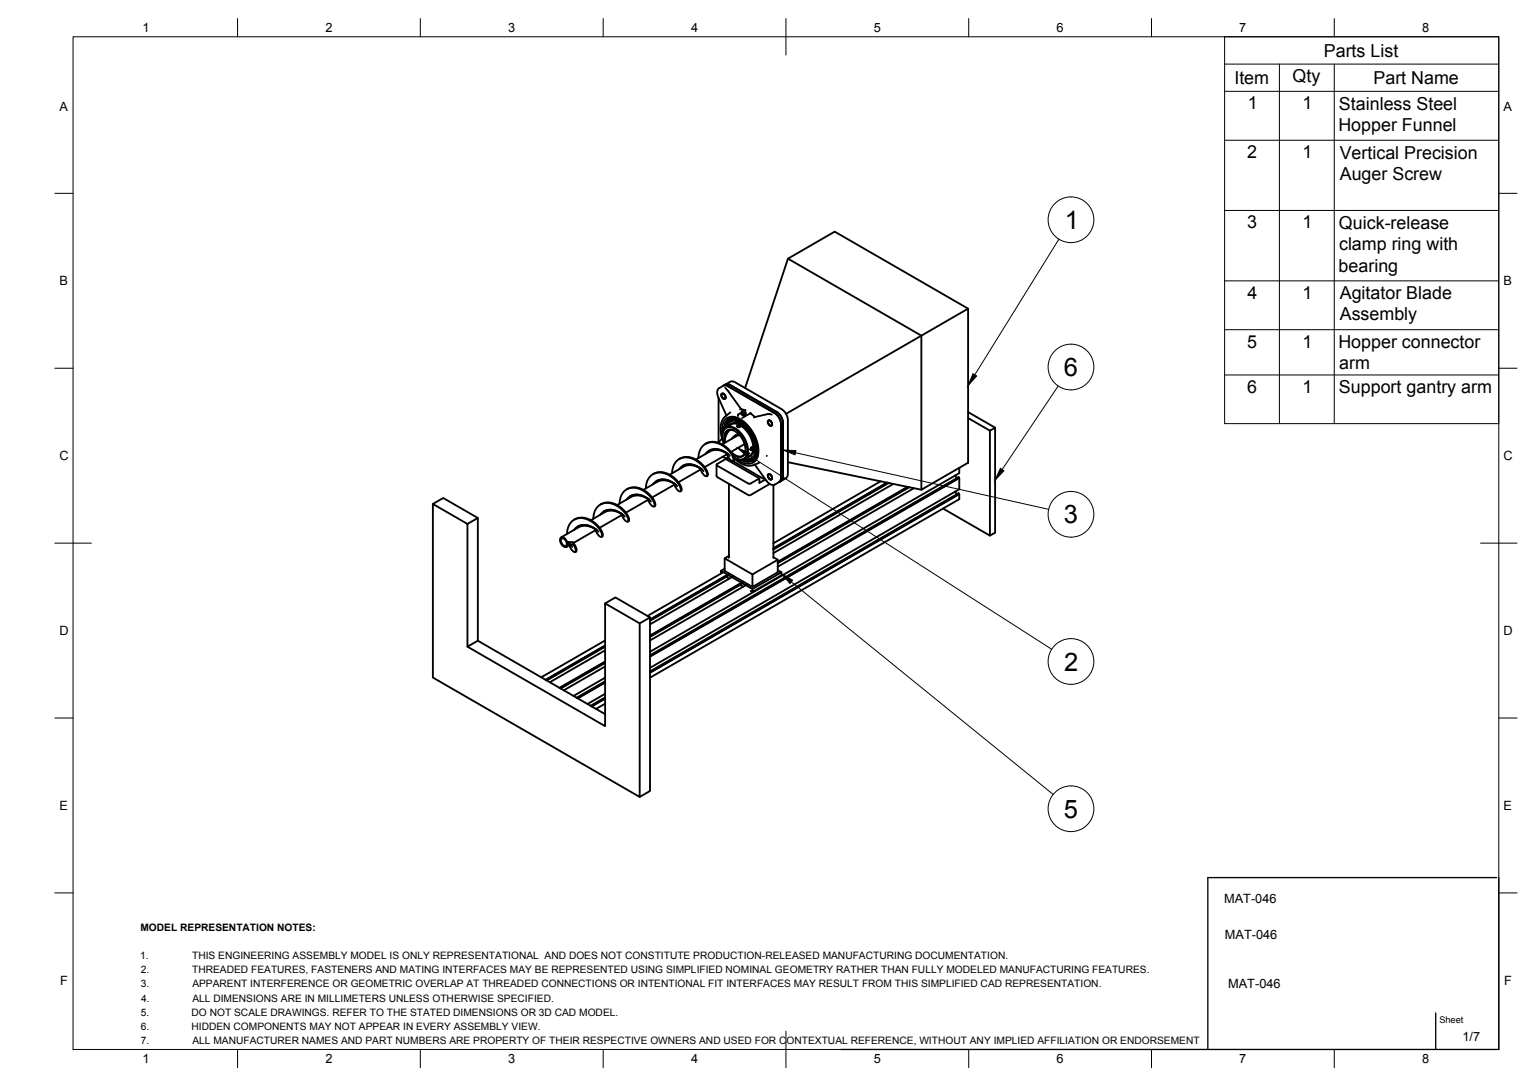
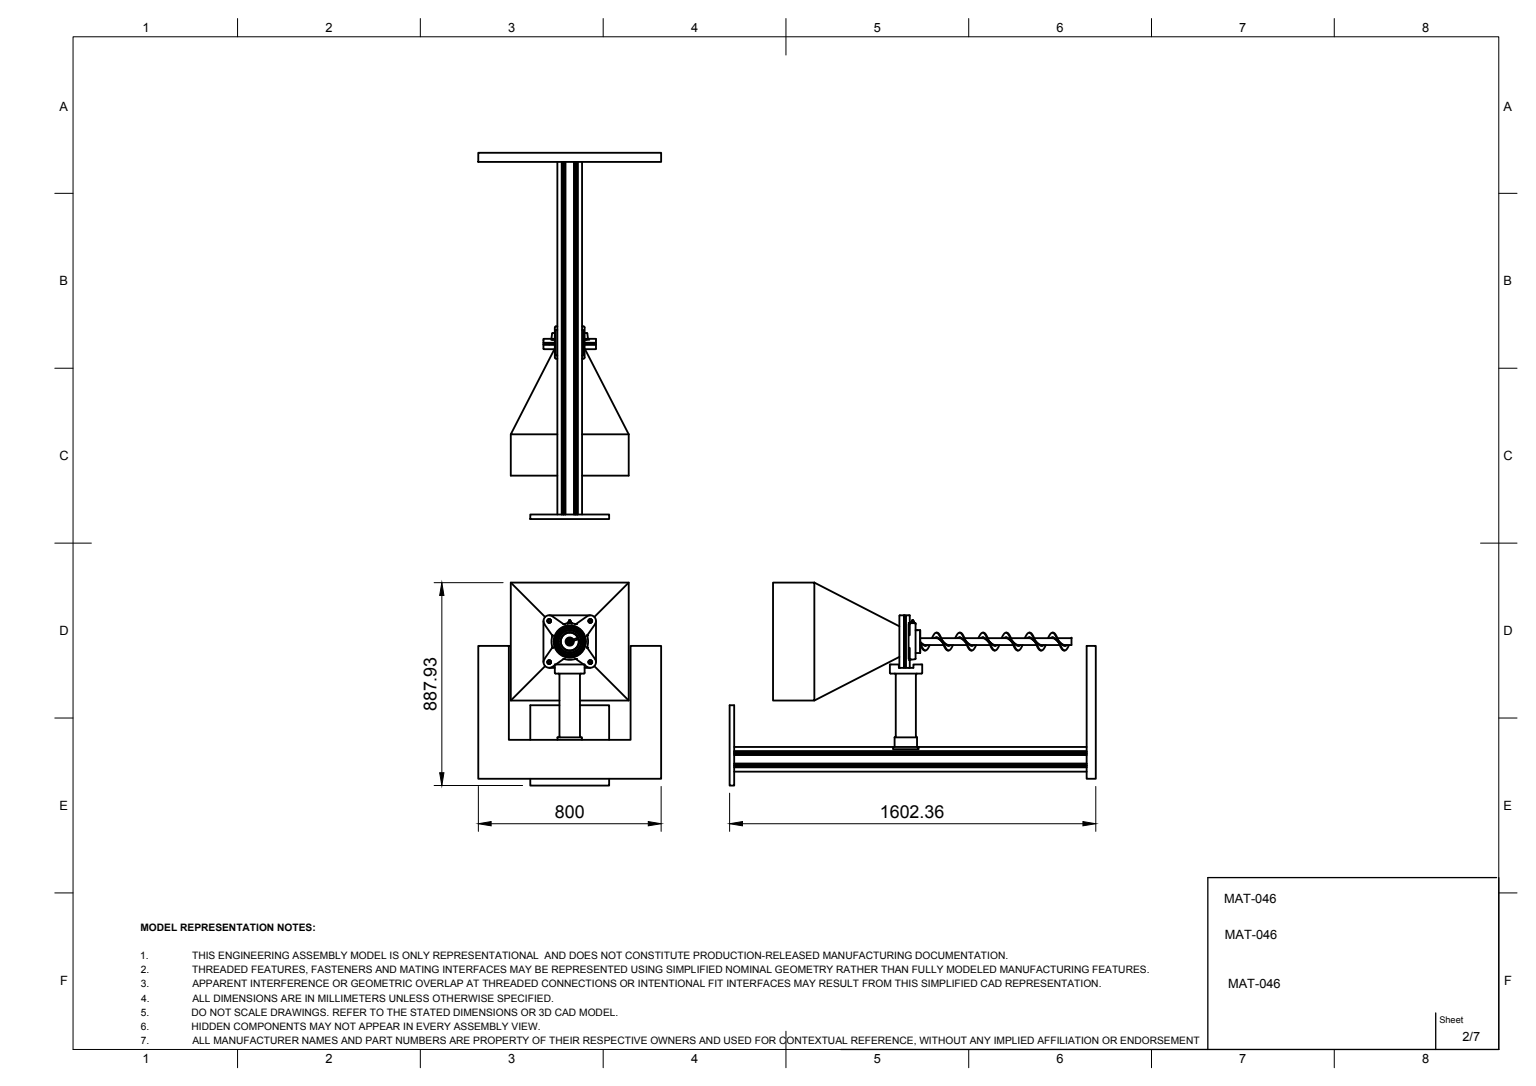
ISO-10303-21;
HEADER;
/* Generated by software containing ST-Developer
 * from STEP Tools, Inc. (www.steptools.com) 
 */

FILE_DESCRIPTION(
/* description */ ('STEP AP214'),
/* implementation_level */ '2;1');

FILE_NAME(
/* name */ 'MAT-046.step',
/* time_stamp */ '2026-11-14T22:16:48-08:00',
/* author */ (''),
/* organization */ (''),
/* preprocessor_version */ 'ST-DEVELOPER v20.2',
/* originating_system */ 'Autodesk Translation Framework v15.17.0.0',
/* authorisation */ '');

FILE_SCHEMA (('AUTOMOTIVE_DESIGN { 1 0 10303 214 3 1 1 }'));
ENDSEC;

DATA;
#10=MECHANICAL_DESIGN_GEOMETRIC_PRESENTATION_REPRESENTATION('',(#5472,#5473,
#5474,#5475,#5476,#5477,#5478,#5479,#5480,#5481,#5482,#5483,#5484,#5485,
#5486,#5487,#5488,#5489,#5490,#5491,#5492,#5493,#5494,#5495,#5496,#5497,
#5498,#5499,#5500),#276462);
#11=ITEM_DEFINED_TRANSFORMATION($,$,#98803,#111667);
#12=ITEM_DEFINED_TRANSFORMATION($,$,#98875,#111668);
#13=ITEM_DEFINED_TRANSFORMATION($,$,#98939,#111669);
#14=ITEM_DEFINED_TRANSFORMATION($,$,#110834,#111670);
#15=ITEM_DEFINED_TRANSFORMATION($,$,#110875,#111671);
#16=ITEM_DEFINED_TRANSFORMATION($,$,#110986,#111672);
#17=(
REPRESENTATION_RELATIONSHIP($,$,#276488,#276487)
REPRESENTATION_RELATIONSHIP_WITH_TRANSFORMATION(#11)
SHAPE_REPRESENTATION_RELATIONSHIP()
);
#18=(
REPRESENTATION_RELATIONSHIP($,$,#276489,#276487)
REPRESENTATION_RELATIONSHIP_WITH_TRANSFORMATION(#12)
SHAPE_REPRESENTATION_RELATIONSHIP()
);
#19=(
REPRESENTATION_RELATIONSHIP($,$,#276490,#276487)
REPRESENTATION_RELATIONSHIP_WITH_TRANSFORMATION(#13)
SHAPE_REPRESENTATION_RELATIONSHIP()
);
#20=(
REPRESENTATION_RELATIONSHIP($,$,#276491,#276487)
REPRESENTATION_RELATIONSHIP_WITH_TRANSFORMATION(#14)
SHAPE_REPRESENTATION_RELATIONSHIP()
);
#21=(
REPRESENTATION_RELATIONSHIP($,$,#276492,#276487)
REPRESENTATION_RELATIONSHIP_WITH_TRANSFORMATION(#15)
SHAPE_REPRESENTATION_RELATIONSHIP()
);
#22=(
REPRESENTATION_RELATIONSHIP($,$,#276493,#276487)
REPRESENTATION_RELATIONSHIP_WITH_TRANSFORMATION(#16)
SHAPE_REPRESENTATION_RELATIONSHIP()
);
#23=CONTEXT_DEPENDENT_SHAPE_REPRESENTATION(#17,#276481);
#24=CONTEXT_DEPENDENT_SHAPE_REPRESENTATION(#18,#276482);
#25=CONTEXT_DEPENDENT_SHAPE_REPRESENTATION(#19,#276483);
#26=CONTEXT_DEPENDENT_SHAPE_REPRESENTATION(#20,#276484);
#27=CONTEXT_DEPENDENT_SHAPE_REPRESENTATION(#21,#276485);
#28=CONTEXT_DEPENDENT_SHAPE_REPRESENTATION(#22,#276486);
#29=NEXT_ASSEMBLY_USAGE_OCCURRENCE('Stainless Steel Hopper Funnel:1',
'Stainless Steel Hopper Funnel:1','Stainless Steel Hopper Funnel:1',#276495,
#276496,'Stainless Steel Hopper Funnel:1');
#30=NEXT_ASSEMBLY_USAGE_OCCURRENCE('Vertical Precision Auger Screw:1',
'Vertical Precision Auger Screw:1','Vertical Precision Auger Screw:1',#276495,
#276497,'Vertical Precision Auger Screw:1');
#31=NEXT_ASSEMBLY_USAGE_OCCURRENCE(
'Quick-release clamp ring with bearing:1',
'Quick-release clamp ring with bearing:1',
'Quick-release clamp ring with bearing:1',#276495,#276498,
'Quick-release clamp ring with bearing:1');
#32=NEXT_ASSEMBLY_USAGE_OCCURRENCE('Agitator Blade Assembly:1',
'Agitator Blade Assembly:1','Agitator Blade Assembly:1',#276495,#276499,
'Agitator Blade Assembly:1');
#33=NEXT_ASSEMBLY_USAGE_OCCURRENCE('hopper connector arm:1',
'hopper connector arm:1','hopper connector arm:1',#276495,#276500,
'hopper connector arm:1');
#34=NEXT_ASSEMBLY_USAGE_OCCURRENCE('support gantry arm:1',
'support gantry arm:1','support gantry arm:1',#276495,#276501,
'support gantry arm:1');
#35=ORIENTED_CLOSED_SHELL('',*,#98725,.F.);
#36=ORIENTED_CLOSED_SHELL('',*,#98726,.F.);
#37=ORIENTED_CLOSED_SHELL('',*,#98727,.F.);
#38=ORIENTED_CLOSED_SHELL('',*,#98728,.F.);
#39=ORIENTED_CLOSED_SHELL('',*,#98729,.F.);
#40=ORIENTED_CLOSED_SHELL('',*,#98730,.F.);
#41=ORIENTED_CLOSED_SHELL('',*,#98731,.F.);
#42=ORIENTED_CLOSED_SHELL('',*,#98732,.F.);
#43=ORIENTED_CLOSED_SHELL('',*,#98733,.F.);
#44=BREP_WITH_VOIDS('Body1',#98734,(#35,#36,#37,#38,#39,#40,#41,#42,#43));
#45=SPHERICAL_SURFACE('',#98960,3.37686862486535);
#46=SPHERICAL_SURFACE('',#110483,1.905);
#47=SPHERICAL_SURFACE('',#110485,1.905);
#48=SPHERICAL_SURFACE('',#110508,0.952499999999998);
#49=SPHERICAL_SURFACE('',#110528,3.17500000000001);
#50=CONICAL_SURFACE('',#98946,5.55625,1.0471975511966);
#51=CONICAL_SURFACE('',#98951,5.55625,1.0471975511966);
#52=CONICAL_SURFACE('',#98954,3.78554799125932,1.22012705768434);
#53=CONICAL_SURFACE('',#98966,2.40973730802039,0.353951387855692);
#54=CONICAL_SURFACE('',#98977,5.55625,1.0471975511966);
#55=CONICAL_SURFACE('',#98978,5.55625,1.0471975511966);
#56=CONICAL_SURFACE('',#98979,5.55625,1.0471975511966);
#57=CONICAL_SURFACE('',#98980,5.55625,1.0471975511966);
#58=CONICAL_SURFACE('',#98981,5.55625,1.0471975511966);
#59=CONICAL_SURFACE('',#98989,5.55625,1.0471975511966);
#60=CONICAL_SURFACE('',#98990,5.55625,1.0471975511966);
#61=CONICAL_SURFACE('',#98991,5.55625,1.0471975511966);
#62=CONICAL_SURFACE('',#98992,5.55625,1.0471975511966);
#63=CONICAL_SURFACE('',#98993,5.55625,1.0471975511966);
#64=CONICAL_SURFACE('',#99119,64.0080199038439,0.558505360638178);
#65=CONICAL_SURFACE('',#99120,62.2224557307631,0.558505360638175);
#66=CONICAL_SURFACE('',#99239,58.6605641730809,0.558505360638184);
#67=CONICAL_SURFACE('',#99359,56.875,0.558505360638184);
#68=CONICAL_SURFACE('',#99369,60.4792282238308,0.523598775598302);
#69=CONICAL_SURFACE('',#99374,61.15975,0.523598775598289);
#70=CONICAL_SURFACE('',#99398,60.4792282238308,0.523598775598302);
#71=CONICAL_SURFACE('',#99403,61.15975,0.523598775598289);
#72=CONICAL_SURFACE('',#99427,60.4792282238308,0.523598775598302);
#73=CONICAL_SURFACE('',#99432,61.15975,0.523598775598289);
#74=CONICAL_SURFACE('',#99456,60.4792282238308,0.523598775598302);
#75=CONICAL_SURFACE('',#99461,61.15975,0.523598775598289);
#76=CONICAL_SURFACE('',#99485,60.4792282238308,0.523598775598302);
#77=CONICAL_SURFACE('',#99490,61.15975,0.523598775598289);
#78=CONICAL_SURFACE('',#99514,60.4792282238308,0.523598775598302);
#79=CONICAL_SURFACE('',#99519,61.15975,0.523598775598289);
#80=CONICAL_SURFACE('',#99543,60.4792282238308,0.523598775598302);
#81=CONICAL_SURFACE('',#99548,61.15975,0.523598775598289);
#82=CONICAL_SURFACE('',#99572,60.4792282238308,0.523598775598302);
#83=CONICAL_SURFACE('',#99577,61.15975,0.523598775598289);
#84=CONICAL_SURFACE('',#99601,60.4792282238308,0.523598775598302);
#85=CONICAL_SURFACE('',#99606,61.15975,0.523598775598289);
#86=CONICAL_SURFACE('',#99630,60.4792282238308,0.523598775598302);
#87=CONICAL_SURFACE('',#99635,61.15975,0.523598775598289);
#88=CONICAL_SURFACE('',#99659,60.4792282238308,0.523598775598302);
#89=CONICAL_SURFACE('',#99664,61.15975,0.523598775598289);
#90=CONICAL_SURFACE('',#99688,60.4792282238308,0.523598775598302);
#91=CONICAL_SURFACE('',#99693,61.15975,0.523598775598289);
#92=CONICAL_SURFACE('',#99717,60.4792282238308,0.523598775598302);
#93=CONICAL_SURFACE('',#99722,61.15975,0.523598775598289);
#94=CONICAL_SURFACE('',#99746,60.4792282238308,0.523598775598302);
#95=CONICAL_SURFACE('',#99751,61.15975,0.523598775598289);
#96=CONICAL_SURFACE('',#99775,60.4792282238308,0.523598775598302);
#97=CONICAL_SURFACE('',#99780,61.15975,0.523598775598289);
#98=CONICAL_SURFACE('',#99804,60.4792282238308,0.523598775598302);
#99=CONICAL_SURFACE('',#99809,61.15975,0.523598775598289);
#100=CONICAL_SURFACE('',#99833,60.4792282238308,0.523598775598302);
#101=CONICAL_SURFACE('',#99838,61.15975,0.523598775598289);
#102=CONICAL_SURFACE('',#99862,60.4792282238308,0.523598775598302);
#103=CONICAL_SURFACE('',#99867,61.15975,0.523598775598289);
#104=CONICAL_SURFACE('',#99891,60.4792282238308,0.523598775598302);
#105=CONICAL_SURFACE('',#99896,61.15975,0.523598775598289);
#106=CONICAL_SURFACE('',#99920,60.4792282238308,0.523598775598302);
#107=CONICAL_SURFACE('',#99925,61.15975,0.523598775598289);
#108=CONICAL_SURFACE('',#99949,60.4792282238308,0.523598775598302);
#109=CONICAL_SURFACE('',#99954,61.15975,0.523598775598289);
#110=CONICAL_SURFACE('',#99978,60.4792282238308,0.523598775598302);
#111=CONICAL_SURFACE('',#99983,61.15975,0.523598775598289);
#112=CONICAL_SURFACE('',#100007,60.4792282238308,0.523598775598302);
#113=CONICAL_SURFACE('',#100012,61.15975,0.523598775598289);
#114=CONICAL_SURFACE('',#100036,60.4792282238308,0.523598775598302);
#115=CONICAL_SURFACE('',#100041,61.15975,0.523598775598289);
#116=CONICAL_SURFACE('',#100065,60.4792282238308,0.523598775598302);
#117=CONICAL_SURFACE('',#100070,61.15975,0.523598775598289);
#118=CONICAL_SURFACE('',#100094,60.4792282238308,0.523598775598302);
#119=CONICAL_SURFACE('',#100099,61.15975,0.523598775598289);
#120=CONICAL_SURFACE('',#100123,60.4792282238308,0.523598775598302);
#121=CONICAL_SURFACE('',#100128,61.15975,0.523598775598289);
#122=CONICAL_SURFACE('',#100152,60.4792282238308,0.523598775598302);
#123=CONICAL_SURFACE('',#100157,61.15975,0.523598775598289);
#124=CONICAL_SURFACE('',#100181,60.4792282238308,0.523598775598302);
#125=CONICAL_SURFACE('',#100186,61.15975,0.523598775598289);
#126=CONICAL_SURFACE('',#100210,60.4792282238308,0.523598775598302);
#127=CONICAL_SURFACE('',#100215,61.15975,0.523598775598289);
#128=CONICAL_SURFACE('',#100239,60.4792282238308,0.523598775598302);
#129=CONICAL_SURFACE('',#100244,61.15975,0.523598775598289);
#130=CONICAL_SURFACE('',#100268,60.4792282238308,0.523598775598302);
#131=CONICAL_SURFACE('',#100273,61.15975,0.523598775598289);
#132=CONICAL_SURFACE('',#100297,60.4792282238308,0.523598775598302);
#133=CONICAL_SURFACE('',#100302,61.15975,0.523598775598289);
#134=CONICAL_SURFACE('',#100326,60.4792282238308,0.523598775598302);
#135=CONICAL_SURFACE('',#100331,61.15975,0.523598775598289);
#136=CONICAL_SURFACE('',#100355,60.4792282238308,0.523598775598302);
#137=CONICAL_SURFACE('',#100360,61.15975,0.523598775598289);
#138=CONICAL_SURFACE('',#100384,60.4792282238308,0.523598775598302);
#139=CONICAL_SURFACE('',#100389,61.15975,0.523598775598289);
#140=CONICAL_SURFACE('',#100413,60.4792282238308,0.523598775598302);
#141=CONICAL_SURFACE('',#100418,61.15975,0.523598775598289);
#142=CONICAL_SURFACE('',#100442,60.4792282238308,0.523598775598302);
#143=CONICAL_SURFACE('',#100447,61.15975,0.523598775598289);
#144=CONICAL_SURFACE('',#100471,60.4792282238308,0.523598775598302);
#145=CONICAL_SURFACE('',#100476,61.15975,0.523598775598289);
#146=CONICAL_SURFACE('',#100500,60.4792282238308,0.523598775598302);
#147=CONICAL_SURFACE('',#100505,61.15975,0.523598775598289);
#148=CONICAL_SURFACE('',#100529,60.4792282238308,0.523598775598302);
#149=CONICAL_SURFACE('',#100534,61.15975,0.523598775598289);
#150=CONICAL_SURFACE('',#100558,60.4792282238308,0.523598775598302);
#151=CONICAL_SURFACE('',#100563,61.15975,0.523598775598289);
#152=CONICAL_SURFACE('',#100587,60.4792282238308,0.523598775598302);
#153=CONICAL_SURFACE('',#100592,61.15975,0.523598775598289);
#154=CONICAL_SURFACE('',#100616,60.4792282238308,0.523598775598302);
#155=CONICAL_SURFACE('',#100621,61.15975,0.523598775598289);
#156=CONICAL_SURFACE('',#100645,60.4792282238308,0.523598775598302);
#157=CONICAL_SURFACE('',#100650,61.15975,0.523598775598289);
#158=CONICAL_SURFACE('',#100674,60.4792282238308,0.523598775598302);
#159=CONICAL_SURFACE('',#100679,61.15975,0.523598775598289);
#160=CONICAL_SURFACE('',#100703,60.4792282238308,0.523598775598302);
#161=CONICAL_SURFACE('',#100708,61.15975,0.523598775598289);
#162=CONICAL_SURFACE('',#100732,60.4792282238308,0.523598775598302);
#163=CONICAL_SURFACE('',#100737,61.15975,0.523598775598289);
#164=CONICAL_SURFACE('',#100761,60.4792282238308,0.523598775598302);
#165=CONICAL_SURFACE('',#100766,61.15975,0.523598775598289);
#166=CONICAL_SURFACE('',#100790,60.4792282238308,0.523598775598302);
#167=CONICAL_SURFACE('',#100795,61.15975,0.523598775598289);
#168=CONICAL_SURFACE('',#100819,60.4792282238308,0.523598775598302);
#169=CONICAL_SURFACE('',#100824,61.15975,0.523598775598289);
#170=CONICAL_SURFACE('',#100848,60.4792282238308,0.523598775598302);
#171=CONICAL_SURFACE('',#100853,61.15975,0.523598775598289);
#172=CONICAL_SURFACE('',#100877,60.4792282238308,0.523598775598302);
#173=CONICAL_SURFACE('',#100882,61.15975,0.523598775598289);
#174=CONICAL_SURFACE('',#100906,60.4792282238308,0.523598775598302);
#175=CONICAL_SURFACE('',#100911,61.15975,0.523598775598289);
#176=CONICAL_SURFACE('',#100935,60.4792282238308,0.523598775598302);
#177=CONICAL_SURFACE('',#100940,61.15975,0.523598775598289);
#178=CONICAL_SURFACE('',#100964,60.4792282238308,0.523598775598302);
#179=CONICAL_SURFACE('',#100969,61.15975,0.523598775598289);
#180=CONICAL_SURFACE('',#100993,60.4792282238308,0.523598775598302);
#181=CONICAL_SURFACE('',#100998,61.15975,0.523598775598289);
#182=CONICAL_SURFACE('',#101022,60.4792282238308,0.523598775598302);
#183=CONICAL_SURFACE('',#101027,61.15975,0.523598775598289);
#184=CONICAL_SURFACE('',#101051,60.4792282238308,0.523598775598302);
#185=CONICAL_SURFACE('',#101056,61.15975,0.523598775598289);
#186=CONICAL_SURFACE('',#101081,60.4792282238308,0.523598775598302);
#187=CONICAL_SURFACE('',#101086,61.15975,0.523598775598289);
#188=CONICAL_SURFACE('',#104673,64.0080199038439,0.558505360638178);
#189=CONICAL_SURFACE('',#104674,62.2224557307631,0.558505360638175);
#190=CONICAL_SURFACE('',#104793,58.6605641730809,0.558505360638184);
#191=CONICAL_SURFACE('',#104913,56.875,0.558505360638184);
#192=CONICAL_SURFACE('',#104923,60.4792282238308,0.523598775598302);
#193=CONICAL_SURFACE('',#104928,61.15975,0.523598775598289);
#194=CONICAL_SURFACE('',#104952,60.4792282238308,0.523598775598302);
#195=CONICAL_SURFACE('',#104957,61.15975,0.523598775598289);
#196=CONICAL_SURFACE('',#104981,60.4792282238308,0.523598775598302);
#197=CONICAL_SURFACE('',#104986,61.15975,0.523598775598289);
#198=CONICAL_SURFACE('',#105010,60.4792282238308,0.523598775598302);
#199=CONICAL_SURFACE('',#105015,61.15975,0.523598775598289);
#200=CONICAL_SURFACE('',#105039,60.4792282238308,0.523598775598302);
#201=CONICAL_SURFACE('',#105044,61.15975,0.523598775598289);
#202=CONICAL_SURFACE('',#105068,60.4792282238308,0.523598775598302);
#203=CONICAL_SURFACE('',#105073,61.15975,0.523598775598289);
#204=CONICAL_SURFACE('',#105097,60.4792282238308,0.523598775598302);
#205=CONICAL_SURFACE('',#105102,61.15975,0.523598775598289);
#206=CONICAL_SURFACE('',#105126,60.4792282238308,0.523598775598302);
#207=CONICAL_SURFACE('',#105131,61.15975,0.523598775598289);
#208=CONICAL_SURFACE('',#105155,60.4792282238308,0.523598775598302);
#209=CONICAL_SURFACE('',#105160,61.15975,0.523598775598289);
#210=CONICAL_SURFACE('',#105184,60.4792282238308,0.523598775598302);
#211=CONICAL_SURFACE('',#105189,61.15975,0.523598775598289);
#212=CONICAL_SURFACE('',#105213,60.4792282238308,0.523598775598302);
#213=CONICAL_SURFACE('',#105218,61.15975,0.523598775598289);
#214=CONICAL_SURFACE('',#105242,60.4792282238308,0.523598775598302);
#215=CONICAL_SURFACE('',#105247,61.15975,0.523598775598289);
#216=CONICAL_SURFACE('',#105271,60.4792282238308,0.523598775598302);
#217=CONICAL_SURFACE('',#105276,61.15975,0.523598775598289);
#218=CONICAL_SURFACE('',#105300,60.4792282238308,0.523598775598302);
#219=CONICAL_SURFACE('',#105305,61.15975,0.523598775598289);
#220=CONICAL_SURFACE('',#105329,60.4792282238308,0.523598775598302);
#221=CONICAL_SURFACE('',#105334,61.15975,0.523598775598289);
#222=CONICAL_SURFACE('',#105358,60.4792282238308,0.523598775598302);
#223=CONICAL_SURFACE('',#105363,61.15975,0.523598775598289);
#224=CONICAL_SURFACE('',#105387,60.4792282238308,0.523598775598302);
#225=CONICAL_SURFACE('',#105392,61.15975,0.523598775598289);
#226=CONICAL_SURFACE('',#105416,60.4792282238308,0.523598775598302);
#227=CONICAL_SURFACE('',#105421,61.15975,0.523598775598289);
#228=CONICAL_SURFACE('',#105445,60.4792282238308,0.523598775598302);
#229=CONICAL_SURFACE('',#105450,61.15975,0.523598775598289);
#230=CONICAL_SURFACE('',#105474,60.4792282238308,0.523598775598302);
#231=CONICAL_SURFACE('',#105479,61.15975,0.523598775598289);
#232=CONICAL_SURFACE('',#105503,60.4792282238308,0.523598775598302);
#233=CONICAL_SURFACE('',#105508,61.15975,0.523598775598289);
#234=CONICAL_SURFACE('',#105532,60.4792282238308,0.523598775598302);
#235=CONICAL_SURFACE('',#105537,61.15975,0.523598775598289);
#236=CONICAL_SURFACE('',#105561,60.4792282238308,0.523598775598302);
#237=CONICAL_SURFACE('',#105566,61.15975,0.523598775598289);
#238=CONICAL_SURFACE('',#105590,60.4792282238308,0.523598775598302);
#239=CONICAL_SURFACE('',#105595,61.15975,0.523598775598289);
#240=CONICAL_SURFACE('',#105619,60.4792282238308,0.523598775598302);
#241=CONICAL_SURFACE('',#105624,61.15975,0.523598775598289);
#242=CONICAL_SURFACE('',#105648,60.4792282238308,0.523598775598302);
#243=CONICAL_SURFACE('',#105653,61.15975,0.523598775598289);
#244=CONICAL_SURFACE('',#105677,60.4792282238308,0.523598775598302);
#245=CONICAL_SURFACE('',#105682,61.15975,0.523598775598289);
#246=CONICAL_SURFACE('',#105706,60.4792282238308,0.523598775598302);
#247=CONICAL_SURFACE('',#105711,61.15975,0.523598775598289);
#248=CONICAL_SURFACE('',#105735,60.4792282238308,0.523598775598302);
#249=CONICAL_SURFACE('',#105740,61.15975,0.523598775598289);
#250=CONICAL_SURFACE('',#105764,60.4792282238308,0.523598775598302);
#251=CONICAL_SURFACE('',#105769,61.15975,0.523598775598289);
#252=CONICAL_SURFACE('',#105793,60.4792282238308,0.523598775598302);
#253=CONICAL_SURFACE('',#105798,61.15975,0.523598775598289);
#254=CONICAL_SURFACE('',#105822,60.4792282238308,0.523598775598302);
#255=CONICAL_SURFACE('',#105827,61.15975,0.523598775598289);
#256=CONICAL_SURFACE('',#105851,60.4792282238308,0.523598775598302);
#257=CONICAL_SURFACE('',#105856,61.15975,0.523598775598289);
#258=CONICAL_SURFACE('',#105880,60.4792282238308,0.523598775598302);
#259=CONICAL_SURFACE('',#105885,61.15975,0.523598775598289);
#260=CONICAL_SURFACE('',#105909,60.4792282238308,0.523598775598302);
#261=CONICAL_SURFACE('',#105914,61.15975,0.523598775598289);
#262=CONICAL_SURFACE('',#105938,60.4792282238308,0.523598775598302);
#263=CONICAL_SURFACE('',#105943,61.15975,0.523598775598289);
#264=CONICAL_SURFACE('',#105967,60.4792282238308,0.523598775598302);
#265=CONICAL_SURFACE('',#105972,61.15975,0.523598775598289);
#266=CONICAL_SURFACE('',#105996,60.4792282238308,0.523598775598302);
#267=CONICAL_SURFACE('',#106001,61.15975,0.523598775598289);
#268=CONICAL_SURFACE('',#106025,60.4792282238308,0.523598775598302);
#269=CONICAL_SURFACE('',#106030,61.15975,0.523598775598289);
#270=CONICAL_SURFACE('',#106054,60.4792282238308,0.523598775598302);
#271=CONICAL_SURFACE('',#106059,61.15975,0.523598775598289);
#272=CONICAL_SURFACE('',#106083,60.4792282238308,0.523598775598302);
#273=CONICAL_SURFACE('',#106088,61.15975,0.523598775598289);
#274=CONICAL_SURFACE('',#106112,60.4792282238308,0.523598775598302);
#275=CONICAL_SURFACE('',#106117,61.15975,0.523598775598289);
#276=CONICAL_SURFACE('',#106141,60.4792282238308,0.523598775598302);
#277=CONICAL_SURFACE('',#106146,61.15975,0.523598775598289);
#278=CONICAL_SURFACE('',#106170,60.4792282238308,0.523598775598302);
#279=CONICAL_SURFACE('',#106175,61.15975,0.523598775598289);
#280=CONICAL_SURFACE('',#106199,60.4792282238308,0.523598775598302);
#281=CONICAL_SURFACE('',#106204,61.15975,0.523598775598289);
#282=CONICAL_SURFACE('',#106228,60.4792282238308,0.523598775598302);
#283=CONICAL_SURFACE('',#106233,61.15975,0.523598775598289);
#284=CONICAL_SURFACE('',#106257,60.4792282238308,0.523598775598302);
#285=CONICAL_SURFACE('',#106262,61.15975,0.523598775598289);
#286=CONICAL_SURFACE('',#106286,60.4792282238308,0.523598775598302);
#287=CONICAL_SURFACE('',#106291,61.15975,0.523598775598289);
#288=CONICAL_SURFACE('',#106315,60.4792282238308,0.523598775598302);
#289=CONICAL_SURFACE('',#106320,61.15975,0.523598775598289);
#290=CONICAL_SURFACE('',#106344,60.4792282238308,0.523598775598302);
#291=CONICAL_SURFACE('',#106349,61.15975,0.523598775598289);
#292=CONICAL_SURFACE('',#106373,60.4792282238308,0.523598775598302);
#293=CONICAL_SURFACE('',#106378,61.15975,0.523598775598289);
#294=CONICAL_SURFACE('',#106402,60.4792282238308,0.523598775598302);
#295=CONICAL_SURFACE('',#106407,61.15975,0.523598775598289);
#296=CONICAL_SURFACE('',#106431,60.4792282238308,0.523598775598302);
#297=CONICAL_SURFACE('',#106436,61.15975,0.523598775598289);
#298=CONICAL_SURFACE('',#106460,60.4792282238308,0.523598775598302);
#299=CONICAL_SURFACE('',#106465,61.15975,0.523598775598289);
#300=CONICAL_SURFACE('',#106489,60.4792282238308,0.523598775598302);
#301=CONICAL_SURFACE('',#106494,61.15975,0.523598775598289);
#302=CONICAL_SURFACE('',#106518,60.4792282238308,0.523598775598302);
#303=CONICAL_SURFACE('',#106523,61.15975,0.523598775598289);
#304=CONICAL_SURFACE('',#106547,60.4792282238308,0.523598775598302);
#305=CONICAL_SURFACE('',#106552,61.15975,0.523598775598289);
#306=CONICAL_SURFACE('',#106576,60.4792282238308,0.523598775598302);
#307=CONICAL_SURFACE('',#106581,61.15975,0.523598775598289);
#308=CONICAL_SURFACE('',#106605,60.4792282238308,0.523598775598302);
#309=CONICAL_SURFACE('',#106610,61.15975,0.523598775598289);
#310=CONICAL_SURFACE('',#106635,60.4792282238308,0.523598775598302);
#311=CONICAL_SURFACE('',#106640,61.15975,0.523598775598289);
#312=CONICAL_SURFACE('',#110283,80.,0.122173047639603);
#313=CONICAL_SURFACE('',#110573,56.2993860673093,0.55850536063818);
#314=CONICAL_SURFACE('',#110574,57.8669800961561,0.558505360638184);
#315=CONICAL_SURFACE('',#110605,4.74980000000001,0.78539816339745);
#316=CONICAL_SURFACE('',#110610,3.98780000000001,0.785398163397452);
#317=CONICAL_SURFACE('',#110625,2.7496306570156,0.78539816339745);
#318=CONICAL_SURFACE('',#110626,2.7496306570156,0.78539816339745);
#319=CONICAL_SURFACE('',#110627,2.7496306570156,0.78539816339745);
#320=CONICAL_SURFACE('',#110628,2.7496306570156,0.78539816339745);
#321=CONICAL_SURFACE('',#110629,2.7496306570156,0.78539816339745);
#322=CONICAL_SURFACE('',#110630,2.7496306570156,0.78539816339745);
#323=CONICAL_SURFACE('',#110657,4.74980000000001,0.78539816339745);
#324=CONICAL_SURFACE('',#110662,3.98780000000001,0.785398163397452);
#325=CONICAL_SURFACE('',#110677,2.7496306570156,0.78539816339745);
#326=CONICAL_SURFACE('',#110678,2.7496306570156,0.78539816339745);
#327=CONICAL_SURFACE('',#110679,2.7496306570156,0.78539816339745);
#328=CONICAL_SURFACE('',#110680,2.7496306570156,0.78539816339745);
#329=CONICAL_SURFACE('',#110681,2.7496306570156,0.78539816339745);
#330=CONICAL_SURFACE('',#110682,2.7496306570156,0.78539816339745);
#331=CONICAL_SURFACE('',#110691,40.,0.698131700797724);
#332=CONICAL_SURFACE('',#110694,40.,0.698131700797741);
#333=CONICAL_SURFACE('',#110698,48.4864729374055,0.872664625997157);
#334=CONICAL_SURFACE('',#110701,48.4864729374054,0.872664625997163);
#335=CONICAL_SURFACE('',#110842,3.4,1.02974425867665);
#336=ELLIPSE('',#98932,245.0752161313,242.710009632518);
#337=ELLIPSE('',#98935,18.0481778016316,18.048088900566);
#338=ELLIPSE('',#99385,0.599370291563849,0.555629413547353);
#339=ELLIPSE('',#99386,0.599370913936212,0.555630771247294);
#340=ELLIPSE('',#99388,0.239805704052526,0.222043163089743);
#341=ELLIPSE('',#99389,0.239805889069737,0.222043643391604);
#342=ELLIPSE('',#99391,0.239805882895812,0.222043378689669);
#343=ELLIPSE('',#99392,0.239805697268466,0.22204289662789);
#344=ELLIPSE('',#99414,0.599370913936647,0.555630771248094);
#345=ELLIPSE('',#99415,0.599370291565284,0.555629413550211);
#346=ELLIPSE('',#99417,0.239805889071228,0.222043643394759);
#347=ELLIPSE('',#99418,0.239805704054646,0.222043163093994);
#348=ELLIPSE('',#99420,0.239805697269572,0.222042896630273);
#349=ELLIPSE('',#99421,0.239805882893992,0.222043378685954);
#350=ELLIPSE('',#99443,0.599370913939605,0.555630771254153);
#351=ELLIPSE('',#99444,0.599370291563661,0.555629413546882);
#352=ELLIPSE('',#99446,0.23980588906817,0.222043643388294);
#353=ELLIPSE('',#99447,0.239805704052944,0.222043163090554);
#354=ELLIPSE('',#99449,0.239805697268366,0.222042896627733);
#355=ELLIPSE('',#99450,0.239805882894834,0.222043378687724);
#356=ELLIPSE('',#99472,0.599370913938154,0.55563077125104);
#357=ELLIPSE('',#99473,0.59937029156276,0.555629413545193);
#358=ELLIPSE('',#99475,0.239805889066608,0.222043643385116);
#359=ELLIPSE('',#99476,0.239805704053829,0.22204316309239);
#360=ELLIPSE('',#99478,0.239805697267153,0.222042896625171);
#361=ELLIPSE('',#99479,0.239805882894158,0.222043378686371);
#362=ELLIPSE('',#99501,0.599370913936745,0.55563077124828);
#363=ELLIPSE('',#99502,0.599370291565539,0.555629413550565);
#364=ELLIPSE('',#99504,0.239805889071284,0.222043643394696);
#365=ELLIPSE('',#99505,0.239805704051857,0.222043163088228);
#366=ELLIPSE('',#99507,0.239805697269279,0.222042896629737);
#367=ELLIPSE('',#99508,0.239805882895886,0.222043378689775);
#368=ELLIPSE('',#99530,0.599370913935051,0.555630771244647);
#369=ELLIPSE('',#99531,0.599370291563104,0.555629413545832);
#370=ELLIPSE('',#99533,0.239805889067115,0.222043643386276);
#371=ELLIPSE('',#99534,0.239805704053193,0.222043163090947);
#372=ELLIPSE('',#99536,0.239805697268009,0.222042896626989);
#373=ELLIPSE('',#99537,0.239805882895764,0.222043378689474);
#374=ELLIPSE('',#99559,0.599370913937216,0.555630771249188);
#375=ELLIPSE('',#99560,0.599370291563396,0.555629413546297);
#376=ELLIPSE('',#99562,0.239805889067743,0.222043643387537);
#377=ELLIPSE('',#99563,0.239805704055465,0.222043163095698);
#378=ELLIPSE('',#99565,0.239805697269418,0.222042896629816);
#379=ELLIPSE('',#99566,0.239805882894163,0.222043378686227);
#380=ELLIPSE('',#99588,0.599370913937631,0.555630771249981);
#381=ELLIPSE('',#99589,0.599370291563643,0.555629413546836);
#382=ELLIPSE('',#99591,0.239805889070487,0.222043643393142);
#383=ELLIPSE('',#99592,0.239805704052451,0.222043163089509);
#384=ELLIPSE('',#99594,0.239805697268519,0.222042896628072);
#385=ELLIPSE('',#99595,0.239805882895209,0.222043378688398);
#386=ELLIPSE('',#99617,0.599370913936379,0.555630771247499);
#387=ELLIPSE('',#99618,0.599370291564538,0.55562941354869);
#388=ELLIPSE('',#99620,0.239805889068884,0.222043643389916);
#389=ELLIPSE('',#99621,0.239805704050981,0.222043163086484);
#390=ELLIPSE('',#99623,0.239805697268942,0.222042896628818);
#391=ELLIPSE('',#99624,0.239805882895923,0.222043378689984);
#392=ELLIPSE('',#99646,0.59937091393689,0.555630771248566);
#393=ELLIPSE('',#99647,0.599370291565025,0.555629413549741);
#394=ELLIPSE('',#99649,0.239805889069351,0.222043643390883);
#395=ELLIPSE('',#99650,0.239805704051609,0.222043163087727);
#396=ELLIPSE('',#99652,0.239805697270396,0.222042896631823);
#397=ELLIPSE('',#99653,0.239805882896325,0.222043378690807);
#398=ELLIPSE('',#99675,0.599370913934826,0.555630771244343);
#399=ELLIPSE('',#99676,0.599370291564194,0.555629413547986);
#400=ELLIPSE('',#99678,0.239805889068253,0.222043643388627);
#401=ELLIPSE('',#99679,0.239805704053178,0.222043163090936);
#402=ELLIPSE('',#99681,0.239805697270034,0.22204289663126);
#403=ELLIPSE('',#99682,0.239805882893466,0.222043378684868);
#404=ELLIPSE('',#99704,0.59937091393641,0.55563077124766);
#405=ELLIPSE('',#99705,0.599370291564805,0.555629413549147);
#406=ELLIPSE('',#99707,0.239805889072066,0.222043643396362);
#407=ELLIPSE('',#99708,0.239805704052236,0.22204316308897);
#408=ELLIPSE('',#99710,0.23980569726934,0.222042896629804);
#409=ELLIPSE('',#99711,0.239805882895727,0.222043378689497);
#410=ELLIPSE('',#99733,0.599370913936658,0.555630771248057);
#411=ELLIPSE('',#99734,0.599370291562746,0.555629413545113);
#412=ELLIPSE('',#99736,0.239805889070185,0.222043643392531);
#413=ELLIPSE('',#99737,0.239805704053294,0.222043163091287);
#414=ELLIPSE('',#99739,0.239805697268977,0.222042896628983);
#415=ELLIPSE('',#99740,0.239805882896423,0.222043378690919);
#416=ELLIPSE('',#99762,0.59937091393644,0.555630771247594);
#417=ELLIPSE('',#99763,0.599370291561981,0.55562941354343);
#418=ELLIPSE('',#99765,0.239805889071035,0.222043643394202);
#419=ELLIPSE('',#99766,0.239805704052008,0.222043163088609);
#420=ELLIPSE('',#99768,0.239805697269648,0.222042896630424);
#421=ELLIPSE('',#99769,0.239805882895413,0.222043378688915);
#422=ELLIPSE('',#99791,0.599370913936381,0.555630771247481);
#423=ELLIPSE('',#99792,0.599370291564673,0.555629413548984);
#424=ELLIPSE('',#99794,0.239805889068991,0.222043643390099);
#425=ELLIPSE('',#99795,0.239805704053787,0.222043163092241);
#426=ELLIPSE('',#99797,0.239805697268383,0.222042896627734);
#427=ELLIPSE('',#99798,0.239805882893284,0.222043378684528);
#428=ELLIPSE('',#99820,0.599370913934144,0.555630771243034);
#429=ELLIPSE('',#99821,0.599370291566355,0.55562941355229);
#430=ELLIPSE('',#99823,0.239805889070614,0.222043643393421);
#431=ELLIPSE('',#99824,0.239805704053183,0.22204316309096);
#432=ELLIPSE('',#99826,0.239805697269667,0.222042896630443);
#433=ELLIPSE('',#99827,0.239805882894449,0.222043378686902);
#434=ELLIPSE('',#99849,0.599370913938034,0.555630771250937);
#435=ELLIPSE('',#99850,0.599370291564758,0.555629413549118);
#436=ELLIPSE('',#99852,0.239805889071379,0.222043643395086);
#437=ELLIPSE('',#99853,0.239805704051962,0.222043163088545);
#438=ELLIPSE('',#99855,0.239805697269236,0.222042896629485);
#439=ELLIPSE('',#99856,0.239805882895064,0.222043378688177);
#440=ELLIPSE('',#99878,0.599370913936816,0.555630771248509);
#441=ELLIPSE('',#99879,0.599370291562686,0.555629413544951);
#442=ELLIPSE('',#99881,0.239805889072334,0.222043643396888);
#443=ELLIPSE('',#99882,0.239805704051859,0.222043163088407);
#444=ELLIPSE('',#99884,0.239805697267012,0.222042896625054);
#445=ELLIPSE('',#99885,0.239805882894425,0.2220433786868);
#446=ELLIPSE('',#99907,0.599370913937916,0.555630771250686);
#447=ELLIPSE('',#99908,0.599370291561844,0.555629413543086);
#448=ELLIPSE('',#99910,0.239805889071215,0.222043643394601);
#449=ELLIPSE('',#99911,0.239805704052586,0.222043163089754);
#450=ELLIPSE('',#99913,0.239805697269129,0.222042896629312);
#451=ELLIPSE('',#99914,0.239805882895691,0.222043378689463);
#452=ELLIPSE('',#99936,0.599370913935739,0.555630771246241);
#453=ELLIPSE('',#99937,0.599370291565713,0.555629413551048);
#454=ELLIPSE('',#99939,0.239805889070012,0.222043643392159);
#455=ELLIPSE('',#99940,0.239805704055269,0.222043163095158);
#456=ELLIPSE('',#99942,0.239805697269079,0.22204289662915);
#457=ELLIPSE('',#99943,0.239805882893285,0.222043378684511);
#458=ELLIPSE('',#99965,0.5993709139378,0.555630771250281);
#459=ELLIPSE('',#99966,0.599370291564487,0.555629413548595);
#460=ELLIPSE('',#99968,0.239805889067021,0.222043643386073);
#461=ELLIPSE('',#99969,0.23980570405032,0.222043163085142);
#462=ELLIPSE('',#99971,0.239805697268822,0.222042896628661);
#463=ELLIPSE('',#99972,0.239805882895231,0.222043378688526);
#464=ELLIPSE('',#99994,0.599370913939247,0.555630771253286);
#465=ELLIPSE('',#99995,0.599370291564407,0.555629413548329);
#466=ELLIPSE('',#99997,0.239805889070316,0.22204364339277);
#467=ELLIPSE('',#99998,0.239805704051555,0.222043163087709);
#468=ELLIPSE('',#100000,0.23980569726812,0.222042896627117);
#469=ELLIPSE('',#100001,0.239805882894233,0.222043378686419);
#470=ELLIPSE('',#100023,0.599370913938812,0.555630771252417);
#471=ELLIPSE('',#100024,0.599370291562947,0.555629413545446);
#472=ELLIPSE('',#100026,0.239805889071155,0.222043643394403);
#473=ELLIPSE('',#100027,0.239805704051147,0.222043163086946);
#474=ELLIPSE('',#100029,0.239805697268128,0.222042896627196);
#475=ELLIPSE('',#100030,0.239805882895692,0.222043378689339);
#476=ELLIPSE('',#100052,0.599370913937403,0.555630771249492);
#477=ELLIPSE('',#100053,0.599370291564698,0.555629413548919);
#478=ELLIPSE('',#100055,0.239805889070393,0.222043643392999);
#479=ELLIPSE('',#100056,0.23980570405366,0.222043163091951);
#480=ELLIPSE('',#100058,0.239805697268035,0.222042896626935);
#481=ELLIPSE('',#100059,0.239805882893378,0.222043378684874);
#482=ELLIPSE('',#100081,0.599370913937259,0.555630771249076);
#483=ELLIPSE('',#100082,0.599370291562252,0.555629413544049);
#484=ELLIPSE('',#100084,0.239805889069568,0.22204364339119);
#485=ELLIPSE('',#100085,0.239805704052158,0.222043163089004);
#486=ELLIPSE('',#100087,0.239805697269194,0.222042896629392);
#487=ELLIPSE('',#100088,0.239805882896074,0.222043378690194);
#488=ELLIPSE('',#100110,0.599370913936119,0.555630771246838);
#489=ELLIPSE('',#100111,0.599370291565987,0.555629413551609);
#490=ELLIPSE('',#100113,0.239805889068597,0.222043643389295);
#491=ELLIPSE('',#100114,0.239805704052637,0.222043163089979);
#492=ELLIPSE('',#100116,0.239805697268707,0.222042896628356);
#493=ELLIPSE('',#100117,0.239805882896297,0.222043378690738);
#494=ELLIPSE('',#100139,0.59937091393601,0.555630771246725);
#495=ELLIPSE('',#100140,0.599370291562778,0.55562941354504);
#496=ELLIPSE('',#100142,0.239805889066727,0.222043643385389);
#497=ELLIPSE('',#100143,0.239805704051771,0.222043163088038);
#498=ELLIPSE('',#100145,0.239805697269733,0.222042896630494);
#499=ELLIPSE('',#100146,0.239805882893609,0.222043378685193);
#500=ELLIPSE('',#100168,0.599370913937713,0.555630771250117);
#501=ELLIPSE('',#100169,0.599370291561973,0.555629413543533);
#502=ELLIPSE('',#100171,0.239805889070764,0.222043643393701);
#503=ELLIPSE('',#100172,0.23980570405167,0.222043163087902);
#504=ELLIPSE('',#100174,0.239805697268835,0.222042896628737);
#505=ELLIPSE('',#100175,0.239805882892975,0.222043378683968);
#506=ELLIPSE('',#100197,0.599370913937063,0.555630771248936);
#507=ELLIPSE('',#100198,0.599370291565828,0.555629413551464);
#508=ELLIPSE('',#100200,0.239805889070764,0.222043643393715);
#509=ELLIPSE('',#100201,0.239805704049691,0.222043163083863);
#510=ELLIPSE('',#100203,0.239805697267964,0.222042896626842);
#511=ELLIPSE('',#100204,0.239805882894855,0.222043378687784);
#512=ELLIPSE('',#100226,0.599370913936629,0.555630771247946);
#513=ELLIPSE('',#100227,0.599370291564561,0.555629413548711);
#514=ELLIPSE('',#100229,0.239805889071998,0.222043643396255);
#515=ELLIPSE('',#100230,0.239805704055809,0.222043163096413);
#516=ELLIPSE('',#100232,0.239805697268767,0.222042896628554);
#517=ELLIPSE('',#100233,0.239805882895225,0.222043378688595);
#518=ELLIPSE('',#100255,0.599370913935967,0.555630771246675);
#519=ELLIPSE('',#100256,0.599370291564349,0.555629413548285);
#520=ELLIPSE('',#100258,0.239805889071902,0.222043643396007);
#521=ELLIPSE('',#100259,0.239805704053452,0.222043163091509);
#522=ELLIPSE('',#100261,0.239805697270489,0.222042896632057);
#523=ELLIPSE('',#100262,0.239805882894835,0.222043378687749);
#524=ELLIPSE('',#100284,0.599370913939248,0.555630771253297);
#525=ELLIPSE('',#100285,0.599370291563863,0.555629413547267);
#526=ELLIPSE('',#100287,0.239805889070602,0.222043643393333);
#527=ELLIPSE('',#100288,0.239805704052742,0.222043163090224);
#528=ELLIPSE('',#100290,0.239805697268792,0.222042896628584);
#529=ELLIPSE('',#100291,0.239805882894068,0.222043378686095);
#530=ELLIPSE('',#100313,0.599370913936219,0.555630771247178);
#531=ELLIPSE('',#100314,0.59937029156409,0.555629413547847);
#532=ELLIPSE('',#100316,0.239805889069997,0.222043643392213);
#533=ELLIPSE('',#100317,0.239805704052893,0.222043163090333);
#534=ELLIPSE('',#100319,0.239805697270079,0.222042896631273);
#535=ELLIPSE('',#100320,0.239805882895664,0.22204337868938);
#536=ELLIPSE('',#100342,0.599370913936394,0.555630771247526);
#537=ELLIPSE('',#100343,0.599370291564918,0.55562941354947);
#538=ELLIPSE('',#100345,0.239805889068249,0.222043643388543);
#539=ELLIPSE('',#100346,0.239805704052389,0.222043163089305);
#540=ELLIPSE('',#100348,0.239805697268477,0.222042896628032);
#541=ELLIPSE('',#100349,0.239805882896082,0.22204337869017);
#542=ELLIPSE('',#100371,0.599370913936562,0.555630771247845);
#543=ELLIPSE('',#100372,0.599370291564012,0.555629413547624);
#544=ELLIPSE('',#100374,0.23980588906986,0.222043643391904);
#545=ELLIPSE('',#100375,0.239805704051993,0.222043163088566);
#546=ELLIPSE('',#100377,0.239805697267169,0.222042896625307);
#547=ELLIPSE('',#100378,0.239805882896219,0.222043378690621);
#548=ELLIPSE('',#100400,0.599370913937084,0.555630771249008);
#549=ELLIPSE('',#100401,0.599370291564365,0.55562941354837);
#550=ELLIPSE('',#100403,0.239805889067811,0.222043643387605);
#551=ELLIPSE('',#100404,0.239805704053666,0.222043163091892);
#552=ELLIPSE('',#100406,0.239805697268621,0.222042896628293);
#553=ELLIPSE('',#100407,0.239805882895389,0.222043378688838);
#554=ELLIPSE('',#100429,0.599370913937905,0.555630771250672);
#555=ELLIPSE('',#100430,0.599370291564906,0.555629413549538);
#556=ELLIPSE('',#100432,0.23980588906824,0.222043643388556);
#557=ELLIPSE('',#100433,0.239805704052944,0.222043163090377);
#558=ELLIPSE('',#100435,0.239805697269778,0.222042896630677);
#559=ELLIPSE('',#100436,0.239805882894411,0.222043378686794);
#560=ELLIPSE('',#100458,0.599370913936309,0.555630771247401);
#561=ELLIPSE('',#100459,0.59937029156245,0.555629413544366);
#562=ELLIPSE('',#100461,0.239805889070967,0.222043643394125);
#563=ELLIPSE('',#100462,0.239805704052184,0.222043163088965);
#564=ELLIPSE('',#100464,0.239805697269359,0.222042896629841);
#565=ELLIPSE('',#100465,0.239805882895676,0.222043378689375);
#566=ELLIPSE('',#100487,0.599370913938664,0.555630771252272);
#567=ELLIPSE('',#100488,0.599370291563739,0.555629413547119);
#568=ELLIPSE('',#100490,0.239805889069012,0.222043643390162);
#569=ELLIPSE('',#100491,0.239805704051928,0.222043163088434);
#570=ELLIPSE('',#100493,0.239805697270961,0.222042896633077);
#571=ELLIPSE('',#100494,0.239805882894207,0.222043378686478);
#572=ELLIPSE('',#100516,0.599370913935456,0.555630771245561);
#573=ELLIPSE('',#100517,0.599370291564729,0.555629413549092);
#574=ELLIPSE('',#100519,0.239805889068523,0.222043643389264);
#575=ELLIPSE('',#100520,0.239805704050355,0.222043163085222);
#576=ELLIPSE('',#100522,0.239805697270177,0.222042896631395);
#577=ELLIPSE('',#100523,0.239805882895827,0.222043378689797);
#578=ELLIPSE('',#100545,0.599370913936989,0.55563077124874);
#579=ELLIPSE('',#100546,0.599370291565551,0.555629413550739);
#580=ELLIPSE('',#100548,0.239805889072759,0.222043643397765);
#581=ELLIPSE('',#100549,0.239805704052168,0.222043163088979);
#582=ELLIPSE('',#100551,0.239805697270002,0.222042896630934);
#583=ELLIPSE('',#100552,0.239805882896146,0.222043378690432);
#584=ELLIPSE('',#100574,0.599370913936148,0.555630771247047);
#585=ELLIPSE('',#100575,0.599370291563679,0.555629413546916);
#586=ELLIPSE('',#100577,0.239805889070217,0.222043643392595);
#587=ELLIPSE('',#100578,0.239805704051158,0.22204316308686);
#588=ELLIPSE('',#100580,0.239805697269515,0.222042896630024);
#589=ELLIPSE('',#100581,0.239805882896034,0.222043378690203);
#590=ELLIPSE('',#100603,0.59937091393771,0.555630771250091);
#591=ELLIPSE('',#100604,0.599370291564638,0.555629413548847);
#592=ELLIPSE('',#100606,0.239805889068323,0.222043643388684);
#593=ELLIPSE('',#100607,0.239805704051787,0.222043163088177);
#594=ELLIPSE('',#100609,0.239805697269453,0.222042896629885);
#595=ELLIPSE('',#100610,0.239805882894651,0.222043378687309);
#596=ELLIPSE('',#100632,0.599370913937892,0.555630771250547);
#597=ELLIPSE('',#100633,0.599370291564007,0.555629413547481);
#598=ELLIPSE('',#100635,0.239805889068112,0.222043643388263);
#599=ELLIPSE('',#100636,0.2398057040517,0.222043163087922);
#600=ELLIPSE('',#100638,0.239805697267627,0.222042896626236);
#601=ELLIPSE('',#100639,0.239805882895515,0.222043378689114);
#602=ELLIPSE('',#100661,0.599370913937969,0.555630771250674);
#603=ELLIPSE('',#100662,0.599370291564076,0.555629413547814);
#604=ELLIPSE('',#100664,0.239805889070403,0.222043643392942);
#605=ELLIPSE('',#100665,0.239805704051981,0.222043163088492);
#606=ELLIPSE('',#100667,0.239805697268631,0.22204289662828);
#607=ELLIPSE('',#100668,0.239805882894013,0.222043378686015);
#608=ELLIPSE('',#100690,0.599370913938002,0.555630771250828);
#609=ELLIPSE('',#100691,0.599370291563501,0.555629413546602);
#610=ELLIPSE('',#100693,0.239805889069064,0.222043643390311);
#611=ELLIPSE('',#100694,0.239805704053694,0.222043163092107);
#612=ELLIPSE('',#100696,0.239805697269181,0.222042896629446);
#613=ELLIPSE('',#100697,0.239805882894764,0.22204337868757);
#614=ELLIPSE('',#100719,0.599370913937269,0.555630771249286);
#615=ELLIPSE('',#100720,0.599370291564187,0.555629413548004);
#616=ELLIPSE('',#100722,0.239805889070155,0.222043643392431);
#617=ELLIPSE('',#100723,0.239805704053049,0.222043163090734);
#618=ELLIPSE('',#100725,0.239805697269303,0.222042896629634);
#619=ELLIPSE('',#100726,0.239805882894004,0.222043378685988);
#620=ELLIPSE('',#100748,0.599370913936729,0.555630771248111);
#621=ELLIPSE('',#100749,0.599370291565056,0.555629413549728);
#622=ELLIPSE('',#100751,0.239805889071609,0.22204364339536);
#623=ELLIPSE('',#100752,0.239805704051184,0.222043163086902);
#624=ELLIPSE('',#100754,0.239805697269678,0.222042896630412);
#625=ELLIPSE('',#100755,0.239805882895219,0.222043378688562);
#626=ELLIPSE('',#100777,0.599370913936915,0.555630771248569);
#627=ELLIPSE('',#100778,0.599370291563785,0.555629413547203);
#628=ELLIPSE('',#100780,0.239805889069398,0.222043643390908);
#629=ELLIPSE('',#100781,0.239805704051609,0.22204316308779);
#630=ELLIPSE('',#100783,0.239805697268669,0.222042896628271);
#631=ELLIPSE('',#100784,0.239805882894659,0.222043378687315);
#632=ELLIPSE('',#100806,0.599370913939075,0.555630771253124);
#633=ELLIPSE('',#100807,0.599370291563701,0.555629413547064);
#634=ELLIPSE('',#100809,0.239805889070192,0.222043643392424);
#635=ELLIPSE('',#100810,0.239805704053763,0.222043163092232);
#636=ELLIPSE('',#100812,0.239805697270319,0.222042896631767);
#637=ELLIPSE('',#100813,0.239805882896116,0.222043378690362);
#638=ELLIPSE('',#100835,0.599370913937333,0.555630771249332);
#639=ELLIPSE('',#100836,0.599370291564169,0.555629413548037);
#640=ELLIPSE('',#100838,0.239805889068326,0.222043643388653);
#641=ELLIPSE('',#100839,0.2398057040546,0.222043163093935);
#642=ELLIPSE('',#100841,0.239805697269039,0.222042896629057);
#643=ELLIPSE('',#100842,0.239805882895526,0.222043378689145);
#644=ELLIPSE('',#100864,0.599370913937793,0.555630771250455);
#645=ELLIPSE('',#100865,0.599370291564337,0.555629413548237);
#646=ELLIPSE('',#100867,0.239805889070937,0.222043643394056);
#647=ELLIPSE('',#100868,0.239805704052185,0.222043163089078);
#648=ELLIPSE('',#100870,0.239805697268221,0.222042896627553);
#649=ELLIPSE('',#100871,0.239805882894638,0.222043378687215);
#650=ELLIPSE('',#100893,0.599370913938291,0.555630771251308);
#651=ELLIPSE('',#100894,0.599370291564336,0.555629413548396);
#652=ELLIPSE('',#100896,0.239805889070951,0.222043643394117);
#653=ELLIPSE('',#100897,0.239805704052956,0.222043163090467);
#654=ELLIPSE('',#100899,0.239805697268216,0.222042896627409);
#655=ELLIPSE('',#100900,0.239805882895213,0.222043378688343);
#656=ELLIPSE('',#100922,0.5993709139375,0.555630771249788);
#657=ELLIPSE('',#100923,0.599370291564678,0.555629413548944);
#658=ELLIPSE('',#100925,0.239805889072709,0.222043643397697);
#659=ELLIPSE('',#100926,0.239805704051998,0.222043163088687);
#660=ELLIPSE('',#100928,0.239805697269515,0.222042896630098);
#661=ELLIPSE('',#100929,0.239805882895996,0.222043378690038);
#662=ELLIPSE('',#100951,0.599370913936987,0.555630771248767);
#663=ELLIPSE('',#100952,0.599370291562368,0.55562941354422);
#664=ELLIPSE('',#100954,0.239805889071445,0.222043643395052);
#665=ELLIPSE('',#100955,0.239805704051795,0.222043163088107);
#666=ELLIPSE('',#100957,0.239805697270211,0.222042896631472);
#667=ELLIPSE('',#100958,0.239805882896537,0.222043378691172);
#668=ELLIPSE('',#100980,0.599370913937439,0.55563077124968);
#669=ELLIPSE('',#100981,0.599370291563737,0.555629413547156);
#670=ELLIPSE('',#100983,0.239805889069886,0.222043643391976);
#671=ELLIPSE('',#100984,0.23980570405216,0.222043163088966);
#672=ELLIPSE('',#100986,0.239805697271986,0.222042896635182);
#673=ELLIPSE('',#100987,0.239805882895563,0.222043378689248);
#674=ELLIPSE('',#101009,0.599370913935863,0.555630771246414);
#675=ELLIPSE('',#101010,0.599370291562441,0.555629413544446);
#676=ELLIPSE('',#101012,0.239805889069274,0.222043643390651);
#677=ELLIPSE('',#101013,0.239805704051074,0.222043163086558);
#678=ELLIPSE('',#101015,0.239805697268375,0.222042896627818);
#679=ELLIPSE('',#101016,0.239805882894152,0.222043378686232);
#680=ELLIPSE('',#101038,0.599370913938186,0.555630771251263);
#681=ELLIPSE('',#101039,0.599370291564916,0.555629413549503);
#682=ELLIPSE('',#101041,0.239805889069667,0.222043643391434);
#683=ELLIPSE('',#101042,0.239805704053102,0.222043163090824);
#684=ELLIPSE('',#101044,0.239805697269289,0.222042896629566);
#685=ELLIPSE('',#101045,0.239805882895496,0.222043378689093);
#686=ELLIPSE('',#101067,0.599370913937337,0.555630771249432);
#687=ELLIPSE('',#101068,0.599370291563716,0.555629413547141);
#688=ELLIPSE('',#101070,0.239805889070521,0.222043643393123);
#689=ELLIPSE('',#101071,0.239805704052324,0.222043163089135);
#690=ELLIPSE('',#101073,0.23980569726921,0.222042896629472);
#691=ELLIPSE('',#101074,0.239805882895584,0.222043378689238);
#692=ELLIPSE('',#101099,0.599370913936554,0.555630771247927);
#693=ELLIPSE('',#101100,0.599370291563314,0.55562941354626);
#694=ELLIPSE('',#101102,0.239805889071973,0.222043643396186);
#695=ELLIPSE('',#101103,0.239805704053213,0.222043163091114);
#696=ELLIPSE('',#101105,0.239805697271176,0.222042896633431);
#697=ELLIPSE('',#101106,0.239805882895932,0.222043378689924);
#698=ELLIPSE('',#101111,0.472049204510934,0.428376857312556);
#699=ELLIPSE('',#101112,0.472048618390948,0.428376332980169);
#700=ELLIPSE('',#101113,0.354420976867702,0.321488380363305);
#701=ELLIPSE('',#101114,0.35442112183661,0.321488565199684);
#702=ELLIPSE('',#101116,0.472048618673449,0.428376333587109);
#703=ELLIPSE('',#101117,0.472049204212692,0.428376856671643);
#704=ELLIPSE('',#101118,0.354421145892225,0.321488604125491);
#705=ELLIPSE('',#101119,0.354421089423447,0.321488612089807);
#706=ELLIPSE('',#101123,0.146692861887116,0.127051669379107);
#707=ELLIPSE('',#101135,0.146691465567175,0.127050784764067);
#708=ELLIPSE('',#101152,0.146692861887708,0.127051669379573);
#709=ELLIPSE('',#101163,0.146691465566821,0.12705078476379);
#710=ELLIPSE('',#101170,0.472049204509289,0.428376857309266);
#711=ELLIPSE('',#101171,0.472048618391431,0.428376332981064);
#712=ELLIPSE('',#101172,0.354420976861821,0.321488380351383);
#713=ELLIPSE('',#101173,0.35442112183555,0.321488565197576);
#714=ELLIPSE('',#101175,0.472048618673252,0.428376333586691);
#715=ELLIPSE('',#101176,0.472049204211803,0.42837685666992);
#716=ELLIPSE('',#101177,0.354421145892588,0.321488604126162);
#717=ELLIPSE('',#101178,0.354421089426214,0.321488612095312);
#718=ELLIPSE('',#101183,0.472049204510492,0.428376857311686);
#719=ELLIPSE('',#101184,0.472048618390858,0.428376332979975);
#720=ELLIPSE('',#101185,0.35442097686338,0.321488380354659);
#721=ELLIPSE('',#101186,0.354421121834003,0.321488565194468);
#722=ELLIPSE('',#101188,0.472048618674824,0.428376333589875);
#723=ELLIPSE('',#101189,0.472049204214783,0.428376856675792);
#724=ELLIPSE('',#101190,0.354421145894039,0.3214886041291);
#725=ELLIPSE('',#101191,0.354421089420356,0.321488612083628);
#726=ELLIPSE('',#101196,0.472049204512028,0.428376857314658);
#727=ELLIPSE('',#101197,0.472048618391491,0.428376332981219);
#728=ELLIPSE('',#101198,0.354420976864179,0.32148838035634);
#729=ELLIPSE('',#101199,0.354421121836554,0.321488565199535);
#730=ELLIPSE('',#101201,0.47204861867433,0.428376333588862);
#731=ELLIPSE('',#101202,0.472049204212632,0.428376856671534);
#732=ELLIPSE('',#101203,0.354421145892885,0.321488604126847);
#733=ELLIPSE('',#101204,0.354421089422622,0.32148861208819);
#734=ELLIPSE('',#101209,0.472049204510256,0.428376857311203);
#735=ELLIPSE('',#101210,0.472048618390729,0.428376332979685);
#736=ELLIPSE('',#101211,0.354420976865746,0.321488380359374);
#737=ELLIPSE('',#101212,0.354421121834367,0.321488565195157);
#738=ELLIPSE('',#101214,0.472048618674276,0.428376333588791);
#739=ELLIPSE('',#101215,0.47204920421503,0.428376856676324);
#740=ELLIPSE('',#101216,0.354421145892976,0.321488604126937);
#741=ELLIPSE('',#101217,0.354421089421022,0.321488612084937);
#742=ELLIPSE('',#101222,0.472049204511253,0.428376857313146);
#743=ELLIPSE('',#101223,0.472048618391128,0.428376332980535);
#744=ELLIPSE('',#101224,0.354420976867073,0.321488380362121);
#745=ELLIPSE('',#101225,0.354421121836193,0.321488565198845);
#746=ELLIPSE('',#101227,0.472048618674679,0.428376333589555);
#747=ELLIPSE('',#101228,0.472049204213367,0.428376856673016);
#748=ELLIPSE('',#101229,0.354421145894509,0.321488604130019);
#749=ELLIPSE('',#101230,0.354421089422398,0.321488612087834);
#750=ELLIPSE('',#101235,0.472049204510515,0.428376857311735);
#751=ELLIPSE('',#101236,0.472048618392408,0.428376332983092);
#752=ELLIPSE('',#101237,0.354420976869297,0.321488380366511);
#753=ELLIPSE('',#101238,0.354421121835321,0.321488565197107);
#754=ELLIPSE('',#101240,0.472048618673807,0.428376333587843);
#755=ELLIPSE('',#101241,0.472049204212756,0.428376856671762);
#756=ELLIPSE('',#101242,0.35442114589341,0.321488604127871);
#757=ELLIPSE('',#101243,0.354421089425903,0.321488612094688);
#758=ELLIPSE('',#101248,0.47204920451107,0.428376857312822);
#759=ELLIPSE('',#101249,0.472048618392803,0.42837633298386);
#760=ELLIPSE('',#101250,0.354420976860346,0.321488380348543);
#761=ELLIPSE('',#101251,0.354421121835633,0.321488565197806);
#762=ELLIPSE('',#101253,0.472048618674335,0.428376333588864);
#763=ELLIPSE('',#101254,0.472049204215952,0.428376856678111);
#764=ELLIPSE('',#101255,0.354421145892473,0.32148860412602);
#765=ELLIPSE('',#101256,0.354421089425772,0.321488612094473);
#766=ELLIPSE('',#101261,0.472049204509577,0.428376857309888);
#767=ELLIPSE('',#101262,0.47204861839227,0.428376332982796);
#768=ELLIPSE('',#101263,0.354420976869843,0.321488380367727);
#769=ELLIPSE('',#101264,0.354421121834772,0.321488565196016);
#770=ELLIPSE('',#101266,0.47204861867332,0.428376333586849);
#771=ELLIPSE('',#101267,0.472049204213765,0.428376856673737);
#772=ELLIPSE('',#101268,0.354421145891297,0.321488604123706);
#773=ELLIPSE('',#101269,0.354421089426494,0.321488612095895);
#774=ELLIPSE('',#101274,0.472049204513559,0.428376857317697);
#775=ELLIPSE('',#101275,0.472048618390786,0.42837633297985);
#776=ELLIPSE('',#101276,0.354420976865086,0.321488380358123);
#777=ELLIPSE('',#101277,0.354421121835652,0.321488565197754);
#778=ELLIPSE('',#101279,0.472048618673356,0.428376333586975);
#779=ELLIPSE('',#101280,0.472049204213523,0.428376856673277);
#780=ELLIPSE('',#101281,0.354421145893169,0.321488604127372);
#781=ELLIPSE('',#101282,0.354421089422401,0.321488612087849);
#782=ELLIPSE('',#101287,0.472049204510991,0.42837685731263);
#783=ELLIPSE('',#101288,0.472048618392257,0.428376332982714);
#784=ELLIPSE('',#101289,0.354420976868145,0.321488380364194);
#785=ELLIPSE('',#101290,0.354421121839984,0.321488565206443);
#786=ELLIPSE('',#101292,0.472048618673911,0.42837633358801);
#787=ELLIPSE('',#101293,0.472049204212241,0.428376856670714);
#788=ELLIPSE('',#101294,0.354421145893723,0.321488604128517);
#789=ELLIPSE('',#101295,0.354421089425117,0.321488612093203);
#790=ELLIPSE('',#101300,0.472049204510948,0.428376857312567);
#791=ELLIPSE('',#101301,0.472048618392567,0.428376332983328);
#792=ELLIPSE('',#101302,0.354420976870575,0.32148838036909);
#793=ELLIPSE('',#101303,0.354421121835812,0.32148856519803);
#794=ELLIPSE('',#101305,0.472048618673876,0.428376333587938);
#795=ELLIPSE('',#101306,0.472049204212521,0.428376856671341);
#796=ELLIPSE('',#101307,0.35442114589272,0.321488604126533);
#797=ELLIPSE('',#101308,0.354421089422786,0.321488612088435);
#798=ELLIPSE('',#101313,0.472049204511237,0.428376857313125);
#799=ELLIPSE('',#101314,0.472048618391984,0.4283763329822);
#800=ELLIPSE('',#101315,0.354420976866854,0.321488380361489);
#801=ELLIPSE('',#101316,0.354421121834466,0.321488565195394);
#802=ELLIPSE('',#101318,0.47204861867381,0.428376333587779);
#803=ELLIPSE('',#101319,0.472049204212592,0.428376856671459);
#804=ELLIPSE('',#101320,0.354421145893299,0.321488604127691);
#805=ELLIPSE('',#101321,0.354421089420226,0.321488612083325);
#806=ELLIPSE('',#101326,0.47204920451174,0.428376857314134);
#807=ELLIPSE('',#101327,0.472048618391901,0.428376332982063);
#808=ELLIPSE('',#101328,0.354420976864801,0.32148838035758);
#809=ELLIPSE('',#101329,0.354421121835268,0.321488565197031);
#810=ELLIPSE('',#101331,0.472048618674594,0.428376333589358);
#811=ELLIPSE('',#101332,0.47204920421434,0.428376856675008);
#812=ELLIPSE('',#101333,0.354421145891958,0.321488604125045);
#813=ELLIPSE('',#101334,0.354421089422399,0.321488612087739);
#814=ELLIPSE('',#101339,0.472049204509969,0.428376857310649);
#815=ELLIPSE('',#101340,0.472048618393256,0.428376332984763);
#816=ELLIPSE('',#101341,0.354420976867452,0.321488380362875);
#817=ELLIPSE('',#101342,0.354421121834484,0.321488565195343);
#818=ELLIPSE('',#101344,0.472048618673314,0.428376333586792);
#819=ELLIPSE('',#101345,0.47204920421347,0.428376856673174);
#820=ELLIPSE('',#101346,0.35442114589289,0.321488604126797);
#821=ELLIPSE('',#101347,0.354421089422546,0.321488612087928);
#822=ELLIPSE('',#101352,0.472049204510775,0.42837685731223);
#823=ELLIPSE('',#101353,0.472048618391864,0.428376332982002);
#824=ELLIPSE('',#101354,0.354420976864984,0.321488380357738);
#825=ELLIPSE('',#101355,0.354421121837171,0.321488565200749);
#826=ELLIPSE('',#101357,0.472048618673496,0.428376333587201);
#827=ELLIPSE('',#101358,0.472049204213379,0.428376856673032);
#828=ELLIPSE('',#101359,0.354421145891953,0.321488604124905);
#829=ELLIPSE('',#101360,0.354421089421714,0.321488612086365);
#830=ELLIPSE('',#101365,0.47204920451033,0.428376857311353);
#831=ELLIPSE('',#101366,0.47204861839312,0.428376332984429);
#832=ELLIPSE('',#101367,0.35442097686122,0.321488380350427);
#833=ELLIPSE('',#101368,0.354421121834249,0.321488565194965);
#834=ELLIPSE('',#101370,0.472048618675574,0.42837633359129);
#835=ELLIPSE('',#101371,0.472049204211857,0.428376856669993);
#836=ELLIPSE('',#101372,0.354421145893558,0.321488604128205);
#837=ELLIPSE('',#101373,0.354421089424109,0.321488612091213);
#838=ELLIPSE('',#101378,0.472049204509653,0.428376857310002);
#839=ELLIPSE('',#101379,0.47204861839197,0.428376332982155);
#840=ELLIPSE('',#101380,0.354420976862621,0.321488380353224);
#841=ELLIPSE('',#101381,0.354421121835799,0.321488565198063);
#842=ELLIPSE('',#101383,0.472048618674322,0.428376333588805);
#843=ELLIPSE('',#101384,0.472049204212596,0.428376856671498);
#844=ELLIPSE('',#101385,0.354421145890905,0.321488604122786);
#845=ELLIPSE('',#101386,0.354421089421594,0.321488612086012);
#846=ELLIPSE('',#101391,0.472049204510696,0.428376857312045);
#847=ELLIPSE('',#101392,0.472048618392718,0.428376332983668);
#848=ELLIPSE('',#101393,0.354420976864736,0.321488380357433);
#849=ELLIPSE('',#101394,0.3544211218364,0.321488565199259);
#850=ELLIPSE('',#101396,0.472048618674399,0.428376333588995);
#851=ELLIPSE('',#101397,0.472049204215212,0.428376856676614);
#852=ELLIPSE('',#101398,0.354421145892403,0.321488604125829);
#853=ELLIPSE('',#101399,0.354421089423517,0.321488612090008);
#854=ELLIPSE('',#101404,0.472049204512178,0.428376857315023);
#855=ELLIPSE('',#101405,0.47204861839185,0.428376332981941);
#856=ELLIPSE('',#101406,0.354420976867694,0.321488380363225);
#857=ELLIPSE('',#101407,0.354421121836556,0.321488565199582);
#858=ELLIPSE('',#101409,0.472048618673223,0.428376333586608);
#859=ELLIPSE('',#101410,0.472049204212149,0.428376856670589);
#860=ELLIPSE('',#101411,0.35442114589271,0.321488604126449);
#861=ELLIPSE('',#101412,0.354421089422371,0.321488612087722);
#862=ELLIPSE('',#101417,0.472049204509814,0.428376857310301);
#863=ELLIPSE('',#101418,0.472048618390664,0.428376332979562);
#864=ELLIPSE('',#101419,0.354420976864669,0.321488380357242);
#865=ELLIPSE('',#101420,0.354421121834253,0.321488565194901);
#866=ELLIPSE('',#101422,0.472048618673726,0.428376333587664);
#867=ELLIPSE('',#101423,0.472049204213629,0.428376856673542);
#868=ELLIPSE('',#101424,0.354421145892419,0.321488604125935);
#869=ELLIPSE('',#101425,0.354421089422999,0.321488612088916);
#870=ELLIPSE('',#101430,0.472049204511287,0.428376857313303);
#871=ELLIPSE('',#101431,0.472048618393151,0.428376332984527);
#872=ELLIPSE('',#101432,0.354420976866975,0.32148838036195);
#873=ELLIPSE('',#101433,0.354421121832796,0.321488565191982);
#874=ELLIPSE('',#101435,0.472048618673619,0.428376333587397);
#875=ELLIPSE('',#101436,0.472049204212268,0.428376856670815);
#876=ELLIPSE('',#101437,0.35442114589314,0.321488604127281);
#877=ELLIPSE('',#101438,0.354421089424284,0.321488612091627);
#878=ELLIPSE('',#101443,0.472049204509935,0.428376857310618);
#879=ELLIPSE('',#101444,0.472048618393844,0.428376332985917);
#880=ELLIPSE('',#101445,0.354420976863435,0.321488380354774);
#881=ELLIPSE('',#101446,0.354421121833964,0.321488565194345);
#882=ELLIPSE('',#101448,0.472048618673275,0.428376333586788);
#883=ELLIPSE('',#101449,0.472049204212259,0.428376856670844);
#884=ELLIPSE('',#101450,0.354421145892702,0.321488604126391);
#885=ELLIPSE('',#101451,0.35442108942423,0.321488612091314);
#886=ELLIPSE('',#101456,0.472049204511814,0.428376857314329);
#887=ELLIPSE('',#101457,0.472048618393361,0.42837633298497);
#888=ELLIPSE('',#101458,0.354420976864889,0.321488380357681);
#889=ELLIPSE('',#101459,0.354421121832822,0.321488565192075);
#890=ELLIPSE('',#101461,0.472048618674648,0.428376333589447);
#891=ELLIPSE('',#101462,0.472049204213791,0.428376856673861);
#892=ELLIPSE('',#101463,0.354421145891276,0.321488604123623);
#893=ELLIPSE('',#101464,0.35442108942329,0.321488612089543);
#894=ELLIPSE('',#101469,0.472049204510388,0.428376857311443);
#895=ELLIPSE('',#101470,0.472048618394646,0.428376332987444);
#896=ELLIPSE('',#101471,0.354420976863241,0.321488380354416);
#897=ELLIPSE('',#101472,0.354421121835884,0.321488565198253);
#898=ELLIPSE('',#101474,0.472048618674055,0.428376333588331);
#899=ELLIPSE('',#101475,0.472049204214137,0.428376856674488);
#900=ELLIPSE('',#101476,0.354421145893446,0.321488604127902);
#901=ELLIPSE('',#101477,0.354421089423459,0.321488612089795);
#902=ELLIPSE('',#101482,0.472049204513525,0.428376857317664);
#903=ELLIPSE('',#101483,0.472048618392254,0.428376332982779);
#904=ELLIPSE('',#101484,0.354420976860599,0.321488380349097);
#905=ELLIPSE('',#101485,0.354421121836793,0.321488565199991);
#906=ELLIPSE('',#101487,0.472048618674402,0.428376333588992);
#907=ELLIPSE('',#101488,0.472049204211988,0.428376856670282);
#908=ELLIPSE('',#101489,0.354421145893076,0.321488604127166);
#909=ELLIPSE('',#101490,0.354421089420329,0.32148861208354);
#910=ELLIPSE('',#101495,0.47204920451197,0.42837685731465);
#911=ELLIPSE('',#101496,0.472048618392666,0.428376332983572);
#912=ELLIPSE('',#101497,0.354420976864991,0.321488380357901);
#913=ELLIPSE('',#101498,0.354421121835,0.321488565196478);
#914=ELLIPSE('',#101500,0.472048618673531,0.4283763335873);
#915=ELLIPSE('',#101501,0.472049204213755,0.42837685667382);
#916=ELLIPSE('',#101502,0.354421145893716,0.321488604128501);
#917=ELLIPSE('',#101503,0.354421089417468,0.3214886120778);
#918=ELLIPSE('',#101508,0.472049204511671,0.428376857313973);
#919=ELLIPSE('',#101509,0.472048618392204,0.428376332982662);
#920=ELLIPSE('',#101510,0.354420976865648,0.321488380359166);
#921=ELLIPSE('',#101511,0.354421121836227,0.321488565198991);
#922=ELLIPSE('',#101513,0.472048618673305,0.428376333586812);
#923=ELLIPSE('',#101514,0.472049204212258,0.428376856670813);
#924=ELLIPSE('',#101515,0.354421145893316,0.321488604127761);
#925=ELLIPSE('',#101516,0.354421089421102,0.321488612085023);
#926=ELLIPSE('',#101521,0.472049204511125,0.42837685731293);
#927=ELLIPSE('',#101522,0.472048618393819,0.428376332985859);
#928=ELLIPSE('',#101523,0.354420976867475,0.321488380362911);
#929=ELLIPSE('',#101524,0.354421121834505,0.321488565195489);
#930=ELLIPSE('',#101526,0.472048618672661,0.428376333585526);
#931=ELLIPSE('',#101527,0.4720492042127,0.428376856671722);
#932=ELLIPSE('',#101528,0.35442114589236,0.321488604125723);
#933=ELLIPSE('',#101529,0.354421089420201,0.321488612083387);
#934=ELLIPSE('',#101534,0.472049204510718,0.428376857312093);
#935=ELLIPSE('',#101535,0.472048618392984,0.428376332984173);
#936=ELLIPSE('',#101536,0.35442097686326,0.321488380354402);
#937=ELLIPSE('',#101537,0.354421121836511,0.321488565199487);
#938=ELLIPSE('',#101539,0.472048618673284,0.428376333586807);
#939=ELLIPSE('',#101540,0.47204920421238,0.428376856671024);
#940=ELLIPSE('',#101541,0.354421145894016,0.32148860412904);
#941=ELLIPSE('',#101542,0.354421089421678,0.321488612086348);
#942=ELLIPSE('',#101545,0.472049204512392,0.428376857315418);
#943=ELLIPSE('',#101546,0.472048618392041,0.428376332982344);
#944=ELLIPSE('',#101547,0.354420976863591,0.321488380355001);
#945=ELLIPSE('',#101548,0.354421121837232,0.321488565200917);
#946=ELLIPSE('',#101550,0.472048618674192,0.428376333588603);
#947=ELLIPSE('',#101551,0.472049204214532,0.428376856675342);
#948=ELLIPSE('',#101552,0.354421145894906,0.32148860413083);
#949=ELLIPSE('',#101553,0.354421089421235,0.321488612085373);
#950=ELLIPSE('',#101558,0.472049204511627,0.428376857313931);
#951=ELLIPSE('',#101559,0.472048618392463,0.428376332983136);
#952=ELLIPSE('',#101560,0.3544209768649,0.321488380357729);
#953=ELLIPSE('',#101561,0.354421121832693,0.321488565191817);
#954=ELLIPSE('',#101563,0.472048618673316,0.428376333586818);
#955=ELLIPSE('',#101564,0.472049204211302,0.428376856668882);
#956=ELLIPSE('',#101565,0.354421145891833,0.321488604124742);
#957=ELLIPSE('',#101566,0.354421089425509,0.321488612093896);
#958=ELLIPSE('',#101571,0.472049204512195,0.428376857315009);
#959=ELLIPSE('',#101572,0.472048618391479,0.428376332981225);
#960=ELLIPSE('',#101573,0.354420976869266,0.321488380366468);
#961=ELLIPSE('',#101574,0.354421121835294,0.321488565196967);
#962=ELLIPSE('',#101576,0.47204861867312,0.428376333586429);
#963=ELLIPSE('',#101577,0.472049204214062,0.428376856674387);
#964=ELLIPSE('',#101578,0.354421145892696,0.321488604126356);
#965=ELLIPSE('',#101579,0.354421089419382,0.321488612081602);
#966=ELLIPSE('',#101584,0.472049204513345,0.428376857317346);
#967=ELLIPSE('',#101585,0.472048618392493,0.428376332983225);
#968=ELLIPSE('',#101586,0.354420976866613,0.321488380361188);
#969=ELLIPSE('',#101587,0.35442112183346,0.321488565193417);
#970=ELLIPSE('',#101589,0.472048618674328,0.428376333588841);
#971=ELLIPSE('',#101590,0.472049204213543,0.428376856673368);
#972=ELLIPSE('',#101591,0.354421145891292,0.321488604123538);
#973=ELLIPSE('',#101592,0.354421089420917,0.321488612084688);
#974=ELLIPSE('',#101597,0.472049204510815,0.42837685731222);
#975=ELLIPSE('',#101598,0.472048618394316,0.428376332986803);
#976=ELLIPSE('',#101599,0.354420976863249,0.321488380354374);
#977=ELLIPSE('',#101600,0.354421121838533,0.321488565203565);
#978=ELLIPSE('',#101602,0.47204861867473,0.428376333589591);
#979=ELLIPSE('',#101603,0.47204920421248,0.428376856671206);
#980=ELLIPSE('',#101604,0.354421145892991,0.321488604127081);
#981=ELLIPSE('',#101605,0.354421089424507,0.321488612091936);
#982=ELLIPSE('',#101610,0.472049204513034,0.428376857316677);
#983=ELLIPSE('',#101611,0.472048618393481,0.428376332985152);
#984=ELLIPSE('',#101612,0.354420976863262,0.321488380354344);
#985=ELLIPSE('',#101613,0.354421121836168,0.321488565198842);
#986=ELLIPSE('',#101615,0.472048618674509,0.428376333589219);
#987=ELLIPSE('',#101616,0.472049204212553,0.428376856671371);
#988=ELLIPSE('',#101617,0.354421145893113,0.321488604127279);
#989=ELLIPSE('',#101618,0.354421089422416,0.321488612087729);
#990=ELLIPSE('',#101623,0.472049204514185,0.42837685731902);
#991=ELLIPSE('',#101624,0.47204861839253,0.428376332983218);
#992=ELLIPSE('',#101625,0.354420976864303,0.321488380356576);
#993=ELLIPSE('',#101626,0.354421121838416,0.321488565203263);
#994=ELLIPSE('',#101628,0.472048618673455,0.428376333587087);
#995=ELLIPSE('',#101629,0.472049204213923,0.428376856674092);
#996=ELLIPSE('',#101630,0.354421145891633,0.321488604124298);
#997=ELLIPSE('',#101631,0.35442108941833,0.321488612079527);
#998=ELLIPSE('',#101636,0.472049204511433,0.428376857313588);
#999=ELLIPSE('',#101637,0.472048618392048,0.428376332982336);
#1000=ELLIPSE('',#101638,0.354420976865362,0.321488380358623);
#1001=ELLIPSE('',#101639,0.354421121836458,0.321488565199375);
#1002=ELLIPSE('',#101641,0.472048618673689,0.428376333587614);
#1003=ELLIPSE('',#101642,0.472049204215152,0.428376856676502);
#1004=ELLIPSE('',#101643,0.354421145892952,0.321488604126922);
#1005=ELLIPSE('',#101644,0.354421089419767,0.321488612082466);
#1006=ELLIPSE('',#101649,0.472049204510861,0.428376857312365);
#1007=ELLIPSE('',#101650,0.472048618392299,0.428376332982868);
#1008=ELLIPSE('',#101651,0.354420976866964,0.321488380361803);
#1009=ELLIPSE('',#101652,0.354421121832281,0.321488565191073);
#1010=ELLIPSE('',#101654,0.472048618674435,0.428376333589046);
#1011=ELLIPSE('',#101655,0.472049204214429,0.428376856675097);
#1012=ELLIPSE('',#101656,0.354421145893817,0.321488604128667);
#1013=ELLIPSE('',#101657,0.354421089421098,0.321488612084989);
#1014=ELLIPSE('',#101662,0.472049204511699,0.428376857314077);
#1015=ELLIPSE('',#101663,0.472048618391712,0.428376332981672);
#1016=ELLIPSE('',#101664,0.354420976866376,0.3214883803606);
#1017=ELLIPSE('',#101665,0.354421121836721,0.321488565199902);
#1018=ELLIPSE('',#101667,0.472048618673185,0.428376333586588);
#1019=ELLIPSE('',#101668,0.47204920421276,0.428376856671811);
#1020=ELLIPSE('',#101669,0.354421145893024,0.321488604127051);
#1021=ELLIPSE('',#101670,0.354421089423307,0.321488612089635);
#1022=ELLIPSE('',#101675,0.472049204511707,0.428376857314097);
#1023=ELLIPSE('',#101676,0.472048618390853,0.428376332979992);
#1024=ELLIPSE('',#101677,0.354420976863852,0.321488380355569);
#1025=ELLIPSE('',#101678,0.354421121835684,0.321488565197847);
#1026=ELLIPSE('',#101680,0.472048618673115,0.428376333586399);
#1027=ELLIPSE('',#101681,0.472049204211315,0.428376856668929);
#1028=ELLIPSE('',#101682,0.354421145892319,0.321488604125627);
#1029=ELLIPSE('',#101683,0.354421089421244,0.321488612085423);
#1030=ELLIPSE('',#101688,0.472049204511408,0.428376857313473);
#1031=ELLIPSE('',#101689,0.472048618391248,0.428376332980779);
#1032=ELLIPSE('',#101690,0.354420976866618,0.321488380361027);
#1033=ELLIPSE('',#101691,0.354421121834844,0.321488565196103);
#1034=ELLIPSE('',#101693,0.472048618673682,0.428376333587622);
#1035=ELLIPSE('',#101694,0.472049204214136,0.428376856674501);
#1036=ELLIPSE('',#101695,0.354421145893116,0.321488604127322);
#1037=ELLIPSE('',#101696,0.354421089422313,0.321488612087442);
#1038=ELLIPSE('',#101701,0.472049204511621,0.428376857313938);
#1039=ELLIPSE('',#101702,0.472048618390109,0.428376332978471);
#1040=ELLIPSE('',#101703,0.354420976868012,0.321488380363899);
#1041=ELLIPSE('',#101704,0.354421121837676,0.321488565201838);
#1042=ELLIPSE('',#101706,0.47204861867375,0.428376333587659);
#1043=ELLIPSE('',#101707,0.472049204213172,0.428376856672594);
#1044=ELLIPSE('',#101708,0.354421145890316,0.321488604121659);
#1045=ELLIPSE('',#101709,0.354421089424265,0.321488612091441);
#1046=ELLIPSE('',#101714,0.472049204512371,0.42837685731542);
#1047=ELLIPSE('',#101715,0.47204861839267,0.428376332983581);
#1048=ELLIPSE('',#101716,0.35442097686673,0.321488380361359);
#1049=ELLIPSE('',#101717,0.354421121837488,0.321488565201474);
#1050=ELLIPSE('',#101719,0.472048618674121,0.428376333588414);
#1051=ELLIPSE('',#101720,0.472049204212625,0.428376856671558);
#1052=ELLIPSE('',#101721,0.354421145894598,0.321488604130197);
#1053=ELLIPSE('',#101722,0.354421089423111,0.321488612089106);
#1054=ELLIPSE('',#101727,0.47204920451016,0.42837685731105);
#1055=ELLIPSE('',#101728,0.472048618391775,0.428376332981819);
#1056=ELLIPSE('',#101729,0.354420976864999,0.321488380357909);
#1057=ELLIPSE('',#101730,0.354421121834633,0.321488565195725);
#1058=ELLIPSE('',#101732,0.472048618674818,0.428376333589819);
#1059=ELLIPSE('',#101733,0.472049204213572,0.428376856673319);
#1060=ELLIPSE('',#101734,0.354421145892993,0.321488604126976);
#1061=ELLIPSE('',#101735,0.354421089423447,0.321488612089824);
#1062=ELLIPSE('',#101738,0.472049204509326,0.428376857309374);
#1063=ELLIPSE('',#101739,0.472048618392612,0.428376332983476);
#1064=ELLIPSE('',#101740,0.354420976864962,0.321488380357948);
#1065=ELLIPSE('',#101741,0.354421121838444,0.321488565203383);
#1066=ELLIPSE('',#101743,0.472048618673401,0.42837633358704);
#1067=ELLIPSE('',#101744,0.472049204213379,0.428376856673032);
#1068=ELLIPSE('',#101745,0.354421145892966,0.32148860412693);
#1069=ELLIPSE('',#101746,0.354421089421848,0.321488612086605);
#1070=ELLIPSE('',#101751,0.472049204510816,0.428376857312366);
#1071=ELLIPSE('',#101752,0.472048618391678,0.428376332981601);
#1072=ELLIPSE('',#101753,0.354420976865417,0.321488380358783);
#1073=ELLIPSE('',#101754,0.354421121835397,0.321488565197237);
#1074=ELLIPSE('',#101756,0.47204861867394,0.428376333588068);
#1075=ELLIPSE('',#101757,0.47204920421229,0.428376856670855);
#1076=ELLIPSE('',#101758,0.354421145891317,0.321488604123643);
#1077=ELLIPSE('',#101759,0.35442108941965,0.321488612082172);
#1078=ELLIPSE('',#101764,0.472049204509708,0.428376857310086);
#1079=ELLIPSE('',#101765,0.472048618392543,0.428376332983298);
#1080=ELLIPSE('',#101766,0.354420976862898,0.321488380353674);
#1081=ELLIPSE('',#101767,0.354421121837047,0.321488565200586);
#1082=ELLIPSE('',#101769,0.472048618674403,0.428376333589021);
#1083=ELLIPSE('',#101770,0.472049204212828,0.428376856671933);
#1084=ELLIPSE('',#101771,0.354421145890464,0.321488604121916);
#1085=ELLIPSE('',#101772,0.354421089425979,0.321488612094869);
#1086=ELLIPSE('',#101777,0.472049204511167,0.428376857313033);
#1087=ELLIPSE('',#101778,0.472048618392917,0.428376332984035);
#1088=ELLIPSE('',#101779,0.354420976866564,0.321488380361024);
#1089=ELLIPSE('',#101780,0.354421121837239,0.321488565201024);
#1090=ELLIPSE('',#101782,0.47204861867434,0.428376333588864);
#1091=ELLIPSE('',#101783,0.472049204215799,0.428376856677852);
#1092=ELLIPSE('',#101784,0.354421145893017,0.321488604127082);
#1093=ELLIPSE('',#101785,0.354421089422275,0.32148861208739);
#1094=ELLIPSE('',#101790,0.472049204510112,0.428376857310949);
#1095=ELLIPSE('',#101791,0.472048618392829,0.428376332983904);
#1096=ELLIPSE('',#101792,0.354420976868174,0.321488380364233);
#1097=ELLIPSE('',#101793,0.354421121835105,0.321488565196644);
#1098=ELLIPSE('',#101795,0.47204861867308,0.428376333586349);
#1099=ELLIPSE('',#101796,0.472049204212913,0.428376856672089);
#1100=ELLIPSE('',#101797,0.354421145893018,0.321488604127051);
#1101=ELLIPSE('',#101798,0.354421089419571,0.321488612081999);
#1102=ELLIPSE('',#101803,0.47204920451173,0.428376857314131);
#1103=ELLIPSE('',#101804,0.472048618391224,0.428376332980738);
#1104=ELLIPSE('',#101805,0.354420976867017,0.321488380361812);
#1105=ELLIPSE('',#101806,0.354421121834112,0.32148856519467);
#1106=ELLIPSE('',#101808,0.472048618673977,0.428376333588137);
#1107=ELLIPSE('',#101809,0.472049204213291,0.428376856672807);
#1108=ELLIPSE('',#101810,0.354421145890671,0.321488604122366);
#1109=ELLIPSE('',#101811,0.354421089422301,0.32148861208759);
#1110=ELLIPSE('',#101816,0.472049204510848,0.428376857312395);
#1111=ELLIPSE('',#101817,0.472048618392992,0.428376332984159);
#1112=ELLIPSE('',#101818,0.354420976860473,0.321488380348803);
#1113=ELLIPSE('',#101819,0.354421121834424,0.321488565195281);
#1114=ELLIPSE('',#101821,0.472048618672387,0.428376333584996);
#1115=ELLIPSE('',#101822,0.472049204212593,0.428376856671442);
#1116=ELLIPSE('',#101823,0.354421145892271,0.321488604125565);
#1117=ELLIPSE('',#101824,0.354421089420506,0.321488612083924);
#1118=ELLIPSE('',#101829,0.472049204511836,0.428376857314351);
#1119=ELLIPSE('',#101830,0.472048618392818,0.4283763329839);
#1120=ELLIPSE('',#101831,0.354420976866767,0.32148838036158);
#1121=ELLIPSE('',#101832,0.354421121834996,0.321488565196547);
#1122=ELLIPSE('',#101834,0.472048618675398,0.428376333590942);
#1123=ELLIPSE('',#101835,0.472049204211585,0.428376856669487);
#1124=ELLIPSE('',#101836,0.354421145891481,0.321488604124059);
#1125=ELLIPSE('',#101837,0.354421089423297,0.321488612089601);
#1126=ELLIPSE('',#101842,0.47204920451136,0.428376857313437);
#1127=ELLIPSE('',#101843,0.472048618391754,0.428376332981795);
#1128=ELLIPSE('',#101844,0.35442097686543,0.321488380358688);
#1129=ELLIPSE('',#101845,0.354421121834514,0.321488565195397);
#1130=ELLIPSE('',#101847,0.472048618674643,0.42837633358945);
#1131=ELLIPSE('',#101848,0.472049204212558,0.428376856671375);
#1132=ELLIPSE('',#101849,0.354421145894868,0.321488604130772);
#1133=ELLIPSE('',#101850,0.354421089425284,0.321488612093512);
#1134=ELLIPSE('',#101855,0.472049204512137,0.428376857314884);
#1135=ELLIPSE('',#101856,0.472048618392142,0.428376332982475);
#1136=ELLIPSE('',#101857,0.354420976863592,0.321488380355156);
#1137=ELLIPSE('',#101858,0.354421121836417,0.321488565199247);
#1138=ELLIPSE('',#101860,0.472048618672645,0.428376333585489);
#1139=ELLIPSE('',#101861,0.472049204214127,0.428376856674531);
#1140=ELLIPSE('',#101862,0.354421145892333,0.321488604125701);
#1141=ELLIPSE('',#101863,0.354421089418798,0.321488612080517);
#1142=ELLIPSE('',#101868,0.472049204508436,0.428376857307603);
#1143=ELLIPSE('',#101869,0.472048618391932,0.428376332982128);
#1144=ELLIPSE('',#101870,0.354420976866755,0.321488380361313);
#1145=ELLIPSE('',#101871,0.35442112183523,0.321488565196882);
#1146=ELLIPSE('',#101873,0.472048618675024,0.428376333590223);
#1147=ELLIPSE('',#101874,0.472049204210922,0.428376856668115);
#1148=ELLIPSE('',#101875,0.354421145894346,0.32148860412975);
#1149=ELLIPSE('',#101876,0.354421089422433,0.321488612087672);
#1150=ELLIPSE('',#101881,0.472049204511066,0.428376857312761);
#1151=ELLIPSE('',#101882,0.472048618392184,0.428376332982542);
#1152=ELLIPSE('',#101883,0.354420976862911,0.321488380353758);
#1153=ELLIPSE('',#101884,0.354421121836188,0.321488565198844);
#1154=ELLIPSE('',#101886,0.472048618673788,0.428376333587768);
#1155=ELLIPSE('',#101887,0.472049204212535,0.428376856671301);
#1156=ELLIPSE('',#101888,0.3544211458936,0.321488604128272);
#1157=ELLIPSE('',#101889,0.354421089422695,0.321488612088294);
#1158=ELLIPSE('',#101894,0.472049204512777,0.428376857316141);
#1159=ELLIPSE('',#101895,0.472048618393533,0.428376332985314);
#1160=ELLIPSE('',#101896,0.35442097686458,0.321488380357273);
#1161=ELLIPSE('',#101897,0.354421121835712,0.321488565197931);
#1162=ELLIPSE('',#101899,0.472048618676399,0.428376333592959);
#1163=ELLIPSE('',#101900,0.472049204210939,0.428376856668195);
#1164=ELLIPSE('',#101901,0.354421145890564,0.321488604122185);
#1165=ELLIPSE('',#101902,0.35442108942679,0.321488612096456);
#1166=ELLIPSE('',#101907,0.472049204511024,0.428376857312705);
#1167=ELLIPSE('',#101908,0.472048618392565,0.428376332983383);
#1168=ELLIPSE('',#101909,0.354420976866851,0.321488380361658);
#1169=ELLIPSE('',#101910,0.3544211218354,0.321488565197227);
#1170=ELLIPSE('',#101912,0.472048618674338,0.428376333588867);
#1171=ELLIPSE('',#101913,0.472049204211911,0.428376856670035);
#1172=ELLIPSE('',#101914,0.354421145891812,0.32148860412464);
#1173=ELLIPSE('',#101915,0.354421089427689,0.321488612098307);
#1174=ELLIPSE('',#101920,0.472049204510186,0.428376857311083);
#1175=ELLIPSE('',#101921,0.472048618393607,0.428376332985412);
#1176=ELLIPSE('',#101922,0.354420976862319,0.321488380352444);
#1177=ELLIPSE('',#101923,0.354421121836503,0.321488565199374);
#1178=ELLIPSE('',#101925,0.472048618672938,0.428376333586069);
#1179=ELLIPSE('',#101926,0.472049204213753,0.428376856673768);
#1180=ELLIPSE('',#101927,0.354421145891945,0.321488604124921);
#1181=ELLIPSE('',#101928,0.354421089420938,0.321488612084783);
#1182=ELLIPSE('',#102048,0.146692861885567,0.127051669378531);
#1183=ELLIPSE('',#102060,0.146691465567121,0.127050784764082);
#1184=ELLIPSE('',#102077,0.146692861887463,0.127051669378996);
#1185=ELLIPSE('',#102088,0.146691465567168,0.12705078476413);
#1186=ELLIPSE('',#102092,0.146692861888896,0.127051669380489);
#1187=ELLIPSE('',#102104,0.146691465567147,0.127050784764154);
#1188=ELLIPSE('',#102121,0.146692861886083,0.127051669378904);
#1189=ELLIPSE('',#102132,0.146691465566885,0.127050784763844);
#1190=ELLIPSE('',#102136,0.14669286188763,0.127051669380222);
#1191=ELLIPSE('',#102148,0.146691465566526,0.127050784763542);
#1192=ELLIPSE('',#102165,0.146692861887613,0.127051669379494);
#1193=ELLIPSE('',#102176,0.146691465566883,0.127050784763874);
#1194=ELLIPSE('',#102180,0.146692861887666,0.127051669380264);
#1195=ELLIPSE('',#102192,0.14669146556646,0.127050784763503);
#1196=ELLIPSE('',#102209,0.146692861889141,0.127051669380783);
#1197=ELLIPSE('',#102220,0.146691465567298,0.127050784764247);
#1198=ELLIPSE('',#102224,0.146692861888368,0.127051669379501);
#1199=ELLIPSE('',#102236,0.146691465567334,0.127050784764234);
#1200=ELLIPSE('',#102253,0.146692861886808,0.12705166937917);
#1201=ELLIPSE('',#102264,0.146691465566578,0.127050784763566);
#1202=ELLIPSE('',#102268,0.146692861888158,0.12705166937956);
#1203=ELLIPSE('',#102280,0.146691465566373,0.127050784763473);
#1204=ELLIPSE('',#102297,0.146692861888516,0.127051669379843);
#1205=ELLIPSE('',#102308,0.146691465566914,0.127050784763955);
#1206=ELLIPSE('',#102312,0.146692861888309,0.127051669380947);
#1207=ELLIPSE('',#102324,0.146691465567861,0.127050784764697);
#1208=ELLIPSE('',#102341,0.146692861885721,0.12705166937859);
#1209=ELLIPSE('',#102352,0.146691465566683,0.127050784763667);
#1210=ELLIPSE('',#102356,0.146692861888495,0.127051669380134);
#1211=ELLIPSE('',#102368,0.146691465567092,0.127050784764018);
#1212=ELLIPSE('',#102385,0.146692861888546,0.127051669380193);
#1213=ELLIPSE('',#102396,0.146691465567027,0.127050784763971);
#1214=ELLIPSE('',#102400,0.146692861887502,0.127051669379823);
#1215=ELLIPSE('',#102412,0.146691465567408,0.127050784764332);
#1216=ELLIPSE('',#102429,0.14669286188688,0.12705166937983);
#1217=ELLIPSE('',#102440,0.146691465567052,0.127050784763936);
#1218=ELLIPSE('',#102444,0.146692861890649,0.12705166938136);
#1219=ELLIPSE('',#102456,0.146691465567283,0.127050784764214);
#1220=ELLIPSE('',#102473,0.14669286188667,0.127051669379132);
#1221=ELLIPSE('',#102484,0.146691465566737,0.127050784763775);
#1222=ELLIPSE('',#102488,0.146692861885645,0.127051669379056);
#1223=ELLIPSE('',#102500,0.146691465566775,0.127050784763843);
#1224=ELLIPSE('',#102517,0.146692861887981,0.127051669380469);
#1225=ELLIPSE('',#102528,0.146691465567127,0.127050784764071);
#1226=ELLIPSE('',#102532,0.14669286188498,0.127051669377859);
#1227=ELLIPSE('',#102544,0.146691465566808,0.12705078476382);
#1228=ELLIPSE('',#102561,0.146692861889004,0.127051669380733);
#1229=ELLIPSE('',#102572,0.146691465567489,0.127050784764374);
#1230=ELLIPSE('',#102576,0.146692861885976,0.127051669378296);
#1231=ELLIPSE('',#102588,0.146691465567608,0.127050784764498);
#1232=ELLIPSE('',#102605,0.146692861886447,0.127051669378633);
#1233=ELLIPSE('',#102616,0.146691465566876,0.127050784763821);
#1234=ELLIPSE('',#102620,0.146692861886796,0.127051669378311);
#1235=ELLIPSE('',#102632,0.146691465567447,0.127050784764411);
#1236=ELLIPSE('',#102649,0.146692861889843,0.127051669381439);
#1237=ELLIPSE('',#102660,0.146691465567239,0.127050784764164);
#1238=ELLIPSE('',#102664,0.146692861890044,0.127051669381479);
#1239=ELLIPSE('',#102676,0.146691465567008,0.127050784763937);
#1240=ELLIPSE('',#102693,0.146692861885891,0.127051669378644);
#1241=ELLIPSE('',#102704,0.146691465567079,0.127050784764031);
#1242=ELLIPSE('',#102708,0.146692861888645,0.127051669380685);
#1243=ELLIPSE('',#102720,0.146691465567215,0.127050784764091);
#1244=ELLIPSE('',#102737,0.14669286188768,0.127051669379306);
#1245=ELLIPSE('',#102748,0.1466914655671,0.127050784764053);
#1246=ELLIPSE('',#102752,0.14669286188937,0.127051669381317);
#1247=ELLIPSE('',#102764,0.146691465567315,0.127050784764199);
#1248=ELLIPSE('',#102781,0.146692861887002,0.12705166937927);
#1249=ELLIPSE('',#102792,0.14669146556677,0.127050784763695);
#1250=ELLIPSE('',#102796,0.146692861887507,0.127051669380439);
#1251=ELLIPSE('',#102808,0.146691465567352,0.127050784764268);
#1252=ELLIPSE('',#102825,0.146692861887076,0.12705166937942);
#1253=ELLIPSE('',#102836,0.146691465566914,0.127050784763854);
#1254=ELLIPSE('',#102840,0.146692861887194,0.127051669379424);
#1255=ELLIPSE('',#102852,0.14669146556758,0.127050784764477);
#1256=ELLIPSE('',#102869,0.146692861888878,0.127051669380784);
#1257=ELLIPSE('',#102880,0.146691465567144,0.127050784764121);
#1258=ELLIPSE('',#102884,0.146692861887721,0.12705166937974);
#1259=ELLIPSE('',#102896,0.146691465567568,0.127050784764376);
#1260=ELLIPSE('',#102913,0.14669286188805,0.12705166938014);
#1261=ELLIPSE('',#102924,0.146691465567017,0.127050784763977);
#1262=ELLIPSE('',#102928,0.14669286188764,0.127051669379003);
#1263=ELLIPSE('',#102940,0.146691465566713,0.127050784763719);
#1264=ELLIPSE('',#102957,0.146692861888337,0.127051669380451);
#1265=ELLIPSE('',#102968,0.146691465567126,0.127050784763968);
#1266=ELLIPSE('',#102972,0.146692861887168,0.127051669379855);
#1267=ELLIPSE('',#102984,0.146691465566658,0.127050784763777);
#1268=ELLIPSE('',#103001,0.146692861887582,0.12705166937951);
#1269=ELLIPSE('',#103012,0.146691465567075,0.127050784764051);
#1270=ELLIPSE('',#103016,0.146692861888137,0.127051669380366);
#1271=ELLIPSE('',#103028,0.146691465567644,0.127050784764539);
#1272=ELLIPSE('',#103045,0.14669286188819,0.127051669379585);
#1273=ELLIPSE('',#103056,0.146691465567195,0.127050784764162);
#1274=ELLIPSE('',#103060,0.146692861889408,0.127051669380712);
#1275=ELLIPSE('',#103072,0.146691465566922,0.127050784763894);
#1276=ELLIPSE('',#103089,0.146692861888037,0.127051669379771);
#1277=ELLIPSE('',#103100,0.14669146556638,0.127050784763349);
#1278=ELLIPSE('',#103104,0.146692861889155,0.127051669380763);
#1279=ELLIPSE('',#103116,0.14669146556706,0.12705078476401);
#1280=ELLIPSE('',#103133,0.146692861882926,0.127051669377485);
#1281=ELLIPSE('',#103144,0.146691465567588,0.127050784764391);
#1282=ELLIPSE('',#103148,0.146692861885302,0.127051669379186);
#1283=ELLIPSE('',#103160,0.14669146556641,0.127050784763393);
#1284=ELLIPSE('',#103177,0.146692861883317,0.127051669378118);
#1285=ELLIPSE('',#103188,0.14669146556702,0.12705078476395);
#1286=ELLIPSE('',#103192,0.146692861885936,0.127051669377782);
#1287=ELLIPSE('',#103204,0.146691465567513,0.12705078476445);
#1288=ELLIPSE('',#103221,0.146692861888335,0.12705166938049);
#1289=ELLIPSE('',#103232,0.146691465567078,0.127050784763984);
#1290=ELLIPSE('',#103236,0.146692861887502,0.127051669379887);
#1291=ELLIPSE('',#103248,0.146691465567418,0.12705078476439);
#1292=ELLIPSE('',#103265,0.14669286188641,0.127051669379223);
#1293=ELLIPSE('',#103276,0.146691465568432,0.127050784765296);
#1294=ELLIPSE('',#103280,0.146692861886973,0.127051669378979);
#1295=ELLIPSE('',#103292,0.146691465567226,0.127050784764225);
#1296=ELLIPSE('',#103309,0.146692861887159,0.127051669379778);
#1297=ELLIPSE('',#103320,0.146691465566851,0.12705078476372);
#1298=ELLIPSE('',#103324,0.14669286188588,0.12705166937876);
#1299=ELLIPSE('',#103336,0.146691465567206,0.127050784764128);
#1300=ELLIPSE('',#103347,0.146692861889522,0.127051669380795);
#1301=ELLIPSE('',#103358,0.146691465567411,0.127050784764298);
#1302=ELLIPSE('',#103362,0.146692861889838,0.127051669381324);
#1303=ELLIPSE('',#103374,0.146691465567167,0.127050784764082);
#1304=ELLIPSE('',#103391,0.146692861887389,0.127051669379282);
#1305=ELLIPSE('',#103402,0.146691465566456,0.127050784763464);
#1306=ELLIPSE('',#103406,0.146692861889915,0.127051669381599);
#1307=ELLIPSE('',#103418,0.146691465567079,0.127050784764074);
#1308=ELLIPSE('',#103435,0.146692861886959,0.127051669379107);
#1309=ELLIPSE('',#103446,0.146691465565599,0.127050784762682);
#1310=ELLIPSE('',#103450,0.146692861886111,0.127051669378854);
#1311=ELLIPSE('',#103462,0.146691465566701,0.127050784763677);
#1312=ELLIPSE('',#103479,0.146692861887203,0.127051669379281);
#1313=ELLIPSE('',#103490,0.14669146556731,0.127050784764204);
#1314=ELLIPSE('',#103494,0.146692861883759,0.127051669378026);
#1315=ELLIPSE('',#103506,0.146691465567332,0.127050784764243);
#1316=ELLIPSE('',#103523,0.146692861886141,0.127051669379513);
#1317=ELLIPSE('',#103534,0.14669146556683,0.127050784763821);
#1318=ELLIPSE('',#103538,0.146692861885915,0.127051669378914);
#1319=ELLIPSE('',#103550,0.146691465566953,0.127050784763947);
#1320=ELLIPSE('',#103567,0.146692861888415,0.12705166938034);
#1321=ELLIPSE('',#103578,0.146691465567478,0.127050784764331);
#1322=ELLIPSE('',#103582,0.146692861891607,0.12705166938209);
#1323=ELLIPSE('',#103594,0.146691465566998,0.127050784763999);
#1324=ELLIPSE('',#103611,0.146692861888674,0.127051669380524);
#1325=ELLIPSE('',#103622,0.146691465567211,0.12705078476419);
#1326=ELLIPSE('',#103626,0.146692861883882,0.12705166937676);
#1327=ELLIPSE('',#103638,0.146691465566793,0.127050784763746);
#1328=ELLIPSE('',#103655,0.146692861887673,0.127051669380417);
#1329=ELLIPSE('',#103666,0.146691465567382,0.127050784764219);
#1330=ELLIPSE('',#103670,0.146692861887705,0.12705166937983);
#1331=ELLIPSE('',#103682,0.146691465566038,0.127050784763052);
#1332=ELLIPSE('',#103699,0.146692861889167,0.127051669380751);
#1333=ELLIPSE('',#103710,0.146691465567573,0.127050784764422);
#1334=ELLIPSE('',#103714,0.146692861889612,0.127051669381335);
#1335=ELLIPSE('',#103726,0.146691465567708,0.127050784764662);
#1336=ELLIPSE('',#103743,0.146692861889342,0.127051669380336);
#1337=ELLIPSE('',#103754,0.146691465567366,0.12705078476425);
#1338=ELLIPSE('',#103758,0.146692861886576,0.127051669378749);
#1339=ELLIPSE('',#103770,0.146691465566999,0.127050784763989);
#1340=ELLIPSE('',#103787,0.146692861884538,0.127051669377373);
#1341=ELLIPSE('',#103798,0.146691465567589,0.127050784764443);
#1342=ELLIPSE('',#103802,0.146692861890103,0.12705166938084);
#1343=ELLIPSE('',#103814,0.146691465567319,0.12705078476426);
#1344=ELLIPSE('',#103831,0.14669286189003,0.127051669381485);
#1345=ELLIPSE('',#103842,0.146691465567331,0.127050784764255);
#1346=ELLIPSE('',#103846,0.146692861888385,0.127051669380528);
#1347=ELLIPSE('',#103858,0.146691465566983,0.127050784763952);
#1348=ELLIPSE('',#103875,0.146692861884411,0.127051669377628);
#1349=ELLIPSE('',#103886,0.14669146556668,0.127050784763682);
#1350=ELLIPSE('',#103890,0.146692861886796,0.127051669378175);
#1351=ELLIPSE('',#103902,0.146691465566957,0.127050784763979);
#1352=ELLIPSE('',#103919,0.146692861887698,0.127051669379726);
#1353=ELLIPSE('',#103930,0.146691465567331,0.127050784764215);
#1354=ELLIPSE('',#103934,0.146692861885919,0.127051669378147);
#1355=ELLIPSE('',#103946,0.146691465566696,0.127050784763722);
#1356=ELLIPSE('',#103963,0.146692861886562,0.127051669379923);
#1357=ELLIPSE('',#103974,0.146691465567798,0.127050784764758);
#1358=ELLIPSE('',#103978,0.146692861888357,0.127051669380143);
#1359=ELLIPSE('',#103990,0.146691465567536,0.127050784764469);
#1360=ELLIPSE('',#104001,0.146692861886404,0.127051669379228);
#1361=ELLIPSE('',#104012,0.146691465567304,0.127050784764238);
#1362=ELLIPSE('',#104016,0.146692861888012,0.127051669380023);
#1363=ELLIPSE('',#104028,0.146691465567932,0.127050784764812);
#1364=ELLIPSE('',#104045,0.146692861885984,0.127051669378374);
#1365=ELLIPSE('',#104056,0.146691465567718,0.127050784764633);
#1366=ELLIPSE('',#104060,0.146692861888494,0.127051669381475);
#1367=ELLIPSE('',#104072,0.146691465566806,0.127050784763805);
#1368=ELLIPSE('',#104089,0.146692861886582,0.127051669379945);
#1369=ELLIPSE('',#104100,0.146691465566983,0.127050784763979);
#1370=ELLIPSE('',#104104,0.146692861885909,0.127051669378487);
#1371=ELLIPSE('',#104116,0.146691465566881,0.127050784763817);
#1372=ELLIPSE('',#104133,0.14669286188397,0.127051669377901);
#1373=ELLIPSE('',#104144,0.14669146556726,0.127050784764136);
#1374=ELLIPSE('',#104148,0.146692861885557,0.127051669377438);
#1375=ELLIPSE('',#104160,0.146691465567094,0.127050784764054);
#1376=ELLIPSE('',#104177,0.146692861888974,0.127051669380765);
#1377=ELLIPSE('',#104188,0.146691465567152,0.127050784764145);
#1378=ELLIPSE('',#104192,0.146692861888481,0.127051669380402);
#1379=ELLIPSE('',#104204,0.146691465566779,0.127050784763768);
#1380=ELLIPSE('',#104221,0.146692861888643,0.127051669380515);
#1381=ELLIPSE('',#104232,0.146691465567502,0.12705078476442);
#1382=ELLIPSE('',#104236,0.146692861890789,0.127051669381522);
#1383=ELLIPSE('',#104248,0.146691465566763,0.127050784763716);
#1384=ELLIPSE('',#104265,0.146692861888623,0.127051669380775);
#1385=ELLIPSE('',#104276,0.146691465566699,0.127050784763675);
#1386=ELLIPSE('',#104280,0.146692861888628,0.127051669380256);
#1387=ELLIPSE('',#104292,0.146691465566495,0.127050784763492);
#1388=ELLIPSE('',#104309,0.146692861887913,0.127051669380643);
#1389=ELLIPSE('',#104320,0.146691465568001,0.127050784764842);
#1390=ELLIPSE('',#104324,0.146692861885188,0.127051669378267);
#1391=ELLIPSE('',#104336,0.146691465566441,0.12705078476341);
#1392=ELLIPSE('',#104353,0.146692861887209,0.127051669379935);
#1393=ELLIPSE('',#104364,0.14669146556709,0.12705078476406);
#1394=ELLIPSE('',#104368,0.146692861890518,0.127051669381353);
#1395=ELLIPSE('',#104380,0.146691465567507,0.127050784764375);
#1396=ELLIPSE('',#104397,0.146692861883823,0.127051669377884);
#1397=ELLIPSE('',#104408,0.146691465567289,0.127050784764197);
#1398=ELLIPSE('',#104412,0.146692861890507,0.127051669381576);
#1399=ELLIPSE('',#104424,0.146691465567104,0.127050784764032);
#1400=ELLIPSE('',#104441,0.146692861883025,0.127051669377497);
#1401=ELLIPSE('',#104452,0.146691465567122,0.127050784764081);
#1402=ELLIPSE('',#104456,0.146692861888651,0.127051669380448);
#1403=ELLIPSE('',#104468,0.146691465567346,0.127050784764286);
#1404=ELLIPSE('',#104485,0.146692861886992,0.127051669380085);
#1405=ELLIPSE('',#104496,0.146691465566997,0.127050784763992);
#1406=ELLIPSE('',#104500,0.146692861887178,0.127051669379325);
#1407=ELLIPSE('',#104512,0.146691465567046,0.127050784763963);
#1408=ELLIPSE('',#104529,0.146692861888523,0.127051669381091);
#1409=ELLIPSE('',#104540,0.146691465567343,0.127050784764274);
#1410=ELLIPSE('',#104544,0.146692861885037,0.127051669378257);
#1411=ELLIPSE('',#104556,0.146691465567072,0.127050784763942);
#1412=ELLIPSE('',#104573,0.146692861888248,0.127051669380601);
#1413=ELLIPSE('',#104584,0.14669146556705,0.12705078476398);
#1414=ELLIPSE('',#104588,0.146692861886568,0.127051669378735);
#1415=ELLIPSE('',#104600,0.146691465566741,0.127050784763756);
#1416=ELLIPSE('',#104617,0.146692861887918,0.127051669379379);
#1417=ELLIPSE('',#104628,0.146691465566682,0.127050784763618);
#1418=ELLIPSE('',#104939,0.599370291563125,0.555629413545895);
#1419=ELLIPSE('',#104940,0.599370913936886,0.555630771248663);
#1420=ELLIPSE('',#104942,0.239805704053497,0.222043163091629);
#1421=ELLIPSE('',#104943,0.239805889070534,0.222043643393249);
#1422=ELLIPSE('',#104945,0.239805882896056,0.222043378690167);
#1423=ELLIPSE('',#104946,0.239805697268546,0.222042896628002);
#1424=ELLIPSE('',#104968,0.599370913936424,0.555630771247676);
#1425=ELLIPSE('',#104969,0.599370291563989,0.555629413547554);
#1426=ELLIPSE('',#104971,0.239805889069708,0.222043643391541);
#1427=ELLIPSE('',#104972,0.239805704051741,0.222043163087965);
#1428=ELLIPSE('',#104974,0.239805697269063,0.222042896629096);
#1429=ELLIPSE('',#104975,0.239805882896364,0.222043378690804);
#1430=ELLIPSE('',#104997,0.599370913938641,0.555630771252141);
#1431=ELLIPSE('',#104998,0.599370291563862,0.555629413547371);
#1432=ELLIPSE('',#105000,0.239805889070602,0.222043643393427);
#1433=ELLIPSE('',#105001,0.23980570405374,0.22204316309224);
#1434=ELLIPSE('',#105003,0.239805697270237,0.222042896631561);
#1435=ELLIPSE('',#105004,0.239805882896258,0.222043378690633);
#1436=ELLIPSE('',#105026,0.599370913937861,0.555630771250355);
#1437=ELLIPSE('',#105027,0.599370291563252,0.555629413546106);
#1438=ELLIPSE('',#105029,0.239805889071049,0.222043643394189);
#1439=ELLIPSE('',#105030,0.239805704053008,0.222043163090523);
#1440=ELLIPSE('',#105032,0.239805697269095,0.222042896629257);
#1441=ELLIPSE('',#105033,0.239805882896199,0.222043378690359);
#1442=ELLIPSE('',#105055,0.599370913937953,0.555630771250761);
#1443=ELLIPSE('',#105056,0.59937029156439,0.555629413548469);
#1444=ELLIPSE('',#105058,0.239805889069954,0.222043643392037);
#1445=ELLIPSE('',#105059,0.239805704051625,0.222043163087767);
#1446=ELLIPSE('',#105061,0.239805697269453,0.222042896629888);
#1447=ELLIPSE('',#105062,0.239805882894231,0.22204337868653);
#1448=ELLIPSE('',#105084,0.599370913935848,0.555630771246351);
#1449=ELLIPSE('',#105085,0.599370291563755,0.555629413547092);
#1450=ELLIPSE('',#105087,0.23980588907091,0.222043643394013);
#1451=ELLIPSE('',#105088,0.23980570405483,0.222043163094366);
#1452=ELLIPSE('',#105090,0.239805697270176,0.222042896631468);
#1453=ELLIPSE('',#105091,0.239805882895749,0.222043378689575);
#1454=ELLIPSE('',#105113,0.599370913938043,0.555630771251001);
#1455=ELLIPSE('',#105114,0.599370291563443,0.555629413546439);
#1456=ELLIPSE('',#105116,0.23980588907133,0.222043643394784);
#1457=ELLIPSE('',#105117,0.239805704053637,0.222043163091898);
#1458=ELLIPSE('',#105119,0.239805697268382,0.222042896627742);
#1459=ELLIPSE('',#105120,0.239805882894225,0.2220433786865);
#1460=ELLIPSE('',#105142,0.599370913937164,0.555630771249295);
#1461=ELLIPSE('',#105143,0.599370291564909,0.555629413549435);
#1462=ELLIPSE('',#105145,0.23980588907154,0.222043643395249);
#1463=ELLIPSE('',#105146,0.239805704053149,0.222043163090889);
#1464=ELLIPSE('',#105148,0.239805697270284,0.222042896631555);
#1465=ELLIPSE('',#105149,0.23980588289412,0.222043378686234);
#1466=ELLIPSE('',#105171,0.599370913937173,0.555630771249146);
#1467=ELLIPSE('',#105172,0.599370291561398,0.555629413542466);
#1468=ELLIPSE('',#105174,0.239805889070354,0.222043643392804);
#1469=ELLIPSE('',#105175,0.239805704053545,0.222043163091733);
#1470=ELLIPSE('',#105177,0.239805697271406,0.222042896633952);
#1471=ELLIPSE('',#105178,0.239805882895816,0.222043378689676);
#1472=ELLIPSE('',#105200,0.599370913937036,0.555630771248811);
#1473=ELLIPSE('',#105201,0.599370291563916,0.555629413547388);
#1474=ELLIPSE('',#105203,0.239805889071604,0.222043643395432);
#1475=ELLIPSE('',#105204,0.239805704053184,0.222043163090952);
#1476=ELLIPSE('',#105206,0.239805697268027,0.222042896626982);
#1477=ELLIPSE('',#105207,0.239805882895104,0.222043378688241);
#1478=ELLIPSE('',#105229,0.599370913938747,0.555630771252324);
#1479=ELLIPSE('',#105230,0.599370291563773,0.555629413547104);
#1480=ELLIPSE('',#105232,0.239805889069953,0.222043643391901);
#1481=ELLIPSE('',#105233,0.239805704053491,0.222043163091448);
#1482=ELLIPSE('',#105235,0.239805697268958,0.222042896628944);
#1483=ELLIPSE('',#105236,0.239805882896265,0.222043378690656);
#1484=ELLIPSE('',#105258,0.59937091393634,0.555630771247396);
#1485=ELLIPSE('',#105259,0.599370291564068,0.555629413547775);
#1486=ELLIPSE('',#105261,0.239805889068713,0.222043643389376);
#1487=ELLIPSE('',#105262,0.239805704053382,0.222043163091307);
#1488=ELLIPSE('',#105264,0.239805697270786,0.222042896632642);
#1489=ELLIPSE('',#105265,0.239805882894861,0.222043378687808);
#1490=ELLIPSE('',#105287,0.59937091393686,0.555630771248516);
#1491=ELLIPSE('',#105288,0.599370291565143,0.555629413549944);
#1492=ELLIPSE('',#105290,0.239805889071215,0.222043643394497);
#1493=ELLIPSE('',#105291,0.239805704050963,0.222043163086415);
#1494=ELLIPSE('',#105293,0.239805697269532,0.222042896630181);
#1495=ELLIPSE('',#105294,0.239805882893921,0.222043378685855);
#1496=ELLIPSE('',#105316,0.599370913938124,0.555630771251031);
#1497=ELLIPSE('',#105317,0.599370291563806,0.555629413547086);
#1498=ELLIPSE('',#105319,0.239805889070086,0.222043643392291);
#1499=ELLIPSE('',#105320,0.239805704054589,0.222043163093833);
#1500=ELLIPSE('',#105322,0.239805697267829,0.222042896626754);
#1501=ELLIPSE('',#105323,0.239805882895978,0.222043378689986);
#1502=ELLIPSE('',#105345,0.599370913938156,0.555630771251131);
#1503=ELLIPSE('',#105346,0.599370291565494,0.555629413550808);
#1504=ELLIPSE('',#105348,0.239805889069306,0.222043643390778);
#1505=ELLIPSE('',#105349,0.239805704052843,0.222043163090263);
#1506=ELLIPSE('',#105351,0.239805697267564,0.222042896626005);
#1507=ELLIPSE('',#105352,0.239805882895109,0.222043378688375);
#1508=ELLIPSE('',#105374,0.599370913936692,0.555630771248211);
#1509=ELLIPSE('',#105375,0.599370291564028,0.555629413547596);
#1510=ELLIPSE('',#105377,0.239805889070008,0.222043643392147);
#1511=ELLIPSE('',#105378,0.239805704053846,0.22204316309233);
#1512=ELLIPSE('',#105380,0.239805697267772,0.222042896626517);
#1513=ELLIPSE('',#105381,0.239805882894887,0.222043378687704);
#1514=ELLIPSE('',#105403,0.599370913937781,0.555630771250321);
#1515=ELLIPSE('',#105404,0.599370291564289,0.555629413548149);
#1516=ELLIPSE('',#105406,0.239805889071197,0.22204364339454);
#1517=ELLIPSE('',#105407,0.239805704052616,0.222043163089868);
#1518=ELLIPSE('',#105409,0.239805697268978,0.222042896629065);
#1519=ELLIPSE('',#105410,0.239805882893747,0.222043378685553);
#1520=ELLIPSE('',#105432,0.599370913937385,0.555630771249585);
#1521=ELLIPSE('',#105433,0.599370291563214,0.555629413545959);
#1522=ELLIPSE('',#105435,0.239805889069715,0.222043643391482);
#1523=ELLIPSE('',#105436,0.239805704052201,0.222043163088935);
#1524=ELLIPSE('',#105438,0.239805697268373,0.22204289662777);
#1525=ELLIPSE('',#105439,0.239805882895439,0.222043378688964);
#1526=ELLIPSE('',#105461,0.599370913937343,0.555630771249459);
#1527=ELLIPSE('',#105462,0.599370291565652,0.555629413550879);
#1528=ELLIPSE('',#105464,0.239805889069491,0.22204364339108);
#1529=ELLIPSE('',#105465,0.239805704052873,0.222043163090334);
#1530=ELLIPSE('',#105467,0.239805697269606,0.222042896630312);
#1531=ELLIPSE('',#105468,0.239805882895383,0.222043378688917);
#1532=ELLIPSE('',#105490,0.599370913936772,0.555630771248262);
#1533=ELLIPSE('',#105491,0.599370291561432,0.555629413542396);
#1534=ELLIPSE('',#105493,0.239805889069508,0.222043643391159);
#1535=ELLIPSE('',#105494,0.239805704052393,0.222043163089365);
#1536=ELLIPSE('',#105496,0.239805697268768,0.222042896628504);
#1537=ELLIPSE('',#105497,0.239805882896303,0.222043378690712);
#1538=ELLIPSE('',#105519,0.599370913936514,0.55563077124775);
#1539=ELLIPSE('',#105520,0.599370291562479,0.555629413544463);
#1540=ELLIPSE('',#105522,0.239805889069246,0.222043643390585);
#1541=ELLIPSE('',#105523,0.239805704052799,0.222043163090167);
#1542=ELLIPSE('',#105525,0.239805697269329,0.222042896629708);
#1543=ELLIPSE('',#105526,0.239805882896447,0.222043378691029);
#1544=ELLIPSE('',#105548,0.599370913936981,0.555630771248714);
#1545=ELLIPSE('',#105549,0.599370291561483,0.555629413542514);
#1546=ELLIPSE('',#105551,0.239805889069226,0.222043643390464);
#1547=ELLIPSE('',#105552,0.239805704052303,0.222043163089193);
#1548=ELLIPSE('',#105554,0.23980569726999,0.222042896631006);
#1549=ELLIPSE('',#105555,0.239805882894476,0.222043378686997);
#1550=ELLIPSE('',#105577,0.59937091393658,0.55563077124799);
#1551=ELLIPSE('',#105578,0.599370291562161,0.555629413543808);
#1552=ELLIPSE('',#105580,0.239805889071181,0.222043643394472);
#1553=ELLIPSE('',#105581,0.239805704051107,0.222043163086687);
#1554=ELLIPSE('',#105583,0.239805697269072,0.222042896629138);
#1555=ELLIPSE('',#105584,0.239805882893892,0.222043378685787);
#1556=ELLIPSE('',#105606,0.599370913936289,0.555630771247213);
#1557=ELLIPSE('',#105607,0.599370291564418,0.55562941354841);
#1558=ELLIPSE('',#105609,0.239805889069663,0.222043643391489);
#1559=ELLIPSE('',#105610,0.239805704053156,0.222043163090918);
#1560=ELLIPSE('',#105612,0.239805697269376,0.222042896629822);
#1561=ELLIPSE('',#105613,0.239805882896806,0.222043378691719);
#1562=ELLIPSE('',#105635,0.599370913938526,0.555630771252064);
#1563=ELLIPSE('',#105636,0.599370291563832,0.555629413547157);
#1564=ELLIPSE('',#105638,0.239805889069048,0.222043643390122);
#1565=ELLIPSE('',#105639,0.23980570405477,0.222043163094288);
#1566=ELLIPSE('',#105641,0.23980569726812,0.2220428966272);
#1567=ELLIPSE('',#105642,0.239805882894018,0.22204337868601);
#1568=ELLIPSE('',#105664,0.599370913936541,0.555630771247853);
#1569=ELLIPSE('',#105665,0.599370291564177,0.555629413547897);
#1570=ELLIPSE('',#105667,0.239805889069938,0.222043643391941);
#1571=ELLIPSE('',#105668,0.239805704053486,0.222043163091714);
#1572=ELLIPSE('',#105670,0.239805697268881,0.22204289662876);
#1573=ELLIPSE('',#105671,0.239805882895112,0.222043378688207);
#1574=ELLIPSE('',#105693,0.599370913938039,0.555630771250867);
#1575=ELLIPSE('',#105694,0.599370291564512,0.555629413548494);
#1576=ELLIPSE('',#105696,0.239805889069684,0.222043643391463);
#1577=ELLIPSE('',#105697,0.239805704053833,0.222043163092344);
#1578=ELLIPSE('',#105699,0.239805697268846,0.222042896628737);
#1579=ELLIPSE('',#105700,0.239805882897031,0.222043378692232);
#1580=ELLIPSE('',#105722,0.599370913936877,0.555630771248588);
#1581=ELLIPSE('',#105723,0.599370291562475,0.555629413544577);
#1582=ELLIPSE('',#105725,0.239805889068947,0.222043643389968);
#1583=ELLIPSE('',#105726,0.239805704052611,0.222043163089871);
#1584=ELLIPSE('',#105728,0.23980569726888,0.222042896628872);
#1585=ELLIPSE('',#105729,0.239805882896037,0.222043378690158);
#1586=ELLIPSE('',#105751,0.599370913936578,0.55563077124794);
#1587=ELLIPSE('',#105752,0.599370291564127,0.555629413547831);
#1588=ELLIPSE('',#105754,0.239805889069815,0.2220436433917);
#1589=ELLIPSE('',#105755,0.23980570405164,0.222043163087847);
#1590=ELLIPSE('',#105757,0.23980569726956,0.222042896630156);
#1591=ELLIPSE('',#105758,0.239805882895319,0.222043378688701);
#1592=ELLIPSE('',#105780,0.599370913938708,0.555630771252267);
#1593=ELLIPSE('',#105781,0.599370291563981,0.555629413547567);
#1594=ELLIPSE('',#105783,0.239805889070531,0.222043643393195);
#1595=ELLIPSE('',#105784,0.239805704052955,0.222043163090464);
#1596=ELLIPSE('',#105786,0.239805697267724,0.222042896626334);
#1597=ELLIPSE('',#105787,0.239805882894363,0.222043378686709);
#1598=ELLIPSE('',#105809,0.599370913938198,0.555630771251102);
#1599=ELLIPSE('',#105810,0.599370291564309,0.555629413548225);
#1600=ELLIPSE('',#105812,0.239805889069912,0.22204364339194);
#1601=ELLIPSE('',#105813,0.239805704052815,0.222043163090226);
#1602=ELLIPSE('',#105815,0.239805697269805,0.222042896630579);
#1603=ELLIPSE('',#105816,0.239805882895327,0.222043378688781);
#1604=ELLIPSE('',#105838,0.5993709139359,0.555630771246453);
#1605=ELLIPSE('',#105839,0.599370291564582,0.555629413548754);
#1606=ELLIPSE('',#105841,0.239805889071206,0.222043643394522);
#1607=ELLIPSE('',#105842,0.239805704053369,0.222043163091383);
#1608=ELLIPSE('',#105844,0.239805697269504,0.222042896630047);
#1609=ELLIPSE('',#105845,0.239805882894382,0.222043378686745);
#1610=ELLIPSE('',#105867,0.599370913938674,0.555630771252144);
#1611=ELLIPSE('',#105868,0.599370291562963,0.555629413545488);
#1612=ELLIPSE('',#105870,0.239805889069481,0.222043643391073);
#1613=ELLIPSE('',#105871,0.239805704050848,0.222043163086202);
#1614=ELLIPSE('',#105873,0.239805697268431,0.222042896627882);
#1615=ELLIPSE('',#105874,0.239805882896349,0.222043378690827);
#1616=ELLIPSE('',#105896,0.599370913936395,0.555630771247448);
#1617=ELLIPSE('',#105897,0.599370291566618,0.555629413552874);
#1618=ELLIPSE('',#105899,0.239805889069956,0.222043643391995);
#1619=ELLIPSE('',#105900,0.239805704052727,0.222043163090096);
#1620=ELLIPSE('',#105902,0.239805697269363,0.222042896629784);
#1621=ELLIPSE('',#105903,0.23980588289559,0.222043378689183);
#1622=ELLIPSE('',#105925,0.599370913937641,0.555630771249903);
#1623=ELLIPSE('',#105926,0.599370291564417,0.555629413548418);
#1624=ELLIPSE('',#105928,0.239805889070735,0.22204364339359);
#1625=ELLIPSE('',#105929,0.239805704054714,0.222043163094138);
#1626=ELLIPSE('',#105931,0.239805697269139,0.222042896629365);
#1627=ELLIPSE('',#105932,0.239805882894918,0.222043378687834);
#1628=ELLIPSE('',#105954,0.599370913937249,0.555630771249287);
#1629=ELLIPSE('',#105955,0.599370291563887,0.555629413547403);
#1630=ELLIPSE('',#105957,0.239805889070777,0.222043643393741);
#1631=ELLIPSE('',#105958,0.239805704051975,0.22204316308848);
#1632=ELLIPSE('',#105960,0.239805697266916,0.222042896624693);
#1633=ELLIPSE('',#105961,0.239805882895061,0.222043378688168);
#1634=ELLIPSE('',#105983,0.599370913938545,0.555630771251985);
#1635=ELLIPSE('',#105984,0.599370291562687,0.555629413544967);
#1636=ELLIPSE('',#105986,0.239805889070212,0.222043643392528);
#1637=ELLIPSE('',#105987,0.239805704051763,0.222043163088153);
#1638=ELLIPSE('',#105989,0.239805697268783,0.222042896628616);
#1639=ELLIPSE('',#105990,0.239805882896158,0.222043378690411);
#1640=ELLIPSE('',#106012,0.599370913937149,0.555630771249181);
#1641=ELLIPSE('',#106013,0.599370291564607,0.555629413548761);
#1642=ELLIPSE('',#106015,0.239805889070846,0.222043643393813);
#1643=ELLIPSE('',#106016,0.239805704053588,0.222043163091749);
#1644=ELLIPSE('',#106018,0.239805697268943,0.222042896628931);
#1645=ELLIPSE('',#106019,0.239805882894556,0.222043378687108);
#1646=ELLIPSE('',#106041,0.599370913936176,0.555630771247153);
#1647=ELLIPSE('',#106042,0.59937029156489,0.555629413549416);
#1648=ELLIPSE('',#106044,0.239805889070307,0.222043643392796);
#1649=ELLIPSE('',#106045,0.239805704052103,0.22204316308874);
#1650=ELLIPSE('',#106047,0.239805697269308,0.222042896629674);
#1651=ELLIPSE('',#106048,0.239805882894806,0.222043378687586);
#1652=ELLIPSE('',#106070,0.599370913937901,0.555630771250564);
#1653=ELLIPSE('',#106071,0.599370291564246,0.555629413548082);
#1654=ELLIPSE('',#106073,0.239805889069668,0.222043643391381);
#1655=ELLIPSE('',#106074,0.239805704051946,0.222043163088454);
#1656=ELLIPSE('',#106076,0.239805697269087,0.222042896629094);
#1657=ELLIPSE('',#106077,0.239805882896672,0.222043378691442);
#1658=ELLIPSE('',#106099,0.599370913936996,0.555630771248784);
#1659=ELLIPSE('',#106100,0.599370291563568,0.555629413546736);
#1660=ELLIPSE('',#106102,0.239805889067455,0.22204364338699);
#1661=ELLIPSE('',#106103,0.239805704051744,0.222043163088029);
#1662=ELLIPSE('',#106105,0.239805697267273,0.222042896625362);
#1663=ELLIPSE('',#106106,0.239805882896202,0.22204337869045);
#1664=ELLIPSE('',#106128,0.599370913939066,0.555630771253014);
#1665=ELLIPSE('',#106129,0.599370291562359,0.555629413544269);
#1666=ELLIPSE('',#106131,0.239805889070273,0.222043643392718);
#1667=ELLIPSE('',#106132,0.239805704052602,0.222043163089835);
#1668=ELLIPSE('',#106134,0.239805697269778,0.222042896630685);
#1669=ELLIPSE('',#106135,0.239805882895276,0.222043378688557);
#1670=ELLIPSE('',#106157,0.599370913937787,0.555630771250463);
#1671=ELLIPSE('',#106158,0.599370291563937,0.555629413547465);
#1672=ELLIPSE('',#106160,0.23980588907131,0.222043643394858);
#1673=ELLIPSE('',#106161,0.239805704051925,0.222043163088452);
#1674=ELLIPSE('',#106163,0.239805697266862,0.222042896624485);
#1675=ELLIPSE('',#106164,0.239805882895514,0.222043378689123);
#1676=ELLIPSE('',#106186,0.599370913938338,0.555630771251542);
#1677=ELLIPSE('',#106187,0.599370291563512,0.555629413546666);
#1678=ELLIPSE('',#106189,0.239805889068806,0.222043643389686);
#1679=ELLIPSE('',#106190,0.239805704052207,0.222043163089033);
#1680=ELLIPSE('',#106192,0.239805697271128,0.222042896633369);
#1681=ELLIPSE('',#106193,0.239805882895001,0.222043378688052);
#1682=ELLIPSE('',#106215,0.599370913937752,0.555630771250446);
#1683=ELLIPSE('',#106216,0.599370291564464,0.555629413548618);
#1684=ELLIPSE('',#106218,0.239805889071983,0.222043643396124);
#1685=ELLIPSE('',#106219,0.239805704051923,0.222043163088459);
#1686=ELLIPSE('',#106221,0.239805697268376,0.222042896627738);
#1687=ELLIPSE('',#106222,0.23980588289422,0.222043378686507);
#1688=ELLIPSE('',#106244,0.599370913937345,0.555630771249436);
#1689=ELLIPSE('',#106245,0.59937029156196,0.555629413543465);
#1690=ELLIPSE('',#106247,0.239805889069961,0.222043643392058);
#1691=ELLIPSE('',#106248,0.239805704053478,0.222043163091603);
#1692=ELLIPSE('',#106250,0.239805697269098,0.22204289662929);
#1693=ELLIPSE('',#106251,0.2398058828958,0.22204337868961);
#1694=ELLIPSE('',#106273,0.599370913937037,0.555630771248897);
#1695=ELLIPSE('',#106274,0.599370291562031,0.555629413543674);
#1696=ELLIPSE('',#106276,0.239805889069035,0.22204364339024);
#1697=ELLIPSE('',#106277,0.239805704052574,0.222043163089708);
#1698=ELLIPSE('',#106279,0.239805697269961,0.222042896631028);
#1699=ELLIPSE('',#106280,0.23980588289584,0.222043378689655);
#1700=ELLIPSE('',#106302,0.599370913936974,0.555630771248813);
#1701=ELLIPSE('',#106303,0.599370291564014,0.555629413547602);
#1702=ELLIPSE('',#106305,0.239805889071759,0.222043643395731);
#1703=ELLIPSE('',#106306,0.239805704052857,0.22204316309031);
#1704=ELLIPSE('',#106308,0.239805697268703,0.222042896628388);
#1705=ELLIPSE('',#106309,0.23980588289455,0.222043378687117);
#1706=ELLIPSE('',#106331,0.599370913936989,0.55563077124864);
#1707=ELLIPSE('',#106332,0.599370291565194,0.555629413549919);
#1708=ELLIPSE('',#106334,0.239805889070791,0.222043643393766);
#1709=ELLIPSE('',#106335,0.239805704052858,0.22204316309034);
#1710=ELLIPSE('',#106337,0.239805697267834,0.222042896626616);
#1711=ELLIPSE('',#106338,0.239805882894524,0.222043378687112);
#1712=ELLIPSE('',#106360,0.599370913937548,0.555630771249916);
#1713=ELLIPSE('',#106361,0.599370291564909,0.555629413549445);
#1714=ELLIPSE('',#106363,0.239805889070836,0.222043643393712);
#1715=ELLIPSE('',#106364,0.239805704052287,0.222043163089176);
#1716=ELLIPSE('',#106366,0.239805697267837,0.222042896626536);
#1717=ELLIPSE('',#106367,0.239805882896042,0.222043378690122);
#1718=ELLIPSE('',#106389,0.599370913937273,0.555630771249356);
#1719=ELLIPSE('',#106390,0.599370291565437,0.555629413550552);
#1720=ELLIPSE('',#106392,0.239805889070935,0.222043643394021);
#1721=ELLIPSE('',#106393,0.239805704053519,0.222043163091695);
#1722=ELLIPSE('',#106395,0.239805697270266,0.222042896631555);
#1723=ELLIPSE('',#106396,0.239805882895611,0.222043378689254);
#1724=ELLIPSE('',#106418,0.599370913937078,0.555630771248908);
#1725=ELLIPSE('',#106419,0.599370291563712,0.555629413547031);
#1726=ELLIPSE('',#106421,0.239805889071625,0.222043643395324);
#1727=ELLIPSE('',#106422,0.239805704053465,0.222043163091574);
#1728=ELLIPSE('',#106424,0.239805697270216,0.222042896631521);
#1729=ELLIPSE('',#106425,0.239805882894735,0.222043378687381);
#1730=ELLIPSE('',#106447,0.59937091393725,0.555630771249377);
#1731=ELLIPSE('',#106448,0.599370291564746,0.55562941354917);
#1732=ELLIPSE('',#106450,0.239805889070006,0.222043643392107);
#1733=ELLIPSE('',#106451,0.239805704052258,0.222043163089137);
#1734=ELLIPSE('',#106453,0.239805697270427,0.222042896631951);
#1735=ELLIPSE('',#106454,0.239805882895842,0.22204337868974);
#1736=ELLIPSE('',#106476,0.599370913936956,0.555630771248539);
#1737=ELLIPSE('',#106477,0.599370291565833,0.555629413551388);
#1738=ELLIPSE('',#106479,0.239805889069105,0.222043643390322);
#1739=ELLIPSE('',#106480,0.239805704054033,0.222043163092783);
#1740=ELLIPSE('',#106482,0.239805697268147,0.222042896627119);
#1741=ELLIPSE('',#106483,0.239805882895254,0.222043378688474);
#1742=ELLIPSE('',#106505,0.599370913937186,0.555630771249278);
#1743=ELLIPSE('',#106506,0.59937029156173,0.555629413543073);
#1744=ELLIPSE('',#106508,0.239805889070897,0.222043643393939);
#1745=ELLIPSE('',#106509,0.239805704052673,0.222043163089943);
#1746=ELLIPSE('',#106511,0.239805697269764,0.222042896630456);
#1747=ELLIPSE('',#106512,0.239805882895431,0.222043378688825);
#1748=ELLIPSE('',#106534,0.59937091393695,0.555630771248692);
#1749=ELLIPSE('',#106535,0.599370291563103,0.555629413545827);
#1750=ELLIPSE('',#106537,0.239805889069582,0.222043643391203);
#1751=ELLIPSE('',#106538,0.239805704053097,0.22204316309083);
#1752=ELLIPSE('',#106540,0.239805697270417,0.222042896631992);
#1753=ELLIPSE('',#106541,0.239805882894859,0.222043378687672);
#1754=ELLIPSE('',#106563,0.599370913936272,0.555630771247367);
#1755=ELLIPSE('',#106564,0.599370291562787,0.555629413545066);
#1756=ELLIPSE('',#106566,0.239805889069898,0.222043643391812);
#1757=ELLIPSE('',#106567,0.239805704053116,0.222043163090822);
#1758=ELLIPSE('',#106569,0.23980569727021,0.222042896631462);
#1759=ELLIPSE('',#106570,0.239805882896488,0.222043378691088);
#1760=ELLIPSE('',#106592,0.599370913937577,0.555630771249974);
#1761=ELLIPSE('',#106593,0.599370291563603,0.555629413546849);
#1762=ELLIPSE('',#106595,0.239805889069516,0.222043643391181);
#1763=ELLIPSE('',#106596,0.239805704052191,0.222043163088941);
#1764=ELLIPSE('',#106598,0.239805697269283,0.222042896629651);
#1765=ELLIPSE('',#106599,0.239805882895395,0.222043378688882);
#1766=ELLIPSE('',#106621,0.599370913936449,0.555630771247687);
#1767=ELLIPSE('',#106622,0.599370291564252,0.555629413548182);
#1768=ELLIPSE('',#106624,0.239805889069627,0.222043643391383);
#1769=ELLIPSE('',#106625,0.23980570405205,0.22204316308868);
#1770=ELLIPSE('',#106627,0.239805697270006,0.22204289663112);
#1771=ELLIPSE('',#106628,0.239805882895028,0.222043378688055);
#1772=ELLIPSE('',#106653,0.599370913935561,0.55563077124596);
#1773=ELLIPSE('',#106654,0.599370291562403,0.555629413544383);
#1774=ELLIPSE('',#106656,0.239805889070797,0.222043643393652);
#1775=ELLIPSE('',#106657,0.23980570405278,0.222043163090117);
#1776=ELLIPSE('',#106659,0.239805697267951,0.222042896626835);
#1777=ELLIPSE('',#106660,0.239805882896207,0.222043378690511);
#1778=ELLIPSE('',#106665,0.472049204511299,0.428376857313292);
#1779=ELLIPSE('',#106666,0.472048618391423,0.428376332981108);
#1780=ELLIPSE('',#106667,0.354420976864826,0.321488380357502);
#1781=ELLIPSE('',#106668,0.354421121835649,0.321488565197775);
#1782=ELLIPSE('',#106670,0.472048618673416,0.428376333587049);
#1783=ELLIPSE('',#106671,0.472049204213287,0.428376856672832);
#1784=ELLIPSE('',#106672,0.354421145892816,0.321488604126673);
#1785=ELLIPSE('',#106673,0.354421089423499,0.321488612089889);
#1786=ELLIPSE('',#106677,0.146692861887334,0.127051669379536);
#1787=ELLIPSE('',#106689,0.146691465566744,0.127050784763687);
#1788=ELLIPSE('',#106706,0.146692861887626,0.127051669379765);
#1789=ELLIPSE('',#106717,0.146691465566936,0.127050784763915);
#1790=ELLIPSE('',#106724,0.47204920451043,0.42837685731154);
#1791=ELLIPSE('',#106725,0.472048618392884,0.428376332983992);
#1792=ELLIPSE('',#106726,0.354420976864662,0.321488380357232);
#1793=ELLIPSE('',#106727,0.354421121835341,0.321488565197164);
#1794=ELLIPSE('',#106729,0.472048618673052,0.428376333586304);
#1795=ELLIPSE('',#106730,0.472049204212421,0.428376856671127);
#1796=ELLIPSE('',#106731,0.354421145893183,0.321488604127369);
#1797=ELLIPSE('',#106732,0.354421089422911,0.321488612088706);
#1798=ELLIPSE('',#106737,0.472049204511464,0.428376857313639);
#1799=ELLIPSE('',#106738,0.472048618392123,0.428376332982553);
#1800=ELLIPSE('',#106739,0.354420976865553,0.321488380358974);
#1801=ELLIPSE('',#106740,0.354421121835029,0.321488565196566);
#1802=ELLIPSE('',#106742,0.472048618673971,0.42837633358811);
#1803=ELLIPSE('',#106743,0.472049204213955,0.428376856674181);
#1804=ELLIPSE('',#106744,0.354421145892627,0.321488604126292);
#1805=ELLIPSE('',#106745,0.354421089421795,0.321488612086537);
#1806=ELLIPSE('',#106750,0.47204920451058,0.428376857311775);
#1807=ELLIPSE('',#106751,0.472048618391896,0.428376332982026);
#1808=ELLIPSE('',#106752,0.354420976864346,0.321488380356575);
#1809=ELLIPSE('',#106753,0.354421121837741,0.321488565201974);
#1810=ELLIPSE('',#106755,0.472048618673973,0.428376333588145);
#1811=ELLIPSE('',#106756,0.472049204212974,0.428376856672254);
#1812=ELLIPSE('',#106757,0.354421145894067,0.321488604129196);
#1813=ELLIPSE('',#106758,0.354421089421142,0.321488612085148);
#1814=ELLIPSE('',#106763,0.472049204511116,0.42837685731288);
#1815=ELLIPSE('',#106764,0.472048618392269,0.428376332982734);
#1816=ELLIPSE('',#106765,0.354420976863336,0.321488380354612);
#1817=ELLIPSE('',#106766,0.354421121839405,0.321488565205236);
#1818=ELLIPSE('',#106768,0.472048618674185,0.428376333588625);
#1819=ELLIPSE('',#106769,0.472049204212207,0.428376856670675);
#1820=ELLIPSE('',#106770,0.354421145890722,0.321488604122502);
#1821=ELLIPSE('',#106771,0.354421089420675,0.321488612084178);
#1822=ELLIPSE('',#106776,0.472049204512402,0.428376857315463);
#1823=ELLIPSE('',#106777,0.47204861839104,0.428376332980329);
#1824=ELLIPSE('',#106778,0.354420976863445,0.321488380354816);
#1825=ELLIPSE('',#106779,0.354421121834752,0.321488565196016);
#1826=ELLIPSE('',#106781,0.472048618673901,0.428376333588);
#1827=ELLIPSE('',#106782,0.472049204214096,0.428376856674452);
#1828=ELLIPSE('',#106783,0.354421145894766,0.321488604130566);
#1829=ELLIPSE('',#106784,0.354421089421831,0.321488612086608);
#1830=ELLIPSE('',#106789,0.472049204510581,0.428376857311865);
#1831=ELLIPSE('',#106790,0.472048618391265,0.42837633298078);
#1832=ELLIPSE('',#106791,0.354420976864482,0.321488380356888);
#1833=ELLIPSE('',#106792,0.354421121837425,0.32148856520138);
#1834=ELLIPSE('',#106794,0.472048618673329,0.42837633358685);
#1835=ELLIPSE('',#106795,0.472049204213157,0.428376856672562);
#1836=ELLIPSE('',#106796,0.354421145894411,0.321488604129916);
#1837=ELLIPSE('',#106797,0.354421089422569,0.321488612087967);
#1838=ELLIPSE('',#106802,0.472049204510999,0.428376857312677);
#1839=ELLIPSE('',#106803,0.472048618392686,0.428376332983611);
#1840=ELLIPSE('',#106804,0.354420976865054,0.32148838035797);
#1841=ELLIPSE('',#106805,0.354421121835212,0.321488565196872);
#1842=ELLIPSE('',#106807,0.472048618672229,0.428376333584709);
#1843=ELLIPSE('',#106808,0.47204920421317,0.428376856672604);
#1844=ELLIPSE('',#106809,0.354421145893081,0.321488604127171);
#1845=ELLIPSE('',#106810,0.354421089422993,0.321488612088897);
#1846=ELLIPSE('',#106815,0.472049204511446,0.428376857313571);
#1847=ELLIPSE('',#106816,0.472048618393155,0.428376332984517);
#1848=ELLIPSE('',#106817,0.354420976864664,0.321488380357234);
#1849=ELLIPSE('',#106818,0.354421121834986,0.321488565196496);
#1850=ELLIPSE('',#106820,0.472048618673363,0.428376333586959);
#1851=ELLIPSE('',#106821,0.472049204211319,0.428376856668897);
#1852=ELLIPSE('',#106822,0.354421145892422,0.32148860412587);
#1853=ELLIPSE('',#106823,0.354421089420983,0.321488612084892);
#1854=ELLIPSE('',#106828,0.472049204511805,0.428376857314261);
#1855=ELLIPSE('',#106829,0.472048618392444,0.428376332983087);
#1856=ELLIPSE('',#106830,0.354420976864753,0.321488380357426);
#1857=ELLIPSE('',#106831,0.354421121834726,0.321488565195851);
#1858=ELLIPSE('',#106833,0.472048618672876,0.428376333585999);
#1859=ELLIPSE('',#106834,0.472049204213336,0.428376856672891);
#1860=ELLIPSE('',#106835,0.354421145892402,0.321488604125789);
#1861=ELLIPSE('',#106836,0.354421089422495,0.321488612087972);
#1862=ELLIPSE('',#106841,0.47204920451177,0.428376857314165);
#1863=ELLIPSE('',#106842,0.472048618392473,0.42837633298315);
#1864=ELLIPSE('',#106843,0.354420976864884,0.321488380357631);
#1865=ELLIPSE('',#106844,0.354421121836591,0.321488565199702);
#1866=ELLIPSE('',#106846,0.472048618674066,0.428376333588222);
#1867=ELLIPSE('',#106847,0.472049204213538,0.428376856673325);
#1868=ELLIPSE('',#106848,0.354421145892755,0.321488604126568);
#1869=ELLIPSE('',#106849,0.354421089419435,0.321488612081731);
#1870=ELLIPSE('',#106854,0.472049204511611,0.428376857313908);
#1871=ELLIPSE('',#106855,0.472048618391763,0.428376332981745);
#1872=ELLIPSE('',#106856,0.354420976865304,0.321488380358487);
#1873=ELLIPSE('',#106857,0.354421121837747,0.321488565201944);
#1874=ELLIPSE('',#106859,0.472048618672451,0.428376333585147);
#1875=ELLIPSE('',#106860,0.47204920421305,0.428376856672371);
#1876=ELLIPSE('',#106861,0.354421145893108,0.321488604127281);
#1877=ELLIPSE('',#106862,0.354421089420954,0.32148861208485);
#1878=ELLIPSE('',#106867,0.472049204509719,0.428376857310066);
#1879=ELLIPSE('',#106868,0.472048618392744,0.428376332983729);
#1880=ELLIPSE('',#106869,0.354420976866554,0.321488380361071);
#1881=ELLIPSE('',#106870,0.354421121835452,0.321488565197322);
#1882=ELLIPSE('',#106872,0.472048618672175,0.428376333584535);
#1883=ELLIPSE('',#106873,0.472049204213562,0.428376856673388);
#1884=ELLIPSE('',#106874,0.354421145891911,0.321488604124825);
#1885=ELLIPSE('',#106875,0.354421089423445,0.321488612089755);
#1886=ELLIPSE('',#106880,0.472049204511528,0.428376857313709);
#1887=ELLIPSE('',#106881,0.472048618393424,0.42837633298505);
#1888=ELLIPSE('',#106882,0.354420976866572,0.321488380361074);
#1889=ELLIPSE('',#106883,0.354421121834629,0.321488565195727);
#1890=ELLIPSE('',#106885,0.472048618671858,0.428376333583949);
#1891=ELLIPSE('',#106886,0.472049204212922,0.42837685667212);
#1892=ELLIPSE('',#106887,0.354421145894853,0.321488604130806);
#1893=ELLIPSE('',#106888,0.354421089421859,0.321488612086603);
#1894=ELLIPSE('',#106893,0.472049204510708,0.428376857312109);
#1895=ELLIPSE('',#106894,0.472048618392905,0.428376332983962);
#1896=ELLIPSE('',#106895,0.354420976864336,0.321488380356588);
#1897=ELLIPSE('',#106896,0.354421121837681,0.321488565201792);
#1898=ELLIPSE('',#106898,0.47204861867398,0.428376333588129);
#1899=ELLIPSE('',#106899,0.472049204212391,0.42837685667103);
#1900=ELLIPSE('',#106900,0.354421145891274,0.321488604123569);
#1901=ELLIPSE('',#106901,0.354421089422014,0.321488612086951);
#1902=ELLIPSE('',#106906,0.472049204509829,0.428376857310356);
#1903=ELLIPSE('',#106907,0.47204861839254,0.428376332983332);
#1904=ELLIPSE('',#106908,0.354420976864865,0.321488380357682);
#1905=ELLIPSE('',#106909,0.354421121834297,0.321488565195027);
#1906=ELLIPSE('',#106911,0.472048618674307,0.428376333588772);
#1907=ELLIPSE('',#106912,0.472049204212345,0.42837685667097);
#1908=ELLIPSE('',#106913,0.354421145891073,0.321488604123106);
#1909=ELLIPSE('',#106914,0.354421089421874,0.321488612086676);
#1910=ELLIPSE('',#106919,0.472049204509867,0.428376857310419);
#1911=ELLIPSE('',#106920,0.472048618391784,0.428376332981756);
#1912=ELLIPSE('',#106921,0.354420976863024,0.321488380353946);
#1913=ELLIPSE('',#106922,0.354421121836327,0.321488565199162);
#1914=ELLIPSE('',#106924,0.472048618674761,0.428376333589649);
#1915=ELLIPSE('',#106925,0.472049204213332,0.428376856672879);
#1916=ELLIPSE('',#106926,0.354421145895874,0.321488604132804);
#1917=ELLIPSE('',#106927,0.354421089422406,0.321488612087776);
#1918=ELLIPSE('',#106932,0.472049204510431,0.428376857311526);
#1919=ELLIPSE('',#106933,0.472048618392641,0.428376332983465);
#1920=ELLIPSE('',#106934,0.354420976866106,0.321488380360133);
#1921=ELLIPSE('',#106935,0.354421121836792,0.321488565199963);
#1922=ELLIPSE('',#106937,0.472048618673813,0.428376333587806);
#1923=ELLIPSE('',#106938,0.472049204213194,0.428376856672618);
#1924=ELLIPSE('',#106939,0.354421145892162,0.321488604125355);
#1925=ELLIPSE('',#106940,0.35442108942166,0.321488612086207);
#1926=ELLIPSE('',#106945,0.472049204510832,0.428376857312327);
#1927=ELLIPSE('',#106946,0.472048618391221,0.428376332980707);
#1928=ELLIPSE('',#106947,0.35442097686472,0.321488380357379);
#1929=ELLIPSE('',#106948,0.35442112183282,0.321488565192222);
#1930=ELLIPSE('',#106950,0.472048618672444,0.428376333585101);
#1931=ELLIPSE('',#106951,0.472049204212583,0.428376856671445);
#1932=ELLIPSE('',#106952,0.354421145893025,0.321488604127087);
#1933=ELLIPSE('',#106953,0.35442108942345,0.321488612089842);
#1934=ELLIPSE('',#106958,0.472049204511797,0.428376857314251);
#1935=ELLIPSE('',#106959,0.472048618392414,0.428376332983038);
#1936=ELLIPSE('',#106960,0.354420976864875,0.321488380357668);
#1937=ELLIPSE('',#106961,0.354421121834933,0.321488565196381);
#1938=ELLIPSE('',#106963,0.472048618671548,0.428376333583326);
#1939=ELLIPSE('',#106964,0.472049204213259,0.428376856672769);
#1940=ELLIPSE('',#106965,0.354421145891538,0.321488604124113);
#1941=ELLIPSE('',#106966,0.354421089423352,0.321488612089676);
#1942=ELLIPSE('',#106971,0.47204920451107,0.428376857312751);
#1943=ELLIPSE('',#106972,0.472048618390752,0.428376332979759);
#1944=ELLIPSE('',#106973,0.354420976865788,0.321488380359456);
#1945=ELLIPSE('',#106974,0.354421121838495,0.321488565203415);
#1946=ELLIPSE('',#106976,0.472048618672205,0.42837633358462);
#1947=ELLIPSE('',#106977,0.472049204213218,0.428376856672709);
#1948=ELLIPSE('',#106978,0.354421145888541,0.321488604118161);
#1949=ELLIPSE('',#106979,0.354421089422543,0.321488612087925);
#1950=ELLIPSE('',#106984,0.472049204511644,0.428376857313924);
#1951=ELLIPSE('',#106985,0.472048618391977,0.428376332982213);
#1952=ELLIPSE('',#106986,0.354420976865027,0.32148838035787);
#1953=ELLIPSE('',#106987,0.35442112183701,0.321488565200554);
#1954=ELLIPSE('',#106989,0.472048618674897,0.428376333589962);
#1955=ELLIPSE('',#106990,0.472049204212709,0.428376856671672);
#1956=ELLIPSE('',#106991,0.354421145893339,0.321488604127641);
#1957=ELLIPSE('',#106992,0.354421089420524,0.321488612084021);
#1958=ELLIPSE('',#106997,0.472049204511113,0.428376857312905);
#1959=ELLIPSE('',#106998,0.472048618391887,0.42837633298201);
#1960=ELLIPSE('',#106999,0.354420976864428,0.32148838035676);
#1961=ELLIPSE('',#107000,0.354421121836451,0.321488565199322);
#1962=ELLIPSE('',#107002,0.472048618673337,0.428376333586849);
#1963=ELLIPSE('',#107003,0.472049204213993,0.42837685667426);
#1964=ELLIPSE('',#107004,0.354421145891899,0.321488604124793);
#1965=ELLIPSE('',#107005,0.354421089420731,0.32148861208434);
#1966=ELLIPSE('',#107010,0.472049204511345,0.428376857313415);
#1967=ELLIPSE('',#107011,0.472048618393512,0.428376332985235);
#1968=ELLIPSE('',#107012,0.354420976865338,0.321488380358552);
#1969=ELLIPSE('',#107013,0.354421121834909,0.321488565196267);
#1970=ELLIPSE('',#107015,0.472048618673628,0.428376333587382);
#1971=ELLIPSE('',#107016,0.472049204212025,0.428376856670342);
#1972=ELLIPSE('',#107017,0.354421145891821,0.321488604124643);
#1973=ELLIPSE('',#107018,0.354421089423547,0.32148861209004);
#1974=ELLIPSE('',#107023,0.472049204511327,0.428376857313316);
#1975=ELLIPSE('',#107024,0.472048618392492,0.428376332983142);
#1976=ELLIPSE('',#107025,0.354420976864652,0.321488380357205);
#1977=ELLIPSE('',#107026,0.354421121836402,0.321488565199307);
#1978=ELLIPSE('',#107028,0.472048618674604,0.42837633358946);
#1979=ELLIPSE('',#107029,0.472049204212897,0.428376856672065);
#1980=ELLIPSE('',#107030,0.354421145891663,0.321488604124326);
#1981=ELLIPSE('',#107031,0.354421089422031,0.321488612086993);
#1982=ELLIPSE('',#107036,0.472049204509891,0.428376857310496);
#1983=ELLIPSE('',#107037,0.472048618391715,0.428376332981714);
#1984=ELLIPSE('',#107038,0.354420976865568,0.321488380359037);
#1985=ELLIPSE('',#107039,0.35442112183639,0.321488565199294);
#1986=ELLIPSE('',#107041,0.472048618673416,0.428376333587058);
#1987=ELLIPSE('',#107042,0.472049204212742,0.428376856671765);
#1988=ELLIPSE('',#107043,0.354421145896618,0.321488604134214);
#1989=ELLIPSE('',#107044,0.354421089421241,0.321488612085355);
#1990=ELLIPSE('',#107049,0.472049204511421,0.428376857313551);
#1991=ELLIPSE('',#107050,0.472048618392505,0.428376332983233);
#1992=ELLIPSE('',#107051,0.354420976863069,0.321488380353995);
#1993=ELLIPSE('',#107052,0.35442112183516,0.321488565196781);
#1994=ELLIPSE('',#107054,0.472048618673188,0.428376333586607);
#1995=ELLIPSE('',#107055,0.472049204213191,0.428376856672666);
#1996=ELLIPSE('',#107056,0.354421145891334,0.321488604123686);
#1997=ELLIPSE('',#107057,0.354421089420386,0.321488612083722);
#1998=ELLIPSE('',#107062,0.472049204510831,0.428376857312323);
#1999=ELLIPSE('',#107063,0.472048618392,0.428376332982215);
#2000=ELLIPSE('',#107064,0.354420976865575,0.32148838035904);
#2001=ELLIPSE('',#107065,0.354421121833158,0.321488565192756);
#2002=ELLIPSE('',#107067,0.472048618673296,0.428376333586792);
#2003=ELLIPSE('',#107068,0.472049204211677,0.428376856669657);
#2004=ELLIPSE('',#107069,0.354421145893456,0.321488604128007);
#2005=ELLIPSE('',#107070,0.354421089420597,0.321488612084059);
#2006=ELLIPSE('',#107075,0.472049204510519,0.428376857311711);
#2007=ELLIPSE('',#107076,0.472048618393586,0.428376332985414);
#2008=ELLIPSE('',#107077,0.354420976863066,0.321488380354067);
#2009=ELLIPSE('',#107078,0.3544211218372,0.321488565200811);
#2010=ELLIPSE('',#107080,0.472048618673438,0.428376333587092);
#2011=ELLIPSE('',#107081,0.472049204211534,0.428376856669341);
#2012=ELLIPSE('',#107082,0.354421145896177,0.321488604133354);
#2013=ELLIPSE('',#107083,0.354421089423546,0.321488612089943);
#2014=ELLIPSE('',#107088,0.472049204511482,0.428376857313627);
#2015=ELLIPSE('',#107089,0.472048618392421,0.428376332983089);
#2016=ELLIPSE('',#107090,0.354420976866456,0.321488380360847);
#2017=ELLIPSE('',#107091,0.354421121834971,0.32148856519634);
#2018=ELLIPSE('',#107093,0.47204861867389,0.428376333587944);
#2019=ELLIPSE('',#107094,0.472049204213437,0.4283768566731);
#2020=ELLIPSE('',#107095,0.35442114589374,0.321488604128488);
#2021=ELLIPSE('',#107096,0.354421089423662,0.321488612090211);
#2022=ELLIPSE('',#107099,0.472049204511149,0.428376857312952);
#2023=ELLIPSE('',#107100,0.472048618391616,0.428376332981492);
#2024=ELLIPSE('',#107101,0.354420976863965,0.321488380355734);
#2025=ELLIPSE('',#107102,0.354421121839368,0.3214885652052);
#2026=ELLIPSE('',#107104,0.472048618673971,0.428376333588171);
#2027=ELLIPSE('',#107105,0.472049204213616,0.428376856673503);
#2028=ELLIPSE('',#107106,0.354421145894116,0.321488604129308);
#2029=ELLIPSE('',#107107,0.354421089421021,0.321488612084896);
#2030=ELLIPSE('',#107112,0.472049204511451,0.428376857313542);
#2031=ELLIPSE('',#107113,0.472048618392002,0.428376332982204);
#2032=ELLIPSE('',#107114,0.354420976865778,0.32148838035945);
#2033=ELLIPSE('',#107115,0.354421121835973,0.321488565198471);
#2034=ELLIPSE('',#107117,0.472048618674194,0.428376333588553);
#2035=ELLIPSE('',#107118,0.472049204212065,0.428376856670387);
#2036=ELLIPSE('',#107119,0.354421145894391,0.321488604129854);
#2037=ELLIPSE('',#107120,0.354421089422029,0.321488612087025);
#2038=ELLIPSE('',#107125,0.472049204511657,0.428376857313933);
#2039=ELLIPSE('',#107126,0.472048618391513,0.428376332981293);
#2040=ELLIPSE('',#107127,0.354420976864311,0.321488380356496);
#2041=ELLIPSE('',#107128,0.354421121837407,0.321488565201336);
#2042=ELLIPSE('',#107130,0.472048618672929,0.42837633358606);
#2043=ELLIPSE('',#107131,0.472049204212117,0.428376856670511);
#2044=ELLIPSE('',#107132,0.354421145894905,0.321488604130814);
#2045=ELLIPSE('',#107133,0.354421089422112,0.321488612087143);
#2046=ELLIPSE('',#107138,0.472049204511992,0.428376857314651);
#2047=ELLIPSE('',#107139,0.472048618392913,0.428376332984082);
#2048=ELLIPSE('',#107140,0.354420976865269,0.321488380358449);
#2049=ELLIPSE('',#107141,0.354421121834688,0.321488565195839);
#2050=ELLIPSE('',#107143,0.472048618673509,0.428376333587237);
#2051=ELLIPSE('',#107144,0.472049204213274,0.428376856672824);
#2052=ELLIPSE('',#107145,0.354421145892845,0.321488604126746);
#2053=ELLIPSE('',#107146,0.354421089425724,0.321488612094367);
#2054=ELLIPSE('',#107151,0.472049204511633,0.428376857313873);
#2055=ELLIPSE('',#107152,0.472048618392605,0.428376332983422);
#2056=ELLIPSE('',#107153,0.354420976864453,0.321488380356726);
#2057=ELLIPSE('',#107154,0.354421121832141,0.321488565190751);
#2058=ELLIPSE('',#107156,0.472048618673539,0.428376333587287);
#2059=ELLIPSE('',#107157,0.472049204213293,0.428376856672817);
#2060=ELLIPSE('',#107158,0.354421145894062,0.321488604129175);
#2061=ELLIPSE('',#107159,0.354421089419115,0.321488612081158);
#2062=ELLIPSE('',#107164,0.472049204511243,0.428376857313128);
#2063=ELLIPSE('',#107165,0.472048618391538,0.428376332981319);
#2064=ELLIPSE('',#107166,0.354420976864454,0.3214883803568);
#2065=ELLIPSE('',#107167,0.354421121833766,0.321488565193981);
#2066=ELLIPSE('',#107169,0.47204861867417,0.428376333588541);
#2067=ELLIPSE('',#107170,0.472049204213016,0.428376856672282);
#2068=ELLIPSE('',#107171,0.354421145891356,0.321488604123696);
#2069=ELLIPSE('',#107172,0.354421089423352,0.321488612089603);
#2070=ELLIPSE('',#107177,0.47204920451092,0.428376857312493);
#2071=ELLIPSE('',#107178,0.472048618392258,0.428376332982749);
#2072=ELLIPSE('',#107179,0.354420976865082,0.321488380358088);
#2073=ELLIPSE('',#107180,0.354421121835669,0.321488565197869);
#2074=ELLIPSE('',#107182,0.472048618673151,0.428376333586468);
#2075=ELLIPSE('',#107183,0.472049204211844,0.428376856669944);
#2076=ELLIPSE('',#107184,0.354421145894343,0.321488604129742);
#2077=ELLIPSE('',#107185,0.354421089422269,0.321488612087402);
#2078=ELLIPSE('',#107190,0.472049204508892,0.428376857308545);
#2079=ELLIPSE('',#107191,0.472048618392121,0.42837633298247);
#2080=ELLIPSE('',#107192,0.354420976863941,0.321488380355759);
#2081=ELLIPSE('',#107193,0.354421121837472,0.32148856520146);
#2082=ELLIPSE('',#107195,0.472048618672543,0.428376333585301);
#2083=ELLIPSE('',#107196,0.472049204213821,0.428376856673893);
#2084=ELLIPSE('',#107197,0.35442114589205,0.321488604125153);
#2085=ELLIPSE('',#107198,0.354421089420019,0.321488612082947);
#2086=ELLIPSE('',#107203,0.472049204511413,0.42837685731347);
#2087=ELLIPSE('',#107204,0.472048618392691,0.428376332983646);
#2088=ELLIPSE('',#107205,0.354420976864115,0.321488380356169);
#2089=ELLIPSE('',#107206,0.354421121832944,0.321488565192392);
#2090=ELLIPSE('',#107208,0.472048618674026,0.428376333588235);
#2091=ELLIPSE('',#107209,0.472049204212005,0.428376856670295);
#2092=ELLIPSE('',#107210,0.354421145892444,0.321488604125956);
#2093=ELLIPSE('',#107211,0.35442108942116,0.321488612085219);
#2094=ELLIPSE('',#107216,0.47204920450981,0.428376857310287);
#2095=ELLIPSE('',#107217,0.472048618392289,0.428376332982821);
#2096=ELLIPSE('',#107218,0.354420976862782,0.321488380353437);
#2097=ELLIPSE('',#107219,0.354421121836506,0.321488565199431);
#2098=ELLIPSE('',#107221,0.472048618672653,0.42837633358548);
#2099=ELLIPSE('',#107222,0.472049204213736,0.428376856673694);
#2100=ELLIPSE('',#107223,0.354421145890053,0.321488604121152);
#2101=ELLIPSE('',#107224,0.354421089423222,0.321488612089361);
#2102=ELLIPSE('',#107229,0.472049204509417,0.428376857309544);
#2103=ELLIPSE('',#107230,0.472048618391604,0.428376332981422);
#2104=ELLIPSE('',#107231,0.354420976862723,0.321488380353292);
#2105=ELLIPSE('',#107232,0.354421121837083,0.32148856520067);
#2106=ELLIPSE('',#107234,0.47204861867469,0.428376333589523);
#2107=ELLIPSE('',#107235,0.47204920421263,0.428376856671494);
#2108=ELLIPSE('',#107236,0.354421145893487,0.321488604127993);
#2109=ELLIPSE('',#107237,0.354421089421634,0.321488612086208);
#2110=ELLIPSE('',#107242,0.47204920450963,0.428376857309992);
#2111=ELLIPSE('',#107243,0.472048618392772,0.428376332983745);
#2112=ELLIPSE('',#107244,0.354420976863782,0.321488380355444);
#2113=ELLIPSE('',#107245,0.354421121836615,0.321488565199704);
#2114=ELLIPSE('',#107247,0.47204861867308,0.428376333586376);
#2115=ELLIPSE('',#107248,0.472049204212482,0.428376856671214);
#2116=ELLIPSE('',#107249,0.354421145892683,0.321488604126402);
#2117=ELLIPSE('',#107250,0.35442108942268,0.321488612088291);
#2118=ELLIPSE('',#107255,0.472049204510717,0.428376857312061);
#2119=ELLIPSE('',#107256,0.472048618391451,0.428376332981167);
#2120=ELLIPSE('',#107257,0.354420976866113,0.321488380360137);
#2121=ELLIPSE('',#107258,0.354421121835235,0.321488565196901);
#2122=ELLIPSE('',#107260,0.4720486186743,0.428376333588738);
#2123=ELLIPSE('',#107261,0.472049204212938,0.428376856672103);
#2124=ELLIPSE('',#107262,0.354421145893203,0.321488604127511);
#2125=ELLIPSE('',#107263,0.354421089424015,0.321488612090953);
#2126=ELLIPSE('',#107268,0.472049204511672,0.428376857313994);
#2127=ELLIPSE('',#107269,0.472048618392936,0.428376332984117);
#2128=ELLIPSE('',#107270,0.354420976863078,0.321488380353981);
#2129=ELLIPSE('',#107271,0.354421121835837,0.321488565198135);
#2130=ELLIPSE('',#107273,0.4720486186744,0.428376333588985);
#2131=ELLIPSE('',#107274,0.472049204212671,0.428376856671578);
#2132=ELLIPSE('',#107275,0.354421145894098,0.321488604129234);
#2133=ELLIPSE('',#107276,0.354421089421883,0.321488612086657);
#2134=ELLIPSE('',#107281,0.472049204510614,0.428376857311898);
#2135=ELLIPSE('',#107282,0.472048618393337,0.428376332984887);
#2136=ELLIPSE('',#107283,0.354420976865991,0.321488380359936);
#2137=ELLIPSE('',#107284,0.354421121835589,0.321488565197568);
#2138=ELLIPSE('',#107286,0.472048618674229,0.428376333588641);
#2139=ELLIPSE('',#107287,0.472049204213025,0.42837685667231);
#2140=ELLIPSE('',#107288,0.35442114589626,0.321488604133465);
#2141=ELLIPSE('',#107289,0.35442108942249,0.321488612087879);
#2142=ELLIPSE('',#107292,0.472049204511229,0.428376857313123);
#2143=ELLIPSE('',#107293,0.47204861839257,0.428376332983376);
#2144=ELLIPSE('',#107294,0.354420976864408,0.321488380356651);
#2145=ELLIPSE('',#107295,0.354421121838439,0.321488565203349);
#2146=ELLIPSE('',#107297,0.472048618674394,0.428376333588988);
#2147=ELLIPSE('',#107298,0.472049204213168,0.428376856672599);
#2148=ELLIPSE('',#107299,0.354421145893815,0.321488604128643);
#2149=ELLIPSE('',#107300,0.354421089424289,0.321488612091436);
#2150=ELLIPSE('',#107305,0.472049204513252,0.42837685731712);
#2151=ELLIPSE('',#107306,0.472048618392165,0.428376332982546);
#2152=ELLIPSE('',#107307,0.35442097686289,0.321488380353694);
#2153=ELLIPSE('',#107308,0.354421121835997,0.321488565198458);
#2154=ELLIPSE('',#107310,0.472048618674151,0.428376333588511);
#2155=ELLIPSE('',#107311,0.472049204211785,0.428376856669885);
#2156=ELLIPSE('',#107312,0.354421145894632,0.321488604130297);
#2157=ELLIPSE('',#107313,0.354421089422824,0.321488612088477);
#2158=ELLIPSE('',#107318,0.472049204511394,0.428376857313407);
#2159=ELLIPSE('',#107319,0.472048618391184,0.428376332980646);
#2160=ELLIPSE('',#107320,0.354420976864394,0.32148838035678);
#2161=ELLIPSE('',#107321,0.354421121834998,0.321488565196511);
#2162=ELLIPSE('',#107323,0.472048618674661,0.428376333589502);
#2163=ELLIPSE('',#107324,0.472049204212487,0.428376856671257);
#2164=ELLIPSE('',#107325,0.354421145891117,0.321488604123307);
#2165=ELLIPSE('',#107326,0.354421089423795,0.321488612090472);
#2166=ELLIPSE('',#107331,0.472049204510894,0.428376857312474);
#2167=ELLIPSE('',#107332,0.472048618391186,0.428376332980609);
#2168=ELLIPSE('',#107333,0.354420976865725,0.321488380359322);
#2169=ELLIPSE('',#107334,0.354421121834588,0.321488565195654);
#2170=ELLIPSE('',#107336,0.472048618673108,0.428376333586399);
#2171=ELLIPSE('',#107337,0.472049204212361,0.428376856671049);
#2172=ELLIPSE('',#107338,0.354421145893163,0.321488604127362);
#2173=ELLIPSE('',#107339,0.354421089423452,0.321488612089836);
#2174=ELLIPSE('',#107344,0.472049204511179,0.428376857313092);
#2175=ELLIPSE('',#107345,0.472048618392961,0.42837633298412);
#2176=ELLIPSE('',#107346,0.354420976863802,0.321488380355433);
#2177=ELLIPSE('',#107347,0.354421121837851,0.321488565202186);
#2178=ELLIPSE('',#107349,0.472048618671871,0.428376333583965);
#2179=ELLIPSE('',#107350,0.472049204211579,0.428376856669446);
#2180=ELLIPSE('',#107351,0.35442114589121,0.32148860412345);
#2181=ELLIPSE('',#107352,0.354421089421435,0.321488612085847);
#2182=ELLIPSE('',#107357,0.472049204511322,0.428376857313307);
#2183=ELLIPSE('',#107358,0.472048618391922,0.428376332982069);
#2184=ELLIPSE('',#107359,0.354420976865897,0.321488380359689);
#2185=ELLIPSE('',#107360,0.35442112183738,0.321488565201278);
#2186=ELLIPSE('',#107362,0.472048618674387,0.428376333588996);
#2187=ELLIPSE('',#107363,0.472049204212476,0.428376856671206);
#2188=ELLIPSE('',#107364,0.354421145894326,0.321488604129683);
#2189=ELLIPSE('',#107365,0.3544210894222,0.321488612087341);
#2190=ELLIPSE('',#107370,0.472049204510946,0.428376857312566);
#2191=ELLIPSE('',#107371,0.472048618391712,0.428376332981558);
#2192=ELLIPSE('',#107372,0.354420976866645,0.321488380361217);
#2193=ELLIPSE('',#107373,0.354421121838504,0.321488565203492);
#2194=ELLIPSE('',#107375,0.472048618673501,0.428376333587255);
#2195=ELLIPSE('',#107376,0.472049204212708,0.428376856671664);
#2196=ELLIPSE('',#107377,0.35442114589414,0.321488604129325);
#2197=ELLIPSE('',#107378,0.354421089422287,0.321488612087437);
#2198=ELLIPSE('',#107383,0.472049204511479,0.42837685731363);
#2199=ELLIPSE('',#107384,0.472048618391853,0.428376332981929);
#2200=ELLIPSE('',#107385,0.354420976866264,0.321488380360526);
#2201=ELLIPSE('',#107386,0.354421121836331,0.321488565199092);
#2202=ELLIPSE('',#107388,0.472048618675346,0.428376333590846);
#2203=ELLIPSE('',#107389,0.47204920421198,0.428376856670232);
#2204=ELLIPSE('',#107390,0.354421145889929,0.321488604120882);
#2205=ELLIPSE('',#107391,0.354421089421345,0.321488612085622);
#2206=ELLIPSE('',#107396,0.472049204509595,0.428376857309901);
#2207=ELLIPSE('',#107397,0.472048618392921,0.428376332984105);
#2208=ELLIPSE('',#107398,0.35442097686446,0.321488380356807);
#2209=ELLIPSE('',#107399,0.35442112183345,0.32148856519335);
#2210=ELLIPSE('',#107401,0.472048618672761,0.428376333585721);
#2211=ELLIPSE('',#107402,0.472049204211995,0.428376856670272);
#2212=ELLIPSE('',#107403,0.354421145890888,0.321488604122831);
#2213=ELLIPSE('',#107404,0.354421089421532,0.321488612085962);
#2214=ELLIPSE('',#107409,0.472049204511288,0.428376857313216);
#2215=ELLIPSE('',#107410,0.472048618391648,0.428376332981492);
#2216=ELLIPSE('',#107411,0.354420976864546,0.321488380357008);
#2217=ELLIPSE('',#107412,0.354421121836294,0.321488565198935);
#2218=ELLIPSE('',#107414,0.472048618674408,0.428376333588983);
#2219=ELLIPSE('',#107415,0.472049204211926,0.428376856670145);
#2220=ELLIPSE('',#107416,0.354421145893214,0.321488604127459);
#2221=ELLIPSE('',#107417,0.354421089423539,0.321488612089965);
#2222=ELLIPSE('',#107422,0.472049204510058,0.428376857310839);
#2223=ELLIPSE('',#107423,0.472048618393402,0.428376332984991);
#2224=ELLIPSE('',#107424,0.354420976865732,0.321488380359386);
#2225=ELLIPSE('',#107425,0.354421121836976,0.321488565200376);
#2226=ELLIPSE('',#107427,0.472048618673465,0.428376333587143);
#2227=ELLIPSE('',#107428,0.472049204213126,0.428376856672526);
#2228=ELLIPSE('',#107429,0.354421145890888,0.321488604122835);
#2229=ELLIPSE('',#107430,0.354421089422305,0.321488612087484);
#2230=ELLIPSE('',#107435,0.472049204511117,0.428376857312922);
#2231=ELLIPSE('',#107436,0.47204861839179,0.428376332981839);
#2232=ELLIPSE('',#107437,0.35442097686677,0.321488380361499);
#2233=ELLIPSE('',#107438,0.354421121836319,0.321488565199035);
#2234=ELLIPSE('',#107440,0.472048618674479,0.428376333589128);
#2235=ELLIPSE('',#107441,0.47204920421329,0.428376856672826);
#2236=ELLIPSE('',#107442,0.354421145894268,0.321488604129596);
#2237=ELLIPSE('',#107443,0.354421089422428,0.321488612087792);
#2238=ELLIPSE('',#107448,0.472049204510683,0.428376857312038);
#2239=ELLIPSE('',#107449,0.472048618393508,0.428376332985237);
#2240=ELLIPSE('',#107450,0.354420976865022,0.32148838035803);
#2241=ELLIPSE('',#107451,0.354421121835537,0.321488565197519);
#2242=ELLIPSE('',#107453,0.472048618673479,0.428376333587187);
#2243=ELLIPSE('',#107454,0.472049204211936,0.428376856670164);
#2244=ELLIPSE('',#107455,0.354421145892554,0.321488604126193);
#2245=ELLIPSE('',#107456,0.354421089420411,0.3214886120837);
#2246=ELLIPSE('',#107461,0.472049204511685,0.428376857314037);
#2247=ELLIPSE('',#107462,0.47204861839225,0.428376332982777);
#2248=ELLIPSE('',#107463,0.354420976864416,0.321488380356758);
#2249=ELLIPSE('',#107464,0.354421121837932,0.321488565202383);
#2250=ELLIPSE('',#107466,0.472048618673388,0.428376333586979);
#2251=ELLIPSE('',#107467,0.472049204211487,0.42837685666926);
#2252=ELLIPSE('',#107468,0.354421145894157,0.32148860412932);
#2253=ELLIPSE('',#107469,0.354421089422988,0.321488612088863);
#2254=ELLIPSE('',#107474,0.472049204510669,0.428376857312049);
#2255=ELLIPSE('',#107475,0.472048618393432,0.428376332985066);
#2256=ELLIPSE('',#107476,0.354420976864168,0.321488380356288);
#2257=ELLIPSE('',#107477,0.354421121837713,0.321488565201861);
#2258=ELLIPSE('',#107479,0.472048618673566,0.428376333587318);
#2259=ELLIPSE('',#107480,0.472049204212713,0.428376856671703);
#2260=ELLIPSE('',#107481,0.354421145892746,0.32148860412653);
#2261=ELLIPSE('',#107482,0.354421089422267,0.321488612087543);
#2262=ELLIPSE('',#107602,0.146692861885778,0.127051669378566);
#2263=ELLIPSE('',#107614,0.146691465566803,0.127050784763753);
#2264=ELLIPSE('',#107631,0.146692861886413,0.127051669378057);
#2265=ELLIPSE('',#107642,0.14669146556691,0.12705078476387);
#2266=ELLIPSE('',#107646,0.146692861887922,0.127051669380119);
#2267=ELLIPSE('',#107658,0.14669146556702,0.127050784764041);
#2268=ELLIPSE('',#107675,0.146692861887039,0.127051669380184);
#2269=ELLIPSE('',#107686,0.146691465566734,0.12705078476371);
#2270=ELLIPSE('',#107690,0.146692861889571,0.127051669380672);
#2271=ELLIPSE('',#107702,0.146691465567211,0.127050784764187);
#2272=ELLIPSE('',#107719,0.146692861887923,0.127051669379853);
#2273=ELLIPSE('',#107730,0.146691465566873,0.127050784763828);
#2274=ELLIPSE('',#107734,0.146692861885695,0.127051669378166);
#2275=ELLIPSE('',#107746,0.146691465566617,0.127050784763644);
#2276=ELLIPSE('',#107763,0.146692861890006,0.12705166938115);
#2277=ELLIPSE('',#107774,0.146691465566989,0.127050784763962);
#2278=ELLIPSE('',#107778,0.146692861886538,0.127051669378574);
#2279=ELLIPSE('',#107790,0.146691465566865,0.127050784763831);
#2280=ELLIPSE('',#107807,0.146692861888534,0.127051669379887);
#2281=ELLIPSE('',#107818,0.14669146556704,0.127050784763975);
#2282=ELLIPSE('',#107822,0.14669286189017,0.127051669381253);
#2283=ELLIPSE('',#107834,0.146691465566333,0.127050784763404);
#2284=ELLIPSE('',#107851,0.146692861888775,0.127051669381276);
#2285=ELLIPSE('',#107862,0.146691465566996,0.127050784763966);
#2286=ELLIPSE('',#107866,0.146692861889956,0.127051669380713);
#2287=ELLIPSE('',#107878,0.146691465567727,0.127050784764622);
#2288=ELLIPSE('',#107895,0.146692861890152,0.127051669381072);
#2289=ELLIPSE('',#107906,0.146691465566229,0.127050784763335);
#2290=ELLIPSE('',#107910,0.146692861889335,0.127051669380942);
#2291=ELLIPSE('',#107922,0.146691465567614,0.127050784764493);
#2292=ELLIPSE('',#107939,0.146692861888875,0.127051669380474);
#2293=ELLIPSE('',#107950,0.146691465567108,0.127050784764015);
#2294=ELLIPSE('',#107954,0.146692861889473,0.127051669380558);
#2295=ELLIPSE('',#107966,0.146691465566935,0.127050784763893);
#2296=ELLIPSE('',#107983,0.146692861888244,0.127051669380723);
#2297=ELLIPSE('',#107994,0.14669146556749,0.127050784764377);
#2298=ELLIPSE('',#107998,0.14669286188738,0.12705166938026);
#2299=ELLIPSE('',#108010,0.146691465566891,0.127050784763883);
#2300=ELLIPSE('',#108027,0.1466928618908,0.127051669382332);
#2301=ELLIPSE('',#108038,0.146691465566753,0.127050784763768);
#2302=ELLIPSE('',#108042,0.146692861886957,0.127051669379919);
#2303=ELLIPSE('',#108054,0.146691465566667,0.127050784763711);
#2304=ELLIPSE('',#108071,0.146692861884917,0.127051669378417);
#2305=ELLIPSE('',#108082,0.146691465566951,0.127050784763875);
#2306=ELLIPSE('',#108086,0.146692861887784,0.127051669379951);
#2307=ELLIPSE('',#108098,0.146691465566662,0.127050784763678);
#2308=ELLIPSE('',#108115,0.146692861892035,0.127051669382384);
#2309=ELLIPSE('',#108126,0.146691465567551,0.127050784764446);
#2310=ELLIPSE('',#108130,0.146692861887898,0.127051669378866);
#2311=ELLIPSE('',#108142,0.146691465567286,0.127050784764234);
#2312=ELLIPSE('',#108159,0.146692861889581,0.127051669381123);
#2313=ELLIPSE('',#108170,0.146691465566912,0.127050784763782);
#2314=ELLIPSE('',#108174,0.146692861886619,0.127051669379193);
#2315=ELLIPSE('',#108186,0.146691465566984,0.127050784763962);
#2316=ELLIPSE('',#108203,0.14669286188925,0.127051669380939);
#2317=ELLIPSE('',#108214,0.146691465567033,0.127050784764007);
#2318=ELLIPSE('',#108218,0.146692861889623,0.127051669381043);
#2319=ELLIPSE('',#108230,0.14669146556684,0.127050784763757);
#2320=ELLIPSE('',#108247,0.146692861888148,0.127051669379703);
#2321=ELLIPSE('',#108258,0.146691465566664,0.127050784763589);
#2322=ELLIPSE('',#108262,0.146692861888369,0.127051669379955);
#2323=ELLIPSE('',#108274,0.146691465566977,0.127050784763914);
#2324=ELLIPSE('',#108291,0.146692861889199,0.127051669380361);
#2325=ELLIPSE('',#108302,0.146691465567016,0.127050784763939);
#2326=ELLIPSE('',#108306,0.146692861888996,0.127051669380984);
#2327=ELLIPSE('',#108318,0.146691465567128,0.127050784764104);
#2328=ELLIPSE('',#108335,0.146692861888997,0.127051669381534);
#2329=ELLIPSE('',#108346,0.146691465567221,0.127050784764197);
#2330=ELLIPSE('',#108350,0.146692861885338,0.12705166937903);
#2331=ELLIPSE('',#108362,0.146691465566555,0.127050784763588);
#2332=ELLIPSE('',#108379,0.146692861886485,0.127051669379774);
#2333=ELLIPSE('',#108390,0.146691465567292,0.127050784764165);
#2334=ELLIPSE('',#108394,0.146692861889409,0.12705166938008);
#2335=ELLIPSE('',#108406,0.146691465567198,0.127050784764133);
#2336=ELLIPSE('',#108423,0.146692861888131,0.127051669379491);
#2337=ELLIPSE('',#108434,0.146691465567096,0.127050784764072);
#2338=ELLIPSE('',#108438,0.146692861890808,0.127051669382308);
#2339=ELLIPSE('',#108450,0.146691465566607,0.127050784763588);
#2340=ELLIPSE('',#108467,0.146692861888626,0.127051669381254);
#2341=ELLIPSE('',#108478,0.1466914655668,0.127050784763833);
#2342=ELLIPSE('',#108482,0.146692861887797,0.127051669379309);
#2343=ELLIPSE('',#108494,0.146691465567039,0.127050784763956);
#2344=ELLIPSE('',#108511,0.146692861888548,0.127051669380616);
#2345=ELLIPSE('',#108522,0.146691465567481,0.127050784764359);
#2346=ELLIPSE('',#108526,0.146692861889464,0.127051669380601);
#2347=ELLIPSE('',#108538,0.146691465567513,0.12705078476439);
#2348=ELLIPSE('',#108555,0.146692861889216,0.127051669380696);
#2349=ELLIPSE('',#108566,0.146691465566864,0.127050784763858);
#2350=ELLIPSE('',#108570,0.146692861885317,0.127051669379159);
#2351=ELLIPSE('',#108582,0.146691465566895,0.127050784763869);
#2352=ELLIPSE('',#108599,0.146692861887918,0.127051669380084);
#2353=ELLIPSE('',#108610,0.146691465568625,0.127050784765417);
#2354=ELLIPSE('',#108614,0.146692861887782,0.127051669379891);
#2355=ELLIPSE('',#108626,0.146691465567337,0.127050784764302);
#2356=ELLIPSE('',#108643,0.146692861890565,0.127051669381493);
#2357=ELLIPSE('',#108654,0.146691465567523,0.127050784764429);
#2358=ELLIPSE('',#108658,0.146692861890385,0.127051669380385);
#2359=ELLIPSE('',#108670,0.14669146556753,0.127050784764438);
#2360=ELLIPSE('',#108687,0.146692861885322,0.127051669378044);
#2361=ELLIPSE('',#108698,0.146691465567394,0.127050784764246);
#2362=ELLIPSE('',#108702,0.146692861888362,0.127051669380383);
#2363=ELLIPSE('',#108714,0.146691465566958,0.127050784763904);
#2364=ELLIPSE('',#108731,0.146692861887648,0.12705166938048);
#2365=ELLIPSE('',#108742,0.146691465567457,0.127050784764309);
#2366=ELLIPSE('',#108746,0.14669286188913,0.127051669379752);
#2367=ELLIPSE('',#108758,0.146691465567296,0.127050784764243);
#2368=ELLIPSE('',#108775,0.146692861888268,0.127051669379853);
#2369=ELLIPSE('',#108786,0.146691465567949,0.127050784764882);
#2370=ELLIPSE('',#108790,0.146692861887034,0.12705166937996);
#2371=ELLIPSE('',#108802,0.146691465566988,0.127050784763918);
#2372=ELLIPSE('',#108819,0.14669286188752,0.127051669380341);
#2373=ELLIPSE('',#108830,0.146691465567924,0.12705078476488);
#2374=ELLIPSE('',#108834,0.146692861887905,0.127051669379344);
#2375=ELLIPSE('',#108846,0.146691465566944,0.127050784763925);
#2376=ELLIPSE('',#108863,0.146692861887371,0.127051669379764);
#2377=ELLIPSE('',#108874,0.146691465566594,0.127050784763522);
#2378=ELLIPSE('',#108878,0.146692861889815,0.127051669381089);
#2379=ELLIPSE('',#108890,0.146691465567249,0.12705078476415);
#2380=ELLIPSE('',#108901,0.146692861890005,0.127051669381267);
#2381=ELLIPSE('',#108912,0.146691465567655,0.12705078476452);
#2382=ELLIPSE('',#108916,0.1466928618887,0.127051669381071);
#2383=ELLIPSE('',#108928,0.146691465566767,0.127050784763724);
#2384=ELLIPSE('',#108945,0.146692861888402,0.127051669379751);
#2385=ELLIPSE('',#108956,0.146691465567649,0.127050784764565);
#2386=ELLIPSE('',#108960,0.146692861888125,0.127051669380703);
#2387=ELLIPSE('',#108972,0.146691465567162,0.127050784764084);
#2388=ELLIPSE('',#108989,0.146692861887572,0.127051669379447);
#2389=ELLIPSE('',#109000,0.146691465566936,0.127050784763924);
#2390=ELLIPSE('',#109004,0.146692861886526,0.127051669379105);
#2391=ELLIPSE('',#109016,0.146691465567167,0.127050784764051);
#2392=ELLIPSE('',#109033,0.146692861888572,0.127051669380327);
#2393=ELLIPSE('',#109044,0.146691465567357,0.127050784764316);
#2394=ELLIPSE('',#109048,0.146692861887322,0.127051669379629);
#2395=ELLIPSE('',#109060,0.146691465567351,0.127050784764243);
#2396=ELLIPSE('',#109077,0.146692861887703,0.127051669380563);
#2397=ELLIPSE('',#109088,0.146691465566607,0.127050784763618);
#2398=ELLIPSE('',#109092,0.146692861885829,0.127051669379383);
#2399=ELLIPSE('',#109104,0.14669146556753,0.127050784764348);
#2400=ELLIPSE('',#109121,0.14669286188798,0.127051669380014);
#2401=ELLIPSE('',#109132,0.146691465566935,0.127050784763918);
#2402=ELLIPSE('',#109136,0.146692861886356,0.127051669379263);
#2403=ELLIPSE('',#109148,0.146691465566887,0.127050784763808);
#2404=ELLIPSE('',#109165,0.146692861885907,0.127051669379342);
#2405=ELLIPSE('',#109176,0.146691465567757,0.127050784764672);
#2406=ELLIPSE('',#109180,0.146692861884678,0.12705166937695);
#2407=ELLIPSE('',#109192,0.146691465567185,0.127050784764166);
#2408=ELLIPSE('',#109209,0.146692861890572,0.127051669381342);
#2409=ELLIPSE('',#109220,0.146691465567066,0.127050784764021);
#2410=ELLIPSE('',#109224,0.146692861888206,0.12705166937956);
#2411=ELLIPSE('',#109236,0.146691465566877,0.127050784763825);
#2412=ELLIPSE('',#109253,0.146692861887242,0.127051669379058);
#2413=ELLIPSE('',#109264,0.146691465568348,0.127050784765209);
#2414=ELLIPSE('',#109268,0.146692861888642,0.127051669380438);
#2415=ELLIPSE('',#109280,0.146691465566805,0.127050784763759);
#2416=ELLIPSE('',#109297,0.146692861889443,0.127051669380692);
#2417=ELLIPSE('',#109308,0.146691465567603,0.127050784764421);
#2418=ELLIPSE('',#109312,0.146692861887422,0.127051669380312);
#2419=ELLIPSE('',#109324,0.14669146556689,0.127050784763862);
#2420=ELLIPSE('',#109341,0.146692861889481,0.127051669381202);
#2421=ELLIPSE('',#109352,0.1466914655671,0.127050784763995);
#2422=ELLIPSE('',#109356,0.146692861887204,0.127051669379616);
#2423=ELLIPSE('',#109368,0.146691465567273,0.127050784764272);
#2424=ELLIPSE('',#109385,0.146692861888368,0.127051669380196);
#2425=ELLIPSE('',#109396,0.146691465567354,0.127050784764149);
#2426=ELLIPSE('',#109400,0.146692861890029,0.127051669381068);
#2427=ELLIPSE('',#109412,0.146691465567345,0.127050784764251);
#2428=ELLIPSE('',#109429,0.146692861886787,0.127051669379225);
#2429=ELLIPSE('',#109440,0.14669146556616,0.127050784763233);
#2430=ELLIPSE('',#109444,0.146692861890226,0.127051669380676);
#2431=ELLIPSE('',#109456,0.146691465567008,0.127050784763999);
#2432=ELLIPSE('',#109473,0.146692861888184,0.127051669380381);
#2433=ELLIPSE('',#109484,0.146691465566748,0.127050784763769);
#2434=ELLIPSE('',#109488,0.146692861885311,0.127051669377263);
#2435=ELLIPSE('',#109500,0.146691465566819,0.127050784763813);
#2436=ELLIPSE('',#109517,0.146692861886789,0.127051669379176);
#2437=ELLIPSE('',#109528,0.146691465567026,0.127050784764011);
#2438=ELLIPSE('',#109532,0.146692861886493,0.127051669378802);
#2439=ELLIPSE('',#109544,0.146691465566968,0.127050784763933);
#2440=ELLIPSE('',#109555,0.146692861884915,0.127051669378065);
#2441=ELLIPSE('',#109566,0.146691465567284,0.127050784764167);
#2442=ELLIPSE('',#109570,0.146692861887552,0.127051669379605);
#2443=ELLIPSE('',#109582,0.146691465567139,0.127050784764066);
#2444=ELLIPSE('',#109599,0.146692861886816,0.12705166937847);
#2445=ELLIPSE('',#109610,0.1466914655673,0.127050784764209);
#2446=ELLIPSE('',#109614,0.146692861889501,0.127051669381896);
#2447=ELLIPSE('',#109626,0.146691465566451,0.127050784763435);
#2448=ELLIPSE('',#109643,0.146692861887066,0.127051669379779);
#2449=ELLIPSE('',#109654,0.14669146556654,0.127050784763608);
#2450=ELLIPSE('',#109658,0.146692861888615,0.12705166938038);
#2451=ELLIPSE('',#109670,0.146691465567071,0.127050784764075);
#2452=ELLIPSE('',#109687,0.146692861887632,0.127051669379309);
#2453=ELLIPSE('',#109698,0.146691465566808,0.127050784763736);
#2454=ELLIPSE('',#109702,0.146692861884796,0.127051669377432);
#2455=ELLIPSE('',#109714,0.146691465567388,0.127050784764305);
#2456=ELLIPSE('',#109731,0.146692861888991,0.127051669380517);
#2457=ELLIPSE('',#109742,0.146691465566864,0.127050784763845);
#2458=ELLIPSE('',#109746,0.146692861884702,0.127051669377471);
#2459=ELLIPSE('',#109758,0.146691465566428,0.127050784763449);
#2460=ELLIPSE('',#109775,0.146692861890953,0.127051669380815);
#2461=ELLIPSE('',#109786,0.146691465567053,0.127050784764001);
#2462=ELLIPSE('',#109790,0.146692861888345,0.1270516693799);
#2463=ELLIPSE('',#109802,0.146691465567222,0.12705078476413);
#2464=ELLIPSE('',#109819,0.146692861888203,0.127051669381085);
#2465=ELLIPSE('',#109830,0.146691465566776,0.12705078476376);
#2466=ELLIPSE('',#109834,0.146692861887467,0.127051669379034);
#2467=ELLIPSE('',#109846,0.14669146556693,0.127050784763931);
#2468=ELLIPSE('',#109863,0.146692861889339,0.127051669380069);
#2469=ELLIPSE('',#109874,0.146691465567031,0.127050784764045);
#2470=ELLIPSE('',#109878,0.146692861888236,0.127051669380494);
#2471=ELLIPSE('',#109890,0.146691465566649,0.127050784763597);
#2472=ELLIPSE('',#109907,0.146692861886606,0.127051669379421);
#2473=ELLIPSE('',#109918,0.14669146556708,0.127050784763953);
#2474=ELLIPSE('',#109922,0.146692861889654,0.127051669380473);
#2475=ELLIPSE('',#109934,0.146691465567106,0.127050784764044);
#2476=ELLIPSE('',#109951,0.146692861882192,0.127051669376308);
#2477=ELLIPSE('',#109962,0.14669146556671,0.127050784763768);
#2478=ELLIPSE('',#109966,0.146692861888881,0.127051669380729);
#2479=ELLIPSE('',#109978,0.14669146556744,0.127050784764356);
#2480=ELLIPSE('',#109995,0.146692861881194,0.127051669375846);
#2481=ELLIPSE('',#110006,0.146691465567076,0.127050784764015);
#2482=ELLIPSE('',#110010,0.146692861885841,0.127051669378297);
#2483=ELLIPSE('',#110022,0.146691465566904,0.127050784763881);
#2484=ELLIPSE('',#110039,0.146692861885695,0.127051669379351);
#2485=ELLIPSE('',#110050,0.146691465567641,0.12705078476453);
#2486=ELLIPSE('',#110054,0.146692861885858,0.127051669378641);
#2487=ELLIPSE('',#110066,0.146691465566973,0.127050784763915);
#2488=ELLIPSE('',#110083,0.146692861889958,0.127051669381835);
#2489=ELLIPSE('',#110094,0.146691465567342,0.127050784764266);
#2490=ELLIPSE('',#110098,0.146692861885233,0.127051669378449);
#2491=ELLIPSE('',#110110,0.146691465566801,0.127050784763771);
#2492=ELLIPSE('',#110127,0.14669286188867,0.127051669380722);
#2493=ELLIPSE('',#110138,0.146691465567151,0.127050784764096);
#2494=ELLIPSE('',#110142,0.146692861885986,0.127051669378141);
#2495=ELLIPSE('',#110154,0.14669146556678,0.127050784763731);
#2496=ELLIPSE('',#110171,0.146692861887676,0.127051669379299);
#2497=ELLIPSE('',#110182,0.146691465566652,0.127050784763613);
#2498=ELLIPSE('',#110386,11.6598168140706,6.11693208644189);
#2499=ELLIPSE('',#110472,1.76555576320667,1.39650815276582);
#2500=ELLIPSE('',#110588,4.72274651081773,4.72274160816237);
#2501=(
BOUNDED_SURFACE()
B_SPLINE_SURFACE(1,2,((#145815,#145816,#145817,#145818,#145819,#145820,
#145821,#145822,#145823,#145824,#145825,#145826,#145827,#145828,#145829,
#145830,#145831,#145832,#145833,#145834,#145835,#145836,#145837,#145838,
#145839,#145840,#145841,#145842,#145843,#145844,#145845,#145846,#145847,
#145848,#145849,#145850,#145851,#145852,#145853,#145854,#145855,#145856,
#145857,#145858,#145859,#145860,#145861,#145862,#145863,#145864,#145865,
#145866,#145867,#145868,#145869,#145870,#145871,#145872,#145873,#145874,
#145875,#145876,#145877,#145878,#145879,#145880,#145881,#145882,#145883,
#145884,#145885,#145886,#145887,#145888,#145889,#145890,#145891,#145892,
#145893,#145894,#145895,#145896,#145897,#145898,#145899,#145900,#145901,
#145902,#145903,#145904,#145905,#145906,#145907,#145908,#145909,#145910,
#145911,#145912,#145913,#145914,#145915,#145916,#145917,#145918,#145919,
#145920,#145921,#145922,#145923,#145924,#145925,#145926,#145927,#145928,
#145929,#145930,#145931,#145932,#145933,#145934,#145935,#145936,#145937,
#145938,#145939,#145940,#145941,#145942,#145943,#145944,#145945,#145946,
#145947,#145948,#145949,#145950,#145951,#145952,#145953,#145954,#145955,
#145956,#145957,#145958,#145959,#145960,#145961,#145962,#145963,#145964,
#145965,#145966,#145967,#145968,#145969,#145970,#145971,#145972,#145973,
#145974,#145975,#145976,#145977,#145978,#145979,#145980,#145981,#145982,
#145983,#145984,#145985,#145986,#145987,#145988,#145989,#145990,#145991,
#145992,#145993,#145994,#145995,#145996,#145997,#145998,#145999,#146000,
#146001,#146002,#146003,#146004,#146005,#146006,#146007,#146008,#146009,
#146010,#146011,#146012,#146013,#146014,#146015,#146016,#146017,#146018,
#146019,#146020,#146021,#146022,#146023,#146024,#146025,#146026,#146027,
#146028,#146029,#146030,#146031,#146032,#146033,#146034,#146035,#146036,
#146037,#146038,#146039,#146040,#146041,#146042,#146043,#146044,#146045,
#146046,#146047,#146048,#146049,#146050,#146051,#146052,#146053,#146054,
#146055,#146056,#146057,#146058,#146059,#146060,#146061,#146062,#146063,
#146064,#146065,#146066,#146067,#146068,#146069,#146070,#146071,#146072,
#146073,#146074,#146075,#146076,#146077,#146078,#146079,#146080,#146081,
#146082,#146083,#146084,#146085,#146086,#146087,#146088,#146089,#146090,
#146091,#146092,#146093,#146094,#146095,#146096,#146097,#146098,#146099,
#146100,#146101,#146102,#146103,#146104,#146105,#146106,#146107,#146108,
#146109,#146110,#146111,#146112,#146113,#146114,#146115,#146116,#146117,
#146118,#146119,#146120,#146121,#146122,#146123,#146124,#146125,#146126,
#146127,#146128,#146129,#146130,#146131,#146132,#146133,#146134,#146135,
#146136,#146137,#146138,#146139,#146140,#146141,#146142,#146143,#146144,
#146145,#146146,#146147,#146148,#146149,#146150,#146151,#146152,#146153,
#146154,#146155,#146156,#146157,#146158,#146159,#146160,#146161,#146162,
#146163,#146164,#146165,#146166,#146167,#146168,#146169,#146170,#146171,
#146172,#146173,#146174,#146175,#146176,#146177,#146178,#146179,#146180,
#146181,#146182,#146183,#146184,#146185,#146186,#146187,#146188,#146189,
#146190,#146191,#146192,#146193,#146194,#146195,#146196,#146197,#146198,
#146199,#146200,#146201,#146202,#146203,#146204,#146205,#146206,#146207,
#146208,#146209,#146210,#146211,#146212,#146213,#146214,#146215,#146216,
#146217,#146218,#146219,#146220,#146221,#146222,#146223,#146224,#146225,
#146226,#146227,#146228,#146229,#146230,#146231,#146232,#146233,#146234,
#146235,#146236,#146237,#146238,#146239,#146240,#146241,#146242,#146243,
#146244,#146245,#146246,#146247,#146248,#146249,#146250,#146251,#146252,
#146253,#146254,#146255,#146256,#146257,#146258,#146259,#146260,#146261,
#146262,#146263,#146264,#146265,#146266,#146267,#146268,#146269,#146270,
#146271,#146272,#146273,#146274,#146275,#146276,#146277,#146278,#146279,
#146280,#146281,#146282,#146283,#146284,#146285,#146286,#146287,#146288,
#146289,#146290,#146291,#146292,#146293,#146294,#146295,#146296,#146297,
#146298,#146299,#146300,#146301,#146302,#146303,#146304,#146305,#146306,
#146307,#146308,#146309,#146310,#146311,#146312,#146313,#146314,#146315,
#146316,#146317,#146318,#146319,#146320,#146321,#146322,#146323,#146324,
#146325,#146326,#146327,#146328,#146329,#146330,#146331,#146332,#146333,
#146334,#146335,#146336,#146337,#146338,#146339,#146340,#146341,#146342,
#146343,#146344,#146345,#146346,#146347,#146348,#146349,#146350,#146351,
#146352,#146353,#146354,#146355,#146356,#146357,#146358,#146359,#146360,
#146361,#146362,#146363,#146364,#146365,#146366,#146367,#146368,#146369,
#146370,#146371,#146372,#146373,#146374,#146375,#146376,#146377,#146378,
#146379,#146380,#146381,#146382,#146383,#146384,#146385,#146386,#146387,
#146388,#146389,#146390,#146391,#146392,#146393,#146394,#146395,#146396,
#146397,#146398,#146399,#146400,#146401,#146402,#146403,#146404,#146405,
#146406,#146407,#146408,#146409,#146410,#146411,#146412,#146413,#146414,
#146415,#146416,#146417,#146418,#146419,#146420,#146421,#146422,#146423,
#146424,#146425,#146426,#146427,#146428,#146429,#146430,#146431,#146432,
#146433,#146434,#146435,#146436,#146437,#146438,#146439,#146440,#146441,
#146442,#146443,#146444,#146445,#146446,#146447,#146448,#146449,#146450,
#146451,#146452,#146453,#146454,#146455,#146456,#146457,#146458,#146459,
#146460,#146461,#146462,#146463,#146464,#146465,#146466,#146467,#146468,
#146469,#146470,#146471,#146472,#146473,#146474,#146475,#146476,#146477,
#146478,#146479,#146480,#146481,#146482,#146483,#146484,#146485,#146486,
#146487,#146488,#146489,#146490,#146491,#146492,#146493,#146494,#146495,
#146496,#146497,#146498,#146499,#146500,#146501,#146502,#146503,#146504,
#146505,#146506,#146507,#146508,#146509,#146510,#146511,#146512,#146513,
#146514,#146515,#146516,#146517,#146518,#146519,#146520,#146521,#146522,
#146523,#146524,#146525,#146526,#146527,#146528,#146529,#146530,#146531,
#146532,#146533,#146534,#146535,#146536,#146537,#146538,#146539,#146540,
#146541,#146542,#146543,#146544,#146545,#146546,#146547,#146548,#146549,
#146550,#146551,#146552,#146553,#146554,#146555,#146556,#146557,#146558,
#146559,#146560,#146561,#146562,#146563,#146564,#146565,#146566,#146567,
#146568,#146569,#146570,#146571,#146572,#146573,#146574,#146575,#146576,
#146577,#146578,#146579,#146580,#146581,#146582,#146583,#146584,#146585,
#146586,#146587,#146588,#146589,#146590,#146591,#146592,#146593,#146594,
#146595,#146596,#146597,#146598,#146599,#146600,#146601,#146602,#146603,
#146604,#146605,#146606,#146607,#146608,#146609,#146610,#146611,#146612,
#146613,#146614,#146615,#146616,#146617,#146618,#146619,#146620,#146621,
#146622,#146623,#146624,#146625,#146626,#146627,#146628,#146629,#146630,
#146631,#146632,#146633,#146634,#146635,#146636,#146637,#146638,#146639,
#146640,#146641,#146642,#146643,#146644,#146645,#146646,#146647,#146648,
#146649,#146650,#146651,#146652,#146653,#146654,#146655,#146656,#146657,
#146658,#146659,#146660,#146661,#146662,#146663,#146664,#146665,#146666,
#146667,#146668,#146669,#146670,#146671,#146672,#146673,#146674,#146675,
#146676,#146677,#146678,#146679,#146680,#146681,#146682,#146683,#146684,
#146685,#146686,#146687,#146688,#146689,#146690,#146691,#146692,#146693,
#146694,#146695,#146696,#146697,#146698,#146699,#146700,#146701,#146702,
#146703,#146704,#146705,#146706,#146707,#146708,#146709,#146710,#146711,
#146712,#146713,#146714,#146715,#146716,#146717,#146718,#146719,#146720,
#146721,#146722,#146723,#146724,#146725,#146726,#146727,#146728,#146729,
#146730,#146731,#146732,#146733,#146734,#146735,#146736,#146737,#146738,
#146739,#146740,#146741,#146742,#146743,#146744,#146745,#146746,#146747,
#146748,#146749,#146750,#146751,#146752,#146753,#146754,#146755,#146756,
#146757,#146758,#146759,#146760,#146761,#146762,#146763,#146764,#146765,
#146766,#146767,#146768,#146769,#146770,#146771,#146772,#146773,#146774,
#146775,#146776,#146777,#146778,#146779,#146780,#146781,#146782,#146783,
#146784,#146785,#146786,#146787,#146788,#146789,#146790,#146791,#146792,
#146793,#146794,#146795,#146796,#146797,#146798,#146799,#146800,#146801,
#146802,#146803,#146804,#146805,#146806,#146807,#146808,#146809,#146810,
#146811,#146812,#146813,#146814,#146815,#146816,#146817,#146818,#146819,
#146820,#146821,#146822,#146823,#146824,#146825,#146826,#146827,#146828,
#146829,#146830,#146831,#146832,#146833,#146834,#146835,#146836,#146837,
#146838,#146839,#146840,#146841,#146842,#146843,#146844,#146845,#146846,
#146847,#146848,#146849,#146850,#146851,#146852,#146853,#146854,#146855,
#146856,#146857,#146858,#146859,#146860,#146861,#146862,#146863,#146864,
#146865,#146866,#146867,#146868,#146869,#146870,#146871,#146872,#146873,
#146874,#146875,#146876,#146877,#146878,#146879,#146880,#146881,#146882,
#146883,#146884,#146885,#146886,#146887,#146888,#146889,#146890,#146891,
#146892,#146893,#146894,#146895,#146896,#146897,#146898,#146899,#146900,
#146901,#146902,#146903,#146904,#146905,#146906,#146907,#146908,#146909,
#146910,#146911,#146912,#146913,#146914,#146915,#146916,#146917,#146918,
#146919,#146920,#146921,#146922,#146923,#146924,#146925,#146926,#146927,
#146928,#146929,#146930,#146931,#146932,#146933,#146934,#146935,#146936,
#146937,#146938,#146939,#146940,#146941,#146942,#146943,#146944,#146945,
#146946,#146947,#146948,#146949,#146950,#146951,#146952,#146953,#146954,
#146955,#146956,#146957,#146958,#146959,#146960,#146961,#146962,#146963,
#146964,#146965,#146966,#146967,#146968,#146969,#146970,#146971,#146972,
#146973,#146974,#146975,#146976,#146977,#146978,#146979,#146980,#146981,
#146982,#146983,#146984,#146985,#146986,#146987,#146988,#146989,#146990,
#146991,#146992,#146993,#146994,#146995,#146996,#146997,#146998,#146999,
#147000,#147001,#147002,#147003,#147004,#147005,#147006,#147007,#147008,
#147009,#147010,#147011,#147012,#147013,#147014,#147015,#147016,#147017,
#147018,#147019,#147020,#147021,#147022,#147023,#147024,#147025,#147026,
#147027,#147028,#147029,#147030,#147031,#147032,#147033,#147034,#147035,
#147036,#147037,#147038,#147039,#147040,#147041,#147042,#147043,#147044,
#147045,#147046,#147047,#147048,#147049,#147050,#147051,#147052,#147053,
#147054,#147055,#147056,#147057,#147058,#147059,#147060,#147061,#147062,
#147063,#147064,#147065,#147066,#147067,#147068,#147069,#147070,#147071,
#147072,#147073,#147074,#147075,#147076,#147077,#147078,#147079,#147080,
#147081,#147082,#147083,#147084,#147085,#147086,#147087,#147088,#147089,
#147090,#147091,#147092,#147093,#147094,#147095,#147096,#147097,#147098,
#147099,#147100,#147101,#147102,#147103,#147104,#147105,#147106,#147107,
#147108,#147109,#147110,#147111,#147112,#147113,#147114,#147115,#147116,
#147117,#147118,#147119,#147120,#147121,#147122,#147123,#147124,#147125,
#147126,#147127,#147128,#147129,#147130,#147131,#147132,#147133,#147134,
#147135,#147136,#147137,#147138,#147139,#147140,#147141,#147142,#147143,
#147144,#147145,#147146,#147147,#147148,#147149,#147150,#147151,#147152,
#147153,#147154,#147155,#147156,#147157,#147158,#147159,#147160,#147161,
#147162,#147163,#147164,#147165,#147166,#147167,#147168,#147169,#147170,
#147171,#147172,#147173,#147174,#147175,#147176,#147177,#147178,#147179,
#147180,#147181,#147182,#147183,#147184,#147185,#147186,#147187,#147188,
#147189,#147190,#147191,#147192,#147193,#147194,#147195,#147196,#147197,
#147198,#147199,#147200,#147201,#147202,#147203,#147204,#147205,#147206,
#147207,#147208,#147209,#147210,#147211,#147212,#147213,#147214,#147215,
#147216,#147217,#147218,#147219,#147220,#147221,#147222,#147223,#147224,
#147225,#147226,#147227,#147228,#147229,#147230,#147231,#147232,#147233,
#147234,#147235,#147236,#147237,#147238,#147239,#147240,#147241,#147242,
#147243,#147244,#147245,#147246,#147247,#147248,#147249,#147250,#147251,
#147252,#147253,#147254,#147255,#147256,#147257,#147258,#147259,#147260,
#147261,#147262,#147263,#147264,#147265,#147266,#147267,#147268,#147269,
#147270,#147271,#147272,#147273,#147274,#147275,#147276,#147277,#147278,
#147279,#147280,#147281,#147282,#147283,#147284,#147285,#147286,#147287,
#147288,#147289,#147290,#147291,#147292,#147293,#147294,#147295,#147296,
#147297,#147298,#147299,#147300,#147301,#147302,#147303,#147304,#147305,
#147306,#147307,#147308,#147309,#147310,#147311,#147312,#147313,#147314,
#147315,#147316,#147317,#147318,#147319,#147320,#147321,#147322,#147323,
#147324,#147325,#147326,#147327,#147328,#147329,#147330,#147331,#147332,
#147333,#147334,#147335,#147336,#147337,#147338,#147339,#147340,#147341,
#147342,#147343,#147344,#147345,#147346,#147347,#147348,#147349,#147350,
#147351,#147352,#147353,#147354,#147355,#147356,#147357,#147358,#147359,
#147360,#147361,#147362,#147363,#147364,#147365,#147366,#147367,#147368,
#147369,#147370,#147371,#147372,#147373,#147374,#147375,#147376,#147377,
#147378,#147379,#147380,#147381,#147382,#147383,#147384,#147385,#147386,
#147387,#147388,#147389,#147390,#147391,#147392,#147393,#147394,#147395,
#147396,#147397,#147398,#147399,#147400,#147401,#147402,#147403,#147404,
#147405,#147406,#147407,#147408,#147409,#147410,#147411,#147412,#147413,
#147414,#147415,#147416,#147417,#147418,#147419,#147420,#147421,#147422,
#147423,#147424,#147425,#147426,#147427,#147428,#147429,#147430,#147431,
#147432,#147433,#147434,#147435,#147436,#147437,#147438,#147439,#147440,
#147441,#147442,#147443,#147444,#147445,#147446,#147447,#147448,#147449,
#147450,#147451,#147452,#147453,#147454,#147455,#147456,#147457,#147458,
#147459,#147460,#147461,#147462,#147463,#147464,#147465,#147466,#147467,
#147468,#147469,#147470,#147471,#147472,#147473,#147474,#147475,#147476,
#147477,#147478,#147479,#147480,#147481,#147482,#147483,#147484,#147485,
#147486,#147487,#147488,#147489,#147490,#147491,#147492,#147493,#147494,
#147495,#147496,#147497,#147498,#147499,#147500,#147501,#147502,#147503,
#147504,#147505,#147506,#147507,#147508,#147509,#147510,#147511,#147512,
#147513,#147514,#147515,#147516,#147517,#147518,#147519,#147520,#147521,
#147522,#147523,#147524,#147525,#147526,#147527,#147528,#147529,#147530,
#147531,#147532,#147533,#147534,#147535,#147536,#147537,#147538,#147539,
#147540,#147541,#147542,#147543,#147544,#147545,#147546,#147547,#147548,
#147549,#147550,#147551,#147552,#147553,#147554,#147555,#147556,#147557,
#147558,#147559,#147560,#147561,#147562,#147563,#147564,#147565,#147566,
#147567,#147568,#147569,#147570,#147571,#147572,#147573,#147574,#147575,
#147576,#147577,#147578,#147579,#147580,#147581,#147582,#147583,#147584,
#147585,#147586,#147587,#147588,#147589,#147590,#147591,#147592,#147593,
#147594,#147595,#147596,#147597,#147598,#147599,#147600,#147601,#147602,
#147603,#147604,#147605,#147606,#147607,#147608,#147609,#147610,#147611,
#147612,#147613,#147614,#147615,#147616,#147617,#147618,#147619,#147620,
#147621,#147622,#147623,#147624,#147625,#147626,#147627,#147628,#147629,
#147630,#147631,#147632,#147633,#147634,#147635,#147636,#147637,#147638,
#147639,#147640,#147641,#147642,#147643,#147644,#147645,#147646,#147647,
#147648,#147649,#147650,#147651,#147652,#147653,#147654,#147655,#147656,
#147657,#147658,#147659,#147660,#147661,#147662,#147663,#147664,#147665,
#147666,#147667,#147668,#147669,#147670,#147671,#147672,#147673,#147674,
#147675,#147676,#147677,#147678,#147679,#147680,#147681,#147682,#147683,
#147684,#147685,#147686,#147687,#147688,#147689,#147690,#147691,#147692,
#147693,#147694,#147695,#147696,#147697,#147698,#147699,#147700,#147701,
#147702,#147703,#147704,#147705,#147706,#147707,#147708,#147709,#147710,
#147711,#147712,#147713,#147714,#147715,#147716,#147717,#147718,#147719,
#147720,#147721,#147722,#147723,#147724,#147725,#147726,#147727,#147728,
#147729,#147730,#147731,#147732,#147733,#147734,#147735,#147736,#147737,
#147738,#147739,#147740,#147741,#147742,#147743,#147744,#147745,#147746,
#147747,#147748,#147749,#147750,#147751,#147752,#147753,#147754,#147755,
#147756,#147757,#147758,#147759,#147760,#147761,#147762,#147763,#147764,
#147765,#147766,#147767,#147768,#147769,#147770,#147771,#147772,#147773,
#147774,#147775,#147776,#147777,#147778,#147779,#147780,#147781,#147782,
#147783,#147784,#147785,#147786,#147787,#147788,#147789,#147790,#147791,
#147792,#147793,#147794,#147795,#147796,#147797,#147798,#147799,#147800,
#147801,#147802,#147803,#147804,#147805,#147806,#147807,#147808,#147809,
#147810,#147811,#147812,#147813,#147814,#147815,#147816,#147817,#147818,
#147819,#147820,#147821,#147822,#147823,#147824,#147825,#147826,#147827),
(#147828,#147829,#147830,#147831,#147832,#147833,#147834,#147835,#147836,
#147837,#147838,#147839,#147840,#147841,#147842,#147843,#147844,#147845,
#147846,#147847,#147848,#147849,#147850,#147851,#147852,#147853,#147854,
#147855,#147856,#147857,#147858,#147859,#147860,#147861,#147862,#147863,
#147864,#147865,#147866,#147867,#147868,#147869,#147870,#147871,#147872,
#147873,#147874,#147875,#147876,#147877,#147878,#147879,#147880,#147881,
#147882,#147883,#147884,#147885,#147886,#147887,#147888,#147889,#147890,
#147891,#147892,#147893,#147894,#147895,#147896,#147897,#147898,#147899,
#147900,#147901,#147902,#147903,#147904,#147905,#147906,#147907,#147908,
#147909,#147910,#147911,#147912,#147913,#147914,#147915,#147916,#147917,
#147918,#147919,#147920,#147921,#147922,#147923,#147924,#147925,#147926,
#147927,#147928,#147929,#147930,#147931,#147932,#147933,#147934,#147935,
#147936,#147937,#147938,#147939,#147940,#147941,#147942,#147943,#147944,
#147945,#147946,#147947,#147948,#147949,#147950,#147951,#147952,#147953,
#147954,#147955,#147956,#147957,#147958,#147959,#147960,#147961,#147962,
#147963,#147964,#147965,#147966,#147967,#147968,#147969,#147970,#147971,
#147972,#147973,#147974,#147975,#147976,#147977,#147978,#147979,#147980,
#147981,#147982,#147983,#147984,#147985,#147986,#147987,#147988,#147989,
#147990,#147991,#147992,#147993,#147994,#147995,#147996,#147997,#147998,
#147999,#148000,#148001,#148002,#148003,#148004,#148005,#148006,#148007,
#148008,#148009,#148010,#148011,#148012,#148013,#148014,#148015,#148016,
#148017,#148018,#148019,#148020,#148021,#148022,#148023,#148024,#148025,
#148026,#148027,#148028,#148029,#148030,#148031,#148032,#148033,#148034,
#148035,#148036,#148037,#148038,#148039,#148040,#148041,#148042,#148043,
#148044,#148045,#148046,#148047,#148048,#148049,#148050,#148051,#148052,
#148053,#148054,#148055,#148056,#148057,#148058,#148059,#148060,#148061,
#148062,#148063,#148064,#148065,#148066,#148067,#148068,#148069,#148070,
#148071,#148072,#148073,#148074,#148075,#148076,#148077,#148078,#148079,
#148080,#148081,#148082,#148083,#148084,#148085,#148086,#148087,#148088,
#148089,#148090,#148091,#148092,#148093,#148094,#148095,#148096,#148097,
#148098,#148099,#148100,#148101,#148102,#148103,#148104,#148105,#148106,
#148107,#148108,#148109,#148110,#148111,#148112,#148113,#148114,#148115,
#148116,#148117,#148118,#148119,#148120,#148121,#148122,#148123,#148124,
#148125,#148126,#148127,#148128,#148129,#148130,#148131,#148132,#148133,
#148134,#148135,#148136,#148137,#148138,#148139,#148140,#148141,#148142,
#148143,#148144,#148145,#148146,#148147,#148148,#148149,#148150,#148151,
#148152,#148153,#148154,#148155,#148156,#148157,#148158,#148159,#148160,
#148161,#148162,#148163,#148164,#148165,#148166,#148167,#148168,#148169,
#148170,#148171,#148172,#148173,#148174,#148175,#148176,#148177,#148178,
#148179,#148180,#148181,#148182,#148183,#148184,#148185,#148186,#148187,
#148188,#148189,#148190,#148191,#148192,#148193,#148194,#148195,#148196,
#148197,#148198,#148199,#148200,#148201,#148202,#148203,#148204,#148205,
#148206,#148207,#148208,#148209,#148210,#148211,#148212,#148213,#148214,
#148215,#148216,#148217,#148218,#148219,#148220,#148221,#148222,#148223,
#148224,#148225,#148226,#148227,#148228,#148229,#148230,#148231,#148232,
#148233,#148234,#148235,#148236,#148237,#148238,#148239,#148240,#148241,
#148242,#148243,#148244,#148245,#148246,#148247,#148248,#148249,#148250,
#148251,#148252,#148253,#148254,#148255,#148256,#148257,#148258,#148259,
#148260,#148261,#148262,#148263,#148264,#148265,#148266,#148267,#148268,
#148269,#148270,#148271,#148272,#148273,#148274,#148275,#148276,#148277,
#148278,#148279,#148280,#148281,#148282,#148283,#148284,#148285,#148286,
#148287,#148288,#148289,#148290,#148291,#148292,#148293,#148294,#148295,
#148296,#148297,#148298,#148299,#148300,#148301,#148302,#148303,#148304,
#148305,#148306,#148307,#148308,#148309,#148310,#148311,#148312,#148313,
#148314,#148315,#148316,#148317,#148318,#148319,#148320,#148321,#148322,
#148323,#148324,#148325,#148326,#148327,#148328,#148329,#148330,#148331,
#148332,#148333,#148334,#148335,#148336,#148337,#148338,#148339,#148340,
#148341,#148342,#148343,#148344,#148345,#148346,#148347,#148348,#148349,
#148350,#148351,#148352,#148353,#148354,#148355,#148356,#148357,#148358,
#148359,#148360,#148361,#148362,#148363,#148364,#148365,#148366,#148367,
#148368,#148369,#148370,#148371,#148372,#148373,#148374,#148375,#148376,
#148377,#148378,#148379,#148380,#148381,#148382,#148383,#148384,#148385,
#148386,#148387,#148388,#148389,#148390,#148391,#148392,#148393,#148394,
#148395,#148396,#148397,#148398,#148399,#148400,#148401,#148402,#148403,
#148404,#148405,#148406,#148407,#148408,#148409,#148410,#148411,#148412,
#148413,#148414,#148415,#148416,#148417,#148418,#148419,#148420,#148421,
#148422,#148423,#148424,#148425,#148426,#148427,#148428,#148429,#148430,
#148431,#148432,#148433,#148434,#148435,#148436,#148437,#148438,#148439,
#148440,#148441,#148442,#148443,#148444,#148445,#148446,#148447,#148448,
#148449,#148450,#148451,#148452,#148453,#148454,#148455,#148456,#148457,
#148458,#148459,#148460,#148461,#148462,#148463,#148464,#148465,#148466,
#148467,#148468,#148469,#148470,#148471,#148472,#148473,#148474,#148475,
#148476,#148477,#148478,#148479,#148480,#148481,#148482,#148483,#148484,
#148485,#148486,#148487,#148488,#148489,#148490,#148491,#148492,#148493,
#148494,#148495,#148496,#148497,#148498,#148499,#148500,#148501,#148502,
#148503,#148504,#148505,#148506,#148507,#148508,#148509,#148510,#148511,
#148512,#148513,#148514,#148515,#148516,#148517,#148518,#148519,#148520,
#148521,#148522,#148523,#148524,#148525,#148526,#148527,#148528,#148529,
#148530,#148531,#148532,#148533,#148534,#148535,#148536,#148537,#148538,
#148539,#148540,#148541,#148542,#148543,#148544,#148545,#148546,#148547,
#148548,#148549,#148550,#148551,#148552,#148553,#148554,#148555,#148556,
#148557,#148558,#148559,#148560,#148561,#148562,#148563,#148564,#148565,
#148566,#148567,#148568,#148569,#148570,#148571,#148572,#148573,#148574,
#148575,#148576,#148577,#148578,#148579,#148580,#148581,#148582,#148583,
#148584,#148585,#148586,#148587,#148588,#148589,#148590,#148591,#148592,
#148593,#148594,#148595,#148596,#148597,#148598,#148599,#148600,#148601,
#148602,#148603,#148604,#148605,#148606,#148607,#148608,#148609,#148610,
#148611,#148612,#148613,#148614,#148615,#148616,#148617,#148618,#148619,
#148620,#148621,#148622,#148623,#148624,#148625,#148626,#148627,#148628,
#148629,#148630,#148631,#148632,#148633,#148634,#148635,#148636,#148637,
#148638,#148639,#148640,#148641,#148642,#148643,#148644,#148645,#148646,
#148647,#148648,#148649,#148650,#148651,#148652,#148653,#148654,#148655,
#148656,#148657,#148658,#148659,#148660,#148661,#148662,#148663,#148664,
#148665,#148666,#148667,#148668,#148669,#148670,#148671,#148672,#148673,
#148674,#148675,#148676,#148677,#148678,#148679,#148680,#148681,#148682,
#148683,#148684,#148685,#148686,#148687,#148688,#148689,#148690,#148691,
#148692,#148693,#148694,#148695,#148696,#148697,#148698,#148699,#148700,
#148701,#148702,#148703,#148704,#148705,#148706,#148707,#148708,#148709,
#148710,#148711,#148712,#148713,#148714,#148715,#148716,#148717,#148718,
#148719,#148720,#148721,#148722,#148723,#148724,#148725,#148726,#148727,
#148728,#148729,#148730,#148731,#148732,#148733,#148734,#148735,#148736,
#148737,#148738,#148739,#148740,#148741,#148742,#148743,#148744,#148745,
#148746,#148747,#148748,#148749,#148750,#148751,#148752,#148753,#148754,
#148755,#148756,#148757,#148758,#148759,#148760,#148761,#148762,#148763,
#148764,#148765,#148766,#148767,#148768,#148769,#148770,#148771,#148772,
#148773,#148774,#148775,#148776,#148777,#148778,#148779,#148780,#148781,
#148782,#148783,#148784,#148785,#148786,#148787,#148788,#148789,#148790,
#148791,#148792,#148793,#148794,#148795,#148796,#148797,#148798,#148799,
#148800,#148801,#148802,#148803,#148804,#148805,#148806,#148807,#148808,
#148809,#148810,#148811,#148812,#148813,#148814,#148815,#148816,#148817,
#148818,#148819,#148820,#148821,#148822,#148823,#148824,#148825,#148826,
#148827,#148828,#148829,#148830,#148831,#148832,#148833,#148834,#148835,
#148836,#148837,#148838,#148839,#148840,#148841,#148842,#148843,#148844,
#148845,#148846,#148847,#148848,#148849,#148850,#148851,#148852,#148853,
#148854,#148855,#148856,#148857,#148858,#148859,#148860,#148861,#148862,
#148863,#148864,#148865,#148866,#148867,#148868,#148869,#148870,#148871,
#148872,#148873,#148874,#148875,#148876,#148877,#148878,#148879,#148880,
#148881,#148882,#148883,#148884,#148885,#148886,#148887,#148888,#148889,
#148890,#148891,#148892,#148893,#148894,#148895,#148896,#148897,#148898,
#148899,#148900,#148901,#148902,#148903,#148904,#148905,#148906,#148907,
#148908,#148909,#148910,#148911,#148912,#148913,#148914,#148915,#148916,
#148917,#148918,#148919,#148920,#148921,#148922,#148923,#148924,#148925,
#148926,#148927,#148928,#148929,#148930,#148931,#148932,#148933,#148934,
#148935,#148936,#148937,#148938,#148939,#148940,#148941,#148942,#148943,
#148944,#148945,#148946,#148947,#148948,#148949,#148950,#148951,#148952,
#148953,#148954,#148955,#148956,#148957,#148958,#148959,#148960,#148961,
#148962,#148963,#148964,#148965,#148966,#148967,#148968,#148969,#148970,
#148971,#148972,#148973,#148974,#148975,#148976,#148977,#148978,#148979,
#148980,#148981,#148982,#148983,#148984,#148985,#148986,#148987,#148988,
#148989,#148990,#148991,#148992,#148993,#148994,#148995,#148996,#148997,
#148998,#148999,#149000,#149001,#149002,#149003,#149004,#149005,#149006,
#149007,#149008,#149009,#149010,#149011,#149012,#149013,#149014,#149015,
#149016,#149017,#149018,#149019,#149020,#149021,#149022,#149023,#149024,
#149025,#149026,#149027,#149028,#149029,#149030,#149031,#149032,#149033,
#149034,#149035,#149036,#149037,#149038,#149039,#149040,#149041,#149042,
#149043,#149044,#149045,#149046,#149047,#149048,#149049,#149050,#149051,
#149052,#149053,#149054,#149055,#149056,#149057,#149058,#149059,#149060,
#149061,#149062,#149063,#149064,#149065,#149066,#149067,#149068,#149069,
#149070,#149071,#149072,#149073,#149074,#149075,#149076,#149077,#149078,
#149079,#149080,#149081,#149082,#149083,#149084,#149085,#149086,#149087,
#149088,#149089,#149090,#149091,#149092,#149093,#149094,#149095,#149096,
#149097,#149098,#149099,#149100,#149101,#149102,#149103,#149104,#149105,
#149106,#149107,#149108,#149109,#149110,#149111,#149112,#149113,#149114,
#149115,#149116,#149117,#149118,#149119,#149120,#149121,#149122,#149123,
#149124,#149125,#149126,#149127,#149128,#149129,#149130,#149131,#149132,
#149133,#149134,#149135,#149136,#149137,#149138,#149139,#149140,#149141,
#149142,#149143,#149144,#149145,#149146,#149147,#149148,#149149,#149150,
#149151,#149152,#149153,#149154,#149155,#149156,#149157,#149158,#149159,
#149160,#149161,#149162,#149163,#149164,#149165,#149166,#149167,#149168,
#149169,#149170,#149171,#149172,#149173,#149174,#149175,#149176,#149177,
#149178,#149179,#149180,#149181,#149182,#149183,#149184,#149185,#149186,
#149187,#149188,#149189,#149190,#149191,#149192,#149193,#149194,#149195,
#149196,#149197,#149198,#149199,#149200,#149201,#149202,#149203,#149204,
#149205,#149206,#149207,#149208,#149209,#149210,#149211,#149212,#149213,
#149214,#149215,#149216,#149217,#149218,#149219,#149220,#149221,#149222,
#149223,#149224,#149225,#149226,#149227,#149228,#149229,#149230,#149231,
#149232,#149233,#149234,#149235,#149236,#149237,#149238,#149239,#149240,
#149241,#149242,#149243,#149244,#149245,#149246,#149247,#149248,#149249,
#149250,#149251,#149252,#149253,#149254,#149255,#149256,#149257,#149258,
#149259,#149260,#149261,#149262,#149263,#149264,#149265,#149266,#149267,
#149268,#149269,#149270,#149271,#149272,#149273,#149274,#149275,#149276,
#149277,#149278,#149279,#149280,#149281,#149282,#149283,#149284,#149285,
#149286,#149287,#149288,#149289,#149290,#149291,#149292,#149293,#149294,
#149295,#149296,#149297,#149298,#149299,#149300,#149301,#149302,#149303,
#149304,#149305,#149306,#149307,#149308,#149309,#149310,#149311,#149312,
#149313,#149314,#149315,#149316,#149317,#149318,#149319,#149320,#149321,
#149322,#149323,#149324,#149325,#149326,#149327,#149328,#149329,#149330,
#149331,#149332,#149333,#149334,#149335,#149336,#149337,#149338,#149339,
#149340,#149341,#149342,#149343,#149344,#149345,#149346,#149347,#149348,
#149349,#149350,#149351,#149352,#149353,#149354,#149355,#149356,#149357,
#149358,#149359,#149360,#149361,#149362,#149363,#149364,#149365,#149366,
#149367,#149368,#149369,#149370,#149371,#149372,#149373,#149374,#149375,
#149376,#149377,#149378,#149379,#149380,#149381,#149382,#149383,#149384,
#149385,#149386,#149387,#149388,#149389,#149390,#149391,#149392,#149393,
#149394,#149395,#149396,#149397,#149398,#149399,#149400,#149401,#149402,
#149403,#149404,#149405,#149406,#149407,#149408,#149409,#149410,#149411,
#149412,#149413,#149414,#149415,#149416,#149417,#149418,#149419,#149420,
#149421,#149422,#149423,#149424,#149425,#149426,#149427,#149428,#149429,
#149430,#149431,#149432,#149433,#149434,#149435,#149436,#149437,#149438,
#149439,#149440,#149441,#149442,#149443,#149444,#149445,#149446,#149447,
#149448,#149449,#149450,#149451,#149452,#149453,#149454,#149455,#149456,
#149457,#149458,#149459,#149460,#149461,#149462,#149463,#149464,#149465,
#149466,#149467,#149468,#149469,#149470,#149471,#149472,#149473,#149474,
#149475,#149476,#149477,#149478,#149479,#149480,#149481,#149482,#149483,
#149484,#149485,#149486,#149487,#149488,#149489,#149490,#149491,#149492,
#149493,#149494,#149495,#149496,#149497,#149498,#149499,#149500,#149501,
#149502,#149503,#149504,#149505,#149506,#149507,#149508,#149509,#149510,
#149511,#149512,#149513,#149514,#149515,#149516,#149517,#149518,#149519,
#149520,#149521,#149522,#149523,#149524,#149525,#149526,#149527,#149528,
#149529,#149530,#149531,#149532,#149533,#149534,#149535,#149536,#149537,
#149538,#149539,#149540,#149541,#149542,#149543,#149544,#149545,#149546,
#149547,#149548,#149549,#149550,#149551,#149552,#149553,#149554,#149555,
#149556,#149557,#149558,#149559,#149560,#149561,#149562,#149563,#149564,
#149565,#149566,#149567,#149568,#149569,#149570,#149571,#149572,#149573,
#149574,#149575,#149576,#149577,#149578,#149579,#149580,#149581,#149582,
#149583,#149584,#149585,#149586,#149587,#149588,#149589,#149590,#149591,
#149592,#149593,#149594,#149595,#149596,#149597,#149598,#149599,#149600,
#149601,#149602,#149603,#149604,#149605,#149606,#149607,#149608,#149609,
#149610,#149611,#149612,#149613,#149614,#149615,#149616,#149617,#149618,
#149619,#149620,#149621,#149622,#149623,#149624,#149625,#149626,#149627,
#149628,#149629,#149630,#149631,#149632,#149633,#149634,#149635,#149636,
#149637,#149638,#149639,#149640,#149641,#149642,#149643,#149644,#149645,
#149646,#149647,#149648,#149649,#149650,#149651,#149652,#149653,#149654,
#149655,#149656,#149657,#149658,#149659,#149660,#149661,#149662,#149663,
#149664,#149665,#149666,#149667,#149668,#149669,#149670,#149671,#149672,
#149673,#149674,#149675,#149676,#149677,#149678,#149679,#149680,#149681,
#149682,#149683,#149684,#149685,#149686,#149687,#149688,#149689,#149690,
#149691,#149692,#149693,#149694,#149695,#149696,#149697,#149698,#149699,
#149700,#149701,#149702,#149703,#149704,#149705,#149706,#149707,#149708,
#149709,#149710,#149711,#149712,#149713,#149714,#149715,#149716,#149717,
#149718,#149719,#149720,#149721,#149722,#149723,#149724,#149725,#149726,
#149727,#149728,#149729,#149730,#149731,#149732,#149733,#149734,#149735,
#149736,#149737,#149738,#149739,#149740,#149741,#149742,#149743,#149744,
#149745,#149746,#149747,#149748,#149749,#149750,#149751,#149752,#149753,
#149754,#149755,#149756,#149757,#149758,#149759,#149760,#149761,#149762,
#149763,#149764,#149765,#149766,#149767,#149768,#149769,#149770,#149771,
#149772,#149773,#149774,#149775,#149776,#149777,#149778,#149779,#149780,
#149781,#149782,#149783,#149784,#149785,#149786,#149787,#149788,#149789,
#149790,#149791,#149792,#149793,#149794,#149795,#149796,#149797,#149798,
#149799,#149800,#149801,#149802,#149803,#149804,#149805,#149806,#149807,
#149808,#149809,#149810,#149811,#149812,#149813,#149814,#149815,#149816,
#149817,#149818,#149819,#149820,#149821,#149822,#149823,#149824,#149825,
#149826,#149827,#149828,#149829,#149830,#149831,#149832,#149833,#149834,
#149835,#149836,#149837,#149838,#149839,#149840)),.UNSPECIFIED.,.F.,.F.,
 .F.)
B_SPLINE_SURFACE_WITH_KNOTS((2,2),(3,2,2,2,2,2,2,2,2,2,2,2,2,2,2,2,2,2,
2,2,2,2,2,2,2,2,2,2,2,2,2,2,2,2,2,2,2,2,2,2,2,2,2,2,2,2,2,2,2,2,2,2,2,2,
2,2,2,2,2,2,2,2,2,2,2,2,2,2,2,2,2,2,2,2,2,2,2,2,2,2,2,2,2,2,2,2,2,2,2,2,
2,2,2,2,2,2,2,2,2,2,2,2,2,2,2,2,2,2,2,2,2,2,2,2,2,2,2,2,2,2,2,2,2,2,2,2,
2,2,2,2,2,2,2,2,2,2,2,2,2,2,2,2,2,2,2,2,2,2,2,2,2,2,2,2,2,2,2,2,2,2,2,2,
2,2,2,2,2,2,2,2,2,2,2,2,2,2,2,2,2,2,2,2,2,2,2,2,2,2,2,2,2,2,2,2,2,2,2,2,
2,2,2,2,2,2,2,2,2,2,2,2,2,2,2,2,2,2,2,2,2,2,2,2,2,2,2,2,2,2,2,2,2,2,2,2,
2,2,2,2,2,2,2,2,2,2,2,2,2,2,2,2,2,2,2,2,2,2,2,2,2,2,2,2,2,2,2,2,2,2,2,2,
2,2,2,2,2,2,2,2,2,2,2,2,2,2,2,2,2,2,2,2,2,2,2,2,2,2,2,2,2,2,2,2,2,2,2,2,
2,2,2,2,2,2,2,2,2,2,2,2,2,2,2,2,2,2,2,2,2,2,2,2,2,2,2,2,2,2,2,2,2,2,2,2,
2,2,2,2,2,2,2,2,2,2,2,2,2,2,2,2,2,2,2,2,2,2,2,2,2,2,2,2,2,2,2,2,2,2,2,2,
2,2,2,2,2,2,2,2,2,2,2,2,2,2,2,2,2,2,2,2,2,2,2,2,2,2,2,2,2,2,2,2,2,2,2,2,
2,2,2,2,2,2,2,2,2,2,2,2,2,2,2,2,2,2,2,2,2,2,2,2,2,2,2,2,2,2,2,2,2,2,2,2,
2,2,2,2,2,2,2,2,2,2,2,2,2,2,2,2,2,2,2,2,2,2,2,2,2,2,2,2,2,2,2,2,2,2,2,2,
2,2,2,2,2,2,2,2,2,2,2,2,2,2,2,2,2,2,2,2,2,2,2,2,2,2,2,2,2,2,2,2,2,2,2,2,
2,2,2,2,2,2,2,2,2,2,2,2,2,2,2,2,2,2,2,2,2,2,2,2,2,2,2,2,2,2,2,2,2,2,2,2,
2,2,2,2,2,2,2,2,2,2,2,2,2,2,2,2,2,2,2,2,2,2,2,2,2,2,2,2,2,2,2,2,2,2,2,2,
2,2,2,2,2,2,2,2,2,2,2,2,2,2,2,2,2,2,2,2,2,2,2,2,2,2,2,2,2,2,2,2,2,2,2,2,
2,2,2,2,2,2,2,2,2,2,2,2,2,2,2,2,2,2,2,2,2,2,2,2,2,2,2,2,2,2,2,2,2,2,2,2,
2,2,2,2,2,2,2,2,2,2,2,2,2,2,2,2,2,2,2,2,2,2,2,2,2,2,2,2,2,2,2,2,2,2,2,2,
2,2,2,2,2,2,2,2,2,2,2,2,2,2,2,2,2,2,2,2,2,2,2,2,2,2,2,2,2,2,2,2,2,2,2,2,
2,2,2,2,2,2,2,2,2,2,2,2,2,2,2,2,2,2,2,2,2,2,2,2,2,2,2,2,2,2,2,2,2,2,2,2,
2,2,2,2,2,2,2,2,2,2,2,2,2,2,2,2,2,2,2,2,2,2,2,2,2,2,2,2,2,2,2,2,2,2,2,2,
2,2,2,2,2,2,2,2,2,2,2,2,2,2,2,2,2,2,2,2,2,2,2,2,2,2,2,2,2,2,2,2,2,2,2,2,
2,2,2,2,2,2,2,2,2,2,2,2,2,2,2,2,2,2,2,2,2,2,2,2,2,2,2,2,2,2,2,2,2,2,2,2,
2,2,2,2,2,2,2,2,2,2,2,2,2,2,2,2,2,2,2,2,2,2,2,2,2,2,2,2,2,2,2,2,2,2,2,2,
2,2,2,2,2,2,2,2,2,2,2,2,2,2,2,2,2,2,2,2,2,2,2,2,2,2,2,2,2,2,2,2,2,2,2,2,
2,2,2,2,2,2,2,2,2,2,2,2,2,2,2,2,2,2,2,2,2,2,2,2,2,2,2,2,2,2,2,2,2,2,2,2,
2,2,2,2,2,2,2,2,2,2,2,2,2,2,2,2,3),(0.,1.),(0.,0.000980392156862745,0.00196078431372549,
0.00294117647058824,0.00392156862745098,0.00490196078431373,0.00588235294117647,
0.00686274509803922,0.00784313725490196,0.00882352941176471,0.00980392156862745,
0.0107843137254902,0.0117647058823529,0.0127450980392157,0.0137254901960784,
0.0147058823529412,0.0156862745098039,0.0166666666666667,0.0176470588235294,
0.0186274509803922,0.0196078431372549,0.0205882352941176,0.0215686274509804,
0.0225490196078431,0.0235294117647059,0.0245098039215686,0.0254901960784314,
0.0264705882352941,0.0274509803921569,0.0284313725490196,0.0294117647058824,
0.0303921568627451,0.0313725490196078,0.0323529411764706,0.0333333333333333,
0.0343137254901961,0.0352941176470588,0.0362745098039216,0.0372549019607843,
0.0382352941176471,0.0392156862745098,0.0401960784313726,0.0411764705882353,
0.042156862745098,0.0431372549019608,0.0441176470588235,0.0450980392156863,
0.046078431372549,0.0470588235294118,0.0480392156862745,0.0490196078431373,
0.05,0.0509803921568627,0.0519607843137255,0.0529411764705882,0.053921568627451,
0.0549019607843137,0.0558823529411765,0.0568627450980392,0.057843137254902,
0.0588235294117647,0.0598039215686275,0.0607843137254902,0.0617647058823529,
0.0627450980392157,0.0637254901960784,0.0647058823529412,0.0656862745098039,
0.0666666666666667,0.0676470588235294,0.0686274509803922,0.0696078431372549,
0.0705882352941176,0.0715686274509804,0.0725490196078431,0.0735294117647059,
0.0745098039215686,0.0754901960784314,0.0764705882352941,0.0774509803921569,
0.0784313725490196,0.0794117647058823,0.0803921568627451,0.0813725490196078,
0.0823529411764706,0.0833333333333333,0.0843137254901961,0.0852941176470588,
0.0862745098039216,0.0872549019607843,0.0882352941176471,0.0892156862745098,
0.0901960784313725,0.0911764705882353,0.092156862745098,0.0931372549019608,
0.0941176470588235,0.0950980392156863,0.096078431372549,0.0970588235294118,
0.0980392156862745,0.0990196078431373,0.1,0.100980392156863,0.101960784313725,
0.102941176470588,0.103921568627451,0.104901960784314,0.105882352941176,
0.106862745098039,0.107843137254902,0.108823529411765,0.109803921568627,
0.11078431372549,0.111764705882353,0.112745098039216,0.113725490196078,
0.114705882352941,0.115686274509804,0.116666666666667,0.117647058823529,
0.118627450980392,0.119607843137255,0.120588235294118,0.12156862745098,
0.122549019607843,0.123529411764706,0.124509803921569,0.125490196078431,
0.126470588235294,0.127450980392157,0.12843137254902,0.129411764705882,
0.130392156862745,0.131372549019608,0.132352941176471,0.133333333333333,
0.134313725490196,0.135294117647059,0.136274509803922,0.137254901960784,
0.138235294117647,0.13921568627451,0.140196078431373,0.141176470588235,
0.142156862745098,0.143137254901961,0.144117647058824,0.145098039215686,
0.146078431372549,0.147058823529412,0.148039215686275,0.149019607843137,
0.15,0.150980392156863,0.151960784313725,0.152941176470588,0.153921568627451,
0.154901960784314,0.155882352941176,0.156862745098039,0.157843137254902,
0.158823529411765,0.159803921568627,0.16078431372549,0.161764705882353,
0.162745098039216,0.163725490196078,0.164705882352941,0.165686274509804,
0.166666666666667,0.167647058823529,0.168627450980392,0.169607843137255,
0.170588235294118,0.17156862745098,0.172549019607843,0.173529411764706,
0.174509803921569,0.175490196078431,0.176470588235294,0.177450980392157,
0.17843137254902,0.179411764705882,0.180392156862745,0.181372549019608,
0.182352941176471,0.183333333333333,0.184313725490196,0.185294117647059,
0.186274509803922,0.187254901960784,0.188235294117647,0.18921568627451,
0.190196078431373,0.191176470588235,0.192156862745098,0.193137254901961,
0.194117647058824,0.195098039215686,0.196078431372549,0.197058823529412,
0.198039215686275,0.199019607843137,0.2,0.200980392156863,0.201960784313725,
0.202941176470588,0.203921568627451,0.204901960784314,0.205882352941176,
0.206862745098039,0.207843137254902,0.208823529411765,0.209803921568627,
0.21078431372549,0.211764705882353,0.212745098039216,0.213725490196078,
0.214705882352941,0.215686274509804,0.216666666666667,0.217647058823529,
0.218627450980392,0.219607843137255,0.220588235294118,0.22156862745098,
0.222549019607843,0.223529411764706,0.224509803921569,0.225490196078431,
0.226470588235294,0.227450980392157,0.22843137254902,0.229411764705882,
0.230392156862745,0.231372549019608,0.232352941176471,0.233333333333333,
0.234313725490196,0.235294117647059,0.236274509803922,0.237254901960784,
0.238235294117647,0.23921568627451,0.240196078431373,0.241176470588235,
0.242156862745098,0.243137254901961,0.244117647058824,0.245098039215686,
0.246078431372549,0.247058823529412,0.248039215686275,0.249019607843137,
0.25,0.250980392156863,0.251960784313725,0.252941176470588,0.253921568627451,
0.254901960784314,0.255882352941176,0.256862745098039,0.257843137254902,
0.258823529411765,0.259803921568627,0.26078431372549,0.261764705882353,
0.262745098039216,0.263725490196078,0.264705882352941,0.265686274509804,
0.266666666666667,0.267647058823529,0.268627450980392,0.269607843137255,
0.270588235294118,0.27156862745098,0.272549019607843,0.273529411764706,
0.274509803921569,0.275490196078431,0.276470588235294,0.277450980392157,
0.27843137254902,0.279411764705882,0.280392156862745,0.281372549019608,
0.282352941176471,0.283333333333333,0.284313725490196,0.285294117647059,
0.286274509803922,0.287254901960784,0.288235294117647,0.28921568627451,
0.290196078431373,0.291176470588235,0.292156862745098,0.293137254901961,
0.294117647058824,0.295098039215686,0.296078431372549,0.297058823529412,
0.298039215686275,0.299019607843137,0.3,0.300980392156863,0.301960784313725,
0.302941176470588,0.303921568627451,0.304901960784314,0.305882352941176,
0.306862745098039,0.307843137254902,0.308823529411765,0.309803921568627,
0.31078431372549,0.311764705882353,0.312745098039216,0.313725490196078,
0.314705882352941,0.315686274509804,0.316666666666667,0.317647058823529,
0.318627450980392,0.319607843137255,0.320588235294118,0.32156862745098,
0.322549019607843,0.323529411764706,0.324509803921569,0.325490196078431,
0.326470588235294,0.327450980392157,0.32843137254902,0.329411764705882,
0.330392156862745,0.331372549019608,0.332352941176471,0.333333333333333,
0.334313725490196,0.335294117647059,0.336274509803922,0.337254901960784,
0.338235294117647,0.33921568627451,0.340196078431373,0.341176470588235,
0.342156862745098,0.343137254901961,0.344117647058824,0.345098039215686,
0.346078431372549,0.347058823529412,0.348039215686274,0.349019607843137,
0.35,0.350980392156863,0.351960784313726,0.352941176470588,0.353921568627451,
0.354901960784314,0.355882352941176,0.356862745098039,0.357843137254902,
0.358823529411765,0.359803921568627,0.36078431372549,0.361764705882353,
0.362745098039216,0.363725490196078,0.364705882352941,0.365686274509804,
0.366666666666667,0.367647058823529,0.368627450980392,0.369607843137255,
0.370588235294118,0.37156862745098,0.372549019607843,0.373529411764706,
0.374509803921569,0.375490196078431,0.376470588235294,0.377450980392157,
0.37843137254902,0.379411764705882,0.380392156862745,0.381372549019608,
0.382352941176471,0.383333333333333,0.384313725490196,0.385294117647059,
0.386274509803922,0.387254901960784,0.388235294117647,0.38921568627451,
0.390196078431373,0.391176470588235,0.392156862745098,0.393137254901961,
0.394117647058824,0.395098039215686,0.396078431372549,0.397058823529412,
0.398039215686274,0.399019607843137,0.4,0.400980392156863,0.401960784313726,
0.402941176470588,0.403921568627451,0.404901960784314,0.405882352941176,
0.406862745098039,0.407843137254902,0.408823529411765,0.409803921568627,
0.41078431372549,0.411764705882353,0.412745098039216,0.413725490196078,
0.414705882352941,0.415686274509804,0.416666666666667,0.417647058823529,
0.418627450980392,0.419607843137255,0.420588235294118,0.42156862745098,
0.422549019607843,0.423529411764706,0.424509803921569,0.425490196078431,
0.426470588235294,0.427450980392157,0.42843137254902,0.429411764705882,
0.430392156862745,0.431372549019608,0.432352941176471,0.433333333333333,
0.434313725490196,0.435294117647059,0.436274509803922,0.437254901960784,
0.438235294117647,0.43921568627451,0.440196078431373,0.441176470588235,
0.442156862745098,0.443137254901961,0.444117647058824,0.445098039215686,
0.446078431372549,0.447058823529412,0.448039215686275,0.449019607843137,
0.45,0.450980392156863,0.451960784313725,0.452941176470588,0.453921568627451,
0.454901960784314,0.455882352941176,0.456862745098039,0.457843137254902,
0.458823529411765,0.459803921568627,0.46078431372549,0.461764705882353,
0.462745098039216,0.463725490196078,0.464705882352941,0.465686274509804,
0.466666666666667,0.467647058823529,0.468627450980392,0.469607843137255,
0.470588235294118,0.47156862745098,0.472549019607843,0.473529411764706,
0.474509803921569,0.475490196078431,0.476470588235294,0.477450980392157,
0.47843137254902,0.479411764705882,0.480392156862745,0.481372549019608,
0.482352941176471,0.483333333333333,0.484313725490196,0.485294117647059,
0.486274509803922,0.487254901960784,0.488235294117647,0.48921568627451,
0.490196078431373,0.491176470588235,0.492156862745098,0.493137254901961,
0.494117647058824,0.495098039215686,0.496078431372549,0.497058823529412,
0.498039215686275,0.499019607843137,0.5,0.500980392156863,0.501960784313725,
0.502941176470588,0.503921568627451,0.504901960784314,0.505882352941176,
0.506862745098039,0.507843137254902,0.508823529411765,0.509803921568627,
0.51078431372549,0.511764705882353,0.512745098039216,0.513725490196078,
0.514705882352941,0.515686274509804,0.516666666666667,0.517647058823529,
0.518627450980392,0.519607843137255,0.520588235294118,0.52156862745098,
0.522549019607843,0.523529411764706,0.524509803921569,0.525490196078431,
0.526470588235294,0.527450980392157,0.52843137254902,0.529411764705882,
0.530392156862745,0.531372549019608,0.532352941176471,0.533333333333333,
0.534313725490196,0.535294117647059,0.536274509803922,0.537254901960784,
0.538235294117647,0.53921568627451,0.540196078431373,0.541176470588235,
0.542156862745098,0.543137254901961,0.544117647058823,0.545098039215686,
0.546078431372549,0.547058823529412,0.548039215686275,0.549019607843137,
0.55,0.550980392156863,0.551960784313726,0.552941176470588,0.553921568627451,
0.554901960784314,0.555882352941176,0.556862745098039,0.557843137254902,
0.558823529411765,0.559803921568627,0.56078431372549,0.561764705882353,
0.562745098039216,0.563725490196078,0.564705882352941,0.565686274509804,
0.566666666666667,0.567647058823529,0.568627450980392,0.569607843137255,
0.570588235294118,0.57156862745098,0.572549019607843,0.573529411764706,
0.574509803921569,0.575490196078431,0.576470588235294,0.577450980392157,
0.57843137254902,0.579411764705882,0.580392156862745,0.581372549019608,
0.582352941176471,0.583333333333333,0.584313725490196,0.585294117647059,
0.586274509803922,0.587254901960784,0.588235294117647,0.58921568627451,
0.590196078431373,0.591176470588235,0.592156862745098,0.593137254901961,
0.594117647058824,0.595098039215686,0.596078431372549,0.597058823529412,
0.598039215686274,0.599019607843137,0.6,0.600980392156863,0.601960784313725,
0.602941176470588,0.603921568627451,0.604901960784314,0.605882352941176,
0.606862745098039,0.607843137254902,0.608823529411765,0.609803921568628,
0.61078431372549,0.611764705882353,0.612745098039216,0.613725490196078,
0.614705882352941,0.615686274509804,0.616666666666667,0.617647058823529,
0.618627450980392,0.619607843137255,0.620588235294118,0.62156862745098,
0.622549019607843,0.623529411764706,0.624509803921569,0.625490196078431,
0.626470588235294,0.627450980392157,0.62843137254902,0.629411764705882,
0.630392156862745,0.631372549019608,0.632352941176471,0.633333333333333,
0.634313725490196,0.635294117647059,0.636274509803922,0.637254901960784,
0.638235294117647,0.63921568627451,0.640196078431372,0.641176470588235,
0.642156862745098,0.643137254901961,0.644117647058824,0.645098039215686,
0.646078431372549,0.647058823529412,0.648039215686275,0.649019607843137,
0.65,0.650980392156863,0.651960784313726,0.652941176470588,0.653921568627451,
0.654901960784314,0.655882352941176,0.656862745098039,0.657843137254902,
0.658823529411765,0.659803921568627,0.66078431372549,0.661764705882353,
0.662745098039216,0.663725490196078,0.664705882352941,0.665686274509804,
0.666666666666667,0.667647058823529,0.668627450980392,0.669607843137255,
0.670588235294118,0.67156862745098,0.672549019607843,0.673529411764706,
0.674509803921569,0.675490196078431,0.676470588235294,0.677450980392157,
0.67843137254902,0.679411764705882,0.680392156862745,0.681372549019608,
0.682352941176471,0.683333333333333,0.684313725490196,0.685294117647059,
0.686274509803922,0.687254901960784,0.688235294117647,0.68921568627451,
0.690196078431373,0.691176470588235,0.692156862745098,0.693137254901961,
0.694117647058824,0.695098039215686,0.696078431372549,0.697058823529412,
0.698039215686274,0.699019607843137,0.7,0.700980392156863,0.701960784313725,
0.702941176470588,0.703921568627451,0.704901960784314,0.705882352941177,
0.706862745098039,0.707843137254902,0.708823529411765,0.709803921568627,
0.71078431372549,0.711764705882353,0.712745098039216,0.713725490196078,
0.714705882352941,0.715686274509804,0.716666666666667,0.717647058823529,
0.718627450980392,0.719607843137255,0.720588235294118,0.72156862745098,
0.722549019607843,0.723529411764706,0.724509803921569,0.725490196078431,
0.726470588235294,0.727450980392157,0.72843137254902,0.729411764705882,
0.730392156862745,0.731372549019608,0.732352941176471,0.733333333333333,
0.734313725490196,0.735294117647059,0.736274509803922,0.737254901960784,
0.738235294117647,0.73921568627451,0.740196078431373,0.741176470588235,
0.742156862745098,0.743137254901961,0.744117647058824,0.745098039215686,
0.746078431372549,0.747058823529412,0.748039215686275,0.749019607843137,
0.75,0.750980392156863,0.751960784313725,0.752941176470588,0.753921568627451,
0.754901960784314,0.755882352941176,0.756862745098039,0.757843137254902,
0.758823529411765,0.759803921568627,0.76078431372549,0.761764705882353,
0.762745098039216,0.763725490196078,0.764705882352941,0.765686274509804,
0.766666666666667,0.767647058823529,0.768627450980392,0.769607843137255,
0.770588235294118,0.77156862745098,0.772549019607843,0.773529411764706,
0.774509803921569,0.775490196078431,0.776470588235294,0.777450980392157,
0.77843137254902,0.779411764705882,0.780392156862745,0.781372549019608,
0.782352941176471,0.783333333333333,0.784313725490196,0.785294117647059,
0.786274509803922,0.787254901960784,0.788235294117647,0.78921568627451,
0.790196078431373,0.791176470588235,0.792156862745098,0.793137254901961,
0.794117647058823,0.795098039215686,0.796078431372549,0.797058823529412,
0.798039215686275,0.799019607843137,0.8,0.800980392156863,0.801960784313726,
0.802941176470588,0.803921568627451,0.804901960784314,0.805882352941176,
0.806862745098039,0.807843137254902,0.808823529411765,0.809803921568627,
0.81078431372549,0.811764705882353,0.812745098039216,0.813725490196078,
0.814705882352941,0.815686274509804,0.816666666666667,0.817647058823529,
0.818627450980392,0.819607843137255,0.820588235294118,0.82156862745098,
0.822549019607843,0.823529411764706,0.824509803921569,0.825490196078431,
0.826470588235294,0.827450980392157,0.82843137254902,0.829411764705882,
0.830392156862745,0.831372549019608,0.832352941176471,0.833333333333333,
0.834313725490196,0.835294117647059,0.836274509803922,0.837254901960784,
0.838235294117647,0.83921568627451,0.840196078431373,0.841176470588235,
0.842156862745098,0.843137254901961,0.844117647058824,0.845098039215686,
0.846078431372549,0.847058823529412,0.848039215686274,0.849019607843137,
0.85,0.850980392156863,0.851960784313725,0.852941176470588,0.853921568627451,
0.854901960784314,0.855882352941176,0.856862745098039,0.857843137254902,
0.858823529411765,0.859803921568628,0.86078431372549,0.861764705882353,
0.862745098039216,0.863725490196078,0.864705882352941,0.865686274509804,
0.866666666666667,0.867647058823529,0.868627450980392,0.869607843137255,
0.870588235294118,0.87156862745098,0.872549019607843,0.873529411764706,
0.874509803921569,0.875490196078431,0.876470588235294,0.877450980392157,
0.87843137254902,0.879411764705882,0.880392156862745,0.881372549019608,
0.882352941176471,0.883333333333333,0.884313725490196,0.885294117647059,
0.886274509803922,0.887254901960784,0.888235294117647,0.88921568627451,
0.890196078431372,0.891176470588235,0.892156862745098,0.893137254901961,
0.894117647058824,0.895098039215686,0.896078431372549,0.897058823529412,
0.898039215686275,0.899019607843137,0.9,0.900980392156863,0.901960784313726,
0.902941176470588,0.903921568627451,0.904901960784314,0.905882352941176,
0.906862745098039,0.907843137254902,0.908823529411765,0.909803921568627,
0.91078431372549,0.911764705882353,0.912745098039216,0.913725490196078,
0.914705882352941,0.915686274509804,0.916666666666667,0.917647058823529,
0.918627450980392,0.919607843137255,0.920588235294118,0.92156862745098,
0.922549019607843,0.923529411764706,0.924509803921569,0.925490196078431,
0.926470588235294,0.927450980392157,0.92843137254902,0.929411764705882,
0.930392156862745,0.931372549019608,0.932352941176471,0.933333333333333,
0.934313725490196,0.935294117647059,0.936274509803922,0.937254901960784,
0.938235294117647,0.93921568627451,0.940196078431373,0.941176470588235,
0.942156862745098,0.943137254901961,0.944117647058824,0.945098039215686,
0.946078431372549,0.947058823529412,0.948039215686274,0.949019607843137,
0.95,0.950980392156863,0.951960784313725,0.952941176470588,0.953921568627451,
0.954901960784314,0.955882352941177,0.956862745098039,0.957843137254902,
0.958823529411765,0.959803921568627,0.96078431372549,0.961764705882353,
0.962745098039216,0.963725490196078,0.964705882352941,0.965686274509804,
0.966666666666667,0.967647058823529,0.968627450980392,0.969607843137255,
0.970588235294118,0.97156862745098,0.972549019607843,0.973529411764706,
0.974509803921569,0.975490196078431,0.976470588235294,0.977450980392157,
0.97843137254902,0.979411764705882,0.980392156862745,0.981372549019608,
0.982352941176471,0.983333333333333,0.984313725490196,0.985294117647059,
0.985937383514281),.UNSPECIFIED.)
GEOMETRIC_REPRESENTATION_ITEM()
RATIONAL_B_SPLINE_SURFACE(((1.,0.995734176295034,1.,0.995734176295034,1.,
0.995734176295034,1.,0.995734176295034,1.,0.995734176295034,1.,0.995734176295034,
1.,0.995734176295034,1.,0.995734176295034,1.,0.995734176295034,1.,0.995734176295034,
1.,0.995734176295034,1.,0.995734176295034,1.,0.995734176295034,1.,0.995734176295034,
1.,0.995734176295034,1.,0.995734176295034,1.,0.995734176295034,1.,0.995734176295034,
1.,0.995734176295034,1.,0.995734176295034,1.,0.995734176295034,1.,0.995734176295034,
1.,0.995734176295034,1.,0.995734176295034,1.,0.995734176295034,1.,0.995734176295034,
1.,0.995734176295034,1.,0.995734176295034,1.,0.995734176295034,1.,0.995734176295034,
1.,0.995734176295034,1.,0.995734176295034,1.,0.995734176295034,1.,0.995734176295034,
1.,0.995734176295034,1.,0.995734176295034,1.,0.995734176295034,1.,0.995734176295034,
1.,0.995734176295034,1.,0.995734176295034,1.,0.995734176295034,1.,0.995734176295034,
1.,0.995734176295034,1.,0.995734176295034,1.,0.995734176295034,1.,0.995734176295034,
1.,0.995734176295034,1.,0.995734176295034,1.,0.995734176295034,1.,0.995734176295034,
1.,0.995734176295034,1.,0.995734176295034,1.,0.995734176295034,1.,0.995734176295034,
1.,0.995734176295034,1.,0.995734176295034,1.,0.995734176295034,1.,0.995734176295034,
1.,0.995734176295034,1.,0.995734176295034,1.,0.995734176295034,1.,0.995734176295034,
1.,0.995734176295034,1.,0.995734176295034,1.,0.995734176295034,1.,0.995734176295034,
1.,0.995734176295034,1.,0.995734176295034,1.,0.995734176295034,1.,0.995734176295034,
1.,0.995734176295034,1.,0.995734176295034,1.,0.995734176295034,1.,0.995734176295034,
1.,0.995734176295034,1.,0.995734176295034,1.,0.995734176295034,1.,0.995734176295034,
1.,0.995734176295034,1.,0.995734176295034,1.,0.995734176295034,1.,0.995734176295034,
1.,0.995734176295034,1.,0.995734176295034,1.,0.995734176295034,1.,0.995734176295034,
1.,0.995734176295034,1.,0.995734176295034,1.,0.995734176295034,1.,0.995734176295034,
1.,0.995734176295034,1.,0.995734176295034,1.,0.995734176295034,1.,0.995734176295034,
1.,0.995734176295034,1.,0.995734176295034,1.,0.995734176295034,1.,0.995734176295034,
1.,0.995734176295034,1.,0.995734176295034,1.,0.995734176295034,1.,0.995734176295034,
1.,0.995734176295034,1.,0.995734176295034,1.,0.995734176295034,1.,0.995734176295034,
1.,0.995734176295034,1.,0.995734176295034,1.,0.995734176295034,1.,0.995734176295034,
1.,0.995734176295034,1.,0.995734176295034,1.,0.995734176295034,1.,0.995734176295034,
1.,0.995734176295034,1.,0.995734176295034,1.,0.995734176295034,1.,0.995734176295034,
1.,0.995734176295034,1.,0.995734176295034,1.,0.995734176295034,1.,0.995734176295034,
1.,0.995734176295034,1.,0.995734176295034,1.,0.995734176295034,1.,0.995734176295034,
1.,0.995734176295034,1.,0.995734176295034,1.,0.995734176295034,1.,0.995734176295034,
1.,0.995734176295034,1.,0.995734176295034,1.,0.995734176295034,1.,0.995734176295034,
1.,0.995734176295034,1.,0.995734176295034,1.,0.995734176295034,1.,0.995734176295034,
1.,0.995734176295034,1.,0.995734176295034,1.,0.995734176295034,1.,0.995734176295034,
1.,0.995734176295034,1.,0.995734176295034,1.,0.995734176295034,1.,0.995734176295034,
1.,0.995734176295034,1.,0.995734176295034,1.,0.995734176295034,1.,0.995734176295034,
1.,0.995734176295034,1.,0.995734176295034,1.,0.995734176295034,1.,0.995734176295034,
1.,0.995734176295034,1.,0.995734176295034,1.,0.995734176295034,1.,0.995734176295034,
1.,0.995734176295034,1.,0.995734176295034,1.,0.995734176295034,1.,0.995734176295034,
1.,0.995734176295034,1.,0.995734176295034,1.,0.995734176295034,1.,0.995734176295034,
1.,0.995734176295034,1.,0.995734176295034,1.,0.995734176295034,1.,0.995734176295034,
1.,0.995734176295034,1.,0.995734176295034,1.,0.995734176295034,1.,0.995734176295034,
1.,0.995734176295034,1.,0.995734176295034,1.,0.995734176295034,1.,0.995734176295034,
1.,0.995734176295034,1.,0.995734176295034,1.,0.995734176295034,1.,0.995734176295034,
1.,0.995734176295034,1.,0.995734176295034,1.,0.995734176295034,1.,0.995734176295034,
1.,0.995734176295034,1.,0.995734176295034,1.,0.995734176295034,1.,0.995734176295034,
1.,0.995734176295034,1.,0.995734176295034,1.,0.995734176295034,1.,0.995734176295034,
1.,0.995734176295034,1.,0.995734176295034,1.,0.995734176295034,1.,0.995734176295034,
1.,0.995734176295034,1.,0.995734176295034,1.,0.995734176295034,1.,0.995734176295034,
1.,0.995734176295034,1.,0.995734176295034,1.,0.995734176295034,1.,0.995734176295034,
1.,0.995734176295034,1.,0.995734176295034,1.,0.995734176295034,1.,0.995734176295034,
1.,0.995734176295034,1.,0.995734176295034,1.,0.995734176295034,1.,0.995734176295034,
1.,0.995734176295034,1.,0.995734176295034,1.,0.995734176295034,1.,0.995734176295034,
1.,0.995734176295034,1.,0.995734176295034,1.,0.995734176295034,1.,0.995734176295034,
1.,0.995734176295034,1.,0.995734176295034,1.,0.995734176295034,1.,0.995734176295034,
1.,0.995734176295034,1.,0.995734176295034,1.,0.995734176295034,1.,0.995734176295034,
1.,0.995734176295034,1.,0.995734176295034,1.,0.995734176295034,1.,0.995734176295034,
1.,0.995734176295034,1.,0.995734176295034,1.,0.995734176295034,1.,0.995734176295034,
1.,0.995734176295034,1.,0.995734176295034,1.,0.995734176295034,1.,0.995734176295034,
1.,0.995734176295034,1.,0.995734176295034,1.,0.995734176295034,1.,0.995734176295034,
1.,0.995734176295034,1.,0.995734176295034,1.,0.995734176295034,1.,0.995734176295034,
1.,0.995734176295034,1.,0.995734176295034,1.,0.995734176295034,1.,0.995734176295034,
1.,0.995734176295034,1.,0.995734176295034,1.,0.995734176295034,1.,0.995734176295034,
1.,0.995734176295034,1.,0.995734176295034,1.,0.995734176295034,1.,0.995734176295034,
1.,0.995734176295034,1.,0.995734176295034,1.,0.995734176295034,1.,0.995734176295034,
1.,0.995734176295034,1.,0.995734176295034,1.,0.995734176295034,1.,0.995734176295034,
1.,0.995734176295034,1.,0.995734176295034,1.,0.995734176295034,1.,0.995734176295034,
1.,0.995734176295034,1.,0.995734176295034,1.,0.995734176295034,1.,0.995734176295034,
1.,0.995734176295034,1.,0.995734176295034,1.,0.995734176295034,1.,0.995734176295034,
1.,0.995734176295034,1.,0.995734176295034,1.,0.995734176295034,1.,0.995734176295034,
1.,0.995734176295034,1.,0.995734176295034,1.,0.995734176295034,1.,0.995734176295034,
1.,0.995734176295034,1.,0.995734176295034,1.,0.995734176295034,1.,0.995734176295034,
1.,0.995734176295034,1.,0.995734176295034,1.,0.995734176295034,1.,0.995734176295034,
1.,0.995734176295034,1.,0.995734176295034,1.,0.995734176295034,1.,0.995734176295034,
1.,0.995734176295034,1.,0.995734176295034,1.,0.995734176295034,1.,0.995734176295034,
1.,0.995734176295034,1.,0.995734176295034,1.,0.995734176295034,1.,0.995734176295034,
1.,0.995734176295034,1.,0.995734176295034,1.,0.995734176295034,1.,0.995734176295034,
1.,0.995734176295034,1.,0.995734176295034,1.,0.995734176295034,1.,0.995734176295034,
1.,0.995734176295034,1.,0.995734176295034,1.,0.995734176295034,1.,0.995734176295034,
1.,0.995734176295034,1.,0.995734176295034,1.,0.995734176295034,1.,0.995734176295034,
1.,0.995734176295034,1.,0.995734176295034,1.,0.995734176295034,1.,0.995734176295034,
1.,0.995734176295034,1.,0.995734176295034,1.,0.995734176295034,1.,0.995734176295034,
1.,0.995734176295034,1.,0.995734176295034,1.,0.995734176295034,1.,0.995734176295034,
1.,0.995734176295034,1.,0.995734176295034,1.,0.995734176295034,1.,0.995734176295034,
1.,0.995734176295034,1.,0.995734176295034,1.,0.995734176295034,1.,0.995734176295034,
1.,0.995734176295034,1.,0.995734176295034,1.,0.995734176295034,1.,0.995734176295034,
1.,0.995734176295034,1.,0.995734176295034,1.,0.995734176295034,1.,0.995734176295034,
1.,0.995734176295034,1.,0.995734176295034,1.,0.995734176295034,1.,0.995734176295034,
1.,0.995734176295034,1.,0.995734176295034,1.,0.995734176295034,1.,0.995734176295034,
1.,0.995734176295034,1.,0.995734176295034,1.,0.995734176295034,1.,0.995734176295034,
1.,0.995734176295034,1.,0.995734176295034,1.,0.995734176295034,1.,0.995734176295034,
1.,0.995734176295034,1.,0.995734176295034,1.,0.995734176295034,1.,0.995734176295034,
1.,0.995734176295034,1.,0.995734176295034,1.,0.995734176295034,1.,0.995734176295034,
1.,0.995734176295034,1.,0.995734176295034,1.,0.995734176295034,1.,0.995734176295034,
1.,0.995734176295034,1.,0.995734176295034,1.,0.995734176295034,1.,0.995734176295034,
1.,0.995734176295034,1.,0.995734176295034,1.,0.995734176295034,1.,0.995734176295034,
1.,0.995734176295034,1.,0.995734176295034,1.,0.995734176295034,1.,0.995734176295034,
1.,0.995734176295034,1.,0.995734176295034,1.,0.995734176295034,1.,0.995734176295034,
1.,0.995734176295034,1.,0.995734176295034,1.,0.995734176295034,1.,0.995734176295034,
1.,0.995734176295034,1.,0.995734176295034,1.,0.995734176295034,1.,0.995734176295034,
1.,0.995734176295034,1.,0.995734176295034,1.,0.995734176295034,1.,0.995734176295034,
1.,0.995734176295034,1.,0.995734176295034,1.,0.995734176295034,1.,0.995734176295034,
1.,0.995734176295034,1.,0.995734176295034,1.,0.995734176295034,1.,0.995734176295034,
1.,0.995734176295034,1.,0.995734176295034,1.,0.995734176295034,1.,0.995734176295034,
1.,0.995734176295034,1.,0.995734176295034,1.,0.995734176295034,1.,0.995734176295034,
1.,0.995734176295034,1.,0.995734176295034,1.,0.995734176295034,1.,0.995734176295034,
1.,0.995734176295034,1.,0.995734176295034,1.,0.995734176295034,1.,0.995734176295034,
1.,0.995734176295034,1.,0.995734176295034,1.,0.995734176295034,1.,0.995734176295034,
1.,0.995734176295034,1.,0.995734176295034,1.,0.995734176295034,1.,0.995734176295034,
1.,0.995734176295034,1.,0.995734176295034,1.,0.995734176295034,1.,0.995734176295034,
1.,0.995734176295034,1.,0.995734176295034,1.,0.995734176295034,1.,0.995734176295034,
1.,0.995734176295034,1.,0.995734176295034,1.,0.995734176295034,1.,0.995734176295034,
1.,0.995734176295034,1.,0.995734176295034,1.,0.995734176295034,1.,0.995734176295034,
1.,0.995734176295034,1.,0.995734176295034,1.,0.995734176295034,1.,0.995734176295034,
1.,0.995734176295034,1.,0.995734176295034,1.,0.995734176295034,1.,0.995734176295034,
1.,0.995734176295034,1.,0.995734176295034,1.,0.995734176295034,1.,0.995734176295034,
1.,0.995734176295034,1.,0.995734176295034,1.,0.995734176295034,1.,0.995734176295034,
1.,0.995734176295034,1.,0.995734176295034,1.,0.995734176295034,1.,0.995734176295034,
1.,0.995734176295034,1.,0.995734176295034,1.,0.995734176295034,1.,0.995734176295034,
1.,0.995734176295034,1.,0.995734176295034,1.,0.995734176295034,1.,0.995734176295034,
1.,0.995734176295034,1.,0.995734176295034,1.,0.995734176295034,1.,0.995734176295034,
1.,0.995734176295034,1.,0.995734176295034,1.,0.995734176295034,1.,0.995734176295034,
1.,0.995734176295034,1.,0.995734176295034,1.,0.995734176295034,1.,0.995734176295034,
1.,0.995734176295034,1.,0.995734176295034,1.,0.995734176295034,1.,0.995734176295034,
1.,0.995734176295034,1.,0.995734176295034,1.,0.995734176295034,1.,0.995734176295034,
1.,0.995734176295034,1.,0.995734176295034,1.,0.995734176295034,1.,0.995734176295034,
1.,0.995734176295034,1.,0.995734176295034,1.,0.995734176295034,1.,0.995734176295034,
1.,0.995734176295034,1.,0.995734176295034,1.,0.995734176295034,1.,0.995734176295034,
1.,0.995734176295034,1.,0.995734176295034,1.,0.995734176295034,1.,0.995734176295034,
1.,0.995734176295034,1.,0.995734176295034,1.,0.995734176295034,1.,0.995734176295034,
1.,0.995734176295034,1.,0.995734176295034,1.,0.995734176295034,1.,0.995734176295034,
1.,0.995734176295034,1.,0.995734176295034,1.,0.995734176295034,1.,0.995734176295034,
1.,0.995734176295034,1.,0.995734176295034,1.,0.995734176295034,1.,0.995734176295034,
1.,0.995734176295034,1.,0.995734176295034,1.,0.995734176295034,1.,0.995734176295034,
1.,0.995734176295034,1.,0.995734176295034,1.,0.995734176295034,1.,0.995734176295034,
1.,0.995734176295034,1.,0.995734176295034,1.,0.995734176295034,1.,0.995734176295034,
1.,0.995734176295034,1.,0.995734176295034,1.,0.995734176295034,1.,0.995734176295034,
1.,0.995734176295034,1.,0.995734176295034,1.,0.995734176295034,1.,0.995734176295034,
1.,0.995734176295034,1.,0.995734176295034,1.,0.995734176295034,1.,0.995734176295034,
1.,0.995734176295034,1.,0.995734176295034,1.,0.995734176295034,1.,0.995734176295034,
1.,0.995734176295034,1.,0.995734176295034,1.,0.995734176295034,1.,0.995734176295034,
1.,0.995734176295034,1.,0.995734176295034,1.,0.995734176295034,1.,0.995734176295034,
1.,0.995734176295034,1.,0.995734176295034,1.,0.995734176295034,1.,0.995734176295034,
1.,0.995734176295034,1.,0.995734176295034,1.,0.995734176295034,1.,0.995734176295034,
1.,0.995734176295034,1.,0.995734176295034,1.,0.995734176295034,1.,0.995734176295034,
1.,0.995734176295034,1.,0.995734176295034,1.,0.995734176295034,1.,0.995734176295034,
1.,0.995734176295034,1.,0.995734176295034,1.,0.995734176295034,1.,0.995734176295034,
1.,0.995734176295034,1.,0.995734176295034,1.,0.995734176295034,1.,0.995734176295034,
1.,0.995734176295034,1.,0.995734176295034,1.,0.995734176295034,1.,0.995734176295034,
1.,0.995734176295034,1.,0.995734176295034,1.,0.995734176295034,1.,0.995734176295034,
1.,0.995734176295034,1.,0.995734176295034,1.,0.995734176295034,1.,0.995734176295034,
1.,0.995734176295034,1.,0.995734176295034,1.,0.995734176295034,1.,0.995734176295034,
1.,0.995734176295034,1.,0.995734176295034,1.,0.995734176295034,1.,0.995734176295034,
1.,0.995734176295034,1.,0.995734176295034,1.,0.995734176295034,1.,0.995734176295034,
1.,0.995734176295034,1.,0.995734176295034,1.,0.995734176295034,1.,0.995734176295034,
1.,0.995734176295034,1.,0.995734176295034,1.,0.995734176295034,1.,0.995734176295034,
1.,0.995734176295034,1.,0.995734176295034,1.,0.995734176295034,1.,0.995734176295034,
1.,0.995734176295034,1.,0.995734176295034,1.,0.995734176295034,1.,0.995734176295034,
1.,0.995734176295034,1.,0.995734176295034,1.,0.995734176295034,1.,0.995734176295034,
1.,0.995734176295034,1.,0.995734176295034,1.,0.995734176295034,1.,0.995734176295034,
1.,0.995734176295034,1.,0.995734176295034,1.,0.995734176295034,1.,0.995734176295034,
1.,0.995734176295034,1.,0.995734176295034,1.,0.995734176295034,1.,0.995734176295034,
1.,0.995734176295034,1.,0.995734176295034,1.,0.995734176295034,1.,0.995734176295034,
1.,0.995734176295034,1.,0.995734176295034,1.,0.995734176295034,1.,0.995734176295034,
1.,0.995734176295034,1.,0.995734176295034,1.,0.995734176295034,1.,0.995734176295034,
1.,0.995734176295034,1.,0.995734176295034,1.,0.995734176295034,1.,0.995734176295034,
1.,0.995734176295034,1.,0.995734176295034,1.,0.995734176295034,1.,0.995734176295034,
1.,0.995734176295034,1.,0.995734176295034,1.,0.995734176295034,1.,0.995734176295034,
1.,0.995734176295034,1.,0.995734176295034,1.,0.995734176295034,1.,0.995734176295034,
1.,0.995734176295034,1.,0.995734176295034,1.,0.995734176295034,1.,0.995734176295034,
1.,0.995734176295034,1.,0.995734176295034,1.,0.995734176295034,1.,0.995734176295034,
1.,0.995734176295034,1.,0.995734176295034,1.,0.995734176295034,1.,0.995734176295034,
1.,0.995734176295034,1.,0.995734176295034,1.,0.995734176295034,1.,0.995734176295034,
1.,0.995734176295034,1.,0.995734176295034,1.,0.995734176295034,1.,0.995734176295034,
1.,0.995734176295034,1.,0.995734176295034,1.,0.995734176295034,1.,0.995734176295034,
1.,0.995734176295034,1.,0.995734176295034,1.,0.995734176295034,1.,0.995734176295034,
1.,0.995734176295034,1.,0.995734176295034,1.,0.995734176295034,1.,0.995734176295034,
1.,0.995734176295034,1.,0.995734176295034,1.,0.995734176295034,1.,0.995734176295034,
1.,0.995734176295034,1.,0.995734176295034,1.,0.995734176295034,1.,0.995734176295034,
1.,0.995734176295034,1.,0.995734176295034,1.,0.995734176295034,1.,0.995734176295034,
1.,0.995734176295034,1.,0.995734176295034,1.,0.995734176295034,1.,0.995734176295034,
1.,0.995734176295034,1.,0.995734176295034,1.,0.995734176295034,1.,0.995734176295034,
1.,0.995734176295034,1.,0.995734176295034,1.,0.995734176295034,1.,0.995734176295034,
1.,0.995734176295034,1.,0.995734176295034,1.,0.995734176295034,1.,0.995734176295034,
1.,0.995734176295034,1.,0.995734176295034,1.,0.995734176295034,1.,0.995734176295034,
1.,0.995734176295034,1.,0.995734176295034,1.,0.995734176295034,1.,0.995734176295034,
1.,0.995734176295034,1.,0.995734176295034,1.,0.995734176295034,1.,0.995734176295034,
1.,0.995734176295034,1.,0.995734176295034,1.,0.995734176295034,1.,0.995734176295034,
1.,0.995734176295034,1.,0.995734176295034,1.,0.995734176295034,1.,0.995734176295034,
1.,0.995734176295034,1.,0.995734176295034,1.,0.995734176295034,1.,0.995734176295034,
1.,0.995734176295034,1.,0.995734176295034,1.,0.995734176295034,1.,0.995734176295034,
1.,0.995734176295034,1.,0.995734176295034,1.,0.995734176295034,1.,0.995734176295034,
1.,0.995734176295034,1.,0.995734176295034,1.,0.995734176295034,1.,0.995734176295034,
1.,0.995734176295034,1.,0.995734176295034,1.,0.995734176295034,1.,0.995734176295034,
1.,0.995734176295034,1.,0.995734176295034,1.,0.995734176295034,1.,0.995734176295034,
1.,0.995734176295034,1.,0.995734176295034,1.,0.995734176295034,1.,0.995734176295034,
1.,0.995734176295034,1.,0.995734176295034,1.,0.995734176295034,1.,0.995734176295034,
1.,0.995734176295034,1.,0.995734176295034,1.,0.995734176295034,1.,0.995734176295034,
1.,0.995734176295034,1.,0.995734176295034,1.,0.995734176295034,1.,0.995734176295034,
1.,0.995734176295034,1.,0.995734176295034,1.,0.995734176295034,1.,0.995734176295034,
1.,0.995734176295034,1.,0.995734176295034,1.,0.995734176295034,1.,0.995734176295034,
1.,0.995734176295034,1.,0.995734176295034,1.,0.995734176295034,1.,0.995734176295034,
1.,0.995734176295034,1.,0.995734176295034,1.,0.995734176295034,1.,0.995734176295034,
1.,0.995734176295034,1.,0.995734176295034,1.,0.995734176295034,1.,0.995734176295034,
1.,0.995734176295034,1.,0.995734176295034,1.,0.995734176295034,1.,0.995734176295034,
1.,0.995734176295034,1.,0.995734176295034,1.,0.995734176295034,1.,0.995734176295034,
1.,0.995734176295034,1.,0.995734176295034,1.,0.995734176295034,1.,0.995734176295034,
1.,0.995734176295034,1.,0.995734176295034,1.,0.995734176295034,1.,0.995734176295034,
1.,0.995734176295034,1.,0.995734176295034,1.,0.995734176295034,1.,0.995734176295034,
1.,0.995734176295034,1.,0.995734176295034,1.,0.995734176295034,1.,0.995734176295034,
1.,0.995734176295034,1.,0.995734176295034,1.,0.995734176295034,1.,0.995734176295034,
1.,0.995734176295034,1.,0.995734176295034,1.,0.995734176295034,1.,0.995734176295034,
1.,0.995734176295034,1.,0.995734176295034,1.,0.995734176295034,1.,0.995734176295034,
1.,0.995734176295034,1.,0.995734176295034,1.,0.995734176295034,1.,0.995734176295034,
1.,0.995734176295034,1.,0.995734176295034,1.,0.995734176295034,1.,0.995734176295034,
1.,0.995734176295034,1.,0.995734176295034,1.,0.995734176295034,1.,0.995734176295034,
1.,0.995734176295034,1.,0.995734176295034,1.,0.995734176295034,1.,0.995734176295034,
1.,0.995734176295034,1.,0.995734176295034,1.,0.995734176295034,1.,0.995734176295034,
1.,0.995734176295034,1.,0.995734176295034,1.,0.995734176295034,1.,0.995734176295034,
1.,0.995734176295034,1.,0.995734176295034,1.,0.995734176295034,1.,0.995734176295034,
1.,0.995734176295034,1.,0.995734176295034,1.,0.995734176295034,1.,0.995734176295034,
1.,0.995734176295034,1.,0.995734176295034,1.,0.995734176295034,1.,0.995734176295034,
1.,0.995734176295034,1.,0.995734176295034,1.,0.995734176295034,1.,0.995734176295034,
1.,0.995734176295034,1.,0.995734176295034,1.,0.995734176295034,1.,0.995734176295034,
1.,0.995734176295034,1.,0.995734176295034,1.,0.995734176295034,1.,0.995734176295034,
1.,0.995734176295034,1.,0.995734176295034,1.,0.995734176295034,1.,0.995734176295034,
1.,0.995734176295034,1.,0.995734176295034,1.,0.995734176295034,1.,0.995734176295034,
1.,0.995734176295034,1.,0.995734176295034,1.,0.995734176295034,1.,0.995734176295034,
1.,0.995734176295034,1.,0.995734176295034,1.,0.995734176295034,1.,0.995734176295034,
1.,0.995734176295034,1.,0.995734176295034,1.,0.995734176295034,1.,0.995734176295034,
1.,0.995734176295034,1.,0.995734176295034,1.,0.995734176295034,1.,0.995734176295034,
1.,0.995734176295034,1.,0.995734176295034,1.,0.995734176295034,1.,0.995734176295034,
1.,0.995734176295034,1.,0.995734176295034,1.,0.995734176295034,1.,0.995734176295034,
1.,0.995734176295034,1.,0.995734176295034,1.,0.995734176295034,1.,0.995734176295034,
1.,0.995734176295034,1.,0.995734176295034,1.,0.995734176295034,1.,0.995734176295034,
1.,0.995734176295034,1.,0.995734176295034,1.,0.995734176295034,1.,0.995734176295034,
1.,0.995734176295034,1.,0.995734176295034,1.,0.995734176295034,1.,0.995734176295034,
1.,0.995734176295034,1.,0.995734176295034,1.,0.995734176295034,1.,0.995734176295034,
1.,0.995734176295034,1.,0.995734176295034,1.,0.995734176295034,1.,0.995734176295034,
1.,0.995734176295034,1.,0.995734176295034,1.,0.995734176295034,1.,0.995734176295034,
1.,0.995734176295034,1.,0.995734176295034,1.,0.995734176295034,1.,0.995734176295034,
1.,0.995734176295034,1.,0.995734176295034,1.,0.995734176295034,1.,0.995734176295034,
1.,0.995734176295034,1.,0.995734176295034,1.,0.995734176295034,1.,0.995734176295034,
1.,0.995734176295034,1.,0.995734176295034,1.,0.995734176295034,1.,0.995734176295034,
1.,0.995734176295034,1.,0.995734176295034,1.,0.995734176295034,1.,0.995734176295034,
1.,0.995734176295034,1.,0.995734176295034,1.,0.995734176295034,1.,0.995734176295034,
1.,0.995734176295034,1.,0.995734176295034,1.,0.995734176295034,1.,0.995734176295034,
1.,0.995734176295034,1.,0.995734176295034,1.,0.995734176295034,1.,0.995734176295034,
1.,0.995734176295034,1.,0.995734176295034,1.,0.995734176295034,1.,0.995734176295034,
1.,0.995734176295034,1.,0.995734176295034,1.,0.995734176295034,1.,0.99720106003931,
0.998075063662495),(1.,0.995734176295034,1.,0.995734176295034,1.,0.995734176295034,
1.,0.995734176295034,1.,0.995734176295034,1.,0.995734176295034,1.,0.995734176295034,
1.,0.995734176295034,1.,0.995734176295034,1.,0.995734176295034,1.,0.995734176295034,
1.,0.995734176295034,1.,0.995734176295034,1.,0.995734176295034,1.,0.995734176295034,
1.,0.995734176295034,1.,0.995734176295034,1.,0.995734176295034,1.,0.995734176295034,
1.,0.995734176295034,1.,0.995734176295034,1.,0.995734176295034,1.,0.995734176295034,
1.,0.995734176295034,1.,0.995734176295034,1.,0.995734176295034,1.,0.995734176295034,
1.,0.995734176295034,1.,0.995734176295034,1.,0.995734176295034,1.,0.995734176295034,
1.,0.995734176295034,1.,0.995734176295034,1.,0.995734176295034,1.,0.995734176295034,
1.,0.995734176295034,1.,0.995734176295034,1.,0.995734176295034,1.,0.995734176295034,
1.,0.995734176295034,1.,0.995734176295034,1.,0.995734176295034,1.,0.995734176295034,
1.,0.995734176295034,1.,0.995734176295034,1.,0.995734176295034,1.,0.995734176295034,
1.,0.995734176295034,1.,0.995734176295034,1.,0.995734176295034,1.,0.995734176295034,
1.,0.995734176295034,1.,0.995734176295034,1.,0.995734176295034,1.,0.995734176295034,
1.,0.995734176295034,1.,0.995734176295034,1.,0.995734176295034,1.,0.995734176295034,
1.,0.995734176295034,1.,0.995734176295034,1.,0.995734176295034,1.,0.995734176295034,
1.,0.995734176295034,1.,0.995734176295034,1.,0.995734176295034,1.,0.995734176295034,
1.,0.995734176295034,1.,0.995734176295034,1.,0.995734176295034,1.,0.995734176295034,
1.,0.995734176295034,1.,0.995734176295034,1.,0.995734176295034,1.,0.995734176295034,
1.,0.995734176295034,1.,0.995734176295034,1.,0.995734176295034,1.,0.995734176295034,
1.,0.995734176295034,1.,0.995734176295034,1.,0.995734176295034,1.,0.995734176295034,
1.,0.995734176295034,1.,0.995734176295034,1.,0.995734176295034,1.,0.995734176295034,
1.,0.995734176295034,1.,0.995734176295034,1.,0.995734176295034,1.,0.995734176295034,
1.,0.995734176295034,1.,0.995734176295034,1.,0.995734176295034,1.,0.995734176295034,
1.,0.995734176295034,1.,0.995734176295034,1.,0.995734176295034,1.,0.995734176295034,
1.,0.995734176295034,1.,0.995734176295034,1.,0.995734176295034,1.,0.995734176295034,
1.,0.995734176295034,1.,0.995734176295034,1.,0.995734176295034,1.,0.995734176295034,
1.,0.995734176295034,1.,0.995734176295034,1.,0.995734176295034,1.,0.995734176295034,
1.,0.995734176295034,1.,0.995734176295034,1.,0.995734176295034,1.,0.995734176295034,
1.,0.995734176295034,1.,0.995734176295034,1.,0.995734176295034,1.,0.995734176295034,
1.,0.995734176295034,1.,0.995734176295034,1.,0.995734176295034,1.,0.995734176295034,
1.,0.995734176295034,1.,0.995734176295034,1.,0.995734176295034,1.,0.995734176295034,
1.,0.995734176295034,1.,0.995734176295034,1.,0.995734176295034,1.,0.995734176295034,
1.,0.995734176295034,1.,0.995734176295034,1.,0.995734176295034,1.,0.995734176295034,
1.,0.995734176295034,1.,0.995734176295034,1.,0.995734176295034,1.,0.995734176295034,
1.,0.995734176295034,1.,0.995734176295034,1.,0.995734176295034,1.,0.995734176295034,
1.,0.995734176295034,1.,0.995734176295034,1.,0.995734176295034,1.,0.995734176295034,
1.,0.995734176295034,1.,0.995734176295034,1.,0.995734176295034,1.,0.995734176295034,
1.,0.995734176295034,1.,0.995734176295034,1.,0.995734176295034,1.,0.995734176295034,
1.,0.995734176295034,1.,0.995734176295034,1.,0.995734176295034,1.,0.995734176295034,
1.,0.995734176295034,1.,0.995734176295034,1.,0.995734176295034,1.,0.995734176295034,
1.,0.995734176295034,1.,0.995734176295034,1.,0.995734176295034,1.,0.995734176295034,
1.,0.995734176295034,1.,0.995734176295034,1.,0.995734176295034,1.,0.995734176295034,
1.,0.995734176295034,1.,0.995734176295034,1.,0.995734176295034,1.,0.995734176295034,
1.,0.995734176295034,1.,0.995734176295034,1.,0.995734176295034,1.,0.995734176295034,
1.,0.995734176295034,1.,0.995734176295034,1.,0.995734176295034,1.,0.995734176295034,
1.,0.995734176295034,1.,0.995734176295034,1.,0.995734176295034,1.,0.995734176295034,
1.,0.995734176295034,1.,0.995734176295034,1.,0.995734176295034,1.,0.995734176295034,
1.,0.995734176295034,1.,0.995734176295034,1.,0.995734176295034,1.,0.995734176295034,
1.,0.995734176295034,1.,0.995734176295034,1.,0.995734176295034,1.,0.995734176295034,
1.,0.995734176295034,1.,0.995734176295034,1.,0.995734176295034,1.,0.995734176295034,
1.,0.995734176295034,1.,0.995734176295034,1.,0.995734176295034,1.,0.995734176295034,
1.,0.995734176295034,1.,0.995734176295034,1.,0.995734176295034,1.,0.995734176295034,
1.,0.995734176295034,1.,0.995734176295034,1.,0.995734176295034,1.,0.995734176295034,
1.,0.995734176295034,1.,0.995734176295034,1.,0.995734176295034,1.,0.995734176295034,
1.,0.995734176295034,1.,0.995734176295034,1.,0.995734176295034,1.,0.995734176295034,
1.,0.995734176295034,1.,0.995734176295034,1.,0.995734176295034,1.,0.995734176295034,
1.,0.995734176295034,1.,0.995734176295034,1.,0.995734176295034,1.,0.995734176295034,
1.,0.995734176295034,1.,0.995734176295034,1.,0.995734176295034,1.,0.995734176295034,
1.,0.995734176295034,1.,0.995734176295034,1.,0.995734176295034,1.,0.995734176295034,
1.,0.995734176295034,1.,0.995734176295034,1.,0.995734176295034,1.,0.995734176295034,
1.,0.995734176295034,1.,0.995734176295034,1.,0.995734176295034,1.,0.995734176295034,
1.,0.995734176295034,1.,0.995734176295034,1.,0.995734176295034,1.,0.995734176295034,
1.,0.995734176295034,1.,0.995734176295034,1.,0.995734176295034,1.,0.995734176295034,
1.,0.995734176295034,1.,0.995734176295034,1.,0.995734176295034,1.,0.995734176295034,
1.,0.995734176295034,1.,0.995734176295034,1.,0.995734176295034,1.,0.995734176295034,
1.,0.995734176295034,1.,0.995734176295034,1.,0.995734176295034,1.,0.995734176295034,
1.,0.995734176295034,1.,0.995734176295034,1.,0.995734176295034,1.,0.995734176295034,
1.,0.995734176295034,1.,0.995734176295034,1.,0.995734176295034,1.,0.995734176295034,
1.,0.995734176295034,1.,0.995734176295034,1.,0.995734176295034,1.,0.995734176295034,
1.,0.995734176295034,1.,0.995734176295034,1.,0.995734176295034,1.,0.995734176295034,
1.,0.995734176295034,1.,0.995734176295034,1.,0.995734176295034,1.,0.995734176295034,
1.,0.995734176295034,1.,0.995734176295034,1.,0.995734176295034,1.,0.995734176295034,
1.,0.995734176295034,1.,0.995734176295034,1.,0.995734176295034,1.,0.995734176295034,
1.,0.995734176295034,1.,0.995734176295034,1.,0.995734176295034,1.,0.995734176295034,
1.,0.995734176295034,1.,0.995734176295034,1.,0.995734176295034,1.,0.995734176295034,
1.,0.995734176295034,1.,0.995734176295034,1.,0.995734176295034,1.,0.995734176295034,
1.,0.995734176295034,1.,0.995734176295034,1.,0.995734176295034,1.,0.995734176295034,
1.,0.995734176295034,1.,0.995734176295034,1.,0.995734176295034,1.,0.995734176295034,
1.,0.995734176295034,1.,0.995734176295034,1.,0.995734176295034,1.,0.995734176295034,
1.,0.995734176295034,1.,0.995734176295034,1.,0.995734176295034,1.,0.995734176295034,
1.,0.995734176295034,1.,0.995734176295034,1.,0.995734176295034,1.,0.995734176295034,
1.,0.995734176295034,1.,0.995734176295034,1.,0.995734176295034,1.,0.995734176295034,
1.,0.995734176295034,1.,0.995734176295034,1.,0.995734176295034,1.,0.995734176295034,
1.,0.995734176295034,1.,0.995734176295034,1.,0.995734176295034,1.,0.995734176295034,
1.,0.995734176295034,1.,0.995734176295034,1.,0.995734176295034,1.,0.995734176295034,
1.,0.995734176295034,1.,0.995734176295034,1.,0.995734176295034,1.,0.995734176295034,
1.,0.995734176295034,1.,0.995734176295034,1.,0.995734176295034,1.,0.995734176295034,
1.,0.995734176295034,1.,0.995734176295034,1.,0.995734176295034,1.,0.995734176295034,
1.,0.995734176295034,1.,0.995734176295034,1.,0.995734176295034,1.,0.995734176295034,
1.,0.995734176295034,1.,0.995734176295034,1.,0.995734176295034,1.,0.995734176295034,
1.,0.995734176295034,1.,0.995734176295034,1.,0.995734176295034,1.,0.995734176295034,
1.,0.995734176295034,1.,0.995734176295034,1.,0.995734176295034,1.,0.995734176295034,
1.,0.995734176295034,1.,0.995734176295034,1.,0.995734176295034,1.,0.995734176295034,
1.,0.995734176295034,1.,0.995734176295034,1.,0.995734176295034,1.,0.995734176295034,
1.,0.995734176295034,1.,0.995734176295034,1.,0.995734176295034,1.,0.995734176295034,
1.,0.995734176295034,1.,0.995734176295034,1.,0.995734176295034,1.,0.995734176295034,
1.,0.995734176295034,1.,0.995734176295034,1.,0.995734176295034,1.,0.995734176295034,
1.,0.995734176295034,1.,0.995734176295034,1.,0.995734176295034,1.,0.995734176295034,
1.,0.995734176295034,1.,0.995734176295034,1.,0.995734176295034,1.,0.995734176295034,
1.,0.995734176295034,1.,0.995734176295034,1.,0.995734176295034,1.,0.995734176295034,
1.,0.995734176295034,1.,0.995734176295034,1.,0.995734176295034,1.,0.995734176295034,
1.,0.995734176295034,1.,0.995734176295034,1.,0.995734176295034,1.,0.995734176295034,
1.,0.995734176295034,1.,0.995734176295034,1.,0.995734176295034,1.,0.995734176295034,
1.,0.995734176295034,1.,0.995734176295034,1.,0.995734176295034,1.,0.995734176295034,
1.,0.995734176295034,1.,0.995734176295034,1.,0.995734176295034,1.,0.995734176295034,
1.,0.995734176295034,1.,0.995734176295034,1.,0.995734176295034,1.,0.995734176295034,
1.,0.995734176295034,1.,0.995734176295034,1.,0.995734176295034,1.,0.995734176295034,
1.,0.995734176295034,1.,0.995734176295034,1.,0.995734176295034,1.,0.995734176295034,
1.,0.995734176295034,1.,0.995734176295034,1.,0.995734176295034,1.,0.995734176295034,
1.,0.995734176295034,1.,0.995734176295034,1.,0.995734176295034,1.,0.995734176295034,
1.,0.995734176295034,1.,0.995734176295034,1.,0.995734176295034,1.,0.995734176295034,
1.,0.995734176295034,1.,0.995734176295034,1.,0.995734176295034,1.,0.995734176295034,
1.,0.995734176295034,1.,0.995734176295034,1.,0.995734176295034,1.,0.995734176295034,
1.,0.995734176295034,1.,0.995734176295034,1.,0.995734176295034,1.,0.995734176295034,
1.,0.995734176295034,1.,0.995734176295034,1.,0.995734176295034,1.,0.995734176295034,
1.,0.995734176295034,1.,0.995734176295034,1.,0.995734176295034,1.,0.995734176295034,
1.,0.995734176295034,1.,0.995734176295034,1.,0.995734176295034,1.,0.995734176295034,
1.,0.995734176295034,1.,0.995734176295034,1.,0.995734176295034,1.,0.995734176295034,
1.,0.995734176295034,1.,0.995734176295034,1.,0.995734176295034,1.,0.995734176295034,
1.,0.995734176295034,1.,0.995734176295034,1.,0.995734176295034,1.,0.995734176295034,
1.,0.995734176295034,1.,0.995734176295034,1.,0.995734176295034,1.,0.995734176295034,
1.,0.995734176295034,1.,0.995734176295034,1.,0.995734176295034,1.,0.995734176295034,
1.,0.995734176295034,1.,0.995734176295034,1.,0.995734176295034,1.,0.995734176295034,
1.,0.995734176295034,1.,0.995734176295034,1.,0.995734176295034,1.,0.995734176295034,
1.,0.995734176295034,1.,0.995734176295034,1.,0.995734176295034,1.,0.995734176295034,
1.,0.995734176295034,1.,0.995734176295034,1.,0.995734176295034,1.,0.995734176295034,
1.,0.995734176295034,1.,0.995734176295034,1.,0.995734176295034,1.,0.995734176295034,
1.,0.995734176295034,1.,0.995734176295034,1.,0.995734176295034,1.,0.995734176295034,
1.,0.995734176295034,1.,0.995734176295034,1.,0.995734176295034,1.,0.995734176295034,
1.,0.995734176295034,1.,0.995734176295034,1.,0.995734176295034,1.,0.995734176295034,
1.,0.995734176295034,1.,0.995734176295034,1.,0.995734176295034,1.,0.995734176295034,
1.,0.995734176295034,1.,0.995734176295034,1.,0.995734176295034,1.,0.995734176295034,
1.,0.995734176295034,1.,0.995734176295034,1.,0.995734176295034,1.,0.995734176295034,
1.,0.995734176295034,1.,0.995734176295034,1.,0.995734176295034,1.,0.995734176295034,
1.,0.995734176295034,1.,0.995734176295034,1.,0.995734176295034,1.,0.995734176295034,
1.,0.995734176295034,1.,0.995734176295034,1.,0.995734176295034,1.,0.995734176295034,
1.,0.995734176295034,1.,0.995734176295034,1.,0.995734176295034,1.,0.995734176295034,
1.,0.995734176295034,1.,0.995734176295034,1.,0.995734176295034,1.,0.995734176295034,
1.,0.995734176295034,1.,0.995734176295034,1.,0.995734176295034,1.,0.995734176295034,
1.,0.995734176295034,1.,0.995734176295034,1.,0.995734176295034,1.,0.995734176295034,
1.,0.995734176295034,1.,0.995734176295034,1.,0.995734176295034,1.,0.995734176295034,
1.,0.995734176295034,1.,0.995734176295034,1.,0.995734176295034,1.,0.995734176295034,
1.,0.995734176295034,1.,0.995734176295034,1.,0.995734176295034,1.,0.995734176295034,
1.,0.995734176295034,1.,0.995734176295034,1.,0.995734176295034,1.,0.995734176295034,
1.,0.995734176295034,1.,0.995734176295034,1.,0.995734176295034,1.,0.995734176295034,
1.,0.995734176295034,1.,0.995734176295034,1.,0.995734176295034,1.,0.995734176295034,
1.,0.995734176295034,1.,0.995734176295034,1.,0.995734176295034,1.,0.995734176295034,
1.,0.995734176295034,1.,0.995734176295034,1.,0.995734176295034,1.,0.995734176295034,
1.,0.995734176295034,1.,0.995734176295034,1.,0.995734176295034,1.,0.995734176295034,
1.,0.995734176295034,1.,0.995734176295034,1.,0.995734176295034,1.,0.995734176295034,
1.,0.995734176295034,1.,0.995734176295034,1.,0.995734176295034,1.,0.995734176295034,
1.,0.995734176295034,1.,0.995734176295034,1.,0.995734176295034,1.,0.995734176295034,
1.,0.995734176295034,1.,0.995734176295034,1.,0.995734176295034,1.,0.995734176295034,
1.,0.995734176295034,1.,0.995734176295034,1.,0.995734176295034,1.,0.995734176295034,
1.,0.995734176295034,1.,0.995734176295034,1.,0.995734176295034,1.,0.995734176295034,
1.,0.995734176295034,1.,0.995734176295034,1.,0.995734176295034,1.,0.995734176295034,
1.,0.995734176295034,1.,0.995734176295034,1.,0.995734176295034,1.,0.995734176295034,
1.,0.995734176295034,1.,0.995734176295034,1.,0.995734176295034,1.,0.995734176295034,
1.,0.995734176295034,1.,0.995734176295034,1.,0.995734176295034,1.,0.995734176295034,
1.,0.995734176295034,1.,0.995734176295034,1.,0.995734176295034,1.,0.995734176295034,
1.,0.995734176295034,1.,0.995734176295034,1.,0.995734176295034,1.,0.995734176295034,
1.,0.995734176295034,1.,0.995734176295034,1.,0.995734176295034,1.,0.995734176295034,
1.,0.995734176295034,1.,0.995734176295034,1.,0.995734176295034,1.,0.995734176295034,
1.,0.995734176295034,1.,0.995734176295034,1.,0.995734176295034,1.,0.995734176295034,
1.,0.995734176295034,1.,0.995734176295034,1.,0.995734176295034,1.,0.995734176295034,
1.,0.995734176295034,1.,0.995734176295034,1.,0.995734176295034,1.,0.995734176295034,
1.,0.995734176295034,1.,0.995734176295034,1.,0.995734176295034,1.,0.995734176295034,
1.,0.995734176295034,1.,0.995734176295034,1.,0.995734176295034,1.,0.995734176295034,
1.,0.995734176295034,1.,0.995734176295034,1.,0.995734176295034,1.,0.995734176295034,
1.,0.995734176295034,1.,0.995734176295034,1.,0.995734176295034,1.,0.995734176295034,
1.,0.995734176295034,1.,0.995734176295034,1.,0.995734176295034,1.,0.995734176295034,
1.,0.995734176295034,1.,0.995734176295034,1.,0.995734176295034,1.,0.995734176295034,
1.,0.995734176295034,1.,0.995734176295034,1.,0.995734176295034,1.,0.995734176295034,
1.,0.995734176295034,1.,0.995734176295034,1.,0.995734176295034,1.,0.995734176295034,
1.,0.995734176295034,1.,0.995734176295034,1.,0.995734176295034,1.,0.995734176295034,
1.,0.995734176295034,1.,0.995734176295034,1.,0.995734176295034,1.,0.995734176295034,
1.,0.995734176295034,1.,0.995734176295034,1.,0.995734176295034,1.,0.995734176295034,
1.,0.995734176295034,1.,0.995734176295034,1.,0.995734176295034,1.,0.995734176295034,
1.,0.995734176295034,1.,0.995734176295034,1.,0.995734176295034,1.,0.995734176295034,
1.,0.995734176295034,1.,0.995734176295034,1.,0.995734176295034,1.,0.995734176295034,
1.,0.995734176295034,1.,0.995734176295034,1.,0.995734176295034,1.,0.995734176295034,
1.,0.995734176295034,1.,0.995734176295034,1.,0.995734176295034,1.,0.995734176295034,
1.,0.995734176295034,1.,0.995734176295034,1.,0.995734176295034,1.,0.995734176295034,
1.,0.995734176295034,1.,0.995734176295034,1.,0.995734176295034,1.,0.995734176295034,
1.,0.995734176295034,1.,0.995734176295034,1.,0.995734176295034,1.,0.995734176295034,
1.,0.995734176295034,1.,0.995734176295034,1.,0.995734176295034,1.,0.995734176295034,
1.,0.995734176295034,1.,0.995734176295034,1.,0.995734176295034,1.,0.995734176295034,
1.,0.995734176295034,1.,0.995734176295034,1.,0.995734176295034,1.,0.995734176295034,
1.,0.995734176295034,1.,0.995734176295034,1.,0.995734176295034,1.,0.995734176295034,
1.,0.995734176295034,1.,0.995734176295034,1.,0.995734176295034,1.,0.995734176295034,
1.,0.995734176295034,1.,0.995734176295034,1.,0.995734176295034,1.,0.995734176295034,
1.,0.995734176295034,1.,0.995734176295034,1.,0.995734176295034,1.,0.995734176295034,
1.,0.995734176295034,1.,0.995734176295034,1.,0.995734176295034,1.,0.995734176295034,
1.,0.995734176295034,1.,0.995734176295034,1.,0.995734176295034,1.,0.995734176295034,
1.,0.995734176295034,1.,0.995734176295034,1.,0.995734176295034,1.,0.995734176295034,
1.,0.995734176295034,1.,0.995734176295034,1.,0.995734176295034,1.,0.995734176295034,
1.,0.995734176295034,1.,0.995734176295034,1.,0.995734176295034,1.,0.995734176295034,
1.,0.995734176295034,1.,0.995734176295034,1.,0.995734176295034,1.,0.995734176295034,
1.,0.995734176295034,1.,0.995734176295034,1.,0.995734176295034,1.,0.995734176295034,
1.,0.995734176295034,1.,0.995734176295034,1.,0.995734176295034,1.,0.995734176295034,
1.,0.995734176295034,1.,0.995734176295034,1.,0.995734176295034,1.,0.995734176295034,
1.,0.995734176295034,1.,0.995734176295034,1.,0.995734176295034,1.,0.995734176295034,
1.,0.995734176295034,1.,0.995734176295034,1.,0.995734176295034,1.,0.995734176295034,
1.,0.995734176295034,1.,0.995734176295034,1.,0.995734176295034,1.,0.995734176295034,
1.,0.995734176295034,1.,0.995734176295034,1.,0.995734176295034,1.,0.995734176295034,
1.,0.995734176295034,1.,0.995734176295034,1.,0.995734176295034,1.,0.995734176295034,
1.,0.995734176295034,1.,0.995734176295034,1.,0.995734176295034,1.,0.995734176295034,
1.,0.995734176295034,1.,0.995734176295034,1.,0.995734176295034,1.,0.995734176295034,
1.,0.995734176295034,1.,0.995734176295034,1.,0.995734176295034,1.,0.995734176295034,
1.,0.995734176295034,1.,0.995734176295034,1.,0.995734176295034,1.,0.995734176295034,
1.,0.995734176295034,1.,0.995734176295034,1.,0.995734176295034,1.,0.995734176295034,
1.,0.995734176295034,1.,0.995734176295034,1.,0.995734176295034,1.,0.995734176295034,
1.,0.995734176295034,1.,0.995734176295034,1.,0.995734176295034,1.,0.995734176295034,
1.,0.995734176295034,1.,0.995734176295034,1.,0.995734176295034,1.,0.995734176295034,
1.,0.995734176295034,1.,0.995734176295034,1.,0.995734176295034,1.,0.995734176295034,
1.,0.995734176295034,1.,0.995734176295034,1.,0.995734176295034,1.,0.995734176295034,
1.,0.995734176295034,1.,0.995734176295034,1.,0.995734176295034,1.,0.995734176295034,
1.,0.995734176295034,1.,0.995734176295034,1.,0.995734176295034,1.,0.995734176295034,
1.,0.995734176295034,1.,0.995734176295034,1.,0.995734176295034,1.,0.995734176295034,
1.,0.995734176295034,1.,0.995734176295034,1.,0.995734176295034,1.,0.995734176295034,
1.,0.995734176295034,1.,0.995734176295034,1.,0.995734176295034,1.,0.995734176295034,
1.,0.995734176295034,1.,0.995734176295034,1.,0.995734176295034,1.,0.995734176295034,
1.,0.995734176295034,1.,0.995734176295034,1.,0.995734176295034,1.,0.995734176295034,
1.,0.995734176295034,1.,0.995734176295034,1.,0.995734176295034,1.,0.995734176295034,
1.,0.995734176295034,1.,0.995734176295034,1.,0.995734176295034,1.,0.995734176295034,
1.,0.995734176295034,1.,0.995734176295034,1.,0.995734176295034,1.,0.995734176295034,
1.,0.995734176295034,1.,0.995734176295034,1.,0.995734176295034,1.,0.995734176295034,
1.,0.995734176295034,1.,0.995734176295034,1.,0.995734176295034,1.,0.995734176295034,
1.,0.995734176295034,1.,0.995734176295034,1.,0.995734176295034,1.,0.995734176295034,
1.,0.995734176295034,1.,0.995734176295034,1.,0.995734176295034,1.,0.995734176295034,
1.,0.995734176295034,1.,0.995734176295034,1.,0.995734176295034,1.,0.995734176295034,
1.,0.995734176295034,1.,0.995734176295034,1.,0.995734176295034,1.,0.995734176295034,
1.,0.995734176295034,1.,0.995734176295034,1.,0.995734176295034,1.,0.995734176295034,
1.,0.995734176295034,1.,0.995734176295034,1.,0.995734176295034,1.,0.995734176295034,
1.,0.995734176295034,1.,0.995734176295034,1.,0.995734176295034,1.,0.995734176295034,
1.,0.995734176295034,1.,0.995734176295034,1.,0.995734176295034,1.,0.995734176295034,
1.,0.995734176295034,1.,0.995734176295034,1.,0.995734176295034,1.,0.995734176295034,
1.,0.995734176295034,1.,0.995734176295034,1.,0.995734176295034,1.,0.995734176295034,
1.,0.995734176295034,1.,0.995734176295034,1.,0.995734176295034,1.,0.995734176295034,
1.,0.995734176295034,1.,0.995734176295034,1.,0.995734176295034,1.,0.995734176295034,
1.,0.995734176295034,1.,0.995734176295034,1.,0.995734176295034,1.,0.995734176295034,
1.,0.995734176295034,1.,0.995734176295034,1.,0.995734176295034,1.,0.995734176295034,
1.,0.995734176295034,1.,0.995734176295034,1.,0.995734176295034,1.,0.995734176295034,
1.,0.995734176295034,1.,0.995734176295034,1.,0.995734176295034,1.,0.995734176295034,
1.,0.995734176295034,1.,0.995734176295034,1.,0.995734176295034,1.,0.995734176295034,
1.,0.995734176295034,1.,0.995734176295034,1.,0.995734176295034,1.,0.995734176295034,
1.,0.995734176295034,1.,0.995734176295034,1.,0.995734176295034,1.,0.995734176295034,
1.,0.995734176295034,1.,0.995734176295034,1.,0.995734176295034,1.,0.995734176295034,
1.,0.995734176295034,1.,0.995734176295034,1.,0.995734176295034,1.,0.995734176295034,
1.,0.995734176295034,1.,0.995734176295034,1.,0.995734176295034,1.,0.995734176295034,
1.,0.995734176295034,1.,0.995734176295034,1.,0.99720106003931,0.998075063662495)))
REPRESENTATION_ITEM('')
SURFACE()
);
#2502=(
BOUNDED_SURFACE()
B_SPLINE_SURFACE(1,2,((#150388,#150389,#150390,#150391,#150392,#150393,
#150394,#150395,#150396,#150397,#150398,#150399,#150400,#150401,#150402,
#150403,#150404,#150405,#150406,#150407,#150408,#150409,#150410,#150411,
#150412,#150413,#150414,#150415,#150416,#150417,#150418,#150419,#150420,
#150421,#150422,#150423,#150424,#150425,#150426,#150427,#150428,#150429,
#150430,#150431,#150432,#150433,#150434,#150435,#150436,#150437,#150438,
#150439,#150440,#150441,#150442,#150443,#150444,#150445,#150446,#150447,
#150448,#150449,#150450,#150451,#150452,#150453,#150454,#150455,#150456,
#150457,#150458,#150459,#150460,#150461,#150462,#150463,#150464,#150465,
#150466,#150467,#150468,#150469,#150470,#150471,#150472,#150473,#150474,
#150475,#150476,#150477,#150478,#150479,#150480,#150481,#150482,#150483,
#150484,#150485,#150486,#150487,#150488,#150489,#150490,#150491,#150492,
#150493,#150494,#150495,#150496,#150497,#150498,#150499,#150500,#150501,
#150502,#150503,#150504,#150505,#150506,#150507,#150508,#150509,#150510,
#150511,#150512,#150513,#150514,#150515,#150516,#150517,#150518,#150519,
#150520,#150521,#150522,#150523,#150524,#150525,#150526,#150527,#150528,
#150529,#150530,#150531,#150532,#150533,#150534,#150535,#150536,#150537,
#150538,#150539,#150540,#150541,#150542,#150543,#150544,#150545,#150546,
#150547,#150548,#150549,#150550,#150551,#150552,#150553,#150554,#150555,
#150556,#150557,#150558,#150559,#150560,#150561,#150562,#150563,#150564,
#150565,#150566,#150567,#150568,#150569,#150570,#150571,#150572,#150573,
#150574,#150575,#150576,#150577,#150578,#150579,#150580,#150581,#150582,
#150583,#150584,#150585,#150586,#150587,#150588,#150589,#150590,#150591,
#150592,#150593,#150594,#150595,#150596,#150597,#150598,#150599,#150600,
#150601,#150602,#150603,#150604,#150605,#150606,#150607,#150608,#150609,
#150610,#150611,#150612,#150613,#150614,#150615,#150616,#150617,#150618,
#150619,#150620,#150621,#150622,#150623,#150624,#150625,#150626,#150627,
#150628,#150629,#150630,#150631,#150632,#150633,#150634,#150635,#150636,
#150637,#150638,#150639,#150640,#150641,#150642,#150643,#150644,#150645,
#150646,#150647,#150648,#150649,#150650,#150651,#150652,#150653,#150654,
#150655,#150656,#150657,#150658,#150659,#150660,#150661,#150662,#150663,
#150664,#150665,#150666,#150667,#150668,#150669,#150670,#150671,#150672,
#150673,#150674,#150675,#150676,#150677,#150678,#150679,#150680,#150681,
#150682,#150683,#150684,#150685,#150686,#150687,#150688,#150689,#150690,
#150691,#150692,#150693,#150694,#150695,#150696,#150697,#150698,#150699,
#150700,#150701,#150702,#150703,#150704,#150705,#150706,#150707,#150708,
#150709,#150710,#150711,#150712,#150713,#150714,#150715,#150716,#150717,
#150718,#150719,#150720,#150721,#150722,#150723,#150724,#150725,#150726,
#150727,#150728,#150729,#150730,#150731,#150732,#150733,#150734,#150735,
#150736,#150737,#150738,#150739,#150740,#150741,#150742,#150743,#150744,
#150745,#150746,#150747,#150748,#150749,#150750,#150751,#150752,#150753,
#150754,#150755,#150756,#150757,#150758,#150759,#150760,#150761,#150762,
#150763,#150764,#150765,#150766,#150767,#150768,#150769,#150770,#150771,
#150772,#150773,#150774,#150775,#150776,#150777,#150778,#150779,#150780,
#150781,#150782,#150783,#150784,#150785,#150786,#150787,#150788,#150789,
#150790,#150791,#150792,#150793,#150794,#150795,#150796,#150797,#150798,
#150799,#150800,#150801,#150802,#150803,#150804,#150805,#150806,#150807,
#150808,#150809,#150810,#150811,#150812,#150813,#150814,#150815,#150816,
#150817,#150818,#150819,#150820,#150821,#150822,#150823,#150824,#150825,
#150826,#150827,#150828,#150829,#150830,#150831,#150832,#150833,#150834,
#150835,#150836,#150837,#150838,#150839,#150840,#150841,#150842,#150843,
#150844,#150845,#150846,#150847,#150848,#150849,#150850,#150851,#150852,
#150853,#150854,#150855,#150856,#150857,#150858,#150859,#150860,#150861,
#150862,#150863,#150864,#150865,#150866,#150867,#150868,#150869,#150870,
#150871,#150872,#150873,#150874,#150875,#150876,#150877,#150878,#150879,
#150880,#150881,#150882,#150883,#150884,#150885,#150886,#150887,#150888,
#150889,#150890,#150891,#150892,#150893,#150894,#150895,#150896,#150897,
#150898,#150899,#150900,#150901,#150902,#150903,#150904,#150905,#150906,
#150907,#150908,#150909,#150910,#150911,#150912,#150913,#150914,#150915,
#150916,#150917,#150918,#150919,#150920,#150921,#150922,#150923,#150924,
#150925,#150926,#150927,#150928,#150929,#150930,#150931,#150932,#150933,
#150934,#150935,#150936,#150937,#150938,#150939,#150940,#150941,#150942,
#150943,#150944,#150945,#150946,#150947,#150948,#150949,#150950,#150951,
#150952,#150953,#150954,#150955,#150956,#150957,#150958,#150959,#150960,
#150961,#150962,#150963,#150964,#150965,#150966,#150967,#150968,#150969,
#150970,#150971,#150972,#150973,#150974,#150975,#150976,#150977,#150978,
#150979,#150980,#150981,#150982,#150983,#150984,#150985,#150986,#150987,
#150988,#150989,#150990,#150991,#150992,#150993,#150994,#150995,#150996,
#150997,#150998,#150999,#151000,#151001,#151002,#151003,#151004,#151005,
#151006,#151007,#151008,#151009,#151010,#151011,#151012,#151013,#151014,
#151015,#151016,#151017,#151018,#151019,#151020,#151021,#151022,#151023,
#151024,#151025,#151026,#151027,#151028,#151029,#151030,#151031,#151032,
#151033,#151034,#151035,#151036,#151037,#151038,#151039,#151040,#151041,
#151042,#151043,#151044,#151045,#151046,#151047,#151048,#151049,#151050,
#151051,#151052,#151053,#151054,#151055,#151056,#151057,#151058,#151059,
#151060,#151061,#151062,#151063,#151064,#151065,#151066,#151067,#151068,
#151069,#151070,#151071,#151072,#151073,#151074,#151075,#151076,#151077,
#151078,#151079,#151080,#151081,#151082,#151083,#151084,#151085,#151086,
#151087,#151088,#151089,#151090,#151091,#151092,#151093,#151094,#151095,
#151096,#151097,#151098,#151099,#151100,#151101,#151102,#151103,#151104,
#151105,#151106,#151107,#151108,#151109,#151110,#151111,#151112,#151113,
#151114,#151115,#151116,#151117,#151118,#151119,#151120,#151121,#151122,
#151123,#151124,#151125,#151126,#151127,#151128,#151129,#151130,#151131,
#151132,#151133,#151134,#151135,#151136,#151137,#151138,#151139,#151140,
#151141,#151142,#151143,#151144,#151145,#151146,#151147,#151148,#151149,
#151150,#151151,#151152,#151153,#151154,#151155,#151156,#151157,#151158,
#151159,#151160,#151161,#151162,#151163,#151164,#151165,#151166,#151167,
#151168,#151169,#151170,#151171,#151172,#151173,#151174,#151175,#151176,
#151177,#151178,#151179,#151180,#151181,#151182,#151183,#151184,#151185,
#151186,#151187,#151188,#151189,#151190,#151191,#151192,#151193,#151194,
#151195,#151196,#151197,#151198,#151199,#151200,#151201,#151202,#151203,
#151204,#151205,#151206,#151207,#151208,#151209,#151210,#151211,#151212,
#151213,#151214,#151215,#151216,#151217,#151218,#151219,#151220,#151221,
#151222,#151223,#151224,#151225,#151226,#151227,#151228,#151229,#151230,
#151231,#151232,#151233,#151234,#151235,#151236,#151237,#151238,#151239,
#151240,#151241,#151242,#151243,#151244,#151245,#151246,#151247,#151248,
#151249,#151250,#151251,#151252,#151253,#151254,#151255,#151256,#151257,
#151258,#151259,#151260,#151261,#151262,#151263,#151264,#151265,#151266,
#151267,#151268,#151269,#151270,#151271,#151272,#151273,#151274,#151275,
#151276,#151277,#151278,#151279,#151280,#151281,#151282,#151283,#151284,
#151285,#151286,#151287,#151288,#151289,#151290,#151291,#151292,#151293,
#151294,#151295,#151296,#151297,#151298,#151299,#151300,#151301,#151302,
#151303,#151304,#151305,#151306,#151307,#151308,#151309,#151310,#151311,
#151312,#151313,#151314,#151315,#151316,#151317,#151318,#151319,#151320,
#151321,#151322,#151323,#151324,#151325,#151326,#151327,#151328,#151329,
#151330,#151331,#151332,#151333,#151334,#151335,#151336,#151337,#151338,
#151339,#151340,#151341,#151342,#151343,#151344,#151345,#151346,#151347,
#151348,#151349,#151350,#151351,#151352,#151353,#151354,#151355,#151356,
#151357,#151358,#151359,#151360,#151361,#151362,#151363,#151364,#151365,
#151366,#151367,#151368,#151369,#151370,#151371,#151372,#151373,#151374,
#151375,#151376,#151377,#151378,#151379,#151380,#151381,#151382,#151383,
#151384,#151385,#151386,#151387,#151388,#151389,#151390,#151391,#151392,
#151393,#151394,#151395,#151396,#151397,#151398,#151399,#151400,#151401,
#151402,#151403,#151404,#151405,#151406,#151407,#151408,#151409,#151410,
#151411,#151412,#151413,#151414,#151415,#151416,#151417,#151418,#151419,
#151420,#151421,#151422,#151423,#151424,#151425,#151426,#151427,#151428,
#151429,#151430,#151431,#151432,#151433,#151434,#151435,#151436,#151437,
#151438,#151439,#151440,#151441,#151442,#151443,#151444,#151445,#151446,
#151447,#151448,#151449,#151450,#151451,#151452,#151453,#151454,#151455,
#151456,#151457,#151458,#151459,#151460,#151461,#151462,#151463,#151464,
#151465,#151466,#151467,#151468,#151469,#151470,#151471,#151472,#151473,
#151474,#151475,#151476,#151477,#151478,#151479,#151480,#151481,#151482,
#151483,#151484,#151485,#151486,#151487,#151488,#151489,#151490,#151491,
#151492,#151493,#151494,#151495,#151496,#151497,#151498,#151499,#151500,
#151501,#151502,#151503,#151504,#151505,#151506,#151507,#151508,#151509,
#151510,#151511,#151512,#151513,#151514,#151515,#151516,#151517,#151518,
#151519,#151520,#151521,#151522,#151523,#151524,#151525,#151526,#151527,
#151528,#151529,#151530,#151531,#151532,#151533,#151534,#151535,#151536,
#151537,#151538,#151539,#151540,#151541,#151542,#151543,#151544,#151545,
#151546,#151547,#151548,#151549,#151550,#151551,#151552,#151553,#151554,
#151555,#151556,#151557,#151558,#151559,#151560,#151561,#151562,#151563,
#151564,#151565,#151566,#151567,#151568,#151569,#151570,#151571,#151572,
#151573,#151574,#151575,#151576,#151577,#151578,#151579,#151580,#151581,
#151582,#151583,#151584,#151585,#151586,#151587,#151588,#151589,#151590,
#151591,#151592,#151593,#151594,#151595,#151596,#151597,#151598,#151599,
#151600,#151601,#151602,#151603,#151604,#151605,#151606,#151607,#151608,
#151609,#151610,#151611,#151612,#151613,#151614,#151615,#151616,#151617,
#151618,#151619,#151620,#151621,#151622,#151623,#151624,#151625,#151626,
#151627,#151628,#151629,#151630,#151631,#151632,#151633,#151634,#151635,
#151636,#151637,#151638,#151639,#151640,#151641,#151642,#151643,#151644,
#151645,#151646,#151647,#151648,#151649,#151650,#151651,#151652,#151653,
#151654,#151655,#151656,#151657,#151658,#151659,#151660,#151661,#151662,
#151663,#151664,#151665,#151666,#151667,#151668,#151669,#151670,#151671,
#151672,#151673,#151674,#151675,#151676,#151677,#151678,#151679,#151680,
#151681,#151682,#151683,#151684,#151685,#151686,#151687,#151688,#151689,
#151690,#151691,#151692,#151693,#151694,#151695,#151696,#151697,#151698,
#151699,#151700,#151701,#151702,#151703,#151704,#151705,#151706,#151707,
#151708,#151709,#151710,#151711,#151712,#151713,#151714,#151715,#151716,
#151717,#151718,#151719,#151720,#151721,#151722,#151723,#151724,#151725,
#151726,#151727,#151728,#151729,#151730,#151731,#151732,#151733,#151734,
#151735,#151736,#151737,#151738,#151739,#151740,#151741,#151742,#151743,
#151744,#151745,#151746,#151747,#151748,#151749,#151750,#151751,#151752,
#151753,#151754,#151755,#151756,#151757,#151758,#151759,#151760,#151761,
#151762,#151763,#151764,#151765,#151766,#151767,#151768,#151769,#151770,
#151771,#151772,#151773,#151774,#151775,#151776,#151777,#151778,#151779,
#151780,#151781,#151782,#151783,#151784,#151785,#151786,#151787,#151788,
#151789,#151790,#151791,#151792,#151793,#151794,#151795,#151796,#151797,
#151798,#151799,#151800,#151801,#151802,#151803,#151804,#151805,#151806,
#151807,#151808,#151809,#151810,#151811,#151812,#151813,#151814,#151815,
#151816,#151817,#151818,#151819,#151820,#151821,#151822,#151823,#151824,
#151825,#151826,#151827,#151828,#151829,#151830,#151831,#151832,#151833,
#151834,#151835,#151836,#151837,#151838,#151839,#151840,#151841,#151842,
#151843,#151844,#151845,#151846,#151847,#151848,#151849,#151850,#151851,
#151852,#151853,#151854,#151855,#151856,#151857,#151858,#151859,#151860,
#151861,#151862,#151863,#151864,#151865,#151866,#151867,#151868,#151869,
#151870,#151871,#151872,#151873,#151874,#151875,#151876,#151877,#151878,
#151879,#151880,#151881,#151882,#151883,#151884,#151885,#151886,#151887,
#151888,#151889,#151890,#151891,#151892,#151893,#151894,#151895,#151896,
#151897,#151898,#151899,#151900,#151901,#151902,#151903,#151904,#151905,
#151906,#151907,#151908,#151909,#151910,#151911,#151912,#151913,#151914,
#151915,#151916,#151917,#151918,#151919,#151920,#151921,#151922,#151923,
#151924,#151925,#151926,#151927,#151928,#151929,#151930,#151931,#151932,
#151933,#151934,#151935,#151936,#151937,#151938,#151939,#151940,#151941,
#151942,#151943,#151944,#151945,#151946,#151947,#151948,#151949,#151950,
#151951,#151952,#151953,#151954,#151955,#151956,#151957,#151958,#151959,
#151960,#151961,#151962,#151963,#151964,#151965,#151966,#151967,#151968,
#151969,#151970,#151971,#151972,#151973,#151974,#151975,#151976,#151977,
#151978,#151979,#151980,#151981,#151982,#151983,#151984,#151985,#151986,
#151987,#151988,#151989,#151990,#151991,#151992,#151993,#151994,#151995,
#151996,#151997,#151998,#151999,#152000,#152001,#152002,#152003,#152004,
#152005,#152006,#152007,#152008,#152009,#152010,#152011,#152012,#152013,
#152014,#152015,#152016,#152017,#152018,#152019,#152020,#152021,#152022,
#152023,#152024,#152025,#152026,#152027,#152028,#152029,#152030,#152031,
#152032,#152033,#152034,#152035,#152036,#152037,#152038,#152039,#152040,
#152041,#152042,#152043,#152044,#152045,#152046,#152047,#152048,#152049,
#152050,#152051,#152052,#152053,#152054,#152055,#152056,#152057,#152058,
#152059,#152060,#152061,#152062,#152063,#152064,#152065,#152066,#152067,
#152068,#152069,#152070,#152071,#152072,#152073,#152074,#152075,#152076,
#152077,#152078,#152079,#152080,#152081,#152082,#152083,#152084,#152085,
#152086,#152087,#152088,#152089,#152090,#152091,#152092,#152093,#152094,
#152095,#152096,#152097,#152098,#152099,#152100,#152101,#152102,#152103,
#152104,#152105,#152106,#152107,#152108,#152109,#152110,#152111,#152112,
#152113,#152114,#152115,#152116,#152117,#152118,#152119,#152120,#152121,
#152122,#152123,#152124,#152125,#152126,#152127,#152128,#152129,#152130,
#152131,#152132,#152133,#152134,#152135,#152136,#152137,#152138,#152139,
#152140,#152141,#152142,#152143,#152144,#152145,#152146,#152147,#152148,
#152149,#152150,#152151,#152152,#152153,#152154,#152155,#152156,#152157,
#152158,#152159,#152160,#152161,#152162,#152163,#152164,#152165,#152166,
#152167,#152168,#152169,#152170,#152171,#152172,#152173,#152174,#152175,
#152176,#152177,#152178,#152179,#152180,#152181,#152182,#152183,#152184,
#152185,#152186,#152187,#152188,#152189,#152190,#152191,#152192,#152193,
#152194,#152195,#152196,#152197,#152198,#152199,#152200,#152201,#152202,
#152203,#152204,#152205,#152206,#152207,#152208,#152209,#152210,#152211,
#152212,#152213,#152214,#152215,#152216,#152217,#152218,#152219,#152220,
#152221,#152222,#152223,#152224,#152225,#152226,#152227,#152228,#152229,
#152230,#152231,#152232,#152233,#152234,#152235,#152236,#152237,#152238,
#152239,#152240,#152241,#152242,#152243,#152244,#152245,#152246,#152247,
#152248,#152249,#152250,#152251,#152252,#152253,#152254,#152255,#152256,
#152257,#152258,#152259,#152260,#152261,#152262,#152263,#152264,#152265,
#152266,#152267,#152268,#152269,#152270,#152271,#152272,#152273,#152274,
#152275,#152276,#152277,#152278,#152279,#152280,#152281,#152282,#152283,
#152284,#152285,#152286,#152287,#152288,#152289,#152290,#152291,#152292,
#152293,#152294,#152295,#152296,#152297,#152298,#152299,#152300,#152301,
#152302,#152303,#152304,#152305,#152306,#152307,#152308,#152309,#152310,
#152311,#152312,#152313,#152314,#152315,#152316,#152317,#152318,#152319,
#152320,#152321,#152322,#152323,#152324,#152325,#152326,#152327,#152328,
#152329,#152330,#152331,#152332,#152333,#152334,#152335,#152336,#152337,
#152338,#152339,#152340,#152341,#152342,#152343,#152344,#152345,#152346,
#152347,#152348,#152349,#152350,#152351,#152352,#152353,#152354,#152355,
#152356,#152357,#152358,#152359,#152360,#152361,#152362,#152363,#152364,
#152365,#152366,#152367,#152368,#152369,#152370,#152371,#152372,#152373,
#152374,#152375,#152376,#152377,#152378,#152379,#152380,#152381,#152382,
#152383,#152384,#152385,#152386,#152387,#152388,#152389,#152390,#152391,
#152392,#152393,#152394,#152395,#152396,#152397,#152398,#152399,#152400),
(#152401,#152402,#152403,#152404,#152405,#152406,#152407,#152408,#152409,
#152410,#152411,#152412,#152413,#152414,#152415,#152416,#152417,#152418,
#152419,#152420,#152421,#152422,#152423,#152424,#152425,#152426,#152427,
#152428,#152429,#152430,#152431,#152432,#152433,#152434,#152435,#152436,
#152437,#152438,#152439,#152440,#152441,#152442,#152443,#152444,#152445,
#152446,#152447,#152448,#152449,#152450,#152451,#152452,#152453,#152454,
#152455,#152456,#152457,#152458,#152459,#152460,#152461,#152462,#152463,
#152464,#152465,#152466,#152467,#152468,#152469,#152470,#152471,#152472,
#152473,#152474,#152475,#152476,#152477,#152478,#152479,#152480,#152481,
#152482,#152483,#152484,#152485,#152486,#152487,#152488,#152489,#152490,
#152491,#152492,#152493,#152494,#152495,#152496,#152497,#152498,#152499,
#152500,#152501,#152502,#152503,#152504,#152505,#152506,#152507,#152508,
#152509,#152510,#152511,#152512,#152513,#152514,#152515,#152516,#152517,
#152518,#152519,#152520,#152521,#152522,#152523,#152524,#152525,#152526,
#152527,#152528,#152529,#152530,#152531,#152532,#152533,#152534,#152535,
#152536,#152537,#152538,#152539,#152540,#152541,#152542,#152543,#152544,
#152545,#152546,#152547,#152548,#152549,#152550,#152551,#152552,#152553,
#152554,#152555,#152556,#152557,#152558,#152559,#152560,#152561,#152562,
#152563,#152564,#152565,#152566,#152567,#152568,#152569,#152570,#152571,
#152572,#152573,#152574,#152575,#152576,#152577,#152578,#152579,#152580,
#152581,#152582,#152583,#152584,#152585,#152586,#152587,#152588,#152589,
#152590,#152591,#152592,#152593,#152594,#152595,#152596,#152597,#152598,
#152599,#152600,#152601,#152602,#152603,#152604,#152605,#152606,#152607,
#152608,#152609,#152610,#152611,#152612,#152613,#152614,#152615,#152616,
#152617,#152618,#152619,#152620,#152621,#152622,#152623,#152624,#152625,
#152626,#152627,#152628,#152629,#152630,#152631,#152632,#152633,#152634,
#152635,#152636,#152637,#152638,#152639,#152640,#152641,#152642,#152643,
#152644,#152645,#152646,#152647,#152648,#152649,#152650,#152651,#152652,
#152653,#152654,#152655,#152656,#152657,#152658,#152659,#152660,#152661,
#152662,#152663,#152664,#152665,#152666,#152667,#152668,#152669,#152670,
#152671,#152672,#152673,#152674,#152675,#152676,#152677,#152678,#152679,
#152680,#152681,#152682,#152683,#152684,#152685,#152686,#152687,#152688,
#152689,#152690,#152691,#152692,#152693,#152694,#152695,#152696,#152697,
#152698,#152699,#152700,#152701,#152702,#152703,#152704,#152705,#152706,
#152707,#152708,#152709,#152710,#152711,#152712,#152713,#152714,#152715,
#152716,#152717,#152718,#152719,#152720,#152721,#152722,#152723,#152724,
#152725,#152726,#152727,#152728,#152729,#152730,#152731,#152732,#152733,
#152734,#152735,#152736,#152737,#152738,#152739,#152740,#152741,#152742,
#152743,#152744,#152745,#152746,#152747,#152748,#152749,#152750,#152751,
#152752,#152753,#152754,#152755,#152756,#152757,#152758,#152759,#152760,
#152761,#152762,#152763,#152764,#152765,#152766,#152767,#152768,#152769,
#152770,#152771,#152772,#152773,#152774,#152775,#152776,#152777,#152778,
#152779,#152780,#152781,#152782,#152783,#152784,#152785,#152786,#152787,
#152788,#152789,#152790,#152791,#152792,#152793,#152794,#152795,#152796,
#152797,#152798,#152799,#152800,#152801,#152802,#152803,#152804,#152805,
#152806,#152807,#152808,#152809,#152810,#152811,#152812,#152813,#152814,
#152815,#152816,#152817,#152818,#152819,#152820,#152821,#152822,#152823,
#152824,#152825,#152826,#152827,#152828,#152829,#152830,#152831,#152832,
#152833,#152834,#152835,#152836,#152837,#152838,#152839,#152840,#152841,
#152842,#152843,#152844,#152845,#152846,#152847,#152848,#152849,#152850,
#152851,#152852,#152853,#152854,#152855,#152856,#152857,#152858,#152859,
#152860,#152861,#152862,#152863,#152864,#152865,#152866,#152867,#152868,
#152869,#152870,#152871,#152872,#152873,#152874,#152875,#152876,#152877,
#152878,#152879,#152880,#152881,#152882,#152883,#152884,#152885,#152886,
#152887,#152888,#152889,#152890,#152891,#152892,#152893,#152894,#152895,
#152896,#152897,#152898,#152899,#152900,#152901,#152902,#152903,#152904,
#152905,#152906,#152907,#152908,#152909,#152910,#152911,#152912,#152913,
#152914,#152915,#152916,#152917,#152918,#152919,#152920,#152921,#152922,
#152923,#152924,#152925,#152926,#152927,#152928,#152929,#152930,#152931,
#152932,#152933,#152934,#152935,#152936,#152937,#152938,#152939,#152940,
#152941,#152942,#152943,#152944,#152945,#152946,#152947,#152948,#152949,
#152950,#152951,#152952,#152953,#152954,#152955,#152956,#152957,#152958,
#152959,#152960,#152961,#152962,#152963,#152964,#152965,#152966,#152967,
#152968,#152969,#152970,#152971,#152972,#152973,#152974,#152975,#152976,
#152977,#152978,#152979,#152980,#152981,#152982,#152983,#152984,#152985,
#152986,#152987,#152988,#152989,#152990,#152991,#152992,#152993,#152994,
#152995,#152996,#152997,#152998,#152999,#153000,#153001,#153002,#153003,
#153004,#153005,#153006,#153007,#153008,#153009,#153010,#153011,#153012,
#153013,#153014,#153015,#153016,#153017,#153018,#153019,#153020,#153021,
#153022,#153023,#153024,#153025,#153026,#153027,#153028,#153029,#153030,
#153031,#153032,#153033,#153034,#153035,#153036,#153037,#153038,#153039,
#153040,#153041,#153042,#153043,#153044,#153045,#153046,#153047,#153048,
#153049,#153050,#153051,#153052,#153053,#153054,#153055,#153056,#153057,
#153058,#153059,#153060,#153061,#153062,#153063,#153064,#153065,#153066,
#153067,#153068,#153069,#153070,#153071,#153072,#153073,#153074,#153075,
#153076,#153077,#153078,#153079,#153080,#153081,#153082,#153083,#153084,
#153085,#153086,#153087,#153088,#153089,#153090,#153091,#153092,#153093,
#153094,#153095,#153096,#153097,#153098,#153099,#153100,#153101,#153102,
#153103,#153104,#153105,#153106,#153107,#153108,#153109,#153110,#153111,
#153112,#153113,#153114,#153115,#153116,#153117,#153118,#153119,#153120,
#153121,#153122,#153123,#153124,#153125,#153126,#153127,#153128,#153129,
#153130,#153131,#153132,#153133,#153134,#153135,#153136,#153137,#153138,
#153139,#153140,#153141,#153142,#153143,#153144,#153145,#153146,#153147,
#153148,#153149,#153150,#153151,#153152,#153153,#153154,#153155,#153156,
#153157,#153158,#153159,#153160,#153161,#153162,#153163,#153164,#153165,
#153166,#153167,#153168,#153169,#153170,#153171,#153172,#153173,#153174,
#153175,#153176,#153177,#153178,#153179,#153180,#153181,#153182,#153183,
#153184,#153185,#153186,#153187,#153188,#153189,#153190,#153191,#153192,
#153193,#153194,#153195,#153196,#153197,#153198,#153199,#153200,#153201,
#153202,#153203,#153204,#153205,#153206,#153207,#153208,#153209,#153210,
#153211,#153212,#153213,#153214,#153215,#153216,#153217,#153218,#153219,
#153220,#153221,#153222,#153223,#153224,#153225,#153226,#153227,#153228,
#153229,#153230,#153231,#153232,#153233,#153234,#153235,#153236,#153237,
#153238,#153239,#153240,#153241,#153242,#153243,#153244,#153245,#153246,
#153247,#153248,#153249,#153250,#153251,#153252,#153253,#153254,#153255,
#153256,#153257,#153258,#153259,#153260,#153261,#153262,#153263,#153264,
#153265,#153266,#153267,#153268,#153269,#153270,#153271,#153272,#153273,
#153274,#153275,#153276,#153277,#153278,#153279,#153280,#153281,#153282,
#153283,#153284,#153285,#153286,#153287,#153288,#153289,#153290,#153291,
#153292,#153293,#153294,#153295,#153296,#153297,#153298,#153299,#153300,
#153301,#153302,#153303,#153304,#153305,#153306,#153307,#153308,#153309,
#153310,#153311,#153312,#153313,#153314,#153315,#153316,#153317,#153318,
#153319,#153320,#153321,#153322,#153323,#153324,#153325,#153326,#153327,
#153328,#153329,#153330,#153331,#153332,#153333,#153334,#153335,#153336,
#153337,#153338,#153339,#153340,#153341,#153342,#153343,#153344,#153345,
#153346,#153347,#153348,#153349,#153350,#153351,#153352,#153353,#153354,
#153355,#153356,#153357,#153358,#153359,#153360,#153361,#153362,#153363,
#153364,#153365,#153366,#153367,#153368,#153369,#153370,#153371,#153372,
#153373,#153374,#153375,#153376,#153377,#153378,#153379,#153380,#153381,
#153382,#153383,#153384,#153385,#153386,#153387,#153388,#153389,#153390,
#153391,#153392,#153393,#153394,#153395,#153396,#153397,#153398,#153399,
#153400,#153401,#153402,#153403,#153404,#153405,#153406,#153407,#153408,
#153409,#153410,#153411,#153412,#153413,#153414,#153415,#153416,#153417,
#153418,#153419,#153420,#153421,#153422,#153423,#153424,#153425,#153426,
#153427,#153428,#153429,#153430,#153431,#153432,#153433,#153434,#153435,
#153436,#153437,#153438,#153439,#153440,#153441,#153442,#153443,#153444,
#153445,#153446,#153447,#153448,#153449,#153450,#153451,#153452,#153453,
#153454,#153455,#153456,#153457,#153458,#153459,#153460,#153461,#153462,
#153463,#153464,#153465,#153466,#153467,#153468,#153469,#153470,#153471,
#153472,#153473,#153474,#153475,#153476,#153477,#153478,#153479,#153480,
#153481,#153482,#153483,#153484,#153485,#153486,#153487,#153488,#153489,
#153490,#153491,#153492,#153493,#153494,#153495,#153496,#153497,#153498,
#153499,#153500,#153501,#153502,#153503,#153504,#153505,#153506,#153507,
#153508,#153509,#153510,#153511,#153512,#153513,#153514,#153515,#153516,
#153517,#153518,#153519,#153520,#153521,#153522,#153523,#153524,#153525,
#153526,#153527,#153528,#153529,#153530,#153531,#153532,#153533,#153534,
#153535,#153536,#153537,#153538,#153539,#153540,#153541,#153542,#153543,
#153544,#153545,#153546,#153547,#153548,#153549,#153550,#153551,#153552,
#153553,#153554,#153555,#153556,#153557,#153558,#153559,#153560,#153561,
#153562,#153563,#153564,#153565,#153566,#153567,#153568,#153569,#153570,
#153571,#153572,#153573,#153574,#153575,#153576,#153577,#153578,#153579,
#153580,#153581,#153582,#153583,#153584,#153585,#153586,#153587,#153588,
#153589,#153590,#153591,#153592,#153593,#153594,#153595,#153596,#153597,
#153598,#153599,#153600,#153601,#153602,#153603,#153604,#153605,#153606,
#153607,#153608,#153609,#153610,#153611,#153612,#153613,#153614,#153615,
#153616,#153617,#153618,#153619,#153620,#153621,#153622,#153623,#153624,
#153625,#153626,#153627,#153628,#153629,#153630,#153631,#153632,#153633,
#153634,#153635,#153636,#153637,#153638,#153639,#153640,#153641,#153642,
#153643,#153644,#153645,#153646,#153647,#153648,#153649,#153650,#153651,
#153652,#153653,#153654,#153655,#153656,#153657,#153658,#153659,#153660,
#153661,#153662,#153663,#153664,#153665,#153666,#153667,#153668,#153669,
#153670,#153671,#153672,#153673,#153674,#153675,#153676,#153677,#153678,
#153679,#153680,#153681,#153682,#153683,#153684,#153685,#153686,#153687,
#153688,#153689,#153690,#153691,#153692,#153693,#153694,#153695,#153696,
#153697,#153698,#153699,#153700,#153701,#153702,#153703,#153704,#153705,
#153706,#153707,#153708,#153709,#153710,#153711,#153712,#153713,#153714,
#153715,#153716,#153717,#153718,#153719,#153720,#153721,#153722,#153723,
#153724,#153725,#153726,#153727,#153728,#153729,#153730,#153731,#153732,
#153733,#153734,#153735,#153736,#153737,#153738,#153739,#153740,#153741,
#153742,#153743,#153744,#153745,#153746,#153747,#153748,#153749,#153750,
#153751,#153752,#153753,#153754,#153755,#153756,#153757,#153758,#153759,
#153760,#153761,#153762,#153763,#153764,#153765,#153766,#153767,#153768,
#153769,#153770,#153771,#153772,#153773,#153774,#153775,#153776,#153777,
#153778,#153779,#153780,#153781,#153782,#153783,#153784,#153785,#153786,
#153787,#153788,#153789,#153790,#153791,#153792,#153793,#153794,#153795,
#153796,#153797,#153798,#153799,#153800,#153801,#153802,#153803,#153804,
#153805,#153806,#153807,#153808,#153809,#153810,#153811,#153812,#153813,
#153814,#153815,#153816,#153817,#153818,#153819,#153820,#153821,#153822,
#153823,#153824,#153825,#153826,#153827,#153828,#153829,#153830,#153831,
#153832,#153833,#153834,#153835,#153836,#153837,#153838,#153839,#153840,
#153841,#153842,#153843,#153844,#153845,#153846,#153847,#153848,#153849,
#153850,#153851,#153852,#153853,#153854,#153855,#153856,#153857,#153858,
#153859,#153860,#153861,#153862,#153863,#153864,#153865,#153866,#153867,
#153868,#153869,#153870,#153871,#153872,#153873,#153874,#153875,#153876,
#153877,#153878,#153879,#153880,#153881,#153882,#153883,#153884,#153885,
#153886,#153887,#153888,#153889,#153890,#153891,#153892,#153893,#153894,
#153895,#153896,#153897,#153898,#153899,#153900,#153901,#153902,#153903,
#153904,#153905,#153906,#153907,#153908,#153909,#153910,#153911,#153912,
#153913,#153914,#153915,#153916,#153917,#153918,#153919,#153920,#153921,
#153922,#153923,#153924,#153925,#153926,#153927,#153928,#153929,#153930,
#153931,#153932,#153933,#153934,#153935,#153936,#153937,#153938,#153939,
#153940,#153941,#153942,#153943,#153944,#153945,#153946,#153947,#153948,
#153949,#153950,#153951,#153952,#153953,#153954,#153955,#153956,#153957,
#153958,#153959,#153960,#153961,#153962,#153963,#153964,#153965,#153966,
#153967,#153968,#153969,#153970,#153971,#153972,#153973,#153974,#153975,
#153976,#153977,#153978,#153979,#153980,#153981,#153982,#153983,#153984,
#153985,#153986,#153987,#153988,#153989,#153990,#153991,#153992,#153993,
#153994,#153995,#153996,#153997,#153998,#153999,#154000,#154001,#154002,
#154003,#154004,#154005,#154006,#154007,#154008,#154009,#154010,#154011,
#154012,#154013,#154014,#154015,#154016,#154017,#154018,#154019,#154020,
#154021,#154022,#154023,#154024,#154025,#154026,#154027,#154028,#154029,
#154030,#154031,#154032,#154033,#154034,#154035,#154036,#154037,#154038,
#154039,#154040,#154041,#154042,#154043,#154044,#154045,#154046,#154047,
#154048,#154049,#154050,#154051,#154052,#154053,#154054,#154055,#154056,
#154057,#154058,#154059,#154060,#154061,#154062,#154063,#154064,#154065,
#154066,#154067,#154068,#154069,#154070,#154071,#154072,#154073,#154074,
#154075,#154076,#154077,#154078,#154079,#154080,#154081,#154082,#154083,
#154084,#154085,#154086,#154087,#154088,#154089,#154090,#154091,#154092,
#154093,#154094,#154095,#154096,#154097,#154098,#154099,#154100,#154101,
#154102,#154103,#154104,#154105,#154106,#154107,#154108,#154109,#154110,
#154111,#154112,#154113,#154114,#154115,#154116,#154117,#154118,#154119,
#154120,#154121,#154122,#154123,#154124,#154125,#154126,#154127,#154128,
#154129,#154130,#154131,#154132,#154133,#154134,#154135,#154136,#154137,
#154138,#154139,#154140,#154141,#154142,#154143,#154144,#154145,#154146,
#154147,#154148,#154149,#154150,#154151,#154152,#154153,#154154,#154155,
#154156,#154157,#154158,#154159,#154160,#154161,#154162,#154163,#154164,
#154165,#154166,#154167,#154168,#154169,#154170,#154171,#154172,#154173,
#154174,#154175,#154176,#154177,#154178,#154179,#154180,#154181,#154182,
#154183,#154184,#154185,#154186,#154187,#154188,#154189,#154190,#154191,
#154192,#154193,#154194,#154195,#154196,#154197,#154198,#154199,#154200,
#154201,#154202,#154203,#154204,#154205,#154206,#154207,#154208,#154209,
#154210,#154211,#154212,#154213,#154214,#154215,#154216,#154217,#154218,
#154219,#154220,#154221,#154222,#154223,#154224,#154225,#154226,#154227,
#154228,#154229,#154230,#154231,#154232,#154233,#154234,#154235,#154236,
#154237,#154238,#154239,#154240,#154241,#154242,#154243,#154244,#154245,
#154246,#154247,#154248,#154249,#154250,#154251,#154252,#154253,#154254,
#154255,#154256,#154257,#154258,#154259,#154260,#154261,#154262,#154263,
#154264,#154265,#154266,#154267,#154268,#154269,#154270,#154271,#154272,
#154273,#154274,#154275,#154276,#154277,#154278,#154279,#154280,#154281,
#154282,#154283,#154284,#154285,#154286,#154287,#154288,#154289,#154290,
#154291,#154292,#154293,#154294,#154295,#154296,#154297,#154298,#154299,
#154300,#154301,#154302,#154303,#154304,#154305,#154306,#154307,#154308,
#154309,#154310,#154311,#154312,#154313,#154314,#154315,#154316,#154317,
#154318,#154319,#154320,#154321,#154322,#154323,#154324,#154325,#154326,
#154327,#154328,#154329,#154330,#154331,#154332,#154333,#154334,#154335,
#154336,#154337,#154338,#154339,#154340,#154341,#154342,#154343,#154344,
#154345,#154346,#154347,#154348,#154349,#154350,#154351,#154352,#154353,
#154354,#154355,#154356,#154357,#154358,#154359,#154360,#154361,#154362,
#154363,#154364,#154365,#154366,#154367,#154368,#154369,#154370,#154371,
#154372,#154373,#154374,#154375,#154376,#154377,#154378,#154379,#154380,
#154381,#154382,#154383,#154384,#154385,#154386,#154387,#154388,#154389,
#154390,#154391,#154392,#154393,#154394,#154395,#154396,#154397,#154398,
#154399,#154400,#154401,#154402,#154403,#154404,#154405,#154406,#154407,
#154408,#154409,#154410,#154411,#154412,#154413)),.UNSPECIFIED.,.F.,.F.,
 .F.)
B_SPLINE_SURFACE_WITH_KNOTS((2,2),(3,2,2,2,2,2,2,2,2,2,2,2,2,2,2,2,2,2,
2,2,2,2,2,2,2,2,2,2,2,2,2,2,2,2,2,2,2,2,2,2,2,2,2,2,2,2,2,2,2,2,2,2,2,2,
2,2,2,2,2,2,2,2,2,2,2,2,2,2,2,2,2,2,2,2,2,2,2,2,2,2,2,2,2,2,2,2,2,2,2,2,
2,2,2,2,2,2,2,2,2,2,2,2,2,2,2,2,2,2,2,2,2,2,2,2,2,2,2,2,2,2,2,2,2,2,2,2,
2,2,2,2,2,2,2,2,2,2,2,2,2,2,2,2,2,2,2,2,2,2,2,2,2,2,2,2,2,2,2,2,2,2,2,2,
2,2,2,2,2,2,2,2,2,2,2,2,2,2,2,2,2,2,2,2,2,2,2,2,2,2,2,2,2,2,2,2,2,2,2,2,
2,2,2,2,2,2,2,2,2,2,2,2,2,2,2,2,2,2,2,2,2,2,2,2,2,2,2,2,2,2,2,2,2,2,2,2,
2,2,2,2,2,2,2,2,2,2,2,2,2,2,2,2,2,2,2,2,2,2,2,2,2,2,2,2,2,2,2,2,2,2,2,2,
2,2,2,2,2,2,2,2,2,2,2,2,2,2,2,2,2,2,2,2,2,2,2,2,2,2,2,2,2,2,2,2,2,2,2,2,
2,2,2,2,2,2,2,2,2,2,2,2,2,2,2,2,2,2,2,2,2,2,2,2,2,2,2,2,2,2,2,2,2,2,2,2,
2,2,2,2,2,2,2,2,2,2,2,2,2,2,2,2,2,2,2,2,2,2,2,2,2,2,2,2,2,2,2,2,2,2,2,2,
2,2,2,2,2,2,2,2,2,2,2,2,2,2,2,2,2,2,2,2,2,2,2,2,2,2,2,2,2,2,2,2,2,2,2,2,
2,2,2,2,2,2,2,2,2,2,2,2,2,2,2,2,2,2,2,2,2,2,2,2,2,2,2,2,2,2,2,2,2,2,2,2,
2,2,2,2,2,2,2,2,2,2,2,2,2,2,2,2,2,2,2,2,2,2,2,2,2,2,2,2,2,2,2,2,2,2,2,2,
2,2,2,2,2,2,2,2,2,2,2,2,2,2,2,2,2,2,2,2,2,2,2,2,2,2,2,2,2,2,2,2,2,2,2,2,
2,2,2,2,2,2,2,2,2,2,2,2,2,2,2,2,2,2,2,2,2,2,2,2,2,2,2,2,2,2,2,2,2,2,2,2,
2,2,2,2,2,2,2,2,2,2,2,2,2,2,2,2,2,2,2,2,2,2,2,2,2,2,2,2,2,2,2,2,2,2,2,2,
2,2,2,2,2,2,2,2,2,2,2,2,2,2,2,2,2,2,2,2,2,2,2,2,2,2,2,2,2,2,2,2,2,2,2,2,
2,2,2,2,2,2,2,2,2,2,2,2,2,2,2,2,2,2,2,2,2,2,2,2,2,2,2,2,2,2,2,2,2,2,2,2,
2,2,2,2,2,2,2,2,2,2,2,2,2,2,2,2,2,2,2,2,2,2,2,2,2,2,2,2,2,2,2,2,2,2,2,2,
2,2,2,2,2,2,2,2,2,2,2,2,2,2,2,2,2,2,2,2,2,2,2,2,2,2,2,2,2,2,2,2,2,2,2,2,
2,2,2,2,2,2,2,2,2,2,2,2,2,2,2,2,2,2,2,2,2,2,2,2,2,2,2,2,2,2,2,2,2,2,2,2,
2,2,2,2,2,2,2,2,2,2,2,2,2,2,2,2,2,2,2,2,2,2,2,2,2,2,2,2,2,2,2,2,2,2,2,2,
2,2,2,2,2,2,2,2,2,2,2,2,2,2,2,2,2,2,2,2,2,2,2,2,2,2,2,2,2,2,2,2,2,2,2,2,
2,2,2,2,2,2,2,2,2,2,2,2,2,2,2,2,2,2,2,2,2,2,2,2,2,2,2,2,2,2,2,2,2,2,2,2,
2,2,2,2,2,2,2,2,2,2,2,2,2,2,2,2,2,2,2,2,2,2,2,2,2,2,2,2,2,2,2,2,2,2,2,2,
2,2,2,2,2,2,2,2,2,2,2,2,2,2,2,2,2,2,2,2,2,2,2,2,2,2,2,2,2,2,2,2,2,2,2,2,
2,2,2,2,2,2,2,2,2,2,2,2,2,2,2,2,2,2,2,2,2,2,2,2,2,2,2,2,2,2,2,2,2,2,2,2,
2,2,2,2,2,2,2,2,2,2,2,2,2,2,2,2,3),(0.,1.),(0.,0.000980392156862745,0.00196078431372549,
0.00294117647058824,0.00392156862745098,0.00490196078431373,0.00588235294117647,
0.00686274509803922,0.00784313725490196,0.00882352941176471,0.00980392156862745,
0.0107843137254902,0.0117647058823529,0.0127450980392157,0.0137254901960784,
0.0147058823529412,0.0156862745098039,0.0166666666666667,0.0176470588235294,
0.0186274509803922,0.0196078431372549,0.0205882352941176,0.0215686274509804,
0.0225490196078431,0.0235294117647059,0.0245098039215686,0.0254901960784314,
0.0264705882352941,0.0274509803921569,0.0284313725490196,0.0294117647058824,
0.0303921568627451,0.0313725490196078,0.0323529411764706,0.0333333333333333,
0.0343137254901961,0.0352941176470588,0.0362745098039216,0.0372549019607843,
0.0382352941176471,0.0392156862745098,0.0401960784313726,0.0411764705882353,
0.042156862745098,0.0431372549019608,0.0441176470588235,0.0450980392156863,
0.046078431372549,0.0470588235294118,0.0480392156862745,0.0490196078431373,
0.05,0.0509803921568627,0.0519607843137255,0.0529411764705882,0.053921568627451,
0.0549019607843137,0.0558823529411765,0.0568627450980392,0.057843137254902,
0.0588235294117647,0.0598039215686275,0.0607843137254902,0.0617647058823529,
0.0627450980392157,0.0637254901960784,0.0647058823529412,0.0656862745098039,
0.0666666666666667,0.0676470588235294,0.0686274509803922,0.0696078431372549,
0.0705882352941176,0.0715686274509804,0.0725490196078431,0.0735294117647059,
0.0745098039215686,0.0754901960784314,0.0764705882352941,0.0774509803921569,
0.0784313725490196,0.0794117647058823,0.0803921568627451,0.0813725490196078,
0.0823529411764706,0.0833333333333333,0.0843137254901961,0.0852941176470588,
0.0862745098039216,0.0872549019607843,0.0882352941176471,0.0892156862745098,
0.0901960784313725,0.0911764705882353,0.092156862745098,0.0931372549019608,
0.0941176470588235,0.0950980392156863,0.096078431372549,0.0970588235294118,
0.0980392156862745,0.0990196078431373,0.1,0.100980392156863,0.101960784313725,
0.102941176470588,0.103921568627451,0.104901960784314,0.105882352941176,
0.106862745098039,0.107843137254902,0.108823529411765,0.109803921568627,
0.11078431372549,0.111764705882353,0.112745098039216,0.113725490196078,
0.114705882352941,0.115686274509804,0.116666666666667,0.117647058823529,
0.118627450980392,0.119607843137255,0.120588235294118,0.12156862745098,
0.122549019607843,0.123529411764706,0.124509803921569,0.125490196078431,
0.126470588235294,0.127450980392157,0.12843137254902,0.129411764705882,
0.130392156862745,0.131372549019608,0.132352941176471,0.133333333333333,
0.134313725490196,0.135294117647059,0.136274509803922,0.137254901960784,
0.138235294117647,0.13921568627451,0.140196078431373,0.141176470588235,
0.142156862745098,0.143137254901961,0.144117647058824,0.145098039215686,
0.146078431372549,0.147058823529412,0.148039215686275,0.149019607843137,
0.15,0.150980392156863,0.151960784313725,0.152941176470588,0.153921568627451,
0.154901960784314,0.155882352941176,0.156862745098039,0.157843137254902,
0.158823529411765,0.159803921568627,0.16078431372549,0.161764705882353,
0.162745098039216,0.163725490196078,0.164705882352941,0.165686274509804,
0.166666666666667,0.167647058823529,0.168627450980392,0.169607843137255,
0.170588235294118,0.17156862745098,0.172549019607843,0.173529411764706,
0.174509803921569,0.175490196078431,0.176470588235294,0.177450980392157,
0.17843137254902,0.179411764705882,0.180392156862745,0.181372549019608,
0.182352941176471,0.183333333333333,0.184313725490196,0.185294117647059,
0.186274509803922,0.187254901960784,0.188235294117647,0.18921568627451,
0.190196078431373,0.191176470588235,0.192156862745098,0.193137254901961,
0.194117647058824,0.195098039215686,0.196078431372549,0.197058823529412,
0.198039215686275,0.199019607843137,0.2,0.200980392156863,0.201960784313725,
0.202941176470588,0.203921568627451,0.204901960784314,0.205882352941176,
0.206862745098039,0.207843137254902,0.208823529411765,0.209803921568627,
0.21078431372549,0.211764705882353,0.212745098039216,0.213725490196078,
0.214705882352941,0.215686274509804,0.216666666666667,0.217647058823529,
0.218627450980392,0.219607843137255,0.220588235294118,0.22156862745098,
0.222549019607843,0.223529411764706,0.224509803921569,0.225490196078431,
0.226470588235294,0.227450980392157,0.22843137254902,0.229411764705882,
0.230392156862745,0.231372549019608,0.232352941176471,0.233333333333333,
0.234313725490196,0.235294117647059,0.236274509803922,0.237254901960784,
0.238235294117647,0.23921568627451,0.240196078431373,0.241176470588235,
0.242156862745098,0.243137254901961,0.244117647058824,0.245098039215686,
0.246078431372549,0.247058823529412,0.248039215686275,0.249019607843137,
0.25,0.250980392156863,0.251960784313725,0.252941176470588,0.253921568627451,
0.254901960784314,0.255882352941176,0.256862745098039,0.257843137254902,
0.258823529411765,0.259803921568627,0.26078431372549,0.261764705882353,
0.262745098039216,0.263725490196078,0.264705882352941,0.265686274509804,
0.266666666666667,0.267647058823529,0.268627450980392,0.269607843137255,
0.270588235294118,0.27156862745098,0.272549019607843,0.273529411764706,
0.274509803921569,0.275490196078431,0.276470588235294,0.277450980392157,
0.27843137254902,0.279411764705882,0.280392156862745,0.281372549019608,
0.282352941176471,0.283333333333333,0.284313725490196,0.285294117647059,
0.286274509803922,0.287254901960784,0.288235294117647,0.28921568627451,
0.290196078431373,0.291176470588235,0.292156862745098,0.293137254901961,
0.294117647058824,0.295098039215686,0.296078431372549,0.297058823529412,
0.298039215686275,0.299019607843137,0.3,0.300980392156863,0.301960784313725,
0.302941176470588,0.303921568627451,0.304901960784314,0.305882352941176,
0.306862745098039,0.307843137254902,0.308823529411765,0.309803921568627,
0.31078431372549,0.311764705882353,0.312745098039216,0.313725490196078,
0.314705882352941,0.315686274509804,0.316666666666667,0.317647058823529,
0.318627450980392,0.319607843137255,0.320588235294118,0.32156862745098,
0.322549019607843,0.323529411764706,0.324509803921569,0.325490196078431,
0.326470588235294,0.327450980392157,0.32843137254902,0.329411764705882,
0.330392156862745,0.331372549019608,0.332352941176471,0.333333333333333,
0.334313725490196,0.335294117647059,0.336274509803922,0.337254901960784,
0.338235294117647,0.33921568627451,0.340196078431373,0.341176470588235,
0.342156862745098,0.343137254901961,0.344117647058824,0.345098039215686,
0.346078431372549,0.347058823529412,0.348039215686274,0.349019607843137,
0.35,0.350980392156863,0.351960784313726,0.352941176470588,0.353921568627451,
0.354901960784314,0.355882352941176,0.356862745098039,0.357843137254902,
0.358823529411765,0.359803921568627,0.36078431372549,0.361764705882353,
0.362745098039216,0.363725490196078,0.364705882352941,0.365686274509804,
0.366666666666667,0.367647058823529,0.368627450980392,0.369607843137255,
0.370588235294118,0.37156862745098,0.372549019607843,0.373529411764706,
0.374509803921569,0.375490196078431,0.376470588235294,0.377450980392157,
0.37843137254902,0.379411764705882,0.380392156862745,0.381372549019608,
0.382352941176471,0.383333333333333,0.384313725490196,0.385294117647059,
0.386274509803922,0.387254901960784,0.388235294117647,0.38921568627451,
0.390196078431373,0.391176470588235,0.392156862745098,0.393137254901961,
0.394117647058824,0.395098039215686,0.396078431372549,0.397058823529412,
0.398039215686274,0.399019607843137,0.4,0.400980392156863,0.401960784313726,
0.402941176470588,0.403921568627451,0.404901960784314,0.405882352941176,
0.406862745098039,0.407843137254902,0.408823529411765,0.409803921568627,
0.41078431372549,0.411764705882353,0.412745098039216,0.413725490196078,
0.414705882352941,0.415686274509804,0.416666666666667,0.417647058823529,
0.418627450980392,0.419607843137255,0.420588235294118,0.42156862745098,
0.422549019607843,0.423529411764706,0.424509803921569,0.425490196078431,
0.426470588235294,0.427450980392157,0.42843137254902,0.429411764705882,
0.430392156862745,0.431372549019608,0.432352941176471,0.433333333333333,
0.434313725490196,0.435294117647059,0.436274509803922,0.437254901960784,
0.438235294117647,0.43921568627451,0.440196078431373,0.441176470588235,
0.442156862745098,0.443137254901961,0.444117647058824,0.445098039215686,
0.446078431372549,0.447058823529412,0.448039215686275,0.449019607843137,
0.45,0.450980392156863,0.451960784313725,0.452941176470588,0.453921568627451,
0.454901960784314,0.455882352941176,0.456862745098039,0.457843137254902,
0.458823529411765,0.459803921568627,0.46078431372549,0.461764705882353,
0.462745098039216,0.463725490196078,0.464705882352941,0.465686274509804,
0.466666666666667,0.467647058823529,0.468627450980392,0.469607843137255,
0.470588235294118,0.47156862745098,0.472549019607843,0.473529411764706,
0.474509803921569,0.475490196078431,0.476470588235294,0.477450980392157,
0.47843137254902,0.479411764705882,0.480392156862745,0.481372549019608,
0.482352941176471,0.483333333333333,0.484313725490196,0.485294117647059,
0.486274509803922,0.487254901960784,0.488235294117647,0.48921568627451,
0.490196078431373,0.491176470588235,0.492156862745098,0.493137254901961,
0.494117647058824,0.495098039215686,0.496078431372549,0.497058823529412,
0.498039215686275,0.499019607843137,0.5,0.500980392156863,0.501960784313725,
0.502941176470588,0.503921568627451,0.504901960784314,0.505882352941176,
0.506862745098039,0.507843137254902,0.508823529411765,0.509803921568627,
0.51078431372549,0.511764705882353,0.512745098039216,0.513725490196078,
0.514705882352941,0.515686274509804,0.516666666666667,0.517647058823529,
0.518627450980392,0.519607843137255,0.520588235294118,0.52156862745098,
0.522549019607843,0.523529411764706,0.524509803921569,0.525490196078431,
0.526470588235294,0.527450980392157,0.52843137254902,0.529411764705882,
0.530392156862745,0.531372549019608,0.532352941176471,0.533333333333333,
0.534313725490196,0.535294117647059,0.536274509803922,0.537254901960784,
0.538235294117647,0.53921568627451,0.540196078431373,0.541176470588235,
0.542156862745098,0.543137254901961,0.544117647058823,0.545098039215686,
0.546078431372549,0.547058823529412,0.548039215686275,0.549019607843137,
0.55,0.550980392156863,0.551960784313726,0.552941176470588,0.553921568627451,
0.554901960784314,0.555882352941176,0.556862745098039,0.557843137254902,
0.558823529411765,0.559803921568627,0.56078431372549,0.561764705882353,
0.562745098039216,0.563725490196078,0.564705882352941,0.565686274509804,
0.566666666666667,0.567647058823529,0.568627450980392,0.569607843137255,
0.570588235294118,0.57156862745098,0.572549019607843,0.573529411764706,
0.574509803921569,0.575490196078431,0.576470588235294,0.577450980392157,
0.57843137254902,0.579411764705882,0.580392156862745,0.581372549019608,
0.582352941176471,0.583333333333333,0.584313725490196,0.585294117647059,
0.586274509803922,0.587254901960784,0.588235294117647,0.58921568627451,
0.590196078431373,0.591176470588235,0.592156862745098,0.593137254901961,
0.594117647058824,0.595098039215686,0.596078431372549,0.597058823529412,
0.598039215686274,0.599019607843137,0.6,0.600980392156863,0.601960784313725,
0.602941176470588,0.603921568627451,0.604901960784314,0.605882352941176,
0.606862745098039,0.607843137254902,0.608823529411765,0.609803921568628,
0.61078431372549,0.611764705882353,0.612745098039216,0.613725490196078,
0.614705882352941,0.615686274509804,0.616666666666667,0.617647058823529,
0.618627450980392,0.619607843137255,0.620588235294118,0.62156862745098,
0.622549019607843,0.623529411764706,0.624509803921569,0.625490196078431,
0.626470588235294,0.627450980392157,0.62843137254902,0.629411764705882,
0.630392156862745,0.631372549019608,0.632352941176471,0.633333333333333,
0.634313725490196,0.635294117647059,0.636274509803922,0.637254901960784,
0.638235294117647,0.63921568627451,0.640196078431372,0.641176470588235,
0.642156862745098,0.643137254901961,0.644117647058824,0.645098039215686,
0.646078431372549,0.647058823529412,0.648039215686275,0.649019607843137,
0.65,0.650980392156863,0.651960784313726,0.652941176470588,0.653921568627451,
0.654901960784314,0.655882352941176,0.656862745098039,0.657843137254902,
0.658823529411765,0.659803921568627,0.66078431372549,0.661764705882353,
0.662745098039216,0.663725490196078,0.664705882352941,0.665686274509804,
0.666666666666667,0.667647058823529,0.668627450980392,0.669607843137255,
0.670588235294118,0.67156862745098,0.672549019607843,0.673529411764706,
0.674509803921569,0.675490196078431,0.676470588235294,0.677450980392157,
0.67843137254902,0.679411764705882,0.680392156862745,0.681372549019608,
0.682352941176471,0.683333333333333,0.684313725490196,0.685294117647059,
0.686274509803922,0.687254901960784,0.688235294117647,0.68921568627451,
0.690196078431373,0.691176470588235,0.692156862745098,0.693137254901961,
0.694117647058824,0.695098039215686,0.696078431372549,0.697058823529412,
0.698039215686274,0.699019607843137,0.7,0.700980392156863,0.701960784313725,
0.702941176470588,0.703921568627451,0.704901960784314,0.705882352941177,
0.706862745098039,0.707843137254902,0.708823529411765,0.709803921568627,
0.71078431372549,0.711764705882353,0.712745098039216,0.713725490196078,
0.714705882352941,0.715686274509804,0.716666666666667,0.717647058823529,
0.718627450980392,0.719607843137255,0.720588235294118,0.72156862745098,
0.722549019607843,0.723529411764706,0.724509803921569,0.725490196078431,
0.726470588235294,0.727450980392157,0.72843137254902,0.729411764705882,
0.730392156862745,0.731372549019608,0.732352941176471,0.733333333333333,
0.734313725490196,0.735294117647059,0.736274509803922,0.737254901960784,
0.738235294117647,0.73921568627451,0.740196078431373,0.741176470588235,
0.742156862745098,0.743137254901961,0.744117647058824,0.745098039215686,
0.746078431372549,0.747058823529412,0.748039215686275,0.749019607843137,
0.75,0.750980392156863,0.751960784313725,0.752941176470588,0.753921568627451,
0.754901960784314,0.755882352941176,0.756862745098039,0.757843137254902,
0.758823529411765,0.759803921568627,0.76078431372549,0.761764705882353,
0.762745098039216,0.763725490196078,0.764705882352941,0.765686274509804,
0.766666666666667,0.767647058823529,0.768627450980392,0.769607843137255,
0.770588235294118,0.77156862745098,0.772549019607843,0.773529411764706,
0.774509803921569,0.775490196078431,0.776470588235294,0.777450980392157,
0.77843137254902,0.779411764705882,0.780392156862745,0.781372549019608,
0.782352941176471,0.783333333333333,0.784313725490196,0.785294117647059,
0.786274509803922,0.787254901960784,0.788235294117647,0.78921568627451,
0.790196078431373,0.791176470588235,0.792156862745098,0.793137254901961,
0.794117647058823,0.795098039215686,0.796078431372549,0.797058823529412,
0.798039215686275,0.799019607843137,0.8,0.800980392156863,0.801960784313726,
0.802941176470588,0.803921568627451,0.804901960784314,0.805882352941176,
0.806862745098039,0.807843137254902,0.808823529411765,0.809803921568627,
0.81078431372549,0.811764705882353,0.812745098039216,0.813725490196078,
0.814705882352941,0.815686274509804,0.816666666666667,0.817647058823529,
0.818627450980392,0.819607843137255,0.820588235294118,0.82156862745098,
0.822549019607843,0.823529411764706,0.824509803921569,0.825490196078431,
0.826470588235294,0.827450980392157,0.82843137254902,0.829411764705882,
0.830392156862745,0.831372549019608,0.832352941176471,0.833333333333333,
0.834313725490196,0.835294117647059,0.836274509803922,0.837254901960784,
0.838235294117647,0.83921568627451,0.840196078431373,0.841176470588235,
0.842156862745098,0.843137254901961,0.844117647058824,0.845098039215686,
0.846078431372549,0.847058823529412,0.848039215686274,0.849019607843137,
0.85,0.850980392156863,0.851960784313725,0.852941176470588,0.853921568627451,
0.854901960784314,0.855882352941176,0.856862745098039,0.857843137254902,
0.858823529411765,0.859803921568628,0.86078431372549,0.861764705882353,
0.862745098039216,0.863725490196078,0.864705882352941,0.865686274509804,
0.866666666666667,0.867647058823529,0.868627450980392,0.869607843137255,
0.870588235294118,0.87156862745098,0.872549019607843,0.873529411764706,
0.874509803921569,0.875490196078431,0.876470588235294,0.877450980392157,
0.87843137254902,0.879411764705882,0.880392156862745,0.881372549019608,
0.882352941176471,0.883333333333333,0.884313725490196,0.885294117647059,
0.886274509803922,0.887254901960784,0.888235294117647,0.88921568627451,
0.890196078431372,0.891176470588235,0.892156862745098,0.893137254901961,
0.894117647058824,0.895098039215686,0.896078431372549,0.897058823529412,
0.898039215686275,0.899019607843137,0.9,0.900980392156863,0.901960784313726,
0.902941176470588,0.903921568627451,0.904901960784314,0.905882352941176,
0.906862745098039,0.907843137254902,0.908823529411765,0.909803921568627,
0.91078431372549,0.911764705882353,0.912745098039216,0.913725490196078,
0.914705882352941,0.915686274509804,0.916666666666667,0.917647058823529,
0.918627450980392,0.919607843137255,0.920588235294118,0.92156862745098,
0.922549019607843,0.923529411764706,0.924509803921569,0.925490196078431,
0.926470588235294,0.927450980392157,0.92843137254902,0.929411764705882,
0.930392156862745,0.931372549019608,0.932352941176471,0.933333333333333,
0.934313725490196,0.935294117647059,0.936274509803922,0.937254901960784,
0.938235294117647,0.93921568627451,0.940196078431373,0.941176470588235,
0.942156862745098,0.943137254901961,0.944117647058824,0.945098039215686,
0.946078431372549,0.947058823529412,0.948039215686274,0.949019607843137,
0.95,0.950980392156863,0.951960784313725,0.952941176470588,0.953921568627451,
0.954901960784314,0.955882352941177,0.956862745098039,0.957843137254902,
0.958823529411765,0.959803921568627,0.96078431372549,0.961764705882353,
0.962745098039216,0.963725490196078,0.964705882352941,0.965686274509804,
0.966666666666667,0.967647058823529,0.968627450980392,0.969607843137255,
0.970588235294118,0.97156862745098,0.972549019607843,0.973529411764706,
0.974509803921569,0.975490196078431,0.976470588235294,0.977450980392157,
0.97843137254902,0.979411764705882,0.980392156862745,0.981372549019608,
0.982352941176471,0.983333333333333,0.984313725490196,0.985294117647059,
0.985937314000279),.UNSPECIFIED.)
GEOMETRIC_REPRESENTATION_ITEM()
RATIONAL_B_SPLINE_SURFACE(((1.,0.995734176295034,1.,0.995734176295034,1.,
0.995734176295034,1.,0.995734176295034,1.,0.995734176295034,1.,0.995734176295034,
1.,0.995734176295034,1.,0.995734176295034,1.,0.995734176295034,1.,0.995734176295034,
1.,0.995734176295034,1.,0.995734176295034,1.,0.995734176295034,1.,0.995734176295034,
1.,0.995734176295034,1.,0.995734176295034,1.,0.995734176295034,1.,0.995734176295034,
1.,0.995734176295034,1.,0.995734176295034,1.,0.995734176295034,1.,0.995734176295034,
1.,0.995734176295034,1.,0.995734176295034,1.,0.995734176295034,1.,0.995734176295034,
1.,0.995734176295034,1.,0.995734176295034,1.,0.995734176295034,1.,0.995734176295034,
1.,0.995734176295034,1.,0.995734176295034,1.,0.995734176295034,1.,0.995734176295034,
1.,0.995734176295034,1.,0.995734176295034,1.,0.995734176295034,1.,0.995734176295034,
1.,0.995734176295034,1.,0.995734176295034,1.,0.995734176295034,1.,0.995734176295034,
1.,0.995734176295034,1.,0.995734176295034,1.,0.995734176295034,1.,0.995734176295034,
1.,0.995734176295034,1.,0.995734176295034,1.,0.995734176295034,1.,0.995734176295034,
1.,0.995734176295034,1.,0.995734176295034,1.,0.995734176295034,1.,0.995734176295034,
1.,0.995734176295034,1.,0.995734176295034,1.,0.995734176295034,1.,0.995734176295034,
1.,0.995734176295034,1.,0.995734176295034,1.,0.995734176295034,1.,0.995734176295034,
1.,0.995734176295034,1.,0.995734176295034,1.,0.995734176295034,1.,0.995734176295034,
1.,0.995734176295034,1.,0.995734176295034,1.,0.995734176295034,1.,0.995734176295034,
1.,0.995734176295034,1.,0.995734176295034,1.,0.995734176295034,1.,0.995734176295034,
1.,0.995734176295034,1.,0.995734176295034,1.,0.995734176295034,1.,0.995734176295034,
1.,0.995734176295034,1.,0.995734176295034,1.,0.995734176295034,1.,0.995734176295034,
1.,0.995734176295034,1.,0.995734176295034,1.,0.995734176295034,1.,0.995734176295034,
1.,0.995734176295034,1.,0.995734176295034,1.,0.995734176295034,1.,0.995734176295034,
1.,0.995734176295034,1.,0.995734176295034,1.,0.995734176295034,1.,0.995734176295034,
1.,0.995734176295034,1.,0.995734176295034,1.,0.995734176295034,1.,0.995734176295034,
1.,0.995734176295034,1.,0.995734176295034,1.,0.995734176295034,1.,0.995734176295034,
1.,0.995734176295034,1.,0.995734176295034,1.,0.995734176295034,1.,0.995734176295034,
1.,0.995734176295034,1.,0.995734176295034,1.,0.995734176295034,1.,0.995734176295034,
1.,0.995734176295034,1.,0.995734176295034,1.,0.995734176295034,1.,0.995734176295034,
1.,0.995734176295034,1.,0.995734176295034,1.,0.995734176295034,1.,0.995734176295034,
1.,0.995734176295034,1.,0.995734176295034,1.,0.995734176295034,1.,0.995734176295034,
1.,0.995734176295034,1.,0.995734176295034,1.,0.995734176295034,1.,0.995734176295034,
1.,0.995734176295034,1.,0.995734176295034,1.,0.995734176295034,1.,0.995734176295034,
1.,0.995734176295034,1.,0.995734176295034,1.,0.995734176295034,1.,0.995734176295034,
1.,0.995734176295034,1.,0.995734176295034,1.,0.995734176295034,1.,0.995734176295034,
1.,0.995734176295034,1.,0.995734176295034,1.,0.995734176295034,1.,0.995734176295034,
1.,0.995734176295034,1.,0.995734176295034,1.,0.995734176295034,1.,0.995734176295034,
1.,0.995734176295034,1.,0.995734176295034,1.,0.995734176295034,1.,0.995734176295034,
1.,0.995734176295034,1.,0.995734176295034,1.,0.995734176295034,1.,0.995734176295034,
1.,0.995734176295034,1.,0.995734176295034,1.,0.995734176295034,1.,0.995734176295034,
1.,0.995734176295034,1.,0.995734176295034,1.,0.995734176295034,1.,0.995734176295034,
1.,0.995734176295034,1.,0.995734176295034,1.,0.995734176295034,1.,0.995734176295034,
1.,0.995734176295034,1.,0.995734176295034,1.,0.995734176295034,1.,0.995734176295034,
1.,0.995734176295034,1.,0.995734176295034,1.,0.995734176295034,1.,0.995734176295034,
1.,0.995734176295034,1.,0.995734176295034,1.,0.995734176295034,1.,0.995734176295034,
1.,0.995734176295034,1.,0.995734176295034,1.,0.995734176295034,1.,0.995734176295034,
1.,0.995734176295034,1.,0.995734176295034,1.,0.995734176295034,1.,0.995734176295034,
1.,0.995734176295034,1.,0.995734176295034,1.,0.995734176295034,1.,0.995734176295034,
1.,0.995734176295034,1.,0.995734176295034,1.,0.995734176295034,1.,0.995734176295034,
1.,0.995734176295034,1.,0.995734176295034,1.,0.995734176295034,1.,0.995734176295034,
1.,0.995734176295034,1.,0.995734176295034,1.,0.995734176295034,1.,0.995734176295034,
1.,0.995734176295034,1.,0.995734176295034,1.,0.995734176295034,1.,0.995734176295034,
1.,0.995734176295034,1.,0.995734176295034,1.,0.995734176295034,1.,0.995734176295034,
1.,0.995734176295034,1.,0.995734176295034,1.,0.995734176295034,1.,0.995734176295034,
1.,0.995734176295034,1.,0.995734176295034,1.,0.995734176295034,1.,0.995734176295034,
1.,0.995734176295034,1.,0.995734176295034,1.,0.995734176295034,1.,0.995734176295034,
1.,0.995734176295034,1.,0.995734176295034,1.,0.995734176295034,1.,0.995734176295034,
1.,0.995734176295034,1.,0.995734176295034,1.,0.995734176295034,1.,0.995734176295034,
1.,0.995734176295034,1.,0.995734176295034,1.,0.995734176295034,1.,0.995734176295034,
1.,0.995734176295034,1.,0.995734176295034,1.,0.995734176295034,1.,0.995734176295034,
1.,0.995734176295034,1.,0.995734176295034,1.,0.995734176295034,1.,0.995734176295034,
1.,0.995734176295034,1.,0.995734176295034,1.,0.995734176295034,1.,0.995734176295034,
1.,0.995734176295034,1.,0.995734176295034,1.,0.995734176295034,1.,0.995734176295034,
1.,0.995734176295034,1.,0.995734176295034,1.,0.995734176295034,1.,0.995734176295034,
1.,0.995734176295034,1.,0.995734176295034,1.,0.995734176295034,1.,0.995734176295034,
1.,0.995734176295034,1.,0.995734176295034,1.,0.995734176295034,1.,0.995734176295034,
1.,0.995734176295034,1.,0.995734176295034,1.,0.995734176295034,1.,0.995734176295034,
1.,0.995734176295034,1.,0.995734176295034,1.,0.995734176295034,1.,0.995734176295034,
1.,0.995734176295034,1.,0.995734176295034,1.,0.995734176295034,1.,0.995734176295034,
1.,0.995734176295034,1.,0.995734176295034,1.,0.995734176295034,1.,0.995734176295034,
1.,0.995734176295034,1.,0.995734176295034,1.,0.995734176295034,1.,0.995734176295034,
1.,0.995734176295034,1.,0.995734176295034,1.,0.995734176295034,1.,0.995734176295034,
1.,0.995734176295034,1.,0.995734176295034,1.,0.995734176295034,1.,0.995734176295034,
1.,0.995734176295034,1.,0.995734176295034,1.,0.995734176295034,1.,0.995734176295034,
1.,0.995734176295034,1.,0.995734176295034,1.,0.995734176295034,1.,0.995734176295034,
1.,0.995734176295034,1.,0.995734176295034,1.,0.995734176295034,1.,0.995734176295034,
1.,0.995734176295034,1.,0.995734176295034,1.,0.995734176295034,1.,0.995734176295034,
1.,0.995734176295034,1.,0.995734176295034,1.,0.995734176295034,1.,0.995734176295034,
1.,0.995734176295034,1.,0.995734176295034,1.,0.995734176295034,1.,0.995734176295034,
1.,0.995734176295034,1.,0.995734176295034,1.,0.995734176295034,1.,0.995734176295034,
1.,0.995734176295034,1.,0.995734176295034,1.,0.995734176295034,1.,0.995734176295034,
1.,0.995734176295034,1.,0.995734176295034,1.,0.995734176295034,1.,0.995734176295034,
1.,0.995734176295034,1.,0.995734176295034,1.,0.995734176295034,1.,0.995734176295034,
1.,0.995734176295034,1.,0.995734176295034,1.,0.995734176295034,1.,0.995734176295034,
1.,0.995734176295034,1.,0.995734176295034,1.,0.995734176295034,1.,0.995734176295034,
1.,0.995734176295034,1.,0.995734176295034,1.,0.995734176295034,1.,0.995734176295034,
1.,0.995734176295034,1.,0.995734176295034,1.,0.995734176295034,1.,0.995734176295034,
1.,0.995734176295034,1.,0.995734176295034,1.,0.995734176295034,1.,0.995734176295034,
1.,0.995734176295034,1.,0.995734176295034,1.,0.995734176295034,1.,0.995734176295034,
1.,0.995734176295034,1.,0.995734176295034,1.,0.995734176295034,1.,0.995734176295034,
1.,0.995734176295034,1.,0.995734176295034,1.,0.995734176295034,1.,0.995734176295034,
1.,0.995734176295034,1.,0.995734176295034,1.,0.995734176295034,1.,0.995734176295034,
1.,0.995734176295034,1.,0.995734176295034,1.,0.995734176295034,1.,0.995734176295034,
1.,0.995734176295034,1.,0.995734176295034,1.,0.995734176295034,1.,0.995734176295034,
1.,0.995734176295034,1.,0.995734176295034,1.,0.995734176295034,1.,0.995734176295034,
1.,0.995734176295034,1.,0.995734176295034,1.,0.995734176295034,1.,0.995734176295034,
1.,0.995734176295034,1.,0.995734176295034,1.,0.995734176295034,1.,0.995734176295034,
1.,0.995734176295034,1.,0.995734176295034,1.,0.995734176295034,1.,0.995734176295034,
1.,0.995734176295034,1.,0.995734176295034,1.,0.995734176295034,1.,0.995734176295034,
1.,0.995734176295034,1.,0.995734176295034,1.,0.995734176295034,1.,0.995734176295034,
1.,0.995734176295034,1.,0.995734176295034,1.,0.995734176295034,1.,0.995734176295034,
1.,0.995734176295034,1.,0.995734176295034,1.,0.995734176295034,1.,0.995734176295034,
1.,0.995734176295034,1.,0.995734176295034,1.,0.995734176295034,1.,0.995734176295034,
1.,0.995734176295034,1.,0.995734176295034,1.,0.995734176295034,1.,0.995734176295034,
1.,0.995734176295034,1.,0.995734176295034,1.,0.995734176295034,1.,0.995734176295034,
1.,0.995734176295034,1.,0.995734176295034,1.,0.995734176295034,1.,0.995734176295034,
1.,0.995734176295034,1.,0.995734176295034,1.,0.995734176295034,1.,0.995734176295034,
1.,0.995734176295034,1.,0.995734176295034,1.,0.995734176295034,1.,0.995734176295034,
1.,0.995734176295034,1.,0.995734176295034,1.,0.995734176295034,1.,0.995734176295034,
1.,0.995734176295034,1.,0.995734176295034,1.,0.995734176295034,1.,0.995734176295034,
1.,0.995734176295034,1.,0.995734176295034,1.,0.995734176295034,1.,0.995734176295034,
1.,0.995734176295034,1.,0.995734176295034,1.,0.995734176295034,1.,0.995734176295034,
1.,0.995734176295034,1.,0.995734176295034,1.,0.995734176295034,1.,0.995734176295034,
1.,0.995734176295034,1.,0.995734176295034,1.,0.995734176295034,1.,0.995734176295034,
1.,0.995734176295034,1.,0.995734176295034,1.,0.995734176295034,1.,0.995734176295034,
1.,0.995734176295034,1.,0.995734176295034,1.,0.995734176295034,1.,0.995734176295034,
1.,0.995734176295034,1.,0.995734176295034,1.,0.995734176295034,1.,0.995734176295034,
1.,0.995734176295034,1.,0.995734176295034,1.,0.995734176295034,1.,0.995734176295034,
1.,0.995734176295034,1.,0.995734176295034,1.,0.995734176295034,1.,0.995734176295034,
1.,0.995734176295034,1.,0.995734176295034,1.,0.995734176295034,1.,0.995734176295034,
1.,0.995734176295034,1.,0.995734176295034,1.,0.995734176295034,1.,0.995734176295034,
1.,0.995734176295034,1.,0.995734176295034,1.,0.995734176295034,1.,0.995734176295034,
1.,0.995734176295034,1.,0.995734176295034,1.,0.995734176295034,1.,0.995734176295034,
1.,0.995734176295034,1.,0.995734176295034,1.,0.995734176295034,1.,0.995734176295034,
1.,0.995734176295034,1.,0.995734176295034,1.,0.995734176295034,1.,0.995734176295034,
1.,0.995734176295034,1.,0.995734176295034,1.,0.995734176295034,1.,0.995734176295034,
1.,0.995734176295034,1.,0.995734176295034,1.,0.995734176295034,1.,0.995734176295034,
1.,0.995734176295034,1.,0.995734176295034,1.,0.995734176295034,1.,0.995734176295034,
1.,0.995734176295034,1.,0.995734176295034,1.,0.995734176295034,1.,0.995734176295034,
1.,0.995734176295034,1.,0.995734176295034,1.,0.995734176295034,1.,0.995734176295034,
1.,0.995734176295034,1.,0.995734176295034,1.,0.995734176295034,1.,0.995734176295034,
1.,0.995734176295034,1.,0.995734176295034,1.,0.995734176295034,1.,0.995734176295034,
1.,0.995734176295034,1.,0.995734176295034,1.,0.995734176295034,1.,0.995734176295034,
1.,0.995734176295034,1.,0.995734176295034,1.,0.995734176295034,1.,0.995734176295034,
1.,0.995734176295034,1.,0.995734176295034,1.,0.995734176295034,1.,0.995734176295034,
1.,0.995734176295034,1.,0.995734176295034,1.,0.995734176295034,1.,0.995734176295034,
1.,0.995734176295034,1.,0.995734176295034,1.,0.995734176295034,1.,0.995734176295034,
1.,0.995734176295034,1.,0.995734176295034,1.,0.995734176295034,1.,0.995734176295034,
1.,0.995734176295034,1.,0.995734176295034,1.,0.995734176295034,1.,0.995734176295034,
1.,0.995734176295034,1.,0.995734176295034,1.,0.995734176295034,1.,0.995734176295034,
1.,0.995734176295034,1.,0.995734176295034,1.,0.995734176295034,1.,0.995734176295034,
1.,0.995734176295034,1.,0.995734176295034,1.,0.995734176295034,1.,0.995734176295034,
1.,0.995734176295034,1.,0.995734176295034,1.,0.995734176295034,1.,0.995734176295034,
1.,0.995734176295034,1.,0.995734176295034,1.,0.995734176295034,1.,0.995734176295034,
1.,0.995734176295034,1.,0.995734176295034,1.,0.995734176295034,1.,0.995734176295034,
1.,0.995734176295034,1.,0.995734176295034,1.,0.995734176295034,1.,0.995734176295034,
1.,0.995734176295034,1.,0.995734176295034,1.,0.995734176295034,1.,0.995734176295034,
1.,0.995734176295034,1.,0.995734176295034,1.,0.995734176295034,1.,0.995734176295034,
1.,0.995734176295034,1.,0.995734176295034,1.,0.995734176295034,1.,0.995734176295034,
1.,0.995734176295034,1.,0.995734176295034,1.,0.995734176295034,1.,0.995734176295034,
1.,0.995734176295034,1.,0.995734176295034,1.,0.995734176295034,1.,0.995734176295034,
1.,0.995734176295034,1.,0.995734176295034,1.,0.995734176295034,1.,0.995734176295034,
1.,0.995734176295034,1.,0.995734176295034,1.,0.995734176295034,1.,0.995734176295034,
1.,0.995734176295034,1.,0.995734176295034,1.,0.995734176295034,1.,0.995734176295034,
1.,0.995734176295034,1.,0.995734176295034,1.,0.995734176295034,1.,0.995734176295034,
1.,0.995734176295034,1.,0.995734176295034,1.,0.995734176295034,1.,0.995734176295034,
1.,0.995734176295034,1.,0.995734176295034,1.,0.995734176295034,1.,0.995734176295034,
1.,0.995734176295034,1.,0.995734176295034,1.,0.995734176295034,1.,0.995734176295034,
1.,0.995734176295034,1.,0.995734176295034,1.,0.995734176295034,1.,0.995734176295034,
1.,0.995734176295034,1.,0.995734176295034,1.,0.995734176295034,1.,0.995734176295034,
1.,0.995734176295034,1.,0.995734176295034,1.,0.995734176295034,1.,0.995734176295034,
1.,0.995734176295034,1.,0.995734176295034,1.,0.995734176295034,1.,0.995734176295034,
1.,0.995734176295034,1.,0.995734176295034,1.,0.995734176295034,1.,0.995734176295034,
1.,0.995734176295034,1.,0.995734176295034,1.,0.995734176295034,1.,0.995734176295034,
1.,0.995734176295034,1.,0.995734176295034,1.,0.995734176295034,1.,0.995734176295034,
1.,0.995734176295034,1.,0.995734176295034,1.,0.995734176295034,1.,0.995734176295034,
1.,0.995734176295034,1.,0.995734176295034,1.,0.995734176295034,1.,0.995734176295034,
1.,0.995734176295034,1.,0.995734176295034,1.,0.995734176295034,1.,0.995734176295034,
1.,0.995734176295034,1.,0.995734176295034,1.,0.995734176295034,1.,0.995734176295034,
1.,0.995734176295034,1.,0.995734176295034,1.,0.995734176295034,1.,0.995734176295034,
1.,0.995734176295034,1.,0.995734176295034,1.,0.995734176295034,1.,0.995734176295034,
1.,0.995734176295034,1.,0.995734176295034,1.,0.995734176295034,1.,0.995734176295034,
1.,0.995734176295034,1.,0.995734176295034,1.,0.995734176295034,1.,0.995734176295034,
1.,0.995734176295034,1.,0.995734176295034,1.,0.995734176295034,1.,0.995734176295034,
1.,0.995734176295034,1.,0.995734176295034,1.,0.995734176295034,1.,0.995734176295034,
1.,0.995734176295034,1.,0.995734176295034,1.,0.995734176295034,1.,0.995734176295034,
1.,0.995734176295034,1.,0.995734176295034,1.,0.995734176295034,1.,0.995734176295034,
1.,0.995734176295034,1.,0.995734176295034,1.,0.995734176295034,1.,0.995734176295034,
1.,0.995734176295034,1.,0.995734176295034,1.,0.995734176295034,1.,0.995734176295034,
1.,0.995734176295034,1.,0.995734176295034,1.,0.995734176295034,1.,0.995734176295034,
1.,0.995734176295034,1.,0.995734176295034,1.,0.995734176295034,1.,0.995734176295034,
1.,0.995734176295034,1.,0.995734176295034,1.,0.995734176295034,1.,0.995734176295034,
1.,0.995734176295034,1.,0.995734176295034,1.,0.995734176295034,1.,0.995734176295034,
1.,0.995734176295034,1.,0.995734176295034,1.,0.995734176295034,1.,0.995734176295034,
1.,0.995734176295034,1.,0.995734176295034,1.,0.995734176295034,1.,0.995734176295034,
1.,0.995734176295034,1.,0.995734176295034,1.,0.995734176295034,1.,0.995734176295034,
1.,0.995734176295034,1.,0.995734176295034,1.,0.995734176295034,1.,0.995734176295034,
1.,0.995734176295034,1.,0.995734176295034,1.,0.995734176295034,1.,0.995734176295034,
1.,0.995734176295034,1.,0.995734176295034,1.,0.995734176295034,1.,0.995734176295034,
1.,0.995734176295034,1.,0.995734176295034,1.,0.995734176295034,1.,0.995734176295034,
1.,0.995734176295034,1.,0.995734176295034,1.,0.995734176295034,1.,0.995734176295034,
1.,0.995734176295034,1.,0.995734176295034,1.,0.995734176295034,1.,0.995734176295034,
1.,0.995734176295034,1.,0.995734176295034,1.,0.995734176295034,1.,0.995734176295034,
1.,0.995734176295034,1.,0.995734176295034,1.,0.995734176295034,1.,0.995734176295034,
1.,0.995734176295034,1.,0.995734176295034,1.,0.995734176295034,1.,0.995734176295034,
1.,0.995734176295034,1.,0.995734176295034,1.,0.995734176295034,1.,0.995734176295034,
1.,0.995734176295034,1.,0.995734176295034,1.,0.995734176295034,1.,0.995734176295034,
1.,0.995734176295034,1.,0.995734176295034,1.,0.995734176295034,1.,0.995734176295034,
1.,0.995734176295034,1.,0.995734176295034,1.,0.995734176295034,1.,0.995734176295034,
1.,0.995734176295034,1.,0.995734176295034,1.,0.995734176295034,1.,0.995734176295034,
1.,0.995734176295034,1.,0.995734176295034,1.,0.995734176295034,1.,0.995734176295034,
1.,0.995734176295034,1.,0.995734176295034,1.,0.995734176295034,1.,0.995734176295034,
1.,0.995734176295034,1.,0.995734176295034,1.,0.995734176295034,1.,0.995734176295034,
1.,0.995734176295034,1.,0.995734176295034,1.,0.995734176295034,1.,0.995734176295034,
1.,0.995734176295034,1.,0.995734176295034,1.,0.995734176295034,1.,0.995734176295034,
1.,0.995734176295034,1.,0.995734176295034,1.,0.995734176295034,1.,0.995734176295034,
1.,0.995734176295034,1.,0.995734176295034,1.,0.995734176295034,1.,0.995734176295034,
1.,0.995734176295034,1.,0.995734176295034,1.,0.995734176295034,1.,0.995734176295034,
1.,0.995734176295034,1.,0.995734176295034,1.,0.995734176295034,1.,0.995734176295034,
1.,0.995734176295034,1.,0.995734176295034,1.,0.995734176295034,1.,0.995734176295034,
1.,0.995734176295034,1.,0.995734176295034,1.,0.995734176295034,1.,0.995734176295034,
1.,0.995734176295034,1.,0.995734176295034,1.,0.995734176295034,1.,0.995734176295034,
1.,0.995734176295034,1.,0.995734176295034,1.,0.995734176295034,1.,0.995734176295034,
1.,0.995734176295034,1.,0.995734176295034,1.,0.995734176295034,1.,0.995734176295034,
1.,0.995734176295034,1.,0.995734176295034,1.,0.995734176295034,1.,0.995734176295034,
1.,0.995734176295034,1.,0.995734176295034,1.,0.995734176295034,1.,0.995734176295034,
1.,0.995734176295034,1.,0.995734176295034,1.,0.995734176295034,1.,0.995734176295034,
1.,0.995734176295034,1.,0.995734176295034,1.,0.995734176295034,1.,0.995734176295034,
1.,0.995734176295034,1.,0.995734176295034,1.,0.995734176295034,1.,0.995734176295034,
1.,0.995734176295034,1.,0.995734176295034,1.,0.995734176295034,1.,0.995734176295034,
1.,0.995734176295034,1.,0.995734176295034,1.,0.995734176295034,1.,0.995734176295034,
1.,0.995734176295034,1.,0.995734176295034,1.,0.995734176295034,1.,0.995734176295034,
1.,0.995734176295034,1.,0.995734176295034,1.,0.995734176295034,1.,0.995734176295034,
1.,0.995734176295034,1.,0.995734176295034,1.,0.995734176295034,1.,0.995734176295034,
1.,0.995734176295034,1.,0.995734176295034,1.,0.995734176295034,1.,0.995734176295034,
1.,0.995734176295034,1.,0.995734176295034,1.,0.995734176295034,1.,0.995734176295034,
1.,0.995734176295034,1.,0.995734176295034,1.,0.995734176295034,1.,0.995734176295034,
1.,0.995734176295034,1.,0.995734176295034,1.,0.995734176295034,1.,0.995734176295034,
1.,0.995734176295034,1.,0.995734176295034,1.,0.995734176295034,1.,0.995734176295034,
1.,0.995734176295034,1.,0.995734176295034,1.,0.995734176295034,1.,0.995734176295034,
1.,0.995734176295034,1.,0.995734176295034,1.,0.995734176295034,1.,0.995734176295034,
1.,0.995734176295034,1.,0.995734176295034,1.,0.995734176295034,1.,0.995734176295034,
1.,0.995734176295034,1.,0.995734176295034,1.,0.995734176295034,1.,0.995734176295034,
1.,0.995734176295034,1.,0.995734176295034,1.,0.995734176295034,1.,0.995734176295034,
1.,0.995734176295034,1.,0.995734176295034,1.,0.995734176295034,1.,0.995734176295034,
1.,0.995734176295034,1.,0.995734176295034,1.,0.995734176295034,1.,0.995734176295034,
1.,0.995734176295034,1.,0.995734176295034,1.,0.995734176295034,1.,0.995734176295034,
1.,0.995734176295034,1.,0.995734176295034,1.,0.995734176295034,1.,0.995734176295034,
1.,0.995734176295034,1.,0.995734176295034,1.,0.995734176295034,1.,0.995734176295034,
1.,0.995734176295034,1.,0.995734176295034,1.,0.995734176295034,1.,0.995734176295034,
1.,0.995734176295034,1.,0.995734176295034,1.,0.995734176295034,1.,0.995734176295034,
1.,0.995734176295034,1.,0.995734176295034,1.,0.995734176295034,1.,0.995734176295034,
1.,0.995734176295034,1.,0.995734176295034,1.,0.995734176295034,1.,0.995734176295034,
1.,0.995734176295034,1.,0.995734176295034,1.,0.995734176295034,1.,0.995734176295034,
1.,0.995734176295034,1.,0.995734176295034,1.,0.995734176295034,1.,0.995734176295034,
1.,0.995734176295034,1.,0.995734176295034,1.,0.995734176295034,1.,0.995734176295034,
1.,0.995734176295034,1.,0.995734176295034,1.,0.995734176295034,1.,0.995734176295034,
1.,0.995734176295034,1.,0.995734176295034,1.,0.995734176295034,1.,0.995734176295034,
1.,0.995734176295034,1.,0.995734176295034,1.,0.995734176295034,1.,0.995734176295034,
1.,0.995734176295034,1.,0.995734176295034,1.,0.995734176295034,1.,0.995734176295034,
1.,0.995734176295034,1.,0.995734176295034,1.,0.995734176295034,1.,0.995734176295034,
1.,0.995734176295034,1.,0.995734176295034,1.,0.995734176295034,1.,0.997201362504478,
0.998074874808407),(1.,0.995734176295034,1.,0.995734176295034,1.,0.995734176295034,
1.,0.995734176295034,1.,0.995734176295034,1.,0.995734176295034,1.,0.995734176295034,
1.,0.995734176295034,1.,0.995734176295034,1.,0.995734176295034,1.,0.995734176295034,
1.,0.995734176295034,1.,0.995734176295034,1.,0.995734176295034,1.,0.995734176295034,
1.,0.995734176295034,1.,0.995734176295034,1.,0.995734176295034,1.,0.995734176295034,
1.,0.995734176295034,1.,0.995734176295034,1.,0.995734176295034,1.,0.995734176295034,
1.,0.995734176295034,1.,0.995734176295034,1.,0.995734176295034,1.,0.995734176295034,
1.,0.995734176295034,1.,0.995734176295034,1.,0.995734176295034,1.,0.995734176295034,
1.,0.995734176295034,1.,0.995734176295034,1.,0.995734176295034,1.,0.995734176295034,
1.,0.995734176295034,1.,0.995734176295034,1.,0.995734176295034,1.,0.995734176295034,
1.,0.995734176295034,1.,0.995734176295034,1.,0.995734176295034,1.,0.995734176295034,
1.,0.995734176295034,1.,0.995734176295034,1.,0.995734176295034,1.,0.995734176295034,
1.,0.995734176295034,1.,0.995734176295034,1.,0.995734176295034,1.,0.995734176295034,
1.,0.995734176295034,1.,0.995734176295034,1.,0.995734176295034,1.,0.995734176295034,
1.,0.995734176295034,1.,0.995734176295034,1.,0.995734176295034,1.,0.995734176295034,
1.,0.995734176295034,1.,0.995734176295034,1.,0.995734176295034,1.,0.995734176295034,
1.,0.995734176295034,1.,0.995734176295034,1.,0.995734176295034,1.,0.995734176295034,
1.,0.995734176295034,1.,0.995734176295034,1.,0.995734176295034,1.,0.995734176295034,
1.,0.995734176295034,1.,0.995734176295034,1.,0.995734176295034,1.,0.995734176295034,
1.,0.995734176295034,1.,0.995734176295034,1.,0.995734176295034,1.,0.995734176295034,
1.,0.995734176295034,1.,0.995734176295034,1.,0.995734176295034,1.,0.995734176295034,
1.,0.995734176295034,1.,0.995734176295034,1.,0.995734176295034,1.,0.995734176295034,
1.,0.995734176295034,1.,0.995734176295034,1.,0.995734176295034,1.,0.995734176295034,
1.,0.995734176295034,1.,0.995734176295034,1.,0.995734176295034,1.,0.995734176295034,
1.,0.995734176295034,1.,0.995734176295034,1.,0.995734176295034,1.,0.995734176295034,
1.,0.995734176295034,1.,0.995734176295034,1.,0.995734176295034,1.,0.995734176295034,
1.,0.995734176295034,1.,0.995734176295034,1.,0.995734176295034,1.,0.995734176295034,
1.,0.995734176295034,1.,0.995734176295034,1.,0.995734176295034,1.,0.995734176295034,
1.,0.995734176295034,1.,0.995734176295034,1.,0.995734176295034,1.,0.995734176295034,
1.,0.995734176295034,1.,0.995734176295034,1.,0.995734176295034,1.,0.995734176295034,
1.,0.995734176295034,1.,0.995734176295034,1.,0.995734176295034,1.,0.995734176295034,
1.,0.995734176295034,1.,0.995734176295034,1.,0.995734176295034,1.,0.995734176295034,
1.,0.995734176295034,1.,0.995734176295034,1.,0.995734176295034,1.,0.995734176295034,
1.,0.995734176295034,1.,0.995734176295034,1.,0.995734176295034,1.,0.995734176295034,
1.,0.995734176295034,1.,0.995734176295034,1.,0.995734176295034,1.,0.995734176295034,
1.,0.995734176295034,1.,0.995734176295034,1.,0.995734176295034,1.,0.995734176295034,
1.,0.995734176295034,1.,0.995734176295034,1.,0.995734176295034,1.,0.995734176295034,
1.,0.995734176295034,1.,0.995734176295034,1.,0.995734176295034,1.,0.995734176295034,
1.,0.995734176295034,1.,0.995734176295034,1.,0.995734176295034,1.,0.995734176295034,
1.,0.995734176295034,1.,0.995734176295034,1.,0.995734176295034,1.,0.995734176295034,
1.,0.995734176295034,1.,0.995734176295034,1.,0.995734176295034,1.,0.995734176295034,
1.,0.995734176295034,1.,0.995734176295034,1.,0.995734176295034,1.,0.995734176295034,
1.,0.995734176295034,1.,0.995734176295034,1.,0.995734176295034,1.,0.995734176295034,
1.,0.995734176295034,1.,0.995734176295034,1.,0.995734176295034,1.,0.995734176295034,
1.,0.995734176295034,1.,0.995734176295034,1.,0.995734176295034,1.,0.995734176295034,
1.,0.995734176295034,1.,0.995734176295034,1.,0.995734176295034,1.,0.995734176295034,
1.,0.995734176295034,1.,0.995734176295034,1.,0.995734176295034,1.,0.995734176295034,
1.,0.995734176295034,1.,0.995734176295034,1.,0.995734176295034,1.,0.995734176295034,
1.,0.995734176295034,1.,0.995734176295034,1.,0.995734176295034,1.,0.995734176295034,
1.,0.995734176295034,1.,0.995734176295034,1.,0.995734176295034,1.,0.995734176295034,
1.,0.995734176295034,1.,0.995734176295034,1.,0.995734176295034,1.,0.995734176295034,
1.,0.995734176295034,1.,0.995734176295034,1.,0.995734176295034,1.,0.995734176295034,
1.,0.995734176295034,1.,0.995734176295034,1.,0.995734176295034,1.,0.995734176295034,
1.,0.995734176295034,1.,0.995734176295034,1.,0.995734176295034,1.,0.995734176295034,
1.,0.995734176295034,1.,0.995734176295034,1.,0.995734176295034,1.,0.995734176295034,
1.,0.995734176295034,1.,0.995734176295034,1.,0.995734176295034,1.,0.995734176295034,
1.,0.995734176295034,1.,0.995734176295034,1.,0.995734176295034,1.,0.995734176295034,
1.,0.995734176295034,1.,0.995734176295034,1.,0.995734176295034,1.,0.995734176295034,
1.,0.995734176295034,1.,0.995734176295034,1.,0.995734176295034,1.,0.995734176295034,
1.,0.995734176295034,1.,0.995734176295034,1.,0.995734176295034,1.,0.995734176295034,
1.,0.995734176295034,1.,0.995734176295034,1.,0.995734176295034,1.,0.995734176295034,
1.,0.995734176295034,1.,0.995734176295034,1.,0.995734176295034,1.,0.995734176295034,
1.,0.995734176295034,1.,0.995734176295034,1.,0.995734176295034,1.,0.995734176295034,
1.,0.995734176295034,1.,0.995734176295034,1.,0.995734176295034,1.,0.995734176295034,
1.,0.995734176295034,1.,0.995734176295034,1.,0.995734176295034,1.,0.995734176295034,
1.,0.995734176295034,1.,0.995734176295034,1.,0.995734176295034,1.,0.995734176295034,
1.,0.995734176295034,1.,0.995734176295034,1.,0.995734176295034,1.,0.995734176295034,
1.,0.995734176295034,1.,0.995734176295034,1.,0.995734176295034,1.,0.995734176295034,
1.,0.995734176295034,1.,0.995734176295034,1.,0.995734176295034,1.,0.995734176295034,
1.,0.995734176295034,1.,0.995734176295034,1.,0.995734176295034,1.,0.995734176295034,
1.,0.995734176295034,1.,0.995734176295034,1.,0.995734176295034,1.,0.995734176295034,
1.,0.995734176295034,1.,0.995734176295034,1.,0.995734176295034,1.,0.995734176295034,
1.,0.995734176295034,1.,0.995734176295034,1.,0.995734176295034,1.,0.995734176295034,
1.,0.995734176295034,1.,0.995734176295034,1.,0.995734176295034,1.,0.995734176295034,
1.,0.995734176295034,1.,0.995734176295034,1.,0.995734176295034,1.,0.995734176295034,
1.,0.995734176295034,1.,0.995734176295034,1.,0.995734176295034,1.,0.995734176295034,
1.,0.995734176295034,1.,0.995734176295034,1.,0.995734176295034,1.,0.995734176295034,
1.,0.995734176295034,1.,0.995734176295034,1.,0.995734176295034,1.,0.995734176295034,
1.,0.995734176295034,1.,0.995734176295034,1.,0.995734176295034,1.,0.995734176295034,
1.,0.995734176295034,1.,0.995734176295034,1.,0.995734176295034,1.,0.995734176295034,
1.,0.995734176295034,1.,0.995734176295034,1.,0.995734176295034,1.,0.995734176295034,
1.,0.995734176295034,1.,0.995734176295034,1.,0.995734176295034,1.,0.995734176295034,
1.,0.995734176295034,1.,0.995734176295034,1.,0.995734176295034,1.,0.995734176295034,
1.,0.995734176295034,1.,0.995734176295034,1.,0.995734176295034,1.,0.995734176295034,
1.,0.995734176295034,1.,0.995734176295034,1.,0.995734176295034,1.,0.995734176295034,
1.,0.995734176295034,1.,0.995734176295034,1.,0.995734176295034,1.,0.995734176295034,
1.,0.995734176295034,1.,0.995734176295034,1.,0.995734176295034,1.,0.995734176295034,
1.,0.995734176295034,1.,0.995734176295034,1.,0.995734176295034,1.,0.995734176295034,
1.,0.995734176295034,1.,0.995734176295034,1.,0.995734176295034,1.,0.995734176295034,
1.,0.995734176295034,1.,0.995734176295034,1.,0.995734176295034,1.,0.995734176295034,
1.,0.995734176295034,1.,0.995734176295034,1.,0.995734176295034,1.,0.995734176295034,
1.,0.995734176295034,1.,0.995734176295034,1.,0.995734176295034,1.,0.995734176295034,
1.,0.995734176295034,1.,0.995734176295034,1.,0.995734176295034,1.,0.995734176295034,
1.,0.995734176295034,1.,0.995734176295034,1.,0.995734176295034,1.,0.995734176295034,
1.,0.995734176295034,1.,0.995734176295034,1.,0.995734176295034,1.,0.995734176295034,
1.,0.995734176295034,1.,0.995734176295034,1.,0.995734176295034,1.,0.995734176295034,
1.,0.995734176295034,1.,0.995734176295034,1.,0.995734176295034,1.,0.995734176295034,
1.,0.995734176295034,1.,0.995734176295034,1.,0.995734176295034,1.,0.995734176295034,
1.,0.995734176295034,1.,0.995734176295034,1.,0.995734176295034,1.,0.995734176295034,
1.,0.995734176295034,1.,0.995734176295034,1.,0.995734176295034,1.,0.995734176295034,
1.,0.995734176295034,1.,0.995734176295034,1.,0.995734176295034,1.,0.995734176295034,
1.,0.995734176295034,1.,0.995734176295034,1.,0.995734176295034,1.,0.995734176295034,
1.,0.995734176295034,1.,0.995734176295034,1.,0.995734176295034,1.,0.995734176295034,
1.,0.995734176295034,1.,0.995734176295034,1.,0.995734176295034,1.,0.995734176295034,
1.,0.995734176295034,1.,0.995734176295034,1.,0.995734176295034,1.,0.995734176295034,
1.,0.995734176295034,1.,0.995734176295034,1.,0.995734176295034,1.,0.995734176295034,
1.,0.995734176295034,1.,0.995734176295034,1.,0.995734176295034,1.,0.995734176295034,
1.,0.995734176295034,1.,0.995734176295034,1.,0.995734176295034,1.,0.995734176295034,
1.,0.995734176295034,1.,0.995734176295034,1.,0.995734176295034,1.,0.995734176295034,
1.,0.995734176295034,1.,0.995734176295034,1.,0.995734176295034,1.,0.995734176295034,
1.,0.995734176295034,1.,0.995734176295034,1.,0.995734176295034,1.,0.995734176295034,
1.,0.995734176295034,1.,0.995734176295034,1.,0.995734176295034,1.,0.995734176295034,
1.,0.995734176295034,1.,0.995734176295034,1.,0.995734176295034,1.,0.995734176295034,
1.,0.995734176295034,1.,0.995734176295034,1.,0.995734176295034,1.,0.995734176295034,
1.,0.995734176295034,1.,0.995734176295034,1.,0.995734176295034,1.,0.995734176295034,
1.,0.995734176295034,1.,0.995734176295034,1.,0.995734176295034,1.,0.995734176295034,
1.,0.995734176295034,1.,0.995734176295034,1.,0.995734176295034,1.,0.995734176295034,
1.,0.995734176295034,1.,0.995734176295034,1.,0.995734176295034,1.,0.995734176295034,
1.,0.995734176295034,1.,0.995734176295034,1.,0.995734176295034,1.,0.995734176295034,
1.,0.995734176295034,1.,0.995734176295034,1.,0.995734176295034,1.,0.995734176295034,
1.,0.995734176295034,1.,0.995734176295034,1.,0.995734176295034,1.,0.995734176295034,
1.,0.995734176295034,1.,0.995734176295034,1.,0.995734176295034,1.,0.995734176295034,
1.,0.995734176295034,1.,0.995734176295034,1.,0.995734176295034,1.,0.995734176295034,
1.,0.995734176295034,1.,0.995734176295034,1.,0.995734176295034,1.,0.995734176295034,
1.,0.995734176295034,1.,0.995734176295034,1.,0.995734176295034,1.,0.995734176295034,
1.,0.995734176295034,1.,0.995734176295034,1.,0.995734176295034,1.,0.995734176295034,
1.,0.995734176295034,1.,0.995734176295034,1.,0.995734176295034,1.,0.995734176295034,
1.,0.995734176295034,1.,0.995734176295034,1.,0.995734176295034,1.,0.995734176295034,
1.,0.995734176295034,1.,0.995734176295034,1.,0.995734176295034,1.,0.995734176295034,
1.,0.995734176295034,1.,0.995734176295034,1.,0.995734176295034,1.,0.995734176295034,
1.,0.995734176295034,1.,0.995734176295034,1.,0.995734176295034,1.,0.995734176295034,
1.,0.995734176295034,1.,0.995734176295034,1.,0.995734176295034,1.,0.995734176295034,
1.,0.995734176295034,1.,0.995734176295034,1.,0.995734176295034,1.,0.995734176295034,
1.,0.995734176295034,1.,0.995734176295034,1.,0.995734176295034,1.,0.995734176295034,
1.,0.995734176295034,1.,0.995734176295034,1.,0.995734176295034,1.,0.995734176295034,
1.,0.995734176295034,1.,0.995734176295034,1.,0.995734176295034,1.,0.995734176295034,
1.,0.995734176295034,1.,0.995734176295034,1.,0.995734176295034,1.,0.995734176295034,
1.,0.995734176295034,1.,0.995734176295034,1.,0.995734176295034,1.,0.995734176295034,
1.,0.995734176295034,1.,0.995734176295034,1.,0.995734176295034,1.,0.995734176295034,
1.,0.995734176295034,1.,0.995734176295034,1.,0.995734176295034,1.,0.995734176295034,
1.,0.995734176295034,1.,0.995734176295034,1.,0.995734176295034,1.,0.995734176295034,
1.,0.995734176295034,1.,0.995734176295034,1.,0.995734176295034,1.,0.995734176295034,
1.,0.995734176295034,1.,0.995734176295034,1.,0.995734176295034,1.,0.995734176295034,
1.,0.995734176295034,1.,0.995734176295034,1.,0.995734176295034,1.,0.995734176295034,
1.,0.995734176295034,1.,0.995734176295034,1.,0.995734176295034,1.,0.995734176295034,
1.,0.995734176295034,1.,0.995734176295034,1.,0.995734176295034,1.,0.995734176295034,
1.,0.995734176295034,1.,0.995734176295034,1.,0.995734176295034,1.,0.995734176295034,
1.,0.995734176295034,1.,0.995734176295034,1.,0.995734176295034,1.,0.995734176295034,
1.,0.995734176295034,1.,0.995734176295034,1.,0.995734176295034,1.,0.995734176295034,
1.,0.995734176295034,1.,0.995734176295034,1.,0.995734176295034,1.,0.995734176295034,
1.,0.995734176295034,1.,0.995734176295034,1.,0.995734176295034,1.,0.995734176295034,
1.,0.995734176295034,1.,0.995734176295034,1.,0.995734176295034,1.,0.995734176295034,
1.,0.995734176295034,1.,0.995734176295034,1.,0.995734176295034,1.,0.995734176295034,
1.,0.995734176295034,1.,0.995734176295034,1.,0.995734176295034,1.,0.995734176295034,
1.,0.995734176295034,1.,0.995734176295034,1.,0.995734176295034,1.,0.995734176295034,
1.,0.995734176295034,1.,0.995734176295034,1.,0.995734176295034,1.,0.995734176295034,
1.,0.995734176295034,1.,0.995734176295034,1.,0.995734176295034,1.,0.995734176295034,
1.,0.995734176295034,1.,0.995734176295034,1.,0.995734176295034,1.,0.995734176295034,
1.,0.995734176295034,1.,0.995734176295034,1.,0.995734176295034,1.,0.995734176295034,
1.,0.995734176295034,1.,0.995734176295034,1.,0.995734176295034,1.,0.995734176295034,
1.,0.995734176295034,1.,0.995734176295034,1.,0.995734176295034,1.,0.995734176295034,
1.,0.995734176295034,1.,0.995734176295034,1.,0.995734176295034,1.,0.995734176295034,
1.,0.995734176295034,1.,0.995734176295034,1.,0.995734176295034,1.,0.995734176295034,
1.,0.995734176295034,1.,0.995734176295034,1.,0.995734176295034,1.,0.995734176295034,
1.,0.995734176295034,1.,0.995734176295034,1.,0.995734176295034,1.,0.995734176295034,
1.,0.995734176295034,1.,0.995734176295034,1.,0.995734176295034,1.,0.995734176295034,
1.,0.995734176295034,1.,0.995734176295034,1.,0.995734176295034,1.,0.995734176295034,
1.,0.995734176295034,1.,0.995734176295034,1.,0.995734176295034,1.,0.995734176295034,
1.,0.995734176295034,1.,0.995734176295034,1.,0.995734176295034,1.,0.995734176295034,
1.,0.995734176295034,1.,0.995734176295034,1.,0.995734176295034,1.,0.995734176295034,
1.,0.995734176295034,1.,0.995734176295034,1.,0.995734176295034,1.,0.995734176295034,
1.,0.995734176295034,1.,0.995734176295034,1.,0.995734176295034,1.,0.995734176295034,
1.,0.995734176295034,1.,0.995734176295034,1.,0.995734176295034,1.,0.995734176295034,
1.,0.995734176295034,1.,0.995734176295034,1.,0.995734176295034,1.,0.995734176295034,
1.,0.995734176295034,1.,0.995734176295034,1.,0.995734176295034,1.,0.995734176295034,
1.,0.995734176295034,1.,0.995734176295034,1.,0.995734176295034,1.,0.995734176295034,
1.,0.995734176295034,1.,0.995734176295034,1.,0.995734176295034,1.,0.995734176295034,
1.,0.995734176295034,1.,0.995734176295034,1.,0.995734176295034,1.,0.995734176295034,
1.,0.995734176295034,1.,0.995734176295034,1.,0.995734176295034,1.,0.995734176295034,
1.,0.995734176295034,1.,0.995734176295034,1.,0.995734176295034,1.,0.995734176295034,
1.,0.995734176295034,1.,0.995734176295034,1.,0.995734176295034,1.,0.995734176295034,
1.,0.995734176295034,1.,0.995734176295034,1.,0.995734176295034,1.,0.995734176295034,
1.,0.995734176295034,1.,0.995734176295034,1.,0.995734176295034,1.,0.995734176295034,
1.,0.995734176295034,1.,0.995734176295034,1.,0.995734176295034,1.,0.995734176295034,
1.,0.995734176295034,1.,0.995734176295034,1.,0.995734176295034,1.,0.995734176295034,
1.,0.995734176295034,1.,0.995734176295034,1.,0.995734176295034,1.,0.995734176295034,
1.,0.995734176295034,1.,0.995734176295034,1.,0.995734176295034,1.,0.995734176295034,
1.,0.995734176295034,1.,0.995734176295034,1.,0.995734176295034,1.,0.995734176295034,
1.,0.995734176295034,1.,0.995734176295034,1.,0.995734176295034,1.,0.995734176295034,
1.,0.995734176295034,1.,0.995734176295034,1.,0.995734176295034,1.,0.995734176295034,
1.,0.995734176295034,1.,0.995734176295034,1.,0.995734176295034,1.,0.995734176295034,
1.,0.995734176295034,1.,0.995734176295034,1.,0.995734176295034,1.,0.995734176295034,
1.,0.995734176295034,1.,0.995734176295034,1.,0.995734176295034,1.,0.995734176295034,
1.,0.995734176295034,1.,0.995734176295034,1.,0.995734176295034,1.,0.995734176295034,
1.,0.995734176295034,1.,0.995734176295034,1.,0.995734176295034,1.,0.995734176295034,
1.,0.995734176295034,1.,0.995734176295034,1.,0.995734176295034,1.,0.995734176295034,
1.,0.995734176295034,1.,0.995734176295034,1.,0.995734176295034,1.,0.995734176295034,
1.,0.995734176295034,1.,0.995734176295034,1.,0.995734176295034,1.,0.995734176295034,
1.,0.995734176295034,1.,0.995734176295034,1.,0.995734176295034,1.,0.995734176295034,
1.,0.995734176295034,1.,0.995734176295034,1.,0.995734176295034,1.,0.995734176295034,
1.,0.995734176295034,1.,0.995734176295034,1.,0.995734176295034,1.,0.995734176295034,
1.,0.995734176295034,1.,0.995734176295034,1.,0.995734176295034,1.,0.995734176295034,
1.,0.995734176295034,1.,0.995734176295034,1.,0.995734176295034,1.,0.995734176295034,
1.,0.995734176295034,1.,0.995734176295034,1.,0.995734176295034,1.,0.995734176295034,
1.,0.995734176295034,1.,0.995734176295034,1.,0.995734176295034,1.,0.995734176295034,
1.,0.995734176295034,1.,0.995734176295034,1.,0.995734176295034,1.,0.995734176295034,
1.,0.995734176295034,1.,0.995734176295034,1.,0.995734176295034,1.,0.995734176295034,
1.,0.995734176295034,1.,0.995734176295034,1.,0.995734176295034,1.,0.995734176295034,
1.,0.995734176295034,1.,0.995734176295034,1.,0.995734176295034,1.,0.995734176295034,
1.,0.995734176295034,1.,0.995734176295034,1.,0.995734176295034,1.,0.995734176295034,
1.,0.995734176295034,1.,0.995734176295034,1.,0.995734176295034,1.,0.995734176295034,
1.,0.995734176295034,1.,0.995734176295034,1.,0.995734176295034,1.,0.995734176295034,
1.,0.995734176295034,1.,0.995734176295034,1.,0.995734176295034,1.,0.995734176295034,
1.,0.995734176295034,1.,0.995734176295034,1.,0.995734176295034,1.,0.995734176295034,
1.,0.995734176295034,1.,0.995734176295034,1.,0.995734176295034,1.,0.995734176295034,
1.,0.995734176295034,1.,0.995734176295034,1.,0.995734176295034,1.,0.995734176295034,
1.,0.995734176295034,1.,0.995734176295034,1.,0.995734176295034,1.,0.995734176295034,
1.,0.995734176295034,1.,0.995734176295034,1.,0.995734176295034,1.,0.995734176295034,
1.,0.995734176295034,1.,0.995734176295034,1.,0.995734176295034,1.,0.995734176295034,
1.,0.995734176295034,1.,0.995734176295034,1.,0.995734176295034,1.,0.995734176295034,
1.,0.995734176295034,1.,0.995734176295034,1.,0.995734176295034,1.,0.995734176295034,
1.,0.995734176295034,1.,0.995734176295034,1.,0.995734176295034,1.,0.995734176295034,
1.,0.995734176295034,1.,0.995734176295034,1.,0.995734176295034,1.,0.995734176295034,
1.,0.995734176295034,1.,0.995734176295034,1.,0.995734176295034,1.,0.995734176295034,
1.,0.995734176295034,1.,0.995734176295034,1.,0.995734176295034,1.,0.995734176295034,
1.,0.995734176295034,1.,0.995734176295034,1.,0.995734176295034,1.,0.995734176295034,
1.,0.995734176295034,1.,0.995734176295034,1.,0.995734176295034,1.,0.995734176295034,
1.,0.995734176295034,1.,0.995734176295034,1.,0.995734176295034,1.,0.995734176295034,
1.,0.995734176295034,1.,0.995734176295034,1.,0.995734176295034,1.,0.995734176295034,
1.,0.995734176295034,1.,0.995734176295034,1.,0.995734176295034,1.,0.995734176295034,
1.,0.995734176295034,1.,0.995734176295034,1.,0.995734176295034,1.,0.995734176295034,
1.,0.995734176295034,1.,0.995734176295034,1.,0.995734176295034,1.,0.995734176295034,
1.,0.995734176295034,1.,0.995734176295034,1.,0.995734176295034,1.,0.995734176295034,
1.,0.995734176295034,1.,0.995734176295034,1.,0.995734176295034,1.,0.995734176295034,
1.,0.995734176295034,1.,0.995734176295034,1.,0.995734176295034,1.,0.995734176295034,
1.,0.995734176295034,1.,0.995734176295034,1.,0.995734176295034,1.,0.995734176295034,
1.,0.995734176295034,1.,0.995734176295034,1.,0.995734176295034,1.,0.995734176295034,
1.,0.995734176295034,1.,0.995734176295034,1.,0.995734176295034,1.,0.995734176295034,
1.,0.995734176295034,1.,0.995734176295034,1.,0.995734176295034,1.,0.995734176295034,
1.,0.995734176295034,1.,0.995734176295034,1.,0.995734176295034,1.,0.995734176295034,
1.,0.995734176295034,1.,0.995734176295034,1.,0.995734176295034,1.,0.995734176295034,
1.,0.995734176295034,1.,0.995734176295034,1.,0.995734176295034,1.,0.995734176295034,
1.,0.995734176295034,1.,0.995734176295034,1.,0.995734176295034,1.,0.995734176295034,
1.,0.995734176295034,1.,0.995734176295034,1.,0.995734176295034,1.,0.995734176295034,
1.,0.995734176295034,1.,0.995734176295034,1.,0.995734176295034,1.,0.995734176295034,
1.,0.995734176295034,1.,0.995734176295034,1.,0.995734176295034,1.,0.995734176295034,
1.,0.995734176295034,1.,0.995734176295034,1.,0.995734176295034,1.,0.995734176295034,
1.,0.995734176295034,1.,0.995734176295034,1.,0.995734176295034,1.,0.995734176295034,
1.,0.995734176295034,1.,0.995734176295034,1.,0.995734176295034,1.,0.995734176295034,
1.,0.995734176295034,1.,0.995734176295034,1.,0.995734176295034,1.,0.995734176295034,
1.,0.995734176295034,1.,0.995734176295034,1.,0.995734176295034,1.,0.995734176295034,
1.,0.995734176295034,1.,0.995734176295034,1.,0.997201362504478,0.998074874808407)))
REPRESENTATION_ITEM('')
SURFACE()
);
#2503=(
BOUNDED_SURFACE()
B_SPLINE_SURFACE(1,2,((#154459,#154460,#154461,#154462,#154463,#154464,
#154465,#154466,#154467,#154468,#154469,#154470,#154471,#154472,#154473,
#154474,#154475,#154476,#154477,#154478,#154479,#154480,#154481,#154482,
#154483,#154484,#154485,#154486,#154487,#154488,#154489,#154490,#154491,
#154492,#154493,#154494,#154495,#154496,#154497,#154498,#154499,#154500,
#154501,#154502,#154503,#154504,#154505,#154506,#154507,#154508,#154509,
#154510,#154511,#154512,#154513,#154514,#154515,#154516,#154517,#154518,
#154519,#154520,#154521,#154522,#154523,#154524,#154525,#154526,#154527,
#154528,#154529,#154530,#154531,#154532,#154533,#154534,#154535,#154536,
#154537,#154538,#154539,#154540,#154541,#154542,#154543,#154544,#154545,
#154546,#154547,#154548,#154549,#154550,#154551,#154552,#154553,#154554,
#154555,#154556,#154557,#154558,#154559,#154560,#154561,#154562,#154563,
#154564,#154565,#154566,#154567,#154568,#154569,#154570,#154571,#154572,
#154573,#154574,#154575,#154576,#154577,#154578,#154579,#154580,#154581,
#154582,#154583,#154584,#154585,#154586,#154587,#154588,#154589,#154590,
#154591,#154592,#154593,#154594,#154595,#154596,#154597,#154598,#154599,
#154600,#154601,#154602,#154603,#154604,#154605,#154606,#154607,#154608,
#154609,#154610,#154611,#154612,#154613,#154614,#154615,#154616,#154617,
#154618,#154619,#154620,#154621,#154622,#154623,#154624,#154625,#154626,
#154627,#154628,#154629,#154630,#154631,#154632,#154633,#154634,#154635,
#154636,#154637,#154638,#154639,#154640,#154641,#154642,#154643,#154644,
#154645,#154646,#154647,#154648,#154649,#154650,#154651,#154652,#154653,
#154654,#154655,#154656,#154657,#154658,#154659,#154660,#154661,#154662,
#154663,#154664,#154665,#154666,#154667,#154668,#154669,#154670,#154671,
#154672,#154673,#154674,#154675,#154676,#154677,#154678,#154679,#154680,
#154681,#154682,#154683,#154684,#154685,#154686,#154687,#154688,#154689,
#154690,#154691,#154692,#154693,#154694,#154695,#154696,#154697,#154698,
#154699,#154700,#154701,#154702,#154703,#154704,#154705,#154706,#154707,
#154708,#154709,#154710,#154711,#154712,#154713,#154714,#154715,#154716,
#154717,#154718,#154719,#154720,#154721,#154722,#154723,#154724,#154725,
#154726,#154727,#154728,#154729,#154730,#154731,#154732,#154733,#154734,
#154735,#154736,#154737,#154738,#154739,#154740,#154741,#154742,#154743,
#154744,#154745,#154746,#154747,#154748,#154749,#154750,#154751,#154752,
#154753,#154754,#154755,#154756,#154757,#154758,#154759,#154760,#154761,
#154762,#154763,#154764,#154765,#154766,#154767,#154768,#154769,#154770,
#154771,#154772,#154773,#154774,#154775,#154776,#154777,#154778,#154779,
#154780,#154781,#154782,#154783,#154784,#154785,#154786,#154787,#154788,
#154789,#154790,#154791,#154792,#154793,#154794,#154795,#154796,#154797,
#154798,#154799,#154800,#154801,#154802,#154803,#154804,#154805,#154806,
#154807,#154808,#154809,#154810,#154811,#154812,#154813,#154814,#154815,
#154816,#154817,#154818,#154819,#154820,#154821,#154822,#154823,#154824,
#154825,#154826,#154827,#154828,#154829,#154830,#154831,#154832,#154833,
#154834,#154835,#154836,#154837,#154838,#154839,#154840,#154841,#154842,
#154843,#154844,#154845,#154846,#154847,#154848,#154849,#154850,#154851,
#154852,#154853,#154854,#154855,#154856,#154857,#154858,#154859,#154860,
#154861,#154862,#154863,#154864,#154865,#154866,#154867,#154868,#154869,
#154870,#154871,#154872,#154873,#154874,#154875,#154876,#154877,#154878,
#154879,#154880,#154881,#154882,#154883,#154884,#154885,#154886,#154887,
#154888,#154889,#154890,#154891,#154892,#154893,#154894,#154895,#154896,
#154897,#154898,#154899,#154900,#154901,#154902,#154903,#154904,#154905,
#154906,#154907,#154908,#154909,#154910,#154911,#154912,#154913,#154914,
#154915,#154916,#154917,#154918,#154919,#154920,#154921,#154922,#154923,
#154924,#154925,#154926,#154927,#154928,#154929,#154930,#154931,#154932,
#154933,#154934,#154935,#154936,#154937,#154938,#154939,#154940,#154941,
#154942,#154943,#154944,#154945,#154946,#154947,#154948,#154949,#154950,
#154951,#154952,#154953,#154954,#154955,#154956,#154957,#154958,#154959,
#154960,#154961,#154962,#154963,#154964,#154965,#154966,#154967,#154968,
#154969,#154970,#154971,#154972,#154973,#154974,#154975,#154976,#154977,
#154978,#154979,#154980,#154981,#154982,#154983,#154984,#154985,#154986,
#154987,#154988,#154989,#154990,#154991,#154992,#154993,#154994,#154995,
#154996,#154997,#154998,#154999,#155000,#155001,#155002,#155003,#155004,
#155005,#155006,#155007,#155008,#155009,#155010,#155011,#155012,#155013,
#155014,#155015,#155016,#155017,#155018,#155019,#155020,#155021,#155022,
#155023,#155024,#155025,#155026,#155027,#155028,#155029,#155030,#155031,
#155032,#155033,#155034,#155035,#155036,#155037,#155038,#155039,#155040,
#155041,#155042,#155043,#155044,#155045,#155046,#155047,#155048,#155049,
#155050,#155051,#155052,#155053,#155054,#155055,#155056,#155057,#155058,
#155059,#155060,#155061,#155062,#155063,#155064,#155065,#155066,#155067,
#155068,#155069,#155070,#155071,#155072,#155073,#155074,#155075,#155076,
#155077,#155078,#155079,#155080,#155081,#155082,#155083,#155084,#155085,
#155086,#155087,#155088,#155089,#155090,#155091,#155092,#155093,#155094,
#155095,#155096,#155097,#155098,#155099,#155100,#155101,#155102,#155103,
#155104,#155105,#155106,#155107,#155108,#155109,#155110,#155111,#155112,
#155113,#155114,#155115,#155116,#155117,#155118,#155119,#155120,#155121,
#155122,#155123,#155124,#155125,#155126,#155127,#155128,#155129,#155130,
#155131,#155132,#155133,#155134,#155135,#155136,#155137,#155138,#155139,
#155140,#155141,#155142,#155143,#155144,#155145,#155146,#155147,#155148,
#155149,#155150,#155151,#155152,#155153,#155154,#155155,#155156,#155157,
#155158,#155159,#155160,#155161,#155162,#155163,#155164,#155165,#155166,
#155167,#155168,#155169,#155170,#155171,#155172,#155173,#155174,#155175,
#155176,#155177,#155178,#155179,#155180,#155181,#155182,#155183,#155184,
#155185,#155186,#155187,#155188,#155189,#155190,#155191,#155192,#155193,
#155194,#155195,#155196,#155197,#155198,#155199,#155200,#155201,#155202,
#155203,#155204,#155205,#155206,#155207,#155208,#155209,#155210,#155211,
#155212,#155213,#155214,#155215,#155216,#155217,#155218,#155219,#155220,
#155221,#155222,#155223,#155224,#155225,#155226,#155227,#155228,#155229,
#155230,#155231,#155232,#155233,#155234,#155235,#155236,#155237,#155238,
#155239,#155240,#155241,#155242,#155243,#155244,#155245,#155246,#155247,
#155248,#155249,#155250,#155251,#155252,#155253,#155254,#155255,#155256,
#155257,#155258,#155259,#155260,#155261,#155262,#155263,#155264,#155265,
#155266,#155267,#155268,#155269,#155270,#155271,#155272,#155273,#155274,
#155275,#155276,#155277,#155278,#155279,#155280,#155281,#155282,#155283,
#155284,#155285,#155286,#155287,#155288,#155289,#155290,#155291,#155292,
#155293,#155294,#155295,#155296,#155297,#155298,#155299,#155300,#155301,
#155302,#155303,#155304,#155305,#155306,#155307,#155308,#155309,#155310,
#155311,#155312,#155313,#155314,#155315,#155316,#155317,#155318,#155319,
#155320,#155321,#155322,#155323,#155324,#155325,#155326,#155327,#155328,
#155329,#155330,#155331,#155332,#155333,#155334,#155335,#155336,#155337,
#155338,#155339,#155340,#155341,#155342,#155343,#155344,#155345,#155346,
#155347,#155348,#155349,#155350,#155351,#155352,#155353,#155354,#155355,
#155356,#155357,#155358,#155359,#155360,#155361,#155362,#155363,#155364,
#155365,#155366,#155367,#155368,#155369,#155370,#155371,#155372,#155373,
#155374,#155375,#155376,#155377,#155378,#155379,#155380,#155381,#155382,
#155383,#155384,#155385,#155386,#155387,#155388,#155389,#155390,#155391,
#155392,#155393,#155394,#155395,#155396,#155397,#155398,#155399,#155400,
#155401,#155402,#155403,#155404,#155405,#155406,#155407,#155408,#155409,
#155410,#155411,#155412,#155413,#155414,#155415,#155416,#155417,#155418,
#155419,#155420,#155421,#155422,#155423,#155424,#155425,#155426,#155427,
#155428,#155429,#155430,#155431,#155432,#155433,#155434,#155435,#155436,
#155437,#155438,#155439,#155440,#155441,#155442,#155443,#155444,#155445,
#155446,#155447,#155448,#155449,#155450,#155451,#155452,#155453,#155454,
#155455,#155456,#155457,#155458,#155459,#155460,#155461,#155462,#155463,
#155464,#155465,#155466,#155467,#155468,#155469,#155470,#155471,#155472,
#155473,#155474,#155475,#155476,#155477,#155478,#155479,#155480,#155481,
#155482,#155483,#155484,#155485,#155486,#155487,#155488,#155489,#155490,
#155491,#155492,#155493,#155494,#155495,#155496,#155497,#155498,#155499,
#155500,#155501,#155502,#155503,#155504,#155505,#155506,#155507,#155508,
#155509,#155510,#155511,#155512,#155513,#155514,#155515,#155516,#155517,
#155518,#155519,#155520,#155521,#155522,#155523,#155524,#155525,#155526,
#155527,#155528,#155529,#155530,#155531,#155532,#155533,#155534,#155535,
#155536,#155537,#155538,#155539,#155540,#155541,#155542,#155543,#155544,
#155545,#155546,#155547,#155548,#155549,#155550,#155551,#155552,#155553,
#155554,#155555,#155556,#155557,#155558,#155559,#155560,#155561,#155562,
#155563,#155564,#155565,#155566,#155567,#155568,#155569,#155570,#155571,
#155572,#155573,#155574,#155575,#155576,#155577,#155578,#155579,#155580,
#155581,#155582,#155583,#155584,#155585,#155586,#155587,#155588,#155589,
#155590,#155591,#155592,#155593,#155594,#155595,#155596,#155597,#155598,
#155599,#155600,#155601,#155602,#155603,#155604,#155605,#155606,#155607,
#155608,#155609,#155610,#155611,#155612,#155613,#155614,#155615,#155616,
#155617,#155618,#155619,#155620,#155621,#155622,#155623,#155624,#155625,
#155626,#155627,#155628,#155629,#155630,#155631,#155632,#155633,#155634,
#155635,#155636,#155637,#155638,#155639,#155640,#155641,#155642,#155643,
#155644,#155645,#155646,#155647,#155648,#155649,#155650,#155651,#155652,
#155653,#155654,#155655,#155656,#155657,#155658,#155659,#155660,#155661,
#155662,#155663,#155664,#155665,#155666,#155667,#155668,#155669,#155670,
#155671,#155672,#155673,#155674,#155675,#155676,#155677,#155678,#155679,
#155680,#155681,#155682,#155683,#155684,#155685,#155686,#155687,#155688,
#155689,#155690,#155691,#155692,#155693,#155694,#155695,#155696,#155697,
#155698,#155699,#155700,#155701,#155702,#155703,#155704,#155705,#155706,
#155707,#155708,#155709,#155710,#155711,#155712,#155713,#155714,#155715,
#155716,#155717,#155718,#155719,#155720,#155721,#155722,#155723,#155724,
#155725,#155726,#155727,#155728,#155729,#155730,#155731,#155732,#155733,
#155734,#155735,#155736,#155737,#155738,#155739,#155740,#155741,#155742,
#155743,#155744,#155745,#155746,#155747,#155748,#155749,#155750,#155751,
#155752,#155753,#155754,#155755,#155756,#155757,#155758,#155759,#155760,
#155761,#155762,#155763,#155764,#155765,#155766,#155767,#155768,#155769,
#155770,#155771,#155772,#155773,#155774,#155775,#155776,#155777,#155778,
#155779,#155780,#155781,#155782,#155783,#155784,#155785,#155786,#155787,
#155788,#155789,#155790,#155791,#155792,#155793,#155794,#155795,#155796,
#155797,#155798,#155799,#155800,#155801,#155802,#155803,#155804,#155805,
#155806,#155807,#155808,#155809,#155810,#155811,#155812,#155813,#155814,
#155815,#155816,#155817,#155818,#155819,#155820,#155821,#155822,#155823,
#155824,#155825,#155826,#155827,#155828,#155829,#155830,#155831,#155832,
#155833,#155834,#155835,#155836,#155837,#155838,#155839,#155840,#155841,
#155842,#155843,#155844,#155845,#155846,#155847,#155848,#155849,#155850,
#155851,#155852,#155853,#155854,#155855,#155856,#155857,#155858,#155859,
#155860,#155861,#155862,#155863,#155864,#155865,#155866,#155867,#155868,
#155869,#155870,#155871,#155872,#155873,#155874,#155875,#155876,#155877,
#155878,#155879,#155880,#155881,#155882,#155883,#155884,#155885,#155886,
#155887,#155888,#155889,#155890,#155891,#155892,#155893,#155894,#155895,
#155896,#155897,#155898,#155899,#155900,#155901,#155902,#155903,#155904,
#155905,#155906,#155907,#155908,#155909,#155910,#155911,#155912,#155913,
#155914,#155915,#155916,#155917,#155918,#155919,#155920,#155921,#155922,
#155923,#155924,#155925,#155926,#155927,#155928,#155929,#155930,#155931,
#155932,#155933,#155934,#155935,#155936,#155937,#155938,#155939,#155940,
#155941,#155942,#155943,#155944,#155945,#155946,#155947,#155948,#155949,
#155950,#155951,#155952,#155953,#155954,#155955,#155956,#155957,#155958,
#155959,#155960,#155961,#155962,#155963,#155964,#155965,#155966,#155967,
#155968,#155969,#155970,#155971,#155972,#155973,#155974,#155975,#155976,
#155977,#155978,#155979,#155980,#155981,#155982,#155983,#155984,#155985,
#155986,#155987,#155988,#155989,#155990,#155991,#155992,#155993,#155994,
#155995,#155996,#155997,#155998,#155999,#156000,#156001,#156002,#156003,
#156004,#156005,#156006,#156007,#156008,#156009,#156010,#156011,#156012,
#156013,#156014,#156015,#156016,#156017,#156018,#156019,#156020,#156021,
#156022,#156023,#156024,#156025,#156026,#156027,#156028,#156029,#156030,
#156031,#156032,#156033,#156034,#156035,#156036,#156037,#156038,#156039,
#156040,#156041,#156042,#156043,#156044,#156045,#156046,#156047,#156048,
#156049,#156050,#156051,#156052,#156053,#156054,#156055,#156056,#156057,
#156058,#156059,#156060,#156061,#156062,#156063,#156064,#156065,#156066,
#156067,#156068,#156069,#156070,#156071,#156072,#156073,#156074,#156075,
#156076,#156077,#156078,#156079,#156080,#156081,#156082,#156083,#156084,
#156085,#156086,#156087,#156088,#156089,#156090,#156091,#156092,#156093,
#156094,#156095,#156096,#156097,#156098,#156099,#156100,#156101,#156102,
#156103,#156104,#156105,#156106,#156107,#156108,#156109,#156110,#156111,
#156112,#156113,#156114,#156115,#156116,#156117,#156118,#156119,#156120,
#156121,#156122,#156123,#156124,#156125,#156126,#156127,#156128,#156129,
#156130,#156131,#156132,#156133,#156134,#156135,#156136,#156137,#156138,
#156139,#156140,#156141,#156142,#156143,#156144,#156145,#156146,#156147,
#156148,#156149,#156150,#156151,#156152,#156153,#156154,#156155,#156156,
#156157,#156158,#156159,#156160,#156161,#156162,#156163,#156164,#156165,
#156166,#156167,#156168,#156169,#156170,#156171,#156172,#156173,#156174,
#156175,#156176,#156177,#156178,#156179,#156180,#156181,#156182,#156183,
#156184,#156185,#156186,#156187,#156188,#156189,#156190,#156191,#156192,
#156193,#156194,#156195,#156196,#156197,#156198,#156199,#156200,#156201,
#156202,#156203,#156204,#156205,#156206,#156207,#156208,#156209,#156210,
#156211,#156212,#156213,#156214,#156215,#156216,#156217,#156218,#156219,
#156220,#156221,#156222,#156223,#156224,#156225,#156226,#156227,#156228,
#156229,#156230,#156231,#156232,#156233,#156234,#156235,#156236,#156237,
#156238,#156239,#156240,#156241,#156242,#156243,#156244,#156245,#156246,
#156247,#156248,#156249,#156250,#156251,#156252,#156253,#156254,#156255,
#156256,#156257,#156258,#156259,#156260,#156261,#156262,#156263,#156264,
#156265,#156266,#156267,#156268,#156269,#156270,#156271,#156272,#156273,
#156274,#156275,#156276,#156277,#156278,#156279,#156280,#156281,#156282,
#156283,#156284,#156285,#156286,#156287,#156288,#156289,#156290,#156291,
#156292,#156293,#156294,#156295,#156296,#156297,#156298,#156299,#156300,
#156301,#156302,#156303,#156304,#156305,#156306,#156307,#156308,#156309,
#156310,#156311,#156312,#156313,#156314,#156315,#156316,#156317,#156318,
#156319,#156320,#156321,#156322,#156323,#156324,#156325,#156326,#156327,
#156328,#156329,#156330,#156331,#156332,#156333,#156334,#156335,#156336,
#156337,#156338,#156339,#156340,#156341,#156342,#156343,#156344,#156345,
#156346,#156347,#156348,#156349,#156350,#156351,#156352,#156353,#156354,
#156355,#156356,#156357,#156358,#156359,#156360,#156361,#156362,#156363,
#156364,#156365,#156366,#156367,#156368,#156369,#156370,#156371,#156372,
#156373,#156374,#156375,#156376,#156377,#156378,#156379,#156380,#156381,
#156382,#156383,#156384,#156385,#156386,#156387,#156388,#156389,#156390,
#156391,#156392,#156393,#156394,#156395,#156396,#156397,#156398,#156399,
#156400,#156401,#156402,#156403,#156404,#156405,#156406,#156407,#156408,
#156409,#156410,#156411,#156412,#156413,#156414,#156415,#156416,#156417,
#156418,#156419,#156420,#156421,#156422,#156423,#156424,#156425,#156426,
#156427,#156428,#156429,#156430,#156431,#156432,#156433,#156434,#156435,
#156436,#156437,#156438,#156439,#156440,#156441,#156442,#156443,#156444,
#156445,#156446,#156447,#156448,#156449,#156450,#156451,#156452,#156453,
#156454,#156455,#156456,#156457,#156458,#156459,#156460,#156461,#156462,
#156463,#156464,#156465,#156466,#156467,#156468,#156469,#156470,#156471,
#156472,#156473),(#156474,#156475,#156476,#156477,#156478,#156479,#156480,
#156481,#156482,#156483,#156484,#156485,#156486,#156487,#156488,#156489,
#156490,#156491,#156492,#156493,#156494,#156495,#156496,#156497,#156498,
#156499,#156500,#156501,#156502,#156503,#156504,#156505,#156506,#156507,
#156508,#156509,#156510,#156511,#156512,#156513,#156514,#156515,#156516,
#156517,#156518,#156519,#156520,#156521,#156522,#156523,#156524,#156525,
#156526,#156527,#156528,#156529,#156530,#156531,#156532,#156533,#156534,
#156535,#156536,#156537,#156538,#156539,#156540,#156541,#156542,#156543,
#156544,#156545,#156546,#156547,#156548,#156549,#156550,#156551,#156552,
#156553,#156554,#156555,#156556,#156557,#156558,#156559,#156560,#156561,
#156562,#156563,#156564,#156565,#156566,#156567,#156568,#156569,#156570,
#156571,#156572,#156573,#156574,#156575,#156576,#156577,#156578,#156579,
#156580,#156581,#156582,#156583,#156584,#156585,#156586,#156587,#156588,
#156589,#156590,#156591,#156592,#156593,#156594,#156595,#156596,#156597,
#156598,#156599,#156600,#156601,#156602,#156603,#156604,#156605,#156606,
#156607,#156608,#156609,#156610,#156611,#156612,#156613,#156614,#156615,
#156616,#156617,#156618,#156619,#156620,#156621,#156622,#156623,#156624,
#156625,#156626,#156627,#156628,#156629,#156630,#156631,#156632,#156633,
#156634,#156635,#156636,#156637,#156638,#156639,#156640,#156641,#156642,
#156643,#156644,#156645,#156646,#156647,#156648,#156649,#156650,#156651,
#156652,#156653,#156654,#156655,#156656,#156657,#156658,#156659,#156660,
#156661,#156662,#156663,#156664,#156665,#156666,#156667,#156668,#156669,
#156670,#156671,#156672,#156673,#156674,#156675,#156676,#156677,#156678,
#156679,#156680,#156681,#156682,#156683,#156684,#156685,#156686,#156687,
#156688,#156689,#156690,#156691,#156692,#156693,#156694,#156695,#156696,
#156697,#156698,#156699,#156700,#156701,#156702,#156703,#156704,#156705,
#156706,#156707,#156708,#156709,#156710,#156711,#156712,#156713,#156714,
#156715,#156716,#156717,#156718,#156719,#156720,#156721,#156722,#156723,
#156724,#156725,#156726,#156727,#156728,#156729,#156730,#156731,#156732,
#156733,#156734,#156735,#156736,#156737,#156738,#156739,#156740,#156741,
#156742,#156743,#156744,#156745,#156746,#156747,#156748,#156749,#156750,
#156751,#156752,#156753,#156754,#156755,#156756,#156757,#156758,#156759,
#156760,#156761,#156762,#156763,#156764,#156765,#156766,#156767,#156768,
#156769,#156770,#156771,#156772,#156773,#156774,#156775,#156776,#156777,
#156778,#156779,#156780,#156781,#156782,#156783,#156784,#156785,#156786,
#156787,#156788,#156789,#156790,#156791,#156792,#156793,#156794,#156795,
#156796,#156797,#156798,#156799,#156800,#156801,#156802,#156803,#156804,
#156805,#156806,#156807,#156808,#156809,#156810,#156811,#156812,#156813,
#156814,#156815,#156816,#156817,#156818,#156819,#156820,#156821,#156822,
#156823,#156824,#156825,#156826,#156827,#156828,#156829,#156830,#156831,
#156832,#156833,#156834,#156835,#156836,#156837,#156838,#156839,#156840,
#156841,#156842,#156843,#156844,#156845,#156846,#156847,#156848,#156849,
#156850,#156851,#156852,#156853,#156854,#156855,#156856,#156857,#156858,
#156859,#156860,#156861,#156862,#156863,#156864,#156865,#156866,#156867,
#156868,#156869,#156870,#156871,#156872,#156873,#156874,#156875,#156876,
#156877,#156878,#156879,#156880,#156881,#156882,#156883,#156884,#156885,
#156886,#156887,#156888,#156889,#156890,#156891,#156892,#156893,#156894,
#156895,#156896,#156897,#156898,#156899,#156900,#156901,#156902,#156903,
#156904,#156905,#156906,#156907,#156908,#156909,#156910,#156911,#156912,
#156913,#156914,#156915,#156916,#156917,#156918,#156919,#156920,#156921,
#156922,#156923,#156924,#156925,#156926,#156927,#156928,#156929,#156930,
#156931,#156932,#156933,#156934,#156935,#156936,#156937,#156938,#156939,
#156940,#156941,#156942,#156943,#156944,#156945,#156946,#156947,#156948,
#156949,#156950,#156951,#156952,#156953,#156954,#156955,#156956,#156957,
#156958,#156959,#156960,#156961,#156962,#156963,#156964,#156965,#156966,
#156967,#156968,#156969,#156970,#156971,#156972,#156973,#156974,#156975,
#156976,#156977,#156978,#156979,#156980,#156981,#156982,#156983,#156984,
#156985,#156986,#156987,#156988,#156989,#156990,#156991,#156992,#156993,
#156994,#156995,#156996,#156997,#156998,#156999,#157000,#157001,#157002,
#157003,#157004,#157005,#157006,#157007,#157008,#157009,#157010,#157011,
#157012,#157013,#157014,#157015,#157016,#157017,#157018,#157019,#157020,
#157021,#157022,#157023,#157024,#157025,#157026,#157027,#157028,#157029,
#157030,#157031,#157032,#157033,#157034,#157035,#157036,#157037,#157038,
#157039,#157040,#157041,#157042,#157043,#157044,#157045,#157046,#157047,
#157048,#157049,#157050,#157051,#157052,#157053,#157054,#157055,#157056,
#157057,#157058,#157059,#157060,#157061,#157062,#157063,#157064,#157065,
#157066,#157067,#157068,#157069,#157070,#157071,#157072,#157073,#157074,
#157075,#157076,#157077,#157078,#157079,#157080,#157081,#157082,#157083,
#157084,#157085,#157086,#157087,#157088,#157089,#157090,#157091,#157092,
#157093,#157094,#157095,#157096,#157097,#157098,#157099,#157100,#157101,
#157102,#157103,#157104,#157105,#157106,#157107,#157108,#157109,#157110,
#157111,#157112,#157113,#157114,#157115,#157116,#157117,#157118,#157119,
#157120,#157121,#157122,#157123,#157124,#157125,#157126,#157127,#157128,
#157129,#157130,#157131,#157132,#157133,#157134,#157135,#157136,#157137,
#157138,#157139,#157140,#157141,#157142,#157143,#157144,#157145,#157146,
#157147,#157148,#157149,#157150,#157151,#157152,#157153,#157154,#157155,
#157156,#157157,#157158,#157159,#157160,#157161,#157162,#157163,#157164,
#157165,#157166,#157167,#157168,#157169,#157170,#157171,#157172,#157173,
#157174,#157175,#157176,#157177,#157178,#157179,#157180,#157181,#157182,
#157183,#157184,#157185,#157186,#157187,#157188,#157189,#157190,#157191,
#157192,#157193,#157194,#157195,#157196,#157197,#157198,#157199,#157200,
#157201,#157202,#157203,#157204,#157205,#157206,#157207,#157208,#157209,
#157210,#157211,#157212,#157213,#157214,#157215,#157216,#157217,#157218,
#157219,#157220,#157221,#157222,#157223,#157224,#157225,#157226,#157227,
#157228,#157229,#157230,#157231,#157232,#157233,#157234,#157235,#157236,
#157237,#157238,#157239,#157240,#157241,#157242,#157243,#157244,#157245,
#157246,#157247,#157248,#157249,#157250,#157251,#157252,#157253,#157254,
#157255,#157256,#157257,#157258,#157259,#157260,#157261,#157262,#157263,
#157264,#157265,#157266,#157267,#157268,#157269,#157270,#157271,#157272,
#157273,#157274,#157275,#157276,#157277,#157278,#157279,#157280,#157281,
#157282,#157283,#157284,#157285,#157286,#157287,#157288,#157289,#157290,
#157291,#157292,#157293,#157294,#157295,#157296,#157297,#157298,#157299,
#157300,#157301,#157302,#157303,#157304,#157305,#157306,#157307,#157308,
#157309,#157310,#157311,#157312,#157313,#157314,#157315,#157316,#157317,
#157318,#157319,#157320,#157321,#157322,#157323,#157324,#157325,#157326,
#157327,#157328,#157329,#157330,#157331,#157332,#157333,#157334,#157335,
#157336,#157337,#157338,#157339,#157340,#157341,#157342,#157343,#157344,
#157345,#157346,#157347,#157348,#157349,#157350,#157351,#157352,#157353,
#157354,#157355,#157356,#157357,#157358,#157359,#157360,#157361,#157362,
#157363,#157364,#157365,#157366,#157367,#157368,#157369,#157370,#157371,
#157372,#157373,#157374,#157375,#157376,#157377,#157378,#157379,#157380,
#157381,#157382,#157383,#157384,#157385,#157386,#157387,#157388,#157389,
#157390,#157391,#157392,#157393,#157394,#157395,#157396,#157397,#157398,
#157399,#157400,#157401,#157402,#157403,#157404,#157405,#157406,#157407,
#157408,#157409,#157410,#157411,#157412,#157413,#157414,#157415,#157416,
#157417,#157418,#157419,#157420,#157421,#157422,#157423,#157424,#157425,
#157426,#157427,#157428,#157429,#157430,#157431,#157432,#157433,#157434,
#157435,#157436,#157437,#157438,#157439,#157440,#157441,#157442,#157443,
#157444,#157445,#157446,#157447,#157448,#157449,#157450,#157451,#157452,
#157453,#157454,#157455,#157456,#157457,#157458,#157459,#157460,#157461,
#157462,#157463,#157464,#157465,#157466,#157467,#157468,#157469,#157470,
#157471,#157472,#157473,#157474,#157475,#157476,#157477,#157478,#157479,
#157480,#157481,#157482,#157483,#157484,#157485,#157486,#157487,#157488,
#157489,#157490,#157491,#157492,#157493,#157494,#157495,#157496,#157497,
#157498,#157499,#157500,#157501,#157502,#157503,#157504,#157505,#157506,
#157507,#157508,#157509,#157510,#157511,#157512,#157513,#157514,#157515,
#157516,#157517,#157518,#157519,#157520,#157521,#157522,#157523,#157524,
#157525,#157526,#157527,#157528,#157529,#157530,#157531,#157532,#157533,
#157534,#157535,#157536,#157537,#157538,#157539,#157540,#157541,#157542,
#157543,#157544,#157545,#157546,#157547,#157548,#157549,#157550,#157551,
#157552,#157553,#157554,#157555,#157556,#157557,#157558,#157559,#157560,
#157561,#157562,#157563,#157564,#157565,#157566,#157567,#157568,#157569,
#157570,#157571,#157572,#157573,#157574,#157575,#157576,#157577,#157578,
#157579,#157580,#157581,#157582,#157583,#157584,#157585,#157586,#157587,
#157588,#157589,#157590,#157591,#157592,#157593,#157594,#157595,#157596,
#157597,#157598,#157599,#157600,#157601,#157602,#157603,#157604,#157605,
#157606,#157607,#157608,#157609,#157610,#157611,#157612,#157613,#157614,
#157615,#157616,#157617,#157618,#157619,#157620,#157621,#157622,#157623,
#157624,#157625,#157626,#157627,#157628,#157629,#157630,#157631,#157632,
#157633,#157634,#157635,#157636,#157637,#157638,#157639,#157640,#157641,
#157642,#157643,#157644,#157645,#157646,#157647,#157648,#157649,#157650,
#157651,#157652,#157653,#157654,#157655,#157656,#157657,#157658,#157659,
#157660,#157661,#157662,#157663,#157664,#157665,#157666,#157667,#157668,
#157669,#157670,#157671,#157672,#157673,#157674,#157675,#157676,#157677,
#157678,#157679,#157680,#157681,#157682,#157683,#157684,#157685,#157686,
#157687,#157688,#157689,#157690,#157691,#157692,#157693,#157694,#157695,
#157696,#157697,#157698,#157699,#157700,#157701,#157702,#157703,#157704,
#157705,#157706,#157707,#157708,#157709,#157710,#157711,#157712,#157713,
#157714,#157715,#157716,#157717,#157718,#157719,#157720,#157721,#157722,
#157723,#157724,#157725,#157726,#157727,#157728,#157729,#157730,#157731,
#157732,#157733,#157734,#157735,#157736,#157737,#157738,#157739,#157740,
#157741,#157742,#157743,#157744,#157745,#157746,#157747,#157748,#157749,
#157750,#157751,#157752,#157753,#157754,#157755,#157756,#157757,#157758,
#157759,#157760,#157761,#157762,#157763,#157764,#157765,#157766,#157767,
#157768,#157769,#157770,#157771,#157772,#157773,#157774,#157775,#157776,
#157777,#157778,#157779,#157780,#157781,#157782,#157783,#157784,#157785,
#157786,#157787,#157788,#157789,#157790,#157791,#157792,#157793,#157794,
#157795,#157796,#157797,#157798,#157799,#157800,#157801,#157802,#157803,
#157804,#157805,#157806,#157807,#157808,#157809,#157810,#157811,#157812,
#157813,#157814,#157815,#157816,#157817,#157818,#157819,#157820,#157821,
#157822,#157823,#157824,#157825,#157826,#157827,#157828,#157829,#157830,
#157831,#157832,#157833,#157834,#157835,#157836,#157837,#157838,#157839,
#157840,#157841,#157842,#157843,#157844,#157845,#157846,#157847,#157848,
#157849,#157850,#157851,#157852,#157853,#157854,#157855,#157856,#157857,
#157858,#157859,#157860,#157861,#157862,#157863,#157864,#157865,#157866,
#157867,#157868,#157869,#157870,#157871,#157872,#157873,#157874,#157875,
#157876,#157877,#157878,#157879,#157880,#157881,#157882,#157883,#157884,
#157885,#157886,#157887,#157888,#157889,#157890,#157891,#157892,#157893,
#157894,#157895,#157896,#157897,#157898,#157899,#157900,#157901,#157902,
#157903,#157904,#157905,#157906,#157907,#157908,#157909,#157910,#157911,
#157912,#157913,#157914,#157915,#157916,#157917,#157918,#157919,#157920,
#157921,#157922,#157923,#157924,#157925,#157926,#157927,#157928,#157929,
#157930,#157931,#157932,#157933,#157934,#157935,#157936,#157937,#157938,
#157939,#157940,#157941,#157942,#157943,#157944,#157945,#157946,#157947,
#157948,#157949,#157950,#157951,#157952,#157953,#157954,#157955,#157956,
#157957,#157958,#157959,#157960,#157961,#157962,#157963,#157964,#157965,
#157966,#157967,#157968,#157969,#157970,#157971,#157972,#157973,#157974,
#157975,#157976,#157977,#157978,#157979,#157980,#157981,#157982,#157983,
#157984,#157985,#157986,#157987,#157988,#157989,#157990,#157991,#157992,
#157993,#157994,#157995,#157996,#157997,#157998,#157999,#158000,#158001,
#158002,#158003,#158004,#158005,#158006,#158007,#158008,#158009,#158010,
#158011,#158012,#158013,#158014,#158015,#158016,#158017,#158018,#158019,
#158020,#158021,#158022,#158023,#158024,#158025,#158026,#158027,#158028,
#158029,#158030,#158031,#158032,#158033,#158034,#158035,#158036,#158037,
#158038,#158039,#158040,#158041,#158042,#158043,#158044,#158045,#158046,
#158047,#158048,#158049,#158050,#158051,#158052,#158053,#158054,#158055,
#158056,#158057,#158058,#158059,#158060,#158061,#158062,#158063,#158064,
#158065,#158066,#158067,#158068,#158069,#158070,#158071,#158072,#158073,
#158074,#158075,#158076,#158077,#158078,#158079,#158080,#158081,#158082,
#158083,#158084,#158085,#158086,#158087,#158088,#158089,#158090,#158091,
#158092,#158093,#158094,#158095,#158096,#158097,#158098,#158099,#158100,
#158101,#158102,#158103,#158104,#158105,#158106,#158107,#158108,#158109,
#158110,#158111,#158112,#158113,#158114,#158115,#158116,#158117,#158118,
#158119,#158120,#158121,#158122,#158123,#158124,#158125,#158126,#158127,
#158128,#158129,#158130,#158131,#158132,#158133,#158134,#158135,#158136,
#158137,#158138,#158139,#158140,#158141,#158142,#158143,#158144,#158145,
#158146,#158147,#158148,#158149,#158150,#158151,#158152,#158153,#158154,
#158155,#158156,#158157,#158158,#158159,#158160,#158161,#158162,#158163,
#158164,#158165,#158166,#158167,#158168,#158169,#158170,#158171,#158172,
#158173,#158174,#158175,#158176,#158177,#158178,#158179,#158180,#158181,
#158182,#158183,#158184,#158185,#158186,#158187,#158188,#158189,#158190,
#158191,#158192,#158193,#158194,#158195,#158196,#158197,#158198,#158199,
#158200,#158201,#158202,#158203,#158204,#158205,#158206,#158207,#158208,
#158209,#158210,#158211,#158212,#158213,#158214,#158215,#158216,#158217,
#158218,#158219,#158220,#158221,#158222,#158223,#158224,#158225,#158226,
#158227,#158228,#158229,#158230,#158231,#158232,#158233,#158234,#158235,
#158236,#158237,#158238,#158239,#158240,#158241,#158242,#158243,#158244,
#158245,#158246,#158247,#158248,#158249,#158250,#158251,#158252,#158253,
#158254,#158255,#158256,#158257,#158258,#158259,#158260,#158261,#158262,
#158263,#158264,#158265,#158266,#158267,#158268,#158269,#158270,#158271,
#158272,#158273,#158274,#158275,#158276,#158277,#158278,#158279,#158280,
#158281,#158282,#158283,#158284,#158285,#158286,#158287,#158288,#158289,
#158290,#158291,#158292,#158293,#158294,#158295,#158296,#158297,#158298,
#158299,#158300,#158301,#158302,#158303,#158304,#158305,#158306,#158307,
#158308,#158309,#158310,#158311,#158312,#158313,#158314,#158315,#158316,
#158317,#158318,#158319,#158320,#158321,#158322,#158323,#158324,#158325,
#158326,#158327,#158328,#158329,#158330,#158331,#158332,#158333,#158334,
#158335,#158336,#158337,#158338,#158339,#158340,#158341,#158342,#158343,
#158344,#158345,#158346,#158347,#158348,#158349,#158350,#158351,#158352,
#158353,#158354,#158355,#158356,#158357,#158358,#158359,#158360,#158361,
#158362,#158363,#158364,#158365,#158366,#158367,#158368,#158369,#158370,
#158371,#158372,#158373,#158374,#158375,#158376,#158377,#158378,#158379,
#158380,#158381,#158382,#158383,#158384,#158385,#158386,#158387,#158388,
#158389,#158390,#158391,#158392,#158393,#158394,#158395,#158396,#158397,
#158398,#158399,#158400,#158401,#158402,#158403,#158404,#158405,#158406,
#158407,#158408,#158409,#158410,#158411,#158412,#158413,#158414,#158415,
#158416,#158417,#158418,#158419,#158420,#158421,#158422,#158423,#158424,
#158425,#158426,#158427,#158428,#158429,#158430,#158431,#158432,#158433,
#158434,#158435,#158436,#158437,#158438,#158439,#158440,#158441,#158442,
#158443,#158444,#158445,#158446,#158447,#158448,#158449,#158450,#158451,
#158452,#158453,#158454,#158455,#158456,#158457,#158458,#158459,#158460,
#158461,#158462,#158463,#158464,#158465,#158466,#158467,#158468,#158469,
#158470,#158471,#158472,#158473,#158474,#158475,#158476,#158477,#158478,
#158479,#158480,#158481,#158482,#158483,#158484,#158485,#158486,#158487,
#158488)),.UNSPECIFIED.,.F.,.F.,.F.)
B_SPLINE_SURFACE_WITH_KNOTS((2,2),(3,2,2,2,2,2,2,2,2,2,2,2,2,2,2,2,2,2,
2,2,2,2,2,2,2,2,2,2,2,2,2,2,2,2,2,2,2,2,2,2,2,2,2,2,2,2,2,2,2,2,2,2,2,2,
2,2,2,2,2,2,2,2,2,2,2,2,2,2,2,2,2,2,2,2,2,2,2,2,2,2,2,2,2,2,2,2,2,2,2,2,
2,2,2,2,2,2,2,2,2,2,2,2,2,2,2,2,2,2,2,2,2,2,2,2,2,2,2,2,2,2,2,2,2,2,2,2,
2,2,2,2,2,2,2,2,2,2,2,2,2,2,2,2,2,2,2,2,2,2,2,2,2,2,2,2,2,2,2,2,2,2,2,2,
2,2,2,2,2,2,2,2,2,2,2,2,2,2,2,2,2,2,2,2,2,2,2,2,2,2,2,2,2,2,2,2,2,2,2,2,
2,2,2,2,2,2,2,2,2,2,2,2,2,2,2,2,2,2,2,2,2,2,2,2,2,2,2,2,2,2,2,2,2,2,2,2,
2,2,2,2,2,2,2,2,2,2,2,2,2,2,2,2,2,2,2,2,2,2,2,2,2,2,2,2,2,2,2,2,2,2,2,2,
2,2,2,2,2,2,2,2,2,2,2,2,2,2,2,2,2,2,2,2,2,2,2,2,2,2,2,2,2,2,2,2,2,2,2,2,
2,2,2,2,2,2,2,2,2,2,2,2,2,2,2,2,2,2,2,2,2,2,2,2,2,2,2,2,2,2,2,2,2,2,2,2,
2,2,2,2,2,2,2,2,2,2,2,2,2,2,2,2,2,2,2,2,2,2,2,2,2,2,2,2,2,2,2,2,2,2,2,2,
2,2,2,2,2,2,2,2,2,2,2,2,2,2,2,2,2,2,2,2,2,2,2,2,2,2,2,2,2,2,2,2,2,2,2,2,
2,2,2,2,2,2,2,2,2,2,2,2,2,2,2,2,2,2,2,2,2,2,2,2,2,2,2,2,2,2,2,2,2,2,2,2,
2,2,2,2,2,2,2,2,2,2,2,2,2,2,2,2,2,2,2,2,2,2,2,2,2,2,2,2,2,2,2,2,2,2,2,2,
2,2,2,2,2,2,2,2,2,2,2,2,2,2,2,2,2,2,2,2,2,2,2,2,2,2,2,2,2,2,2,2,2,2,2,2,
2,2,2,2,2,2,2,2,2,2,2,2,2,2,2,2,2,2,2,2,2,2,2,2,2,2,2,2,2,2,2,2,2,2,2,2,
2,2,2,2,2,2,2,2,2,2,2,2,2,2,2,2,2,2,2,2,2,2,2,2,2,2,2,2,2,2,2,2,2,2,2,2,
2,2,2,2,2,2,2,2,2,2,2,2,2,2,2,2,2,2,2,2,2,2,2,2,2,2,2,2,2,2,2,2,2,2,2,2,
2,2,2,2,2,2,2,2,2,2,2,2,2,2,2,2,2,2,2,2,2,2,2,2,2,2,2,2,2,2,2,2,2,2,2,2,
2,2,2,2,2,2,2,2,2,2,2,2,2,2,2,2,2,2,2,2,2,2,2,2,2,2,2,2,2,2,2,2,2,2,2,2,
2,2,2,2,2,2,2,2,2,2,2,2,2,2,2,2,2,2,2,2,2,2,2,2,2,2,2,2,2,2,2,2,2,2,2,2,
2,2,2,2,2,2,2,2,2,2,2,2,2,2,2,2,2,2,2,2,2,2,2,2,2,2,2,2,2,2,2,2,2,2,2,2,
2,2,2,2,2,2,2,2,2,2,2,2,2,2,2,2,2,2,2,2,2,2,2,2,2,2,2,2,2,2,2,2,2,2,2,2,
2,2,2,2,2,2,2,2,2,2,2,2,2,2,2,2,2,2,2,2,2,2,2,2,2,2,2,2,2,2,2,2,2,2,2,2,
2,2,2,2,2,2,2,2,2,2,2,2,2,2,2,2,2,2,2,2,2,2,2,2,2,2,2,2,2,2,2,2,2,2,2,2,
2,2,2,2,2,2,2,2,2,2,2,2,2,2,2,2,2,2,2,2,2,2,2,2,2,2,2,2,2,2,2,2,2,2,2,2,
2,2,2,2,2,2,2,2,2,2,2,2,2,2,2,2,2,2,2,2,2,2,2,2,2,2,2,2,2,2,2,2,2,2,2,2,
2,2,2,2,2,2,2,2,2,2,2,2,2,2,2,2,2,2,2,2,2,2,2,2,2,2,2,2,2,2,2,2,2,2,2,2,
2,2,2,2,2,2,2,2,2,2,2,2,2,2,2,2,2,3),(0.,1.),(0.,0.000980392156862745,0.00196078431372549,
0.00294117647058824,0.00392156862745098,0.00490196078431373,0.00588235294117647,
0.00686274509803922,0.00784313725490196,0.00882352941176471,0.00980392156862745,
0.0107843137254902,0.0117647058823529,0.0127450980392157,0.0137254901960784,
0.0147058823529412,0.0156862745098039,0.0166666666666667,0.0176470588235294,
0.0186274509803922,0.0196078431372549,0.0205882352941176,0.0215686274509804,
0.0225490196078431,0.0235294117647059,0.0245098039215686,0.0254901960784314,
0.0264705882352941,0.0274509803921569,0.0284313725490196,0.0294117647058824,
0.0303921568627451,0.0313725490196078,0.0323529411764706,0.0333333333333333,
0.0343137254901961,0.0352941176470588,0.0362745098039216,0.0372549019607843,
0.0382352941176471,0.0392156862745098,0.0401960784313726,0.0411764705882353,
0.042156862745098,0.0431372549019608,0.0441176470588235,0.0450980392156863,
0.046078431372549,0.0470588235294118,0.0480392156862745,0.0490196078431373,
0.05,0.0509803921568627,0.0519607843137255,0.0529411764705882,0.053921568627451,
0.0549019607843137,0.0558823529411765,0.0568627450980392,0.057843137254902,
0.0588235294117647,0.0598039215686275,0.0607843137254902,0.0617647058823529,
0.0627450980392157,0.0637254901960784,0.0647058823529412,0.0656862745098039,
0.0666666666666667,0.0676470588235294,0.0686274509803922,0.0696078431372549,
0.0705882352941176,0.0715686274509804,0.0725490196078431,0.0735294117647059,
0.0745098039215686,0.0754901960784314,0.0764705882352941,0.0774509803921569,
0.0784313725490196,0.0794117647058823,0.0803921568627451,0.0813725490196078,
0.0823529411764706,0.0833333333333333,0.0843137254901961,0.0852941176470588,
0.0862745098039216,0.0872549019607843,0.0882352941176471,0.0892156862745098,
0.0901960784313725,0.0911764705882353,0.092156862745098,0.0931372549019608,
0.0941176470588235,0.0950980392156863,0.096078431372549,0.0970588235294118,
0.0980392156862745,0.0990196078431373,0.1,0.100980392156863,0.101960784313725,
0.102941176470588,0.103921568627451,0.104901960784314,0.105882352941176,
0.106862745098039,0.107843137254902,0.108823529411765,0.109803921568627,
0.11078431372549,0.111764705882353,0.112745098039216,0.113725490196078,
0.114705882352941,0.115686274509804,0.116666666666667,0.117647058823529,
0.118627450980392,0.119607843137255,0.120588235294118,0.12156862745098,
0.122549019607843,0.123529411764706,0.124509803921569,0.125490196078431,
0.126470588235294,0.127450980392157,0.12843137254902,0.129411764705882,
0.130392156862745,0.131372549019608,0.132352941176471,0.133333333333333,
0.134313725490196,0.135294117647059,0.136274509803922,0.137254901960784,
0.138235294117647,0.13921568627451,0.140196078431373,0.141176470588235,
0.142156862745098,0.143137254901961,0.144117647058824,0.145098039215686,
0.146078431372549,0.147058823529412,0.148039215686275,0.149019607843137,
0.15,0.150980392156863,0.151960784313725,0.152941176470588,0.153921568627451,
0.154901960784314,0.155882352941176,0.156862745098039,0.157843137254902,
0.158823529411765,0.159803921568627,0.16078431372549,0.161764705882353,
0.162745098039216,0.163725490196078,0.164705882352941,0.165686274509804,
0.166666666666667,0.167647058823529,0.168627450980392,0.169607843137255,
0.170588235294118,0.17156862745098,0.172549019607843,0.173529411764706,
0.174509803921569,0.175490196078431,0.176470588235294,0.177450980392157,
0.17843137254902,0.179411764705882,0.180392156862745,0.181372549019608,
0.182352941176471,0.183333333333333,0.184313725490196,0.185294117647059,
0.186274509803922,0.187254901960784,0.188235294117647,0.18921568627451,
0.190196078431373,0.191176470588235,0.192156862745098,0.193137254901961,
0.194117647058824,0.195098039215686,0.196078431372549,0.197058823529412,
0.198039215686275,0.199019607843137,0.2,0.200980392156863,0.201960784313725,
0.202941176470588,0.203921568627451,0.204901960784314,0.205882352941176,
0.206862745098039,0.207843137254902,0.208823529411765,0.209803921568627,
0.21078431372549,0.211764705882353,0.212745098039216,0.213725490196078,
0.214705882352941,0.215686274509804,0.216666666666667,0.217647058823529,
0.218627450980392,0.219607843137255,0.220588235294118,0.22156862745098,
0.222549019607843,0.223529411764706,0.224509803921569,0.225490196078431,
0.226470588235294,0.227450980392157,0.22843137254902,0.229411764705882,
0.230392156862745,0.231372549019608,0.232352941176471,0.233333333333333,
0.234313725490196,0.235294117647059,0.236274509803922,0.237254901960784,
0.238235294117647,0.23921568627451,0.240196078431373,0.241176470588235,
0.242156862745098,0.243137254901961,0.244117647058824,0.245098039215686,
0.246078431372549,0.247058823529412,0.248039215686275,0.249019607843137,
0.25,0.250980392156863,0.251960784313725,0.252941176470588,0.253921568627451,
0.254901960784314,0.255882352941176,0.256862745098039,0.257843137254902,
0.258823529411765,0.259803921568627,0.26078431372549,0.261764705882353,
0.262745098039216,0.263725490196078,0.264705882352941,0.265686274509804,
0.266666666666667,0.267647058823529,0.268627450980392,0.269607843137255,
0.270588235294118,0.27156862745098,0.272549019607843,0.273529411764706,
0.274509803921569,0.275490196078431,0.276470588235294,0.277450980392157,
0.27843137254902,0.279411764705882,0.280392156862745,0.281372549019608,
0.282352941176471,0.283333333333333,0.284313725490196,0.285294117647059,
0.286274509803922,0.287254901960784,0.288235294117647,0.28921568627451,
0.290196078431373,0.291176470588235,0.292156862745098,0.293137254901961,
0.294117647058824,0.295098039215686,0.296078431372549,0.297058823529412,
0.298039215686275,0.299019607843137,0.3,0.300980392156863,0.301960784313725,
0.302941176470588,0.303921568627451,0.304901960784314,0.305882352941176,
0.306862745098039,0.307843137254902,0.308823529411765,0.309803921568627,
0.31078431372549,0.311764705882353,0.312745098039216,0.313725490196078,
0.314705882352941,0.315686274509804,0.316666666666667,0.317647058823529,
0.318627450980392,0.319607843137255,0.320588235294118,0.32156862745098,
0.322549019607843,0.323529411764706,0.324509803921569,0.325490196078431,
0.326470588235294,0.327450980392157,0.32843137254902,0.329411764705882,
0.330392156862745,0.331372549019608,0.332352941176471,0.333333333333333,
0.334313725490196,0.335294117647059,0.336274509803922,0.337254901960784,
0.338235294117647,0.33921568627451,0.340196078431373,0.341176470588235,
0.342156862745098,0.343137254901961,0.344117647058824,0.345098039215686,
0.346078431372549,0.347058823529412,0.348039215686274,0.349019607843137,
0.35,0.350980392156863,0.351960784313726,0.352941176470588,0.353921568627451,
0.354901960784314,0.355882352941176,0.356862745098039,0.357843137254902,
0.358823529411765,0.359803921568627,0.36078431372549,0.361764705882353,
0.362745098039216,0.363725490196078,0.364705882352941,0.365686274509804,
0.366666666666667,0.367647058823529,0.368627450980392,0.369607843137255,
0.370588235294118,0.37156862745098,0.372549019607843,0.373529411764706,
0.374509803921569,0.375490196078431,0.376470588235294,0.377450980392157,
0.37843137254902,0.379411764705882,0.380392156862745,0.381372549019608,
0.382352941176471,0.383333333333333,0.384313725490196,0.385294117647059,
0.386274509803922,0.387254901960784,0.388235294117647,0.38921568627451,
0.390196078431373,0.391176470588235,0.392156862745098,0.393137254901961,
0.394117647058824,0.395098039215686,0.396078431372549,0.397058823529412,
0.398039215686274,0.399019607843137,0.4,0.400980392156863,0.401960784313726,
0.402941176470588,0.403921568627451,0.404901960784314,0.405882352941176,
0.406862745098039,0.407843137254902,0.408823529411765,0.409803921568627,
0.41078431372549,0.411764705882353,0.412745098039216,0.413725490196078,
0.414705882352941,0.415686274509804,0.416666666666667,0.417647058823529,
0.418627450980392,0.419607843137255,0.420588235294118,0.42156862745098,
0.422549019607843,0.423529411764706,0.424509803921569,0.425490196078431,
0.426470588235294,0.427450980392157,0.42843137254902,0.429411764705882,
0.430392156862745,0.431372549019608,0.432352941176471,0.433333333333333,
0.434313725490196,0.435294117647059,0.436274509803922,0.437254901960784,
0.438235294117647,0.43921568627451,0.440196078431373,0.441176470588235,
0.442156862745098,0.443137254901961,0.444117647058824,0.445098039215686,
0.446078431372549,0.447058823529412,0.448039215686275,0.449019607843137,
0.45,0.450980392156863,0.451960784313725,0.452941176470588,0.453921568627451,
0.454901960784314,0.455882352941176,0.456862745098039,0.457843137254902,
0.458823529411765,0.459803921568627,0.46078431372549,0.461764705882353,
0.462745098039216,0.463725490196078,0.464705882352941,0.465686274509804,
0.466666666666667,0.467647058823529,0.468627450980392,0.469607843137255,
0.470588235294118,0.47156862745098,0.472549019607843,0.473529411764706,
0.474509803921569,0.475490196078431,0.476470588235294,0.477450980392157,
0.47843137254902,0.479411764705882,0.480392156862745,0.481372549019608,
0.482352941176471,0.483333333333333,0.484313725490196,0.485294117647059,
0.486274509803922,0.487254901960784,0.488235294117647,0.48921568627451,
0.490196078431373,0.491176470588235,0.492156862745098,0.493137254901961,
0.494117647058824,0.495098039215686,0.496078431372549,0.497058823529412,
0.498039215686275,0.499019607843137,0.5,0.500980392156863,0.501960784313725,
0.502941176470588,0.503921568627451,0.504901960784314,0.505882352941176,
0.506862745098039,0.507843137254902,0.508823529411765,0.509803921568627,
0.51078431372549,0.511764705882353,0.512745098039216,0.513725490196078,
0.514705882352941,0.515686274509804,0.516666666666667,0.517647058823529,
0.518627450980392,0.519607843137255,0.520588235294118,0.52156862745098,
0.522549019607843,0.523529411764706,0.524509803921569,0.525490196078431,
0.526470588235294,0.527450980392157,0.52843137254902,0.529411764705882,
0.530392156862745,0.531372549019608,0.532352941176471,0.533333333333333,
0.534313725490196,0.535294117647059,0.536274509803922,0.537254901960784,
0.538235294117647,0.53921568627451,0.540196078431373,0.541176470588235,
0.542156862745098,0.543137254901961,0.544117647058823,0.545098039215686,
0.546078431372549,0.547058823529412,0.548039215686275,0.549019607843137,
0.55,0.550980392156863,0.551960784313726,0.552941176470588,0.553921568627451,
0.554901960784314,0.555882352941176,0.556862745098039,0.557843137254902,
0.558823529411765,0.559803921568627,0.56078431372549,0.561764705882353,
0.562745098039216,0.563725490196078,0.564705882352941,0.565686274509804,
0.566666666666667,0.567647058823529,0.568627450980392,0.569607843137255,
0.570588235294118,0.57156862745098,0.572549019607843,0.573529411764706,
0.574509803921569,0.575490196078431,0.576470588235294,0.577450980392157,
0.57843137254902,0.579411764705882,0.580392156862745,0.581372549019608,
0.582352941176471,0.583333333333333,0.584313725490196,0.585294117647059,
0.586274509803922,0.587254901960784,0.588235294117647,0.58921568627451,
0.590196078431373,0.591176470588235,0.592156862745098,0.593137254901961,
0.594117647058824,0.595098039215686,0.596078431372549,0.597058823529412,
0.598039215686274,0.599019607843137,0.6,0.600980392156863,0.601960784313725,
0.602941176470588,0.603921568627451,0.604901960784314,0.605882352941176,
0.606862745098039,0.607843137254902,0.608823529411765,0.609803921568628,
0.61078431372549,0.611764705882353,0.612745098039216,0.613725490196078,
0.614705882352941,0.615686274509804,0.616666666666667,0.617647058823529,
0.618627450980392,0.619607843137255,0.620588235294118,0.62156862745098,
0.622549019607843,0.623529411764706,0.624509803921569,0.625490196078431,
0.626470588235294,0.627450980392157,0.62843137254902,0.629411764705882,
0.630392156862745,0.631372549019608,0.632352941176471,0.633333333333333,
0.634313725490196,0.635294117647059,0.636274509803922,0.637254901960784,
0.638235294117647,0.63921568627451,0.640196078431372,0.641176470588235,
0.642156862745098,0.643137254901961,0.644117647058824,0.645098039215686,
0.646078431372549,0.647058823529412,0.648039215686275,0.649019607843137,
0.65,0.650980392156863,0.651960784313726,0.652941176470588,0.653921568627451,
0.654901960784314,0.655882352941176,0.656862745098039,0.657843137254902,
0.658823529411765,0.659803921568627,0.66078431372549,0.661764705882353,
0.662745098039216,0.663725490196078,0.664705882352941,0.665686274509804,
0.666666666666667,0.667647058823529,0.668627450980392,0.669607843137255,
0.670588235294118,0.67156862745098,0.672549019607843,0.673529411764706,
0.674509803921569,0.675490196078431,0.676470588235294,0.677450980392157,
0.67843137254902,0.679411764705882,0.680392156862745,0.681372549019608,
0.682352941176471,0.683333333333333,0.684313725490196,0.685294117647059,
0.686274509803922,0.687254901960784,0.688235294117647,0.68921568627451,
0.690196078431373,0.691176470588235,0.692156862745098,0.693137254901961,
0.694117647058824,0.695098039215686,0.696078431372549,0.697058823529412,
0.698039215686274,0.699019607843137,0.7,0.700980392156863,0.701960784313725,
0.702941176470588,0.703921568627451,0.704901960784314,0.705882352941177,
0.706862745098039,0.707843137254902,0.708823529411765,0.709803921568627,
0.71078431372549,0.711764705882353,0.712745098039216,0.713725490196078,
0.714705882352941,0.715686274509804,0.716666666666667,0.717647058823529,
0.718627450980392,0.719607843137255,0.720588235294118,0.72156862745098,
0.722549019607843,0.723529411764706,0.724509803921569,0.725490196078431,
0.726470588235294,0.727450980392157,0.72843137254902,0.729411764705882,
0.730392156862745,0.731372549019608,0.732352941176471,0.733333333333333,
0.734313725490196,0.735294117647059,0.736274509803922,0.737254901960784,
0.738235294117647,0.73921568627451,0.740196078431373,0.741176470588235,
0.742156862745098,0.743137254901961,0.744117647058824,0.745098039215686,
0.746078431372549,0.747058823529412,0.748039215686275,0.749019607843137,
0.75,0.750980392156863,0.751960784313725,0.752941176470588,0.753921568627451,
0.754901960784314,0.755882352941176,0.756862745098039,0.757843137254902,
0.758823529411765,0.759803921568627,0.76078431372549,0.761764705882353,
0.762745098039216,0.763725490196078,0.764705882352941,0.765686274509804,
0.766666666666667,0.767647058823529,0.768627450980392,0.769607843137255,
0.770588235294118,0.77156862745098,0.772549019607843,0.773529411764706,
0.774509803921569,0.775490196078431,0.776470588235294,0.777450980392157,
0.77843137254902,0.779411764705882,0.780392156862745,0.781372549019608,
0.782352941176471,0.783333333333333,0.784313725490196,0.785294117647059,
0.786274509803922,0.787254901960784,0.788235294117647,0.78921568627451,
0.790196078431373,0.791176470588235,0.792156862745098,0.793137254901961,
0.794117647058823,0.795098039215686,0.796078431372549,0.797058823529412,
0.798039215686275,0.799019607843137,0.8,0.800980392156863,0.801960784313726,
0.802941176470588,0.803921568627451,0.804901960784314,0.805882352941176,
0.806862745098039,0.807843137254902,0.808823529411765,0.809803921568627,
0.81078431372549,0.811764705882353,0.812745098039216,0.813725490196078,
0.814705882352941,0.815686274509804,0.816666666666667,0.817647058823529,
0.818627450980392,0.819607843137255,0.820588235294118,0.82156862745098,
0.822549019607843,0.823529411764706,0.824509803921569,0.825490196078431,
0.826470588235294,0.827450980392157,0.82843137254902,0.829411764705882,
0.830392156862745,0.831372549019608,0.832352941176471,0.833333333333333,
0.834313725490196,0.835294117647059,0.836274509803922,0.837254901960784,
0.838235294117647,0.83921568627451,0.840196078431373,0.841176470588235,
0.842156862745098,0.843137254901961,0.844117647058824,0.845098039215686,
0.846078431372549,0.847058823529412,0.848039215686274,0.849019607843137,
0.85,0.850980392156863,0.851960784313725,0.852941176470588,0.853921568627451,
0.854901960784314,0.855882352941176,0.856862745098039,0.857843137254902,
0.858823529411765,0.859803921568628,0.86078431372549,0.861764705882353,
0.862745098039216,0.863725490196078,0.864705882352941,0.865686274509804,
0.866666666666667,0.867647058823529,0.868627450980392,0.869607843137255,
0.870588235294118,0.87156862745098,0.872549019607843,0.873529411764706,
0.874509803921569,0.875490196078431,0.876470588235294,0.877450980392157,
0.87843137254902,0.879411764705882,0.880392156862745,0.881372549019608,
0.882352941176471,0.883333333333333,0.884313725490196,0.885294117647059,
0.886274509803922,0.887254901960784,0.888235294117647,0.88921568627451,
0.890196078431372,0.891176470588235,0.892156862745098,0.893137254901961,
0.894117647058824,0.895098039215686,0.896078431372549,0.897058823529412,
0.898039215686275,0.899019607843137,0.9,0.900980392156863,0.901960784313726,
0.902941176470588,0.903921568627451,0.904901960784314,0.905882352941176,
0.906862745098039,0.907843137254902,0.908823529411765,0.909803921568627,
0.91078431372549,0.911764705882353,0.912745098039216,0.913725490196078,
0.914705882352941,0.915686274509804,0.916666666666667,0.917647058823529,
0.918627450980392,0.919607843137255,0.920588235294118,0.92156862745098,
0.922549019607843,0.923529411764706,0.924509803921569,0.925490196078431,
0.926470588235294,0.927450980392157,0.92843137254902,0.929411764705882,
0.930392156862745,0.931372549019608,0.932352941176471,0.933333333333333,
0.934313725490196,0.935294117647059,0.936274509803922,0.937254901960784,
0.938235294117647,0.93921568627451,0.940196078431373,0.941176470588235,
0.942156862745098,0.943137254901961,0.944117647058824,0.945098039215686,
0.946078431372549,0.947058823529412,0.948039215686274,0.949019607843137,
0.95,0.950980392156863,0.951960784313725,0.952941176470588,0.953921568627451,
0.954901960784314,0.955882352941177,0.956862745098039,0.957843137254902,
0.958823529411765,0.959803921568627,0.96078431372549,0.961764705882353,
0.962745098039216,0.963725490196078,0.964705882352941,0.965686274509804,
0.966666666666667,0.967647058823529,0.968627450980392,0.969607843137255,
0.970588235294118,0.97156862745098,0.972549019607843,0.973529411764706,
0.974509803921569,0.975490196078431,0.976470588235294,0.977450980392157,
0.97843137254902,0.979411764705882,0.980392156862745,0.981372549019608,
0.982352941176471,0.983333333333333,0.984313725490196,0.985294117647059,
0.985937295874546,0.995796668833291),.UNSPECIFIED.)
GEOMETRIC_REPRESENTATION_ITEM()
RATIONAL_B_SPLINE_SURFACE(((1.,0.995734176295034,1.,0.995734176295034,1.,
0.995734176295034,1.,0.995734176295034,1.,0.995734176295034,1.,0.995734176295034,
1.,0.995734176295034,1.,0.995734176295034,1.,0.995734176295034,1.,0.995734176295034,
1.,0.995734176295034,1.,0.995734176295034,1.,0.995734176295034,1.,0.995734176295034,
1.,0.995734176295034,1.,0.995734176295034,1.,0.995734176295034,1.,0.995734176295034,
1.,0.995734176295034,1.,0.995734176295034,1.,0.995734176295034,1.,0.995734176295034,
1.,0.995734176295034,1.,0.995734176295034,1.,0.995734176295034,1.,0.995734176295034,
1.,0.995734176295034,1.,0.995734176295034,1.,0.995734176295034,1.,0.995734176295034,
1.,0.995734176295034,1.,0.995734176295034,1.,0.995734176295034,1.,0.995734176295034,
1.,0.995734176295034,1.,0.995734176295034,1.,0.995734176295034,1.,0.995734176295034,
1.,0.995734176295034,1.,0.995734176295034,1.,0.995734176295034,1.,0.995734176295034,
1.,0.995734176295034,1.,0.995734176295034,1.,0.995734176295034,1.,0.995734176295034,
1.,0.995734176295034,1.,0.995734176295034,1.,0.995734176295034,1.,0.995734176295034,
1.,0.995734176295034,1.,0.995734176295034,1.,0.995734176295034,1.,0.995734176295034,
1.,0.995734176295034,1.,0.995734176295034,1.,0.995734176295034,1.,0.995734176295034,
1.,0.995734176295034,1.,0.995734176295034,1.,0.995734176295034,1.,0.995734176295034,
1.,0.995734176295034,1.,0.995734176295034,1.,0.995734176295034,1.,0.995734176295034,
1.,0.995734176295034,1.,0.995734176295034,1.,0.995734176295034,1.,0.995734176295034,
1.,0.995734176295034,1.,0.995734176295034,1.,0.995734176295034,1.,0.995734176295034,
1.,0.995734176295034,1.,0.995734176295034,1.,0.995734176295034,1.,0.995734176295034,
1.,0.995734176295034,1.,0.995734176295034,1.,0.995734176295034,1.,0.995734176295034,
1.,0.995734176295034,1.,0.995734176295034,1.,0.995734176295034,1.,0.995734176295034,
1.,0.995734176295034,1.,0.995734176295034,1.,0.995734176295034,1.,0.995734176295034,
1.,0.995734176295034,1.,0.995734176295034,1.,0.995734176295034,1.,0.995734176295034,
1.,0.995734176295034,1.,0.995734176295034,1.,0.995734176295034,1.,0.995734176295034,
1.,0.995734176295034,1.,0.995734176295034,1.,0.995734176295034,1.,0.995734176295034,
1.,0.995734176295034,1.,0.995734176295034,1.,0.995734176295034,1.,0.995734176295034,
1.,0.995734176295034,1.,0.995734176295034,1.,0.995734176295034,1.,0.995734176295034,
1.,0.995734176295034,1.,0.995734176295034,1.,0.995734176295034,1.,0.995734176295034,
1.,0.995734176295034,1.,0.995734176295034,1.,0.995734176295034,1.,0.995734176295034,
1.,0.995734176295034,1.,0.995734176295034,1.,0.995734176295034,1.,0.995734176295034,
1.,0.995734176295034,1.,0.995734176295034,1.,0.995734176295034,1.,0.995734176295034,
1.,0.995734176295034,1.,0.995734176295034,1.,0.995734176295034,1.,0.995734176295034,
1.,0.995734176295034,1.,0.995734176295034,1.,0.995734176295034,1.,0.995734176295034,
1.,0.995734176295034,1.,0.995734176295034,1.,0.995734176295034,1.,0.995734176295034,
1.,0.995734176295034,1.,0.995734176295034,1.,0.995734176295034,1.,0.995734176295034,
1.,0.995734176295034,1.,0.995734176295034,1.,0.995734176295034,1.,0.995734176295034,
1.,0.995734176295034,1.,0.995734176295034,1.,0.995734176295034,1.,0.995734176295034,
1.,0.995734176295034,1.,0.995734176295034,1.,0.995734176295034,1.,0.995734176295034,
1.,0.995734176295034,1.,0.995734176295034,1.,0.995734176295034,1.,0.995734176295034,
1.,0.995734176295034,1.,0.995734176295034,1.,0.995734176295034,1.,0.995734176295034,
1.,0.995734176295034,1.,0.995734176295034,1.,0.995734176295034,1.,0.995734176295034,
1.,0.995734176295034,1.,0.995734176295034,1.,0.995734176295034,1.,0.995734176295034,
1.,0.995734176295034,1.,0.995734176295034,1.,0.995734176295034,1.,0.995734176295034,
1.,0.995734176295034,1.,0.995734176295034,1.,0.995734176295034,1.,0.995734176295034,
1.,0.995734176295034,1.,0.995734176295034,1.,0.995734176295034,1.,0.995734176295034,
1.,0.995734176295034,1.,0.995734176295034,1.,0.995734176295034,1.,0.995734176295034,
1.,0.995734176295034,1.,0.995734176295034,1.,0.995734176295034,1.,0.995734176295034,
1.,0.995734176295034,1.,0.995734176295034,1.,0.995734176295034,1.,0.995734176295034,
1.,0.995734176295034,1.,0.995734176295034,1.,0.995734176295034,1.,0.995734176295034,
1.,0.995734176295034,1.,0.995734176295034,1.,0.995734176295034,1.,0.995734176295034,
1.,0.995734176295034,1.,0.995734176295034,1.,0.995734176295034,1.,0.995734176295034,
1.,0.995734176295034,1.,0.995734176295034,1.,0.995734176295034,1.,0.995734176295034,
1.,0.995734176295034,1.,0.995734176295034,1.,0.995734176295034,1.,0.995734176295034,
1.,0.995734176295034,1.,0.995734176295034,1.,0.995734176295034,1.,0.995734176295034,
1.,0.995734176295034,1.,0.995734176295034,1.,0.995734176295034,1.,0.995734176295034,
1.,0.995734176295034,1.,0.995734176295034,1.,0.995734176295034,1.,0.995734176295034,
1.,0.995734176295034,1.,0.995734176295034,1.,0.995734176295034,1.,0.995734176295034,
1.,0.995734176295034,1.,0.995734176295034,1.,0.995734176295034,1.,0.995734176295034,
1.,0.995734176295034,1.,0.995734176295034,1.,0.995734176295034,1.,0.995734176295034,
1.,0.995734176295034,1.,0.995734176295034,1.,0.995734176295034,1.,0.995734176295034,
1.,0.995734176295034,1.,0.995734176295034,1.,0.995734176295034,1.,0.995734176295034,
1.,0.995734176295034,1.,0.995734176295034,1.,0.995734176295034,1.,0.995734176295034,
1.,0.995734176295034,1.,0.995734176295034,1.,0.995734176295034,1.,0.995734176295034,
1.,0.995734176295034,1.,0.995734176295034,1.,0.995734176295034,1.,0.995734176295034,
1.,0.995734176295034,1.,0.995734176295034,1.,0.995734176295034,1.,0.995734176295034,
1.,0.995734176295034,1.,0.995734176295034,1.,0.995734176295034,1.,0.995734176295034,
1.,0.995734176295034,1.,0.995734176295034,1.,0.995734176295034,1.,0.995734176295034,
1.,0.995734176295034,1.,0.995734176295034,1.,0.995734176295034,1.,0.995734176295034,
1.,0.995734176295034,1.,0.995734176295034,1.,0.995734176295034,1.,0.995734176295034,
1.,0.995734176295034,1.,0.995734176295034,1.,0.995734176295034,1.,0.995734176295034,
1.,0.995734176295034,1.,0.995734176295034,1.,0.995734176295034,1.,0.995734176295034,
1.,0.995734176295034,1.,0.995734176295034,1.,0.995734176295034,1.,0.995734176295034,
1.,0.995734176295034,1.,0.995734176295034,1.,0.995734176295034,1.,0.995734176295034,
1.,0.995734176295034,1.,0.995734176295034,1.,0.995734176295034,1.,0.995734176295034,
1.,0.995734176295034,1.,0.995734176295034,1.,0.995734176295034,1.,0.995734176295034,
1.,0.995734176295034,1.,0.995734176295034,1.,0.995734176295034,1.,0.995734176295034,
1.,0.995734176295034,1.,0.995734176295034,1.,0.995734176295034,1.,0.995734176295034,
1.,0.995734176295034,1.,0.995734176295034,1.,0.995734176295034,1.,0.995734176295034,
1.,0.995734176295034,1.,0.995734176295034,1.,0.995734176295034,1.,0.995734176295034,
1.,0.995734176295034,1.,0.995734176295034,1.,0.995734176295034,1.,0.995734176295034,
1.,0.995734176295034,1.,0.995734176295034,1.,0.995734176295034,1.,0.995734176295034,
1.,0.995734176295034,1.,0.995734176295034,1.,0.995734176295034,1.,0.995734176295034,
1.,0.995734176295034,1.,0.995734176295034,1.,0.995734176295034,1.,0.995734176295034,
1.,0.995734176295034,1.,0.995734176295034,1.,0.995734176295034,1.,0.995734176295034,
1.,0.995734176295034,1.,0.995734176295034,1.,0.995734176295034,1.,0.995734176295034,
1.,0.995734176295034,1.,0.995734176295034,1.,0.995734176295034,1.,0.995734176295034,
1.,0.995734176295034,1.,0.995734176295034,1.,0.995734176295034,1.,0.995734176295034,
1.,0.995734176295034,1.,0.995734176295034,1.,0.995734176295034,1.,0.995734176295034,
1.,0.995734176295034,1.,0.995734176295034,1.,0.995734176295034,1.,0.995734176295034,
1.,0.995734176295034,1.,0.995734176295034,1.,0.995734176295034,1.,0.995734176295034,
1.,0.995734176295034,1.,0.995734176295034,1.,0.995734176295034,1.,0.995734176295034,
1.,0.995734176295034,1.,0.995734176295034,1.,0.995734176295034,1.,0.995734176295034,
1.,0.995734176295034,1.,0.995734176295034,1.,0.995734176295034,1.,0.995734176295034,
1.,0.995734176295034,1.,0.995734176295034,1.,0.995734176295034,1.,0.995734176295034,
1.,0.995734176295034,1.,0.995734176295034,1.,0.995734176295034,1.,0.995734176295034,
1.,0.995734176295034,1.,0.995734176295034,1.,0.995734176295034,1.,0.995734176295034,
1.,0.995734176295034,1.,0.995734176295034,1.,0.995734176295034,1.,0.995734176295034,
1.,0.995734176295034,1.,0.995734176295034,1.,0.995734176295034,1.,0.995734176295034,
1.,0.995734176295034,1.,0.995734176295034,1.,0.995734176295034,1.,0.995734176295034,
1.,0.995734176295034,1.,0.995734176295034,1.,0.995734176295034,1.,0.995734176295034,
1.,0.995734176295034,1.,0.995734176295034,1.,0.995734176295034,1.,0.995734176295034,
1.,0.995734176295034,1.,0.995734176295034,1.,0.995734176295034,1.,0.995734176295034,
1.,0.995734176295034,1.,0.995734176295034,1.,0.995734176295034,1.,0.995734176295034,
1.,0.995734176295034,1.,0.995734176295034,1.,0.995734176295034,1.,0.995734176295034,
1.,0.995734176295034,1.,0.995734176295034,1.,0.995734176295034,1.,0.995734176295034,
1.,0.995734176295034,1.,0.995734176295034,1.,0.995734176295034,1.,0.995734176295034,
1.,0.995734176295034,1.,0.995734176295034,1.,0.995734176295034,1.,0.995734176295034,
1.,0.995734176295034,1.,0.995734176295034,1.,0.995734176295034,1.,0.995734176295034,
1.,0.995734176295034,1.,0.995734176295034,1.,0.995734176295034,1.,0.995734176295034,
1.,0.995734176295034,1.,0.995734176295034,1.,0.995734176295034,1.,0.995734176295034,
1.,0.995734176295034,1.,0.995734176295034,1.,0.995734176295034,1.,0.995734176295034,
1.,0.995734176295034,1.,0.995734176295034,1.,0.995734176295034,1.,0.995734176295034,
1.,0.995734176295034,1.,0.995734176295034,1.,0.995734176295034,1.,0.995734176295034,
1.,0.995734176295034,1.,0.995734176295034,1.,0.995734176295034,1.,0.995734176295034,
1.,0.995734176295034,1.,0.995734176295034,1.,0.995734176295034,1.,0.995734176295034,
1.,0.995734176295034,1.,0.995734176295034,1.,0.995734176295034,1.,0.995734176295034,
1.,0.995734176295034,1.,0.995734176295034,1.,0.995734176295034,1.,0.995734176295034,
1.,0.995734176295034,1.,0.995734176295034,1.,0.995734176295034,1.,0.995734176295034,
1.,0.995734176295034,1.,0.995734176295034,1.,0.995734176295034,1.,0.995734176295034,
1.,0.995734176295034,1.,0.995734176295034,1.,0.995734176295034,1.,0.995734176295034,
1.,0.995734176295034,1.,0.995734176295034,1.,0.995734176295034,1.,0.995734176295034,
1.,0.995734176295034,1.,0.995734176295034,1.,0.995734176295034,1.,0.995734176295034,
1.,0.995734176295034,1.,0.995734176295034,1.,0.995734176295034,1.,0.995734176295034,
1.,0.995734176295034,1.,0.995734176295034,1.,0.995734176295034,1.,0.995734176295034,
1.,0.995734176295034,1.,0.995734176295034,1.,0.995734176295034,1.,0.995734176295034,
1.,0.995734176295034,1.,0.995734176295034,1.,0.995734176295034,1.,0.995734176295034,
1.,0.995734176295034,1.,0.995734176295034,1.,0.995734176295034,1.,0.995734176295034,
1.,0.995734176295034,1.,0.995734176295034,1.,0.995734176295034,1.,0.995734176295034,
1.,0.995734176295034,1.,0.995734176295034,1.,0.995734176295034,1.,0.995734176295034,
1.,0.995734176295034,1.,0.995734176295034,1.,0.995734176295034,1.,0.995734176295034,
1.,0.995734176295034,1.,0.995734176295034,1.,0.995734176295034,1.,0.995734176295034,
1.,0.995734176295034,1.,0.995734176295034,1.,0.995734176295034,1.,0.995734176295034,
1.,0.995734176295034,1.,0.995734176295034,1.,0.995734176295034,1.,0.995734176295034,
1.,0.995734176295034,1.,0.995734176295034,1.,0.995734176295034,1.,0.995734176295034,
1.,0.995734176295034,1.,0.995734176295034,1.,0.995734176295034,1.,0.995734176295034,
1.,0.995734176295034,1.,0.995734176295034,1.,0.995734176295034,1.,0.995734176295034,
1.,0.995734176295034,1.,0.995734176295034,1.,0.995734176295034,1.,0.995734176295034,
1.,0.995734176295034,1.,0.995734176295034,1.,0.995734176295034,1.,0.995734176295034,
1.,0.995734176295034,1.,0.995734176295034,1.,0.995734176295034,1.,0.995734176295034,
1.,0.995734176295034,1.,0.995734176295034,1.,0.995734176295034,1.,0.995734176295034,
1.,0.995734176295034,1.,0.995734176295034,1.,0.995734176295034,1.,0.995734176295034,
1.,0.995734176295034,1.,0.995734176295034,1.,0.995734176295034,1.,0.995734176295034,
1.,0.995734176295034,1.,0.995734176295034,1.,0.995734176295034,1.,0.995734176295034,
1.,0.995734176295034,1.,0.995734176295034,1.,0.995734176295034,1.,0.995734176295034,
1.,0.995734176295034,1.,0.995734176295034,1.,0.995734176295034,1.,0.995734176295034,
1.,0.995734176295034,1.,0.995734176295034,1.,0.995734176295034,1.,0.995734176295034,
1.,0.995734176295034,1.,0.995734176295034,1.,0.995734176295034,1.,0.995734176295034,
1.,0.995734176295034,1.,0.995734176295034,1.,0.995734176295034,1.,0.995734176295034,
1.,0.995734176295034,1.,0.995734176295034,1.,0.995734176295034,1.,0.995734176295034,
1.,0.995734176295034,1.,0.995734176295034,1.,0.995734176295034,1.,0.995734176295034,
1.,0.995734176295034,1.,0.995734176295034,1.,0.995734176295034,1.,0.995734176295034,
1.,0.995734176295034,1.,0.995734176295034,1.,0.995734176295034,1.,0.995734176295034,
1.,0.995734176295034,1.,0.995734176295034,1.,0.995734176295034,1.,0.995734176295034,
1.,0.995734176295034,1.,0.995734176295034,1.,0.995734176295034,1.,0.995734176295034,
1.,0.995734176295034,1.,0.995734176295034,1.,0.995734176295034,1.,0.995734176295034,
1.,0.995734176295034,1.,0.995734176295034,1.,0.995734176295034,1.,0.995734176295034,
1.,0.995734176295034,1.,0.995734176295034,1.,0.995734176295034,1.,0.995734176295034,
1.,0.995734176295034,1.,0.995734176295034,1.,0.995734176295034,1.,0.995734176295034,
1.,0.995734176295034,1.,0.995734176295034,1.,0.995734176295034,1.,0.995734176295034,
1.,0.995734176295034,1.,0.995734176295034,1.,0.995734176295034,1.,0.995734176295034,
1.,0.995734176295034,1.,0.995734176295034,1.,0.995734176295034,1.,0.995734176295034,
1.,0.995734176295034,1.,0.995734176295034,1.,0.995734176295034,1.,0.995734176295034,
1.,0.995734176295034,1.,0.995734176295034,1.,0.995734176295034,1.,0.995734176295034,
1.,0.995734176295034,1.,0.995734176295034,1.,0.995734176295034,1.,0.995734176295034,
1.,0.995734176295034,1.,0.995734176295034,1.,0.995734176295034,1.,0.995734176295034,
1.,0.995734176295034,1.,0.995734176295034,1.,0.995734176295034,1.,0.995734176295034,
1.,0.995734176295034,1.,0.995734176295034,1.,0.995734176295034,1.,0.995734176295034,
1.,0.995734176295034,1.,0.995734176295034,1.,0.995734176295034,1.,0.995734176295034,
1.,0.995734176295034,1.,0.995734176295034,1.,0.995734176295034,1.,0.995734176295034,
1.,0.995734176295034,1.,0.995734176295034,1.,0.995734176295034,1.,0.995734176295034,
1.,0.995734176295034,1.,0.995734176295034,1.,0.995734176295034,1.,0.995734176295034,
1.,0.995734176295034,1.,0.995734176295034,1.,0.995734176295034,1.,0.995734176295034,
1.,0.995734176295034,1.,0.995734176295034,1.,0.995734176295034,1.,0.995734176295034,
1.,0.995734176295034,1.,0.995734176295034,1.,0.995734176295034,1.,0.995734176295034,
1.,0.995734176295034,1.,0.995734176295034,1.,0.995734176295034,1.,0.995734176295034,
1.,0.995734176295034,1.,0.995734176295034,1.,0.995734176295034,1.,0.995734176295034,
1.,0.995734176295034,1.,0.995734176295034,1.,0.995734176295034,1.,0.995734176295034,
1.,0.995734176295034,1.,0.995734176295034,1.,0.995734176295034,1.,0.995734176295034,
1.,0.995734176295034,1.,0.995734176295034,1.,0.995734176295034,1.,0.995734176295034,
1.,0.995734176295034,1.,0.995734176295034,1.,0.995734176295034,1.,0.995734176295034,
1.,0.995734176295034,1.,0.995734176295034,1.,0.995734176295034,1.,0.995734176295034,
1.,0.995734176295034,1.,0.995734176295034,1.,0.995734176295034,1.,0.995734176295034,
1.,0.995734176295034,1.,0.995734176295034,1.,0.995734176295034,1.,0.995734176295034,
1.,0.995734176295034,1.,0.995734176295034,1.,0.995734176295034,1.,0.995734176295034,
1.,0.995734176295034,1.,0.995734176295034,1.,0.995734176295034,1.,0.995734176295034,
1.,0.995734176295034,1.,0.995734176295034,1.,0.995734176295034,1.,0.995734176295034,
1.,0.995734176295034,1.,0.995734176295034,1.,0.995734176295034,1.,0.995734176295034,
1.,0.995734176295034,1.,0.995734176295034,1.,0.995734176295034,1.,0.995734176295034,
1.,0.995734176295034,1.,0.995734176295034,1.,0.995734176295034,1.,0.995734176295034,
1.,0.995734176295034,1.,0.995734176295034,1.,0.995734176295034,1.,0.995734176295034,
1.,0.995734176295034,1.,0.995734176295034,1.,0.995734176295034,1.,0.995734176295034,
1.,0.995734176295034,1.,0.995734176295034,1.,0.995734176295034,1.,0.995734176295034,
1.,0.995734176295034,1.,0.995734176295034,1.,0.995734176295034,1.,0.995734176295034,
1.,0.995734176295034,1.,0.995734176295034,1.,0.995734176295034,1.,0.995734176295034,
1.,0.995734176295034,1.,0.995734176295034,1.,0.995734176295034,1.,0.995734176295034,
1.,0.995734176295034,1.,0.995734176295034,1.,0.995734176295034,1.,0.995734176295034,
1.,0.995734176295034,1.,0.995734176295034,1.,0.995734176295034,1.,0.995734176295034,
1.,0.995734176295034,1.,0.995734176295034,1.,0.995734176295034,1.,0.995734176295034,
1.,0.995734176295034,1.,0.995734176295034,1.,0.995734176295034,1.,0.995734176295034,
1.,0.995734176295034,1.,0.995734176295034,1.,0.995734176295034,1.,0.995734176295034,
1.,0.995734176295034,1.,0.995734176295034,1.,0.995734176295034,1.,0.995734176295034,
1.,0.995734176295034,1.,0.995734176295034,1.,0.995734176295034,1.,0.995734176295034,
1.,0.995734176295034,1.,0.995734176295034,1.,0.995734176295034,1.,0.995734176295034,
1.,0.995734176295034,1.,0.995734176295034,1.,0.995734176295034,1.,0.995734176295034,
1.,0.995734176295034,1.,0.995734176295034,1.,0.995734176295034,1.,0.995734176295034,
1.,0.995734176295034,1.,0.995734176295034,1.,0.995734176295034,1.,0.995734176295034,
1.,0.995734176295034,1.,0.995734176295034,1.,0.995734176295034,1.,0.995734176295034,
1.,0.995734176295034,1.,0.995734176295034,1.,0.995734176295034,1.,0.995734176295034,
1.,0.995734176295034,1.,0.995734176295034,1.,0.995734176295034,1.,0.995734176295034,
1.,0.995734176295034,1.,0.995734176295034,1.,0.995734176295034,1.,0.995734176295034,
1.,0.995734176295034,1.,0.995734176295034,1.,0.995734176295034,1.,0.995734176295034,
1.,0.995734176295034,1.,0.995734176295034,1.,0.995734176295034,1.,0.995734176295034,
1.,0.995734176295034,1.,0.995734176295034,1.,0.995734176295034,1.,0.995734176295034,
1.,0.995734176295034,1.,0.995734176295034,1.,0.995734176295034,1.,0.995734176295034,
1.,0.995734176295034,1.,0.995734176295034,1.,0.995734176295034,1.,0.995734176295034,
1.,0.995734176295034,1.,0.995734176295034,1.,0.995734176295034,1.,0.995734176295034,
1.,0.995734176295034,1.,0.995734176295034,1.,0.995734176295034,1.,0.995734176295034,
1.,0.995734176295034,1.,0.995734176295034,1.,0.995734176295034,1.,0.995734176295034,
1.,0.995734176295034,1.,0.995734176295034,1.,0.995734176295034,1.,0.995734176295034,
1.,0.995734176295034,1.,0.995734176295034,1.,0.995734176295034,1.,0.995734176295034,
1.,0.995734176295034,1.,0.995734176295034,1.,0.995734176295034,1.,0.995734176295034,
1.,0.995734176295034,1.,0.995734176295034,1.,0.995734176295034,1.,0.995734176295034,
1.,0.995734176295034,1.,0.995734176295034,1.,0.995734176295034,1.,0.995734176295034,
1.,0.995734176295034,1.,0.995734176295034,1.,0.995734176295034,1.,0.995734176295034,
1.,0.995734176295034,1.,0.995734176295034,1.,0.995734176295034,1.,0.995734176295034,
1.,0.995734176295034,1.,0.995734176295034,1.,0.995734176295034,1.,0.995734176295034,
1.,0.995734176295034,1.,0.995734176295034,1.,0.995734176295034,1.,0.995734176295034,
1.,0.995734176295034,1.,0.995734176295034,1.,0.995734176295034,1.,0.995734176295034,
1.,0.995734176295034,1.,0.995734176295034,1.,0.995734176295034,1.,0.995734176295034,
1.,0.995734176295034,1.,0.995734176295034,1.,0.995734176295034,1.,0.995734176295034,
1.,0.995734176295034,1.,0.995734176295034,1.,0.995734176295034,1.,0.995734176295034,
1.,0.995734176295034,1.,0.995734176295034,1.,0.995734176295034,1.,0.995734176295034,
1.,0.995734176295034,1.,0.995734176295034,1.,0.995734176295034,1.,0.995734176295034,
1.,0.995734176295034,1.,0.995734176295034,1.,0.995734176295034,1.,0.995734176295034,
1.,0.995734176295034,1.,0.995734176295034,1.,0.995734176295034,1.,0.995734176295034,
1.,0.995734176295034,1.,0.995734176295034,1.,0.995734176295034,1.,0.995734176295034,
1.,0.995734176295034,1.,0.995734176295034,1.,0.995734176295034,1.,0.995734176295034,
1.,0.995734176295034,1.,0.995734176295034,1.,0.995734176295034,1.,0.995734176295034,
1.,0.995734176295034,1.,0.995734176295034,1.,0.995734176295034,1.,0.995734176295034,
1.,0.995734176295034,1.,0.995734176295034,1.,0.995734176295034,1.,0.995734176295034,
1.,0.995734176295034,1.,0.995734176295034,1.,0.995734176295034,1.,0.995734176295034,
1.,0.995734176295034,1.,0.995734176295034,1.,0.995734176295034,1.,0.995734176295034,
1.,0.995734176295034,1.,0.995734176295034,1.,0.995734176295034,1.,0.995734176295034,
1.,0.995734176295034,1.,0.995734176295034,1.,0.995734176295034,1.,0.995734176295034,
1.,0.995734176295034,1.,0.995734176295034,1.,0.995734176295034,1.,0.995734176295034,
1.,0.995734176295034,1.,0.995734176295034,1.,0.995734176295034,1.,0.995734176295034,
1.,0.995734176295034,1.,0.995734176295034,1.,0.995734176295034,1.,0.995734176295034,
1.,0.995734176295034,1.,0.995734176295034,1.,0.995734176295034,1.,0.995734176295034,
1.,0.995734176295034,1.,0.995734176295034,1.,0.995734176295034,1.,0.995734176295034,
1.,0.995734176295034,1.,0.995734176295034,1.,0.995734176295034,1.,0.995734176295034,
1.,0.995734176295034,1.,0.995734176295034,1.,0.995734176295034,1.,0.997201441372082,
0.998074825578922,0.998074825578922,0.998074825578922),(1.,0.995734176295034,
1.,0.995734176295034,1.,0.995734176295034,1.,0.995734176295034,1.,0.995734176295034,
1.,0.995734176295034,1.,0.995734176295034,1.,0.995734176295034,1.,0.995734176295034,
1.,0.995734176295034,1.,0.995734176295034,1.,0.995734176295034,1.,0.995734176295034,
1.,0.995734176295034,1.,0.995734176295034,1.,0.995734176295034,1.,0.995734176295034,
1.,0.995734176295034,1.,0.995734176295034,1.,0.995734176295034,1.,0.995734176295034,
1.,0.995734176295034,1.,0.995734176295034,1.,0.995734176295034,1.,0.995734176295034,
1.,0.995734176295034,1.,0.995734176295034,1.,0.995734176295034,1.,0.995734176295034,
1.,0.995734176295034,1.,0.995734176295034,1.,0.995734176295034,1.,0.995734176295034,
1.,0.995734176295034,1.,0.995734176295034,1.,0.995734176295034,1.,0.995734176295034,
1.,0.995734176295034,1.,0.995734176295034,1.,0.995734176295034,1.,0.995734176295034,
1.,0.995734176295034,1.,0.995734176295034,1.,0.995734176295034,1.,0.995734176295034,
1.,0.995734176295034,1.,0.995734176295034,1.,0.995734176295034,1.,0.995734176295034,
1.,0.995734176295034,1.,0.995734176295034,1.,0.995734176295034,1.,0.995734176295034,
1.,0.995734176295034,1.,0.995734176295034,1.,0.995734176295034,1.,0.995734176295034,
1.,0.995734176295034,1.,0.995734176295034,1.,0.995734176295034,1.,0.995734176295034,
1.,0.995734176295034,1.,0.995734176295034,1.,0.995734176295034,1.,0.995734176295034,
1.,0.995734176295034,1.,0.995734176295034,1.,0.995734176295034,1.,0.995734176295034,
1.,0.995734176295034,1.,0.995734176295034,1.,0.995734176295034,1.,0.995734176295034,
1.,0.995734176295034,1.,0.995734176295034,1.,0.995734176295034,1.,0.995734176295034,
1.,0.995734176295034,1.,0.995734176295034,1.,0.995734176295034,1.,0.995734176295034,
1.,0.995734176295034,1.,0.995734176295034,1.,0.995734176295034,1.,0.995734176295034,
1.,0.995734176295034,1.,0.995734176295034,1.,0.995734176295034,1.,0.995734176295034,
1.,0.995734176295034,1.,0.995734176295034,1.,0.995734176295034,1.,0.995734176295034,
1.,0.995734176295034,1.,0.995734176295034,1.,0.995734176295034,1.,0.995734176295034,
1.,0.995734176295034,1.,0.995734176295034,1.,0.995734176295034,1.,0.995734176295034,
1.,0.995734176295034,1.,0.995734176295034,1.,0.995734176295034,1.,0.995734176295034,
1.,0.995734176295034,1.,0.995734176295034,1.,0.995734176295034,1.,0.995734176295034,
1.,0.995734176295034,1.,0.995734176295034,1.,0.995734176295034,1.,0.995734176295034,
1.,0.995734176295034,1.,0.995734176295034,1.,0.995734176295034,1.,0.995734176295034,
1.,0.995734176295034,1.,0.995734176295034,1.,0.995734176295034,1.,0.995734176295034,
1.,0.995734176295034,1.,0.995734176295034,1.,0.995734176295034,1.,0.995734176295034,
1.,0.995734176295034,1.,0.995734176295034,1.,0.995734176295034,1.,0.995734176295034,
1.,0.995734176295034,1.,0.995734176295034,1.,0.995734176295034,1.,0.995734176295034,
1.,0.995734176295034,1.,0.995734176295034,1.,0.995734176295034,1.,0.995734176295034,
1.,0.995734176295034,1.,0.995734176295034,1.,0.995734176295034,1.,0.995734176295034,
1.,0.995734176295034,1.,0.995734176295034,1.,0.995734176295034,1.,0.995734176295034,
1.,0.995734176295034,1.,0.995734176295034,1.,0.995734176295034,1.,0.995734176295034,
1.,0.995734176295034,1.,0.995734176295034,1.,0.995734176295034,1.,0.995734176295034,
1.,0.995734176295034,1.,0.995734176295034,1.,0.995734176295034,1.,0.995734176295034,
1.,0.995734176295034,1.,0.995734176295034,1.,0.995734176295034,1.,0.995734176295034,
1.,0.995734176295034,1.,0.995734176295034,1.,0.995734176295034,1.,0.995734176295034,
1.,0.995734176295034,1.,0.995734176295034,1.,0.995734176295034,1.,0.995734176295034,
1.,0.995734176295034,1.,0.995734176295034,1.,0.995734176295034,1.,0.995734176295034,
1.,0.995734176295034,1.,0.995734176295034,1.,0.995734176295034,1.,0.995734176295034,
1.,0.995734176295034,1.,0.995734176295034,1.,0.995734176295034,1.,0.995734176295034,
1.,0.995734176295034,1.,0.995734176295034,1.,0.995734176295034,1.,0.995734176295034,
1.,0.995734176295034,1.,0.995734176295034,1.,0.995734176295034,1.,0.995734176295034,
1.,0.995734176295034,1.,0.995734176295034,1.,0.995734176295034,1.,0.995734176295034,
1.,0.995734176295034,1.,0.995734176295034,1.,0.995734176295034,1.,0.995734176295034,
1.,0.995734176295034,1.,0.995734176295034,1.,0.995734176295034,1.,0.995734176295034,
1.,0.995734176295034,1.,0.995734176295034,1.,0.995734176295034,1.,0.995734176295034,
1.,0.995734176295034,1.,0.995734176295034,1.,0.995734176295034,1.,0.995734176295034,
1.,0.995734176295034,1.,0.995734176295034,1.,0.995734176295034,1.,0.995734176295034,
1.,0.995734176295034,1.,0.995734176295034,1.,0.995734176295034,1.,0.995734176295034,
1.,0.995734176295034,1.,0.995734176295034,1.,0.995734176295034,1.,0.995734176295034,
1.,0.995734176295034,1.,0.995734176295034,1.,0.995734176295034,1.,0.995734176295034,
1.,0.995734176295034,1.,0.995734176295034,1.,0.995734176295034,1.,0.995734176295034,
1.,0.995734176295034,1.,0.995734176295034,1.,0.995734176295034,1.,0.995734176295034,
1.,0.995734176295034,1.,0.995734176295034,1.,0.995734176295034,1.,0.995734176295034,
1.,0.995734176295034,1.,0.995734176295034,1.,0.995734176295034,1.,0.995734176295034,
1.,0.995734176295034,1.,0.995734176295034,1.,0.995734176295034,1.,0.995734176295034,
1.,0.995734176295034,1.,0.995734176295034,1.,0.995734176295034,1.,0.995734176295034,
1.,0.995734176295034,1.,0.995734176295034,1.,0.995734176295034,1.,0.995734176295034,
1.,0.995734176295034,1.,0.995734176295034,1.,0.995734176295034,1.,0.995734176295034,
1.,0.995734176295034,1.,0.995734176295034,1.,0.995734176295034,1.,0.995734176295034,
1.,0.995734176295034,1.,0.995734176295034,1.,0.995734176295034,1.,0.995734176295034,
1.,0.995734176295034,1.,0.995734176295034,1.,0.995734176295034,1.,0.995734176295034,
1.,0.995734176295034,1.,0.995734176295034,1.,0.995734176295034,1.,0.995734176295034,
1.,0.995734176295034,1.,0.995734176295034,1.,0.995734176295034,1.,0.995734176295034,
1.,0.995734176295034,1.,0.995734176295034,1.,0.995734176295034,1.,0.995734176295034,
1.,0.995734176295034,1.,0.995734176295034,1.,0.995734176295034,1.,0.995734176295034,
1.,0.995734176295034,1.,0.995734176295034,1.,0.995734176295034,1.,0.995734176295034,
1.,0.995734176295034,1.,0.995734176295034,1.,0.995734176295034,1.,0.995734176295034,
1.,0.995734176295034,1.,0.995734176295034,1.,0.995734176295034,1.,0.995734176295034,
1.,0.995734176295034,1.,0.995734176295034,1.,0.995734176295034,1.,0.995734176295034,
1.,0.995734176295034,1.,0.995734176295034,1.,0.995734176295034,1.,0.995734176295034,
1.,0.995734176295034,1.,0.995734176295034,1.,0.995734176295034,1.,0.995734176295034,
1.,0.995734176295034,1.,0.995734176295034,1.,0.995734176295034,1.,0.995734176295034,
1.,0.995734176295034,1.,0.995734176295034,1.,0.995734176295034,1.,0.995734176295034,
1.,0.995734176295034,1.,0.995734176295034,1.,0.995734176295034,1.,0.995734176295034,
1.,0.995734176295034,1.,0.995734176295034,1.,0.995734176295034,1.,0.995734176295034,
1.,0.995734176295034,1.,0.995734176295034,1.,0.995734176295034,1.,0.995734176295034,
1.,0.995734176295034,1.,0.995734176295034,1.,0.995734176295034,1.,0.995734176295034,
1.,0.995734176295034,1.,0.995734176295034,1.,0.995734176295034,1.,0.995734176295034,
1.,0.995734176295034,1.,0.995734176295034,1.,0.995734176295034,1.,0.995734176295034,
1.,0.995734176295034,1.,0.995734176295034,1.,0.995734176295034,1.,0.995734176295034,
1.,0.995734176295034,1.,0.995734176295034,1.,0.995734176295034,1.,0.995734176295034,
1.,0.995734176295034,1.,0.995734176295034,1.,0.995734176295034,1.,0.995734176295034,
1.,0.995734176295034,1.,0.995734176295034,1.,0.995734176295034,1.,0.995734176295034,
1.,0.995734176295034,1.,0.995734176295034,1.,0.995734176295034,1.,0.995734176295034,
1.,0.995734176295034,1.,0.995734176295034,1.,0.995734176295034,1.,0.995734176295034,
1.,0.995734176295034,1.,0.995734176295034,1.,0.995734176295034,1.,0.995734176295034,
1.,0.995734176295034,1.,0.995734176295034,1.,0.995734176295034,1.,0.995734176295034,
1.,0.995734176295034,1.,0.995734176295034,1.,0.995734176295034,1.,0.995734176295034,
1.,0.995734176295034,1.,0.995734176295034,1.,0.995734176295034,1.,0.995734176295034,
1.,0.995734176295034,1.,0.995734176295034,1.,0.995734176295034,1.,0.995734176295034,
1.,0.995734176295034,1.,0.995734176295034,1.,0.995734176295034,1.,0.995734176295034,
1.,0.995734176295034,1.,0.995734176295034,1.,0.995734176295034,1.,0.995734176295034,
1.,0.995734176295034,1.,0.995734176295034,1.,0.995734176295034,1.,0.995734176295034,
1.,0.995734176295034,1.,0.995734176295034,1.,0.995734176295034,1.,0.995734176295034,
1.,0.995734176295034,1.,0.995734176295034,1.,0.995734176295034,1.,0.995734176295034,
1.,0.995734176295034,1.,0.995734176295034,1.,0.995734176295034,1.,0.995734176295034,
1.,0.995734176295034,1.,0.995734176295034,1.,0.995734176295034,1.,0.995734176295034,
1.,0.995734176295034,1.,0.995734176295034,1.,0.995734176295034,1.,0.995734176295034,
1.,0.995734176295034,1.,0.995734176295034,1.,0.995734176295034,1.,0.995734176295034,
1.,0.995734176295034,1.,0.995734176295034,1.,0.995734176295034,1.,0.995734176295034,
1.,0.995734176295034,1.,0.995734176295034,1.,0.995734176295034,1.,0.995734176295034,
1.,0.995734176295034,1.,0.995734176295034,1.,0.995734176295034,1.,0.995734176295034,
1.,0.995734176295034,1.,0.995734176295034,1.,0.995734176295034,1.,0.995734176295034,
1.,0.995734176295034,1.,0.995734176295034,1.,0.995734176295034,1.,0.995734176295034,
1.,0.995734176295034,1.,0.995734176295034,1.,0.995734176295034,1.,0.995734176295034,
1.,0.995734176295034,1.,0.995734176295034,1.,0.995734176295034,1.,0.995734176295034,
1.,0.995734176295034,1.,0.995734176295034,1.,0.995734176295034,1.,0.995734176295034,
1.,0.995734176295034,1.,0.995734176295034,1.,0.995734176295034,1.,0.995734176295034,
1.,0.995734176295034,1.,0.995734176295034,1.,0.995734176295034,1.,0.995734176295034,
1.,0.995734176295034,1.,0.995734176295034,1.,0.995734176295034,1.,0.995734176295034,
1.,0.995734176295034,1.,0.995734176295034,1.,0.995734176295034,1.,0.995734176295034,
1.,0.995734176295034,1.,0.995734176295034,1.,0.995734176295034,1.,0.995734176295034,
1.,0.995734176295034,1.,0.995734176295034,1.,0.995734176295034,1.,0.995734176295034,
1.,0.995734176295034,1.,0.995734176295034,1.,0.995734176295034,1.,0.995734176295034,
1.,0.995734176295034,1.,0.995734176295034,1.,0.995734176295034,1.,0.995734176295034,
1.,0.995734176295034,1.,0.995734176295034,1.,0.995734176295034,1.,0.995734176295034,
1.,0.995734176295034,1.,0.995734176295034,1.,0.995734176295034,1.,0.995734176295034,
1.,0.995734176295034,1.,0.995734176295034,1.,0.995734176295034,1.,0.995734176295034,
1.,0.995734176295034,1.,0.995734176295034,1.,0.995734176295034,1.,0.995734176295034,
1.,0.995734176295034,1.,0.995734176295034,1.,0.995734176295034,1.,0.995734176295034,
1.,0.995734176295034,1.,0.995734176295034,1.,0.995734176295034,1.,0.995734176295034,
1.,0.995734176295034,1.,0.995734176295034,1.,0.995734176295034,1.,0.995734176295034,
1.,0.995734176295034,1.,0.995734176295034,1.,0.995734176295034,1.,0.995734176295034,
1.,0.995734176295034,1.,0.995734176295034,1.,0.995734176295034,1.,0.995734176295034,
1.,0.995734176295034,1.,0.995734176295034,1.,0.995734176295034,1.,0.995734176295034,
1.,0.995734176295034,1.,0.995734176295034,1.,0.995734176295034,1.,0.995734176295034,
1.,0.995734176295034,1.,0.995734176295034,1.,0.995734176295034,1.,0.995734176295034,
1.,0.995734176295034,1.,0.995734176295034,1.,0.995734176295034,1.,0.995734176295034,
1.,0.995734176295034,1.,0.995734176295034,1.,0.995734176295034,1.,0.995734176295034,
1.,0.995734176295034,1.,0.995734176295034,1.,0.995734176295034,1.,0.995734176295034,
1.,0.995734176295034,1.,0.995734176295034,1.,0.995734176295034,1.,0.995734176295034,
1.,0.995734176295034,1.,0.995734176295034,1.,0.995734176295034,1.,0.995734176295034,
1.,0.995734176295034,1.,0.995734176295034,1.,0.995734176295034,1.,0.995734176295034,
1.,0.995734176295034,1.,0.995734176295034,1.,0.995734176295034,1.,0.995734176295034,
1.,0.995734176295034,1.,0.995734176295034,1.,0.995734176295034,1.,0.995734176295034,
1.,0.995734176295034,1.,0.995734176295034,1.,0.995734176295034,1.,0.995734176295034,
1.,0.995734176295034,1.,0.995734176295034,1.,0.995734176295034,1.,0.995734176295034,
1.,0.995734176295034,1.,0.995734176295034,1.,0.995734176295034,1.,0.995734176295034,
1.,0.995734176295034,1.,0.995734176295034,1.,0.995734176295034,1.,0.995734176295034,
1.,0.995734176295034,1.,0.995734176295034,1.,0.995734176295034,1.,0.995734176295034,
1.,0.995734176295034,1.,0.995734176295034,1.,0.995734176295034,1.,0.995734176295034,
1.,0.995734176295034,1.,0.995734176295034,1.,0.995734176295034,1.,0.995734176295034,
1.,0.995734176295034,1.,0.995734176295034,1.,0.995734176295034,1.,0.995734176295034,
1.,0.995734176295034,1.,0.995734176295034,1.,0.995734176295034,1.,0.995734176295034,
1.,0.995734176295034,1.,0.995734176295034,1.,0.995734176295034,1.,0.995734176295034,
1.,0.995734176295034,1.,0.995734176295034,1.,0.995734176295034,1.,0.995734176295034,
1.,0.995734176295034,1.,0.995734176295034,1.,0.995734176295034,1.,0.995734176295034,
1.,0.995734176295034,1.,0.995734176295034,1.,0.995734176295034,1.,0.995734176295034,
1.,0.995734176295034,1.,0.995734176295034,1.,0.995734176295034,1.,0.995734176295034,
1.,0.995734176295034,1.,0.995734176295034,1.,0.995734176295034,1.,0.995734176295034,
1.,0.995734176295034,1.,0.995734176295034,1.,0.995734176295034,1.,0.995734176295034,
1.,0.995734176295034,1.,0.995734176295034,1.,0.995734176295034,1.,0.995734176295034,
1.,0.995734176295034,1.,0.995734176295034,1.,0.995734176295034,1.,0.995734176295034,
1.,0.995734176295034,1.,0.995734176295034,1.,0.995734176295034,1.,0.995734176295034,
1.,0.995734176295034,1.,0.995734176295034,1.,0.995734176295034,1.,0.995734176295034,
1.,0.995734176295034,1.,0.995734176295034,1.,0.995734176295034,1.,0.995734176295034,
1.,0.995734176295034,1.,0.995734176295034,1.,0.995734176295034,1.,0.995734176295034,
1.,0.995734176295034,1.,0.995734176295034,1.,0.995734176295034,1.,0.995734176295034,
1.,0.995734176295034,1.,0.995734176295034,1.,0.995734176295034,1.,0.995734176295034,
1.,0.995734176295034,1.,0.995734176295034,1.,0.995734176295034,1.,0.995734176295034,
1.,0.995734176295034,1.,0.995734176295034,1.,0.995734176295034,1.,0.995734176295034,
1.,0.995734176295034,1.,0.995734176295034,1.,0.995734176295034,1.,0.995734176295034,
1.,0.995734176295034,1.,0.995734176295034,1.,0.995734176295034,1.,0.995734176295034,
1.,0.995734176295034,1.,0.995734176295034,1.,0.995734176295034,1.,0.995734176295034,
1.,0.995734176295034,1.,0.995734176295034,1.,0.995734176295034,1.,0.995734176295034,
1.,0.995734176295034,1.,0.995734176295034,1.,0.995734176295034,1.,0.995734176295034,
1.,0.995734176295034,1.,0.995734176295034,1.,0.995734176295034,1.,0.995734176295034,
1.,0.995734176295034,1.,0.995734176295034,1.,0.995734176295034,1.,0.995734176295034,
1.,0.995734176295034,1.,0.995734176295034,1.,0.995734176295034,1.,0.995734176295034,
1.,0.995734176295034,1.,0.995734176295034,1.,0.995734176295034,1.,0.995734176295034,
1.,0.995734176295034,1.,0.995734176295034,1.,0.995734176295034,1.,0.995734176295034,
1.,0.995734176295034,1.,0.995734176295034,1.,0.995734176295034,1.,0.995734176295034,
1.,0.995734176295034,1.,0.995734176295034,1.,0.995734176295034,1.,0.995734176295034,
1.,0.995734176295034,1.,0.995734176295034,1.,0.995734176295034,1.,0.995734176295034,
1.,0.995734176295034,1.,0.995734176295034,1.,0.995734176295034,1.,0.995734176295034,
1.,0.995734176295034,1.,0.995734176295034,1.,0.995734176295034,1.,0.995734176295034,
1.,0.995734176295034,1.,0.995734176295034,1.,0.995734176295034,1.,0.995734176295034,
1.,0.995734176295034,1.,0.995734176295034,1.,0.995734176295034,1.,0.995734176295034,
1.,0.995734176295034,1.,0.995734176295034,1.,0.995734176295034,1.,0.995734176295034,
1.,0.995734176295034,1.,0.995734176295034,1.,0.995734176295034,1.,0.995734176295034,
1.,0.995734176295034,1.,0.995734176295034,1.,0.995734176295034,1.,0.995734176295034,
1.,0.995734176295034,1.,0.995734176295034,1.,0.995734176295034,1.,0.995734176295034,
1.,0.995734176295034,1.,0.995734176295034,1.,0.995734176295034,1.,0.995734176295034,
1.,0.995734176295034,1.,0.995734176295034,1.,0.995734176295034,1.,0.995734176295034,
1.,0.995734176295034,1.,0.995734176295034,1.,0.995734176295034,1.,0.995734176295034,
1.,0.995734176295034,1.,0.995734176295034,1.,0.995734176295034,1.,0.995734176295034,
1.,0.995734176295034,1.,0.995734176295034,1.,0.995734176295034,1.,0.995734176295034,
1.,0.995734176295034,1.,0.995734176295034,1.,0.995734176295034,1.,0.995734176295034,
1.,0.995734176295034,1.,0.995734176295034,1.,0.995734176295034,1.,0.995734176295034,
1.,0.995734176295034,1.,0.995734176295034,1.,0.995734176295034,1.,0.995734176295034,
1.,0.995734176295034,1.,0.995734176295034,1.,0.995734176295034,1.,0.995734176295034,
1.,0.995734176295034,1.,0.995734176295034,1.,0.995734176295034,1.,0.995734176295034,
1.,0.995734176295034,1.,0.995734176295034,1.,0.995734176295034,1.,0.995734176295034,
1.,0.995734176295034,1.,0.995734176295034,1.,0.995734176295034,1.,0.995734176295034,
1.,0.995734176295034,1.,0.995734176295034,1.,0.995734176295034,1.,0.995734176295034,
1.,0.995734176295034,1.,0.995734176295034,1.,0.995734176295034,1.,0.995734176295034,
1.,0.995734176295034,1.,0.995734176295034,1.,0.995734176295034,1.,0.995734176295034,
1.,0.995734176295034,1.,0.995734176295034,1.,0.995734176295034,1.,0.995734176295034,
1.,0.995734176295034,1.,0.995734176295034,1.,0.995734176295034,1.,0.995734176295034,
1.,0.995734176295034,1.,0.995734176295034,1.,0.995734176295034,1.,0.995734176295034,
1.,0.995734176295034,1.,0.995734176295034,1.,0.995734176295034,1.,0.995734176295034,
1.,0.995734176295034,1.,0.995734176295034,1.,0.995734176295034,1.,0.995734176295034,
1.,0.995734176295034,1.,0.995734176295034,1.,0.995734176295034,1.,0.995734176295034,
1.,0.995734176295034,1.,0.995734176295034,1.,0.995734176295034,1.,0.995734176295034,
1.,0.995734176295034,1.,0.995734176295034,1.,0.995734176295034,1.,0.995734176295034,
1.,0.995734176295034,1.,0.995734176295034,1.,0.995734176295034,1.,0.995734176295034,
1.,0.995734176295034,1.,0.995734176295034,1.,0.995734176295034,1.,0.995734176295034,
1.,0.995734176295034,1.,0.995734176295034,1.,0.995734176295034,1.,0.995734176295034,
1.,0.995734176295034,1.,0.995734176295034,1.,0.995734176295034,1.,0.995734176295034,
1.,0.995734176295034,1.,0.995734176295034,1.,0.995734176295034,1.,0.995734176295034,
1.,0.995734176295034,1.,0.995734176295034,1.,0.995734176295034,1.,0.995734176295034,
1.,0.995734176295034,1.,0.995734176295034,1.,0.995734176295034,1.,0.995734176295034,
1.,0.995734176295034,1.,0.995734176295034,1.,0.995734176295034,1.,0.995734176295034,
1.,0.995734176295034,1.,0.995734176295034,1.,0.995734176295034,1.,0.995734176295034,
1.,0.995734176295034,1.,0.995734176295034,1.,0.995734176295034,1.,0.995734176295034,
1.,0.995734176295034,1.,0.995734176295034,1.,0.995734176295034,1.,0.995734176295034,
1.,0.995734176295034,1.,0.995734176295034,1.,0.995734176295034,1.,0.995734176295034,
1.,0.995734176295034,1.,0.995734176295034,1.,0.995734176295034,1.,0.995734176295034,
1.,0.995734176295034,1.,0.995734176295034,1.,0.995734176295034,1.,0.995734176295034,
1.,0.995734176295034,1.,0.995734176295034,1.,0.995734176295034,1.,0.995734176295034,
1.,0.995734176295034,1.,0.995734176295034,1.,0.995734176295034,1.,0.995734176295034,
1.,0.995734176295034,1.,0.995734176295034,1.,0.995734176295034,1.,0.995734176295034,
1.,0.995734176295034,1.,0.995734176295034,1.,0.995734176295034,1.,0.995734176295034,
1.,0.995734176295034,1.,0.995734176295034,1.,0.995734176295034,1.,0.995734176295034,
1.,0.995734176295034,1.,0.995734176295034,1.,0.995734176295034,1.,0.995734176295034,
1.,0.995734176295034,1.,0.995734176295034,1.,0.995734176295034,1.,0.995734176295034,
1.,0.995734176295034,1.,0.995734176295034,1.,0.995734176295034,1.,0.995734176295034,
1.,0.995734176295034,1.,0.995734176295034,1.,0.995734176295034,1.,0.995734176295034,
1.,0.995734176295034,1.,0.995734176295034,1.,0.995734176295034,1.,0.995734176295034,
1.,0.995734176295034,1.,0.995734176295034,1.,0.995734176295034,1.,0.995734176295034,
1.,0.995734176295034,1.,0.995734176295034,1.,0.995734176295034,1.,0.995734176295034,
1.,0.995734176295034,1.,0.995734176295034,1.,0.995734176295034,1.,0.995734176295034,
1.,0.995734176295034,1.,0.995734176295034,1.,0.995734176295034,1.,0.995734176295034,
1.,0.995734176295034,1.,0.995734176295034,1.,0.995734176295034,1.,0.995734176295034,
1.,0.995734176295034,1.,0.995734176295034,1.,0.995734176295034,1.,0.995734176295034,
1.,0.995734176295034,1.,0.995734176295034,1.,0.995734176295034,1.,0.995734176295034,
1.,0.995734176295034,1.,0.995734176295034,1.,0.995734176295034,1.,0.995734176295034,
1.,0.995734176295034,1.,0.995734176295034,1.,0.995734176295034,1.,0.995734176295034,
1.,0.995734176295034,1.,0.995734176295034,1.,0.995734176295034,1.,0.995734176295034,
1.,0.995734176295034,1.,0.995734176295034,1.,0.995734176295034,1.,0.995734176295034,
1.,0.995734176295034,1.,0.995734176295034,1.,0.995734176295034,1.,0.995734176295034,
1.,0.995734176295034,1.,0.995734176295034,1.,0.995734176295034,1.,0.995734176295034,
1.,0.995734176295034,1.,0.995734176295034,1.,0.995734176295034,1.,0.995734176295034,
1.,0.995734176295034,1.,0.995734176295034,1.,0.995734176295034,1.,0.995734176295034,
1.,0.995734176295034,1.,0.995734176295034,1.,0.995734176295034,1.,0.995734176295034,
1.,0.997201441372082,0.998074825578922,0.998074825578922,0.998074825578922)))
REPRESENTATION_ITEM('')
SURFACE()
);
#2504=(
BOUNDED_SURFACE()
B_SPLINE_SURFACE(1,2,((#158529,#158530,#158531,#158532,#158533,#158534,
#158535,#158536,#158537,#158538,#158539,#158540,#158541,#158542,#158543,
#158544,#158545,#158546,#158547,#158548,#158549,#158550,#158551,#158552,
#158553,#158554,#158555,#158556,#158557,#158558,#158559,#158560,#158561,
#158562,#158563,#158564,#158565,#158566,#158567,#158568,#158569,#158570,
#158571,#158572,#158573,#158574,#158575,#158576,#158577,#158578,#158579,
#158580,#158581,#158582,#158583,#158584,#158585,#158586,#158587,#158588,
#158589,#158590,#158591,#158592,#158593,#158594,#158595,#158596,#158597,
#158598,#158599,#158600,#158601,#158602,#158603,#158604,#158605,#158606,
#158607,#158608,#158609,#158610,#158611,#158612,#158613,#158614,#158615,
#158616,#158617,#158618,#158619,#158620,#158621,#158622,#158623,#158624,
#158625,#158626,#158627,#158628,#158629,#158630,#158631,#158632,#158633,
#158634,#158635,#158636,#158637,#158638,#158639,#158640,#158641,#158642,
#158643,#158644,#158645,#158646,#158647,#158648,#158649,#158650,#158651,
#158652,#158653,#158654,#158655,#158656,#158657,#158658,#158659,#158660,
#158661,#158662,#158663,#158664,#158665,#158666,#158667,#158668,#158669,
#158670,#158671,#158672,#158673,#158674,#158675,#158676,#158677,#158678,
#158679,#158680,#158681,#158682,#158683,#158684,#158685,#158686,#158687,
#158688,#158689,#158690,#158691,#158692,#158693,#158694,#158695,#158696,
#158697,#158698,#158699,#158700,#158701,#158702,#158703,#158704,#158705,
#158706,#158707,#158708,#158709,#158710,#158711,#158712,#158713,#158714,
#158715,#158716,#158717,#158718,#158719,#158720,#158721,#158722,#158723,
#158724,#158725,#158726,#158727,#158728,#158729,#158730,#158731,#158732,
#158733,#158734,#158735,#158736,#158737,#158738,#158739,#158740,#158741,
#158742,#158743,#158744,#158745,#158746,#158747,#158748,#158749,#158750,
#158751,#158752,#158753,#158754,#158755,#158756,#158757,#158758,#158759,
#158760,#158761,#158762,#158763,#158764,#158765,#158766,#158767,#158768,
#158769,#158770,#158771,#158772,#158773,#158774,#158775,#158776,#158777,
#158778,#158779,#158780,#158781,#158782,#158783,#158784,#158785,#158786,
#158787,#158788,#158789,#158790,#158791,#158792,#158793,#158794,#158795,
#158796,#158797,#158798,#158799,#158800,#158801,#158802,#158803,#158804,
#158805,#158806,#158807,#158808,#158809,#158810,#158811,#158812,#158813,
#158814,#158815,#158816,#158817,#158818,#158819,#158820,#158821,#158822,
#158823,#158824,#158825,#158826,#158827,#158828,#158829,#158830,#158831,
#158832,#158833,#158834,#158835,#158836,#158837,#158838,#158839,#158840,
#158841,#158842,#158843,#158844,#158845,#158846,#158847,#158848,#158849,
#158850,#158851,#158852,#158853,#158854,#158855,#158856,#158857,#158858,
#158859,#158860,#158861,#158862,#158863,#158864,#158865,#158866,#158867,
#158868,#158869,#158870,#158871,#158872,#158873,#158874,#158875,#158876,
#158877,#158878,#158879,#158880,#158881,#158882,#158883,#158884,#158885,
#158886,#158887,#158888,#158889,#158890,#158891,#158892,#158893,#158894,
#158895,#158896,#158897,#158898,#158899,#158900,#158901,#158902,#158903,
#158904,#158905,#158906,#158907,#158908,#158909,#158910,#158911,#158912,
#158913,#158914,#158915,#158916,#158917,#158918,#158919,#158920,#158921,
#158922,#158923,#158924,#158925,#158926,#158927,#158928,#158929,#158930,
#158931,#158932,#158933,#158934,#158935,#158936,#158937,#158938,#158939,
#158940,#158941,#158942,#158943,#158944,#158945,#158946,#158947,#158948,
#158949,#158950,#158951,#158952,#158953,#158954,#158955,#158956,#158957,
#158958,#158959,#158960,#158961,#158962,#158963,#158964,#158965,#158966,
#158967,#158968,#158969,#158970,#158971,#158972,#158973,#158974,#158975,
#158976,#158977,#158978,#158979,#158980,#158981,#158982,#158983,#158984,
#158985,#158986,#158987,#158988,#158989,#158990,#158991,#158992,#158993,
#158994,#158995,#158996,#158997,#158998,#158999,#159000,#159001,#159002,
#159003,#159004,#159005,#159006,#159007,#159008,#159009,#159010,#159011,
#159012,#159013,#159014,#159015,#159016,#159017,#159018,#159019,#159020,
#159021,#159022,#159023,#159024,#159025,#159026,#159027,#159028,#159029,
#159030,#159031,#159032,#159033,#159034,#159035,#159036,#159037,#159038,
#159039,#159040,#159041,#159042,#159043,#159044,#159045,#159046,#159047,
#159048,#159049,#159050,#159051,#159052,#159053,#159054,#159055,#159056,
#159057,#159058,#159059,#159060,#159061,#159062,#159063,#159064,#159065,
#159066,#159067,#159068,#159069,#159070,#159071,#159072,#159073,#159074,
#159075,#159076,#159077,#159078,#159079,#159080,#159081,#159082,#159083,
#159084,#159085,#159086,#159087,#159088,#159089,#159090,#159091,#159092,
#159093,#159094,#159095,#159096,#159097,#159098,#159099,#159100,#159101,
#159102,#159103,#159104,#159105,#159106,#159107,#159108,#159109,#159110,
#159111,#159112,#159113,#159114,#159115,#159116,#159117,#159118,#159119,
#159120,#159121,#159122,#159123,#159124,#159125,#159126,#159127,#159128,
#159129,#159130,#159131,#159132,#159133,#159134,#159135,#159136,#159137,
#159138,#159139,#159140,#159141,#159142,#159143,#159144,#159145,#159146,
#159147,#159148,#159149,#159150,#159151,#159152,#159153,#159154,#159155,
#159156,#159157,#159158,#159159,#159160,#159161,#159162,#159163,#159164,
#159165,#159166,#159167,#159168,#159169,#159170,#159171,#159172,#159173,
#159174,#159175,#159176,#159177,#159178,#159179,#159180,#159181,#159182,
#159183,#159184,#159185,#159186,#159187,#159188,#159189,#159190,#159191,
#159192,#159193,#159194,#159195,#159196,#159197,#159198,#159199,#159200,
#159201,#159202,#159203,#159204,#159205,#159206,#159207,#159208,#159209,
#159210,#159211,#159212,#159213,#159214,#159215,#159216,#159217,#159218,
#159219,#159220,#159221,#159222,#159223,#159224,#159225,#159226,#159227,
#159228,#159229,#159230,#159231,#159232,#159233,#159234,#159235,#159236,
#159237,#159238,#159239,#159240,#159241,#159242,#159243,#159244,#159245,
#159246,#159247,#159248,#159249,#159250,#159251,#159252,#159253,#159254,
#159255,#159256,#159257,#159258,#159259,#159260,#159261,#159262,#159263,
#159264,#159265,#159266,#159267,#159268,#159269,#159270,#159271,#159272,
#159273,#159274,#159275,#159276,#159277,#159278,#159279,#159280,#159281,
#159282,#159283,#159284,#159285,#159286,#159287,#159288,#159289,#159290,
#159291,#159292,#159293,#159294,#159295,#159296,#159297,#159298,#159299,
#159300,#159301,#159302,#159303,#159304,#159305,#159306,#159307,#159308,
#159309,#159310,#159311,#159312,#159313,#159314,#159315,#159316,#159317,
#159318,#159319,#159320,#159321,#159322,#159323,#159324,#159325,#159326,
#159327,#159328,#159329,#159330,#159331,#159332,#159333,#159334,#159335,
#159336,#159337,#159338,#159339,#159340,#159341,#159342,#159343,#159344,
#159345,#159346,#159347,#159348,#159349,#159350,#159351,#159352,#159353,
#159354,#159355,#159356,#159357,#159358,#159359,#159360,#159361,#159362,
#159363,#159364,#159365,#159366,#159367,#159368,#159369,#159370,#159371,
#159372,#159373,#159374,#159375,#159376,#159377,#159378,#159379,#159380,
#159381,#159382,#159383,#159384,#159385,#159386,#159387,#159388,#159389,
#159390,#159391,#159392,#159393,#159394,#159395,#159396,#159397,#159398,
#159399,#159400,#159401,#159402,#159403,#159404,#159405,#159406,#159407,
#159408,#159409,#159410,#159411,#159412,#159413,#159414,#159415,#159416,
#159417,#159418,#159419,#159420,#159421,#159422,#159423,#159424,#159425,
#159426,#159427,#159428,#159429,#159430,#159431,#159432,#159433,#159434,
#159435,#159436,#159437,#159438,#159439,#159440,#159441,#159442,#159443,
#159444,#159445,#159446,#159447,#159448,#159449,#159450,#159451,#159452,
#159453,#159454,#159455,#159456,#159457,#159458,#159459,#159460,#159461,
#159462,#159463,#159464,#159465,#159466,#159467,#159468,#159469,#159470,
#159471,#159472,#159473,#159474,#159475,#159476,#159477,#159478,#159479,
#159480,#159481,#159482,#159483,#159484,#159485,#159486,#159487,#159488,
#159489,#159490,#159491,#159492,#159493,#159494,#159495,#159496,#159497,
#159498,#159499,#159500,#159501,#159502,#159503,#159504,#159505,#159506,
#159507,#159508,#159509,#159510,#159511,#159512,#159513,#159514,#159515,
#159516,#159517,#159518,#159519,#159520,#159521,#159522,#159523,#159524,
#159525,#159526,#159527,#159528,#159529,#159530,#159531,#159532,#159533,
#159534,#159535,#159536,#159537,#159538,#159539,#159540,#159541,#159542,
#159543,#159544,#159545,#159546,#159547,#159548,#159549,#159550,#159551,
#159552,#159553,#159554,#159555,#159556,#159557,#159558,#159559,#159560,
#159561,#159562,#159563,#159564,#159565,#159566,#159567,#159568,#159569,
#159570,#159571,#159572,#159573,#159574,#159575,#159576,#159577,#159578,
#159579,#159580,#159581,#159582,#159583,#159584,#159585,#159586,#159587,
#159588,#159589,#159590,#159591,#159592,#159593,#159594,#159595,#159596,
#159597,#159598,#159599,#159600,#159601,#159602,#159603,#159604,#159605,
#159606,#159607,#159608,#159609,#159610,#159611,#159612,#159613,#159614,
#159615,#159616,#159617,#159618,#159619,#159620,#159621,#159622,#159623,
#159624,#159625,#159626,#159627,#159628,#159629,#159630,#159631,#159632,
#159633,#159634,#159635,#159636,#159637,#159638,#159639,#159640,#159641,
#159642,#159643,#159644,#159645,#159646,#159647,#159648,#159649,#159650,
#159651,#159652,#159653,#159654,#159655,#159656,#159657,#159658,#159659,
#159660,#159661,#159662,#159663,#159664,#159665,#159666,#159667,#159668,
#159669,#159670,#159671,#159672,#159673,#159674,#159675,#159676,#159677,
#159678,#159679,#159680,#159681,#159682,#159683,#159684,#159685,#159686,
#159687,#159688,#159689,#159690,#159691,#159692,#159693,#159694,#159695,
#159696,#159697,#159698,#159699,#159700,#159701,#159702,#159703,#159704,
#159705,#159706,#159707,#159708,#159709,#159710,#159711,#159712,#159713,
#159714,#159715,#159716,#159717,#159718,#159719,#159720,#159721,#159722,
#159723,#159724,#159725,#159726,#159727,#159728,#159729,#159730,#159731,
#159732,#159733,#159734,#159735,#159736,#159737,#159738,#159739,#159740,
#159741,#159742,#159743,#159744,#159745,#159746,#159747,#159748,#159749,
#159750,#159751,#159752,#159753,#159754,#159755,#159756,#159757,#159758,
#159759,#159760,#159761,#159762,#159763,#159764,#159765,#159766,#159767,
#159768,#159769,#159770,#159771,#159772,#159773,#159774,#159775,#159776,
#159777,#159778,#159779,#159780,#159781,#159782,#159783,#159784,#159785,
#159786,#159787,#159788,#159789,#159790,#159791,#159792,#159793,#159794,
#159795,#159796,#159797,#159798,#159799,#159800,#159801,#159802,#159803,
#159804,#159805,#159806,#159807,#159808,#159809,#159810,#159811,#159812,
#159813,#159814,#159815,#159816,#159817,#159818,#159819,#159820,#159821,
#159822,#159823,#159824,#159825,#159826,#159827,#159828,#159829,#159830,
#159831,#159832,#159833,#159834,#159835,#159836,#159837,#159838,#159839,
#159840,#159841,#159842,#159843,#159844,#159845,#159846,#159847,#159848,
#159849,#159850,#159851,#159852,#159853,#159854,#159855,#159856,#159857,
#159858,#159859,#159860,#159861,#159862,#159863,#159864,#159865,#159866,
#159867,#159868,#159869,#159870,#159871,#159872,#159873,#159874,#159875,
#159876,#159877,#159878,#159879,#159880,#159881,#159882,#159883,#159884,
#159885,#159886,#159887,#159888,#159889,#159890,#159891,#159892,#159893,
#159894,#159895,#159896,#159897,#159898,#159899,#159900,#159901,#159902,
#159903,#159904,#159905,#159906,#159907,#159908,#159909,#159910,#159911,
#159912,#159913,#159914,#159915,#159916,#159917,#159918,#159919,#159920,
#159921,#159922,#159923,#159924,#159925,#159926,#159927,#159928,#159929,
#159930,#159931,#159932,#159933,#159934,#159935,#159936,#159937,#159938,
#159939,#159940,#159941,#159942,#159943,#159944,#159945,#159946,#159947,
#159948,#159949,#159950,#159951,#159952,#159953,#159954,#159955,#159956,
#159957,#159958,#159959,#159960,#159961,#159962,#159963,#159964,#159965,
#159966,#159967,#159968,#159969,#159970,#159971,#159972,#159973,#159974,
#159975,#159976,#159977,#159978,#159979,#159980,#159981,#159982,#159983,
#159984,#159985,#159986,#159987,#159988,#159989,#159990,#159991,#159992,
#159993,#159994,#159995,#159996,#159997,#159998,#159999,#160000,#160001,
#160002,#160003,#160004,#160005,#160006,#160007,#160008,#160009,#160010,
#160011,#160012,#160013,#160014,#160015,#160016,#160017,#160018,#160019,
#160020,#160021,#160022,#160023,#160024,#160025,#160026,#160027,#160028,
#160029,#160030,#160031,#160032,#160033,#160034,#160035,#160036,#160037,
#160038,#160039,#160040,#160041,#160042,#160043,#160044,#160045,#160046,
#160047,#160048,#160049,#160050,#160051,#160052,#160053,#160054,#160055,
#160056,#160057,#160058,#160059,#160060,#160061,#160062,#160063,#160064,
#160065,#160066,#160067,#160068,#160069,#160070,#160071,#160072,#160073,
#160074,#160075,#160076,#160077,#160078,#160079,#160080,#160081,#160082,
#160083,#160084,#160085,#160086,#160087,#160088,#160089,#160090,#160091,
#160092,#160093,#160094,#160095,#160096,#160097,#160098,#160099,#160100,
#160101,#160102,#160103,#160104,#160105,#160106,#160107,#160108,#160109,
#160110,#160111,#160112,#160113,#160114,#160115,#160116,#160117,#160118,
#160119,#160120,#160121,#160122,#160123,#160124,#160125,#160126,#160127,
#160128,#160129,#160130,#160131,#160132,#160133,#160134,#160135,#160136,
#160137,#160138,#160139,#160140,#160141,#160142,#160143,#160144,#160145,
#160146,#160147,#160148,#160149,#160150,#160151,#160152,#160153,#160154,
#160155,#160156,#160157,#160158,#160159,#160160,#160161,#160162,#160163,
#160164,#160165,#160166,#160167,#160168,#160169,#160170,#160171,#160172,
#160173,#160174,#160175,#160176,#160177,#160178,#160179,#160180,#160181,
#160182,#160183,#160184,#160185,#160186,#160187,#160188,#160189,#160190,
#160191,#160192,#160193,#160194,#160195,#160196,#160197,#160198,#160199,
#160200,#160201,#160202,#160203,#160204,#160205,#160206,#160207,#160208,
#160209,#160210,#160211,#160212,#160213,#160214,#160215,#160216,#160217,
#160218,#160219,#160220,#160221,#160222,#160223,#160224,#160225,#160226,
#160227,#160228,#160229,#160230,#160231,#160232,#160233,#160234,#160235,
#160236,#160237,#160238,#160239,#160240,#160241,#160242,#160243,#160244,
#160245,#160246,#160247,#160248,#160249,#160250,#160251,#160252,#160253,
#160254,#160255,#160256,#160257,#160258,#160259,#160260,#160261,#160262,
#160263,#160264,#160265,#160266,#160267,#160268,#160269,#160270,#160271,
#160272,#160273,#160274,#160275,#160276,#160277,#160278,#160279,#160280,
#160281,#160282,#160283,#160284,#160285,#160286,#160287,#160288,#160289,
#160290,#160291,#160292,#160293,#160294,#160295,#160296,#160297,#160298,
#160299,#160300,#160301,#160302,#160303,#160304,#160305,#160306,#160307,
#160308,#160309,#160310,#160311,#160312,#160313,#160314,#160315,#160316,
#160317,#160318,#160319,#160320,#160321,#160322,#160323,#160324,#160325,
#160326,#160327,#160328,#160329,#160330,#160331,#160332,#160333,#160334,
#160335,#160336,#160337,#160338,#160339,#160340,#160341,#160342,#160343,
#160344,#160345,#160346,#160347,#160348,#160349,#160350,#160351,#160352,
#160353,#160354,#160355,#160356,#160357,#160358,#160359,#160360,#160361,
#160362,#160363,#160364,#160365,#160366,#160367,#160368,#160369,#160370,
#160371,#160372,#160373,#160374,#160375,#160376,#160377,#160378,#160379,
#160380,#160381,#160382,#160383,#160384,#160385,#160386,#160387,#160388,
#160389,#160390,#160391,#160392,#160393,#160394,#160395,#160396,#160397,
#160398,#160399,#160400,#160401,#160402,#160403,#160404,#160405,#160406,
#160407,#160408,#160409,#160410,#160411,#160412,#160413,#160414,#160415,
#160416,#160417,#160418,#160419,#160420,#160421,#160422,#160423,#160424,
#160425,#160426,#160427,#160428,#160429,#160430,#160431,#160432,#160433,
#160434,#160435,#160436,#160437,#160438,#160439,#160440,#160441,#160442,
#160443,#160444,#160445,#160446,#160447,#160448,#160449,#160450,#160451,
#160452,#160453,#160454,#160455,#160456,#160457,#160458,#160459,#160460,
#160461,#160462,#160463,#160464,#160465,#160466,#160467,#160468,#160469,
#160470,#160471,#160472,#160473,#160474,#160475,#160476,#160477,#160478,
#160479,#160480,#160481,#160482,#160483,#160484,#160485,#160486,#160487,
#160488,#160489,#160490,#160491,#160492,#160493,#160494,#160495,#160496,
#160497,#160498,#160499,#160500,#160501,#160502,#160503,#160504,#160505,
#160506,#160507,#160508,#160509,#160510,#160511,#160512,#160513,#160514,
#160515,#160516,#160517,#160518,#160519,#160520,#160521,#160522,#160523,
#160524,#160525,#160526,#160527,#160528,#160529,#160530,#160531,#160532,
#160533,#160534,#160535,#160536,#160537,#160538,#160539,#160540,#160541),
(#160542,#160543,#160544,#160545,#160546,#160547,#160548,#160549,#160550,
#160551,#160552,#160553,#160554,#160555,#160556,#160557,#160558,#160559,
#160560,#160561,#160562,#160563,#160564,#160565,#160566,#160567,#160568,
#160569,#160570,#160571,#160572,#160573,#160574,#160575,#160576,#160577,
#160578,#160579,#160580,#160581,#160582,#160583,#160584,#160585,#160586,
#160587,#160588,#160589,#160590,#160591,#160592,#160593,#160594,#160595,
#160596,#160597,#160598,#160599,#160600,#160601,#160602,#160603,#160604,
#160605,#160606,#160607,#160608,#160609,#160610,#160611,#160612,#160613,
#160614,#160615,#160616,#160617,#160618,#160619,#160620,#160621,#160622,
#160623,#160624,#160625,#160626,#160627,#160628,#160629,#160630,#160631,
#160632,#160633,#160634,#160635,#160636,#160637,#160638,#160639,#160640,
#160641,#160642,#160643,#160644,#160645,#160646,#160647,#160648,#160649,
#160650,#160651,#160652,#160653,#160654,#160655,#160656,#160657,#160658,
#160659,#160660,#160661,#160662,#160663,#160664,#160665,#160666,#160667,
#160668,#160669,#160670,#160671,#160672,#160673,#160674,#160675,#160676,
#160677,#160678,#160679,#160680,#160681,#160682,#160683,#160684,#160685,
#160686,#160687,#160688,#160689,#160690,#160691,#160692,#160693,#160694,
#160695,#160696,#160697,#160698,#160699,#160700,#160701,#160702,#160703,
#160704,#160705,#160706,#160707,#160708,#160709,#160710,#160711,#160712,
#160713,#160714,#160715,#160716,#160717,#160718,#160719,#160720,#160721,
#160722,#160723,#160724,#160725,#160726,#160727,#160728,#160729,#160730,
#160731,#160732,#160733,#160734,#160735,#160736,#160737,#160738,#160739,
#160740,#160741,#160742,#160743,#160744,#160745,#160746,#160747,#160748,
#160749,#160750,#160751,#160752,#160753,#160754,#160755,#160756,#160757,
#160758,#160759,#160760,#160761,#160762,#160763,#160764,#160765,#160766,
#160767,#160768,#160769,#160770,#160771,#160772,#160773,#160774,#160775,
#160776,#160777,#160778,#160779,#160780,#160781,#160782,#160783,#160784,
#160785,#160786,#160787,#160788,#160789,#160790,#160791,#160792,#160793,
#160794,#160795,#160796,#160797,#160798,#160799,#160800,#160801,#160802,
#160803,#160804,#160805,#160806,#160807,#160808,#160809,#160810,#160811,
#160812,#160813,#160814,#160815,#160816,#160817,#160818,#160819,#160820,
#160821,#160822,#160823,#160824,#160825,#160826,#160827,#160828,#160829,
#160830,#160831,#160832,#160833,#160834,#160835,#160836,#160837,#160838,
#160839,#160840,#160841,#160842,#160843,#160844,#160845,#160846,#160847,
#160848,#160849,#160850,#160851,#160852,#160853,#160854,#160855,#160856,
#160857,#160858,#160859,#160860,#160861,#160862,#160863,#160864,#160865,
#160866,#160867,#160868,#160869,#160870,#160871,#160872,#160873,#160874,
#160875,#160876,#160877,#160878,#160879,#160880,#160881,#160882,#160883,
#160884,#160885,#160886,#160887,#160888,#160889,#160890,#160891,#160892,
#160893,#160894,#160895,#160896,#160897,#160898,#160899,#160900,#160901,
#160902,#160903,#160904,#160905,#160906,#160907,#160908,#160909,#160910,
#160911,#160912,#160913,#160914,#160915,#160916,#160917,#160918,#160919,
#160920,#160921,#160922,#160923,#160924,#160925,#160926,#160927,#160928,
#160929,#160930,#160931,#160932,#160933,#160934,#160935,#160936,#160937,
#160938,#160939,#160940,#160941,#160942,#160943,#160944,#160945,#160946,
#160947,#160948,#160949,#160950,#160951,#160952,#160953,#160954,#160955,
#160956,#160957,#160958,#160959,#160960,#160961,#160962,#160963,#160964,
#160965,#160966,#160967,#160968,#160969,#160970,#160971,#160972,#160973,
#160974,#160975,#160976,#160977,#160978,#160979,#160980,#160981,#160982,
#160983,#160984,#160985,#160986,#160987,#160988,#160989,#160990,#160991,
#160992,#160993,#160994,#160995,#160996,#160997,#160998,#160999,#161000,
#161001,#161002,#161003,#161004,#161005,#161006,#161007,#161008,#161009,
#161010,#161011,#161012,#161013,#161014,#161015,#161016,#161017,#161018,
#161019,#161020,#161021,#161022,#161023,#161024,#161025,#161026,#161027,
#161028,#161029,#161030,#161031,#161032,#161033,#161034,#161035,#161036,
#161037,#161038,#161039,#161040,#161041,#161042,#161043,#161044,#161045,
#161046,#161047,#161048,#161049,#161050,#161051,#161052,#161053,#161054,
#161055,#161056,#161057,#161058,#161059,#161060,#161061,#161062,#161063,
#161064,#161065,#161066,#161067,#161068,#161069,#161070,#161071,#161072,
#161073,#161074,#161075,#161076,#161077,#161078,#161079,#161080,#161081,
#161082,#161083,#161084,#161085,#161086,#161087,#161088,#161089,#161090,
#161091,#161092,#161093,#161094,#161095,#161096,#161097,#161098,#161099,
#161100,#161101,#161102,#161103,#161104,#161105,#161106,#161107,#161108,
#161109,#161110,#161111,#161112,#161113,#161114,#161115,#161116,#161117,
#161118,#161119,#161120,#161121,#161122,#161123,#161124,#161125,#161126,
#161127,#161128,#161129,#161130,#161131,#161132,#161133,#161134,#161135,
#161136,#161137,#161138,#161139,#161140,#161141,#161142,#161143,#161144,
#161145,#161146,#161147,#161148,#161149,#161150,#161151,#161152,#161153,
#161154,#161155,#161156,#161157,#161158,#161159,#161160,#161161,#161162,
#161163,#161164,#161165,#161166,#161167,#161168,#161169,#161170,#161171,
#161172,#161173,#161174,#161175,#161176,#161177,#161178,#161179,#161180,
#161181,#161182,#161183,#161184,#161185,#161186,#161187,#161188,#161189,
#161190,#161191,#161192,#161193,#161194,#161195,#161196,#161197,#161198,
#161199,#161200,#161201,#161202,#161203,#161204,#161205,#161206,#161207,
#161208,#161209,#161210,#161211,#161212,#161213,#161214,#161215,#161216,
#161217,#161218,#161219,#161220,#161221,#161222,#161223,#161224,#161225,
#161226,#161227,#161228,#161229,#161230,#161231,#161232,#161233,#161234,
#161235,#161236,#161237,#161238,#161239,#161240,#161241,#161242,#161243,
#161244,#161245,#161246,#161247,#161248,#161249,#161250,#161251,#161252,
#161253,#161254,#161255,#161256,#161257,#161258,#161259,#161260,#161261,
#161262,#161263,#161264,#161265,#161266,#161267,#161268,#161269,#161270,
#161271,#161272,#161273,#161274,#161275,#161276,#161277,#161278,#161279,
#161280,#161281,#161282,#161283,#161284,#161285,#161286,#161287,#161288,
#161289,#161290,#161291,#161292,#161293,#161294,#161295,#161296,#161297,
#161298,#161299,#161300,#161301,#161302,#161303,#161304,#161305,#161306,
#161307,#161308,#161309,#161310,#161311,#161312,#161313,#161314,#161315,
#161316,#161317,#161318,#161319,#161320,#161321,#161322,#161323,#161324,
#161325,#161326,#161327,#161328,#161329,#161330,#161331,#161332,#161333,
#161334,#161335,#161336,#161337,#161338,#161339,#161340,#161341,#161342,
#161343,#161344,#161345,#161346,#161347,#161348,#161349,#161350,#161351,
#161352,#161353,#161354,#161355,#161356,#161357,#161358,#161359,#161360,
#161361,#161362,#161363,#161364,#161365,#161366,#161367,#161368,#161369,
#161370,#161371,#161372,#161373,#161374,#161375,#161376,#161377,#161378,
#161379,#161380,#161381,#161382,#161383,#161384,#161385,#161386,#161387,
#161388,#161389,#161390,#161391,#161392,#161393,#161394,#161395,#161396,
#161397,#161398,#161399,#161400,#161401,#161402,#161403,#161404,#161405,
#161406,#161407,#161408,#161409,#161410,#161411,#161412,#161413,#161414,
#161415,#161416,#161417,#161418,#161419,#161420,#161421,#161422,#161423,
#161424,#161425,#161426,#161427,#161428,#161429,#161430,#161431,#161432,
#161433,#161434,#161435,#161436,#161437,#161438,#161439,#161440,#161441,
#161442,#161443,#161444,#161445,#161446,#161447,#161448,#161449,#161450,
#161451,#161452,#161453,#161454,#161455,#161456,#161457,#161458,#161459,
#161460,#161461,#161462,#161463,#161464,#161465,#161466,#161467,#161468,
#161469,#161470,#161471,#161472,#161473,#161474,#161475,#161476,#161477,
#161478,#161479,#161480,#161481,#161482,#161483,#161484,#161485,#161486,
#161487,#161488,#161489,#161490,#161491,#161492,#161493,#161494,#161495,
#161496,#161497,#161498,#161499,#161500,#161501,#161502,#161503,#161504,
#161505,#161506,#161507,#161508,#161509,#161510,#161511,#161512,#161513,
#161514,#161515,#161516,#161517,#161518,#161519,#161520,#161521,#161522,
#161523,#161524,#161525,#161526,#161527,#161528,#161529,#161530,#161531,
#161532,#161533,#161534,#161535,#161536,#161537,#161538,#161539,#161540,
#161541,#161542,#161543,#161544,#161545,#161546,#161547,#161548,#161549,
#161550,#161551,#161552,#161553,#161554,#161555,#161556,#161557,#161558,
#161559,#161560,#161561,#161562,#161563,#161564,#161565,#161566,#161567,
#161568,#161569,#161570,#161571,#161572,#161573,#161574,#161575,#161576,
#161577,#161578,#161579,#161580,#161581,#161582,#161583,#161584,#161585,
#161586,#161587,#161588,#161589,#161590,#161591,#161592,#161593,#161594,
#161595,#161596,#161597,#161598,#161599,#161600,#161601,#161602,#161603,
#161604,#161605,#161606,#161607,#161608,#161609,#161610,#161611,#161612,
#161613,#161614,#161615,#161616,#161617,#161618,#161619,#161620,#161621,
#161622,#161623,#161624,#161625,#161626,#161627,#161628,#161629,#161630,
#161631,#161632,#161633,#161634,#161635,#161636,#161637,#161638,#161639,
#161640,#161641,#161642,#161643,#161644,#161645,#161646,#161647,#161648,
#161649,#161650,#161651,#161652,#161653,#161654,#161655,#161656,#161657,
#161658,#161659,#161660,#161661,#161662,#161663,#161664,#161665,#161666,
#161667,#161668,#161669,#161670,#161671,#161672,#161673,#161674,#161675,
#161676,#161677,#161678,#161679,#161680,#161681,#161682,#161683,#161684,
#161685,#161686,#161687,#161688,#161689,#161690,#161691,#161692,#161693,
#161694,#161695,#161696,#161697,#161698,#161699,#161700,#161701,#161702,
#161703,#161704,#161705,#161706,#161707,#161708,#161709,#161710,#161711,
#161712,#161713,#161714,#161715,#161716,#161717,#161718,#161719,#161720,
#161721,#161722,#161723,#161724,#161725,#161726,#161727,#161728,#161729,
#161730,#161731,#161732,#161733,#161734,#161735,#161736,#161737,#161738,
#161739,#161740,#161741,#161742,#161743,#161744,#161745,#161746,#161747,
#161748,#161749,#161750,#161751,#161752,#161753,#161754,#161755,#161756,
#161757,#161758,#161759,#161760,#161761,#161762,#161763,#161764,#161765,
#161766,#161767,#161768,#161769,#161770,#161771,#161772,#161773,#161774,
#161775,#161776,#161777,#161778,#161779,#161780,#161781,#161782,#161783,
#161784,#161785,#161786,#161787,#161788,#161789,#161790,#161791,#161792,
#161793,#161794,#161795,#161796,#161797,#161798,#161799,#161800,#161801,
#161802,#161803,#161804,#161805,#161806,#161807,#161808,#161809,#161810,
#161811,#161812,#161813,#161814,#161815,#161816,#161817,#161818,#161819,
#161820,#161821,#161822,#161823,#161824,#161825,#161826,#161827,#161828,
#161829,#161830,#161831,#161832,#161833,#161834,#161835,#161836,#161837,
#161838,#161839,#161840,#161841,#161842,#161843,#161844,#161845,#161846,
#161847,#161848,#161849,#161850,#161851,#161852,#161853,#161854,#161855,
#161856,#161857,#161858,#161859,#161860,#161861,#161862,#161863,#161864,
#161865,#161866,#161867,#161868,#161869,#161870,#161871,#161872,#161873,
#161874,#161875,#161876,#161877,#161878,#161879,#161880,#161881,#161882,
#161883,#161884,#161885,#161886,#161887,#161888,#161889,#161890,#161891,
#161892,#161893,#161894,#161895,#161896,#161897,#161898,#161899,#161900,
#161901,#161902,#161903,#161904,#161905,#161906,#161907,#161908,#161909,
#161910,#161911,#161912,#161913,#161914,#161915,#161916,#161917,#161918,
#161919,#161920,#161921,#161922,#161923,#161924,#161925,#161926,#161927,
#161928,#161929,#161930,#161931,#161932,#161933,#161934,#161935,#161936,
#161937,#161938,#161939,#161940,#161941,#161942,#161943,#161944,#161945,
#161946,#161947,#161948,#161949,#161950,#161951,#161952,#161953,#161954,
#161955,#161956,#161957,#161958,#161959,#161960,#161961,#161962,#161963,
#161964,#161965,#161966,#161967,#161968,#161969,#161970,#161971,#161972,
#161973,#161974,#161975,#161976,#161977,#161978,#161979,#161980,#161981,
#161982,#161983,#161984,#161985,#161986,#161987,#161988,#161989,#161990,
#161991,#161992,#161993,#161994,#161995,#161996,#161997,#161998,#161999,
#162000,#162001,#162002,#162003,#162004,#162005,#162006,#162007,#162008,
#162009,#162010,#162011,#162012,#162013,#162014,#162015,#162016,#162017,
#162018,#162019,#162020,#162021,#162022,#162023,#162024,#162025,#162026,
#162027,#162028,#162029,#162030,#162031,#162032,#162033,#162034,#162035,
#162036,#162037,#162038,#162039,#162040,#162041,#162042,#162043,#162044,
#162045,#162046,#162047,#162048,#162049,#162050,#162051,#162052,#162053,
#162054,#162055,#162056,#162057,#162058,#162059,#162060,#162061,#162062,
#162063,#162064,#162065,#162066,#162067,#162068,#162069,#162070,#162071,
#162072,#162073,#162074,#162075,#162076,#162077,#162078,#162079,#162080,
#162081,#162082,#162083,#162084,#162085,#162086,#162087,#162088,#162089,
#162090,#162091,#162092,#162093,#162094,#162095,#162096,#162097,#162098,
#162099,#162100,#162101,#162102,#162103,#162104,#162105,#162106,#162107,
#162108,#162109,#162110,#162111,#162112,#162113,#162114,#162115,#162116,
#162117,#162118,#162119,#162120,#162121,#162122,#162123,#162124,#162125,
#162126,#162127,#162128,#162129,#162130,#162131,#162132,#162133,#162134,
#162135,#162136,#162137,#162138,#162139,#162140,#162141,#162142,#162143,
#162144,#162145,#162146,#162147,#162148,#162149,#162150,#162151,#162152,
#162153,#162154,#162155,#162156,#162157,#162158,#162159,#162160,#162161,
#162162,#162163,#162164,#162165,#162166,#162167,#162168,#162169,#162170,
#162171,#162172,#162173,#162174,#162175,#162176,#162177,#162178,#162179,
#162180,#162181,#162182,#162183,#162184,#162185,#162186,#162187,#162188,
#162189,#162190,#162191,#162192,#162193,#162194,#162195,#162196,#162197,
#162198,#162199,#162200,#162201,#162202,#162203,#162204,#162205,#162206,
#162207,#162208,#162209,#162210,#162211,#162212,#162213,#162214,#162215,
#162216,#162217,#162218,#162219,#162220,#162221,#162222,#162223,#162224,
#162225,#162226,#162227,#162228,#162229,#162230,#162231,#162232,#162233,
#162234,#162235,#162236,#162237,#162238,#162239,#162240,#162241,#162242,
#162243,#162244,#162245,#162246,#162247,#162248,#162249,#162250,#162251,
#162252,#162253,#162254,#162255,#162256,#162257,#162258,#162259,#162260,
#162261,#162262,#162263,#162264,#162265,#162266,#162267,#162268,#162269,
#162270,#162271,#162272,#162273,#162274,#162275,#162276,#162277,#162278,
#162279,#162280,#162281,#162282,#162283,#162284,#162285,#162286,#162287,
#162288,#162289,#162290,#162291,#162292,#162293,#162294,#162295,#162296,
#162297,#162298,#162299,#162300,#162301,#162302,#162303,#162304,#162305,
#162306,#162307,#162308,#162309,#162310,#162311,#162312,#162313,#162314,
#162315,#162316,#162317,#162318,#162319,#162320,#162321,#162322,#162323,
#162324,#162325,#162326,#162327,#162328,#162329,#162330,#162331,#162332,
#162333,#162334,#162335,#162336,#162337,#162338,#162339,#162340,#162341,
#162342,#162343,#162344,#162345,#162346,#162347,#162348,#162349,#162350,
#162351,#162352,#162353,#162354,#162355,#162356,#162357,#162358,#162359,
#162360,#162361,#162362,#162363,#162364,#162365,#162366,#162367,#162368,
#162369,#162370,#162371,#162372,#162373,#162374,#162375,#162376,#162377,
#162378,#162379,#162380,#162381,#162382,#162383,#162384,#162385,#162386,
#162387,#162388,#162389,#162390,#162391,#162392,#162393,#162394,#162395,
#162396,#162397,#162398,#162399,#162400,#162401,#162402,#162403,#162404,
#162405,#162406,#162407,#162408,#162409,#162410,#162411,#162412,#162413,
#162414,#162415,#162416,#162417,#162418,#162419,#162420,#162421,#162422,
#162423,#162424,#162425,#162426,#162427,#162428,#162429,#162430,#162431,
#162432,#162433,#162434,#162435,#162436,#162437,#162438,#162439,#162440,
#162441,#162442,#162443,#162444,#162445,#162446,#162447,#162448,#162449,
#162450,#162451,#162452,#162453,#162454,#162455,#162456,#162457,#162458,
#162459,#162460,#162461,#162462,#162463,#162464,#162465,#162466,#162467,
#162468,#162469,#162470,#162471,#162472,#162473,#162474,#162475,#162476,
#162477,#162478,#162479,#162480,#162481,#162482,#162483,#162484,#162485,
#162486,#162487,#162488,#162489,#162490,#162491,#162492,#162493,#162494,
#162495,#162496,#162497,#162498,#162499,#162500,#162501,#162502,#162503,
#162504,#162505,#162506,#162507,#162508,#162509,#162510,#162511,#162512,
#162513,#162514,#162515,#162516,#162517,#162518,#162519,#162520,#162521,
#162522,#162523,#162524,#162525,#162526,#162527,#162528,#162529,#162530,
#162531,#162532,#162533,#162534,#162535,#162536,#162537,#162538,#162539,
#162540,#162541,#162542,#162543,#162544,#162545,#162546,#162547,#162548,
#162549,#162550,#162551,#162552,#162553,#162554)),.UNSPECIFIED.,.F.,.F.,
 .F.)
B_SPLINE_SURFACE_WITH_KNOTS((2,2),(3,2,2,2,2,2,2,2,2,2,2,2,2,2,2,2,2,2,
2,2,2,2,2,2,2,2,2,2,2,2,2,2,2,2,2,2,2,2,2,2,2,2,2,2,2,2,2,2,2,2,2,2,2,2,
2,2,2,2,2,2,2,2,2,2,2,2,2,2,2,2,2,2,2,2,2,2,2,2,2,2,2,2,2,2,2,2,2,2,2,2,
2,2,2,2,2,2,2,2,2,2,2,2,2,2,2,2,2,2,2,2,2,2,2,2,2,2,2,2,2,2,2,2,2,2,2,2,
2,2,2,2,2,2,2,2,2,2,2,2,2,2,2,2,2,2,2,2,2,2,2,2,2,2,2,2,2,2,2,2,2,2,2,2,
2,2,2,2,2,2,2,2,2,2,2,2,2,2,2,2,2,2,2,2,2,2,2,2,2,2,2,2,2,2,2,2,2,2,2,2,
2,2,2,2,2,2,2,2,2,2,2,2,2,2,2,2,2,2,2,2,2,2,2,2,2,2,2,2,2,2,2,2,2,2,2,2,
2,2,2,2,2,2,2,2,2,2,2,2,2,2,2,2,2,2,2,2,2,2,2,2,2,2,2,2,2,2,2,2,2,2,2,2,
2,2,2,2,2,2,2,2,2,2,2,2,2,2,2,2,2,2,2,2,2,2,2,2,2,2,2,2,2,2,2,2,2,2,2,2,
2,2,2,2,2,2,2,2,2,2,2,2,2,2,2,2,2,2,2,2,2,2,2,2,2,2,2,2,2,2,2,2,2,2,2,2,
2,2,2,2,2,2,2,2,2,2,2,2,2,2,2,2,2,2,2,2,2,2,2,2,2,2,2,2,2,2,2,2,2,2,2,2,
2,2,2,2,2,2,2,2,2,2,2,2,2,2,2,2,2,2,2,2,2,2,2,2,2,2,2,2,2,2,2,2,2,2,2,2,
2,2,2,2,2,2,2,2,2,2,2,2,2,2,2,2,2,2,2,2,2,2,2,2,2,2,2,2,2,2,2,2,2,2,2,2,
2,2,2,2,2,2,2,2,2,2,2,2,2,2,2,2,2,2,2,2,2,2,2,2,2,2,2,2,2,2,2,2,2,2,2,2,
2,2,2,2,2,2,2,2,2,2,2,2,2,2,2,2,2,2,2,2,2,2,2,2,2,2,2,2,2,2,2,2,2,2,2,2,
2,2,2,2,2,2,2,2,2,2,2,2,2,2,2,2,2,2,2,2,2,2,2,2,2,2,2,2,2,2,2,2,2,2,2,2,
2,2,2,2,2,2,2,2,2,2,2,2,2,2,2,2,2,2,2,2,2,2,2,2,2,2,2,2,2,2,2,2,2,2,2,2,
2,2,2,2,2,2,2,2,2,2,2,2,2,2,2,2,2,2,2,2,2,2,2,2,2,2,2,2,2,2,2,2,2,2,2,2,
2,2,2,2,2,2,2,2,2,2,2,2,2,2,2,2,2,2,2,2,2,2,2,2,2,2,2,2,2,2,2,2,2,2,2,2,
2,2,2,2,2,2,2,2,2,2,2,2,2,2,2,2,2,2,2,2,2,2,2,2,2,2,2,2,2,2,2,2,2,2,2,2,
2,2,2,2,2,2,2,2,2,2,2,2,2,2,2,2,2,2,2,2,2,2,2,2,2,2,2,2,2,2,2,2,2,2,2,2,
2,2,2,2,2,2,2,2,2,2,2,2,2,2,2,2,2,2,2,2,2,2,2,2,2,2,2,2,2,2,2,2,2,2,2,2,
2,2,2,2,2,2,2,2,2,2,2,2,2,2,2,2,2,2,2,2,2,2,2,2,2,2,2,2,2,2,2,2,2,2,2,2,
2,2,2,2,2,2,2,2,2,2,2,2,2,2,2,2,2,2,2,2,2,2,2,2,2,2,2,2,2,2,2,2,2,2,2,2,
2,2,2,2,2,2,2,2,2,2,2,2,2,2,2,2,2,2,2,2,2,2,2,2,2,2,2,2,2,2,2,2,2,2,2,2,
2,2,2,2,2,2,2,2,2,2,2,2,2,2,2,2,2,2,2,2,2,2,2,2,2,2,2,2,2,2,2,2,2,2,2,2,
2,2,2,2,2,2,2,2,2,2,2,2,2,2,2,2,2,2,2,2,2,2,2,2,2,2,2,2,2,2,2,2,2,2,2,2,
2,2,2,2,2,2,2,2,2,2,2,2,2,2,2,2,2,2,2,2,2,2,2,2,2,2,2,2,2,2,2,2,2,2,2,2,
2,2,2,2,2,2,2,2,2,2,2,2,2,2,2,2,3),(0.,1.),(0.,0.000980392156862745,0.00196078431372549,
0.00294117647058824,0.00392156862745098,0.00490196078431373,0.00588235294117647,
0.00686274509803922,0.00784313725490196,0.00882352941176471,0.00980392156862745,
0.0107843137254902,0.0117647058823529,0.0127450980392157,0.0137254901960784,
0.0147058823529412,0.0156862745098039,0.0166666666666667,0.0176470588235294,
0.0186274509803922,0.0196078431372549,0.0205882352941176,0.0215686274509804,
0.0225490196078431,0.0235294117647059,0.0245098039215686,0.0254901960784314,
0.0264705882352941,0.0274509803921569,0.0284313725490196,0.0294117647058824,
0.0303921568627451,0.0313725490196078,0.0323529411764706,0.0333333333333333,
0.0343137254901961,0.0352941176470588,0.0362745098039216,0.0372549019607843,
0.0382352941176471,0.0392156862745098,0.0401960784313726,0.0411764705882353,
0.042156862745098,0.0431372549019608,0.0441176470588235,0.0450980392156863,
0.046078431372549,0.0470588235294118,0.0480392156862745,0.0490196078431373,
0.05,0.0509803921568627,0.0519607843137255,0.0529411764705882,0.053921568627451,
0.0549019607843137,0.0558823529411765,0.0568627450980392,0.057843137254902,
0.0588235294117647,0.0598039215686275,0.0607843137254902,0.0617647058823529,
0.0627450980392157,0.0637254901960784,0.0647058823529412,0.0656862745098039,
0.0666666666666667,0.0676470588235294,0.0686274509803922,0.0696078431372549,
0.0705882352941176,0.0715686274509804,0.0725490196078431,0.0735294117647059,
0.0745098039215686,0.0754901960784314,0.0764705882352941,0.0774509803921569,
0.0784313725490196,0.0794117647058823,0.0803921568627451,0.0813725490196078,
0.0823529411764706,0.0833333333333333,0.0843137254901961,0.0852941176470588,
0.0862745098039216,0.0872549019607843,0.0882352941176471,0.0892156862745098,
0.0901960784313725,0.0911764705882353,0.092156862745098,0.0931372549019608,
0.0941176470588235,0.0950980392156863,0.096078431372549,0.0970588235294118,
0.0980392156862745,0.0990196078431373,0.1,0.100980392156863,0.101960784313725,
0.102941176470588,0.103921568627451,0.104901960784314,0.105882352941176,
0.106862745098039,0.107843137254902,0.108823529411765,0.109803921568627,
0.11078431372549,0.111764705882353,0.112745098039216,0.113725490196078,
0.114705882352941,0.115686274509804,0.116666666666667,0.117647058823529,
0.118627450980392,0.119607843137255,0.120588235294118,0.12156862745098,
0.122549019607843,0.123529411764706,0.124509803921569,0.125490196078431,
0.126470588235294,0.127450980392157,0.12843137254902,0.129411764705882,
0.130392156862745,0.131372549019608,0.132352941176471,0.133333333333333,
0.134313725490196,0.135294117647059,0.136274509803922,0.137254901960784,
0.138235294117647,0.13921568627451,0.140196078431373,0.141176470588235,
0.142156862745098,0.143137254901961,0.144117647058824,0.145098039215686,
0.146078431372549,0.147058823529412,0.148039215686275,0.149019607843137,
0.15,0.150980392156863,0.151960784313725,0.152941176470588,0.153921568627451,
0.154901960784314,0.155882352941176,0.156862745098039,0.157843137254902,
0.158823529411765,0.159803921568627,0.16078431372549,0.161764705882353,
0.162745098039216,0.163725490196078,0.164705882352941,0.165686274509804,
0.166666666666667,0.167647058823529,0.168627450980392,0.169607843137255,
0.170588235294118,0.17156862745098,0.172549019607843,0.173529411764706,
0.174509803921569,0.175490196078431,0.176470588235294,0.177450980392157,
0.17843137254902,0.179411764705882,0.180392156862745,0.181372549019608,
0.182352941176471,0.183333333333333,0.184313725490196,0.185294117647059,
0.186274509803922,0.187254901960784,0.188235294117647,0.18921568627451,
0.190196078431373,0.191176470588235,0.192156862745098,0.193137254901961,
0.194117647058824,0.195098039215686,0.196078431372549,0.197058823529412,
0.198039215686275,0.199019607843137,0.2,0.200980392156863,0.201960784313725,
0.202941176470588,0.203921568627451,0.204901960784314,0.205882352941176,
0.206862745098039,0.207843137254902,0.208823529411765,0.209803921568627,
0.21078431372549,0.211764705882353,0.212745098039216,0.213725490196078,
0.214705882352941,0.215686274509804,0.216666666666667,0.217647058823529,
0.218627450980392,0.219607843137255,0.220588235294118,0.22156862745098,
0.222549019607843,0.223529411764706,0.224509803921569,0.225490196078431,
0.226470588235294,0.227450980392157,0.22843137254902,0.229411764705882,
0.230392156862745,0.231372549019608,0.232352941176471,0.233333333333333,
0.234313725490196,0.235294117647059,0.236274509803922,0.237254901960784,
0.238235294117647,0.23921568627451,0.240196078431373,0.241176470588235,
0.242156862745098,0.243137254901961,0.244117647058824,0.245098039215686,
0.246078431372549,0.247058823529412,0.248039215686275,0.249019607843137,
0.25,0.250980392156863,0.251960784313725,0.252941176470588,0.253921568627451,
0.254901960784314,0.255882352941176,0.256862745098039,0.257843137254902,
0.258823529411765,0.259803921568627,0.26078431372549,0.261764705882353,
0.262745098039216,0.263725490196078,0.264705882352941,0.265686274509804,
0.266666666666667,0.267647058823529,0.268627450980392,0.269607843137255,
0.270588235294118,0.27156862745098,0.272549019607843,0.273529411764706,
0.274509803921569,0.275490196078431,0.276470588235294,0.277450980392157,
0.27843137254902,0.279411764705882,0.280392156862745,0.281372549019608,
0.282352941176471,0.283333333333333,0.284313725490196,0.285294117647059,
0.286274509803922,0.287254901960784,0.288235294117647,0.28921568627451,
0.290196078431373,0.291176470588235,0.292156862745098,0.293137254901961,
0.294117647058824,0.295098039215686,0.296078431372549,0.297058823529412,
0.298039215686275,0.299019607843137,0.3,0.300980392156863,0.301960784313725,
0.302941176470588,0.303921568627451,0.304901960784314,0.305882352941176,
0.306862745098039,0.307843137254902,0.308823529411765,0.309803921568627,
0.31078431372549,0.311764705882353,0.312745098039216,0.313725490196078,
0.314705882352941,0.315686274509804,0.316666666666667,0.317647058823529,
0.318627450980392,0.319607843137255,0.320588235294118,0.32156862745098,
0.322549019607843,0.323529411764706,0.324509803921569,0.325490196078431,
0.326470588235294,0.327450980392157,0.32843137254902,0.329411764705882,
0.330392156862745,0.331372549019608,0.332352941176471,0.333333333333333,
0.334313725490196,0.335294117647059,0.336274509803922,0.337254901960784,
0.338235294117647,0.33921568627451,0.340196078431373,0.341176470588235,
0.342156862745098,0.343137254901961,0.344117647058824,0.345098039215686,
0.346078431372549,0.347058823529412,0.348039215686274,0.349019607843137,
0.35,0.350980392156863,0.351960784313726,0.352941176470588,0.353921568627451,
0.354901960784314,0.355882352941176,0.356862745098039,0.357843137254902,
0.358823529411765,0.359803921568627,0.36078431372549,0.361764705882353,
0.362745098039216,0.363725490196078,0.364705882352941,0.365686274509804,
0.366666666666667,0.367647058823529,0.368627450980392,0.369607843137255,
0.370588235294118,0.37156862745098,0.372549019607843,0.373529411764706,
0.374509803921569,0.375490196078431,0.376470588235294,0.377450980392157,
0.37843137254902,0.379411764705882,0.380392156862745,0.381372549019608,
0.382352941176471,0.383333333333333,0.384313725490196,0.385294117647059,
0.386274509803922,0.387254901960784,0.388235294117647,0.38921568627451,
0.390196078431373,0.391176470588235,0.392156862745098,0.393137254901961,
0.394117647058824,0.395098039215686,0.396078431372549,0.397058823529412,
0.398039215686274,0.399019607843137,0.4,0.400980392156863,0.401960784313726,
0.402941176470588,0.403921568627451,0.404901960784314,0.405882352941176,
0.406862745098039,0.407843137254902,0.408823529411765,0.409803921568627,
0.41078431372549,0.411764705882353,0.412745098039216,0.413725490196078,
0.414705882352941,0.415686274509804,0.416666666666667,0.417647058823529,
0.418627450980392,0.419607843137255,0.420588235294118,0.42156862745098,
0.422549019607843,0.423529411764706,0.424509803921569,0.425490196078431,
0.426470588235294,0.427450980392157,0.42843137254902,0.429411764705882,
0.430392156862745,0.431372549019608,0.432352941176471,0.433333333333333,
0.434313725490196,0.435294117647059,0.436274509803922,0.437254901960784,
0.438235294117647,0.43921568627451,0.440196078431373,0.441176470588235,
0.442156862745098,0.443137254901961,0.444117647058824,0.445098039215686,
0.446078431372549,0.447058823529412,0.448039215686275,0.449019607843137,
0.45,0.450980392156863,0.451960784313725,0.452941176470588,0.453921568627451,
0.454901960784314,0.455882352941176,0.456862745098039,0.457843137254902,
0.458823529411765,0.459803921568627,0.46078431372549,0.461764705882353,
0.462745098039216,0.463725490196078,0.464705882352941,0.465686274509804,
0.466666666666667,0.467647058823529,0.468627450980392,0.469607843137255,
0.470588235294118,0.47156862745098,0.472549019607843,0.473529411764706,
0.474509803921569,0.475490196078431,0.476470588235294,0.477450980392157,
0.47843137254902,0.479411764705882,0.480392156862745,0.481372549019608,
0.482352941176471,0.483333333333333,0.484313725490196,0.485294117647059,
0.486274509803922,0.487254901960784,0.488235294117647,0.48921568627451,
0.490196078431373,0.491176470588235,0.492156862745098,0.493137254901961,
0.494117647058824,0.495098039215686,0.496078431372549,0.497058823529412,
0.498039215686275,0.499019607843137,0.5,0.500980392156863,0.501960784313725,
0.502941176470588,0.503921568627451,0.504901960784314,0.505882352941176,
0.506862745098039,0.507843137254902,0.508823529411765,0.509803921568627,
0.51078431372549,0.511764705882353,0.512745098039216,0.513725490196078,
0.514705882352941,0.515686274509804,0.516666666666667,0.517647058823529,
0.518627450980392,0.519607843137255,0.520588235294118,0.52156862745098,
0.522549019607843,0.523529411764706,0.524509803921569,0.525490196078431,
0.526470588235294,0.527450980392157,0.52843137254902,0.529411764705882,
0.530392156862745,0.531372549019608,0.532352941176471,0.533333333333333,
0.534313725490196,0.535294117647059,0.536274509803922,0.537254901960784,
0.538235294117647,0.53921568627451,0.540196078431373,0.541176470588235,
0.542156862745098,0.543137254901961,0.544117647058823,0.545098039215686,
0.546078431372549,0.547058823529412,0.548039215686275,0.549019607843137,
0.55,0.550980392156863,0.551960784313726,0.552941176470588,0.553921568627451,
0.554901960784314,0.555882352941176,0.556862745098039,0.557843137254902,
0.558823529411765,0.559803921568627,0.56078431372549,0.561764705882353,
0.562745098039216,0.563725490196078,0.564705882352941,0.565686274509804,
0.566666666666667,0.567647058823529,0.568627450980392,0.569607843137255,
0.570588235294118,0.57156862745098,0.572549019607843,0.573529411764706,
0.574509803921569,0.575490196078431,0.576470588235294,0.577450980392157,
0.57843137254902,0.579411764705882,0.580392156862745,0.581372549019608,
0.582352941176471,0.583333333333333,0.584313725490196,0.585294117647059,
0.586274509803922,0.587254901960784,0.588235294117647,0.58921568627451,
0.590196078431373,0.591176470588235,0.592156862745098,0.593137254901961,
0.594117647058824,0.595098039215686,0.596078431372549,0.597058823529412,
0.598039215686274,0.599019607843137,0.6,0.600980392156863,0.601960784313725,
0.602941176470588,0.603921568627451,0.604901960784314,0.605882352941176,
0.606862745098039,0.607843137254902,0.608823529411765,0.609803921568628,
0.61078431372549,0.611764705882353,0.612745098039216,0.613725490196078,
0.614705882352941,0.615686274509804,0.616666666666667,0.617647058823529,
0.618627450980392,0.619607843137255,0.620588235294118,0.62156862745098,
0.622549019607843,0.623529411764706,0.624509803921569,0.625490196078431,
0.626470588235294,0.627450980392157,0.62843137254902,0.629411764705882,
0.630392156862745,0.631372549019608,0.632352941176471,0.633333333333333,
0.634313725490196,0.635294117647059,0.636274509803922,0.637254901960784,
0.638235294117647,0.63921568627451,0.640196078431372,0.641176470588235,
0.642156862745098,0.643137254901961,0.644117647058824,0.645098039215686,
0.646078431372549,0.647058823529412,0.648039215686275,0.649019607843137,
0.65,0.650980392156863,0.651960784313726,0.652941176470588,0.653921568627451,
0.654901960784314,0.655882352941176,0.656862745098039,0.657843137254902,
0.658823529411765,0.659803921568627,0.66078431372549,0.661764705882353,
0.662745098039216,0.663725490196078,0.664705882352941,0.665686274509804,
0.666666666666667,0.667647058823529,0.668627450980392,0.669607843137255,
0.670588235294118,0.67156862745098,0.672549019607843,0.673529411764706,
0.674509803921569,0.675490196078431,0.676470588235294,0.677450980392157,
0.67843137254902,0.679411764705882,0.680392156862745,0.681372549019608,
0.682352941176471,0.683333333333333,0.684313725490196,0.685294117647059,
0.686274509803922,0.687254901960784,0.688235294117647,0.68921568627451,
0.690196078431373,0.691176470588235,0.692156862745098,0.693137254901961,
0.694117647058824,0.695098039215686,0.696078431372549,0.697058823529412,
0.698039215686274,0.699019607843137,0.7,0.700980392156863,0.701960784313725,
0.702941176470588,0.703921568627451,0.704901960784314,0.705882352941177,
0.706862745098039,0.707843137254902,0.708823529411765,0.709803921568627,
0.71078431372549,0.711764705882353,0.712745098039216,0.713725490196078,
0.714705882352941,0.715686274509804,0.716666666666667,0.717647058823529,
0.718627450980392,0.719607843137255,0.720588235294118,0.72156862745098,
0.722549019607843,0.723529411764706,0.724509803921569,0.725490196078431,
0.726470588235294,0.727450980392157,0.72843137254902,0.729411764705882,
0.730392156862745,0.731372549019608,0.732352941176471,0.733333333333333,
0.734313725490196,0.735294117647059,0.736274509803922,0.737254901960784,
0.738235294117647,0.73921568627451,0.740196078431373,0.741176470588235,
0.742156862745098,0.743137254901961,0.744117647058824,0.745098039215686,
0.746078431372549,0.747058823529412,0.748039215686275,0.749019607843137,
0.75,0.750980392156863,0.751960784313725,0.752941176470588,0.753921568627451,
0.754901960784314,0.755882352941176,0.756862745098039,0.757843137254902,
0.758823529411765,0.759803921568627,0.76078431372549,0.761764705882353,
0.762745098039216,0.763725490196078,0.764705882352941,0.765686274509804,
0.766666666666667,0.767647058823529,0.768627450980392,0.769607843137255,
0.770588235294118,0.77156862745098,0.772549019607843,0.773529411764706,
0.774509803921569,0.775490196078431,0.776470588235294,0.777450980392157,
0.77843137254902,0.779411764705882,0.780392156862745,0.781372549019608,
0.782352941176471,0.783333333333333,0.784313725490196,0.785294117647059,
0.786274509803922,0.787254901960784,0.788235294117647,0.78921568627451,
0.790196078431373,0.791176470588235,0.792156862745098,0.793137254901961,
0.794117647058823,0.795098039215686,0.796078431372549,0.797058823529412,
0.798039215686275,0.799019607843137,0.8,0.800980392156863,0.801960784313726,
0.802941176470588,0.803921568627451,0.804901960784314,0.805882352941176,
0.806862745098039,0.807843137254902,0.808823529411765,0.809803921568627,
0.81078431372549,0.811764705882353,0.812745098039216,0.813725490196078,
0.814705882352941,0.815686274509804,0.816666666666667,0.817647058823529,
0.818627450980392,0.819607843137255,0.820588235294118,0.82156862745098,
0.822549019607843,0.823529411764706,0.824509803921569,0.825490196078431,
0.826470588235294,0.827450980392157,0.82843137254902,0.829411764705882,
0.830392156862745,0.831372549019608,0.832352941176471,0.833333333333333,
0.834313725490196,0.835294117647059,0.836274509803922,0.837254901960784,
0.838235294117647,0.83921568627451,0.840196078431373,0.841176470588235,
0.842156862745098,0.843137254901961,0.844117647058824,0.845098039215686,
0.846078431372549,0.847058823529412,0.848039215686274,0.849019607843137,
0.85,0.850980392156863,0.851960784313725,0.852941176470588,0.853921568627451,
0.854901960784314,0.855882352941176,0.856862745098039,0.857843137254902,
0.858823529411765,0.859803921568628,0.86078431372549,0.861764705882353,
0.862745098039216,0.863725490196078,0.864705882352941,0.865686274509804,
0.866666666666667,0.867647058823529,0.868627450980392,0.869607843137255,
0.870588235294118,0.87156862745098,0.872549019607843,0.873529411764706,
0.874509803921569,0.875490196078431,0.876470588235294,0.877450980392157,
0.87843137254902,0.879411764705882,0.880392156862745,0.881372549019608,
0.882352941176471,0.883333333333333,0.884313725490196,0.885294117647059,
0.886274509803922,0.887254901960784,0.888235294117647,0.88921568627451,
0.890196078431372,0.891176470588235,0.892156862745098,0.893137254901961,
0.894117647058824,0.895098039215686,0.896078431372549,0.897058823529412,
0.898039215686275,0.899019607843137,0.9,0.900980392156863,0.901960784313726,
0.902941176470588,0.903921568627451,0.904901960784314,0.905882352941176,
0.906862745098039,0.907843137254902,0.908823529411765,0.909803921568627,
0.91078431372549,0.911764705882353,0.912745098039216,0.913725490196078,
0.914705882352941,0.915686274509804,0.916666666666667,0.917647058823529,
0.918627450980392,0.919607843137255,0.920588235294118,0.92156862745098,
0.922549019607843,0.923529411764706,0.924509803921569,0.925490196078431,
0.926470588235294,0.927450980392157,0.92843137254902,0.929411764705882,
0.930392156862745,0.931372549019608,0.932352941176471,0.933333333333333,
0.934313725490196,0.935294117647059,0.936274509803922,0.937254901960784,
0.938235294117647,0.93921568627451,0.940196078431373,0.941176470588235,
0.942156862745098,0.943137254901961,0.944117647058824,0.945098039215686,
0.946078431372549,0.947058823529412,0.948039215686274,0.949019607843137,
0.95,0.950980392156863,0.951960784313725,0.952941176470588,0.953921568627451,
0.954901960784314,0.955882352941177,0.956862745098039,0.957843137254902,
0.958823529411765,0.959803921568627,0.96078431372549,0.961764705882353,
0.962745098039216,0.963725490196078,0.964705882352941,0.965686274509804,
0.966666666666667,0.967647058823529,0.968627450980392,0.969607843137255,
0.970588235294118,0.97156862745098,0.972549019607843,0.973529411764706,
0.974509803921569,0.975490196078431,0.976470588235294,0.977450980392157,
0.97843137254902,0.979411764705882,0.980392156862745,0.981372549019608,
0.982352941176471,0.983333333333333,0.984313725490196,0.985294117647059,
0.985937314000278),.UNSPECIFIED.)
GEOMETRIC_REPRESENTATION_ITEM()
RATIONAL_B_SPLINE_SURFACE(((1.,0.995734176295034,1.,0.995734176295034,1.,
0.995734176295034,1.,0.995734176295034,1.,0.995734176295034,1.,0.995734176295034,
1.,0.995734176295034,1.,0.995734176295034,1.,0.995734176295034,1.,0.995734176295034,
1.,0.995734176295034,1.,0.995734176295034,1.,0.995734176295034,1.,0.995734176295034,
1.,0.995734176295034,1.,0.995734176295034,1.,0.995734176295034,1.,0.995734176295034,
1.,0.995734176295034,1.,0.995734176295034,1.,0.995734176295034,1.,0.995734176295034,
1.,0.995734176295034,1.,0.995734176295034,1.,0.995734176295034,1.,0.995734176295034,
1.,0.995734176295034,1.,0.995734176295034,1.,0.995734176295034,1.,0.995734176295034,
1.,0.995734176295034,1.,0.995734176295034,1.,0.995734176295034,1.,0.995734176295034,
1.,0.995734176295034,1.,0.995734176295034,1.,0.995734176295034,1.,0.995734176295034,
1.,0.995734176295034,1.,0.995734176295034,1.,0.995734176295034,1.,0.995734176295034,
1.,0.995734176295034,1.,0.995734176295034,1.,0.995734176295034,1.,0.995734176295034,
1.,0.995734176295034,1.,0.995734176295034,1.,0.995734176295034,1.,0.995734176295034,
1.,0.995734176295034,1.,0.995734176295034,1.,0.995734176295034,1.,0.995734176295034,
1.,0.995734176295034,1.,0.995734176295034,1.,0.995734176295034,1.,0.995734176295034,
1.,0.995734176295034,1.,0.995734176295034,1.,0.995734176295034,1.,0.995734176295034,
1.,0.995734176295034,1.,0.995734176295034,1.,0.995734176295034,1.,0.995734176295034,
1.,0.995734176295034,1.,0.995734176295034,1.,0.995734176295034,1.,0.995734176295034,
1.,0.995734176295034,1.,0.995734176295034,1.,0.995734176295034,1.,0.995734176295034,
1.,0.995734176295034,1.,0.995734176295034,1.,0.995734176295034,1.,0.995734176295034,
1.,0.995734176295034,1.,0.995734176295034,1.,0.995734176295034,1.,0.995734176295034,
1.,0.995734176295034,1.,0.995734176295034,1.,0.995734176295034,1.,0.995734176295034,
1.,0.995734176295034,1.,0.995734176295034,1.,0.995734176295034,1.,0.995734176295034,
1.,0.995734176295034,1.,0.995734176295034,1.,0.995734176295034,1.,0.995734176295034,
1.,0.995734176295034,1.,0.995734176295034,1.,0.995734176295034,1.,0.995734176295034,
1.,0.995734176295034,1.,0.995734176295034,1.,0.995734176295034,1.,0.995734176295034,
1.,0.995734176295034,1.,0.995734176295034,1.,0.995734176295034,1.,0.995734176295034,
1.,0.995734176295034,1.,0.995734176295034,1.,0.995734176295034,1.,0.995734176295034,
1.,0.995734176295034,1.,0.995734176295034,1.,0.995734176295034,1.,0.995734176295034,
1.,0.995734176295034,1.,0.995734176295034,1.,0.995734176295034,1.,0.995734176295034,
1.,0.995734176295034,1.,0.995734176295034,1.,0.995734176295034,1.,0.995734176295034,
1.,0.995734176295034,1.,0.995734176295034,1.,0.995734176295034,1.,0.995734176295034,
1.,0.995734176295034,1.,0.995734176295034,1.,0.995734176295034,1.,0.995734176295034,
1.,0.995734176295034,1.,0.995734176295034,1.,0.995734176295034,1.,0.995734176295034,
1.,0.995734176295034,1.,0.995734176295034,1.,0.995734176295034,1.,0.995734176295034,
1.,0.995734176295034,1.,0.995734176295034,1.,0.995734176295034,1.,0.995734176295034,
1.,0.995734176295034,1.,0.995734176295034,1.,0.995734176295034,1.,0.995734176295034,
1.,0.995734176295034,1.,0.995734176295034,1.,0.995734176295034,1.,0.995734176295034,
1.,0.995734176295034,1.,0.995734176295034,1.,0.995734176295034,1.,0.995734176295034,
1.,0.995734176295034,1.,0.995734176295034,1.,0.995734176295034,1.,0.995734176295034,
1.,0.995734176295034,1.,0.995734176295034,1.,0.995734176295034,1.,0.995734176295034,
1.,0.995734176295034,1.,0.995734176295034,1.,0.995734176295034,1.,0.995734176295034,
1.,0.995734176295034,1.,0.995734176295034,1.,0.995734176295034,1.,0.995734176295034,
1.,0.995734176295034,1.,0.995734176295034,1.,0.995734176295034,1.,0.995734176295034,
1.,0.995734176295034,1.,0.995734176295034,1.,0.995734176295034,1.,0.995734176295034,
1.,0.995734176295034,1.,0.995734176295034,1.,0.995734176295034,1.,0.995734176295034,
1.,0.995734176295034,1.,0.995734176295034,1.,0.995734176295034,1.,0.995734176295034,
1.,0.995734176295034,1.,0.995734176295034,1.,0.995734176295034,1.,0.995734176295034,
1.,0.995734176295034,1.,0.995734176295034,1.,0.995734176295034,1.,0.995734176295034,
1.,0.995734176295034,1.,0.995734176295034,1.,0.995734176295034,1.,0.995734176295034,
1.,0.995734176295034,1.,0.995734176295034,1.,0.995734176295034,1.,0.995734176295034,
1.,0.995734176295034,1.,0.995734176295034,1.,0.995734176295034,1.,0.995734176295034,
1.,0.995734176295034,1.,0.995734176295034,1.,0.995734176295034,1.,0.995734176295034,
1.,0.995734176295034,1.,0.995734176295034,1.,0.995734176295034,1.,0.995734176295034,
1.,0.995734176295034,1.,0.995734176295034,1.,0.995734176295034,1.,0.995734176295034,
1.,0.995734176295034,1.,0.995734176295034,1.,0.995734176295034,1.,0.995734176295034,
1.,0.995734176295034,1.,0.995734176295034,1.,0.995734176295034,1.,0.995734176295034,
1.,0.995734176295034,1.,0.995734176295034,1.,0.995734176295034,1.,0.995734176295034,
1.,0.995734176295034,1.,0.995734176295034,1.,0.995734176295034,1.,0.995734176295034,
1.,0.995734176295034,1.,0.995734176295034,1.,0.995734176295034,1.,0.995734176295034,
1.,0.995734176295034,1.,0.995734176295034,1.,0.995734176295034,1.,0.995734176295034,
1.,0.995734176295034,1.,0.995734176295034,1.,0.995734176295034,1.,0.995734176295034,
1.,0.995734176295034,1.,0.995734176295034,1.,0.995734176295034,1.,0.995734176295034,
1.,0.995734176295034,1.,0.995734176295034,1.,0.995734176295034,1.,0.995734176295034,
1.,0.995734176295034,1.,0.995734176295034,1.,0.995734176295034,1.,0.995734176295034,
1.,0.995734176295034,1.,0.995734176295034,1.,0.995734176295034,1.,0.995734176295034,
1.,0.995734176295034,1.,0.995734176295034,1.,0.995734176295034,1.,0.995734176295034,
1.,0.995734176295034,1.,0.995734176295034,1.,0.995734176295034,1.,0.995734176295034,
1.,0.995734176295034,1.,0.995734176295034,1.,0.995734176295034,1.,0.995734176295034,
1.,0.995734176295034,1.,0.995734176295034,1.,0.995734176295034,1.,0.995734176295034,
1.,0.995734176295034,1.,0.995734176295034,1.,0.995734176295034,1.,0.995734176295034,
1.,0.995734176295034,1.,0.995734176295034,1.,0.995734176295034,1.,0.995734176295034,
1.,0.995734176295034,1.,0.995734176295034,1.,0.995734176295034,1.,0.995734176295034,
1.,0.995734176295034,1.,0.995734176295034,1.,0.995734176295034,1.,0.995734176295034,
1.,0.995734176295034,1.,0.995734176295034,1.,0.995734176295034,1.,0.995734176295034,
1.,0.995734176295034,1.,0.995734176295034,1.,0.995734176295034,1.,0.995734176295034,
1.,0.995734176295034,1.,0.995734176295034,1.,0.995734176295034,1.,0.995734176295034,
1.,0.995734176295034,1.,0.995734176295034,1.,0.995734176295034,1.,0.995734176295034,
1.,0.995734176295034,1.,0.995734176295034,1.,0.995734176295034,1.,0.995734176295034,
1.,0.995734176295034,1.,0.995734176295034,1.,0.995734176295034,1.,0.995734176295034,
1.,0.995734176295034,1.,0.995734176295034,1.,0.995734176295034,1.,0.995734176295034,
1.,0.995734176295034,1.,0.995734176295034,1.,0.995734176295034,1.,0.995734176295034,
1.,0.995734176295034,1.,0.995734176295034,1.,0.995734176295034,1.,0.995734176295034,
1.,0.995734176295034,1.,0.995734176295034,1.,0.995734176295034,1.,0.995734176295034,
1.,0.995734176295034,1.,0.995734176295034,1.,0.995734176295034,1.,0.995734176295034,
1.,0.995734176295034,1.,0.995734176295034,1.,0.995734176295034,1.,0.995734176295034,
1.,0.995734176295034,1.,0.995734176295034,1.,0.995734176295034,1.,0.995734176295034,
1.,0.995734176295034,1.,0.995734176295034,1.,0.995734176295034,1.,0.995734176295034,
1.,0.995734176295034,1.,0.995734176295034,1.,0.995734176295034,1.,0.995734176295034,
1.,0.995734176295034,1.,0.995734176295034,1.,0.995734176295034,1.,0.995734176295034,
1.,0.995734176295034,1.,0.995734176295034,1.,0.995734176295034,1.,0.995734176295034,
1.,0.995734176295034,1.,0.995734176295034,1.,0.995734176295034,1.,0.995734176295034,
1.,0.995734176295034,1.,0.995734176295034,1.,0.995734176295034,1.,0.995734176295034,
1.,0.995734176295034,1.,0.995734176295034,1.,0.995734176295034,1.,0.995734176295034,
1.,0.995734176295034,1.,0.995734176295034,1.,0.995734176295034,1.,0.995734176295034,
1.,0.995734176295034,1.,0.995734176295034,1.,0.995734176295034,1.,0.995734176295034,
1.,0.995734176295034,1.,0.995734176295034,1.,0.995734176295034,1.,0.995734176295034,
1.,0.995734176295034,1.,0.995734176295034,1.,0.995734176295034,1.,0.995734176295034,
1.,0.995734176295034,1.,0.995734176295034,1.,0.995734176295034,1.,0.995734176295034,
1.,0.995734176295034,1.,0.995734176295034,1.,0.995734176295034,1.,0.995734176295034,
1.,0.995734176295034,1.,0.995734176295034,1.,0.995734176295034,1.,0.995734176295034,
1.,0.995734176295034,1.,0.995734176295034,1.,0.995734176295034,1.,0.995734176295034,
1.,0.995734176295034,1.,0.995734176295034,1.,0.995734176295034,1.,0.995734176295034,
1.,0.995734176295034,1.,0.995734176295034,1.,0.995734176295034,1.,0.995734176295034,
1.,0.995734176295034,1.,0.995734176295034,1.,0.995734176295034,1.,0.995734176295034,
1.,0.995734176295034,1.,0.995734176295034,1.,0.995734176295034,1.,0.995734176295034,
1.,0.995734176295034,1.,0.995734176295034,1.,0.995734176295034,1.,0.995734176295034,
1.,0.995734176295034,1.,0.995734176295034,1.,0.995734176295034,1.,0.995734176295034,
1.,0.995734176295034,1.,0.995734176295034,1.,0.995734176295034,1.,0.995734176295034,
1.,0.995734176295034,1.,0.995734176295034,1.,0.995734176295034,1.,0.995734176295034,
1.,0.995734176295034,1.,0.995734176295034,1.,0.995734176295034,1.,0.995734176295034,
1.,0.995734176295034,1.,0.995734176295034,1.,0.995734176295034,1.,0.995734176295034,
1.,0.995734176295034,1.,0.995734176295034,1.,0.995734176295034,1.,0.995734176295034,
1.,0.995734176295034,1.,0.995734176295034,1.,0.995734176295034,1.,0.995734176295034,
1.,0.995734176295034,1.,0.995734176295034,1.,0.995734176295034,1.,0.995734176295034,
1.,0.995734176295034,1.,0.995734176295034,1.,0.995734176295034,1.,0.995734176295034,
1.,0.995734176295034,1.,0.995734176295034,1.,0.995734176295034,1.,0.995734176295034,
1.,0.995734176295034,1.,0.995734176295034,1.,0.995734176295034,1.,0.995734176295034,
1.,0.995734176295034,1.,0.995734176295034,1.,0.995734176295034,1.,0.995734176295034,
1.,0.995734176295034,1.,0.995734176295034,1.,0.995734176295034,1.,0.995734176295034,
1.,0.995734176295034,1.,0.995734176295034,1.,0.995734176295034,1.,0.995734176295034,
1.,0.995734176295034,1.,0.995734176295034,1.,0.995734176295034,1.,0.995734176295034,
1.,0.995734176295034,1.,0.995734176295034,1.,0.995734176295034,1.,0.995734176295034,
1.,0.995734176295034,1.,0.995734176295034,1.,0.995734176295034,1.,0.995734176295034,
1.,0.995734176295034,1.,0.995734176295034,1.,0.995734176295034,1.,0.995734176295034,
1.,0.995734176295034,1.,0.995734176295034,1.,0.995734176295034,1.,0.995734176295034,
1.,0.995734176295034,1.,0.995734176295034,1.,0.995734176295034,1.,0.995734176295034,
1.,0.995734176295034,1.,0.995734176295034,1.,0.995734176295034,1.,0.995734176295034,
1.,0.995734176295034,1.,0.995734176295034,1.,0.995734176295034,1.,0.995734176295034,
1.,0.995734176295034,1.,0.995734176295034,1.,0.995734176295034,1.,0.995734176295034,
1.,0.995734176295034,1.,0.995734176295034,1.,0.995734176295034,1.,0.995734176295034,
1.,0.995734176295034,1.,0.995734176295034,1.,0.995734176295034,1.,0.995734176295034,
1.,0.995734176295034,1.,0.995734176295034,1.,0.995734176295034,1.,0.995734176295034,
1.,0.995734176295034,1.,0.995734176295034,1.,0.995734176295034,1.,0.995734176295034,
1.,0.995734176295034,1.,0.995734176295034,1.,0.995734176295034,1.,0.995734176295034,
1.,0.995734176295034,1.,0.995734176295034,1.,0.995734176295034,1.,0.995734176295034,
1.,0.995734176295034,1.,0.995734176295034,1.,0.995734176295034,1.,0.995734176295034,
1.,0.995734176295034,1.,0.995734176295034,1.,0.995734176295034,1.,0.995734176295034,
1.,0.995734176295034,1.,0.995734176295034,1.,0.995734176295034,1.,0.995734176295034,
1.,0.995734176295034,1.,0.995734176295034,1.,0.995734176295034,1.,0.995734176295034,
1.,0.995734176295034,1.,0.995734176295034,1.,0.995734176295034,1.,0.995734176295034,
1.,0.995734176295034,1.,0.995734176295034,1.,0.995734176295034,1.,0.995734176295034,
1.,0.995734176295034,1.,0.995734176295034,1.,0.995734176295034,1.,0.995734176295034,
1.,0.995734176295034,1.,0.995734176295034,1.,0.995734176295034,1.,0.995734176295034,
1.,0.995734176295034,1.,0.995734176295034,1.,0.995734176295034,1.,0.995734176295034,
1.,0.995734176295034,1.,0.995734176295034,1.,0.995734176295034,1.,0.995734176295034,
1.,0.995734176295034,1.,0.995734176295034,1.,0.995734176295034,1.,0.995734176295034,
1.,0.995734176295034,1.,0.995734176295034,1.,0.995734176295034,1.,0.995734176295034,
1.,0.995734176295034,1.,0.995734176295034,1.,0.995734176295034,1.,0.995734176295034,
1.,0.995734176295034,1.,0.995734176295034,1.,0.995734176295034,1.,0.995734176295034,
1.,0.995734176295034,1.,0.995734176295034,1.,0.995734176295034,1.,0.995734176295034,
1.,0.995734176295034,1.,0.995734176295034,1.,0.995734176295034,1.,0.995734176295034,
1.,0.995734176295034,1.,0.995734176295034,1.,0.995734176295034,1.,0.995734176295034,
1.,0.995734176295034,1.,0.995734176295034,1.,0.995734176295034,1.,0.995734176295034,
1.,0.995734176295034,1.,0.995734176295034,1.,0.995734176295034,1.,0.995734176295034,
1.,0.995734176295034,1.,0.995734176295034,1.,0.995734176295034,1.,0.995734176295034,
1.,0.995734176295034,1.,0.995734176295034,1.,0.995734176295034,1.,0.995734176295034,
1.,0.995734176295034,1.,0.995734176295034,1.,0.995734176295034,1.,0.995734176295034,
1.,0.995734176295034,1.,0.995734176295034,1.,0.995734176295034,1.,0.995734176295034,
1.,0.995734176295034,1.,0.995734176295034,1.,0.995734176295034,1.,0.995734176295034,
1.,0.995734176295034,1.,0.995734176295034,1.,0.995734176295034,1.,0.995734176295034,
1.,0.995734176295034,1.,0.995734176295034,1.,0.995734176295034,1.,0.995734176295034,
1.,0.995734176295034,1.,0.995734176295034,1.,0.995734176295034,1.,0.995734176295034,
1.,0.995734176295034,1.,0.995734176295034,1.,0.995734176295034,1.,0.995734176295034,
1.,0.995734176295034,1.,0.995734176295034,1.,0.995734176295034,1.,0.995734176295034,
1.,0.995734176295034,1.,0.995734176295034,1.,0.995734176295034,1.,0.995734176295034,
1.,0.995734176295034,1.,0.995734176295034,1.,0.995734176295034,1.,0.995734176295034,
1.,0.995734176295034,1.,0.995734176295034,1.,0.995734176295034,1.,0.995734176295034,
1.,0.995734176295034,1.,0.995734176295034,1.,0.995734176295034,1.,0.995734176295034,
1.,0.995734176295034,1.,0.995734176295034,1.,0.995734176295034,1.,0.995734176295034,
1.,0.995734176295034,1.,0.995734176295034,1.,0.995734176295034,1.,0.995734176295034,
1.,0.995734176295034,1.,0.995734176295034,1.,0.995734176295034,1.,0.995734176295034,
1.,0.995734176295034,1.,0.995734176295034,1.,0.995734176295034,1.,0.995734176295034,
1.,0.995734176295034,1.,0.995734176295034,1.,0.995734176295034,1.,0.995734176295034,
1.,0.995734176295034,1.,0.995734176295034,1.,0.995734176295034,1.,0.995734176295034,
1.,0.995734176295034,1.,0.995734176295034,1.,0.995734176295034,1.,0.995734176295034,
1.,0.995734176295034,1.,0.995734176295034,1.,0.995734176295034,1.,0.995734176295034,
1.,0.995734176295034,1.,0.995734176295034,1.,0.995734176295034,1.,0.995734176295034,
1.,0.995734176295034,1.,0.995734176295034,1.,0.995734176295034,1.,0.995734176295034,
1.,0.995734176295034,1.,0.995734176295034,1.,0.995734176295034,1.,0.995734176295034,
1.,0.995734176295034,1.,0.995734176295034,1.,0.995734176295034,1.,0.995734176295034,
1.,0.995734176295034,1.,0.995734176295034,1.,0.995734176295034,1.,0.995734176295034,
1.,0.995734176295034,1.,0.995734176295034,1.,0.995734176295034,1.,0.995734176295034,
1.,0.995734176295034,1.,0.995734176295034,1.,0.995734176295034,1.,0.995734176295034,
1.,0.995734176295034,1.,0.995734176295034,1.,0.995734176295034,1.,0.995734176295034,
1.,0.995734176295034,1.,0.995734176295034,1.,0.995734176295034,1.,0.995734176295034,
1.,0.995734176295034,1.,0.995734176295034,1.,0.995734176295034,1.,0.995734176295034,
1.,0.995734176295034,1.,0.995734176295034,1.,0.995734176295034,1.,0.995734176295034,
1.,0.995734176295034,1.,0.995734176295034,1.,0.995734176295034,1.,0.995734176295034,
1.,0.995734176295034,1.,0.995734176295034,1.,0.995734176295034,1.,0.995734176295034,
1.,0.995734176295034,1.,0.995734176295034,1.,0.995734176295034,1.,0.995734176295034,
1.,0.995734176295034,1.,0.995734176295034,1.,0.995734176295034,1.,0.995734176295034,
1.,0.995734176295034,1.,0.995734176295034,1.,0.995734176295034,1.,0.995734176295034,
1.,0.995734176295034,1.,0.995734176295034,1.,0.995734176295034,1.,0.995734176295034,
1.,0.995734176295034,1.,0.995734176295034,1.,0.995734176295034,1.,0.995734176295034,
1.,0.995734176295034,1.,0.995734176295034,1.,0.995734176295034,1.,0.995734176295034,
1.,0.995734176295034,1.,0.995734176295034,1.,0.995734176295034,1.,0.995734176295034,
1.,0.995734176295034,1.,0.995734176295034,1.,0.995734176295034,1.,0.995734176295034,
1.,0.995734176295034,1.,0.995734176295034,1.,0.995734176295034,1.,0.995734176295034,
1.,0.995734176295034,1.,0.995734176295034,1.,0.995734176295034,1.,0.995734176295034,
1.,0.995734176295034,1.,0.995734176295034,1.,0.995734176295034,1.,0.995734176295034,
1.,0.995734176295034,1.,0.995734176295034,1.,0.995734176295034,1.,0.995734176295034,
1.,0.995734176295034,1.,0.995734176295034,1.,0.995734176295034,1.,0.995734176295034,
1.,0.995734176295034,1.,0.995734176295034,1.,0.995734176295034,1.,0.995734176295034,
1.,0.995734176295034,1.,0.995734176295034,1.,0.995734176295034,1.,0.995734176295034,
1.,0.995734176295034,1.,0.995734176295034,1.,0.995734176295034,1.,0.995734176295034,
1.,0.995734176295034,1.,0.995734176295034,1.,0.995734176295034,1.,0.995734176295034,
1.,0.995734176295034,1.,0.995734176295034,1.,0.995734176295034,1.,0.995734176295034,
1.,0.995734176295034,1.,0.995734176295034,1.,0.995734176295034,1.,0.995734176295034,
1.,0.995734176295034,1.,0.995734176295034,1.,0.995734176295034,1.,0.995734176295034,
1.,0.995734176295034,1.,0.995734176295034,1.,0.995734176295034,1.,0.995734176295034,
1.,0.995734176295034,1.,0.995734176295034,1.,0.995734176295034,1.,0.995734176295034,
1.,0.995734176295034,1.,0.995734176295034,1.,0.995734176295034,1.,0.995734176295034,
1.,0.995734176295034,1.,0.995734176295034,1.,0.995734176295034,1.,0.995734176295034,
1.,0.995734176295034,1.,0.995734176295034,1.,0.995734176295034,1.,0.995734176295034,
1.,0.995734176295034,1.,0.995734176295034,1.,0.995734176295034,1.,0.995734176295034,
1.,0.995734176295034,1.,0.995734176295034,1.,0.995734176295034,1.,0.995734176295034,
1.,0.995734176295034,1.,0.995734176295034,1.,0.995734176295034,1.,0.995734176295034,
1.,0.995734176295034,1.,0.995734176295034,1.,0.995734176295034,1.,0.995734176295034,
1.,0.995734176295034,1.,0.995734176295034,1.,0.995734176295034,1.,0.995734176295034,
1.,0.995734176295034,1.,0.995734176295034,1.,0.995734176295034,1.,0.995734176295034,
1.,0.995734176295034,1.,0.995734176295034,1.,0.995734176295034,1.,0.995734176295034,
1.,0.995734176295034,1.,0.995734176295034,1.,0.995734176295034,1.,0.995734176295034,
1.,0.995734176295034,1.,0.995734176295034,1.,0.995734176295034,1.,0.995734176295034,
1.,0.995734176295034,1.,0.995734176295034,1.,0.995734176295034,1.,0.995734176295034,
1.,0.995734176295034,1.,0.995734176295034,1.,0.995734176295034,1.,0.995734176295034,
1.,0.995734176295034,1.,0.995734176295034,1.,0.995734176295034,1.,0.995734176295034,
1.,0.995734176295034,1.,0.995734176295034,1.,0.995734176295034,1.,0.995734176295034,
1.,0.995734176295034,1.,0.995734176295034,1.,0.995734176295034,1.,0.995734176295034,
1.,0.995734176295034,1.,0.995734176295034,1.,0.995734176295034,1.,0.995734176295034,
1.,0.995734176295034,1.,0.995734176295034,1.,0.995734176295034,1.,0.995734176295034,
1.,0.995734176295034,1.,0.995734176295034,1.,0.995734176295034,1.,0.995734176295034,
1.,0.995734176295034,1.,0.995734176295034,1.,0.995734176295034,1.,0.995734176295034,
1.,0.995734176295034,1.,0.995734176295034,1.,0.995734176295034,1.,0.995734176295034,
1.,0.995734176295034,1.,0.995734176295034,1.,0.995734176295034,1.,0.995734176295034,
1.,0.995734176295034,1.,0.995734176295034,1.,0.995734176295034,1.,0.995734176295034,
1.,0.995734176295034,1.,0.995734176295034,1.,0.995734176295034,1.,0.995734176295034,
1.,0.995734176295034,1.,0.995734176295034,1.,0.995734176295034,1.,0.995734176295034,
1.,0.995734176295034,1.,0.995734176295034,1.,0.995734176295034,1.,0.995734176295034,
1.,0.995734176295034,1.,0.995734176295034,1.,0.995734176295034,1.,0.995734176295034,
1.,0.995734176295034,1.,0.995734176295034,1.,0.995734176295034,1.,0.995734176295034,
1.,0.995734176295034,1.,0.995734176295034,1.,0.995734176295034,1.,0.995734176295034,
1.,0.995734176295034,1.,0.995734176295034,1.,0.995734176295034,1.,0.995734176295034,
1.,0.995734176295034,1.,0.995734176295034,1.,0.995734176295034,1.,0.995734176295034,
1.,0.995734176295034,1.,0.995734176295034,1.,0.995734176295034,1.,0.995734176295034,
1.,0.995734176295034,1.,0.995734176295034,1.,0.995734176295034,1.,0.995734176295034,
1.,0.995734176295034,1.,0.995734176295034,1.,0.995734176295034,1.,0.995734176295034,
1.,0.995734176295034,1.,0.995734176295034,1.,0.995734176295034,1.,0.995734176295034,
1.,0.995734176295034,1.,0.995734176295034,1.,0.995734176295034,1.,0.995734176295034,
1.,0.995734176295034,1.,0.995734176295034,1.,0.995734176295034,1.,0.995734176295034,
1.,0.995734176295034,1.,0.995734176295034,1.,0.995734176295034,1.,0.995734176295034,
1.,0.995734176295034,1.,0.995734176295034,1.,0.995734176295034,1.,0.997201362504479,
0.998074874808407),(1.,0.995734176295034,1.,0.995734176295034,1.,0.995734176295034,
1.,0.995734176295034,1.,0.995734176295034,1.,0.995734176295034,1.,0.995734176295034,
1.,0.995734176295034,1.,0.995734176295034,1.,0.995734176295034,1.,0.995734176295034,
1.,0.995734176295034,1.,0.995734176295034,1.,0.995734176295034,1.,0.995734176295034,
1.,0.995734176295034,1.,0.995734176295034,1.,0.995734176295034,1.,0.995734176295034,
1.,0.995734176295034,1.,0.995734176295034,1.,0.995734176295034,1.,0.995734176295034,
1.,0.995734176295034,1.,0.995734176295034,1.,0.995734176295034,1.,0.995734176295034,
1.,0.995734176295034,1.,0.995734176295034,1.,0.995734176295034,1.,0.995734176295034,
1.,0.995734176295034,1.,0.995734176295034,1.,0.995734176295034,1.,0.995734176295034,
1.,0.995734176295034,1.,0.995734176295034,1.,0.995734176295034,1.,0.995734176295034,
1.,0.995734176295034,1.,0.995734176295034,1.,0.995734176295034,1.,0.995734176295034,
1.,0.995734176295034,1.,0.995734176295034,1.,0.995734176295034,1.,0.995734176295034,
1.,0.995734176295034,1.,0.995734176295034,1.,0.995734176295034,1.,0.995734176295034,
1.,0.995734176295034,1.,0.995734176295034,1.,0.995734176295034,1.,0.995734176295034,
1.,0.995734176295034,1.,0.995734176295034,1.,0.995734176295034,1.,0.995734176295034,
1.,0.995734176295034,1.,0.995734176295034,1.,0.995734176295034,1.,0.995734176295034,
1.,0.995734176295034,1.,0.995734176295034,1.,0.995734176295034,1.,0.995734176295034,
1.,0.995734176295034,1.,0.995734176295034,1.,0.995734176295034,1.,0.995734176295034,
1.,0.995734176295034,1.,0.995734176295034,1.,0.995734176295034,1.,0.995734176295034,
1.,0.995734176295034,1.,0.995734176295034,1.,0.995734176295034,1.,0.995734176295034,
1.,0.995734176295034,1.,0.995734176295034,1.,0.995734176295034,1.,0.995734176295034,
1.,0.995734176295034,1.,0.995734176295034,1.,0.995734176295034,1.,0.995734176295034,
1.,0.995734176295034,1.,0.995734176295034,1.,0.995734176295034,1.,0.995734176295034,
1.,0.995734176295034,1.,0.995734176295034,1.,0.995734176295034,1.,0.995734176295034,
1.,0.995734176295034,1.,0.995734176295034,1.,0.995734176295034,1.,0.995734176295034,
1.,0.995734176295034,1.,0.995734176295034,1.,0.995734176295034,1.,0.995734176295034,
1.,0.995734176295034,1.,0.995734176295034,1.,0.995734176295034,1.,0.995734176295034,
1.,0.995734176295034,1.,0.995734176295034,1.,0.995734176295034,1.,0.995734176295034,
1.,0.995734176295034,1.,0.995734176295034,1.,0.995734176295034,1.,0.995734176295034,
1.,0.995734176295034,1.,0.995734176295034,1.,0.995734176295034,1.,0.995734176295034,
1.,0.995734176295034,1.,0.995734176295034,1.,0.995734176295034,1.,0.995734176295034,
1.,0.995734176295034,1.,0.995734176295034,1.,0.995734176295034,1.,0.995734176295034,
1.,0.995734176295034,1.,0.995734176295034,1.,0.995734176295034,1.,0.995734176295034,
1.,0.995734176295034,1.,0.995734176295034,1.,0.995734176295034,1.,0.995734176295034,
1.,0.995734176295034,1.,0.995734176295034,1.,0.995734176295034,1.,0.995734176295034,
1.,0.995734176295034,1.,0.995734176295034,1.,0.995734176295034,1.,0.995734176295034,
1.,0.995734176295034,1.,0.995734176295034,1.,0.995734176295034,1.,0.995734176295034,
1.,0.995734176295034,1.,0.995734176295034,1.,0.995734176295034,1.,0.995734176295034,
1.,0.995734176295034,1.,0.995734176295034,1.,0.995734176295034,1.,0.995734176295034,
1.,0.995734176295034,1.,0.995734176295034,1.,0.995734176295034,1.,0.995734176295034,
1.,0.995734176295034,1.,0.995734176295034,1.,0.995734176295034,1.,0.995734176295034,
1.,0.995734176295034,1.,0.995734176295034,1.,0.995734176295034,1.,0.995734176295034,
1.,0.995734176295034,1.,0.995734176295034,1.,0.995734176295034,1.,0.995734176295034,
1.,0.995734176295034,1.,0.995734176295034,1.,0.995734176295034,1.,0.995734176295034,
1.,0.995734176295034,1.,0.995734176295034,1.,0.995734176295034,1.,0.995734176295034,
1.,0.995734176295034,1.,0.995734176295034,1.,0.995734176295034,1.,0.995734176295034,
1.,0.995734176295034,1.,0.995734176295034,1.,0.995734176295034,1.,0.995734176295034,
1.,0.995734176295034,1.,0.995734176295034,1.,0.995734176295034,1.,0.995734176295034,
1.,0.995734176295034,1.,0.995734176295034,1.,0.995734176295034,1.,0.995734176295034,
1.,0.995734176295034,1.,0.995734176295034,1.,0.995734176295034,1.,0.995734176295034,
1.,0.995734176295034,1.,0.995734176295034,1.,0.995734176295034,1.,0.995734176295034,
1.,0.995734176295034,1.,0.995734176295034,1.,0.995734176295034,1.,0.995734176295034,
1.,0.995734176295034,1.,0.995734176295034,1.,0.995734176295034,1.,0.995734176295034,
1.,0.995734176295034,1.,0.995734176295034,1.,0.995734176295034,1.,0.995734176295034,
1.,0.995734176295034,1.,0.995734176295034,1.,0.995734176295034,1.,0.995734176295034,
1.,0.995734176295034,1.,0.995734176295034,1.,0.995734176295034,1.,0.995734176295034,
1.,0.995734176295034,1.,0.995734176295034,1.,0.995734176295034,1.,0.995734176295034,
1.,0.995734176295034,1.,0.995734176295034,1.,0.995734176295034,1.,0.995734176295034,
1.,0.995734176295034,1.,0.995734176295034,1.,0.995734176295034,1.,0.995734176295034,
1.,0.995734176295034,1.,0.995734176295034,1.,0.995734176295034,1.,0.995734176295034,
1.,0.995734176295034,1.,0.995734176295034,1.,0.995734176295034,1.,0.995734176295034,
1.,0.995734176295034,1.,0.995734176295034,1.,0.995734176295034,1.,0.995734176295034,
1.,0.995734176295034,1.,0.995734176295034,1.,0.995734176295034,1.,0.995734176295034,
1.,0.995734176295034,1.,0.995734176295034,1.,0.995734176295034,1.,0.995734176295034,
1.,0.995734176295034,1.,0.995734176295034,1.,0.995734176295034,1.,0.995734176295034,
1.,0.995734176295034,1.,0.995734176295034,1.,0.995734176295034,1.,0.995734176295034,
1.,0.995734176295034,1.,0.995734176295034,1.,0.995734176295034,1.,0.995734176295034,
1.,0.995734176295034,1.,0.995734176295034,1.,0.995734176295034,1.,0.995734176295034,
1.,0.995734176295034,1.,0.995734176295034,1.,0.995734176295034,1.,0.995734176295034,
1.,0.995734176295034,1.,0.995734176295034,1.,0.995734176295034,1.,0.995734176295034,
1.,0.995734176295034,1.,0.995734176295034,1.,0.995734176295034,1.,0.995734176295034,
1.,0.995734176295034,1.,0.995734176295034,1.,0.995734176295034,1.,0.995734176295034,
1.,0.995734176295034,1.,0.995734176295034,1.,0.995734176295034,1.,0.995734176295034,
1.,0.995734176295034,1.,0.995734176295034,1.,0.995734176295034,1.,0.995734176295034,
1.,0.995734176295034,1.,0.995734176295034,1.,0.995734176295034,1.,0.995734176295034,
1.,0.995734176295034,1.,0.995734176295034,1.,0.995734176295034,1.,0.995734176295034,
1.,0.995734176295034,1.,0.995734176295034,1.,0.995734176295034,1.,0.995734176295034,
1.,0.995734176295034,1.,0.995734176295034,1.,0.995734176295034,1.,0.995734176295034,
1.,0.995734176295034,1.,0.995734176295034,1.,0.995734176295034,1.,0.995734176295034,
1.,0.995734176295034,1.,0.995734176295034,1.,0.995734176295034,1.,0.995734176295034,
1.,0.995734176295034,1.,0.995734176295034,1.,0.995734176295034,1.,0.995734176295034,
1.,0.995734176295034,1.,0.995734176295034,1.,0.995734176295034,1.,0.995734176295034,
1.,0.995734176295034,1.,0.995734176295034,1.,0.995734176295034,1.,0.995734176295034,
1.,0.995734176295034,1.,0.995734176295034,1.,0.995734176295034,1.,0.995734176295034,
1.,0.995734176295034,1.,0.995734176295034,1.,0.995734176295034,1.,0.995734176295034,
1.,0.995734176295034,1.,0.995734176295034,1.,0.995734176295034,1.,0.995734176295034,
1.,0.995734176295034,1.,0.995734176295034,1.,0.995734176295034,1.,0.995734176295034,
1.,0.995734176295034,1.,0.995734176295034,1.,0.995734176295034,1.,0.995734176295034,
1.,0.995734176295034,1.,0.995734176295034,1.,0.995734176295034,1.,0.995734176295034,
1.,0.995734176295034,1.,0.995734176295034,1.,0.995734176295034,1.,0.995734176295034,
1.,0.995734176295034,1.,0.995734176295034,1.,0.995734176295034,1.,0.995734176295034,
1.,0.995734176295034,1.,0.995734176295034,1.,0.995734176295034,1.,0.995734176295034,
1.,0.995734176295034,1.,0.995734176295034,1.,0.995734176295034,1.,0.995734176295034,
1.,0.995734176295034,1.,0.995734176295034,1.,0.995734176295034,1.,0.995734176295034,
1.,0.995734176295034,1.,0.995734176295034,1.,0.995734176295034,1.,0.995734176295034,
1.,0.995734176295034,1.,0.995734176295034,1.,0.995734176295034,1.,0.995734176295034,
1.,0.995734176295034,1.,0.995734176295034,1.,0.995734176295034,1.,0.995734176295034,
1.,0.995734176295034,1.,0.995734176295034,1.,0.995734176295034,1.,0.995734176295034,
1.,0.995734176295034,1.,0.995734176295034,1.,0.995734176295034,1.,0.995734176295034,
1.,0.995734176295034,1.,0.995734176295034,1.,0.995734176295034,1.,0.995734176295034,
1.,0.995734176295034,1.,0.995734176295034,1.,0.995734176295034,1.,0.995734176295034,
1.,0.995734176295034,1.,0.995734176295034,1.,0.995734176295034,1.,0.995734176295034,
1.,0.995734176295034,1.,0.995734176295034,1.,0.995734176295034,1.,0.995734176295034,
1.,0.995734176295034,1.,0.995734176295034,1.,0.995734176295034,1.,0.995734176295034,
1.,0.995734176295034,1.,0.995734176295034,1.,0.995734176295034,1.,0.995734176295034,
1.,0.995734176295034,1.,0.995734176295034,1.,0.995734176295034,1.,0.995734176295034,
1.,0.995734176295034,1.,0.995734176295034,1.,0.995734176295034,1.,0.995734176295034,
1.,0.995734176295034,1.,0.995734176295034,1.,0.995734176295034,1.,0.995734176295034,
1.,0.995734176295034,1.,0.995734176295034,1.,0.995734176295034,1.,0.995734176295034,
1.,0.995734176295034,1.,0.995734176295034,1.,0.995734176295034,1.,0.995734176295034,
1.,0.995734176295034,1.,0.995734176295034,1.,0.995734176295034,1.,0.995734176295034,
1.,0.995734176295034,1.,0.995734176295034,1.,0.995734176295034,1.,0.995734176295034,
1.,0.995734176295034,1.,0.995734176295034,1.,0.995734176295034,1.,0.995734176295034,
1.,0.995734176295034,1.,0.995734176295034,1.,0.995734176295034,1.,0.995734176295034,
1.,0.995734176295034,1.,0.995734176295034,1.,0.995734176295034,1.,0.995734176295034,
1.,0.995734176295034,1.,0.995734176295034,1.,0.995734176295034,1.,0.995734176295034,
1.,0.995734176295034,1.,0.995734176295034,1.,0.995734176295034,1.,0.995734176295034,
1.,0.995734176295034,1.,0.995734176295034,1.,0.995734176295034,1.,0.995734176295034,
1.,0.995734176295034,1.,0.995734176295034,1.,0.995734176295034,1.,0.995734176295034,
1.,0.995734176295034,1.,0.995734176295034,1.,0.995734176295034,1.,0.995734176295034,
1.,0.995734176295034,1.,0.995734176295034,1.,0.995734176295034,1.,0.995734176295034,
1.,0.995734176295034,1.,0.995734176295034,1.,0.995734176295034,1.,0.995734176295034,
1.,0.995734176295034,1.,0.995734176295034,1.,0.995734176295034,1.,0.995734176295034,
1.,0.995734176295034,1.,0.995734176295034,1.,0.995734176295034,1.,0.995734176295034,
1.,0.995734176295034,1.,0.995734176295034,1.,0.995734176295034,1.,0.995734176295034,
1.,0.995734176295034,1.,0.995734176295034,1.,0.995734176295034,1.,0.995734176295034,
1.,0.995734176295034,1.,0.995734176295034,1.,0.995734176295034,1.,0.995734176295034,
1.,0.995734176295034,1.,0.995734176295034,1.,0.995734176295034,1.,0.995734176295034,
1.,0.995734176295034,1.,0.995734176295034,1.,0.995734176295034,1.,0.995734176295034,
1.,0.995734176295034,1.,0.995734176295034,1.,0.995734176295034,1.,0.995734176295034,
1.,0.995734176295034,1.,0.995734176295034,1.,0.995734176295034,1.,0.995734176295034,
1.,0.995734176295034,1.,0.995734176295034,1.,0.995734176295034,1.,0.995734176295034,
1.,0.995734176295034,1.,0.995734176295034,1.,0.995734176295034,1.,0.995734176295034,
1.,0.995734176295034,1.,0.995734176295034,1.,0.995734176295034,1.,0.995734176295034,
1.,0.995734176295034,1.,0.995734176295034,1.,0.995734176295034,1.,0.995734176295034,
1.,0.995734176295034,1.,0.995734176295034,1.,0.995734176295034,1.,0.995734176295034,
1.,0.995734176295034,1.,0.995734176295034,1.,0.995734176295034,1.,0.995734176295034,
1.,0.995734176295034,1.,0.995734176295034,1.,0.995734176295034,1.,0.995734176295034,
1.,0.995734176295034,1.,0.995734176295034,1.,0.995734176295034,1.,0.995734176295034,
1.,0.995734176295034,1.,0.995734176295034,1.,0.995734176295034,1.,0.995734176295034,
1.,0.995734176295034,1.,0.995734176295034,1.,0.995734176295034,1.,0.995734176295034,
1.,0.995734176295034,1.,0.995734176295034,1.,0.995734176295034,1.,0.995734176295034,
1.,0.995734176295034,1.,0.995734176295034,1.,0.995734176295034,1.,0.995734176295034,
1.,0.995734176295034,1.,0.995734176295034,1.,0.995734176295034,1.,0.995734176295034,
1.,0.995734176295034,1.,0.995734176295034,1.,0.995734176295034,1.,0.995734176295034,
1.,0.995734176295034,1.,0.995734176295034,1.,0.995734176295034,1.,0.995734176295034,
1.,0.995734176295034,1.,0.995734176295034,1.,0.995734176295034,1.,0.995734176295034,
1.,0.995734176295034,1.,0.995734176295034,1.,0.995734176295034,1.,0.995734176295034,
1.,0.995734176295034,1.,0.995734176295034,1.,0.995734176295034,1.,0.995734176295034,
1.,0.995734176295034,1.,0.995734176295034,1.,0.995734176295034,1.,0.995734176295034,
1.,0.995734176295034,1.,0.995734176295034,1.,0.995734176295034,1.,0.995734176295034,
1.,0.995734176295034,1.,0.995734176295034,1.,0.995734176295034,1.,0.995734176295034,
1.,0.995734176295034,1.,0.995734176295034,1.,0.995734176295034,1.,0.995734176295034,
1.,0.995734176295034,1.,0.995734176295034,1.,0.995734176295034,1.,0.995734176295034,
1.,0.995734176295034,1.,0.995734176295034,1.,0.995734176295034,1.,0.995734176295034,
1.,0.995734176295034,1.,0.995734176295034,1.,0.995734176295034,1.,0.995734176295034,
1.,0.995734176295034,1.,0.995734176295034,1.,0.995734176295034,1.,0.995734176295034,
1.,0.995734176295034,1.,0.995734176295034,1.,0.995734176295034,1.,0.995734176295034,
1.,0.995734176295034,1.,0.995734176295034,1.,0.995734176295034,1.,0.995734176295034,
1.,0.995734176295034,1.,0.995734176295034,1.,0.995734176295034,1.,0.995734176295034,
1.,0.995734176295034,1.,0.995734176295034,1.,0.995734176295034,1.,0.995734176295034,
1.,0.995734176295034,1.,0.995734176295034,1.,0.995734176295034,1.,0.995734176295034,
1.,0.995734176295034,1.,0.995734176295034,1.,0.995734176295034,1.,0.995734176295034,
1.,0.995734176295034,1.,0.995734176295034,1.,0.995734176295034,1.,0.995734176295034,
1.,0.995734176295034,1.,0.995734176295034,1.,0.995734176295034,1.,0.995734176295034,
1.,0.995734176295034,1.,0.995734176295034,1.,0.995734176295034,1.,0.995734176295034,
1.,0.995734176295034,1.,0.995734176295034,1.,0.995734176295034,1.,0.995734176295034,
1.,0.995734176295034,1.,0.995734176295034,1.,0.995734176295034,1.,0.995734176295034,
1.,0.995734176295034,1.,0.995734176295034,1.,0.995734176295034,1.,0.995734176295034,
1.,0.995734176295034,1.,0.995734176295034,1.,0.995734176295034,1.,0.995734176295034,
1.,0.995734176295034,1.,0.995734176295034,1.,0.995734176295034,1.,0.995734176295034,
1.,0.995734176295034,1.,0.995734176295034,1.,0.995734176295034,1.,0.995734176295034,
1.,0.995734176295034,1.,0.995734176295034,1.,0.995734176295034,1.,0.995734176295034,
1.,0.995734176295034,1.,0.995734176295034,1.,0.995734176295034,1.,0.995734176295034,
1.,0.995734176295034,1.,0.995734176295034,1.,0.995734176295034,1.,0.995734176295034,
1.,0.995734176295034,1.,0.995734176295034,1.,0.995734176295034,1.,0.995734176295034,
1.,0.995734176295034,1.,0.995734176295034,1.,0.995734176295034,1.,0.995734176295034,
1.,0.995734176295034,1.,0.995734176295034,1.,0.995734176295034,1.,0.995734176295034,
1.,0.995734176295034,1.,0.995734176295034,1.,0.995734176295034,1.,0.995734176295034,
1.,0.995734176295034,1.,0.995734176295034,1.,0.995734176295034,1.,0.995734176295034,
1.,0.995734176295034,1.,0.995734176295034,1.,0.995734176295034,1.,0.995734176295034,
1.,0.995734176295034,1.,0.995734176295034,1.,0.995734176295034,1.,0.995734176295034,
1.,0.995734176295034,1.,0.995734176295034,1.,0.995734176295034,1.,0.995734176295034,
1.,0.995734176295034,1.,0.995734176295034,1.,0.995734176295034,1.,0.995734176295034,
1.,0.995734176295034,1.,0.995734176295034,1.,0.995734176295034,1.,0.995734176295034,
1.,0.995734176295034,1.,0.995734176295034,1.,0.995734176295034,1.,0.995734176295034,
1.,0.995734176295034,1.,0.995734176295034,1.,0.995734176295034,1.,0.995734176295034,
1.,0.995734176295034,1.,0.995734176295034,1.,0.995734176295034,1.,0.995734176295034,
1.,0.995734176295034,1.,0.995734176295034,1.,0.995734176295034,1.,0.995734176295034,
1.,0.995734176295034,1.,0.995734176295034,1.,0.995734176295034,1.,0.995734176295034,
1.,0.995734176295034,1.,0.995734176295034,1.,0.995734176295034,1.,0.995734176295034,
1.,0.995734176295034,1.,0.995734176295034,1.,0.995734176295034,1.,0.995734176295034,
1.,0.995734176295034,1.,0.995734176295034,1.,0.995734176295034,1.,0.995734176295034,
1.,0.995734176295034,1.,0.995734176295034,1.,0.995734176295034,1.,0.995734176295034,
1.,0.995734176295034,1.,0.995734176295034,1.,0.995734176295034,1.,0.995734176295034,
1.,0.995734176295034,1.,0.995734176295034,1.,0.995734176295034,1.,0.995734176295034,
1.,0.995734176295034,1.,0.995734176295034,1.,0.995734176295034,1.,0.995734176295034,
1.,0.995734176295034,1.,0.995734176295034,1.,0.995734176295034,1.,0.995734176295034,
1.,0.995734176295034,1.,0.995734176295034,1.,0.995734176295034,1.,0.995734176295034,
1.,0.995734176295034,1.,0.995734176295034,1.,0.995734176295034,1.,0.995734176295034,
1.,0.995734176295034,1.,0.995734176295034,1.,0.995734176295034,1.,0.995734176295034,
1.,0.995734176295034,1.,0.995734176295034,1.,0.995734176295034,1.,0.995734176295034,
1.,0.995734176295034,1.,0.995734176295034,1.,0.995734176295034,1.,0.995734176295034,
1.,0.995734176295034,1.,0.995734176295034,1.,0.995734176295034,1.,0.995734176295034,
1.,0.995734176295034,1.,0.995734176295034,1.,0.995734176295034,1.,0.995734176295034,
1.,0.995734176295034,1.,0.995734176295034,1.,0.995734176295034,1.,0.995734176295034,
1.,0.995734176295034,1.,0.995734176295034,1.,0.995734176295034,1.,0.995734176295034,
1.,0.995734176295034,1.,0.995734176295034,1.,0.995734176295034,1.,0.995734176295034,
1.,0.995734176295034,1.,0.995734176295034,1.,0.995734176295034,1.,0.995734176295034,
1.,0.995734176295034,1.,0.995734176295034,1.,0.995734176295034,1.,0.995734176295034,
1.,0.995734176295034,1.,0.995734176295034,1.,0.995734176295034,1.,0.995734176295034,
1.,0.995734176295034,1.,0.995734176295034,1.,0.995734176295034,1.,0.995734176295034,
1.,0.995734176295034,1.,0.995734176295034,1.,0.995734176295034,1.,0.995734176295034,
1.,0.995734176295034,1.,0.995734176295034,1.,0.995734176295034,1.,0.995734176295034,
1.,0.995734176295034,1.,0.995734176295034,1.,0.995734176295034,1.,0.995734176295034,
1.,0.995734176295034,1.,0.995734176295034,1.,0.995734176295034,1.,0.995734176295034,
1.,0.995734176295034,1.,0.995734176295034,1.,0.995734176295034,1.,0.995734176295034,
1.,0.995734176295034,1.,0.995734176295034,1.,0.995734176295034,1.,0.995734176295034,
1.,0.995734176295034,1.,0.995734176295034,1.,0.995734176295034,1.,0.995734176295034,
1.,0.995734176295034,1.,0.995734176295034,1.,0.995734176295034,1.,0.995734176295034,
1.,0.995734176295034,1.,0.995734176295034,1.,0.995734176295034,1.,0.995734176295034,
1.,0.995734176295034,1.,0.995734176295034,1.,0.995734176295034,1.,0.995734176295034,
1.,0.995734176295034,1.,0.995734176295034,1.,0.995734176295034,1.,0.995734176295034,
1.,0.995734176295034,1.,0.995734176295034,1.,0.995734176295034,1.,0.995734176295034,
1.,0.995734176295034,1.,0.995734176295034,1.,0.995734176295034,1.,0.995734176295034,
1.,0.995734176295034,1.,0.995734176295034,1.,0.995734176295034,1.,0.995734176295034,
1.,0.995734176295034,1.,0.995734176295034,1.,0.995734176295034,1.,0.995734176295034,
1.,0.995734176295034,1.,0.995734176295034,1.,0.995734176295034,1.,0.995734176295034,
1.,0.995734176295034,1.,0.995734176295034,1.,0.995734176295034,1.,0.995734176295034,
1.,0.995734176295034,1.,0.995734176295034,1.,0.995734176295034,1.,0.995734176295034,
1.,0.995734176295034,1.,0.995734176295034,1.,0.995734176295034,1.,0.995734176295034,
1.,0.995734176295034,1.,0.995734176295034,1.,0.995734176295034,1.,0.995734176295034,
1.,0.995734176295034,1.,0.995734176295034,1.,0.995734176295034,1.,0.995734176295034,
1.,0.995734176295034,1.,0.995734176295034,1.,0.995734176295034,1.,0.995734176295034,
1.,0.995734176295034,1.,0.995734176295034,1.,0.995734176295034,1.,0.995734176295034,
1.,0.995734176295034,1.,0.995734176295034,1.,0.995734176295034,1.,0.995734176295034,
1.,0.995734176295034,1.,0.995734176295034,1.,0.995734176295034,1.,0.995734176295034,
1.,0.995734176295034,1.,0.995734176295034,1.,0.995734176295034,1.,0.995734176295034,
1.,0.995734176295034,1.,0.995734176295034,1.,0.995734176295034,1.,0.995734176295034,
1.,0.995734176295034,1.,0.995734176295034,1.,0.995734176295034,1.,0.995734176295034,
1.,0.995734176295034,1.,0.995734176295034,1.,0.995734176295034,1.,0.995734176295034,
1.,0.995734176295034,1.,0.995734176295034,1.,0.995734176295034,1.,0.995734176295034,
1.,0.995734176295034,1.,0.995734176295034,1.,0.995734176295034,1.,0.995734176295034,
1.,0.995734176295034,1.,0.995734176295034,1.,0.995734176295034,1.,0.995734176295034,
1.,0.995734176295034,1.,0.995734176295034,1.,0.995734176295034,1.,0.995734176295034,
1.,0.995734176295034,1.,0.995734176295034,1.,0.995734176295034,1.,0.995734176295034,
1.,0.995734176295034,1.,0.995734176295034,1.,0.995734176295034,1.,0.995734176295034,
1.,0.995734176295034,1.,0.995734176295034,1.,0.995734176295034,1.,0.995734176295034,
1.,0.995734176295034,1.,0.995734176295034,1.,0.995734176295034,1.,0.995734176295034,
1.,0.995734176295034,1.,0.995734176295034,1.,0.995734176295034,1.,0.995734176295034,
1.,0.995734176295034,1.,0.995734176295034,1.,0.995734176295034,1.,0.995734176295034,
1.,0.995734176295034,1.,0.995734176295034,1.,0.997201362504479,0.998074874808407)))
REPRESENTATION_ITEM('')
SURFACE()
);
#2505=(
BOUNDED_SURFACE()
B_SPLINE_SURFACE(1,2,((#163107,#163108,#163109,#163110,#163111,#163112,
#163113,#163114,#163115,#163116,#163117,#163118,#163119,#163120,#163121,
#163122,#163123,#163124,#163125,#163126,#163127,#163128,#163129,#163130,
#163131,#163132,#163133,#163134,#163135,#163136,#163137,#163138,#163139,
#163140,#163141,#163142,#163143,#163144,#163145,#163146,#163147,#163148,
#163149,#163150,#163151,#163152,#163153,#163154,#163155,#163156,#163157,
#163158,#163159,#163160,#163161,#163162,#163163,#163164,#163165,#163166,
#163167,#163168,#163169,#163170,#163171,#163172,#163173,#163174,#163175,
#163176,#163177,#163178,#163179,#163180,#163181,#163182,#163183,#163184,
#163185,#163186,#163187,#163188,#163189,#163190,#163191,#163192,#163193,
#163194,#163195,#163196,#163197,#163198,#163199,#163200,#163201,#163202,
#163203,#163204,#163205,#163206,#163207,#163208,#163209,#163210,#163211,
#163212,#163213,#163214,#163215,#163216,#163217,#163218,#163219,#163220,
#163221,#163222,#163223,#163224,#163225,#163226,#163227,#163228,#163229,
#163230,#163231,#163232,#163233,#163234,#163235,#163236,#163237,#163238,
#163239,#163240,#163241,#163242,#163243,#163244,#163245,#163246,#163247,
#163248,#163249,#163250,#163251,#163252,#163253,#163254,#163255,#163256,
#163257,#163258,#163259,#163260,#163261,#163262,#163263,#163264,#163265,
#163266,#163267,#163268,#163269,#163270,#163271,#163272,#163273,#163274,
#163275,#163276,#163277,#163278,#163279,#163280,#163281,#163282,#163283,
#163284,#163285,#163286,#163287,#163288,#163289,#163290,#163291,#163292,
#163293,#163294,#163295,#163296,#163297,#163298,#163299,#163300,#163301,
#163302,#163303,#163304,#163305,#163306,#163307,#163308,#163309,#163310,
#163311,#163312,#163313,#163314,#163315,#163316,#163317,#163318,#163319,
#163320,#163321,#163322,#163323,#163324,#163325,#163326,#163327,#163328,
#163329,#163330,#163331,#163332,#163333,#163334,#163335,#163336,#163337,
#163338,#163339,#163340,#163341,#163342,#163343,#163344,#163345,#163346,
#163347,#163348,#163349,#163350,#163351,#163352,#163353,#163354,#163355,
#163356,#163357,#163358,#163359,#163360,#163361,#163362,#163363,#163364,
#163365,#163366,#163367,#163368,#163369,#163370,#163371,#163372,#163373,
#163374,#163375,#163376,#163377,#163378,#163379,#163380,#163381,#163382,
#163383,#163384,#163385,#163386,#163387,#163388,#163389,#163390,#163391,
#163392,#163393,#163394,#163395,#163396,#163397,#163398,#163399,#163400,
#163401,#163402,#163403,#163404,#163405,#163406,#163407,#163408,#163409,
#163410,#163411,#163412,#163413,#163414,#163415,#163416,#163417,#163418,
#163419,#163420,#163421,#163422,#163423,#163424,#163425,#163426,#163427,
#163428,#163429,#163430,#163431,#163432,#163433,#163434,#163435,#163436,
#163437,#163438,#163439,#163440,#163441,#163442,#163443,#163444,#163445,
#163446,#163447,#163448,#163449,#163450,#163451,#163452,#163453,#163454,
#163455,#163456,#163457,#163458,#163459,#163460,#163461,#163462,#163463,
#163464,#163465,#163466,#163467,#163468,#163469,#163470,#163471,#163472,
#163473,#163474,#163475,#163476,#163477,#163478,#163479,#163480,#163481,
#163482,#163483,#163484,#163485,#163486,#163487,#163488,#163489,#163490,
#163491,#163492,#163493,#163494,#163495,#163496,#163497,#163498,#163499,
#163500,#163501,#163502,#163503,#163504,#163505,#163506,#163507,#163508,
#163509,#163510,#163511,#163512,#163513,#163514,#163515,#163516,#163517,
#163518,#163519,#163520,#163521,#163522,#163523,#163524,#163525,#163526,
#163527,#163528,#163529,#163530,#163531,#163532,#163533,#163534,#163535,
#163536,#163537,#163538,#163539,#163540,#163541,#163542,#163543,#163544,
#163545,#163546,#163547,#163548,#163549,#163550,#163551,#163552,#163553,
#163554,#163555,#163556,#163557,#163558,#163559,#163560,#163561,#163562,
#163563,#163564,#163565,#163566,#163567,#163568,#163569,#163570,#163571,
#163572,#163573,#163574,#163575,#163576,#163577,#163578,#163579,#163580,
#163581,#163582,#163583,#163584,#163585,#163586,#163587,#163588,#163589,
#163590,#163591,#163592,#163593,#163594,#163595,#163596,#163597,#163598,
#163599,#163600,#163601,#163602,#163603,#163604,#163605,#163606,#163607,
#163608,#163609,#163610,#163611,#163612,#163613,#163614,#163615,#163616,
#163617,#163618,#163619,#163620,#163621,#163622,#163623,#163624,#163625,
#163626,#163627,#163628,#163629,#163630,#163631,#163632,#163633,#163634,
#163635,#163636,#163637,#163638,#163639,#163640,#163641,#163642,#163643,
#163644,#163645,#163646,#163647,#163648,#163649,#163650,#163651,#163652,
#163653,#163654,#163655,#163656,#163657,#163658,#163659,#163660,#163661,
#163662,#163663,#163664,#163665,#163666,#163667,#163668,#163669,#163670,
#163671,#163672,#163673,#163674,#163675,#163676,#163677,#163678,#163679,
#163680,#163681,#163682,#163683,#163684,#163685,#163686,#163687,#163688,
#163689,#163690,#163691,#163692,#163693,#163694,#163695,#163696,#163697,
#163698,#163699,#163700,#163701,#163702,#163703,#163704,#163705,#163706,
#163707,#163708,#163709,#163710,#163711,#163712,#163713,#163714,#163715,
#163716,#163717,#163718,#163719,#163720,#163721,#163722,#163723,#163724,
#163725,#163726,#163727,#163728,#163729,#163730,#163731,#163732,#163733,
#163734,#163735,#163736,#163737,#163738,#163739,#163740,#163741,#163742,
#163743,#163744,#163745,#163746,#163747,#163748,#163749,#163750,#163751,
#163752,#163753,#163754,#163755,#163756,#163757,#163758,#163759,#163760,
#163761,#163762,#163763,#163764,#163765,#163766,#163767,#163768,#163769,
#163770,#163771,#163772,#163773,#163774,#163775,#163776,#163777,#163778,
#163779,#163780,#163781,#163782,#163783,#163784,#163785,#163786,#163787,
#163788,#163789,#163790,#163791,#163792,#163793,#163794,#163795,#163796,
#163797,#163798,#163799,#163800,#163801,#163802,#163803,#163804,#163805,
#163806,#163807,#163808,#163809,#163810,#163811,#163812,#163813,#163814,
#163815,#163816,#163817,#163818,#163819,#163820,#163821,#163822,#163823,
#163824,#163825,#163826,#163827,#163828,#163829,#163830,#163831,#163832,
#163833,#163834,#163835,#163836,#163837,#163838,#163839,#163840,#163841,
#163842,#163843,#163844,#163845,#163846,#163847,#163848,#163849,#163850,
#163851,#163852,#163853,#163854,#163855,#163856,#163857,#163858,#163859,
#163860,#163861,#163862,#163863,#163864,#163865,#163866,#163867,#163868,
#163869,#163870,#163871,#163872,#163873,#163874,#163875,#163876,#163877,
#163878,#163879,#163880,#163881,#163882,#163883,#163884,#163885,#163886,
#163887,#163888,#163889,#163890,#163891,#163892,#163893,#163894,#163895,
#163896,#163897,#163898,#163899,#163900,#163901,#163902,#163903,#163904,
#163905,#163906,#163907,#163908,#163909,#163910,#163911,#163912,#163913,
#163914,#163915,#163916,#163917,#163918,#163919,#163920,#163921,#163922,
#163923,#163924,#163925,#163926,#163927,#163928,#163929,#163930,#163931,
#163932,#163933,#163934,#163935,#163936,#163937,#163938,#163939,#163940,
#163941,#163942,#163943,#163944,#163945,#163946,#163947,#163948,#163949,
#163950,#163951,#163952,#163953,#163954,#163955,#163956,#163957,#163958,
#163959,#163960,#163961,#163962,#163963,#163964,#163965,#163966,#163967,
#163968,#163969,#163970,#163971,#163972,#163973,#163974,#163975,#163976,
#163977,#163978,#163979,#163980,#163981,#163982,#163983,#163984,#163985,
#163986,#163987,#163988,#163989,#163990,#163991,#163992,#163993,#163994,
#163995,#163996,#163997,#163998,#163999,#164000,#164001,#164002,#164003,
#164004,#164005,#164006,#164007,#164008,#164009,#164010,#164011,#164012,
#164013,#164014,#164015,#164016,#164017,#164018,#164019,#164020,#164021,
#164022,#164023,#164024,#164025,#164026,#164027,#164028,#164029,#164030,
#164031,#164032,#164033,#164034,#164035,#164036,#164037,#164038,#164039,
#164040,#164041,#164042,#164043,#164044,#164045,#164046,#164047,#164048,
#164049,#164050,#164051,#164052,#164053,#164054,#164055,#164056,#164057,
#164058,#164059,#164060,#164061,#164062,#164063,#164064,#164065,#164066,
#164067,#164068,#164069,#164070,#164071,#164072,#164073,#164074,#164075,
#164076,#164077,#164078,#164079,#164080,#164081,#164082,#164083,#164084,
#164085,#164086,#164087,#164088,#164089,#164090,#164091,#164092,#164093,
#164094,#164095,#164096,#164097,#164098,#164099,#164100,#164101,#164102,
#164103,#164104,#164105,#164106,#164107,#164108,#164109,#164110,#164111,
#164112,#164113,#164114,#164115,#164116,#164117,#164118,#164119,#164120,
#164121,#164122,#164123,#164124,#164125,#164126,#164127,#164128,#164129,
#164130,#164131,#164132,#164133,#164134,#164135,#164136,#164137,#164138,
#164139,#164140,#164141,#164142,#164143,#164144,#164145,#164146,#164147,
#164148,#164149,#164150,#164151,#164152,#164153,#164154,#164155,#164156,
#164157,#164158,#164159,#164160,#164161,#164162,#164163,#164164,#164165,
#164166,#164167,#164168,#164169,#164170,#164171,#164172,#164173,#164174,
#164175,#164176,#164177,#164178,#164179,#164180,#164181,#164182,#164183,
#164184,#164185,#164186,#164187,#164188,#164189,#164190,#164191,#164192,
#164193,#164194,#164195,#164196,#164197,#164198,#164199,#164200,#164201,
#164202,#164203,#164204,#164205,#164206,#164207,#164208,#164209,#164210,
#164211,#164212,#164213,#164214,#164215,#164216,#164217,#164218,#164219,
#164220,#164221,#164222,#164223,#164224,#164225,#164226,#164227,#164228,
#164229,#164230,#164231,#164232,#164233,#164234,#164235,#164236,#164237,
#164238,#164239,#164240,#164241,#164242,#164243,#164244,#164245,#164246,
#164247,#164248,#164249,#164250,#164251,#164252,#164253,#164254,#164255,
#164256,#164257,#164258,#164259,#164260,#164261,#164262,#164263,#164264,
#164265,#164266,#164267,#164268,#164269,#164270,#164271,#164272,#164273,
#164274,#164275,#164276,#164277,#164278,#164279,#164280,#164281,#164282,
#164283,#164284,#164285,#164286,#164287,#164288,#164289,#164290,#164291,
#164292,#164293,#164294,#164295,#164296,#164297,#164298,#164299,#164300,
#164301,#164302,#164303,#164304,#164305,#164306,#164307,#164308,#164309,
#164310,#164311,#164312,#164313,#164314,#164315,#164316,#164317,#164318,
#164319,#164320,#164321,#164322,#164323,#164324,#164325,#164326,#164327,
#164328,#164329,#164330,#164331,#164332,#164333,#164334,#164335,#164336,
#164337,#164338,#164339,#164340,#164341,#164342,#164343,#164344,#164345,
#164346,#164347,#164348,#164349,#164350,#164351,#164352,#164353,#164354,
#164355,#164356,#164357,#164358,#164359,#164360,#164361,#164362,#164363,
#164364,#164365,#164366,#164367,#164368,#164369,#164370,#164371,#164372,
#164373,#164374,#164375,#164376,#164377,#164378,#164379,#164380,#164381,
#164382,#164383,#164384,#164385,#164386,#164387,#164388,#164389,#164390,
#164391,#164392,#164393,#164394,#164395,#164396,#164397,#164398,#164399,
#164400,#164401,#164402,#164403,#164404,#164405,#164406,#164407,#164408,
#164409,#164410,#164411,#164412,#164413,#164414,#164415,#164416,#164417,
#164418,#164419,#164420,#164421,#164422,#164423,#164424,#164425,#164426,
#164427,#164428,#164429,#164430,#164431,#164432,#164433,#164434,#164435,
#164436,#164437,#164438,#164439,#164440,#164441,#164442,#164443,#164444,
#164445,#164446,#164447,#164448,#164449,#164450,#164451,#164452,#164453,
#164454,#164455,#164456,#164457,#164458,#164459,#164460,#164461,#164462,
#164463,#164464,#164465,#164466,#164467,#164468,#164469,#164470,#164471,
#164472,#164473,#164474,#164475,#164476,#164477,#164478,#164479,#164480,
#164481,#164482,#164483,#164484,#164485,#164486,#164487,#164488,#164489,
#164490,#164491,#164492,#164493,#164494,#164495,#164496,#164497,#164498,
#164499,#164500,#164501,#164502,#164503,#164504,#164505,#164506,#164507,
#164508,#164509,#164510,#164511,#164512,#164513,#164514,#164515,#164516,
#164517,#164518,#164519,#164520,#164521,#164522,#164523,#164524,#164525,
#164526,#164527,#164528,#164529,#164530,#164531,#164532,#164533,#164534,
#164535,#164536,#164537,#164538,#164539,#164540,#164541,#164542,#164543,
#164544,#164545,#164546,#164547,#164548,#164549,#164550,#164551,#164552,
#164553,#164554,#164555,#164556,#164557,#164558,#164559,#164560,#164561,
#164562,#164563,#164564,#164565,#164566,#164567,#164568,#164569,#164570,
#164571,#164572,#164573,#164574,#164575,#164576,#164577,#164578,#164579,
#164580,#164581,#164582,#164583,#164584,#164585,#164586,#164587,#164588,
#164589,#164590,#164591,#164592,#164593,#164594,#164595,#164596,#164597,
#164598,#164599,#164600,#164601,#164602,#164603,#164604,#164605,#164606,
#164607,#164608,#164609,#164610,#164611,#164612,#164613,#164614,#164615,
#164616,#164617,#164618,#164619,#164620,#164621,#164622,#164623,#164624,
#164625,#164626,#164627,#164628,#164629,#164630,#164631,#164632,#164633,
#164634,#164635,#164636,#164637,#164638,#164639,#164640,#164641,#164642,
#164643,#164644,#164645,#164646,#164647,#164648,#164649,#164650,#164651,
#164652,#164653,#164654,#164655,#164656,#164657,#164658,#164659,#164660,
#164661,#164662,#164663,#164664,#164665,#164666,#164667,#164668,#164669,
#164670,#164671,#164672,#164673,#164674,#164675,#164676,#164677,#164678,
#164679,#164680,#164681,#164682,#164683,#164684,#164685,#164686,#164687,
#164688,#164689,#164690,#164691,#164692,#164693,#164694,#164695,#164696,
#164697,#164698,#164699,#164700,#164701,#164702,#164703,#164704,#164705,
#164706,#164707,#164708,#164709,#164710,#164711,#164712,#164713,#164714,
#164715,#164716,#164717,#164718,#164719,#164720,#164721,#164722,#164723,
#164724,#164725,#164726,#164727,#164728,#164729,#164730,#164731,#164732,
#164733,#164734,#164735,#164736,#164737,#164738,#164739,#164740,#164741,
#164742,#164743,#164744,#164745,#164746,#164747,#164748,#164749,#164750,
#164751,#164752,#164753,#164754,#164755,#164756,#164757,#164758,#164759,
#164760,#164761,#164762,#164763,#164764,#164765,#164766,#164767,#164768,
#164769,#164770,#164771,#164772,#164773,#164774,#164775,#164776,#164777,
#164778,#164779,#164780,#164781,#164782,#164783,#164784,#164785,#164786,
#164787,#164788,#164789,#164790,#164791,#164792,#164793,#164794,#164795,
#164796,#164797,#164798,#164799,#164800,#164801,#164802,#164803,#164804,
#164805,#164806,#164807,#164808,#164809,#164810,#164811,#164812,#164813,
#164814,#164815,#164816,#164817,#164818,#164819,#164820,#164821,#164822,
#164823,#164824,#164825,#164826,#164827,#164828,#164829,#164830,#164831,
#164832,#164833,#164834,#164835,#164836,#164837,#164838,#164839,#164840,
#164841,#164842,#164843,#164844,#164845,#164846,#164847,#164848,#164849,
#164850,#164851,#164852,#164853,#164854,#164855,#164856,#164857,#164858,
#164859,#164860,#164861,#164862,#164863,#164864,#164865,#164866,#164867,
#164868,#164869,#164870,#164871,#164872,#164873,#164874,#164875,#164876,
#164877,#164878,#164879,#164880,#164881,#164882,#164883,#164884,#164885,
#164886,#164887,#164888,#164889,#164890,#164891,#164892,#164893,#164894,
#164895,#164896,#164897,#164898,#164899,#164900,#164901,#164902,#164903,
#164904,#164905,#164906,#164907,#164908,#164909,#164910,#164911,#164912,
#164913,#164914,#164915,#164916,#164917,#164918,#164919,#164920,#164921,
#164922,#164923,#164924,#164925,#164926,#164927,#164928,#164929,#164930,
#164931,#164932,#164933,#164934,#164935,#164936,#164937,#164938,#164939,
#164940,#164941,#164942,#164943,#164944,#164945,#164946,#164947,#164948,
#164949,#164950,#164951,#164952,#164953,#164954,#164955,#164956,#164957,
#164958,#164959,#164960,#164961,#164962,#164963,#164964,#164965,#164966,
#164967,#164968,#164969,#164970,#164971,#164972,#164973,#164974,#164975,
#164976,#164977,#164978,#164979,#164980,#164981,#164982,#164983,#164984,
#164985,#164986,#164987,#164988,#164989,#164990,#164991,#164992,#164993,
#164994,#164995,#164996,#164997,#164998,#164999,#165000,#165001,#165002,
#165003,#165004,#165005,#165006,#165007,#165008,#165009,#165010,#165011,
#165012,#165013,#165014,#165015,#165016,#165017,#165018,#165019,#165020,
#165021,#165022,#165023,#165024,#165025,#165026,#165027,#165028,#165029,
#165030,#165031,#165032,#165033,#165034,#165035,#165036,#165037,#165038,
#165039,#165040,#165041,#165042,#165043,#165044,#165045,#165046,#165047,
#165048,#165049,#165050,#165051,#165052,#165053,#165054,#165055,#165056,
#165057,#165058,#165059,#165060,#165061,#165062,#165063,#165064,#165065,
#165066,#165067,#165068,#165069,#165070,#165071,#165072,#165073,#165074,
#165075,#165076,#165077,#165078,#165079,#165080,#165081,#165082,#165083,
#165084,#165085,#165086,#165087,#165088,#165089,#165090,#165091,#165092,
#165093,#165094,#165095,#165096,#165097,#165098,#165099,#165100,#165101,
#165102,#165103,#165104,#165105,#165106,#165107,#165108,#165109,#165110,
#165111,#165112,#165113,#165114,#165115,#165116,#165117,#165118,#165119,
#165120,#165121),(#165122,#165123,#165124,#165125,#165126,#165127,#165128,
#165129,#165130,#165131,#165132,#165133,#165134,#165135,#165136,#165137,
#165138,#165139,#165140,#165141,#165142,#165143,#165144,#165145,#165146,
#165147,#165148,#165149,#165150,#165151,#165152,#165153,#165154,#165155,
#165156,#165157,#165158,#165159,#165160,#165161,#165162,#165163,#165164,
#165165,#165166,#165167,#165168,#165169,#165170,#165171,#165172,#165173,
#165174,#165175,#165176,#165177,#165178,#165179,#165180,#165181,#165182,
#165183,#165184,#165185,#165186,#165187,#165188,#165189,#165190,#165191,
#165192,#165193,#165194,#165195,#165196,#165197,#165198,#165199,#165200,
#165201,#165202,#165203,#165204,#165205,#165206,#165207,#165208,#165209,
#165210,#165211,#165212,#165213,#165214,#165215,#165216,#165217,#165218,
#165219,#165220,#165221,#165222,#165223,#165224,#165225,#165226,#165227,
#165228,#165229,#165230,#165231,#165232,#165233,#165234,#165235,#165236,
#165237,#165238,#165239,#165240,#165241,#165242,#165243,#165244,#165245,
#165246,#165247,#165248,#165249,#165250,#165251,#165252,#165253,#165254,
#165255,#165256,#165257,#165258,#165259,#165260,#165261,#165262,#165263,
#165264,#165265,#165266,#165267,#165268,#165269,#165270,#165271,#165272,
#165273,#165274,#165275,#165276,#165277,#165278,#165279,#165280,#165281,
#165282,#165283,#165284,#165285,#165286,#165287,#165288,#165289,#165290,
#165291,#165292,#165293,#165294,#165295,#165296,#165297,#165298,#165299,
#165300,#165301,#165302,#165303,#165304,#165305,#165306,#165307,#165308,
#165309,#165310,#165311,#165312,#165313,#165314,#165315,#165316,#165317,
#165318,#165319,#165320,#165321,#165322,#165323,#165324,#165325,#165326,
#165327,#165328,#165329,#165330,#165331,#165332,#165333,#165334,#165335,
#165336,#165337,#165338,#165339,#165340,#165341,#165342,#165343,#165344,
#165345,#165346,#165347,#165348,#165349,#165350,#165351,#165352,#165353,
#165354,#165355,#165356,#165357,#165358,#165359,#165360,#165361,#165362,
#165363,#165364,#165365,#165366,#165367,#165368,#165369,#165370,#165371,
#165372,#165373,#165374,#165375,#165376,#165377,#165378,#165379,#165380,
#165381,#165382,#165383,#165384,#165385,#165386,#165387,#165388,#165389,
#165390,#165391,#165392,#165393,#165394,#165395,#165396,#165397,#165398,
#165399,#165400,#165401,#165402,#165403,#165404,#165405,#165406,#165407,
#165408,#165409,#165410,#165411,#165412,#165413,#165414,#165415,#165416,
#165417,#165418,#165419,#165420,#165421,#165422,#165423,#165424,#165425,
#165426,#165427,#165428,#165429,#165430,#165431,#165432,#165433,#165434,
#165435,#165436,#165437,#165438,#165439,#165440,#165441,#165442,#165443,
#165444,#165445,#165446,#165447,#165448,#165449,#165450,#165451,#165452,
#165453,#165454,#165455,#165456,#165457,#165458,#165459,#165460,#165461,
#165462,#165463,#165464,#165465,#165466,#165467,#165468,#165469,#165470,
#165471,#165472,#165473,#165474,#165475,#165476,#165477,#165478,#165479,
#165480,#165481,#165482,#165483,#165484,#165485,#165486,#165487,#165488,
#165489,#165490,#165491,#165492,#165493,#165494,#165495,#165496,#165497,
#165498,#165499,#165500,#165501,#165502,#165503,#165504,#165505,#165506,
#165507,#165508,#165509,#165510,#165511,#165512,#165513,#165514,#165515,
#165516,#165517,#165518,#165519,#165520,#165521,#165522,#165523,#165524,
#165525,#165526,#165527,#165528,#165529,#165530,#165531,#165532,#165533,
#165534,#165535,#165536,#165537,#165538,#165539,#165540,#165541,#165542,
#165543,#165544,#165545,#165546,#165547,#165548,#165549,#165550,#165551,
#165552,#165553,#165554,#165555,#165556,#165557,#165558,#165559,#165560,
#165561,#165562,#165563,#165564,#165565,#165566,#165567,#165568,#165569,
#165570,#165571,#165572,#165573,#165574,#165575,#165576,#165577,#165578,
#165579,#165580,#165581,#165582,#165583,#165584,#165585,#165586,#165587,
#165588,#165589,#165590,#165591,#165592,#165593,#165594,#165595,#165596,
#165597,#165598,#165599,#165600,#165601,#165602,#165603,#165604,#165605,
#165606,#165607,#165608,#165609,#165610,#165611,#165612,#165613,#165614,
#165615,#165616,#165617,#165618,#165619,#165620,#165621,#165622,#165623,
#165624,#165625,#165626,#165627,#165628,#165629,#165630,#165631,#165632,
#165633,#165634,#165635,#165636,#165637,#165638,#165639,#165640,#165641,
#165642,#165643,#165644,#165645,#165646,#165647,#165648,#165649,#165650,
#165651,#165652,#165653,#165654,#165655,#165656,#165657,#165658,#165659,
#165660,#165661,#165662,#165663,#165664,#165665,#165666,#165667,#165668,
#165669,#165670,#165671,#165672,#165673,#165674,#165675,#165676,#165677,
#165678,#165679,#165680,#165681,#165682,#165683,#165684,#165685,#165686,
#165687,#165688,#165689,#165690,#165691,#165692,#165693,#165694,#165695,
#165696,#165697,#165698,#165699,#165700,#165701,#165702,#165703,#165704,
#165705,#165706,#165707,#165708,#165709,#165710,#165711,#165712,#165713,
#165714,#165715,#165716,#165717,#165718,#165719,#165720,#165721,#165722,
#165723,#165724,#165725,#165726,#165727,#165728,#165729,#165730,#165731,
#165732,#165733,#165734,#165735,#165736,#165737,#165738,#165739,#165740,
#165741,#165742,#165743,#165744,#165745,#165746,#165747,#165748,#165749,
#165750,#165751,#165752,#165753,#165754,#165755,#165756,#165757,#165758,
#165759,#165760,#165761,#165762,#165763,#165764,#165765,#165766,#165767,
#165768,#165769,#165770,#165771,#165772,#165773,#165774,#165775,#165776,
#165777,#165778,#165779,#165780,#165781,#165782,#165783,#165784,#165785,
#165786,#165787,#165788,#165789,#165790,#165791,#165792,#165793,#165794,
#165795,#165796,#165797,#165798,#165799,#165800,#165801,#165802,#165803,
#165804,#165805,#165806,#165807,#165808,#165809,#165810,#165811,#165812,
#165813,#165814,#165815,#165816,#165817,#165818,#165819,#165820,#165821,
#165822,#165823,#165824,#165825,#165826,#165827,#165828,#165829,#165830,
#165831,#165832,#165833,#165834,#165835,#165836,#165837,#165838,#165839,
#165840,#165841,#165842,#165843,#165844,#165845,#165846,#165847,#165848,
#165849,#165850,#165851,#165852,#165853,#165854,#165855,#165856,#165857,
#165858,#165859,#165860,#165861,#165862,#165863,#165864,#165865,#165866,
#165867,#165868,#165869,#165870,#165871,#165872,#165873,#165874,#165875,
#165876,#165877,#165878,#165879,#165880,#165881,#165882,#165883,#165884,
#165885,#165886,#165887,#165888,#165889,#165890,#165891,#165892,#165893,
#165894,#165895,#165896,#165897,#165898,#165899,#165900,#165901,#165902,
#165903,#165904,#165905,#165906,#165907,#165908,#165909,#165910,#165911,
#165912,#165913,#165914,#165915,#165916,#165917,#165918,#165919,#165920,
#165921,#165922,#165923,#165924,#165925,#165926,#165927,#165928,#165929,
#165930,#165931,#165932,#165933,#165934,#165935,#165936,#165937,#165938,
#165939,#165940,#165941,#165942,#165943,#165944,#165945,#165946,#165947,
#165948,#165949,#165950,#165951,#165952,#165953,#165954,#165955,#165956,
#165957,#165958,#165959,#165960,#165961,#165962,#165963,#165964,#165965,
#165966,#165967,#165968,#165969,#165970,#165971,#165972,#165973,#165974,
#165975,#165976,#165977,#165978,#165979,#165980,#165981,#165982,#165983,
#165984,#165985,#165986,#165987,#165988,#165989,#165990,#165991,#165992,
#165993,#165994,#165995,#165996,#165997,#165998,#165999,#166000,#166001,
#166002,#166003,#166004,#166005,#166006,#166007,#166008,#166009,#166010,
#166011,#166012,#166013,#166014,#166015,#166016,#166017,#166018,#166019,
#166020,#166021,#166022,#166023,#166024,#166025,#166026,#166027,#166028,
#166029,#166030,#166031,#166032,#166033,#166034,#166035,#166036,#166037,
#166038,#166039,#166040,#166041,#166042,#166043,#166044,#166045,#166046,
#166047,#166048,#166049,#166050,#166051,#166052,#166053,#166054,#166055,
#166056,#166057,#166058,#166059,#166060,#166061,#166062,#166063,#166064,
#166065,#166066,#166067,#166068,#166069,#166070,#166071,#166072,#166073,
#166074,#166075,#166076,#166077,#166078,#166079,#166080,#166081,#166082,
#166083,#166084,#166085,#166086,#166087,#166088,#166089,#166090,#166091,
#166092,#166093,#166094,#166095,#166096,#166097,#166098,#166099,#166100,
#166101,#166102,#166103,#166104,#166105,#166106,#166107,#166108,#166109,
#166110,#166111,#166112,#166113,#166114,#166115,#166116,#166117,#166118,
#166119,#166120,#166121,#166122,#166123,#166124,#166125,#166126,#166127,
#166128,#166129,#166130,#166131,#166132,#166133,#166134,#166135,#166136,
#166137,#166138,#166139,#166140,#166141,#166142,#166143,#166144,#166145,
#166146,#166147,#166148,#166149,#166150,#166151,#166152,#166153,#166154,
#166155,#166156,#166157,#166158,#166159,#166160,#166161,#166162,#166163,
#166164,#166165,#166166,#166167,#166168,#166169,#166170,#166171,#166172,
#166173,#166174,#166175,#166176,#166177,#166178,#166179,#166180,#166181,
#166182,#166183,#166184,#166185,#166186,#166187,#166188,#166189,#166190,
#166191,#166192,#166193,#166194,#166195,#166196,#166197,#166198,#166199,
#166200,#166201,#166202,#166203,#166204,#166205,#166206,#166207,#166208,
#166209,#166210,#166211,#166212,#166213,#166214,#166215,#166216,#166217,
#166218,#166219,#166220,#166221,#166222,#166223,#166224,#166225,#166226,
#166227,#166228,#166229,#166230,#166231,#166232,#166233,#166234,#166235,
#166236,#166237,#166238,#166239,#166240,#166241,#166242,#166243,#166244,
#166245,#166246,#166247,#166248,#166249,#166250,#166251,#166252,#166253,
#166254,#166255,#166256,#166257,#166258,#166259,#166260,#166261,#166262,
#166263,#166264,#166265,#166266,#166267,#166268,#166269,#166270,#166271,
#166272,#166273,#166274,#166275,#166276,#166277,#166278,#166279,#166280,
#166281,#166282,#166283,#166284,#166285,#166286,#166287,#166288,#166289,
#166290,#166291,#166292,#166293,#166294,#166295,#166296,#166297,#166298,
#166299,#166300,#166301,#166302,#166303,#166304,#166305,#166306,#166307,
#166308,#166309,#166310,#166311,#166312,#166313,#166314,#166315,#166316,
#166317,#166318,#166319,#166320,#166321,#166322,#166323,#166324,#166325,
#166326,#166327,#166328,#166329,#166330,#166331,#166332,#166333,#166334,
#166335,#166336,#166337,#166338,#166339,#166340,#166341,#166342,#166343,
#166344,#166345,#166346,#166347,#166348,#166349,#166350,#166351,#166352,
#166353,#166354,#166355,#166356,#166357,#166358,#166359,#166360,#166361,
#166362,#166363,#166364,#166365,#166366,#166367,#166368,#166369,#166370,
#166371,#166372,#166373,#166374,#166375,#166376,#166377,#166378,#166379,
#166380,#166381,#166382,#166383,#166384,#166385,#166386,#166387,#166388,
#166389,#166390,#166391,#166392,#166393,#166394,#166395,#166396,#166397,
#166398,#166399,#166400,#166401,#166402,#166403,#166404,#166405,#166406,
#166407,#166408,#166409,#166410,#166411,#166412,#166413,#166414,#166415,
#166416,#166417,#166418,#166419,#166420,#166421,#166422,#166423,#166424,
#166425,#166426,#166427,#166428,#166429,#166430,#166431,#166432,#166433,
#166434,#166435,#166436,#166437,#166438,#166439,#166440,#166441,#166442,
#166443,#166444,#166445,#166446,#166447,#166448,#166449,#166450,#166451,
#166452,#166453,#166454,#166455,#166456,#166457,#166458,#166459,#166460,
#166461,#166462,#166463,#166464,#166465,#166466,#166467,#166468,#166469,
#166470,#166471,#166472,#166473,#166474,#166475,#166476,#166477,#166478,
#166479,#166480,#166481,#166482,#166483,#166484,#166485,#166486,#166487,
#166488,#166489,#166490,#166491,#166492,#166493,#166494,#166495,#166496,
#166497,#166498,#166499,#166500,#166501,#166502,#166503,#166504,#166505,
#166506,#166507,#166508,#166509,#166510,#166511,#166512,#166513,#166514,
#166515,#166516,#166517,#166518,#166519,#166520,#166521,#166522,#166523,
#166524,#166525,#166526,#166527,#166528,#166529,#166530,#166531,#166532,
#166533,#166534,#166535,#166536,#166537,#166538,#166539,#166540,#166541,
#166542,#166543,#166544,#166545,#166546,#166547,#166548,#166549,#166550,
#166551,#166552,#166553,#166554,#166555,#166556,#166557,#166558,#166559,
#166560,#166561,#166562,#166563,#166564,#166565,#166566,#166567,#166568,
#166569,#166570,#166571,#166572,#166573,#166574,#166575,#166576,#166577,
#166578,#166579,#166580,#166581,#166582,#166583,#166584,#166585,#166586,
#166587,#166588,#166589,#166590,#166591,#166592,#166593,#166594,#166595,
#166596,#166597,#166598,#166599,#166600,#166601,#166602,#166603,#166604,
#166605,#166606,#166607,#166608,#166609,#166610,#166611,#166612,#166613,
#166614,#166615,#166616,#166617,#166618,#166619,#166620,#166621,#166622,
#166623,#166624,#166625,#166626,#166627,#166628,#166629,#166630,#166631,
#166632,#166633,#166634,#166635,#166636,#166637,#166638,#166639,#166640,
#166641,#166642,#166643,#166644,#166645,#166646,#166647,#166648,#166649,
#166650,#166651,#166652,#166653,#166654,#166655,#166656,#166657,#166658,
#166659,#166660,#166661,#166662,#166663,#166664,#166665,#166666,#166667,
#166668,#166669,#166670,#166671,#166672,#166673,#166674,#166675,#166676,
#166677,#166678,#166679,#166680,#166681,#166682,#166683,#166684,#166685,
#166686,#166687,#166688,#166689,#166690,#166691,#166692,#166693,#166694,
#166695,#166696,#166697,#166698,#166699,#166700,#166701,#166702,#166703,
#166704,#166705,#166706,#166707,#166708,#166709,#166710,#166711,#166712,
#166713,#166714,#166715,#166716,#166717,#166718,#166719,#166720,#166721,
#166722,#166723,#166724,#166725,#166726,#166727,#166728,#166729,#166730,
#166731,#166732,#166733,#166734,#166735,#166736,#166737,#166738,#166739,
#166740,#166741,#166742,#166743,#166744,#166745,#166746,#166747,#166748,
#166749,#166750,#166751,#166752,#166753,#166754,#166755,#166756,#166757,
#166758,#166759,#166760,#166761,#166762,#166763,#166764,#166765,#166766,
#166767,#166768,#166769,#166770,#166771,#166772,#166773,#166774,#166775,
#166776,#166777,#166778,#166779,#166780,#166781,#166782,#166783,#166784,
#166785,#166786,#166787,#166788,#166789,#166790,#166791,#166792,#166793,
#166794,#166795,#166796,#166797,#166798,#166799,#166800,#166801,#166802,
#166803,#166804,#166805,#166806,#166807,#166808,#166809,#166810,#166811,
#166812,#166813,#166814,#166815,#166816,#166817,#166818,#166819,#166820,
#166821,#166822,#166823,#166824,#166825,#166826,#166827,#166828,#166829,
#166830,#166831,#166832,#166833,#166834,#166835,#166836,#166837,#166838,
#166839,#166840,#166841,#166842,#166843,#166844,#166845,#166846,#166847,
#166848,#166849,#166850,#166851,#166852,#166853,#166854,#166855,#166856,
#166857,#166858,#166859,#166860,#166861,#166862,#166863,#166864,#166865,
#166866,#166867,#166868,#166869,#166870,#166871,#166872,#166873,#166874,
#166875,#166876,#166877,#166878,#166879,#166880,#166881,#166882,#166883,
#166884,#166885,#166886,#166887,#166888,#166889,#166890,#166891,#166892,
#166893,#166894,#166895,#166896,#166897,#166898,#166899,#166900,#166901,
#166902,#166903,#166904,#166905,#166906,#166907,#166908,#166909,#166910,
#166911,#166912,#166913,#166914,#166915,#166916,#166917,#166918,#166919,
#166920,#166921,#166922,#166923,#166924,#166925,#166926,#166927,#166928,
#166929,#166930,#166931,#166932,#166933,#166934,#166935,#166936,#166937,
#166938,#166939,#166940,#166941,#166942,#166943,#166944,#166945,#166946,
#166947,#166948,#166949,#166950,#166951,#166952,#166953,#166954,#166955,
#166956,#166957,#166958,#166959,#166960,#166961,#166962,#166963,#166964,
#166965,#166966,#166967,#166968,#166969,#166970,#166971,#166972,#166973,
#166974,#166975,#166976,#166977,#166978,#166979,#166980,#166981,#166982,
#166983,#166984,#166985,#166986,#166987,#166988,#166989,#166990,#166991,
#166992,#166993,#166994,#166995,#166996,#166997,#166998,#166999,#167000,
#167001,#167002,#167003,#167004,#167005,#167006,#167007,#167008,#167009,
#167010,#167011,#167012,#167013,#167014,#167015,#167016,#167017,#167018,
#167019,#167020,#167021,#167022,#167023,#167024,#167025,#167026,#167027,
#167028,#167029,#167030,#167031,#167032,#167033,#167034,#167035,#167036,
#167037,#167038,#167039,#167040,#167041,#167042,#167043,#167044,#167045,
#167046,#167047,#167048,#167049,#167050,#167051,#167052,#167053,#167054,
#167055,#167056,#167057,#167058,#167059,#167060,#167061,#167062,#167063,
#167064,#167065,#167066,#167067,#167068,#167069,#167070,#167071,#167072,
#167073,#167074,#167075,#167076,#167077,#167078,#167079,#167080,#167081,
#167082,#167083,#167084,#167085,#167086,#167087,#167088,#167089,#167090,
#167091,#167092,#167093,#167094,#167095,#167096,#167097,#167098,#167099,
#167100,#167101,#167102,#167103,#167104,#167105,#167106,#167107,#167108,
#167109,#167110,#167111,#167112,#167113,#167114,#167115,#167116,#167117,
#167118,#167119,#167120,#167121,#167122,#167123,#167124,#167125,#167126,
#167127,#167128,#167129,#167130,#167131,#167132,#167133,#167134,#167135,
#167136)),.UNSPECIFIED.,.F.,.F.,.F.)
B_SPLINE_SURFACE_WITH_KNOTS((2,2),(3,2,2,2,2,2,2,2,2,2,2,2,2,2,2,2,2,2,
2,2,2,2,2,2,2,2,2,2,2,2,2,2,2,2,2,2,2,2,2,2,2,2,2,2,2,2,2,2,2,2,2,2,2,2,
2,2,2,2,2,2,2,2,2,2,2,2,2,2,2,2,2,2,2,2,2,2,2,2,2,2,2,2,2,2,2,2,2,2,2,2,
2,2,2,2,2,2,2,2,2,2,2,2,2,2,2,2,2,2,2,2,2,2,2,2,2,2,2,2,2,2,2,2,2,2,2,2,
2,2,2,2,2,2,2,2,2,2,2,2,2,2,2,2,2,2,2,2,2,2,2,2,2,2,2,2,2,2,2,2,2,2,2,2,
2,2,2,2,2,2,2,2,2,2,2,2,2,2,2,2,2,2,2,2,2,2,2,2,2,2,2,2,2,2,2,2,2,2,2,2,
2,2,2,2,2,2,2,2,2,2,2,2,2,2,2,2,2,2,2,2,2,2,2,2,2,2,2,2,2,2,2,2,2,2,2,2,
2,2,2,2,2,2,2,2,2,2,2,2,2,2,2,2,2,2,2,2,2,2,2,2,2,2,2,2,2,2,2,2,2,2,2,2,
2,2,2,2,2,2,2,2,2,2,2,2,2,2,2,2,2,2,2,2,2,2,2,2,2,2,2,2,2,2,2,2,2,2,2,2,
2,2,2,2,2,2,2,2,2,2,2,2,2,2,2,2,2,2,2,2,2,2,2,2,2,2,2,2,2,2,2,2,2,2,2,2,
2,2,2,2,2,2,2,2,2,2,2,2,2,2,2,2,2,2,2,2,2,2,2,2,2,2,2,2,2,2,2,2,2,2,2,2,
2,2,2,2,2,2,2,2,2,2,2,2,2,2,2,2,2,2,2,2,2,2,2,2,2,2,2,2,2,2,2,2,2,2,2,2,
2,2,2,2,2,2,2,2,2,2,2,2,2,2,2,2,2,2,2,2,2,2,2,2,2,2,2,2,2,2,2,2,2,2,2,2,
2,2,2,2,2,2,2,2,2,2,2,2,2,2,2,2,2,2,2,2,2,2,2,2,2,2,2,2,2,2,2,2,2,2,2,2,
2,2,2,2,2,2,2,2,2,2,2,2,2,2,2,2,2,2,2,2,2,2,2,2,2,2,2,2,2,2,2,2,2,2,2,2,
2,2,2,2,2,2,2,2,2,2,2,2,2,2,2,2,2,2,2,2,2,2,2,2,2,2,2,2,2,2,2,2,2,2,2,2,
2,2,2,2,2,2,2,2,2,2,2,2,2,2,2,2,2,2,2,2,2,2,2,2,2,2,2,2,2,2,2,2,2,2,2,2,
2,2,2,2,2,2,2,2,2,2,2,2,2,2,2,2,2,2,2,2,2,2,2,2,2,2,2,2,2,2,2,2,2,2,2,2,
2,2,2,2,2,2,2,2,2,2,2,2,2,2,2,2,2,2,2,2,2,2,2,2,2,2,2,2,2,2,2,2,2,2,2,2,
2,2,2,2,2,2,2,2,2,2,2,2,2,2,2,2,2,2,2,2,2,2,2,2,2,2,2,2,2,2,2,2,2,2,2,2,
2,2,2,2,2,2,2,2,2,2,2,2,2,2,2,2,2,2,2,2,2,2,2,2,2,2,2,2,2,2,2,2,2,2,2,2,
2,2,2,2,2,2,2,2,2,2,2,2,2,2,2,2,2,2,2,2,2,2,2,2,2,2,2,2,2,2,2,2,2,2,2,2,
2,2,2,2,2,2,2,2,2,2,2,2,2,2,2,2,2,2,2,2,2,2,2,2,2,2,2,2,2,2,2,2,2,2,2,2,
2,2,2,2,2,2,2,2,2,2,2,2,2,2,2,2,2,2,2,2,2,2,2,2,2,2,2,2,2,2,2,2,2,2,2,2,
2,2,2,2,2,2,2,2,2,2,2,2,2,2,2,2,2,2,2,2,2,2,2,2,2,2,2,2,2,2,2,2,2,2,2,2,
2,2,2,2,2,2,2,2,2,2,2,2,2,2,2,2,2,2,2,2,2,2,2,2,2,2,2,2,2,2,2,2,2,2,2,2,
2,2,2,2,2,2,2,2,2,2,2,2,2,2,2,2,2,2,2,2,2,2,2,2,2,2,2,2,2,2,2,2,2,2,2,2,
2,2,2,2,2,2,2,2,2,2,2,2,2,2,2,2,2,2,2,2,2,2,2,2,2,2,2,2,2,2,2,2,2,2,2,2,
2,2,2,2,2,2,2,2,2,2,2,2,2,2,2,2,2,3),(0.,1.),(0.,0.000980392156862745,0.00196078431372549,
0.00294117647058824,0.00392156862745098,0.00490196078431373,0.00588235294117647,
0.00686274509803922,0.00784313725490196,0.00882352941176471,0.00980392156862745,
0.0107843137254902,0.0117647058823529,0.0127450980392157,0.0137254901960784,
0.0147058823529412,0.0156862745098039,0.0166666666666667,0.0176470588235294,
0.0186274509803922,0.0196078431372549,0.0205882352941176,0.0215686274509804,
0.0225490196078431,0.0235294117647059,0.0245098039215686,0.0254901960784314,
0.0264705882352941,0.0274509803921569,0.0284313725490196,0.0294117647058824,
0.0303921568627451,0.0313725490196078,0.0323529411764706,0.0333333333333333,
0.0343137254901961,0.0352941176470588,0.0362745098039216,0.0372549019607843,
0.0382352941176471,0.0392156862745098,0.0401960784313726,0.0411764705882353,
0.042156862745098,0.0431372549019608,0.0441176470588235,0.0450980392156863,
0.046078431372549,0.0470588235294118,0.0480392156862745,0.0490196078431373,
0.05,0.0509803921568627,0.0519607843137255,0.0529411764705882,0.053921568627451,
0.0549019607843137,0.0558823529411765,0.0568627450980392,0.057843137254902,
0.0588235294117647,0.0598039215686275,0.0607843137254902,0.0617647058823529,
0.0627450980392157,0.0637254901960784,0.0647058823529412,0.0656862745098039,
0.0666666666666667,0.0676470588235294,0.0686274509803922,0.0696078431372549,
0.0705882352941176,0.0715686274509804,0.0725490196078431,0.0735294117647059,
0.0745098039215686,0.0754901960784314,0.0764705882352941,0.0774509803921569,
0.0784313725490196,0.0794117647058823,0.0803921568627451,0.0813725490196078,
0.0823529411764706,0.0833333333333333,0.0843137254901961,0.0852941176470588,
0.0862745098039216,0.0872549019607843,0.0882352941176471,0.0892156862745098,
0.0901960784313725,0.0911764705882353,0.092156862745098,0.0931372549019608,
0.0941176470588235,0.0950980392156863,0.096078431372549,0.0970588235294118,
0.0980392156862745,0.0990196078431373,0.1,0.100980392156863,0.101960784313725,
0.102941176470588,0.103921568627451,0.104901960784314,0.105882352941176,
0.106862745098039,0.107843137254902,0.108823529411765,0.109803921568627,
0.11078431372549,0.111764705882353,0.112745098039216,0.113725490196078,
0.114705882352941,0.115686274509804,0.116666666666667,0.117647058823529,
0.118627450980392,0.119607843137255,0.120588235294118,0.12156862745098,
0.122549019607843,0.123529411764706,0.124509803921569,0.125490196078431,
0.126470588235294,0.127450980392157,0.12843137254902,0.129411764705882,
0.130392156862745,0.131372549019608,0.132352941176471,0.133333333333333,
0.134313725490196,0.135294117647059,0.136274509803922,0.137254901960784,
0.138235294117647,0.13921568627451,0.140196078431373,0.141176470588235,
0.142156862745098,0.143137254901961,0.144117647058824,0.145098039215686,
0.146078431372549,0.147058823529412,0.148039215686275,0.149019607843137,
0.15,0.150980392156863,0.151960784313725,0.152941176470588,0.153921568627451,
0.154901960784314,0.155882352941176,0.156862745098039,0.157843137254902,
0.158823529411765,0.159803921568627,0.16078431372549,0.161764705882353,
0.162745098039216,0.163725490196078,0.164705882352941,0.165686274509804,
0.166666666666667,0.167647058823529,0.168627450980392,0.169607843137255,
0.170588235294118,0.17156862745098,0.172549019607843,0.173529411764706,
0.174509803921569,0.175490196078431,0.176470588235294,0.177450980392157,
0.17843137254902,0.179411764705882,0.180392156862745,0.181372549019608,
0.182352941176471,0.183333333333333,0.184313725490196,0.185294117647059,
0.186274509803922,0.187254901960784,0.188235294117647,0.18921568627451,
0.190196078431373,0.191176470588235,0.192156862745098,0.193137254901961,
0.194117647058824,0.195098039215686,0.196078431372549,0.197058823529412,
0.198039215686275,0.199019607843137,0.2,0.200980392156863,0.201960784313725,
0.202941176470588,0.203921568627451,0.204901960784314,0.205882352941176,
0.206862745098039,0.207843137254902,0.208823529411765,0.209803921568627,
0.21078431372549,0.211764705882353,0.212745098039216,0.213725490196078,
0.214705882352941,0.215686274509804,0.216666666666667,0.217647058823529,
0.218627450980392,0.219607843137255,0.220588235294118,0.22156862745098,
0.222549019607843,0.223529411764706,0.224509803921569,0.225490196078431,
0.226470588235294,0.227450980392157,0.22843137254902,0.229411764705882,
0.230392156862745,0.231372549019608,0.232352941176471,0.233333333333333,
0.234313725490196,0.235294117647059,0.236274509803922,0.237254901960784,
0.238235294117647,0.23921568627451,0.240196078431373,0.241176470588235,
0.242156862745098,0.243137254901961,0.244117647058824,0.245098039215686,
0.246078431372549,0.247058823529412,0.248039215686275,0.249019607843137,
0.25,0.250980392156863,0.251960784313725,0.252941176470588,0.253921568627451,
0.254901960784314,0.255882352941176,0.256862745098039,0.257843137254902,
0.258823529411765,0.259803921568627,0.26078431372549,0.261764705882353,
0.262745098039216,0.263725490196078,0.264705882352941,0.265686274509804,
0.266666666666667,0.267647058823529,0.268627450980392,0.269607843137255,
0.270588235294118,0.27156862745098,0.272549019607843,0.273529411764706,
0.274509803921569,0.275490196078431,0.276470588235294,0.277450980392157,
0.27843137254902,0.279411764705882,0.280392156862745,0.281372549019608,
0.282352941176471,0.283333333333333,0.284313725490196,0.285294117647059,
0.286274509803922,0.287254901960784,0.288235294117647,0.28921568627451,
0.290196078431373,0.291176470588235,0.292156862745098,0.293137254901961,
0.294117647058824,0.295098039215686,0.296078431372549,0.297058823529412,
0.298039215686275,0.299019607843137,0.3,0.300980392156863,0.301960784313725,
0.302941176470588,0.303921568627451,0.304901960784314,0.305882352941176,
0.306862745098039,0.307843137254902,0.308823529411765,0.309803921568627,
0.31078431372549,0.311764705882353,0.312745098039216,0.313725490196078,
0.314705882352941,0.315686274509804,0.316666666666667,0.317647058823529,
0.318627450980392,0.319607843137255,0.320588235294118,0.32156862745098,
0.322549019607843,0.323529411764706,0.324509803921569,0.325490196078431,
0.326470588235294,0.327450980392157,0.32843137254902,0.329411764705882,
0.330392156862745,0.331372549019608,0.332352941176471,0.333333333333333,
0.334313725490196,0.335294117647059,0.336274509803922,0.337254901960784,
0.338235294117647,0.33921568627451,0.340196078431373,0.341176470588235,
0.342156862745098,0.343137254901961,0.344117647058824,0.345098039215686,
0.346078431372549,0.347058823529412,0.348039215686274,0.349019607843137,
0.35,0.350980392156863,0.351960784313726,0.352941176470588,0.353921568627451,
0.354901960784314,0.355882352941176,0.356862745098039,0.357843137254902,
0.358823529411765,0.359803921568627,0.36078431372549,0.361764705882353,
0.362745098039216,0.363725490196078,0.364705882352941,0.365686274509804,
0.366666666666667,0.367647058823529,0.368627450980392,0.369607843137255,
0.370588235294118,0.37156862745098,0.372549019607843,0.373529411764706,
0.374509803921569,0.375490196078431,0.376470588235294,0.377450980392157,
0.37843137254902,0.379411764705882,0.380392156862745,0.381372549019608,
0.382352941176471,0.383333333333333,0.384313725490196,0.385294117647059,
0.386274509803922,0.387254901960784,0.388235294117647,0.38921568627451,
0.390196078431373,0.391176470588235,0.392156862745098,0.393137254901961,
0.394117647058824,0.395098039215686,0.396078431372549,0.397058823529412,
0.398039215686274,0.399019607843137,0.4,0.400980392156863,0.401960784313726,
0.402941176470588,0.403921568627451,0.404901960784314,0.405882352941176,
0.406862745098039,0.407843137254902,0.408823529411765,0.409803921568627,
0.41078431372549,0.411764705882353,0.412745098039216,0.413725490196078,
0.414705882352941,0.415686274509804,0.416666666666667,0.417647058823529,
0.418627450980392,0.419607843137255,0.420588235294118,0.42156862745098,
0.422549019607843,0.423529411764706,0.424509803921569,0.425490196078431,
0.426470588235294,0.427450980392157,0.42843137254902,0.429411764705882,
0.430392156862745,0.431372549019608,0.432352941176471,0.433333333333333,
0.434313725490196,0.435294117647059,0.436274509803922,0.437254901960784,
0.438235294117647,0.43921568627451,0.440196078431373,0.441176470588235,
0.442156862745098,0.443137254901961,0.444117647058824,0.445098039215686,
0.446078431372549,0.447058823529412,0.448039215686275,0.449019607843137,
0.45,0.450980392156863,0.451960784313725,0.452941176470588,0.453921568627451,
0.454901960784314,0.455882352941176,0.456862745098039,0.457843137254902,
0.458823529411765,0.459803921568627,0.46078431372549,0.461764705882353,
0.462745098039216,0.463725490196078,0.464705882352941,0.465686274509804,
0.466666666666667,0.467647058823529,0.468627450980392,0.469607843137255,
0.470588235294118,0.47156862745098,0.472549019607843,0.473529411764706,
0.474509803921569,0.475490196078431,0.476470588235294,0.477450980392157,
0.47843137254902,0.479411764705882,0.480392156862745,0.481372549019608,
0.482352941176471,0.483333333333333,0.484313725490196,0.485294117647059,
0.486274509803922,0.487254901960784,0.488235294117647,0.48921568627451,
0.490196078431373,0.491176470588235,0.492156862745098,0.493137254901961,
0.494117647058824,0.495098039215686,0.496078431372549,0.497058823529412,
0.498039215686275,0.499019607843137,0.5,0.500980392156863,0.501960784313725,
0.502941176470588,0.503921568627451,0.504901960784314,0.505882352941176,
0.506862745098039,0.507843137254902,0.508823529411765,0.509803921568627,
0.51078431372549,0.511764705882353,0.512745098039216,0.513725490196078,
0.514705882352941,0.515686274509804,0.516666666666667,0.517647058823529,
0.518627450980392,0.519607843137255,0.520588235294118,0.52156862745098,
0.522549019607843,0.523529411764706,0.524509803921569,0.525490196078431,
0.526470588235294,0.527450980392157,0.52843137254902,0.529411764705882,
0.530392156862745,0.531372549019608,0.532352941176471,0.533333333333333,
0.534313725490196,0.535294117647059,0.536274509803922,0.537254901960784,
0.538235294117647,0.53921568627451,0.540196078431373,0.541176470588235,
0.542156862745098,0.543137254901961,0.544117647058823,0.545098039215686,
0.546078431372549,0.547058823529412,0.548039215686275,0.549019607843137,
0.55,0.550980392156863,0.551960784313726,0.552941176470588,0.553921568627451,
0.554901960784314,0.555882352941176,0.556862745098039,0.557843137254902,
0.558823529411765,0.559803921568627,0.56078431372549,0.561764705882353,
0.562745098039216,0.563725490196078,0.564705882352941,0.565686274509804,
0.566666666666667,0.567647058823529,0.568627450980392,0.569607843137255,
0.570588235294118,0.57156862745098,0.572549019607843,0.573529411764706,
0.574509803921569,0.575490196078431,0.576470588235294,0.577450980392157,
0.57843137254902,0.579411764705882,0.580392156862745,0.581372549019608,
0.582352941176471,0.583333333333333,0.584313725490196,0.585294117647059,
0.586274509803922,0.587254901960784,0.588235294117647,0.58921568627451,
0.590196078431373,0.591176470588235,0.592156862745098,0.593137254901961,
0.594117647058824,0.595098039215686,0.596078431372549,0.597058823529412,
0.598039215686274,0.599019607843137,0.6,0.600980392156863,0.601960784313725,
0.602941176470588,0.603921568627451,0.604901960784314,0.605882352941176,
0.606862745098039,0.607843137254902,0.608823529411765,0.609803921568628,
0.61078431372549,0.611764705882353,0.612745098039216,0.613725490196078,
0.614705882352941,0.615686274509804,0.616666666666667,0.617647058823529,
0.618627450980392,0.619607843137255,0.620588235294118,0.62156862745098,
0.622549019607843,0.623529411764706,0.624509803921569,0.625490196078431,
0.626470588235294,0.627450980392157,0.62843137254902,0.629411764705882,
0.630392156862745,0.631372549019608,0.632352941176471,0.633333333333333,
0.634313725490196,0.635294117647059,0.636274509803922,0.637254901960784,
0.638235294117647,0.63921568627451,0.640196078431372,0.641176470588235,
0.642156862745098,0.643137254901961,0.644117647058824,0.645098039215686,
0.646078431372549,0.647058823529412,0.648039215686275,0.649019607843137,
0.65,0.650980392156863,0.651960784313726,0.652941176470588,0.653921568627451,
0.654901960784314,0.655882352941176,0.656862745098039,0.657843137254902,
0.658823529411765,0.659803921568627,0.66078431372549,0.661764705882353,
0.662745098039216,0.663725490196078,0.664705882352941,0.665686274509804,
0.666666666666667,0.667647058823529,0.668627450980392,0.669607843137255,
0.670588235294118,0.67156862745098,0.672549019607843,0.673529411764706,
0.674509803921569,0.675490196078431,0.676470588235294,0.677450980392157,
0.67843137254902,0.679411764705882,0.680392156862745,0.681372549019608,
0.682352941176471,0.683333333333333,0.684313725490196,0.685294117647059,
0.686274509803922,0.687254901960784,0.688235294117647,0.68921568627451,
0.690196078431373,0.691176470588235,0.692156862745098,0.693137254901961,
0.694117647058824,0.695098039215686,0.696078431372549,0.697058823529412,
0.698039215686274,0.699019607843137,0.7,0.700980392156863,0.701960784313725,
0.702941176470588,0.703921568627451,0.704901960784314,0.705882352941177,
0.706862745098039,0.707843137254902,0.708823529411765,0.709803921568627,
0.71078431372549,0.711764705882353,0.712745098039216,0.713725490196078,
0.714705882352941,0.715686274509804,0.716666666666667,0.717647058823529,
0.718627450980392,0.719607843137255,0.720588235294118,0.72156862745098,
0.722549019607843,0.723529411764706,0.724509803921569,0.725490196078431,
0.726470588235294,0.727450980392157,0.72843137254902,0.729411764705882,
0.730392156862745,0.731372549019608,0.732352941176471,0.733333333333333,
0.734313725490196,0.735294117647059,0.736274509803922,0.737254901960784,
0.738235294117647,0.73921568627451,0.740196078431373,0.741176470588235,
0.742156862745098,0.743137254901961,0.744117647058824,0.745098039215686,
0.746078431372549,0.747058823529412,0.748039215686275,0.749019607843137,
0.75,0.750980392156863,0.751960784313725,0.752941176470588,0.753921568627451,
0.754901960784314,0.755882352941176,0.756862745098039,0.757843137254902,
0.758823529411765,0.759803921568627,0.76078431372549,0.761764705882353,
0.762745098039216,0.763725490196078,0.764705882352941,0.765686274509804,
0.766666666666667,0.767647058823529,0.768627450980392,0.769607843137255,
0.770588235294118,0.77156862745098,0.772549019607843,0.773529411764706,
0.774509803921569,0.775490196078431,0.776470588235294,0.777450980392157,
0.77843137254902,0.779411764705882,0.780392156862745,0.781372549019608,
0.782352941176471,0.783333333333333,0.784313725490196,0.785294117647059,
0.786274509803922,0.787254901960784,0.788235294117647,0.78921568627451,
0.790196078431373,0.791176470588235,0.792156862745098,0.793137254901961,
0.794117647058823,0.795098039215686,0.796078431372549,0.797058823529412,
0.798039215686275,0.799019607843137,0.8,0.800980392156863,0.801960784313726,
0.802941176470588,0.803921568627451,0.804901960784314,0.805882352941176,
0.806862745098039,0.807843137254902,0.808823529411765,0.809803921568627,
0.81078431372549,0.811764705882353,0.812745098039216,0.813725490196078,
0.814705882352941,0.815686274509804,0.816666666666667,0.817647058823529,
0.818627450980392,0.819607843137255,0.820588235294118,0.82156862745098,
0.822549019607843,0.823529411764706,0.824509803921569,0.825490196078431,
0.826470588235294,0.827450980392157,0.82843137254902,0.829411764705882,
0.830392156862745,0.831372549019608,0.832352941176471,0.833333333333333,
0.834313725490196,0.835294117647059,0.836274509803922,0.837254901960784,
0.838235294117647,0.83921568627451,0.840196078431373,0.841176470588235,
0.842156862745098,0.843137254901961,0.844117647058824,0.845098039215686,
0.846078431372549,0.847058823529412,0.848039215686274,0.849019607843137,
0.85,0.850980392156863,0.851960784313725,0.852941176470588,0.853921568627451,
0.854901960784314,0.855882352941176,0.856862745098039,0.857843137254902,
0.858823529411765,0.859803921568628,0.86078431372549,0.861764705882353,
0.862745098039216,0.863725490196078,0.864705882352941,0.865686274509804,
0.866666666666667,0.867647058823529,0.868627450980392,0.869607843137255,
0.870588235294118,0.87156862745098,0.872549019607843,0.873529411764706,
0.874509803921569,0.875490196078431,0.876470588235294,0.877450980392157,
0.87843137254902,0.879411764705882,0.880392156862745,0.881372549019608,
0.882352941176471,0.883333333333333,0.884313725490196,0.885294117647059,
0.886274509803922,0.887254901960784,0.888235294117647,0.88921568627451,
0.890196078431372,0.891176470588235,0.892156862745098,0.893137254901961,
0.894117647058824,0.895098039215686,0.896078431372549,0.897058823529412,
0.898039215686275,0.899019607843137,0.9,0.900980392156863,0.901960784313726,
0.902941176470588,0.903921568627451,0.904901960784314,0.905882352941176,
0.906862745098039,0.907843137254902,0.908823529411765,0.909803921568627,
0.91078431372549,0.911764705882353,0.912745098039216,0.913725490196078,
0.914705882352941,0.915686274509804,0.916666666666667,0.917647058823529,
0.918627450980392,0.919607843137255,0.920588235294118,0.92156862745098,
0.922549019607843,0.923529411764706,0.924509803921569,0.925490196078431,
0.926470588235294,0.927450980392157,0.92843137254902,0.929411764705882,
0.930392156862745,0.931372549019608,0.932352941176471,0.933333333333333,
0.934313725490196,0.935294117647059,0.936274509803922,0.937254901960784,
0.938235294117647,0.93921568627451,0.940196078431373,0.941176470588235,
0.942156862745098,0.943137254901961,0.944117647058824,0.945098039215686,
0.946078431372549,0.947058823529412,0.948039215686274,0.949019607843137,
0.95,0.950980392156863,0.951960784313725,0.952941176470588,0.953921568627451,
0.954901960784314,0.955882352941177,0.956862745098039,0.957843137254902,
0.958823529411765,0.959803921568627,0.96078431372549,0.961764705882353,
0.962745098039216,0.963725490196078,0.964705882352941,0.965686274509804,
0.966666666666667,0.967647058823529,0.968627450980392,0.969607843137255,
0.970588235294118,0.97156862745098,0.972549019607843,0.973529411764706,
0.974509803921569,0.975490196078431,0.976470588235294,0.977450980392157,
0.97843137254902,0.979411764705882,0.980392156862745,0.981372549019608,
0.982352941176471,0.983333333333333,0.984313725490196,0.985294117647059,
0.985937314000278,0.995796687140281),.UNSPECIFIED.)
GEOMETRIC_REPRESENTATION_ITEM()
RATIONAL_B_SPLINE_SURFACE(((1.,0.995734176295034,1.,0.995734176295034,1.,
0.995734176295034,1.,0.995734176295034,1.,0.995734176295034,1.,0.995734176295034,
1.,0.995734176295034,1.,0.995734176295034,1.,0.995734176295034,1.,0.995734176295034,
1.,0.995734176295034,1.,0.995734176295034,1.,0.995734176295034,1.,0.995734176295034,
1.,0.995734176295034,1.,0.995734176295034,1.,0.995734176295034,1.,0.995734176295034,
1.,0.995734176295034,1.,0.995734176295034,1.,0.995734176295034,1.,0.995734176295034,
1.,0.995734176295034,1.,0.995734176295034,1.,0.995734176295034,1.,0.995734176295034,
1.,0.995734176295034,1.,0.995734176295034,1.,0.995734176295034,1.,0.995734176295034,
1.,0.995734176295034,1.,0.995734176295034,1.,0.995734176295034,1.,0.995734176295034,
1.,0.995734176295034,1.,0.995734176295034,1.,0.995734176295034,1.,0.995734176295034,
1.,0.995734176295034,1.,0.995734176295034,1.,0.995734176295034,1.,0.995734176295034,
1.,0.995734176295034,1.,0.995734176295034,1.,0.995734176295034,1.,0.995734176295034,
1.,0.995734176295034,1.,0.995734176295034,1.,0.995734176295034,1.,0.995734176295034,
1.,0.995734176295034,1.,0.995734176295034,1.,0.995734176295034,1.,0.995734176295034,
1.,0.995734176295034,1.,0.995734176295034,1.,0.995734176295034,1.,0.995734176295034,
1.,0.995734176295034,1.,0.995734176295034,1.,0.995734176295034,1.,0.995734176295034,
1.,0.995734176295034,1.,0.995734176295034,1.,0.995734176295034,1.,0.995734176295034,
1.,0.995734176295034,1.,0.995734176295034,1.,0.995734176295034,1.,0.995734176295034,
1.,0.995734176295034,1.,0.995734176295034,1.,0.995734176295034,1.,0.995734176295034,
1.,0.995734176295034,1.,0.995734176295034,1.,0.995734176295034,1.,0.995734176295034,
1.,0.995734176295034,1.,0.995734176295034,1.,0.995734176295034,1.,0.995734176295034,
1.,0.995734176295034,1.,0.995734176295034,1.,0.995734176295034,1.,0.995734176295034,
1.,0.995734176295034,1.,0.995734176295034,1.,0.995734176295034,1.,0.995734176295034,
1.,0.995734176295034,1.,0.995734176295034,1.,0.995734176295034,1.,0.995734176295034,
1.,0.995734176295034,1.,0.995734176295034,1.,0.995734176295034,1.,0.995734176295034,
1.,0.995734176295034,1.,0.995734176295034,1.,0.995734176295034,1.,0.995734176295034,
1.,0.995734176295034,1.,0.995734176295034,1.,0.995734176295034,1.,0.995734176295034,
1.,0.995734176295034,1.,0.995734176295034,1.,0.995734176295034,1.,0.995734176295034,
1.,0.995734176295034,1.,0.995734176295034,1.,0.995734176295034,1.,0.995734176295034,
1.,0.995734176295034,1.,0.995734176295034,1.,0.995734176295034,1.,0.995734176295034,
1.,0.995734176295034,1.,0.995734176295034,1.,0.995734176295034,1.,0.995734176295034,
1.,0.995734176295034,1.,0.995734176295034,1.,0.995734176295034,1.,0.995734176295034,
1.,0.995734176295034,1.,0.995734176295034,1.,0.995734176295034,1.,0.995734176295034,
1.,0.995734176295034,1.,0.995734176295034,1.,0.995734176295034,1.,0.995734176295034,
1.,0.995734176295034,1.,0.995734176295034,1.,0.995734176295034,1.,0.995734176295034,
1.,0.995734176295034,1.,0.995734176295034,1.,0.995734176295034,1.,0.995734176295034,
1.,0.995734176295034,1.,0.995734176295034,1.,0.995734176295034,1.,0.995734176295034,
1.,0.995734176295034,1.,0.995734176295034,1.,0.995734176295034,1.,0.995734176295034,
1.,0.995734176295034,1.,0.995734176295034,1.,0.995734176295034,1.,0.995734176295034,
1.,0.995734176295034,1.,0.995734176295034,1.,0.995734176295034,1.,0.995734176295034,
1.,0.995734176295034,1.,0.995734176295034,1.,0.995734176295034,1.,0.995734176295034,
1.,0.995734176295034,1.,0.995734176295034,1.,0.995734176295034,1.,0.995734176295034,
1.,0.995734176295034,1.,0.995734176295034,1.,0.995734176295034,1.,0.995734176295034,
1.,0.995734176295034,1.,0.995734176295034,1.,0.995734176295034,1.,0.995734176295034,
1.,0.995734176295034,1.,0.995734176295034,1.,0.995734176295034,1.,0.995734176295034,
1.,0.995734176295034,1.,0.995734176295034,1.,0.995734176295034,1.,0.995734176295034,
1.,0.995734176295034,1.,0.995734176295034,1.,0.995734176295034,1.,0.995734176295034,
1.,0.995734176295034,1.,0.995734176295034,1.,0.995734176295034,1.,0.995734176295034,
1.,0.995734176295034,1.,0.995734176295034,1.,0.995734176295034,1.,0.995734176295034,
1.,0.995734176295034,1.,0.995734176295034,1.,0.995734176295034,1.,0.995734176295034,
1.,0.995734176295034,1.,0.995734176295034,1.,0.995734176295034,1.,0.995734176295034,
1.,0.995734176295034,1.,0.995734176295034,1.,0.995734176295034,1.,0.995734176295034,
1.,0.995734176295034,1.,0.995734176295034,1.,0.995734176295034,1.,0.995734176295034,
1.,0.995734176295034,1.,0.995734176295034,1.,0.995734176295034,1.,0.995734176295034,
1.,0.995734176295034,1.,0.995734176295034,1.,0.995734176295034,1.,0.995734176295034,
1.,0.995734176295034,1.,0.995734176295034,1.,0.995734176295034,1.,0.995734176295034,
1.,0.995734176295034,1.,0.995734176295034,1.,0.995734176295034,1.,0.995734176295034,
1.,0.995734176295034,1.,0.995734176295034,1.,0.995734176295034,1.,0.995734176295034,
1.,0.995734176295034,1.,0.995734176295034,1.,0.995734176295034,1.,0.995734176295034,
1.,0.995734176295034,1.,0.995734176295034,1.,0.995734176295034,1.,0.995734176295034,
1.,0.995734176295034,1.,0.995734176295034,1.,0.995734176295034,1.,0.995734176295034,
1.,0.995734176295034,1.,0.995734176295034,1.,0.995734176295034,1.,0.995734176295034,
1.,0.995734176295034,1.,0.995734176295034,1.,0.995734176295034,1.,0.995734176295034,
1.,0.995734176295034,1.,0.995734176295034,1.,0.995734176295034,1.,0.995734176295034,
1.,0.995734176295034,1.,0.995734176295034,1.,0.995734176295034,1.,0.995734176295034,
1.,0.995734176295034,1.,0.995734176295034,1.,0.995734176295034,1.,0.995734176295034,
1.,0.995734176295034,1.,0.995734176295034,1.,0.995734176295034,1.,0.995734176295034,
1.,0.995734176295034,1.,0.995734176295034,1.,0.995734176295034,1.,0.995734176295034,
1.,0.995734176295034,1.,0.995734176295034,1.,0.995734176295034,1.,0.995734176295034,
1.,0.995734176295034,1.,0.995734176295034,1.,0.995734176295034,1.,0.995734176295034,
1.,0.995734176295034,1.,0.995734176295034,1.,0.995734176295034,1.,0.995734176295034,
1.,0.995734176295034,1.,0.995734176295034,1.,0.995734176295034,1.,0.995734176295034,
1.,0.995734176295034,1.,0.995734176295034,1.,0.995734176295034,1.,0.995734176295034,
1.,0.995734176295034,1.,0.995734176295034,1.,0.995734176295034,1.,0.995734176295034,
1.,0.995734176295034,1.,0.995734176295034,1.,0.995734176295034,1.,0.995734176295034,
1.,0.995734176295034,1.,0.995734176295034,1.,0.995734176295034,1.,0.995734176295034,
1.,0.995734176295034,1.,0.995734176295034,1.,0.995734176295034,1.,0.995734176295034,
1.,0.995734176295034,1.,0.995734176295034,1.,0.995734176295034,1.,0.995734176295034,
1.,0.995734176295034,1.,0.995734176295034,1.,0.995734176295034,1.,0.995734176295034,
1.,0.995734176295034,1.,0.995734176295034,1.,0.995734176295034,1.,0.995734176295034,
1.,0.995734176295034,1.,0.995734176295034,1.,0.995734176295034,1.,0.995734176295034,
1.,0.995734176295034,1.,0.995734176295034,1.,0.995734176295034,1.,0.995734176295034,
1.,0.995734176295034,1.,0.995734176295034,1.,0.995734176295034,1.,0.995734176295034,
1.,0.995734176295034,1.,0.995734176295034,1.,0.995734176295034,1.,0.995734176295034,
1.,0.995734176295034,1.,0.995734176295034,1.,0.995734176295034,1.,0.995734176295034,
1.,0.995734176295034,1.,0.995734176295034,1.,0.995734176295034,1.,0.995734176295034,
1.,0.995734176295034,1.,0.995734176295034,1.,0.995734176295034,1.,0.995734176295034,
1.,0.995734176295034,1.,0.995734176295034,1.,0.995734176295034,1.,0.995734176295034,
1.,0.995734176295034,1.,0.995734176295034,1.,0.995734176295034,1.,0.995734176295034,
1.,0.995734176295034,1.,0.995734176295034,1.,0.995734176295034,1.,0.995734176295034,
1.,0.995734176295034,1.,0.995734176295034,1.,0.995734176295034,1.,0.995734176295034,
1.,0.995734176295034,1.,0.995734176295034,1.,0.995734176295034,1.,0.995734176295034,
1.,0.995734176295034,1.,0.995734176295034,1.,0.995734176295034,1.,0.995734176295034,
1.,0.995734176295034,1.,0.995734176295034,1.,0.995734176295034,1.,0.995734176295034,
1.,0.995734176295034,1.,0.995734176295034,1.,0.995734176295034,1.,0.995734176295034,
1.,0.995734176295034,1.,0.995734176295034,1.,0.995734176295034,1.,0.995734176295034,
1.,0.995734176295034,1.,0.995734176295034,1.,0.995734176295034,1.,0.995734176295034,
1.,0.995734176295034,1.,0.995734176295034,1.,0.995734176295034,1.,0.995734176295034,
1.,0.995734176295034,1.,0.995734176295034,1.,0.995734176295034,1.,0.995734176295034,
1.,0.995734176295034,1.,0.995734176295034,1.,0.995734176295034,1.,0.995734176295034,
1.,0.995734176295034,1.,0.995734176295034,1.,0.995734176295034,1.,0.995734176295034,
1.,0.995734176295034,1.,0.995734176295034,1.,0.995734176295034,1.,0.995734176295034,
1.,0.995734176295034,1.,0.995734176295034,1.,0.995734176295034,1.,0.995734176295034,
1.,0.995734176295034,1.,0.995734176295034,1.,0.995734176295034,1.,0.995734176295034,
1.,0.995734176295034,1.,0.995734176295034,1.,0.995734176295034,1.,0.995734176295034,
1.,0.995734176295034,1.,0.995734176295034,1.,0.995734176295034,1.,0.995734176295034,
1.,0.995734176295034,1.,0.995734176295034,1.,0.995734176295034,1.,0.995734176295034,
1.,0.995734176295034,1.,0.995734176295034,1.,0.995734176295034,1.,0.995734176295034,
1.,0.995734176295034,1.,0.995734176295034,1.,0.995734176295034,1.,0.995734176295034,
1.,0.995734176295034,1.,0.995734176295034,1.,0.995734176295034,1.,0.995734176295034,
1.,0.995734176295034,1.,0.995734176295034,1.,0.995734176295034,1.,0.995734176295034,
1.,0.995734176295034,1.,0.995734176295034,1.,0.995734176295034,1.,0.995734176295034,
1.,0.995734176295034,1.,0.995734176295034,1.,0.995734176295034,1.,0.995734176295034,
1.,0.995734176295034,1.,0.995734176295034,1.,0.995734176295034,1.,0.995734176295034,
1.,0.995734176295034,1.,0.995734176295034,1.,0.995734176295034,1.,0.995734176295034,
1.,0.995734176295034,1.,0.995734176295034,1.,0.995734176295034,1.,0.995734176295034,
1.,0.995734176295034,1.,0.995734176295034,1.,0.995734176295034,1.,0.995734176295034,
1.,0.995734176295034,1.,0.995734176295034,1.,0.995734176295034,1.,0.995734176295034,
1.,0.995734176295034,1.,0.995734176295034,1.,0.995734176295034,1.,0.995734176295034,
1.,0.995734176295034,1.,0.995734176295034,1.,0.995734176295034,1.,0.995734176295034,
1.,0.995734176295034,1.,0.995734176295034,1.,0.995734176295034,1.,0.995734176295034,
1.,0.995734176295034,1.,0.995734176295034,1.,0.995734176295034,1.,0.995734176295034,
1.,0.995734176295034,1.,0.995734176295034,1.,0.995734176295034,1.,0.995734176295034,
1.,0.995734176295034,1.,0.995734176295034,1.,0.995734176295034,1.,0.995734176295034,
1.,0.995734176295034,1.,0.995734176295034,1.,0.995734176295034,1.,0.995734176295034,
1.,0.995734176295034,1.,0.995734176295034,1.,0.995734176295034,1.,0.995734176295034,
1.,0.995734176295034,1.,0.995734176295034,1.,0.995734176295034,1.,0.995734176295034,
1.,0.995734176295034,1.,0.995734176295034,1.,0.995734176295034,1.,0.995734176295034,
1.,0.995734176295034,1.,0.995734176295034,1.,0.995734176295034,1.,0.995734176295034,
1.,0.995734176295034,1.,0.995734176295034,1.,0.995734176295034,1.,0.995734176295034,
1.,0.995734176295034,1.,0.995734176295034,1.,0.995734176295034,1.,0.995734176295034,
1.,0.995734176295034,1.,0.995734176295034,1.,0.995734176295034,1.,0.995734176295034,
1.,0.995734176295034,1.,0.995734176295034,1.,0.995734176295034,1.,0.995734176295034,
1.,0.995734176295034,1.,0.995734176295034,1.,0.995734176295034,1.,0.995734176295034,
1.,0.995734176295034,1.,0.995734176295034,1.,0.995734176295034,1.,0.995734176295034,
1.,0.995734176295034,1.,0.995734176295034,1.,0.995734176295034,1.,0.995734176295034,
1.,0.995734176295034,1.,0.995734176295034,1.,0.995734176295034,1.,0.995734176295034,
1.,0.995734176295034,1.,0.995734176295034,1.,0.995734176295034,1.,0.995734176295034,
1.,0.995734176295034,1.,0.995734176295034,1.,0.995734176295034,1.,0.995734176295034,
1.,0.995734176295034,1.,0.995734176295034,1.,0.995734176295034,1.,0.995734176295034,
1.,0.995734176295034,1.,0.995734176295034,1.,0.995734176295034,1.,0.995734176295034,
1.,0.995734176295034,1.,0.995734176295034,1.,0.995734176295034,1.,0.995734176295034,
1.,0.995734176295034,1.,0.995734176295034,1.,0.995734176295034,1.,0.995734176295034,
1.,0.995734176295034,1.,0.995734176295034,1.,0.995734176295034,1.,0.995734176295034,
1.,0.995734176295034,1.,0.995734176295034,1.,0.995734176295034,1.,0.995734176295034,
1.,0.995734176295034,1.,0.995734176295034,1.,0.995734176295034,1.,0.995734176295034,
1.,0.995734176295034,1.,0.995734176295034,1.,0.995734176295034,1.,0.995734176295034,
1.,0.995734176295034,1.,0.995734176295034,1.,0.995734176295034,1.,0.995734176295034,
1.,0.995734176295034,1.,0.995734176295034,1.,0.995734176295034,1.,0.995734176295034,
1.,0.995734176295034,1.,0.995734176295034,1.,0.995734176295034,1.,0.995734176295034,
1.,0.995734176295034,1.,0.995734176295034,1.,0.995734176295034,1.,0.995734176295034,
1.,0.995734176295034,1.,0.995734176295034,1.,0.995734176295034,1.,0.995734176295034,
1.,0.995734176295034,1.,0.995734176295034,1.,0.995734176295034,1.,0.995734176295034,
1.,0.995734176295034,1.,0.995734176295034,1.,0.995734176295034,1.,0.995734176295034,
1.,0.995734176295034,1.,0.995734176295034,1.,0.995734176295034,1.,0.995734176295034,
1.,0.995734176295034,1.,0.995734176295034,1.,0.995734176295034,1.,0.995734176295034,
1.,0.995734176295034,1.,0.995734176295034,1.,0.995734176295034,1.,0.995734176295034,
1.,0.995734176295034,1.,0.995734176295034,1.,0.995734176295034,1.,0.995734176295034,
1.,0.995734176295034,1.,0.995734176295034,1.,0.995734176295034,1.,0.995734176295034,
1.,0.995734176295034,1.,0.995734176295034,1.,0.995734176295034,1.,0.995734176295034,
1.,0.995734176295034,1.,0.995734176295034,1.,0.995734176295034,1.,0.995734176295034,
1.,0.995734176295034,1.,0.995734176295034,1.,0.995734176295034,1.,0.995734176295034,
1.,0.995734176295034,1.,0.995734176295034,1.,0.995734176295034,1.,0.995734176295034,
1.,0.995734176295034,1.,0.995734176295034,1.,0.995734176295034,1.,0.995734176295034,
1.,0.995734176295034,1.,0.995734176295034,1.,0.995734176295034,1.,0.995734176295034,
1.,0.995734176295034,1.,0.995734176295034,1.,0.995734176295034,1.,0.995734176295034,
1.,0.995734176295034,1.,0.995734176295034,1.,0.995734176295034,1.,0.995734176295034,
1.,0.995734176295034,1.,0.995734176295034,1.,0.995734176295034,1.,0.995734176295034,
1.,0.995734176295034,1.,0.995734176295034,1.,0.995734176295034,1.,0.995734176295034,
1.,0.995734176295034,1.,0.995734176295034,1.,0.995734176295034,1.,0.995734176295034,
1.,0.995734176295034,1.,0.995734176295034,1.,0.995734176295034,1.,0.995734176295034,
1.,0.995734176295034,1.,0.995734176295034,1.,0.995734176295034,1.,0.995734176295034,
1.,0.995734176295034,1.,0.995734176295034,1.,0.995734176295034,1.,0.995734176295034,
1.,0.995734176295034,1.,0.995734176295034,1.,0.995734176295034,1.,0.995734176295034,
1.,0.995734176295034,1.,0.995734176295034,1.,0.995734176295034,1.,0.995734176295034,
1.,0.995734176295034,1.,0.995734176295034,1.,0.995734176295034,1.,0.995734176295034,
1.,0.995734176295034,1.,0.995734176295034,1.,0.995734176295034,1.,0.995734176295034,
1.,0.995734176295034,1.,0.995734176295034,1.,0.995734176295034,1.,0.995734176295034,
1.,0.995734176295034,1.,0.995734176295034,1.,0.995734176295034,1.,0.995734176295034,
1.,0.995734176295034,1.,0.995734176295034,1.,0.995734176295034,1.,0.995734176295034,
1.,0.995734176295034,1.,0.995734176295034,1.,0.995734176295034,1.,0.995734176295034,
1.,0.995734176295034,1.,0.995734176295034,1.,0.995734176295034,1.,0.995734176295034,
1.,0.995734176295034,1.,0.995734176295034,1.,0.995734176295034,1.,0.995734176295034,
1.,0.995734176295034,1.,0.995734176295034,1.,0.995734176295034,1.,0.995734176295034,
1.,0.995734176295034,1.,0.995734176295034,1.,0.995734176295034,1.,0.995734176295034,
1.,0.995734176295034,1.,0.995734176295034,1.,0.995734176295034,1.,0.995734176295034,
1.,0.995734176295034,1.,0.995734176295034,1.,0.995734176295034,1.,0.995734176295034,
1.,0.995734176295034,1.,0.995734176295034,1.,0.995734176295034,1.,0.995734176295034,
1.,0.995734176295034,1.,0.995734176295034,1.,0.995734176295034,1.,0.995734176295034,
1.,0.995734176295034,1.,0.995734176295034,1.,0.995734176295034,1.,0.995734176295034,
1.,0.995734176295034,1.,0.995734176295034,1.,0.995734176295034,1.,0.995734176295034,
1.,0.995734176295034,1.,0.995734176295034,1.,0.995734176295034,1.,0.995734176295034,
1.,0.995734176295034,1.,0.995734176295034,1.,0.995734176295034,1.,0.995734176295034,
1.,0.995734176295034,1.,0.995734176295034,1.,0.995734176295034,1.,0.995734176295034,
1.,0.995734176295034,1.,0.995734176295034,1.,0.995734176295034,1.,0.995734176295034,
1.,0.995734176295034,1.,0.995734176295034,1.,0.995734176295034,1.,0.995734176295034,
1.,0.995734176295034,1.,0.995734176295034,1.,0.995734176295034,1.,0.995734176295034,
1.,0.995734176295034,1.,0.995734176295034,1.,0.995734176295034,1.,0.995734176295034,
1.,0.995734176295034,1.,0.995734176295034,1.,0.995734176295034,1.,0.995734176295034,
1.,0.995734176295034,1.,0.995734176295034,1.,0.995734176295034,1.,0.995734176295034,
1.,0.995734176295034,1.,0.995734176295034,1.,0.995734176295034,1.,0.995734176295034,
1.,0.995734176295034,1.,0.995734176295034,1.,0.995734176295034,1.,0.995734176295034,
1.,0.995734176295034,1.,0.995734176295034,1.,0.995734176295034,1.,0.995734176295034,
1.,0.995734176295034,1.,0.995734176295034,1.,0.995734176295034,1.,0.995734176295034,
1.,0.995734176295034,1.,0.995734176295034,1.,0.995734176295034,1.,0.995734176295034,
1.,0.995734176295034,1.,0.995734176295034,1.,0.995734176295034,1.,0.995734176295034,
1.,0.995734176295034,1.,0.995734176295034,1.,0.995734176295034,1.,0.995734176295034,
1.,0.995734176295034,1.,0.995734176295034,1.,0.995734176295034,1.,0.995734176295034,
1.,0.995734176295034,1.,0.995734176295034,1.,0.995734176295034,1.,0.995734176295034,
1.,0.995734176295034,1.,0.995734176295034,1.,0.995734176295034,1.,0.995734176295034,
1.,0.995734176295034,1.,0.995734176295034,1.,0.995734176295034,1.,0.995734176295034,
1.,0.995734176295034,1.,0.995734176295034,1.,0.995734176295034,1.,0.995734176295034,
1.,0.995734176295034,1.,0.995734176295034,1.,0.995734176295034,1.,0.995734176295034,
1.,0.995734176295034,1.,0.995734176295034,1.,0.995734176295034,1.,0.995734176295034,
1.,0.995734176295034,1.,0.995734176295034,1.,0.995734176295034,1.,0.995734176295034,
1.,0.995734176295034,1.,0.995734176295034,1.,0.995734176295034,1.,0.995734176295034,
1.,0.995734176295034,1.,0.995734176295034,1.,0.995734176295034,1.,0.995734176295034,
1.,0.995734176295034,1.,0.995734176295034,1.,0.995734176295034,1.,0.995734176295034,
1.,0.995734176295034,1.,0.995734176295034,1.,0.995734176295034,1.,0.995734176295034,
1.,0.995734176295034,1.,0.995734176295034,1.,0.995734176295034,1.,0.995734176295034,
1.,0.995734176295034,1.,0.995734176295034,1.,0.995734176295034,1.,0.995734176295034,
1.,0.995734176295034,1.,0.995734176295034,1.,0.995734176295034,1.,0.995734176295034,
1.,0.995734176295034,1.,0.995734176295034,1.,0.995734176295034,1.,0.995734176295034,
1.,0.995734176295034,1.,0.995734176295034,1.,0.995734176295034,1.,0.995734176295034,
1.,0.995734176295034,1.,0.995734176295034,1.,0.995734176295034,1.,0.995734176295034,
1.,0.995734176295034,1.,0.995734176295034,1.,0.995734176295034,1.,0.995734176295034,
1.,0.995734176295034,1.,0.995734176295034,1.,0.995734176295034,1.,0.995734176295034,
1.,0.995734176295034,1.,0.995734176295034,1.,0.995734176295034,1.,0.995734176295034,
1.,0.995734176295034,1.,0.995734176295034,1.,0.995734176295034,1.,0.995734176295034,
1.,0.995734176295034,1.,0.995734176295034,1.,0.995734176295034,1.,0.995734176295034,
1.,0.995734176295034,1.,0.995734176295034,1.,0.995734176295034,1.,0.995734176295034,
1.,0.995734176295034,1.,0.995734176295034,1.,0.995734176295034,1.,0.995734176295034,
1.,0.995734176295034,1.,0.995734176295034,1.,0.995734176295034,1.,0.995734176295034,
1.,0.995734176295034,1.,0.995734176295034,1.,0.995734176295034,1.,0.995734176295034,
1.,0.995734176295034,1.,0.995734176295034,1.,0.995734176295034,1.,0.995734176295034,
1.,0.995734176295034,1.,0.995734176295034,1.,0.995734176295034,1.,0.995734176295034,
1.,0.995734176295034,1.,0.995734176295034,1.,0.995734176295034,1.,0.995734176295034,
1.,0.995734176295034,1.,0.995734176295034,1.,0.995734176295034,1.,0.995734176295034,
1.,0.995734176295034,1.,0.995734176295034,1.,0.995734176295034,1.,0.995734176295034,
1.,0.995734176295034,1.,0.995734176295034,1.,0.995734176295034,1.,0.995734176295034,
1.,0.995734176295034,1.,0.995734176295034,1.,0.995734176295034,1.,0.995734176295034,
1.,0.995734176295034,1.,0.995734176295034,1.,0.995734176295034,1.,0.995734176295034,
1.,0.995734176295034,1.,0.995734176295034,1.,0.995734176295034,1.,0.995734176295034,
1.,0.995734176295034,1.,0.995734176295034,1.,0.995734176295034,1.,0.995734176295034,
1.,0.995734176295034,1.,0.995734176295034,1.,0.995734176295034,1.,0.995734176295034,
1.,0.995734176295034,1.,0.995734176295034,1.,0.995734176295034,1.,0.995734176295034,
1.,0.995734176295034,1.,0.995734176295034,1.,0.995734176295034,1.,0.995734176295034,
1.,0.995734176295034,1.,0.995734176295034,1.,0.995734176295034,1.,0.995734176295034,
1.,0.995734176295034,1.,0.995734176295034,1.,0.995734176295034,1.,0.995734176295034,
1.,0.995734176295034,1.,0.995734176295034,1.,0.995734176295034,1.,0.995734176295034,
1.,0.995734176295034,1.,0.995734176295034,1.,0.995734176295034,1.,0.995734176295034,
1.,0.995734176295034,1.,0.995734176295034,1.,0.995734176295034,1.,0.997201362504481,
0.998074874808405,0.998074874808405,0.998074874808405),(1.,0.995734176295034,
1.,0.995734176295034,1.,0.995734176295034,1.,0.995734176295034,1.,0.995734176295034,
1.,0.995734176295034,1.,0.995734176295034,1.,0.995734176295034,1.,0.995734176295034,
1.,0.995734176295034,1.,0.995734176295034,1.,0.995734176295034,1.,0.995734176295034,
1.,0.995734176295034,1.,0.995734176295034,1.,0.995734176295034,1.,0.995734176295034,
1.,0.995734176295034,1.,0.995734176295034,1.,0.995734176295034,1.,0.995734176295034,
1.,0.995734176295034,1.,0.995734176295034,1.,0.995734176295034,1.,0.995734176295034,
1.,0.995734176295034,1.,0.995734176295034,1.,0.995734176295034,1.,0.995734176295034,
1.,0.995734176295034,1.,0.995734176295034,1.,0.995734176295034,1.,0.995734176295034,
1.,0.995734176295034,1.,0.995734176295034,1.,0.995734176295034,1.,0.995734176295034,
1.,0.995734176295034,1.,0.995734176295034,1.,0.995734176295034,1.,0.995734176295034,
1.,0.995734176295034,1.,0.995734176295034,1.,0.995734176295034,1.,0.995734176295034,
1.,0.995734176295034,1.,0.995734176295034,1.,0.995734176295034,1.,0.995734176295034,
1.,0.995734176295034,1.,0.995734176295034,1.,0.995734176295034,1.,0.995734176295034,
1.,0.995734176295034,1.,0.995734176295034,1.,0.995734176295034,1.,0.995734176295034,
1.,0.995734176295034,1.,0.995734176295034,1.,0.995734176295034,1.,0.995734176295034,
1.,0.995734176295034,1.,0.995734176295034,1.,0.995734176295034,1.,0.995734176295034,
1.,0.995734176295034,1.,0.995734176295034,1.,0.995734176295034,1.,0.995734176295034,
1.,0.995734176295034,1.,0.995734176295034,1.,0.995734176295034,1.,0.995734176295034,
1.,0.995734176295034,1.,0.995734176295034,1.,0.995734176295034,1.,0.995734176295034,
1.,0.995734176295034,1.,0.995734176295034,1.,0.995734176295034,1.,0.995734176295034,
1.,0.995734176295034,1.,0.995734176295034,1.,0.995734176295034,1.,0.995734176295034,
1.,0.995734176295034,1.,0.995734176295034,1.,0.995734176295034,1.,0.995734176295034,
1.,0.995734176295034,1.,0.995734176295034,1.,0.995734176295034,1.,0.995734176295034,
1.,0.995734176295034,1.,0.995734176295034,1.,0.995734176295034,1.,0.995734176295034,
1.,0.995734176295034,1.,0.995734176295034,1.,0.995734176295034,1.,0.995734176295034,
1.,0.995734176295034,1.,0.995734176295034,1.,0.995734176295034,1.,0.995734176295034,
1.,0.995734176295034,1.,0.995734176295034,1.,0.995734176295034,1.,0.995734176295034,
1.,0.995734176295034,1.,0.995734176295034,1.,0.995734176295034,1.,0.995734176295034,
1.,0.995734176295034,1.,0.995734176295034,1.,0.995734176295034,1.,0.995734176295034,
1.,0.995734176295034,1.,0.995734176295034,1.,0.995734176295034,1.,0.995734176295034,
1.,0.995734176295034,1.,0.995734176295034,1.,0.995734176295034,1.,0.995734176295034,
1.,0.995734176295034,1.,0.995734176295034,1.,0.995734176295034,1.,0.995734176295034,
1.,0.995734176295034,1.,0.995734176295034,1.,0.995734176295034,1.,0.995734176295034,
1.,0.995734176295034,1.,0.995734176295034,1.,0.995734176295034,1.,0.995734176295034,
1.,0.995734176295034,1.,0.995734176295034,1.,0.995734176295034,1.,0.995734176295034,
1.,0.995734176295034,1.,0.995734176295034,1.,0.995734176295034,1.,0.995734176295034,
1.,0.995734176295034,1.,0.995734176295034,1.,0.995734176295034,1.,0.995734176295034,
1.,0.995734176295034,1.,0.995734176295034,1.,0.995734176295034,1.,0.995734176295034,
1.,0.995734176295034,1.,0.995734176295034,1.,0.995734176295034,1.,0.995734176295034,
1.,0.995734176295034,1.,0.995734176295034,1.,0.995734176295034,1.,0.995734176295034,
1.,0.995734176295034,1.,0.995734176295034,1.,0.995734176295034,1.,0.995734176295034,
1.,0.995734176295034,1.,0.995734176295034,1.,0.995734176295034,1.,0.995734176295034,
1.,0.995734176295034,1.,0.995734176295034,1.,0.995734176295034,1.,0.995734176295034,
1.,0.995734176295034,1.,0.995734176295034,1.,0.995734176295034,1.,0.995734176295034,
1.,0.995734176295034,1.,0.995734176295034,1.,0.995734176295034,1.,0.995734176295034,
1.,0.995734176295034,1.,0.995734176295034,1.,0.995734176295034,1.,0.995734176295034,
1.,0.995734176295034,1.,0.995734176295034,1.,0.995734176295034,1.,0.995734176295034,
1.,0.995734176295034,1.,0.995734176295034,1.,0.995734176295034,1.,0.995734176295034,
1.,0.995734176295034,1.,0.995734176295034,1.,0.995734176295034,1.,0.995734176295034,
1.,0.995734176295034,1.,0.995734176295034,1.,0.995734176295034,1.,0.995734176295034,
1.,0.995734176295034,1.,0.995734176295034,1.,0.995734176295034,1.,0.995734176295034,
1.,0.995734176295034,1.,0.995734176295034,1.,0.995734176295034,1.,0.995734176295034,
1.,0.995734176295034,1.,0.995734176295034,1.,0.995734176295034,1.,0.995734176295034,
1.,0.995734176295034,1.,0.995734176295034,1.,0.995734176295034,1.,0.995734176295034,
1.,0.995734176295034,1.,0.995734176295034,1.,0.995734176295034,1.,0.995734176295034,
1.,0.995734176295034,1.,0.995734176295034,1.,0.995734176295034,1.,0.995734176295034,
1.,0.995734176295034,1.,0.995734176295034,1.,0.995734176295034,1.,0.995734176295034,
1.,0.995734176295034,1.,0.995734176295034,1.,0.995734176295034,1.,0.995734176295034,
1.,0.995734176295034,1.,0.995734176295034,1.,0.995734176295034,1.,0.995734176295034,
1.,0.995734176295034,1.,0.995734176295034,1.,0.995734176295034,1.,0.995734176295034,
1.,0.995734176295034,1.,0.995734176295034,1.,0.995734176295034,1.,0.995734176295034,
1.,0.995734176295034,1.,0.995734176295034,1.,0.995734176295034,1.,0.995734176295034,
1.,0.995734176295034,1.,0.995734176295034,1.,0.995734176295034,1.,0.995734176295034,
1.,0.995734176295034,1.,0.995734176295034,1.,0.995734176295034,1.,0.995734176295034,
1.,0.995734176295034,1.,0.995734176295034,1.,0.995734176295034,1.,0.995734176295034,
1.,0.995734176295034,1.,0.995734176295034,1.,0.995734176295034,1.,0.995734176295034,
1.,0.995734176295034,1.,0.995734176295034,1.,0.995734176295034,1.,0.995734176295034,
1.,0.995734176295034,1.,0.995734176295034,1.,0.995734176295034,1.,0.995734176295034,
1.,0.995734176295034,1.,0.995734176295034,1.,0.995734176295034,1.,0.995734176295034,
1.,0.995734176295034,1.,0.995734176295034,1.,0.995734176295034,1.,0.995734176295034,
1.,0.995734176295034,1.,0.995734176295034,1.,0.995734176295034,1.,0.995734176295034,
1.,0.995734176295034,1.,0.995734176295034,1.,0.995734176295034,1.,0.995734176295034,
1.,0.995734176295034,1.,0.995734176295034,1.,0.995734176295034,1.,0.995734176295034,
1.,0.995734176295034,1.,0.995734176295034,1.,0.995734176295034,1.,0.995734176295034,
1.,0.995734176295034,1.,0.995734176295034,1.,0.995734176295034,1.,0.995734176295034,
1.,0.995734176295034,1.,0.995734176295034,1.,0.995734176295034,1.,0.995734176295034,
1.,0.995734176295034,1.,0.995734176295034,1.,0.995734176295034,1.,0.995734176295034,
1.,0.995734176295034,1.,0.995734176295034,1.,0.995734176295034,1.,0.995734176295034,
1.,0.995734176295034,1.,0.995734176295034,1.,0.995734176295034,1.,0.995734176295034,
1.,0.995734176295034,1.,0.995734176295034,1.,0.995734176295034,1.,0.995734176295034,
1.,0.995734176295034,1.,0.995734176295034,1.,0.995734176295034,1.,0.995734176295034,
1.,0.995734176295034,1.,0.995734176295034,1.,0.995734176295034,1.,0.995734176295034,
1.,0.995734176295034,1.,0.995734176295034,1.,0.995734176295034,1.,0.995734176295034,
1.,0.995734176295034,1.,0.995734176295034,1.,0.995734176295034,1.,0.995734176295034,
1.,0.995734176295034,1.,0.995734176295034,1.,0.995734176295034,1.,0.995734176295034,
1.,0.995734176295034,1.,0.995734176295034,1.,0.995734176295034,1.,0.995734176295034,
1.,0.995734176295034,1.,0.995734176295034,1.,0.995734176295034,1.,0.995734176295034,
1.,0.995734176295034,1.,0.995734176295034,1.,0.995734176295034,1.,0.995734176295034,
1.,0.995734176295034,1.,0.995734176295034,1.,0.995734176295034,1.,0.995734176295034,
1.,0.995734176295034,1.,0.995734176295034,1.,0.995734176295034,1.,0.995734176295034,
1.,0.995734176295034,1.,0.995734176295034,1.,0.995734176295034,1.,0.995734176295034,
1.,0.995734176295034,1.,0.995734176295034,1.,0.995734176295034,1.,0.995734176295034,
1.,0.995734176295034,1.,0.995734176295034,1.,0.995734176295034,1.,0.995734176295034,
1.,0.995734176295034,1.,0.995734176295034,1.,0.995734176295034,1.,0.995734176295034,
1.,0.995734176295034,1.,0.995734176295034,1.,0.995734176295034,1.,0.995734176295034,
1.,0.995734176295034,1.,0.995734176295034,1.,0.995734176295034,1.,0.995734176295034,
1.,0.995734176295034,1.,0.995734176295034,1.,0.995734176295034,1.,0.995734176295034,
1.,0.995734176295034,1.,0.995734176295034,1.,0.995734176295034,1.,0.995734176295034,
1.,0.995734176295034,1.,0.995734176295034,1.,0.995734176295034,1.,0.995734176295034,
1.,0.995734176295034,1.,0.995734176295034,1.,0.995734176295034,1.,0.995734176295034,
1.,0.995734176295034,1.,0.995734176295034,1.,0.995734176295034,1.,0.995734176295034,
1.,0.995734176295034,1.,0.995734176295034,1.,0.995734176295034,1.,0.995734176295034,
1.,0.995734176295034,1.,0.995734176295034,1.,0.995734176295034,1.,0.995734176295034,
1.,0.995734176295034,1.,0.995734176295034,1.,0.995734176295034,1.,0.995734176295034,
1.,0.995734176295034,1.,0.995734176295034,1.,0.995734176295034,1.,0.995734176295034,
1.,0.995734176295034,1.,0.995734176295034,1.,0.995734176295034,1.,0.995734176295034,
1.,0.995734176295034,1.,0.995734176295034,1.,0.995734176295034,1.,0.995734176295034,
1.,0.995734176295034,1.,0.995734176295034,1.,0.995734176295034,1.,0.995734176295034,
1.,0.995734176295034,1.,0.995734176295034,1.,0.995734176295034,1.,0.995734176295034,
1.,0.995734176295034,1.,0.995734176295034,1.,0.995734176295034,1.,0.995734176295034,
1.,0.995734176295034,1.,0.995734176295034,1.,0.995734176295034,1.,0.995734176295034,
1.,0.995734176295034,1.,0.995734176295034,1.,0.995734176295034,1.,0.995734176295034,
1.,0.995734176295034,1.,0.995734176295034,1.,0.995734176295034,1.,0.995734176295034,
1.,0.995734176295034,1.,0.995734176295034,1.,0.995734176295034,1.,0.995734176295034,
1.,0.995734176295034,1.,0.995734176295034,1.,0.995734176295034,1.,0.995734176295034,
1.,0.995734176295034,1.,0.995734176295034,1.,0.995734176295034,1.,0.995734176295034,
1.,0.995734176295034,1.,0.995734176295034,1.,0.995734176295034,1.,0.995734176295034,
1.,0.995734176295034,1.,0.995734176295034,1.,0.995734176295034,1.,0.995734176295034,
1.,0.995734176295034,1.,0.995734176295034,1.,0.995734176295034,1.,0.995734176295034,
1.,0.995734176295034,1.,0.995734176295034,1.,0.995734176295034,1.,0.995734176295034,
1.,0.995734176295034,1.,0.995734176295034,1.,0.995734176295034,1.,0.995734176295034,
1.,0.995734176295034,1.,0.995734176295034,1.,0.995734176295034,1.,0.995734176295034,
1.,0.995734176295034,1.,0.995734176295034,1.,0.995734176295034,1.,0.995734176295034,
1.,0.995734176295034,1.,0.995734176295034,1.,0.995734176295034,1.,0.995734176295034,
1.,0.995734176295034,1.,0.995734176295034,1.,0.995734176295034,1.,0.995734176295034,
1.,0.995734176295034,1.,0.995734176295034,1.,0.995734176295034,1.,0.995734176295034,
1.,0.995734176295034,1.,0.995734176295034,1.,0.995734176295034,1.,0.995734176295034,
1.,0.995734176295034,1.,0.995734176295034,1.,0.995734176295034,1.,0.995734176295034,
1.,0.995734176295034,1.,0.995734176295034,1.,0.995734176295034,1.,0.995734176295034,
1.,0.995734176295034,1.,0.995734176295034,1.,0.995734176295034,1.,0.995734176295034,
1.,0.995734176295034,1.,0.995734176295034,1.,0.995734176295034,1.,0.995734176295034,
1.,0.995734176295034,1.,0.995734176295034,1.,0.995734176295034,1.,0.995734176295034,
1.,0.995734176295034,1.,0.995734176295034,1.,0.995734176295034,1.,0.995734176295034,
1.,0.995734176295034,1.,0.995734176295034,1.,0.995734176295034,1.,0.995734176295034,
1.,0.995734176295034,1.,0.995734176295034,1.,0.995734176295034,1.,0.995734176295034,
1.,0.995734176295034,1.,0.995734176295034,1.,0.995734176295034,1.,0.995734176295034,
1.,0.995734176295034,1.,0.995734176295034,1.,0.995734176295034,1.,0.995734176295034,
1.,0.995734176295034,1.,0.995734176295034,1.,0.995734176295034,1.,0.995734176295034,
1.,0.995734176295034,1.,0.995734176295034,1.,0.995734176295034,1.,0.995734176295034,
1.,0.995734176295034,1.,0.995734176295034,1.,0.995734176295034,1.,0.995734176295034,
1.,0.995734176295034,1.,0.995734176295034,1.,0.995734176295034,1.,0.995734176295034,
1.,0.995734176295034,1.,0.995734176295034,1.,0.995734176295034,1.,0.995734176295034,
1.,0.995734176295034,1.,0.995734176295034,1.,0.995734176295034,1.,0.995734176295034,
1.,0.995734176295034,1.,0.995734176295034,1.,0.995734176295034,1.,0.995734176295034,
1.,0.995734176295034,1.,0.995734176295034,1.,0.995734176295034,1.,0.995734176295034,
1.,0.995734176295034,1.,0.995734176295034,1.,0.995734176295034,1.,0.995734176295034,
1.,0.995734176295034,1.,0.995734176295034,1.,0.995734176295034,1.,0.995734176295034,
1.,0.995734176295034,1.,0.995734176295034,1.,0.995734176295034,1.,0.995734176295034,
1.,0.995734176295034,1.,0.995734176295034,1.,0.995734176295034,1.,0.995734176295034,
1.,0.995734176295034,1.,0.995734176295034,1.,0.995734176295034,1.,0.995734176295034,
1.,0.995734176295034,1.,0.995734176295034,1.,0.995734176295034,1.,0.995734176295034,
1.,0.995734176295034,1.,0.995734176295034,1.,0.995734176295034,1.,0.995734176295034,
1.,0.995734176295034,1.,0.995734176295034,1.,0.995734176295034,1.,0.995734176295034,
1.,0.995734176295034,1.,0.995734176295034,1.,0.995734176295034,1.,0.995734176295034,
1.,0.995734176295034,1.,0.995734176295034,1.,0.995734176295034,1.,0.995734176295034,
1.,0.995734176295034,1.,0.995734176295034,1.,0.995734176295034,1.,0.995734176295034,
1.,0.995734176295034,1.,0.995734176295034,1.,0.995734176295034,1.,0.995734176295034,
1.,0.995734176295034,1.,0.995734176295034,1.,0.995734176295034,1.,0.995734176295034,
1.,0.995734176295034,1.,0.995734176295034,1.,0.995734176295034,1.,0.995734176295034,
1.,0.995734176295034,1.,0.995734176295034,1.,0.995734176295034,1.,0.995734176295034,
1.,0.995734176295034,1.,0.995734176295034,1.,0.995734176295034,1.,0.995734176295034,
1.,0.995734176295034,1.,0.995734176295034,1.,0.995734176295034,1.,0.995734176295034,
1.,0.995734176295034,1.,0.995734176295034,1.,0.995734176295034,1.,0.995734176295034,
1.,0.995734176295034,1.,0.995734176295034,1.,0.995734176295034,1.,0.995734176295034,
1.,0.995734176295034,1.,0.995734176295034,1.,0.995734176295034,1.,0.995734176295034,
1.,0.995734176295034,1.,0.995734176295034,1.,0.995734176295034,1.,0.995734176295034,
1.,0.995734176295034,1.,0.995734176295034,1.,0.995734176295034,1.,0.995734176295034,
1.,0.995734176295034,1.,0.995734176295034,1.,0.995734176295034,1.,0.995734176295034,
1.,0.995734176295034,1.,0.995734176295034,1.,0.995734176295034,1.,0.995734176295034,
1.,0.995734176295034,1.,0.995734176295034,1.,0.995734176295034,1.,0.995734176295034,
1.,0.995734176295034,1.,0.995734176295034,1.,0.995734176295034,1.,0.995734176295034,
1.,0.995734176295034,1.,0.995734176295034,1.,0.995734176295034,1.,0.995734176295034,
1.,0.995734176295034,1.,0.995734176295034,1.,0.995734176295034,1.,0.995734176295034,
1.,0.995734176295034,1.,0.995734176295034,1.,0.995734176295034,1.,0.995734176295034,
1.,0.995734176295034,1.,0.995734176295034,1.,0.995734176295034,1.,0.995734176295034,
1.,0.995734176295034,1.,0.995734176295034,1.,0.995734176295034,1.,0.995734176295034,
1.,0.995734176295034,1.,0.995734176295034,1.,0.995734176295034,1.,0.995734176295034,
1.,0.995734176295034,1.,0.995734176295034,1.,0.995734176295034,1.,0.995734176295034,
1.,0.995734176295034,1.,0.995734176295034,1.,0.995734176295034,1.,0.995734176295034,
1.,0.995734176295034,1.,0.995734176295034,1.,0.995734176295034,1.,0.995734176295034,
1.,0.995734176295034,1.,0.995734176295034,1.,0.995734176295034,1.,0.995734176295034,
1.,0.995734176295034,1.,0.995734176295034,1.,0.995734176295034,1.,0.995734176295034,
1.,0.995734176295034,1.,0.995734176295034,1.,0.995734176295034,1.,0.995734176295034,
1.,0.995734176295034,1.,0.995734176295034,1.,0.995734176295034,1.,0.995734176295034,
1.,0.995734176295034,1.,0.995734176295034,1.,0.995734176295034,1.,0.995734176295034,
1.,0.995734176295034,1.,0.995734176295034,1.,0.995734176295034,1.,0.995734176295034,
1.,0.995734176295034,1.,0.995734176295034,1.,0.995734176295034,1.,0.995734176295034,
1.,0.995734176295034,1.,0.995734176295034,1.,0.995734176295034,1.,0.995734176295034,
1.,0.995734176295034,1.,0.995734176295034,1.,0.995734176295034,1.,0.995734176295034,
1.,0.995734176295034,1.,0.995734176295034,1.,0.995734176295034,1.,0.995734176295034,
1.,0.995734176295034,1.,0.995734176295034,1.,0.995734176295034,1.,0.995734176295034,
1.,0.995734176295034,1.,0.995734176295034,1.,0.995734176295034,1.,0.995734176295034,
1.,0.995734176295034,1.,0.995734176295034,1.,0.995734176295034,1.,0.995734176295034,
1.,0.995734176295034,1.,0.995734176295034,1.,0.995734176295034,1.,0.995734176295034,
1.,0.995734176295034,1.,0.995734176295034,1.,0.995734176295034,1.,0.995734176295034,
1.,0.995734176295034,1.,0.995734176295034,1.,0.995734176295034,1.,0.995734176295034,
1.,0.995734176295034,1.,0.995734176295034,1.,0.995734176295034,1.,0.995734176295034,
1.,0.995734176295034,1.,0.995734176295034,1.,0.995734176295034,1.,0.995734176295034,
1.,0.995734176295034,1.,0.995734176295034,1.,0.995734176295034,1.,0.995734176295034,
1.,0.995734176295034,1.,0.995734176295034,1.,0.995734176295034,1.,0.995734176295034,
1.,0.995734176295034,1.,0.995734176295034,1.,0.995734176295034,1.,0.995734176295034,
1.,0.995734176295034,1.,0.995734176295034,1.,0.995734176295034,1.,0.995734176295034,
1.,0.995734176295034,1.,0.995734176295034,1.,0.995734176295034,1.,0.995734176295034,
1.,0.995734176295034,1.,0.995734176295034,1.,0.995734176295034,1.,0.995734176295034,
1.,0.995734176295034,1.,0.995734176295034,1.,0.995734176295034,1.,0.995734176295034,
1.,0.995734176295034,1.,0.995734176295034,1.,0.995734176295034,1.,0.995734176295034,
1.,0.995734176295034,1.,0.995734176295034,1.,0.995734176295034,1.,0.995734176295034,
1.,0.995734176295034,1.,0.995734176295034,1.,0.995734176295034,1.,0.995734176295034,
1.,0.995734176295034,1.,0.995734176295034,1.,0.995734176295034,1.,0.995734176295034,
1.,0.995734176295034,1.,0.995734176295034,1.,0.995734176295034,1.,0.995734176295034,
1.,0.995734176295034,1.,0.995734176295034,1.,0.995734176295034,1.,0.995734176295034,
1.,0.995734176295034,1.,0.995734176295034,1.,0.995734176295034,1.,0.995734176295034,
1.,0.995734176295034,1.,0.995734176295034,1.,0.995734176295034,1.,0.995734176295034,
1.,0.995734176295034,1.,0.995734176295034,1.,0.995734176295034,1.,0.995734176295034,
1.,0.995734176295034,1.,0.995734176295034,1.,0.995734176295034,1.,0.995734176295034,
1.,0.995734176295034,1.,0.995734176295034,1.,0.995734176295034,1.,0.995734176295034,
1.,0.995734176295034,1.,0.995734176295034,1.,0.995734176295034,1.,0.995734176295034,
1.,0.995734176295034,1.,0.995734176295034,1.,0.995734176295034,1.,0.995734176295034,
1.,0.995734176295034,1.,0.995734176295034,1.,0.995734176295034,1.,0.995734176295034,
1.,0.995734176295034,1.,0.995734176295034,1.,0.995734176295034,1.,0.995734176295034,
1.,0.995734176295034,1.,0.995734176295034,1.,0.995734176295034,1.,0.995734176295034,
1.,0.995734176295034,1.,0.995734176295034,1.,0.995734176295034,1.,0.995734176295034,
1.,0.995734176295034,1.,0.995734176295034,1.,0.995734176295034,1.,0.995734176295034,
1.,0.995734176295034,1.,0.995734176295034,1.,0.995734176295034,1.,0.995734176295034,
1.,0.995734176295034,1.,0.995734176295034,1.,0.995734176295034,1.,0.995734176295034,
1.,0.995734176295034,1.,0.995734176295034,1.,0.995734176295034,1.,0.995734176295034,
1.,0.995734176295034,1.,0.995734176295034,1.,0.995734176295034,1.,0.995734176295034,
1.,0.995734176295034,1.,0.995734176295034,1.,0.995734176295034,1.,0.995734176295034,
1.,0.995734176295034,1.,0.995734176295034,1.,0.995734176295034,1.,0.995734176295034,
1.,0.995734176295034,1.,0.995734176295034,1.,0.995734176295034,1.,0.995734176295034,
1.,0.995734176295034,1.,0.995734176295034,1.,0.995734176295034,1.,0.995734176295034,
1.,0.995734176295034,1.,0.995734176295034,1.,0.995734176295034,1.,0.995734176295034,
1.,0.995734176295034,1.,0.995734176295034,1.,0.995734176295034,1.,0.995734176295034,
1.,0.995734176295034,1.,0.995734176295034,1.,0.995734176295034,1.,0.995734176295034,
1.,0.995734176295034,1.,0.995734176295034,1.,0.995734176295034,1.,0.995734176295034,
1.,0.995734176295034,1.,0.995734176295034,1.,0.995734176295034,1.,0.995734176295034,
1.,0.995734176295034,1.,0.995734176295034,1.,0.995734176295034,1.,0.995734176295034,
1.,0.995734176295034,1.,0.995734176295034,1.,0.995734176295034,1.,0.995734176295034,
1.,0.995734176295034,1.,0.995734176295034,1.,0.995734176295034,1.,0.995734176295034,
1.,0.995734176295034,1.,0.995734176295034,1.,0.995734176295034,1.,0.995734176295034,
1.,0.995734176295034,1.,0.995734176295034,1.,0.995734176295034,1.,0.995734176295034,
1.,0.995734176295034,1.,0.995734176295034,1.,0.995734176295034,1.,0.995734176295034,
1.,0.995734176295034,1.,0.995734176295034,1.,0.995734176295034,1.,0.995734176295034,
1.,0.995734176295034,1.,0.995734176295034,1.,0.995734176295034,1.,0.995734176295034,
1.,0.995734176295034,1.,0.995734176295034,1.,0.995734176295034,1.,0.995734176295034,
1.,0.995734176295034,1.,0.995734176295034,1.,0.995734176295034,1.,0.995734176295034,
1.,0.995734176295034,1.,0.995734176295034,1.,0.995734176295034,1.,0.995734176295034,
1.,0.995734176295034,1.,0.995734176295034,1.,0.995734176295034,1.,0.995734176295034,
1.,0.995734176295034,1.,0.995734176295034,1.,0.995734176295034,1.,0.995734176295034,
1.,0.995734176295034,1.,0.995734176295034,1.,0.995734176295034,1.,0.995734176295034,
1.,0.995734176295034,1.,0.995734176295034,1.,0.995734176295034,1.,0.995734176295034,
1.,0.997201362504481,0.998074874808405,0.998074874808405,0.998074874808405)))
REPRESENTATION_ITEM('')
SURFACE()
);
#2506=(
BOUNDED_SURFACE()
B_SPLINE_SURFACE(3,2,((#182277,#182278,#182279),(#182280,#182281,#182282),
(#182283,#182284,#182285),(#182286,#182287,#182288)),.UNSPECIFIED.,.F.,
 .F.,.F.)
B_SPLINE_SURFACE_WITH_KNOTS((4,4),(3,3),(0.,0.000397394410828739),(0.,1.),
 .UNSPECIFIED.)
GEOMETRIC_REPRESENTATION_ITEM()
RATIONAL_B_SPLINE_SURFACE(((1.,0.708689770883314,1.),(1.,0.708376440034512,
1.),(1.,0.707750498698405,1.),(1.,0.707106781186548,1.)))
REPRESENTATION_ITEM('')
SURFACE()
);
#2507=(
BOUNDED_SURFACE()
B_SPLINE_SURFACE(3,2,((#182294,#182295,#182296),(#182297,#182298,#182299),
(#182300,#182301,#182302),(#182303,#182304,#182305)),.UNSPECIFIED.,.F.,
 .F.,.F.)
B_SPLINE_SURFACE_WITH_KNOTS((4,4),(3,3),(0.,0.000511815090126176),(0.,1.00105592270548),
 .UNSPECIFIED.)
GEOMETRIC_REPRESENTATION_ITEM()
RATIONAL_B_SPLINE_SURFACE(((1.,0.70526624271652,1.00062243213277),(1.,0.705584085908178,
1.00062176089709),(1.,0.706182089449526,1.00062049800605),(1.,0.706797508586522,
1.00061919833597)))
REPRESENTATION_ITEM('')
SURFACE()
);
#2508=(
BOUNDED_SURFACE()
B_SPLINE_SURFACE(3,2,((#182307,#182308,#182309),(#182310,#182311,#182312),
(#182313,#182314,#182315),(#182316,#182317,#182318)),.UNSPECIFIED.,.F.,
 .F.,.F.)
B_SPLINE_SURFACE_WITH_KNOTS((4,4),(3,3),(-6.85757874097082E-18,0.000397394428086617),
(0.,1.),.UNSPECIFIED.)
GEOMETRIC_REPRESENTATION_ITEM()
RATIONAL_B_SPLINE_SURFACE(((1.,0.707106781186548,1.),(1.,0.706459846759102,
1.),(1.,0.705820510737261,1.),(1.,0.705498956110752,1.)))
REPRESENTATION_ITEM('')
SURFACE()
);
#2509=(
BOUNDED_SURFACE()
B_SPLINE_SURFACE(3,2,((#182324,#182325,#182326),(#182327,#182328,#182329),
(#182330,#182331,#182332),(#182333,#182334,#182335),(#182336,#182337,#182338),
(#182339,#182340,#182341)),.UNSPECIFIED.,.F.,.F.,.F.)
B_SPLINE_SURFACE_WITH_KNOTS((4,2,4),(3,3),(0.,0.000257953807872846,0.000515907615745692),
(0.,1.),.UNSPECIFIED.)
GEOMETRIC_REPRESENTATION_ITEM()
RATIONAL_B_SPLINE_SURFACE(((1.,0.874619707139392,1.),(1.,0.874834349678941,
1.),(1.,0.854686104157853,1.),(1.,0.792476597915084,1.),(1.,0.750887854595174,
1.),(1.,0.705585838031441,1.)))
REPRESENTATION_ITEM('')
SURFACE()
);
#2510=(
BOUNDED_SURFACE()
B_SPLINE_SURFACE(3,2,((#182347,#182348,#182349),(#182350,#182351,#182352),
(#182353,#182354,#182355),(#182356,#182357,#182358)),.UNSPECIFIED.,.F.,
 .F.,.F.)
B_SPLINE_SURFACE_WITH_KNOTS((4,4),(3,3),(0.,0.000511815437699147),(0.,1.00105881331497),
 .UNSPECIFIED.)
GEOMETRIC_REPRESENTATION_ITEM()
RATIONAL_B_SPLINE_SURFACE(((1.,0.706796661946604,1.00062089519665),(1.,
0.707430821225471,1.00061955228407),(1.,0.708058545830999,1.00061822299773),
(1.,0.708394505252984,1.00061751156111)))
REPRESENTATION_ITEM('')
SURFACE()
);
#2511=(
BOUNDED_SURFACE()
B_SPLINE_SURFACE(3,2,((#182360,#182361,#182362),(#182363,#182364,#182365),
(#182366,#182367,#182368),(#182369,#182370,#182371),(#182372,#182373,#182374),
(#182375,#182376,#182377)),.UNSPECIFIED.,.F.,.F.,.F.)
B_SPLINE_SURFACE_WITH_KNOTS((4,2,4),(3,3),(0.,0.000256915317531259,0.000513830635062519),
(0.,1.),.UNSPECIFIED.)
GEOMETRIC_REPRESENTATION_ITEM()
RATIONAL_B_SPLINE_SURFACE(((1.,0.705585838031441,1.),(1.,0.750902433542908,
1.),(1.,0.7923295300823,1.),(1.,0.854288401594408,1.),(1.,0.874998031124972,
1.),(1.,0.874619707139392,1.)))
REPRESENTATION_ITEM('')
SURFACE()
);
#2512=(
BOUNDED_SURFACE()
B_SPLINE_SURFACE(3,2,((#182383,#182384,#182385),(#182386,#182387,#182388),
(#182389,#182390,#182391),(#182392,#182393,#182394),(#182395,#182396,#182397),
(#182398,#182399,#182400)),.UNSPECIFIED.,.F.,.F.,.F.)
B_SPLINE_SURFACE_WITH_KNOTS((4,2,4),(3,3),(-1.35525271560688E-19,0.000256592814262156,
0.000513185628524312),(0.,1.),.UNSPECIFIED.)
GEOMETRIC_REPRESENTATION_ITEM()
RATIONAL_B_SPLINE_SURFACE(((1.,0.708712527163663,1.),(1.,0.753780902613751,
1.),(1.,0.794538995768995,1.),(1.,0.855070770331318,1.),(1.,0.875018427445164,
1.),(1.,0.874619707139396,1.)))
REPRESENTATION_ITEM('')
SURFACE()
);
#2513=(
BOUNDED_SURFACE()
B_SPLINE_SURFACE(3,2,((#182402,#182403,#182404),(#182405,#182406,#182407),
(#182408,#182409,#182410),(#182411,#182412,#182413)),.UNSPECIFIED.,.F.,
 .F.,.F.)
B_SPLINE_SURFACE_WITH_KNOTS((4,4),(3,3),(2.71050543121376E-20,0.000511815072430401),
(0.,1.00105598366171),.UNSPECIFIED.)
GEOMETRIC_REPRESENTATION_ITEM()
RATIONAL_B_SPLINE_SURFACE(((1.,0.706797490732854,1.00061923411872),(1.,
0.706182062145767,1.00062053388378),(1.,0.705584062768141,1.00062179683893),
(1.,0.70526622476961,1.0006224681024)))
REPRESENTATION_ITEM('')
SURFACE()
);
#2514=(
BOUNDED_SURFACE()
B_SPLINE_SURFACE(3,2,((#182419,#182420,#182421),(#182422,#182423,#182424),
(#182425,#182426,#182427),(#182428,#182429,#182430),(#182431,#182432,#182433),
(#182434,#182435,#182436)),.UNSPECIFIED.,.F.,.F.,.F.)
B_SPLINE_SURFACE_WITH_KNOTS((4,2,4),(3,3),(0.,0.000257652232350879,0.000515304464701757),
(0.,1.),.UNSPECIFIED.)
GEOMETRIC_REPRESENTATION_ITEM()
RATIONAL_B_SPLINE_SURFACE(((1.,0.87461970713939,1.),(1.,0.874861180430742,
1.),(1.,0.855455725920812,1.),(1.,0.794699358955327,1.),(1.,0.753768977788612,
1.),(1.,0.708712527163663,1.)))
REPRESENTATION_ITEM('')
SURFACE()
);
#2515=(
BOUNDED_SURFACE()
B_SPLINE_SURFACE(3,2,((#182442,#182443,#182444),(#182445,#182446,#182447),
(#182448,#182449,#182450),(#182451,#182452,#182453)),.UNSPECIFIED.,.F.,
 .F.,.F.)
B_SPLINE_SURFACE_WITH_KNOTS((4,4),(3,3),(0.,0.000397394373651911),(0.,1.),
 .UNSPECIFIED.)
GEOMETRIC_REPRESENTATION_ITEM()
RATIONAL_B_SPLINE_SURFACE(((1.,0.707106781186548,1.),(1.,0.707752587915878,
1.),(1.,0.708377654540693,1.),(1.,0.708689770883314,1.)))
REPRESENTATION_ITEM('')
SURFACE()
);
#2516=(
BOUNDED_SURFACE()
B_SPLINE_SURFACE(3,2,((#182455,#182456,#182457),(#182458,#182459,#182460),
(#182461,#182462,#182463),(#182464,#182465,#182466)),.UNSPECIFIED.,.F.,
 .F.,.F.)
B_SPLINE_SURFACE_WITH_KNOTS((4,4),(3,3),(-6.42389787197661E-18,0.000511815456479793),
(0.,1.00105873159743),.UNSPECIFIED.)
GEOMETRIC_REPRESENTATION_ITEM()
RATIONAL_B_SPLINE_SURFACE(((1.,0.70839452905708,1.00061746385214),(1.,0.708058564167607,
1.00061817524543),(1.,0.707430835372803,1.00061950443805),(1.,0.706796685881118,
1.00062084722626)))
REPRESENTATION_ITEM('')
SURFACE()
);
#2517=(
BOUNDED_SURFACE()
B_SPLINE_SURFACE(3,2,((#182472,#182473,#182474),(#182475,#182476,#182477),
(#182478,#182479,#182480),(#182481,#182482,#182483)),.UNSPECIFIED.,.F.,
 .F.,.F.)
B_SPLINE_SURFACE_WITH_KNOTS((4,4),(3,3),(0.,0.000397394465448317),(0.,1.),
 .UNSPECIFIED.)
GEOMETRIC_REPRESENTATION_ITEM()
RATIONAL_B_SPLINE_SURFACE(((1.,0.705498956110752,1.),(1.,0.705821764811793,
1.),(1.,0.70646195252114,1.),(1.,0.707106781186548,1.)))
REPRESENTATION_ITEM('')
SURFACE()
);
#2518=(
BOUNDED_SURFACE()
B_SPLINE_SURFACE(3,2,((#197994,#197995,#197996),(#197997,#197998,#197999),
(#198000,#198001,#198002),(#198003,#198004,#198005)),.UNSPECIFIED.,.F.,
 .F.,.F.)
B_SPLINE_SURFACE_WITH_KNOTS((4,4),(3,3),(0.,0.000397394410828745),(0.,1.),
 .UNSPECIFIED.)
GEOMETRIC_REPRESENTATION_ITEM()
RATIONAL_B_SPLINE_SURFACE(((1.,0.708689770883337,1.),(1.,0.708376440034498,
1.),(1.,0.707750498698412,1.),(1.,0.707106781186545,1.)))
REPRESENTATION_ITEM('')
SURFACE()
);
#2519=(
BOUNDED_SURFACE()
B_SPLINE_SURFACE(3,2,((#198011,#198012,#198013),(#198014,#198015,#198016),
(#198017,#198018,#198019),(#198020,#198021,#198022)),.UNSPECIFIED.,.F.,
 .F.,.F.)
B_SPLINE_SURFACE_WITH_KNOTS((4,4),(3,3),(0.,0.000511815090126173),(0.,1.0010559227043),
 .UNSPECIFIED.)
GEOMETRIC_REPRESENTATION_ITEM()
RATIONAL_B_SPLINE_SURFACE(((1.,0.705266242716861,1.00062243213208),(1.,
0.705584085908513,1.00062176089639),(1.,0.706182089449887,1.00062049800536),
(1.,0.706797508586863,1.00061919833528)))
REPRESENTATION_ITEM('')
SURFACE()
);
#2520=(
BOUNDED_SURFACE()
B_SPLINE_SURFACE(3,2,((#198024,#198025,#198026),(#198027,#198028,#198029),
(#198030,#198031,#198032),(#198033,#198034,#198035)),.UNSPECIFIED.,.F.,
 .F.,.F.)
B_SPLINE_SURFACE_WITH_KNOTS((4,4),(3,3),(0.,0.000397394428086619),(0.,1.),
 .UNSPECIFIED.)
GEOMETRIC_REPRESENTATION_ITEM()
RATIONAL_B_SPLINE_SURFACE(((1.,0.70710678118655,1.),(1.,0.706459846759069,
1.),(1.,0.705820510737317,1.),(1.,0.705498956110744,1.)))
REPRESENTATION_ITEM('')
SURFACE()
);
#2521=(
BOUNDED_SURFACE()
B_SPLINE_SURFACE(3,2,((#198041,#198042,#198043),(#198044,#198045,#198046),
(#198047,#198048,#198049),(#198050,#198051,#198052),(#198053,#198054,#198055),
(#198056,#198057,#198058)),.UNSPECIFIED.,.F.,.F.,.F.)
B_SPLINE_SURFACE_WITH_KNOTS((4,2,4),(3,3),(0.,0.000257953807872849,0.000515907615745699),
(0.,1.),.UNSPECIFIED.)
GEOMETRIC_REPRESENTATION_ITEM()
RATIONAL_B_SPLINE_SURFACE(((1.,0.874619707139388,1.),(1.,0.874834349679073,
1.),(1.,0.854686104157671,1.),(1.,0.792476597915277,1.),(1.,0.750887854595045,
1.),(1.,0.705585838031441,1.)))
REPRESENTATION_ITEM('')
SURFACE()
);
#2522=(
BOUNDED_SURFACE()
B_SPLINE_SURFACE(3,2,((#198064,#198065,#198066),(#198067,#198068,#198069),
(#198070,#198071,#198072),(#198073,#198074,#198075)),.UNSPECIFIED.,.F.,
 .F.,.F.)
B_SPLINE_SURFACE_WITH_KNOTS((4,4),(3,3),(0.,0.000511815437699156),(0.,1.00105881331658),
 .UNSPECIFIED.)
GEOMETRIC_REPRESENTATION_ITEM()
RATIONAL_B_SPLINE_SURFACE(((1.,0.706796661946134,1.00062089519759),(1.,
0.707430821225006,1.00061955228502),(1.,0.708058545830511,1.00061822299867),
(1.,0.708394505252524,1.00061751156205)))
REPRESENTATION_ITEM('')
SURFACE()
);
#2523=(
BOUNDED_SURFACE()
B_SPLINE_SURFACE(3,2,((#198077,#198078,#198079),(#198080,#198081,#198082),
(#198083,#198084,#198085),(#198086,#198087,#198088),(#198089,#198090,#198091),
(#198092,#198093,#198094)),.UNSPECIFIED.,.F.,.F.,.F.)
B_SPLINE_SURFACE_WITH_KNOTS((4,2,4),(3,3),(0.,0.000256915317531264,0.000513830635062528),
(0.,1.),.UNSPECIFIED.)
GEOMETRIC_REPRESENTATION_ITEM()
RATIONAL_B_SPLINE_SURFACE(((1.,0.70558583803145,1.),(1.,0.750902433543446,
1.),(1.,0.792329530081587,1.),(1.,0.854288401595139,1.),(1.,0.874998031124452,
1.),(1.,0.874619707139387,1.)))
REPRESENTATION_ITEM('')
SURFACE()
);
#2524=(
BOUNDED_SURFACE()
B_SPLINE_SURFACE(3,2,((#198100,#198101,#198102),(#198103,#198104,#198105),
(#198106,#198107,#198108),(#198109,#198110,#198111),(#198112,#198113,#198114),
(#198115,#198116,#198117)),.UNSPECIFIED.,.F.,.F.,.F.)
B_SPLINE_SURFACE_WITH_KNOTS((4,2,4),(3,3),(0.,0.000256592814262158,0.000513185628524315),
(0.,1.),.UNSPECIFIED.)
GEOMETRIC_REPRESENTATION_ITEM()
RATIONAL_B_SPLINE_SURFACE(((1.,0.708712527163671,1.),(1.,0.753780902613744,
1.),(1.,0.794538995768995,1.),(1.,0.855070770331309,1.),(1.,0.875018427445166,
1.),(1.,0.87461970713939,1.)))
REPRESENTATION_ITEM('')
SURFACE()
);
#2525=(
BOUNDED_SURFACE()
B_SPLINE_SURFACE(3,2,((#198119,#198120,#198121),(#198122,#198123,#198124),
(#198125,#198126,#198127),(#198128,#198129,#198130)),.UNSPECIFIED.,.F.,
 .F.,.F.)
B_SPLINE_SURFACE_WITH_KNOTS((4,4),(3,3),(0.,0.000511815072430398),(0.,1.00105598365828),
 .UNSPECIFIED.)
GEOMETRIC_REPRESENTATION_ITEM()
RATIONAL_B_SPLINE_SURFACE(((1.,0.70679749073386,1.0006192341167),(1.,0.706182062146784,
1.00062053388176),(1.,0.705584062769139,1.00062179683691),(1.,0.705266224770628,
1.00062246810037)))
REPRESENTATION_ITEM('')
SURFACE()
);
#2526=(
BOUNDED_SURFACE()
B_SPLINE_SURFACE(3,2,((#198136,#198137,#198138),(#198139,#198140,#198141),
(#198142,#198143,#198144),(#198145,#198146,#198147),(#198148,#198149,#198150),
(#198151,#198152,#198153)),.UNSPECIFIED.,.F.,.F.,.F.)
B_SPLINE_SURFACE_WITH_KNOTS((4,2,4),(3,3),(1.35525271560688E-20,0.000257652232350883,
0.000515304464701766),(0.,1.),.UNSPECIFIED.)
GEOMETRIC_REPRESENTATION_ITEM()
RATIONAL_B_SPLINE_SURFACE(((1.,0.874619707139378,1.),(1.,0.874861180430966,
1.),(1.,0.855455725920513,1.),(1.,0.794699358955603,1.),(1.,0.753768977788378,
1.),(1.,0.708712527163653,1.)))
REPRESENTATION_ITEM('')
SURFACE()
);
#2527=(
BOUNDED_SURFACE()
B_SPLINE_SURFACE(3,2,((#198159,#198160,#198161),(#198162,#198163,#198164),
(#198165,#198166,#198167),(#198168,#198169,#198170)),.UNSPECIFIED.,.F.,
 .F.,.F.)
B_SPLINE_SURFACE_WITH_KNOTS((4,4),(3,3),(-2.71050543121376E-20,0.00039739437365192),
(0.,1.),.UNSPECIFIED.)
GEOMETRIC_REPRESENTATION_ITEM()
RATIONAL_B_SPLINE_SURFACE(((1.,0.707106781186548,1.),(1.,0.707752587915895,
1.),(1.,0.70837765454067,1.),(1.,0.708689770883327,1.)))
REPRESENTATION_ITEM('')
SURFACE()
);
#2528=(
BOUNDED_SURFACE()
B_SPLINE_SURFACE(3,2,((#198172,#198173,#198174),(#198175,#198176,#198177),
(#198178,#198179,#198180),(#198181,#198182,#198183)),.UNSPECIFIED.,.F.,
 .F.,.F.)
B_SPLINE_SURFACE_WITH_KNOTS((4,4),(3,3),(0.,0.000511815456479787),(0.,1.00105873159873),
 .UNSPECIFIED.)
GEOMETRIC_REPRESENTATION_ITEM()
RATIONAL_B_SPLINE_SURFACE(((1.,0.708394529056677,1.0006174638529),(1.,0.708058564167213,
1.00061817524619),(1.,0.707430835372427,1.00061950443881),(1.,0.706796685880734,
1.00062084722702)))
REPRESENTATION_ITEM('')
SURFACE()
);
#2529=(
BOUNDED_SURFACE()
B_SPLINE_SURFACE(3,2,((#198189,#198190,#198191),(#198192,#198193,#198194),
(#198195,#198196,#198197),(#198198,#198199,#198200)),.UNSPECIFIED.,.F.,
 .F.,.F.)
B_SPLINE_SURFACE_WITH_KNOTS((4,4),(3,3),(0.,0.000397394465448306),(0.,1.),
 .UNSPECIFIED.)
GEOMETRIC_REPRESENTATION_ITEM()
RATIONAL_B_SPLINE_SURFACE(((1.,0.70549895611076,1.),(1.,0.705821764811791,
1.),(1.,0.70646195252114,1.),(1.,0.707106781186548,1.)))
REPRESENTATION_ITEM('')
SURFACE()
);
#2530=(
BOUNDED_SURFACE()
B_SPLINE_SURFACE(3,2,((#198206,#198207,#198208),(#198209,#198210,#198211),
(#198212,#198213,#198214),(#198215,#198216,#198217)),.UNSPECIFIED.,.F.,
 .F.,.F.)
B_SPLINE_SURFACE_WITH_KNOTS((4,4),(3,3),(0.,0.000397394410828732),(0.,1.),
 .UNSPECIFIED.)
GEOMETRIC_REPRESENTATION_ITEM()
RATIONAL_B_SPLINE_SURFACE(((1.,0.70868977088332,1.),(1.,0.708376440034513,
1.),(1.,0.707750498698404,1.),(1.,0.707106781186548,1.)))
REPRESENTATION_ITEM('')
SURFACE()
);
#2531=(
BOUNDED_SURFACE()
B_SPLINE_SURFACE(3,2,((#198223,#198224,#198225),(#198226,#198227,#198228),
(#198229,#198230,#198231),(#198232,#198233,#198234)),.UNSPECIFIED.,.F.,
 .F.,.F.)
B_SPLINE_SURFACE_WITH_KNOTS((4,4),(3,3),(0.,0.000511815090126187),(0.,1.0010559227001),
 .UNSPECIFIED.)
GEOMETRIC_REPRESENTATION_ITEM()
RATIONAL_B_SPLINE_SURFACE(((1.,0.705266242718086,1.0006224321296),(1.,0.705584085909768,
1.00062176089392),(1.,0.706182089451109,1.00062049800289),(1.,0.706797508588093,
1.00061919833282)))
REPRESENTATION_ITEM('')
SURFACE()
);
#2532=(
BOUNDED_SURFACE()
B_SPLINE_SURFACE(3,2,((#198236,#198237,#198238),(#198239,#198240,#198241),
(#198242,#198243,#198244),(#198245,#198246,#198247)),.UNSPECIFIED.,.F.,
 .F.,.F.)
B_SPLINE_SURFACE_WITH_KNOTS((4,4),(3,3),(0.,0.000397394428086622),(0.,1.),
 .UNSPECIFIED.)
GEOMETRIC_REPRESENTATION_ITEM()
RATIONAL_B_SPLINE_SURFACE(((1.,0.707106781186544,1.),(1.,0.706459846759088,
1.),(1.,0.705820510737285,1.),(1.,0.70549895611075,1.)))
REPRESENTATION_ITEM('')
SURFACE()
);
#2533=(
BOUNDED_SURFACE()
B_SPLINE_SURFACE(3,2,((#198253,#198254,#198255),(#198256,#198257,#198258),
(#198259,#198260,#198261),(#198262,#198263,#198264),(#198265,#198266,#198267),
(#198268,#198269,#198270)),.UNSPECIFIED.,.F.,.F.,.F.)
B_SPLINE_SURFACE_WITH_KNOTS((4,2,4),(3,3),(0.,0.000257953807872845,0.000515907615745691),
(0.,1.),.UNSPECIFIED.)
GEOMETRIC_REPRESENTATION_ITEM()
RATIONAL_B_SPLINE_SURFACE(((1.,0.874619707139393,1.),(1.,0.874834349679163,
1.),(1.,0.854686104157555,1.),(1.,0.792476597915392,1.),(1.,0.750887854594916,
1.),(1.,0.705585838031459,1.)))
REPRESENTATION_ITEM('')
SURFACE()
);
#2534=(
BOUNDED_SURFACE()
B_SPLINE_SURFACE(3,2,((#198276,#198277,#198278),(#198279,#198280,#198281),
(#198282,#198283,#198284),(#198285,#198286,#198287)),.UNSPECIFIED.,.F.,
 .F.,.F.)
B_SPLINE_SURFACE_WITH_KNOTS((4,4),(3,3),(0.,0.000511815437699162),(0.,1.00105881331787),
 .UNSPECIFIED.)
GEOMETRIC_REPRESENTATION_ITEM()
RATIONAL_B_SPLINE_SURFACE(((1.,0.706796661945754,1.00062089519835),(1.,
0.707430821224618,1.00061955228577),(1.,0.708058545830163,1.00061822299943),
(1.,0.70839450525214,1.00061751156281)))
REPRESENTATION_ITEM('')
SURFACE()
);
#2535=(
BOUNDED_SURFACE()
B_SPLINE_SURFACE(3,2,((#198289,#198290,#198291),(#198292,#198293,#198294),
(#198295,#198296,#198297),(#198298,#198299,#198300),(#198301,#198302,#198303),
(#198304,#198305,#198306)),.UNSPECIFIED.,.F.,.F.,.F.)
B_SPLINE_SURFACE_WITH_KNOTS((4,2,4),(3,3),(0.,0.000256915317531265,0.000513830635062529),
(0.,1.),.UNSPECIFIED.)
GEOMETRIC_REPRESENTATION_ITEM()
RATIONAL_B_SPLINE_SURFACE(((1.,0.705585838031458,1.),(1.,0.750902433542261,
1.),(1.,0.792329530083196,1.),(1.,0.854288401593537,1.),(1.,0.874998031125653,
1.),(1.,0.87461970713941,1.)))
REPRESENTATION_ITEM('')
SURFACE()
);
#2536=(
BOUNDED_SURFACE()
B_SPLINE_SURFACE(3,2,((#198312,#198313,#198314),(#198315,#198316,#198317),
(#198318,#198319,#198320),(#198321,#198322,#198323),(#198324,#198325,#198326),
(#198327,#198328,#198329)),.UNSPECIFIED.,.F.,.F.,.F.)
B_SPLINE_SURFACE_WITH_KNOTS((4,2,4),(3,3),(0.,0.000256592814262157,0.000513185628524314),
(0.,1.),.UNSPECIFIED.)
GEOMETRIC_REPRESENTATION_ITEM()
RATIONAL_B_SPLINE_SURFACE(((1.,0.708712527163673,1.),(1.,0.753780902613744,
1.),(1.,0.794538995768969,1.),(1.,0.855070770331331,1.),(1.,0.875018427445154,
1.),(1.,0.874619707139393,1.)))
REPRESENTATION_ITEM('')
SURFACE()
);
#2537=(
BOUNDED_SURFACE()
B_SPLINE_SURFACE(3,2,((#198331,#198332,#198333),(#198334,#198335,#198336),
(#198337,#198338,#198339),(#198340,#198341,#198342)),.UNSPECIFIED.,.F.,
 .F.,.F.)
B_SPLINE_SURFACE_WITH_KNOTS((4,4),(3,3),(0.,0.000511815072430393),(0.,1.00105598365973),
 .UNSPECIFIED.)
GEOMETRIC_REPRESENTATION_ITEM()
RATIONAL_B_SPLINE_SURFACE(((1.,0.706797490733436,1.00061923411755),(1.,
0.706182062146356,1.00062053388262),(1.,0.705584062768711,1.00062179683776),
(1.,0.7052662247702,1.00062246810122)))
REPRESENTATION_ITEM('')
SURFACE()
);
#2538=(
BOUNDED_SURFACE()
B_SPLINE_SURFACE(3,2,((#198348,#198349,#198350),(#198351,#198352,#198353),
(#198354,#198355,#198356),(#198357,#198358,#198359),(#198360,#198361,#198362),
(#198363,#198364,#198365)),.UNSPECIFIED.,.F.,.F.,.F.)
B_SPLINE_SURFACE_WITH_KNOTS((4,2,4),(3,3),(-1.70761842166467E-18,0.000257652232350888,
0.000515304464701778),(0.,1.),.UNSPECIFIED.)
GEOMETRIC_REPRESENTATION_ITEM()
RATIONAL_B_SPLINE_SURFACE(((1.,0.874619707139376,1.),(1.,0.874861180430913,
1.),(1.,0.85545572592056,1.),(1.,0.794699358955552,1.),(1.,0.753768977788407,
1.),(1.,0.708712527163644,1.)))
REPRESENTATION_ITEM('')
SURFACE()
);
#2539=(
BOUNDED_SURFACE()
B_SPLINE_SURFACE(3,2,((#198371,#198372,#198373),(#198374,#198375,#198376),
(#198377,#198378,#198379),(#198380,#198381,#198382)),.UNSPECIFIED.,.F.,
 .F.,.F.)
B_SPLINE_SURFACE_WITH_KNOTS((4,4),(3,3),(-7.04731412115578E-18,0.000397394373651905),
(0.,1.),.UNSPECIFIED.)
GEOMETRIC_REPRESENTATION_ITEM()
RATIONAL_B_SPLINE_SURFACE(((1.,0.707106781186542,1.),(1.,0.707752587915911,
1.),(1.,0.708377654540645,1.),(1.,0.708689770883334,1.)))
REPRESENTATION_ITEM('')
SURFACE()
);
#2540=(
BOUNDED_SURFACE()
B_SPLINE_SURFACE(3,2,((#198384,#198385,#198386),(#198387,#198388,#198389),
(#198390,#198391,#198392),(#198393,#198394,#198395)),.UNSPECIFIED.,.F.,
 .F.,.F.)
B_SPLINE_SURFACE_WITH_KNOTS((4,4),(3,3),(0.,0.000511815456479787),(0.,1.00105873159852),
 .UNSPECIFIED.)
GEOMETRIC_REPRESENTATION_ITEM()
RATIONAL_B_SPLINE_SURFACE(((1.,0.708394529056741,1.00061746385278),(1.,
0.708058564167289,1.00061817524607),(1.,0.707430835372482,1.00061950443869),
(1.,0.706796685880791,1.0006208472269)))
REPRESENTATION_ITEM('')
SURFACE()
);
#2541=(
BOUNDED_SURFACE()
B_SPLINE_SURFACE(3,2,((#198401,#198402,#198403),(#198404,#198405,#198406),
(#198407,#198408,#198409),(#198410,#198411,#198412)),.UNSPECIFIED.,.F.,
 .F.,.F.)
B_SPLINE_SURFACE_WITH_KNOTS((4,4),(3,3),(0.,0.000397394465448288),(0.,1.),
 .UNSPECIFIED.)
GEOMETRIC_REPRESENTATION_ITEM()
RATIONAL_B_SPLINE_SURFACE(((1.,0.705498956110755,1.),(1.,0.705821764811768,
1.),(1.,0.706461952521147,1.),(1.,0.707106781186548,1.)))
REPRESENTATION_ITEM('')
SURFACE()
);
#2542=(
BOUNDED_SURFACE()
B_SPLINE_SURFACE(3,2,((#198418,#198419,#198420),(#198421,#198422,#198423),
(#198424,#198425,#198426),(#198427,#198428,#198429)),.UNSPECIFIED.,.F.,
 .F.,.F.)
B_SPLINE_SURFACE_WITH_KNOTS((4,4),(3,3),(0.,0.000397394410828734),(0.,1.),
 .UNSPECIFIED.)
GEOMETRIC_REPRESENTATION_ITEM()
RATIONAL_B_SPLINE_SURFACE(((1.,0.708689770883327,1.),(1.,0.708376440034476,
1.),(1.,0.707750498698407,1.),(1.,0.707106781186548,1.)))
REPRESENTATION_ITEM('')
SURFACE()
);
#2543=(
BOUNDED_SURFACE()
B_SPLINE_SURFACE(3,2,((#198435,#198436,#198437),(#198438,#198439,#198440),
(#198441,#198442,#198443),(#198444,#198445,#198446)),.UNSPECIFIED.,.F.,
 .F.,.F.)
B_SPLINE_SURFACE_WITH_KNOTS((4,4),(3,3),(0.,0.000511815090126176),(0.,1.00105592270127),
 .UNSPECIFIED.)
GEOMETRIC_REPRESENTATION_ITEM()
RATIONAL_B_SPLINE_SURFACE(((1.,0.705266242717785,1.00062243213029),(1.,
0.705584085909388,1.00062176089461),(1.,0.706182089450783,1.00062049800358),
(1.,0.706797508587755,1.0006191983335)))
REPRESENTATION_ITEM('')
SURFACE()
);
#2544=(
BOUNDED_SURFACE()
B_SPLINE_SURFACE(3,2,((#198448,#198449,#198450),(#198451,#198452,#198453),
(#198454,#198455,#198456),(#198457,#198458,#198459)),.UNSPECIFIED.,.F.,
 .F.,.F.)
B_SPLINE_SURFACE_WITH_KNOTS((4,4),(3,3),(-7.56231015308639E-18,0.000397394428086627),
(0.,1.),.UNSPECIFIED.)
GEOMETRIC_REPRESENTATION_ITEM()
RATIONAL_B_SPLINE_SURFACE(((1.,0.707106781186548,1.),(1.,0.70645984675909,
1.),(1.,0.705820510737292,1.),(1.,0.705498956110763,1.)))
REPRESENTATION_ITEM('')
SURFACE()
);
#2545=(
BOUNDED_SURFACE()
B_SPLINE_SURFACE(3,2,((#198465,#198466,#198467),(#198468,#198469,#198470),
(#198471,#198472,#198473),(#198474,#198475,#198476),(#198477,#198478,#198479),
(#198480,#198481,#198482)),.UNSPECIFIED.,.F.,.F.,.F.)
B_SPLINE_SURFACE_WITH_KNOTS((4,2,4),(3,3),(0.,0.000257953807872845,0.00051590761574569),
(0.,1.),.UNSPECIFIED.)
GEOMETRIC_REPRESENTATION_ITEM()
RATIONAL_B_SPLINE_SURFACE(((1.,0.874619707139392,1.),(1.,0.87483434967877,
1.),(1.,0.854686104158095,1.),(1.,0.792476597914846,1.),(1.,0.75088785459531,
1.),(1.,0.705585838031467,1.)))
REPRESENTATION_ITEM('')
SURFACE()
);
#2546=(
BOUNDED_SURFACE()
B_SPLINE_SURFACE(3,2,((#198488,#198489,#198490),(#198491,#198492,#198493),
(#198494,#198495,#198496),(#198497,#198498,#198499)),.UNSPECIFIED.,.F.,
 .F.,.F.)
B_SPLINE_SURFACE_WITH_KNOTS((4,4),(3,3),(-7.56231015308639E-18,0.00051181543769914),
(0.,1.00105881331445),.UNSPECIFIED.)
GEOMETRIC_REPRESENTATION_ITEM()
RATIONAL_B_SPLINE_SURFACE(((1.,0.706796661946756,1.00062089519634),(1.,
0.707430821225626,1.00061955228377),(1.,0.70805854583114,1.00061822299743),
(1.,0.708394505253128,1.00061751156081)))
REPRESENTATION_ITEM('')
SURFACE()
);
#2547=(
BOUNDED_SURFACE()
B_SPLINE_SURFACE(3,2,((#198501,#198502,#198503),(#198504,#198505,#198506),
(#198507,#198508,#198509),(#198510,#198511,#198512),(#198513,#198514,#198515),
(#198516,#198517,#198518)),.UNSPECIFIED.,.F.,.F.,.F.)
B_SPLINE_SURFACE_WITH_KNOTS((4,2,4),(3,3),(0.,0.000256915317531265,0.000513830635062529),
(0.,1.),.UNSPECIFIED.)
GEOMETRIC_REPRESENTATION_ITEM()
RATIONAL_B_SPLINE_SURFACE(((1.,0.705585838031461,1.),(1.,0.750902433542682,
1.),(1.,0.792329530082583,1.),(1.,0.854288401594147,1.),(1.,0.874998031125177,
1.),(1.,0.874619707139394,1.)))
REPRESENTATION_ITEM('')
SURFACE()
);
#2548=(
BOUNDED_SURFACE()
B_SPLINE_SURFACE(3,2,((#198524,#198525,#198526),(#198527,#198528,#198529),
(#198530,#198531,#198532),(#198533,#198534,#198535),(#198536,#198537,#198538),
(#198539,#198540,#198541)),.UNSPECIFIED.,.F.,.F.,.F.)
B_SPLINE_SURFACE_WITH_KNOTS((4,2,4),(3,3),(-9.62229428080885E-18,0.000256592814262153,
0.000513185628524316),(0.,1.),.UNSPECIFIED.)
GEOMETRIC_REPRESENTATION_ITEM()
RATIONAL_B_SPLINE_SURFACE(((1.,0.708712527163657,1.),(1.,0.753780902614083,
1.),(1.,0.794538995768547,1.),(1.,0.855070770331749,1.),(1.,0.875018427444824,
1.),(1.,0.874619707139393,1.)))
REPRESENTATION_ITEM('')
SURFACE()
);
#2549=(
BOUNDED_SURFACE()
B_SPLINE_SURFACE(3,2,((#198543,#198544,#198545),(#198546,#198547,#198548),
(#198549,#198550,#198551),(#198552,#198553,#198554)),.UNSPECIFIED.,.F.,
 .F.,.F.)
B_SPLINE_SURFACE_WITH_KNOTS((4,4),(3,3),(2.71050543121376E-20,0.000511815072430402),
(0.,1.00105598365994),.UNSPECIFIED.)
GEOMETRIC_REPRESENTATION_ITEM()
RATIONAL_B_SPLINE_SURFACE(((1.,0.706797490733375,1.00061923411768),(1.,
0.706182062146284,1.00062053388274),(1.,0.705584062768653,1.00062179683788),
(1.,0.705266224770126,1.00062246810135)))
REPRESENTATION_ITEM('')
SURFACE()
);
#2550=(
BOUNDED_SURFACE()
B_SPLINE_SURFACE(3,2,((#198560,#198561,#198562),(#198563,#198564,#198565),
(#198566,#198567,#198568),(#198569,#198570,#198571),(#198572,#198573,#198574),
(#198575,#198576,#198577)),.UNSPECIFIED.,.F.,.F.,.F.)
B_SPLINE_SURFACE_WITH_KNOTS((4,2,4),(3,3),(-3.34747420754899E-18,0.000257652232350879,
0.000515304464701762),(0.,1.),.UNSPECIFIED.)
GEOMETRIC_REPRESENTATION_ITEM()
RATIONAL_B_SPLINE_SURFACE(((1.,0.874619707139387,1.),(1.,0.874861180430757,
1.),(1.,0.855455725920779,1.),(1.,0.79469935895536,1.),(1.,0.753768977788535,
1.),(1.,0.70871252716367,1.)))
REPRESENTATION_ITEM('')
SURFACE()
);
#2551=(
BOUNDED_SURFACE()
B_SPLINE_SURFACE(3,2,((#198583,#198584,#198585),(#198586,#198587,#198588),
(#198589,#198590,#198591),(#198592,#198593,#198594)),.UNSPECIFIED.,.F.,
 .F.,.F.)
B_SPLINE_SURFACE_WITH_KNOTS((4,4),(3,3),(0.,0.000397394373651928),(0.,1.),
 .UNSPECIFIED.)
GEOMETRIC_REPRESENTATION_ITEM()
RATIONAL_B_SPLINE_SURFACE(((1.,0.707106781186542,1.),(1.,0.70775258791588,
1.),(1.,0.708377654540697,1.),(1.,0.708689770883335,1.)))
REPRESENTATION_ITEM('')
SURFACE()
);
#2552=(
BOUNDED_SURFACE()
B_SPLINE_SURFACE(3,2,((#198596,#198597,#198598),(#198599,#198600,#198601),
(#198602,#198603,#198604),(#198605,#198606,#198607)),.UNSPECIFIED.,.F.,
 .F.,.F.)
B_SPLINE_SURFACE_WITH_KNOTS((4,4),(3,3),(0.,0.000511815456479793),(0.,1.00105873159883),
 .UNSPECIFIED.)
GEOMETRIC_REPRESENTATION_ITEM()
RATIONAL_B_SPLINE_SURFACE(((1.,0.708394529056664,1.00061746385296),(1.,
0.70805856416722,1.00061817524625),(1.,0.707430835372394,1.00061950443887),
(1.,0.706796685880702,1.00062084722708)))
REPRESENTATION_ITEM('')
SURFACE()
);
#2553=(
BOUNDED_SURFACE()
B_SPLINE_SURFACE(3,2,((#198613,#198614,#198615),(#198616,#198617,#198618),
(#198619,#198620,#198621),(#198622,#198623,#198624)),.UNSPECIFIED.,.F.,
 .F.,.F.)
B_SPLINE_SURFACE_WITH_KNOTS((4,4),(3,3),(0.,0.000397394465448311),(0.,1.),
 .UNSPECIFIED.)
GEOMETRIC_REPRESENTATION_ITEM()
RATIONAL_B_SPLINE_SURFACE(((1.,0.705498956110748,1.),(1.,0.705821764811775,
1.),(1.,0.706461952521139,1.),(1.,0.707106781186553,1.)))
REPRESENTATION_ITEM('')
SURFACE()
);
#2554=(
BOUNDED_SURFACE()
B_SPLINE_SURFACE(3,2,((#198630,#198631,#198632),(#198633,#198634,#198635),
(#198636,#198637,#198638),(#198639,#198640,#198641)),.UNSPECIFIED.,.F.,
 .F.,.F.)
B_SPLINE_SURFACE_WITH_KNOTS((4,4),(3,3),(0.,0.000397394410828753),(0.,1.),
 .UNSPECIFIED.)
GEOMETRIC_REPRESENTATION_ITEM()
RATIONAL_B_SPLINE_SURFACE(((1.,0.70868977088332,1.),(1.,0.708376440034504,
1.),(1.,0.707750498698403,1.),(1.,0.707106781186555,1.)))
REPRESENTATION_ITEM('')
SURFACE()
);
#2555=(
BOUNDED_SURFACE()
B_SPLINE_SURFACE(3,2,((#198647,#198648,#198649),(#198650,#198651,#198652),
(#198653,#198654,#198655),(#198656,#198657,#198658)),.UNSPECIFIED.,.F.,
 .F.,.F.)
B_SPLINE_SURFACE_WITH_KNOTS((4,4),(3,3),(0.,0.000511815090126176),(0.,1.00105592270358),
 .UNSPECIFIED.)
GEOMETRIC_REPRESENTATION_ITEM()
RATIONAL_B_SPLINE_SURFACE(((1.,0.705266242717103,1.00062243213165),(1.,
0.705584085908695,1.00062176089597),(1.,0.706182089450119,1.00062049800494),
(1.,0.706797508587078,1.00061919833486)))
REPRESENTATION_ITEM('')
SURFACE()
);
#2556=(
BOUNDED_SURFACE()
B_SPLINE_SURFACE(3,2,((#198660,#198661,#198662),(#198663,#198664,#198665),
(#198666,#198667,#198668),(#198669,#198670,#198671)),.UNSPECIFIED.,.F.,
 .F.,.F.)
B_SPLINE_SURFACE_WITH_KNOTS((4,4),(3,3),(0.,0.000397394428086627),(0.,1.),
 .UNSPECIFIED.)
GEOMETRIC_REPRESENTATION_ITEM()
RATIONAL_B_SPLINE_SURFACE(((1.,0.707106781186548,1.),(1.,0.706459846759099,
1.),(1.,0.705820510737278,1.),(1.,0.705498956110748,1.)))
REPRESENTATION_ITEM('')
SURFACE()
);
#2557=(
BOUNDED_SURFACE()
B_SPLINE_SURFACE(3,2,((#198677,#198678,#198679),(#198680,#198681,#198682),
(#198683,#198684,#198685),(#198686,#198687,#198688),(#198689,#198690,#198691),
(#198692,#198693,#198694)),.UNSPECIFIED.,.F.,.F.,.F.)
B_SPLINE_SURFACE_WITH_KNOTS((4,2,4),(3,3),(0.,0.000257953807872848,0.000515907615745695),
(0.,1.),.UNSPECIFIED.)
GEOMETRIC_REPRESENTATION_ITEM()
RATIONAL_B_SPLINE_SURFACE(((1.,0.874619707139388,1.),(1.,0.874834349678974,
1.),(1.,0.854686104157824,1.),(1.,0.792476597915113,1.),(1.,0.750887854595142,
1.),(1.,0.70558583803144,1.)))
REPRESENTATION_ITEM('')
SURFACE()
);
#2558=(
BOUNDED_SURFACE()
B_SPLINE_SURFACE(3,2,((#198700,#198701,#198702),(#198703,#198704,#198705),
(#198706,#198707,#198708),(#198709,#198710,#198711)),.UNSPECIFIED.,.F.,
 .F.,.F.)
B_SPLINE_SURFACE_WITH_KNOTS((4,4),(3,3),(0.,0.000511815437699155),(0.,1.0010588133174),
 .UNSPECIFIED.)
GEOMETRIC_REPRESENTATION_ITEM()
RATIONAL_B_SPLINE_SURFACE(((1.,0.706796661945892,1.00062089519808),(1.,
0.707430821224748,1.0006195522855),(1.,0.708058545830306,1.00061822299915),
(1.,0.708394505252271,1.00061751156253)))
REPRESENTATION_ITEM('')
SURFACE()
);
#2559=(
BOUNDED_SURFACE()
B_SPLINE_SURFACE(3,2,((#198713,#198714,#198715),(#198716,#198717,#198718),
(#198719,#198720,#198721),(#198722,#198723,#198724),(#198725,#198726,#198727),
(#198728,#198729,#198730)),.UNSPECIFIED.,.F.,.F.,.F.)
B_SPLINE_SURFACE_WITH_KNOTS((4,2,4),(3,3),(2.71050543121376E-20,0.000256915317531262,
0.000513830635062523),(0.,1.),.UNSPECIFIED.)
GEOMETRIC_REPRESENTATION_ITEM()
RATIONAL_B_SPLINE_SURFACE(((1.,0.705585838031443,1.),(1.,0.750902433542627,
1.),(1.,0.79232953008266,1.),(1.,0.854288401594061,1.),(1.,0.874998031125236,
1.),(1.,0.874619707139394,1.)))
REPRESENTATION_ITEM('')
SURFACE()
);
#2560=(
BOUNDED_SURFACE()
B_SPLINE_SURFACE(3,2,((#198736,#198737,#198738),(#198739,#198740,#198741),
(#198742,#198743,#198744),(#198745,#198746,#198747),(#198748,#198749,#198750),
(#198751,#198752,#198753)),.UNSPECIFIED.,.F.,.F.,.F.)
B_SPLINE_SURFACE_WITH_KNOTS((4,2,4),(3,3),(0.,0.000256592814262158,0.000513185628524317),
(0.,1.),.UNSPECIFIED.)
GEOMETRIC_REPRESENTATION_ITEM()
RATIONAL_B_SPLINE_SURFACE(((1.,0.708712527163662,1.),(1.,0.753780902613367,
1.),(1.,0.794538995769507,1.),(1.,0.855070770330791,1.),(1.,0.875018427445557,
1.),(1.,0.874619707139389,1.)))
REPRESENTATION_ITEM('')
SURFACE()
);
#2561=(
BOUNDED_SURFACE()
B_SPLINE_SURFACE(3,2,((#198755,#198756,#198757),(#198758,#198759,#198760),
(#198761,#198762,#198763),(#198764,#198765,#198766)),.UNSPECIFIED.,.F.,
 .F.,.F.)
B_SPLINE_SURFACE_WITH_KNOTS((4,4),(3,3),(0.,0.000511815072430394),(0.,1.00105598365809),
 .UNSPECIFIED.)
GEOMETRIC_REPRESENTATION_ITEM()
RATIONAL_B_SPLINE_SURFACE(((1.,0.706797490733914,1.00061923411659),(1.,
0.706182062146832,1.00062053388166),(1.,0.705584062769191,1.0006217968368),
(1.,0.705266224770676,1.00062246810026)))
REPRESENTATION_ITEM('')
SURFACE()
);
#2562=(
BOUNDED_SURFACE()
B_SPLINE_SURFACE(3,2,((#198772,#198773,#198774),(#198775,#198776,#198777),
(#198778,#198779,#198780),(#198781,#198782,#198783),(#198784,#198785,#198786),
(#198787,#198788,#198789)),.UNSPECIFIED.,.F.,.F.,.F.)
B_SPLINE_SURFACE_WITH_KNOTS((4,2,4),(3,3),(1.35525271560688E-20,0.000257652232350875,
0.00051530446470175),(0.,1.),.UNSPECIFIED.)
GEOMETRIC_REPRESENTATION_ITEM()
RATIONAL_B_SPLINE_SURFACE(((1.,0.87461970713939,1.),(1.,0.874861180430533,
1.),(1.,0.855455725921098,1.),(1.,0.794699358955019,1.),(1.,0.753768977788807,
1.),(1.,0.708712527163686,1.)))
REPRESENTATION_ITEM('')
SURFACE()
);
#2563=(
BOUNDED_SURFACE()
B_SPLINE_SURFACE(3,2,((#198795,#198796,#198797),(#198798,#198799,#198800),
(#198801,#198802,#198803),(#198804,#198805,#198806)),.UNSPECIFIED.,.F.,
 .F.,.F.)
B_SPLINE_SURFACE_WITH_KNOTS((4,4),(3,3),(0.,0.000397394373651918),(0.,1.),
 .UNSPECIFIED.)
GEOMETRIC_REPRESENTATION_ITEM()
RATIONAL_B_SPLINE_SURFACE(((1.,0.707106781186539,1.),(1.,0.707752587915889,
1.),(1.,0.708377654540736,1.),(1.,0.708689770883308,1.)))
REPRESENTATION_ITEM('')
SURFACE()
);
#2564=(
BOUNDED_SURFACE()
B_SPLINE_SURFACE(3,2,((#198808,#198809,#198810),(#198811,#198812,#198813),
(#198814,#198815,#198816),(#198817,#198818,#198819)),.UNSPECIFIED.,.F.,
 .F.,.F.)
B_SPLINE_SURFACE_WITH_KNOTS((4,4),(3,3),(0.,0.000511815456479787),(0.,1.00105873159994),
 .UNSPECIFIED.)
GEOMETRIC_REPRESENTATION_ITEM()
RATIONAL_B_SPLINE_SURFACE(((1.,0.708394529056337,1.00061746385361),(1.,
0.708058564166901,1.0006181752469),(1.,0.707430835372077,1.00061950443952),
(1.,0.706796685880364,1.00062084722773)))
REPRESENTATION_ITEM('')
SURFACE()
);
#2565=(
BOUNDED_SURFACE()
B_SPLINE_SURFACE(3,2,((#198825,#198826,#198827),(#198828,#198829,#198830),
(#198831,#198832,#198833),(#198834,#198835,#198836)),.UNSPECIFIED.,.F.,
 .F.,.F.)
B_SPLINE_SURFACE_WITH_KNOTS((4,4),(3,3),(0.,0.000397394465448305),(0.,1.),
 .UNSPECIFIED.)
GEOMETRIC_REPRESENTATION_ITEM()
RATIONAL_B_SPLINE_SURFACE(((1.,0.70549895611075,1.),(1.,0.705821764811781,
1.),(1.,0.706461952521129,1.),(1.,0.707106781186548,1.)))
REPRESENTATION_ITEM('')
SURFACE()
);
#2566=(
BOUNDED_SURFACE()
B_SPLINE_SURFACE(3,2,((#198842,#198843,#198844),(#198845,#198846,#198847),
(#198848,#198849,#198850),(#198851,#198852,#198853)),.UNSPECIFIED.,.F.,
 .F.,.F.)
B_SPLINE_SURFACE_WITH_KNOTS((4,4),(3,3),(0.,0.000397394410828723),(0.,1.),
 .UNSPECIFIED.)
GEOMETRIC_REPRESENTATION_ITEM()
RATIONAL_B_SPLINE_SURFACE(((1.,0.708689770883325,1.),(1.,0.708376440034514,
1.),(1.,0.707750498698386,1.),(1.,0.707106781186546,1.)))
REPRESENTATION_ITEM('')
SURFACE()
);
#2567=(
BOUNDED_SURFACE()
B_SPLINE_SURFACE(3,2,((#198859,#198860,#198861),(#198862,#198863,#198864),
(#198865,#198866,#198867),(#198868,#198869,#198870)),.UNSPECIFIED.,.F.,
 .F.,.F.)
B_SPLINE_SURFACE_WITH_KNOTS((4,4),(3,3),(0.,0.000511815090126178),(0.,1.00105592270211),
 .UNSPECIFIED.)
GEOMETRIC_REPRESENTATION_ITEM()
RATIONAL_B_SPLINE_SURFACE(((1.,0.705266242717508,1.00062243213079),(1.,
0.705584085909156,1.0006217608951),(1.,0.706182089450541,1.00062049800407),
(1.,0.706797508587497,1.000619198334)))
REPRESENTATION_ITEM('')
SURFACE()
);
#2568=(
BOUNDED_SURFACE()
B_SPLINE_SURFACE(3,2,((#198872,#198873,#198874),(#198875,#198876,#198877),
(#198878,#198879,#198880),(#198881,#198882,#198883)),.UNSPECIFIED.,.F.,
 .F.,.F.)
B_SPLINE_SURFACE_WITH_KNOTS((4,4),(3,3),(0.,0.000397394428086619),(0.,1.),
 .UNSPECIFIED.)
GEOMETRIC_REPRESENTATION_ITEM()
RATIONAL_B_SPLINE_SURFACE(((1.,0.707106781186549,1.),(1.,0.706459846759122,
1.),(1.,0.705820510737269,1.),(1.,0.705498956110763,1.)))
REPRESENTATION_ITEM('')
SURFACE()
);
#2569=(
BOUNDED_SURFACE()
B_SPLINE_SURFACE(3,2,((#198889,#198890,#198891),(#198892,#198893,#198894),
(#198895,#198896,#198897),(#198898,#198899,#198900),(#198901,#198902,#198903),
(#198904,#198905,#198906)),.UNSPECIFIED.,.F.,.F.,.F.)
B_SPLINE_SURFACE_WITH_KNOTS((4,2,4),(3,3),(0.,0.000257953807872851,0.000515907615745703),
(0.,1.),.UNSPECIFIED.)
GEOMETRIC_REPRESENTATION_ITEM()
RATIONAL_B_SPLINE_SURFACE(((1.,0.874619707139391,1.),(1.,0.874834349679242,
1.),(1.,0.854686104157454,1.),(1.,0.792476597915482,1.),(1.,0.750887854594861,
1.),(1.,0.70558583803145,1.)))
REPRESENTATION_ITEM('')
SURFACE()
);
#2570=(
BOUNDED_SURFACE()
B_SPLINE_SURFACE(3,2,((#198912,#198913,#198914),(#198915,#198916,#198917),
(#198918,#198919,#198920),(#198921,#198922,#198923)),.UNSPECIFIED.,.F.,
 .F.,.F.)
B_SPLINE_SURFACE_WITH_KNOTS((4,4),(3,3),(0.,0.000511815437699147),(0.,1.00105881331765),
 .UNSPECIFIED.)
GEOMETRIC_REPRESENTATION_ITEM()
RATIONAL_B_SPLINE_SURFACE(((1.,0.706796661945819,1.00062089519822),(1.,
0.707430821224719,1.00061955228564),(1.,0.708058545830186,1.0006182229993),
(1.,0.7083945052522,1.00061751156268)))
REPRESENTATION_ITEM('')
SURFACE()
);
#2571=(
BOUNDED_SURFACE()
B_SPLINE_SURFACE(3,2,((#198925,#198926,#198927),(#198928,#198929,#198930),
(#198931,#198932,#198933),(#198934,#198935,#198936),(#198937,#198938,#198939),
(#198940,#198941,#198942)),.UNSPECIFIED.,.F.,.F.,.F.)
B_SPLINE_SURFACE_WITH_KNOTS((4,2,4),(3,3),(0.,0.00025691531753126,0.00051383063506252),
(0.,1.),.UNSPECIFIED.)
GEOMETRIC_REPRESENTATION_ITEM()
RATIONAL_B_SPLINE_SURFACE(((1.,0.705585838031443,1.),(1.,0.75090243354212,
1.),(1.,0.792329530083374,1.),(1.,0.854288401593351,1.),(1.,0.874998031125783,
1.),(1.,0.874619707139395,1.)))
REPRESENTATION_ITEM('')
SURFACE()
);
#2572=(
BOUNDED_SURFACE()
B_SPLINE_SURFACE(3,2,((#198948,#198949,#198950),(#198951,#198952,#198953),
(#198954,#198955,#198956),(#198957,#198958,#198959),(#198960,#198961,#198962),
(#198963,#198964,#198965)),.UNSPECIFIED.,.F.,.F.,.F.)
B_SPLINE_SURFACE_WITH_KNOTS((4,2,4),(3,3),(-5.77337656848531E-18,0.000256592814262152,
0.00051318562852431),(0.,1.),.UNSPECIFIED.)
GEOMETRIC_REPRESENTATION_ITEM()
RATIONAL_B_SPLINE_SURFACE(((1.,0.708712527163664,1.),(1.,0.753780902613285,
1.),(1.,0.794538995769614,1.),(1.,0.855070770330688,1.),(1.,0.87501842744564,
1.),(1.,0.874619707139388,1.)))
REPRESENTATION_ITEM('')
SURFACE()
);
#2573=(
BOUNDED_SURFACE()
B_SPLINE_SURFACE(3,2,((#198967,#198968,#198969),(#198970,#198971,#198972),
(#198973,#198974,#198975),(#198976,#198977,#198978)),.UNSPECIFIED.,.F.,
 .F.,.F.)
B_SPLINE_SURFACE_WITH_KNOTS((4,4),(3,3),(0.,0.000511815072430395),(0.,1.00105598365917),
 .UNSPECIFIED.)
GEOMETRIC_REPRESENTATION_ITEM()
RATIONAL_B_SPLINE_SURFACE(((1.,0.706797490733591,1.00061923411722),(1.,
0.706182062146506,1.00062053388229),(1.,0.705584062768884,1.00062179683743),
(1.,0.70526622477036,1.00062246810089)))
REPRESENTATION_ITEM('')
SURFACE()
);
#2574=(
BOUNDED_SURFACE()
B_SPLINE_SURFACE(3,2,((#198984,#198985,#198986),(#198987,#198988,#198989),
(#198990,#198991,#198992),(#198993,#198994,#198995),(#198996,#198997,#198998),
(#198999,#199000,#199001)),.UNSPECIFIED.,.F.,.F.,.F.)
B_SPLINE_SURFACE_WITH_KNOTS((4,2,4),(3,3),(-3.13063377305189E-18,0.000257652232350879,
0.00051530446470176),(0.,1.),.UNSPECIFIED.)
GEOMETRIC_REPRESENTATION_ITEM()
RATIONAL_B_SPLINE_SURFACE(((1.,0.874619707139394,1.),(1.,0.874861180430667,
1.),(1.,0.855455725920895,1.),(1.,0.794699358955227,1.),(1.,0.75376897778868,
1.),(1.,0.708712527163649,1.)))
REPRESENTATION_ITEM('')
SURFACE()
);
#2575=(
BOUNDED_SURFACE()
B_SPLINE_SURFACE(3,2,((#199007,#199008,#199009),(#199010,#199011,#199012),
(#199013,#199014,#199015),(#199016,#199017,#199018)),.UNSPECIFIED.,.F.,
 .F.,.F.)
B_SPLINE_SURFACE_WITH_KNOTS((4,4),(3,3),(0.,0.000397394373651914),(0.,1.),
 .UNSPECIFIED.)
GEOMETRIC_REPRESENTATION_ITEM()
RATIONAL_B_SPLINE_SURFACE(((1.,0.707106781186546,1.),(1.,0.707752587915888,
1.),(1.,0.708377654540688,1.),(1.,0.708689770883326,1.)))
REPRESENTATION_ITEM('')
SURFACE()
);
#2576=(
BOUNDED_SURFACE()
B_SPLINE_SURFACE(3,2,((#199020,#199021,#199022),(#199023,#199024,#199025),
(#199026,#199027,#199028),(#199029,#199030,#199031)),.UNSPECIFIED.,.F.,
 .F.,.F.)
B_SPLINE_SURFACE_WITH_KNOTS((4,4),(3,3),(0.,0.000511815456479789),(0.,1.00105873159875),
 .UNSPECIFIED.)
GEOMETRIC_REPRESENTATION_ITEM()
RATIONAL_B_SPLINE_SURFACE(((1.,0.708394529056679,1.00061746385291),(1.,
0.708058564167215,1.0006181752462),(1.,0.707430835372418,1.00061950443882),
(1.,0.706796685880729,1.00062084722703)))
REPRESENTATION_ITEM('')
SURFACE()
);
#2577=(
BOUNDED_SURFACE()
B_SPLINE_SURFACE(3,2,((#199037,#199038,#199039),(#199040,#199041,#199042),
(#199043,#199044,#199045),(#199046,#199047,#199048)),.UNSPECIFIED.,.F.,
 .F.,.F.)
B_SPLINE_SURFACE_WITH_KNOTS((4,4),(3,3),(0.,0.000397394465448298),(0.,1.),
 .UNSPECIFIED.)
GEOMETRIC_REPRESENTATION_ITEM()
RATIONAL_B_SPLINE_SURFACE(((1.,0.705498956110748,1.),(1.,0.705821764811764,
1.),(1.,0.706461952521152,1.),(1.,0.707106781186548,1.)))
REPRESENTATION_ITEM('')
SURFACE()
);
#2578=(
BOUNDED_SURFACE()
B_SPLINE_SURFACE(3,2,((#199054,#199055,#199056),(#199057,#199058,#199059),
(#199060,#199061,#199062),(#199063,#199064,#199065)),.UNSPECIFIED.,.F.,
 .F.,.F.)
B_SPLINE_SURFACE_WITH_KNOTS((4,4),(3,3),(0.,0.000397394410828738),(0.,1.),
 .UNSPECIFIED.)
GEOMETRIC_REPRESENTATION_ITEM()
RATIONAL_B_SPLINE_SURFACE(((1.,0.70868977088332,1.),(1.,0.708376440034514,
1.),(1.,0.707750498698361,1.),(1.,0.70710678118657,1.)))
REPRESENTATION_ITEM('')
SURFACE()
);
#2579=(
BOUNDED_SURFACE()
B_SPLINE_SURFACE(3,2,((#199071,#199072,#199073),(#199074,#199075,#199076),
(#199077,#199078,#199079),(#199080,#199081,#199082)),.UNSPECIFIED.,.F.,
 .F.,.F.)
B_SPLINE_SURFACE_WITH_KNOTS((4,4),(3,3),(0.,0.000511815090126175),(0.,1.00105592270382),
 .UNSPECIFIED.)
GEOMETRIC_REPRESENTATION_ITEM()
RATIONAL_B_SPLINE_SURFACE(((1.,0.705266242717021,1.00062243213179),(1.,
0.705584085908677,1.00062176089611),(1.,0.706182089450028,1.00062049800508),
(1.,0.706797508586997,1.000619198335)))
REPRESENTATION_ITEM('')
SURFACE()
);
#2580=(
BOUNDED_SURFACE()
B_SPLINE_SURFACE(3,2,((#199084,#199085,#199086),(#199087,#199088,#199089),
(#199090,#199091,#199092),(#199093,#199094,#199095)),.UNSPECIFIED.,.F.,
 .F.,.F.)
B_SPLINE_SURFACE_WITH_KNOTS((4,4),(3,3),(0.,0.000397394428086619),(0.,1.),
 .UNSPECIFIED.)
GEOMETRIC_REPRESENTATION_ITEM()
RATIONAL_B_SPLINE_SURFACE(((1.,0.707106781186548,1.),(1.,0.706459846759101,
1.),(1.,0.705820510737285,1.),(1.,0.705498956110761,1.)))
REPRESENTATION_ITEM('')
SURFACE()
);
#2581=(
BOUNDED_SURFACE()
B_SPLINE_SURFACE(3,2,((#199101,#199102,#199103),(#199104,#199105,#199106),
(#199107,#199108,#199109),(#199110,#199111,#199112),(#199113,#199114,#199115),
(#199116,#199117,#199118)),.UNSPECIFIED.,.F.,.F.,.F.)
B_SPLINE_SURFACE_WITH_KNOTS((4,2,4),(3,3),(0.,0.000257953807872853,0.000515907615745706),
(0.,1.),.UNSPECIFIED.)
GEOMETRIC_REPRESENTATION_ITEM()
RATIONAL_B_SPLINE_SURFACE(((1.,0.874619707139386,1.),(1.,0.874834349678556,
1.),(1.,0.854686104158394,1.),(1.,0.792476597914528,1.),(1.,0.750887854595574,
1.),(1.,0.705585838031473,1.)))
REPRESENTATION_ITEM('')
SURFACE()
);
#2582=(
BOUNDED_SURFACE()
B_SPLINE_SURFACE(3,2,((#199124,#199125,#199126),(#199127,#199128,#199129),
(#199130,#199131,#199132),(#199133,#199134,#199135)),.UNSPECIFIED.,.F.,
 .F.,.F.)
B_SPLINE_SURFACE_WITH_KNOTS((4,4),(3,3),(-5.52943107967607E-18,0.000511815437699143),
(0.,1.00105881331528),.UNSPECIFIED.)
GEOMETRIC_REPRESENTATION_ITEM()
RATIONAL_B_SPLINE_SURFACE(((1.,0.706796661946501,1.00062089519683),(1.,
0.707430821225412,1.00061955228425),(1.,0.70805854583087,1.00061822299791),
(1.,0.708394505252892,1.00061751156129)))
REPRESENTATION_ITEM('')
SURFACE()
);
#2583=(
BOUNDED_SURFACE()
B_SPLINE_SURFACE(3,2,((#199137,#199138,#199139),(#199140,#199141,#199142),
(#199143,#199144,#199145),(#199146,#199147,#199148),(#199149,#199150,#199151),
(#199152,#199153,#199154)),.UNSPECIFIED.,.F.,.F.,.F.)
B_SPLINE_SURFACE_WITH_KNOTS((4,2,4),(3,3),(0.,0.000256915317531257,0.000513830635062514),
(0.,1.),.UNSPECIFIED.)
GEOMETRIC_REPRESENTATION_ITEM()
RATIONAL_B_SPLINE_SURFACE(((1.,0.705585838031436,1.),(1.,0.750902433542675,
1.),(1.,0.792329530082598,1.),(1.,0.854288401594112,1.),(1.,0.874998031125178,
1.),(1.,0.874619707139397,1.)))
REPRESENTATION_ITEM('')
SURFACE()
);
#2584=(
BOUNDED_SURFACE()
B_SPLINE_SURFACE(3,2,((#199160,#199161,#199162),(#199163,#199164,#199165),
(#199166,#199167,#199168),(#199169,#199170,#199171),(#199172,#199173,#199174),
(#199175,#199176,#199177)),.UNSPECIFIED.,.F.,.F.,.F.)
B_SPLINE_SURFACE_WITH_KNOTS((4,2,4),(3,3),(0.,0.000256592814262161,0.000513185628524321),
(0.,1.),.UNSPECIFIED.)
GEOMETRIC_REPRESENTATION_ITEM()
RATIONAL_B_SPLINE_SURFACE(((1.,0.70871252716365,1.),(1.,0.753780902613521,
1.),(1.,0.794538995769307,1.),(1.,0.855070770330992,1.),(1.,0.875018427445423,
1.),(1.,0.874619707139387,1.)))
REPRESENTATION_ITEM('')
SURFACE()
);
#2585=(
BOUNDED_SURFACE()
B_SPLINE_SURFACE(3,2,((#199179,#199180,#199181),(#199182,#199183,#199184),
(#199185,#199186,#199187),(#199188,#199189,#199190)),.UNSPECIFIED.,.F.,
 .F.,.F.)
B_SPLINE_SURFACE_WITH_KNOTS((4,4),(3,3),(-2.71050543121376E-20,0.000511815072430412),
(0.,1.00105598365811),.UNSPECIFIED.)
GEOMETRIC_REPRESENTATION_ITEM()
RATIONAL_B_SPLINE_SURFACE(((1.,0.70679749073391,1.0006192341166),(1.,0.706182062146828,
1.00062053388166),(1.,0.705584062769189,1.0006217968368),(1.,0.705266224770668,
1.00062246810027)))
REPRESENTATION_ITEM('')
SURFACE()
);
#2586=(
BOUNDED_SURFACE()
B_SPLINE_SURFACE(3,2,((#199196,#199197,#199198),(#199199,#199200,#199201),
(#199202,#199203,#199204),(#199205,#199206,#199207),(#199208,#199209,#199210),
(#199211,#199212,#199213)),.UNSPECIFIED.,.F.,.F.,.F.)
B_SPLINE_SURFACE_WITH_KNOTS((4,2,4),(3,3),(-1.35525271560688E-20,0.000257652232350877,
0.000515304464701753),(0.,1.),.UNSPECIFIED.)
GEOMETRIC_REPRESENTATION_ITEM()
RATIONAL_B_SPLINE_SURFACE(((1.,0.874619707139393,1.),(1.,0.874861180430549,
1.),(1.,0.855455725921079,1.),(1.,0.794699358955038,1.),(1.,0.753768977788861,
1.),(1.,0.708712527163647,1.)))
REPRESENTATION_ITEM('')
SURFACE()
);
#2587=(
BOUNDED_SURFACE()
B_SPLINE_SURFACE(3,2,((#199219,#199220,#199221),(#199222,#199223,#199224),
(#199225,#199226,#199227),(#199228,#199229,#199230)),.UNSPECIFIED.,.F.,
 .F.,.F.)
B_SPLINE_SURFACE_WITH_KNOTS((4,4),(3,3),(-9.54097911787244E-18,0.000397394373651899),
(0.,1.),.UNSPECIFIED.)
GEOMETRIC_REPRESENTATION_ITEM()
RATIONAL_B_SPLINE_SURFACE(((1.,0.707106781186559,1.),(1.,0.707752587915868,
1.),(1.,0.708377654540717,1.),(1.,0.708689770883331,1.)))
REPRESENTATION_ITEM('')
SURFACE()
);
#2588=(
BOUNDED_SURFACE()
B_SPLINE_SURFACE(3,2,((#199232,#199233,#199234),(#199235,#199236,#199237),
(#199238,#199239,#199240),(#199241,#199242,#199243)),.UNSPECIFIED.,.F.,
 .F.,.F.)
B_SPLINE_SURFACE_WITH_KNOTS((4,4),(3,3),(-6.42389787197661E-18,0.000511815456479784),
(0.,1.00105873159871),.UNSPECIFIED.)
GEOMETRIC_REPRESENTATION_ITEM()
RATIONAL_B_SPLINE_SURFACE(((1.,0.708394529056701,1.00061746385289),(1.,
0.708058564167209,1.00061817524618),(1.,0.707430835372458,1.0006195044388),
(1.,0.706796685880743,1.00062084722701)))
REPRESENTATION_ITEM('')
SURFACE()
);
#2589=(
BOUNDED_SURFACE()
B_SPLINE_SURFACE(3,2,((#199249,#199250,#199251),(#199252,#199253,#199254),
(#199255,#199256,#199257),(#199258,#199259,#199260)),.UNSPECIFIED.,.F.,
 .F.,.F.)
B_SPLINE_SURFACE_WITH_KNOTS((4,4),(3,3),(0.,0.000397394465448303),(0.,1.),
 .UNSPECIFIED.)
GEOMETRIC_REPRESENTATION_ITEM()
RATIONAL_B_SPLINE_SURFACE(((1.,0.705498956110736,1.),(1.,0.705821764811768,
1.),(1.,0.706461952521143,1.),(1.,0.707106781186548,1.)))
REPRESENTATION_ITEM('')
SURFACE()
);
#2590=(
BOUNDED_SURFACE()
B_SPLINE_SURFACE(3,2,((#199266,#199267,#199268),(#199269,#199270,#199271),
(#199272,#199273,#199274),(#199275,#199276,#199277)),.UNSPECIFIED.,.F.,
 .F.,.F.)
B_SPLINE_SURFACE_WITH_KNOTS((4,4),(3,3),(0.,0.00039739441082874),(0.,1.),
 .UNSPECIFIED.)
GEOMETRIC_REPRESENTATION_ITEM()
RATIONAL_B_SPLINE_SURFACE(((1.,0.708689770883341,1.),(1.,0.708376440034484,
1.),(1.,0.707750498698422,1.),(1.,0.707106781186548,1.)))
REPRESENTATION_ITEM('')
SURFACE()
);
#2591=(
BOUNDED_SURFACE()
B_SPLINE_SURFACE(3,2,((#199283,#199284,#199285),(#199286,#199287,#199288),
(#199289,#199290,#199291),(#199292,#199293,#199294)),.UNSPECIFIED.,.F.,
 .F.,.F.)
B_SPLINE_SURFACE_WITH_KNOTS((4,4),(3,3),(0.,0.00051181509012618),(0.,1.0010559227041),
 .UNSPECIFIED.)
GEOMETRIC_REPRESENTATION_ITEM()
RATIONAL_B_SPLINE_SURFACE(((1.,0.705266242716924,1.00062243213196),(1.,
0.705584085908585,1.00062176089628),(1.,0.706182089449929,1.00062049800524),
(1.,0.706797508586937,1.00061919833517)))
REPRESENTATION_ITEM('')
SURFACE()
);
#2592=(
BOUNDED_SURFACE()
B_SPLINE_SURFACE(3,2,((#199296,#199297,#199298),(#199299,#199300,#199301),
(#199302,#199303,#199304),(#199305,#199306,#199307)),.UNSPECIFIED.,.F.,
 .F.,.F.)
B_SPLINE_SURFACE_WITH_KNOTS((4,4),(3,3),(0.,0.00039739442808663),(0.,1.),
 .UNSPECIFIED.)
GEOMETRIC_REPRESENTATION_ITEM()
RATIONAL_B_SPLINE_SURFACE(((1.,0.707106781186535,1.),(1.,0.706459846759098,
1.),(1.,0.705820510737295,1.),(1.,0.705498956110716,1.)))
REPRESENTATION_ITEM('')
SURFACE()
);
#2593=(
BOUNDED_SURFACE()
B_SPLINE_SURFACE(3,2,((#199313,#199314,#199315),(#199316,#199317,#199318),
(#199319,#199320,#199321),(#199322,#199323,#199324),(#199325,#199326,#199327),
(#199328,#199329,#199330)),.UNSPECIFIED.,.F.,.F.,.F.)
B_SPLINE_SURFACE_WITH_KNOTS((4,2,4),(3,3),(0.,0.000257953807872849,0.000515907615745698),
(0.,1.),.UNSPECIFIED.)
GEOMETRIC_REPRESENTATION_ITEM()
RATIONAL_B_SPLINE_SURFACE(((1.,0.874619707139392,1.),(1.,0.874834349679019,
1.),(1.,0.854686104157764,1.),(1.,0.792476597915158,1.),(1.,0.750887854595128,
1.),(1.,0.705585838031423,1.)))
REPRESENTATION_ITEM('')
SURFACE()
);
#2594=(
BOUNDED_SURFACE()
B_SPLINE_SURFACE(3,2,((#199336,#199337,#199338),(#199339,#199340,#199341),
(#199342,#199343,#199344),(#199345,#199346,#199347)),.UNSPECIFIED.,.F.,
 .F.,.F.)
B_SPLINE_SURFACE_WITH_KNOTS((4,4),(3,3),(0.,0.000511815437699143),(0.,1.00105881331394),
 .UNSPECIFIED.)
GEOMETRIC_REPRESENTATION_ITEM()
RATIONAL_B_SPLINE_SURFACE(((1.,0.706796661946904,1.00062089519605),(1.,
0.707430821225788,1.00061955228347),(1.,0.708058545831295,1.00061822299713),
(1.,0.70839450525329,1.00061751156051)))
REPRESENTATION_ITEM('')
SURFACE()
);
#2595=(
BOUNDED_SURFACE()
B_SPLINE_SURFACE(3,2,((#199349,#199350,#199351),(#199352,#199353,#199354),
(#199355,#199356,#199357),(#199358,#199359,#199360),(#199361,#199362,#199363),
(#199364,#199365,#199366)),.UNSPECIFIED.,.F.,.F.,.F.)
B_SPLINE_SURFACE_WITH_KNOTS((4,2,4),(3,3),(2.71050543121376E-20,0.000256915317531268,
0.000513830635062535),(0.,1.),.UNSPECIFIED.)
GEOMETRIC_REPRESENTATION_ITEM()
RATIONAL_B_SPLINE_SURFACE(((1.,0.705585838031462,1.),(1.,0.750902433543319,
1.),(1.,0.792329530081728,1.),(1.,0.854288401595,1.),(1.,0.874998031124529,
1.),(1.,0.874619707139394,1.)))
REPRESENTATION_ITEM('')
SURFACE()
);
#2596=(
BOUNDED_SURFACE()
B_SPLINE_SURFACE(3,2,((#199372,#199373,#199374),(#199375,#199376,#199377),
(#199378,#199379,#199380),(#199381,#199382,#199383),(#199384,#199385,#199386),
(#199387,#199388,#199389)),.UNSPECIFIED.,.F.,.F.,.F.)
B_SPLINE_SURFACE_WITH_KNOTS((4,2,4),(3,3),(-9.32413868337534E-18,0.000256592814262153,
0.000513185628524316),(0.,1.),.UNSPECIFIED.)
GEOMETRIC_REPRESENTATION_ITEM()
RATIONAL_B_SPLINE_SURFACE(((1.,0.708712527163675,1.),(1.,0.753780902613644,
1.),(1.,0.794538995769133,1.),(1.,0.855070770331152,1.),(1.,0.875018427445311,
1.),(1.,0.874619707139391,1.)))
REPRESENTATION_ITEM('')
SURFACE()
);
#2597=(
BOUNDED_SURFACE()
B_SPLINE_SURFACE(3,2,((#199391,#199392,#199393),(#199394,#199395,#199396),
(#199397,#199398,#199399),(#199400,#199401,#199402)),.UNSPECIFIED.,.F.,
 .F.,.F.)
B_SPLINE_SURFACE_WITH_KNOTS((4,4),(3,3),(0.,0.000511815072430403),(0.,1.00105598365889),
 .UNSPECIFIED.)
GEOMETRIC_REPRESENTATION_ITEM()
RATIONAL_B_SPLINE_SURFACE(((1.,0.706797490733682,1.00061923411706),(1.,
0.706182062146602,1.00062053388212),(1.,0.705584062768974,1.00062179683726),
(1.,0.705266224770452,1.00062246810073)))
REPRESENTATION_ITEM('')
SURFACE()
);
#2598=(
BOUNDED_SURFACE()
B_SPLINE_SURFACE(3,2,((#199408,#199409,#199410),(#199411,#199412,#199413),
(#199414,#199415,#199416),(#199417,#199418,#199419),(#199420,#199421,#199422),
(#199423,#199424,#199425)),.UNSPECIFIED.,.F.,.F.,.F.)
B_SPLINE_SURFACE_WITH_KNOTS((4,2,4),(3,3),(0.,0.000257652232350887,0.000515304464701775),
(0.,1.),.UNSPECIFIED.)
GEOMETRIC_REPRESENTATION_ITEM()
RATIONAL_B_SPLINE_SURFACE(((1.,0.874619707139393,1.),(1.,0.874861180430824,
1.),(1.,0.855455725920693,1.),(1.,0.794699358955462,1.),(1.,0.753768977788463,
1.),(1.,0.708712527163685,1.)))
REPRESENTATION_ITEM('')
SURFACE()
);
#2599=(
BOUNDED_SURFACE()
B_SPLINE_SURFACE(3,2,((#199431,#199432,#199433),(#199434,#199435,#199436),
(#199437,#199438,#199439),(#199440,#199441,#199442)),.UNSPECIFIED.,.F.,
 .F.,.F.)
B_SPLINE_SURFACE_WITH_KNOTS((4,4),(3,3),(0.,0.000397394373651918),(0.,1.),
 .UNSPECIFIED.)
GEOMETRIC_REPRESENTATION_ITEM()
RATIONAL_B_SPLINE_SURFACE(((1.,0.707106781186548,1.),(1.,0.707752587915853,
1.),(1.,0.708377654540688,1.),(1.,0.708689770883324,1.)))
REPRESENTATION_ITEM('')
SURFACE()
);
#2600=(
BOUNDED_SURFACE()
B_SPLINE_SURFACE(3,2,((#199444,#199445,#199446),(#199447,#199448,#199449),
(#199450,#199451,#199452),(#199453,#199454,#199455)),.UNSPECIFIED.,.F.,
 .F.,.F.)
B_SPLINE_SURFACE_WITH_KNOTS((4,4),(3,3),(0.,0.00051181545647979),(0.,1.00105873159766),
 .UNSPECIFIED.)
GEOMETRIC_REPRESENTATION_ITEM()
RATIONAL_B_SPLINE_SURFACE(((1.,0.708394529056991,1.00061746385228),(1.,
0.708058564167539,1.00061817524556),(1.,0.707430835372731,1.00061950443818),
(1.,0.70679668588105,1.00062084722639)))
REPRESENTATION_ITEM('')
SURFACE()
);
#2601=(
BOUNDED_SURFACE()
B_SPLINE_SURFACE(3,2,((#199461,#199462,#199463),(#199464,#199465,#199466),
(#199467,#199468,#199469),(#199470,#199471,#199472)),.UNSPECIFIED.,.F.,
 .F.,.F.)
B_SPLINE_SURFACE_WITH_KNOTS((4,4),(3,3),(-6.50521303491303E-18,0.000397394465448297),
(0.,1.),.UNSPECIFIED.)
GEOMETRIC_REPRESENTATION_ITEM()
RATIONAL_B_SPLINE_SURFACE(((1.,0.705498956110752,1.),(1.,0.705821764811808,
1.),(1.,0.706461952521121,1.),(1.,0.707106781186562,1.)))
REPRESENTATION_ITEM('')
SURFACE()
);
#2602=(
BOUNDED_SURFACE()
B_SPLINE_SURFACE(3,2,((#199478,#199479,#199480),(#199481,#199482,#199483),
(#199484,#199485,#199486),(#199487,#199488,#199489)),.UNSPECIFIED.,.F.,
 .F.,.F.)
B_SPLINE_SURFACE_WITH_KNOTS((4,4),(3,3),(0.,0.000397394410828735),(0.,1.),
 .UNSPECIFIED.)
GEOMETRIC_REPRESENTATION_ITEM()
RATIONAL_B_SPLINE_SURFACE(((1.,0.708689770883324,1.),(1.,0.708376440034495,
1.),(1.,0.707750498698409,1.),(1.,0.707106781186548,1.)))
REPRESENTATION_ITEM('')
SURFACE()
);
#2603=(
BOUNDED_SURFACE()
B_SPLINE_SURFACE(3,2,((#199495,#199496,#199497),(#199498,#199499,#199500),
(#199501,#199502,#199503),(#199504,#199505,#199506)),.UNSPECIFIED.,.F.,
 .F.,.F.)
B_SPLINE_SURFACE_WITH_KNOTS((4,4),(3,3),(0.,0.000511815090126181),(0.,1.00105592270387),
 .UNSPECIFIED.)
GEOMETRIC_REPRESENTATION_ITEM()
RATIONAL_B_SPLINE_SURFACE(((1.,0.705266242717002,1.00062243213182),(1.,
0.705584085908638,1.00062176089614),(1.,0.706182089450009,1.00062049800511),
(1.,0.706797508586993,1.00061919833503)))
REPRESENTATION_ITEM('')
SURFACE()
);
#2604=(
BOUNDED_SURFACE()
B_SPLINE_SURFACE(3,2,((#199508,#199509,#199510),(#199511,#199512,#199513),
(#199514,#199515,#199516),(#199517,#199518,#199519)),.UNSPECIFIED.,.F.,
 .F.,.F.)
B_SPLINE_SURFACE_WITH_KNOTS((4,4),(3,3),(-5.09575021068187E-18,0.000397394428086632),
(0.,1.),.UNSPECIFIED.)
GEOMETRIC_REPRESENTATION_ITEM()
RATIONAL_B_SPLINE_SURFACE(((1.,0.707106781186535,1.),(1.,0.70645984675911,
1.),(1.,0.705820510737273,1.),(1.,0.705498956110752,1.)))
REPRESENTATION_ITEM('')
SURFACE()
);
#2605=(
BOUNDED_SURFACE()
B_SPLINE_SURFACE(3,2,((#199525,#199526,#199527),(#199528,#199529,#199530),
(#199531,#199532,#199533),(#199534,#199535,#199536),(#199537,#199538,#199539),
(#199540,#199541,#199542)),.UNSPECIFIED.,.F.,.F.,.F.)
B_SPLINE_SURFACE_WITH_KNOTS((4,2,4),(3,3),(0.,0.000257953807872843,0.000515907615745686),
(0.,1.),.UNSPECIFIED.)
GEOMETRIC_REPRESENTATION_ITEM()
RATIONAL_B_SPLINE_SURFACE(((1.,0.874619707139381,1.),(1.,0.874834349679065,
1.),(1.,0.854686104157677,1.),(1.,0.792476597915275,1.),(1.,0.750887854595022,
1.),(1.,0.705585838031447,1.)))
REPRESENTATION_ITEM('')
SURFACE()
);
#2606=(
BOUNDED_SURFACE()
B_SPLINE_SURFACE(3,2,((#199548,#199549,#199550),(#199551,#199552,#199553),
(#199554,#199555,#199556),(#199557,#199558,#199559)),.UNSPECIFIED.,.F.,
 .F.,.F.)
B_SPLINE_SURFACE_WITH_KNOTS((4,4),(3,3),(-9.64939933512099E-18,0.000511815437699146),
(0.,1.00105881331722),.UNSPECIFIED.)
GEOMETRIC_REPRESENTATION_ITEM()
RATIONAL_B_SPLINE_SURFACE(((1.,0.706796661945945,1.00062089519797),(1.,
0.707430821224828,1.00061955228539),(1.,0.708058545830313,1.00061822299905),
(1.,0.708394505252324,1.00061751156243)))
REPRESENTATION_ITEM('')
SURFACE()
);
#2607=(
BOUNDED_SURFACE()
B_SPLINE_SURFACE(3,2,((#199561,#199562,#199563),(#199564,#199565,#199566),
(#199567,#199568,#199569),(#199570,#199571,#199572),(#199573,#199574,#199575),
(#199576,#199577,#199578)),.UNSPECIFIED.,.F.,.F.,.F.)
B_SPLINE_SURFACE_WITH_KNOTS((4,2,4),(3,3),(0.,0.000256915317531262,0.000513830635062524),
(0.,1.),.UNSPECIFIED.)
GEOMETRIC_REPRESENTATION_ITEM()
RATIONAL_B_SPLINE_SURFACE(((1.,0.705585838031416,1.),(1.,0.750902433542617,
1.),(1.,0.792329530082699,1.),(1.,0.854288401594014,1.),(1.,0.874998031125278,
1.),(1.,0.874619707139387,1.)))
REPRESENTATION_ITEM('')
SURFACE()
);
#2608=(
BOUNDED_SURFACE()
B_SPLINE_SURFACE(3,2,((#199584,#199585,#199586),(#199587,#199588,#199589),
(#199590,#199591,#199592),(#199593,#199594,#199595),(#199596,#199597,#199598),
(#199599,#199600,#199601)),.UNSPECIFIED.,.F.,.F.,.F.)
B_SPLINE_SURFACE_WITH_KNOTS((4,2,4),(3,3),(0.,0.000256592814262154,0.000513185628524309),
(0.,1.),.UNSPECIFIED.)
GEOMETRIC_REPRESENTATION_ITEM()
RATIONAL_B_SPLINE_SURFACE(((1.,0.70871252716366,1.),(1.,0.753780902613466,
1.),(1.,0.794538995769324,1.),(1.,0.855070770330988,1.),(1.,0.875018427445413,
1.),(1.,0.874619707139393,1.)))
REPRESENTATION_ITEM('')
SURFACE()
);
#2609=(
BOUNDED_SURFACE()
B_SPLINE_SURFACE(3,2,((#199603,#199604,#199605),(#199606,#199607,#199608),
(#199609,#199610,#199611),(#199612,#199613,#199614)),.UNSPECIFIED.,.F.,
 .F.,.F.)
B_SPLINE_SURFACE_WITH_KNOTS((4,4),(3,3),(0.,0.000511815072430401),(0.,1.00105598365676),
 .UNSPECIFIED.)
GEOMETRIC_REPRESENTATION_ITEM()
RATIONAL_B_SPLINE_SURFACE(((1.,0.706797490734305,1.00061923411581),(1.,
0.706182062147239,1.00062053388087),(1.,0.705584062769544,1.00062179683601),
(1.,0.705266224771083,1.00062246809947)))
REPRESENTATION_ITEM('')
SURFACE()
);
#2610=(
BOUNDED_SURFACE()
B_SPLINE_SURFACE(3,2,((#199620,#199621,#199622),(#199623,#199624,#199625),
(#199626,#199627,#199628),(#199629,#199630,#199631),(#199632,#199633,#199634),
(#199635,#199636,#199637)),.UNSPECIFIED.,.F.,.F.,.F.)
B_SPLINE_SURFACE_WITH_KNOTS((4,2,4),(3,3),(0.,0.000257652232350877,0.000515304464701754),
(0.,1.),.UNSPECIFIED.)
GEOMETRIC_REPRESENTATION_ITEM()
RATIONAL_B_SPLINE_SURFACE(((1.,0.874619707139381,1.),(1.,0.874861180430772,
1.),(1.,0.855455725920791,1.),(1.,0.794699358955345,1.),(1.,0.753768977788573,
1.),(1.,0.708712527163675,1.)))
REPRESENTATION_ITEM('')
SURFACE()
);
#2611=(
BOUNDED_SURFACE()
B_SPLINE_SURFACE(3,2,((#199643,#199644,#199645),(#199646,#199647,#199648),
(#199649,#199650,#199651),(#199652,#199653,#199654)),.UNSPECIFIED.,.F.,
 .F.,.F.)
B_SPLINE_SURFACE_WITH_KNOTS((4,4),(3,3),(0.,0.000397394373651921),(0.,1.),
 .UNSPECIFIED.)
GEOMETRIC_REPRESENTATION_ITEM()
RATIONAL_B_SPLINE_SURFACE(((1.,0.707106781186548,1.),(1.,0.70775258791592,
1.),(1.,0.708377654540668,1.),(1.,0.70868977088334,1.)))
REPRESENTATION_ITEM('')
SURFACE()
);
#2612=(
BOUNDED_SURFACE()
B_SPLINE_SURFACE(3,2,((#199656,#199657,#199658),(#199659,#199660,#199661),
(#199662,#199663,#199664),(#199665,#199666,#199667)),.UNSPECIFIED.,.F.,
 .F.,.F.)
B_SPLINE_SURFACE_WITH_KNOTS((4,4),(3,3),(0.,0.000511815456479783),(0.,1.00105873159891),
 .UNSPECIFIED.)
GEOMETRIC_REPRESENTATION_ITEM()
RATIONAL_B_SPLINE_SURFACE(((1.,0.708394529056628,1.000617463853),(1.,0.708058564167186,
1.00061817524629),(1.,0.707430835372387,1.00061950443891),(1.,0.706796685880672,
1.00062084722712)))
REPRESENTATION_ITEM('')
SURFACE()
);
#2613=(
BOUNDED_SURFACE()
B_SPLINE_SURFACE(3,2,((#199673,#199674,#199675),(#199676,#199677,#199678),
(#199679,#199680,#199681),(#199682,#199683,#199684)),.UNSPECIFIED.,.F.,
 .F.,.F.)
B_SPLINE_SURFACE_WITH_KNOTS((4,4),(3,3),(0.,0.000397394465448299),(0.,1.),
 .UNSPECIFIED.)
GEOMETRIC_REPRESENTATION_ITEM()
RATIONAL_B_SPLINE_SURFACE(((1.,0.705498956110742,1.),(1.,0.705821764811775,
1.),(1.,0.706461952521124,1.),(1.,0.707106781186548,1.)))
REPRESENTATION_ITEM('')
SURFACE()
);
#2614=(
BOUNDED_SURFACE()
B_SPLINE_SURFACE(3,2,((#199690,#199691,#199692),(#199693,#199694,#199695),
(#199696,#199697,#199698),(#199699,#199700,#199701)),.UNSPECIFIED.,.F.,
 .F.,.F.)
B_SPLINE_SURFACE_WITH_KNOTS((4,4),(3,3),(0.,0.000397394410828729),(0.,1.),
 .UNSPECIFIED.)
GEOMETRIC_REPRESENTATION_ITEM()
RATIONAL_B_SPLINE_SURFACE(((1.,0.708689770883367,1.),(1.,0.708376440034488,
1.),(1.,0.707750498698389,1.),(1.,0.707106781186548,1.)))
REPRESENTATION_ITEM('')
SURFACE()
);
#2615=(
BOUNDED_SURFACE()
B_SPLINE_SURFACE(3,2,((#199707,#199708,#199709),(#199710,#199711,#199712),
(#199713,#199714,#199715),(#199716,#199717,#199718)),.UNSPECIFIED.,.F.,
 .F.,.F.)
B_SPLINE_SURFACE_WITH_KNOTS((4,4),(3,3),(0.,0.000511815090126175),(0.,1.00105592270219),
 .UNSPECIFIED.)
GEOMETRIC_REPRESENTATION_ITEM()
RATIONAL_B_SPLINE_SURFACE(((1.,0.705266242717483,1.00062243213083),(1.,
0.705584085909122,1.00062176089515),(1.,0.706182089450485,1.00062049800412),
(1.,0.706797508587486,1.00061919833404)))
REPRESENTATION_ITEM('')
SURFACE()
);
#2616=(
BOUNDED_SURFACE()
B_SPLINE_SURFACE(3,2,((#199720,#199721,#199722),(#199723,#199724,#199725),
(#199726,#199727,#199728),(#199729,#199730,#199731)),.UNSPECIFIED.,.F.,
 .F.,.F.)
B_SPLINE_SURFACE_WITH_KNOTS((4,4),(3,3),(-5.52943107967607E-18,0.000397394428086625),
(0.,1.),.UNSPECIFIED.)
GEOMETRIC_REPRESENTATION_ITEM()
RATIONAL_B_SPLINE_SURFACE(((1.,0.707106781186548,1.),(1.,0.706459846759112,
1.),(1.,0.705820510737253,1.),(1.,0.705498956110736,1.)))
REPRESENTATION_ITEM('')
SURFACE()
);
#2617=(
BOUNDED_SURFACE()
B_SPLINE_SURFACE(3,2,((#199737,#199738,#199739),(#199740,#199741,#199742),
(#199743,#199744,#199745),(#199746,#199747,#199748),(#199749,#199750,#199751),
(#199752,#199753,#199754)),.UNSPECIFIED.,.F.,.F.,.F.)
B_SPLINE_SURFACE_WITH_KNOTS((4,2,4),(3,3),(0.,0.000257953807872841,0.000515907615745682),
(0.,1.),.UNSPECIFIED.)
GEOMETRIC_REPRESENTATION_ITEM()
RATIONAL_B_SPLINE_SURFACE(((1.,0.874619707139397,1.),(1.,0.874834349678708,
1.),(1.,0.85468610415817,1.),(1.,0.792476597914768,1.),(1.,0.750887854595433,
1.),(1.,0.705585838031436,1.)))
REPRESENTATION_ITEM('')
SURFACE()
);
#2618=(
BOUNDED_SURFACE()
B_SPLINE_SURFACE(3,2,((#199760,#199761,#199762),(#199763,#199764,#199765),
(#199766,#199767,#199768),(#199769,#199770,#199771)),.UNSPECIFIED.,.F.,
 .F.,.F.)
B_SPLINE_SURFACE_WITH_KNOTS((4,4),(3,3),(0.,0.000511815437699146),(0.,1.00105881331768),
 .UNSPECIFIED.)
GEOMETRIC_REPRESENTATION_ITEM()
RATIONAL_B_SPLINE_SURFACE(((1.,0.706796661945808,1.00062089519824),(1.,
0.707430821224685,1.00061955228566),(1.,0.708058545830195,1.00061822299932),
(1.,0.708394505252203,1.0006175115627)))
REPRESENTATION_ITEM('')
SURFACE()
);
#2619=(
BOUNDED_SURFACE()
B_SPLINE_SURFACE(3,2,((#199773,#199774,#199775),(#199776,#199777,#199778),
(#199779,#199780,#199781),(#199782,#199783,#199784),(#199785,#199786,#199787),
(#199788,#199789,#199790)),.UNSPECIFIED.,.F.,.F.,.F.)
B_SPLINE_SURFACE_WITH_KNOTS((4,2,4),(3,3),(-5.77337656848531E-18,0.000256915317531248,
0.000513830635062502),(0.,1.),.UNSPECIFIED.)
GEOMETRIC_REPRESENTATION_ITEM()
RATIONAL_B_SPLINE_SURFACE(((1.,0.705585838031448,1.),(1.,0.750902433542038,
1.),(1.,0.792329530083478,1.),(1.,0.854288401593252,1.),(1.,0.874998031125851,
1.),(1.,0.874619707139389,1.)))
REPRESENTATION_ITEM('')
SURFACE()
);
#2620=(
BOUNDED_SURFACE()
B_SPLINE_SURFACE(3,2,((#199796,#199797,#199798),(#199799,#199800,#199801),
(#199802,#199803,#199804),(#199805,#199806,#199807),(#199808,#199809,#199810),
(#199811,#199812,#199813)),.UNSPECIFIED.,.F.,.F.,.F.)
B_SPLINE_SURFACE_WITH_KNOTS((4,2,4),(3,3),(-8.91756286869327E-18,0.000256592814262157,
0.000513185628524322),(0.,1.),.UNSPECIFIED.)
GEOMETRIC_REPRESENTATION_ITEM()
RATIONAL_B_SPLINE_SURFACE(((1.,0.70871252716367,1.),(1.,0.753780902614205,
1.),(1.,0.794538995768374,1.),(1.,0.855070770331893,1.),(1.,0.875018427444734,
1.),(1.,0.874619707139393,1.)))
REPRESENTATION_ITEM('')
SURFACE()
);
#2621=(
BOUNDED_SURFACE()
B_SPLINE_SURFACE(3,2,((#199815,#199816,#199817),(#199818,#199819,#199820),
(#199821,#199822,#199823),(#199824,#199825,#199826)),.UNSPECIFIED.,.F.,
 .F.,.F.)
B_SPLINE_SURFACE_WITH_KNOTS((4,4),(3,3),(-9.54097911787244E-18,0.000511815072430398),
(0.,1.0010559836562),.UNSPECIFIED.)
GEOMETRIC_REPRESENTATION_ITEM()
RATIONAL_B_SPLINE_SURFACE(((1.,0.70679749073447,1.00061923411548),(1.,0.706182062147385,
1.00062053388054),(1.,0.705584062769784,1.00062179683568),(1.,0.705266224771247,
1.00062246809914)))
REPRESENTATION_ITEM('')
SURFACE()
);
#2622=(
BOUNDED_SURFACE()
B_SPLINE_SURFACE(3,2,((#199832,#199833,#199834),(#199835,#199836,#199837),
(#199838,#199839,#199840),(#199841,#199842,#199843),(#199844,#199845,#199846),
(#199847,#199848,#199849)),.UNSPECIFIED.,.F.,.F.,.F.)
B_SPLINE_SURFACE_WITH_KNOTS((4,2,4),(3,3),(0.,0.000257652232350877,0.000515304464701755),
(0.,1.),.UNSPECIFIED.)
GEOMETRIC_REPRESENTATION_ITEM()
RATIONAL_B_SPLINE_SURFACE(((1.,0.874619707139387,1.),(1.,0.874861180430636,
1.),(1.,0.855455725920972,1.),(1.,0.794699358955189,1.),(1.,0.753768977788693,
1.),(1.,0.70871252716365,1.)))
REPRESENTATION_ITEM('')
SURFACE()
);
#2623=(
BOUNDED_SURFACE()
B_SPLINE_SURFACE(3,2,((#199855,#199856,#199857),(#199858,#199859,#199860),
(#199861,#199862,#199863),(#199864,#199865,#199866)),.UNSPECIFIED.,.F.,
 .F.,.F.)
B_SPLINE_SURFACE_WITH_KNOTS((4,4),(3,3),(-5.52943107967607E-18,0.000397394373651916),
(0.,1.),.UNSPECIFIED.)
GEOMETRIC_REPRESENTATION_ITEM()
RATIONAL_B_SPLINE_SURFACE(((1.,0.707106781186548,1.),(1.,0.707752587915911,
1.),(1.,0.708377654540664,1.),(1.,0.708689770883322,1.)))
REPRESENTATION_ITEM('')
SURFACE()
);
#2624=(
BOUNDED_SURFACE()
B_SPLINE_SURFACE(3,2,((#199868,#199869,#199870),(#199871,#199872,#199873),
(#199874,#199875,#199876),(#199877,#199878,#199879)),.UNSPECIFIED.,.F.,
 .F.,.F.)
B_SPLINE_SURFACE_WITH_KNOTS((4,4),(3,3),(0.,0.000511815456479781),(0.,1.00105873159962),
 .UNSPECIFIED.)
GEOMETRIC_REPRESENTATION_ITEM()
RATIONAL_B_SPLINE_SURFACE(((1.,0.70839452905641,1.00061746385342),(1.,0.708058564166979,
1.00061817524671),(1.,0.707430835372153,1.00061950443933),(1.,0.706796685880476,
1.00062084722754)))
REPRESENTATION_ITEM('')
SURFACE()
);
#2625=(
BOUNDED_SURFACE()
B_SPLINE_SURFACE(3,2,((#199885,#199886,#199887),(#199888,#199889,#199890),
(#199891,#199892,#199893),(#199894,#199895,#199896)),.UNSPECIFIED.,.F.,
 .F.,.F.)
B_SPLINE_SURFACE_WITH_KNOTS((4,4),(3,3),(0.,0.000397394465448313),(0.,1.),
 .UNSPECIFIED.)
GEOMETRIC_REPRESENTATION_ITEM()
RATIONAL_B_SPLINE_SURFACE(((1.,0.705498956110761,1.),(1.,0.705821764811814,
1.),(1.,0.706461952521111,1.),(1.,0.707106781186548,1.)))
REPRESENTATION_ITEM('')
SURFACE()
);
#2626=(
BOUNDED_SURFACE()
B_SPLINE_SURFACE(3,2,((#199902,#199903,#199904),(#199905,#199906,#199907),
(#199908,#199909,#199910),(#199911,#199912,#199913)),.UNSPECIFIED.,.F.,
 .F.,.F.)
B_SPLINE_SURFACE_WITH_KNOTS((4,4),(3,3),(0.,0.000397394410828733),(0.,1.),
 .UNSPECIFIED.)
GEOMETRIC_REPRESENTATION_ITEM()
RATIONAL_B_SPLINE_SURFACE(((1.,0.708689770883358,1.),(1.,0.708376440034475,
1.),(1.,0.707750498698409,1.),(1.,0.707106781186548,1.)))
REPRESENTATION_ITEM('')
SURFACE()
);
#2627=(
BOUNDED_SURFACE()
B_SPLINE_SURFACE(3,2,((#199919,#199920,#199921),(#199922,#199923,#199924),
(#199925,#199926,#199927),(#199928,#199929,#199930)),.UNSPECIFIED.,.F.,
 .F.,.F.)
B_SPLINE_SURFACE_WITH_KNOTS((4,4),(3,3),(0.,0.000511815090126173),(0.,1.00105592270345),
 .UNSPECIFIED.)
GEOMETRIC_REPRESENTATION_ITEM()
RATIONAL_B_SPLINE_SURFACE(((1.,0.705266242717092,1.00062243213157),(1.,
0.7055840859088,1.00062176089589),(1.,0.706182089450108,1.00062049800486),
(1.,0.706797508587117,1.00061919833478)))
REPRESENTATION_ITEM('')
SURFACE()
);
#2628=(
BOUNDED_SURFACE()
B_SPLINE_SURFACE(3,2,((#199932,#199933,#199934),(#199935,#199936,#199937),
(#199938,#199939,#199940),(#199941,#199942,#199943)),.UNSPECIFIED.,.F.,
 .F.,.F.)
B_SPLINE_SURFACE_WITH_KNOTS((4,4),(3,3),(-7.64362531602281E-18,0.000397394428086619),
(0.,1.),.UNSPECIFIED.)
GEOMETRIC_REPRESENTATION_ITEM()
RATIONAL_B_SPLINE_SURFACE(((1.,0.707106781186539,1.),(1.,0.706459846759101,
1.),(1.,0.705820510737287,1.),(1.,0.705498956110748,1.)))
REPRESENTATION_ITEM('')
SURFACE()
);
#2629=(
BOUNDED_SURFACE()
B_SPLINE_SURFACE(3,2,((#199949,#199950,#199951),(#199952,#199953,#199954),
(#199955,#199956,#199957),(#199958,#199959,#199960),(#199961,#199962,#199963),
(#199964,#199965,#199966)),.UNSPECIFIED.,.F.,.F.,.F.)
B_SPLINE_SURFACE_WITH_KNOTS((4,2,4),(3,3),(0.,0.000257953807872845,0.00051590761574569),
(0.,1.),.UNSPECIFIED.)
GEOMETRIC_REPRESENTATION_ITEM()
RATIONAL_B_SPLINE_SURFACE(((1.,0.874619707139383,1.),(1.,0.874834349679653,
1.),(1.,0.854686104156939,1.),(1.,0.792476597916007,1.),(1.,0.750887854594488,
1.),(1.,0.705585838031433,1.)))
REPRESENTATION_ITEM('')
SURFACE()
);
#2630=(
BOUNDED_SURFACE()
B_SPLINE_SURFACE(3,2,((#199972,#199973,#199974),(#199975,#199976,#199977),
(#199978,#199979,#199980),(#199981,#199982,#199983)),.UNSPECIFIED.,.F.,
 .F.,.F.)
B_SPLINE_SURFACE_WITH_KNOTS((4,4),(3,3),(-7.61652026171067E-18,0.000511815437699149),
(0.,1.00105881331741),.UNSPECIFIED.)
GEOMETRIC_REPRESENTATION_ITEM()
RATIONAL_B_SPLINE_SURFACE(((1.,0.706796661945879,1.00062089519808),(1.,
0.707430821224774,1.0006195522855),(1.,0.70805854583029,1.00061822299916),
(1.,0.708394505252249,1.00061751156254)))
REPRESENTATION_ITEM('')
SURFACE()
);
#2631=(
BOUNDED_SURFACE()
B_SPLINE_SURFACE(3,2,((#199985,#199986,#199987),(#199988,#199989,#199990),
(#199991,#199992,#199993),(#199994,#199995,#199996),(#199997,#199998,#199999),
(#200000,#200001,#200002)),.UNSPECIFIED.,.F.,.F.,.F.)
B_SPLINE_SURFACE_WITH_KNOTS((4,2,4),(3,3),(0.,0.000256915317531265,0.000513830635062531),
(0.,1.),.UNSPECIFIED.)
GEOMETRIC_REPRESENTATION_ITEM()
RATIONAL_B_SPLINE_SURFACE(((1.,0.705585838031483,1.),(1.,0.750902433542739,
1.),(1.,0.792329530082514,1.),(1.,0.854288401594209,1.),(1.,0.87499803112514,
1.),(1.,0.874619707139408,1.)))
REPRESENTATION_ITEM('')
SURFACE()
);
#2632=(
BOUNDED_SURFACE()
B_SPLINE_SURFACE(3,2,((#200008,#200009,#200010),(#200011,#200012,#200013),
(#200014,#200015,#200016),(#200017,#200018,#200019),(#200020,#200021,#200022),
(#200023,#200024,#200025)),.UNSPECIFIED.,.F.,.F.,.F.)
B_SPLINE_SURFACE_WITH_KNOTS((4,2,4),(3,3),(0.,0.000256592814262162,0.000513185628524324),
(0.,1.),.UNSPECIFIED.)
GEOMETRIC_REPRESENTATION_ITEM()
RATIONAL_B_SPLINE_SURFACE(((1.,0.708712527163667,1.),(1.,0.753780902613371,
1.),(1.,0.794538995769506,1.),(1.,0.855070770330781,1.),(1.,0.875018427445574,
1.),(1.,0.874619707139391,1.)))
REPRESENTATION_ITEM('')
SURFACE()
);
#2633=(
BOUNDED_SURFACE()
B_SPLINE_SURFACE(3,2,((#200027,#200028,#200029),(#200030,#200031,#200032),
(#200033,#200034,#200035),(#200036,#200037,#200038)),.UNSPECIFIED.,.F.,
 .F.,.F.)
B_SPLINE_SURFACE_WITH_KNOTS((4,4),(3,3),(0.,0.000511815072430398),(0.,1.00105598366041),
 .UNSPECIFIED.)
GEOMETRIC_REPRESENTATION_ITEM()
RATIONAL_B_SPLINE_SURFACE(((1.,0.706797490733237,1.00061923411795),(1.,
0.706182062146155,1.00062053388302),(1.,0.705584062768535,1.00062179683816),
(1.,0.705266224770017,1.00062246810163)))
REPRESENTATION_ITEM('')
SURFACE()
);
#2634=(
BOUNDED_SURFACE()
B_SPLINE_SURFACE(3,2,((#200044,#200045,#200046),(#200047,#200048,#200049),
(#200050,#200051,#200052),(#200053,#200054,#200055),(#200056,#200057,#200058),
(#200059,#200060,#200061)),.UNSPECIFIED.,.F.,.F.,.F.)
B_SPLINE_SURFACE_WITH_KNOTS((4,2,4),(3,3),(0.,0.000257652232350879,0.000515304464701758),
(0.,1.),.UNSPECIFIED.)
GEOMETRIC_REPRESENTATION_ITEM()
RATIONAL_B_SPLINE_SURFACE(((1.,0.874619707139379,1.),(1.,0.87486118043056,
1.),(1.,0.855455725921018,1.),(1.,0.794699358955082,1.),(1.,0.753768977788767,
1.),(1.,0.708712527163641,1.)))
REPRESENTATION_ITEM('')
SURFACE()
);
#2635=(
BOUNDED_SURFACE()
B_SPLINE_SURFACE(3,2,((#200067,#200068,#200069),(#200070,#200071,#200072),
(#200073,#200074,#200075),(#200076,#200077,#200078)),.UNSPECIFIED.,.F.,
 .F.,.F.)
B_SPLINE_SURFACE_WITH_KNOTS((4,4),(3,3),(0.,0.000397394373651927),(0.,1.),
 .UNSPECIFIED.)
GEOMETRIC_REPRESENTATION_ITEM()
RATIONAL_B_SPLINE_SURFACE(((1.,0.707106781186548,1.),(1.,0.707752587915909,
1.),(1.,0.708377654540638,1.),(1.,0.708689770883346,1.)))
REPRESENTATION_ITEM('')
SURFACE()
);
#2636=(
BOUNDED_SURFACE()
B_SPLINE_SURFACE(3,2,((#200080,#200081,#200082),(#200083,#200084,#200085),
(#200086,#200087,#200088),(#200089,#200090,#200091)),.UNSPECIFIED.,.F.,
 .F.,.F.)
B_SPLINE_SURFACE_WITH_KNOTS((4,4),(3,3),(0.,0.000511815456479783),(0.,1.00105873160187),
 .UNSPECIFIED.)
GEOMETRIC_REPRESENTATION_ITEM()
RATIONAL_B_SPLINE_SURFACE(((1.,0.708394529055766,1.00061746385473),(1.,
0.70805856416633,1.00061817524803),(1.,0.707430835371486,1.00061950444065),
(1.,0.706796685879816,1.00062084722886)))
REPRESENTATION_ITEM('')
SURFACE()
);
#2637=(
BOUNDED_SURFACE()
B_SPLINE_SURFACE(3,2,((#200097,#200098,#200099),(#200100,#200101,#200102),
(#200103,#200104,#200105),(#200106,#200107,#200108)),.UNSPECIFIED.,.F.,
 .F.,.F.)
B_SPLINE_SURFACE_WITH_KNOTS((4,4),(3,3),(0.,0.000397394465448308),(0.,1.),
 .UNSPECIFIED.)
GEOMETRIC_REPRESENTATION_ITEM()
RATIONAL_B_SPLINE_SURFACE(((1.,0.705498956110759,1.),(1.,0.705821764811768,
1.),(1.,0.706461952521157,1.),(1.,0.707106781186548,1.)))
REPRESENTATION_ITEM('')
SURFACE()
);
#2638=(
BOUNDED_SURFACE()
B_SPLINE_SURFACE(3,2,((#200114,#200115,#200116),(#200117,#200118,#200119),
(#200120,#200121,#200122),(#200123,#200124,#200125)),.UNSPECIFIED.,.F.,
 .F.,.F.)
B_SPLINE_SURFACE_WITH_KNOTS((4,4),(3,3),(0.,0.000397394410828734),(0.,1.),
 .UNSPECIFIED.)
GEOMETRIC_REPRESENTATION_ITEM()
RATIONAL_B_SPLINE_SURFACE(((1.,0.708689770883336,1.),(1.,0.708376440034494,
1.),(1.,0.70775049869841,1.),(1.,0.707106781186548,1.)))
REPRESENTATION_ITEM('')
SURFACE()
);
#2639=(
BOUNDED_SURFACE()
B_SPLINE_SURFACE(3,2,((#200131,#200132,#200133),(#200134,#200135,#200136),
(#200137,#200138,#200139),(#200140,#200141,#200142)),.UNSPECIFIED.,.F.,
 .F.,.F.)
B_SPLINE_SURFACE_WITH_KNOTS((4,4),(3,3),(0.,0.000511815090126178),(0.,1.00105592270253),
 .UNSPECIFIED.)
GEOMETRIC_REPRESENTATION_ITEM()
RATIONAL_B_SPLINE_SURFACE(((1.,0.705266242717381,1.00062243213103),(1.,
0.705584085909037,1.00062176089535),(1.,0.706182089450398,1.00062049800432),
(1.,0.706797508587385,1.00061919833424)))
REPRESENTATION_ITEM('')
SURFACE()
);
#2640=(
BOUNDED_SURFACE()
B_SPLINE_SURFACE(3,2,((#200144,#200145,#200146),(#200147,#200148,#200149),
(#200150,#200151,#200152),(#200153,#200154,#200155)),.UNSPECIFIED.,.F.,
 .F.,.F.)
B_SPLINE_SURFACE_WITH_KNOTS((4,4),(3,3),(-1.52601455777335E-17,0.000397394428086621),
(0.,1.),.UNSPECIFIED.)
GEOMETRIC_REPRESENTATION_ITEM()
RATIONAL_B_SPLINE_SURFACE(((1.,0.707106781186548,1.),(1.,0.706459846759085,
1.),(1.,0.705820510737268,1.),(1.,0.70549895611075,1.)))
REPRESENTATION_ITEM('')
SURFACE()
);
#2641=(
BOUNDED_SURFACE()
B_SPLINE_SURFACE(3,2,((#200161,#200162,#200163),(#200164,#200165,#200166),
(#200167,#200168,#200169),(#200170,#200171,#200172),(#200173,#200174,#200175),
(#200176,#200177,#200178)),.UNSPECIFIED.,.F.,.F.,.F.)
B_SPLINE_SURFACE_WITH_KNOTS((4,2,4),(3,3),(0.,0.000257953807872852,0.000515907615745704),
(0.,1.),.UNSPECIFIED.)
GEOMETRIC_REPRESENTATION_ITEM()
RATIONAL_B_SPLINE_SURFACE(((1.,0.874619707139392,1.),(1.,0.874834349679401,
1.),(1.,0.854686104157248,1.),(1.,0.79247659791567,1.),(1.,0.75088785459474,
1.),(1.,0.705585838031443,1.)))
REPRESENTATION_ITEM('')
SURFACE()
);
#2642=(
BOUNDED_SURFACE()
B_SPLINE_SURFACE(3,2,((#200184,#200185,#200186),(#200187,#200188,#200189),
(#200190,#200191,#200192),(#200193,#200194,#200195)),.UNSPECIFIED.,.F.,
 .F.,.F.)
B_SPLINE_SURFACE_WITH_KNOTS((4,4),(3,3),(0.,0.000511815437699151),(0.,1.00105881331662),
 .UNSPECIFIED.)
GEOMETRIC_REPRESENTATION_ITEM()
RATIONAL_B_SPLINE_SURFACE(((1.,0.706796661946136,1.00062089519762),(1.,
0.707430821224989,1.00061955228504),(1.,0.708058545830515,1.0006182229987),
(1.,0.708394505252514,1.00061751156208)))
REPRESENTATION_ITEM('')
SURFACE()
);
#2643=(
BOUNDED_SURFACE()
B_SPLINE_SURFACE(3,2,((#200197,#200198,#200199),(#200200,#200201,#200202),
(#200203,#200204,#200205),(#200206,#200207,#200208),(#200209,#200210,#200211),
(#200212,#200213,#200214)),.UNSPECIFIED.,.F.,.F.,.F.)
B_SPLINE_SURFACE_WITH_KNOTS((4,2,4),(3,3),(0.,0.000256915317531256,0.000513830635062512),
(0.,1.),.UNSPECIFIED.)
GEOMETRIC_REPRESENTATION_ITEM()
RATIONAL_B_SPLINE_SURFACE(((1.,0.705585838031448,1.),(1.,0.750902433542508,
1.),(1.,0.792329530082831,1.),(1.,0.854288401593858,1.),(1.,0.874998031125374,
1.),(1.,0.874619707139394,1.)))
REPRESENTATION_ITEM('')
SURFACE()
);
#2644=(
BOUNDED_SURFACE()
B_SPLINE_SURFACE(3,2,((#200220,#200221,#200222),(#200223,#200224,#200225),
(#200226,#200227,#200228),(#200229,#200230,#200231),(#200232,#200233,#200234),
(#200235,#200236,#200237)),.UNSPECIFIED.,.F.,.F.,.F.)
B_SPLINE_SURFACE_WITH_KNOTS((4,2,4),(3,3),(0.,0.000256592814262157,0.000513185628524313),
(0.,1.),.UNSPECIFIED.)
GEOMETRIC_REPRESENTATION_ITEM()
RATIONAL_B_SPLINE_SURFACE(((1.,0.708712527163664,1.),(1.,0.753780902613601,
1.),(1.,0.794538995769178,1.),(1.,0.855070770331139,1.),(1.,0.8750184274453,
1.),(1.,0.87461970713939,1.)))
REPRESENTATION_ITEM('')
SURFACE()
);
#2645=(
BOUNDED_SURFACE()
B_SPLINE_SURFACE(3,2,((#200239,#200240,#200241),(#200242,#200243,#200244),
(#200245,#200246,#200247),(#200248,#200249,#200250)),.UNSPECIFIED.,.F.,
 .F.,.F.)
B_SPLINE_SURFACE_WITH_KNOTS((4,4),(3,3),(-7.61652026171067E-18,0.000511815072430393),
(0.,1.00105598365944),.UNSPECIFIED.)
GEOMETRIC_REPRESENTATION_ITEM()
RATIONAL_B_SPLINE_SURFACE(((1.,0.70679749073352,1.00061923411738),(1.,0.706182062146414,
1.00062053388245),(1.,0.705584062768852,1.00062179683759),(1.,0.705266224770258,
1.00062246810105)))
REPRESENTATION_ITEM('')
SURFACE()
);
#2646=(
BOUNDED_SURFACE()
B_SPLINE_SURFACE(3,2,((#200256,#200257,#200258),(#200259,#200260,#200261),
(#200262,#200263,#200264),(#200265,#200266,#200267),(#200268,#200269,#200270),
(#200271,#200272,#200273)),.UNSPECIFIED.,.F.,.F.,.F.)
B_SPLINE_SURFACE_WITH_KNOTS((4,2,4),(3,3),(0.,0.000257652232350884,0.000515304464701767),
(0.,1.),.UNSPECIFIED.)
GEOMETRIC_REPRESENTATION_ITEM()
RATIONAL_B_SPLINE_SURFACE(((1.,0.874619707139383,1.),(1.,0.874861180430228,
1.),(1.,0.855455725921542,1.),(1.,0.794699358954615,1.),(1.,0.75376897778914,
1.),(1.,0.708712527163655,1.)))
REPRESENTATION_ITEM('')
SURFACE()
);
#2647=(
BOUNDED_SURFACE()
B_SPLINE_SURFACE(3,2,((#200279,#200280,#200281),(#200282,#200283,#200284),
(#200285,#200286,#200287),(#200288,#200289,#200290)),.UNSPECIFIED.,.F.,
 .F.,.F.)
B_SPLINE_SURFACE_WITH_KNOTS((4,4),(3,3),(0.,0.000397394373651933),(0.,1.),
 .UNSPECIFIED.)
GEOMETRIC_REPRESENTATION_ITEM()
RATIONAL_B_SPLINE_SURFACE(((1.,0.707106781186555,1.),(1.,0.70775258791589,
1.),(1.,0.708377654540668,1.),(1.,0.708689770883335,1.)))
REPRESENTATION_ITEM('')
SURFACE()
);
#2648=(
BOUNDED_SURFACE()
B_SPLINE_SURFACE(3,2,((#200292,#200293,#200294),(#200295,#200296,#200297),
(#200298,#200299,#200300),(#200301,#200302,#200303)),.UNSPECIFIED.,.F.,
 .F.,.F.)
B_SPLINE_SURFACE_WITH_KNOTS((4,4),(3,3),(0.,0.000511815456479785),(0.,1.00105873159945),
 .UNSPECIFIED.)
GEOMETRIC_REPRESENTATION_ITEM()
RATIONAL_B_SPLINE_SURFACE(((1.,0.70839452905647,1.00061746385332),(1.,0.708058564167016,
1.00061817524661),(1.,0.707430835372208,1.00061950443923),(1.,0.706796685880517,
1.00062084722744)))
REPRESENTATION_ITEM('')
SURFACE()
);
#2649=(
BOUNDED_SURFACE()
B_SPLINE_SURFACE(3,2,((#200309,#200310,#200311),(#200312,#200313,#200314),
(#200315,#200316,#200317),(#200318,#200319,#200320)),.UNSPECIFIED.,.F.,
 .F.,.F.)
B_SPLINE_SURFACE_WITH_KNOTS((4,4),(3,3),(0.,0.000397394465448311),(0.,1.),
 .UNSPECIFIED.)
GEOMETRIC_REPRESENTATION_ITEM()
RATIONAL_B_SPLINE_SURFACE(((1.,0.705498956110775,1.),(1.,0.705821764811747,
1.),(1.,0.706461952521171,1.),(1.,0.707106781186548,1.)))
REPRESENTATION_ITEM('')
SURFACE()
);
#2650=(
BOUNDED_SURFACE()
B_SPLINE_SURFACE(3,2,((#200326,#200327,#200328),(#200329,#200330,#200331),
(#200332,#200333,#200334),(#200335,#200336,#200337)),.UNSPECIFIED.,.F.,
 .F.,.F.)
B_SPLINE_SURFACE_WITH_KNOTS((4,4),(3,3),(0.,0.000397394410828724),(0.,1.),
 .UNSPECIFIED.)
GEOMETRIC_REPRESENTATION_ITEM()
RATIONAL_B_SPLINE_SURFACE(((1.,0.708689770883335,1.),(1.,0.708376440034495,
1.),(1.,0.707750498698407,1.),(1.,0.707106781186548,1.)))
REPRESENTATION_ITEM('')
SURFACE()
);
#2651=(
BOUNDED_SURFACE()
B_SPLINE_SURFACE(3,2,((#200343,#200344,#200345),(#200346,#200347,#200348),
(#200349,#200350,#200351),(#200352,#200353,#200354)),.UNSPECIFIED.,.F.,
 .F.,.F.)
B_SPLINE_SURFACE_WITH_KNOTS((4,4),(3,3),(-6.42389787197661E-18,0.000511815090126184),
(0.,1.00105592270257),.UNSPECIFIED.)
GEOMETRIC_REPRESENTATION_ITEM()
RATIONAL_B_SPLINE_SURFACE(((1.,0.705266242717368,1.00062243213106),(1.,
0.705584085909023,1.00062176089537),(1.,0.706182089450383,1.00062049800434),
(1.,0.706797508587373,1.00061919833427)))
REPRESENTATION_ITEM('')
SURFACE()
);
#2652=(
BOUNDED_SURFACE()
B_SPLINE_SURFACE(3,2,((#200356,#200357,#200358),(#200359,#200360,#200361),
(#200362,#200363,#200364),(#200365,#200366,#200367)),.UNSPECIFIED.,.F.,
 .F.,.F.)
B_SPLINE_SURFACE_WITH_KNOTS((4,4),(3,3),(0.,0.000397394428086622),(0.,1.),
 .UNSPECIFIED.)
GEOMETRIC_REPRESENTATION_ITEM()
RATIONAL_B_SPLINE_SURFACE(((1.,0.707106781186548,1.),(1.,0.70645984675908,
1.),(1.,0.705820510737275,1.),(1.,0.705498956110738,1.)))
REPRESENTATION_ITEM('')
SURFACE()
);
#2653=(
BOUNDED_SURFACE()
B_SPLINE_SURFACE(3,2,((#200373,#200374,#200375),(#200376,#200377,#200378),
(#200379,#200380,#200381),(#200382,#200383,#200384),(#200385,#200386,#200387),
(#200388,#200389,#200390)),.UNSPECIFIED.,.F.,.F.,.F.)
B_SPLINE_SURFACE_WITH_KNOTS((4,2,4),(3,3),(0.,0.000257953807872845,0.000515907615745689),
(0.,1.),.UNSPECIFIED.)
GEOMETRIC_REPRESENTATION_ITEM()
RATIONAL_B_SPLINE_SURFACE(((1.,0.874619707139392,1.),(1.,0.874834349679044,
1.),(1.,0.854686104157737,1.),(1.,0.79247659791519,1.),(1.,0.750887854595087,
1.),(1.,0.705585838031451,1.)))
REPRESENTATION_ITEM('')
SURFACE()
);
#2654=(
BOUNDED_SURFACE()
B_SPLINE_SURFACE(3,2,((#200396,#200397,#200398),(#200399,#200400,#200401),
(#200402,#200403,#200404),(#200405,#200406,#200407)),.UNSPECIFIED.,.F.,
 .F.,.F.)
B_SPLINE_SURFACE_WITH_KNOTS((4,4),(3,3),(-7.56231015308639E-18,0.00051181543769915),
(0.,1.00105881331788),.UNSPECIFIED.)
GEOMETRIC_REPRESENTATION_ITEM()
RATIONAL_B_SPLINE_SURFACE(((1.,0.706796661945751,1.00062089519836),(1.,
0.707430821224625,1.00061955228578),(1.,0.708058545830148,1.00061822299943),
(1.,0.708394505252144,1.00061751156281)))
REPRESENTATION_ITEM('')
SURFACE()
);
#2655=(
BOUNDED_SURFACE()
B_SPLINE_SURFACE(3,2,((#200409,#200410,#200411),(#200412,#200413,#200414),
(#200415,#200416,#200417),(#200418,#200419,#200420),(#200421,#200422,#200423),
(#200424,#200425,#200426)),.UNSPECIFIED.,.F.,.F.,.F.)
B_SPLINE_SURFACE_WITH_KNOTS((4,2,4),(3,3),(0.,0.000256915317531263,0.000513830635062527),
(0.,1.),.UNSPECIFIED.)
GEOMETRIC_REPRESENTATION_ITEM()
RATIONAL_B_SPLINE_SURFACE(((1.,0.705585838031485,1.),(1.,0.750902433542256,
1.),(1.,0.792329530083194,1.),(1.,0.854288401593554,1.),(1.,0.874998031125639,
1.),(1.,0.874619707139405,1.)))
REPRESENTATION_ITEM('')
SURFACE()
);
#2656=(
BOUNDED_SURFACE()
B_SPLINE_SURFACE(3,2,((#200432,#200433,#200434),(#200435,#200436,#200437),
(#200438,#200439,#200440),(#200441,#200442,#200443),(#200444,#200445,#200446),
(#200447,#200448,#200449)),.UNSPECIFIED.,.F.,.F.,.F.)
B_SPLINE_SURFACE_WITH_KNOTS((4,2,4),(3,3),(-6.93889390390723E-18,0.000256592814262155,
0.000513185628524316),(0.,1.),.UNSPECIFIED.)
GEOMETRIC_REPRESENTATION_ITEM()
RATIONAL_B_SPLINE_SURFACE(((1.,0.708712527163686,1.),(1.,0.75378090261287,
1.),(1.,0.794538995770134,1.),(1.,0.855070770330187,1.),(1.,0.875018427446025,
1.),(1.,0.874619707139389,1.)))
REPRESENTATION_ITEM('')
SURFACE()
);
#2657=(
BOUNDED_SURFACE()
B_SPLINE_SURFACE(3,2,((#200451,#200452,#200453),(#200454,#200455,#200456),
(#200457,#200458,#200459),(#200460,#200461,#200462)),.UNSPECIFIED.,.F.,
 .F.,.F.)
B_SPLINE_SURFACE_WITH_KNOTS((4,4),(3,3),(-7.56231015308639E-18,0.000511815072430404),
(0.,1.00105598365537),.UNSPECIFIED.)
GEOMETRIC_REPRESENTATION_ITEM()
RATIONAL_B_SPLINE_SURFACE(((1.,0.706797490734704,1.000619234115),(1.,0.706182062147624,
1.00062053388006),(1.,0.70558406277,1.00062179683519),(1.,0.70526622477148,
1.00062246809866)))
REPRESENTATION_ITEM('')
SURFACE()
);
#2658=(
BOUNDED_SURFACE()
B_SPLINE_SURFACE(3,2,((#200468,#200469,#200470),(#200471,#200472,#200473),
(#200474,#200475,#200476),(#200477,#200478,#200479),(#200480,#200481,#200482),
(#200483,#200484,#200485)),.UNSPECIFIED.,.F.,.F.,.F.)
B_SPLINE_SURFACE_WITH_KNOTS((4,2,4),(3,3),(0.,0.000257652232350885,0.000515304464701771),
(0.,1.),.UNSPECIFIED.)
GEOMETRIC_REPRESENTATION_ITEM()
RATIONAL_B_SPLINE_SURFACE(((1.,0.874619707139378,1.),(1.,0.874861180430567,
1.),(1.,0.855455725921006,1.),(1.,0.794699358955097,1.),(1.,0.753768977788738,
1.),(1.,0.708712527163638,1.)))
REPRESENTATION_ITEM('')
SURFACE()
);
#2659=(
BOUNDED_SURFACE()
B_SPLINE_SURFACE(3,2,((#200491,#200492,#200493),(#200494,#200495,#200496),
(#200497,#200498,#200499),(#200500,#200501,#200502)),.UNSPECIFIED.,.F.,
 .F.,.F.)
B_SPLINE_SURFACE_WITH_KNOTS((4,4),(3,3),(-7.58941520739853E-18,0.0003973943736519),
(0.,1.),.UNSPECIFIED.)
GEOMETRIC_REPRESENTATION_ITEM()
RATIONAL_B_SPLINE_SURFACE(((1.,0.707106781186536,1.),(1.,0.707752587915898,
1.),(1.,0.708377654540667,1.),(1.,0.708689770883327,1.)))
REPRESENTATION_ITEM('')
SURFACE()
);
#2660=(
BOUNDED_SURFACE()
B_SPLINE_SURFACE(3,2,((#200504,#200505,#200506),(#200507,#200508,#200509),
(#200510,#200511,#200512),(#200513,#200514,#200515)),.UNSPECIFIED.,.F.,
 .F.,.F.)
B_SPLINE_SURFACE_WITH_KNOTS((4,4),(3,3),(0.,0.000511815456479782),(0.,1.00105873159924),
 .UNSPECIFIED.)
GEOMETRIC_REPRESENTATION_ITEM()
RATIONAL_B_SPLINE_SURFACE(((1.,0.708394529056535,1.0006174638532),(1.,0.708058564167083,
1.00061817524649),(1.,0.707430835372263,1.00061950443911),(1.,0.706796685880587,
1.00062084722732)))
REPRESENTATION_ITEM('')
SURFACE()
);
#2661=(
BOUNDED_SURFACE()
B_SPLINE_SURFACE(3,2,((#200521,#200522,#200523),(#200524,#200525,#200526),
(#200527,#200528,#200529),(#200530,#200531,#200532)),.UNSPECIFIED.,.F.,
 .F.,.F.)
B_SPLINE_SURFACE_WITH_KNOTS((4,4),(3,3),(0.,0.000397394465448297),(0.,1.),
 .UNSPECIFIED.)
GEOMETRIC_REPRESENTATION_ITEM()
RATIONAL_B_SPLINE_SURFACE(((1.,0.705498956110763,1.),(1.,0.705821764811784,
1.),(1.,0.706461952521129,1.),(1.,0.707106781186553,1.)))
REPRESENTATION_ITEM('')
SURFACE()
);
#2662=(
BOUNDED_SURFACE()
B_SPLINE_SURFACE(3,2,((#200538,#200539,#200540),(#200541,#200542,#200543),
(#200544,#200545,#200546),(#200547,#200548,#200549)),.UNSPECIFIED.,.F.,
 .F.,.F.)
B_SPLINE_SURFACE_WITH_KNOTS((4,4),(3,3),(0.,0.000397394410828749),(0.,1.),
 .UNSPECIFIED.)
GEOMETRIC_REPRESENTATION_ITEM()
RATIONAL_B_SPLINE_SURFACE(((1.,0.708689770883354,1.),(1.,0.708376440034453,
1.),(1.,0.70775049869843,1.),(1.,0.707106781186548,1.)))
REPRESENTATION_ITEM('')
SURFACE()
);
#2663=(
BOUNDED_SURFACE()
B_SPLINE_SURFACE(3,2,((#200555,#200556,#200557),(#200558,#200559,#200560),
(#200561,#200562,#200563),(#200564,#200565,#200566)),.UNSPECIFIED.,.F.,
 .F.,.F.)
B_SPLINE_SURFACE_WITH_KNOTS((4,4),(3,3),(0.,0.000511815090126162),(0.,1.00105592270184),
 .UNSPECIFIED.)
GEOMETRIC_REPRESENTATION_ITEM()
RATIONAL_B_SPLINE_SURFACE(((1.,0.705266242717591,1.00062243213062),(1.,
0.705584085909254,1.00062176089494),(1.,0.706182089450601,1.00062049800391),
(1.,0.706797508587589,1.00061919833383)))
REPRESENTATION_ITEM('')
SURFACE()
);
#2664=(
BOUNDED_SURFACE()
B_SPLINE_SURFACE(3,2,((#200568,#200569,#200570),(#200571,#200572,#200573),
(#200574,#200575,#200576),(#200577,#200578,#200579)),.UNSPECIFIED.,.F.,
 .F.,.F.)
B_SPLINE_SURFACE_WITH_KNOTS((4,4),(3,3),(0.,0.000397394428086619),(0.,1.),
 .UNSPECIFIED.)
GEOMETRIC_REPRESENTATION_ITEM()
RATIONAL_B_SPLINE_SURFACE(((1.,0.707106781186543,1.),(1.,0.706459846759101,
1.),(1.,0.705820510737265,1.),(1.,0.705498956110755,1.)))
REPRESENTATION_ITEM('')
SURFACE()
);
#2665=(
BOUNDED_SURFACE()
B_SPLINE_SURFACE(3,2,((#200585,#200586,#200587),(#200588,#200589,#200590),
(#200591,#200592,#200593),(#200594,#200595,#200596),(#200597,#200598,#200599),
(#200600,#200601,#200602)),.UNSPECIFIED.,.F.,.F.,.F.)
B_SPLINE_SURFACE_WITH_KNOTS((4,2,4),(3,3),(0.,0.000257953807872845,0.00051590761574569),
(0.,1.),.UNSPECIFIED.)
GEOMETRIC_REPRESENTATION_ITEM()
RATIONAL_B_SPLINE_SURFACE(((1.,0.874619707139385,1.),(1.,0.874834349679072,
1.),(1.,0.854686104157708,1.),(1.,0.792476597915247,1.),(1.,0.750887854595038,
1.),(1.,0.705585838031441,1.)))
REPRESENTATION_ITEM('')
SURFACE()
);
#2666=(
BOUNDED_SURFACE()
B_SPLINE_SURFACE(3,2,((#200608,#200609,#200610),(#200611,#200612,#200613),
(#200614,#200615,#200616),(#200617,#200618,#200619)),.UNSPECIFIED.,.F.,
 .F.,.F.)
B_SPLINE_SURFACE_WITH_KNOTS((4,4),(3,3),(0.,0.000511815437699156),(0.,1.00105881331423),
 .UNSPECIFIED.)
GEOMETRIC_REPRESENTATION_ITEM()
RATIONAL_B_SPLINE_SURFACE(((1.,0.706796661946819,1.00062089519622),(1.,
0.707430821225705,1.00061955228364),(1.,0.708058545831191,1.0006182229973),
(1.,0.708394505253199,1.00061751156068)))
REPRESENTATION_ITEM('')
SURFACE()
);
#2667=(
BOUNDED_SURFACE()
B_SPLINE_SURFACE(3,2,((#200621,#200622,#200623),(#200624,#200625,#200626),
(#200627,#200628,#200629),(#200630,#200631,#200632),(#200633,#200634,#200635),
(#200636,#200637,#200638)),.UNSPECIFIED.,.F.,.F.,.F.)
B_SPLINE_SURFACE_WITH_KNOTS((4,2,4),(3,3),(-2.71050543121376E-20,0.000256915317531268,
0.000513830635062536),(0.,1.),.UNSPECIFIED.)
GEOMETRIC_REPRESENTATION_ITEM()
RATIONAL_B_SPLINE_SURFACE(((1.,0.705585838031435,1.),(1.,0.750902433542923,
1.),(1.,0.792329530082311,1.),(1.,0.85428840159443,1.),(1.,0.874998031124965,
1.),(1.,0.874619707139413,1.)))
REPRESENTATION_ITEM('')
SURFACE()
);
#2668=(
BOUNDED_SURFACE()
B_SPLINE_SURFACE(3,2,((#200644,#200645,#200646),(#200647,#200648,#200649),
(#200650,#200651,#200652),(#200653,#200654,#200655),(#200656,#200657,#200658),
(#200659,#200660,#200661)),.UNSPECIFIED.,.F.,.F.,.F.)
B_SPLINE_SURFACE_WITH_KNOTS((4,2,4),(3,3),(0.,0.00025659281426216,0.000513185628524319),
(0.,1.),.UNSPECIFIED.)
GEOMETRIC_REPRESENTATION_ITEM()
RATIONAL_B_SPLINE_SURFACE(((1.,0.708712527163666,1.),(1.,0.753780902613624,
1.),(1.,0.794538995769114,1.),(1.,0.8550707703312,1.),(1.,0.875018427445238,
1.),(1.,0.874619707139389,1.)))
REPRESENTATION_ITEM('')
SURFACE()
);
#2669=(
BOUNDED_SURFACE()
B_SPLINE_SURFACE(3,2,((#200663,#200664,#200665),(#200666,#200667,#200668),
(#200669,#200670,#200671),(#200672,#200673,#200674)),.UNSPECIFIED.,.F.,
 .F.,.F.)
B_SPLINE_SURFACE_WITH_KNOTS((4,4),(3,3),(0.,0.000511815072430393),(0.,1.001055983657),
 .UNSPECIFIED.)
GEOMETRIC_REPRESENTATION_ITEM()
RATIONAL_B_SPLINE_SURFACE(((1.,0.706797490734239,1.00061923411595),(1.,
0.706182062147121,1.00062053388101),(1.,0.705584062769543,1.00062179683615),
(1.,0.705266224770998,1.00062246809961)))
REPRESENTATION_ITEM('')
SURFACE()
);
#2670=(
BOUNDED_SURFACE()
B_SPLINE_SURFACE(3,2,((#200680,#200681,#200682),(#200683,#200684,#200685),
(#200686,#200687,#200688),(#200689,#200690,#200691),(#200692,#200693,#200694),
(#200695,#200696,#200697)),.UNSPECIFIED.,.F.,.F.,.F.)
B_SPLINE_SURFACE_WITH_KNOTS((4,2,4),(3,3),(0.,0.000257652232350883,0.000515304464701766),
(0.,1.),.UNSPECIFIED.)
GEOMETRIC_REPRESENTATION_ITEM()
RATIONAL_B_SPLINE_SURFACE(((1.,0.874619707139393,1.),(1.,0.87486118043087,
1.),(1.,0.85545572592062,1.),(1.,0.794699358955489,1.),(1.,0.753768977788488,
1.),(1.,0.708712527163643,1.)))
REPRESENTATION_ITEM('')
SURFACE()
);
#2671=(
BOUNDED_SURFACE()
B_SPLINE_SURFACE(3,2,((#200703,#200704,#200705),(#200706,#200707,#200708),
(#200709,#200710,#200711),(#200712,#200713,#200714)),.UNSPECIFIED.,.F.,
 .F.,.F.)
B_SPLINE_SURFACE_WITH_KNOTS((4,4),(3,3),(0.,0.00039739437365191),(0.,1.),
 .UNSPECIFIED.)
GEOMETRIC_REPRESENTATION_ITEM()
RATIONAL_B_SPLINE_SURFACE(((1.,0.707106781186552,1.),(1.,0.707752587915889,
1.),(1.,0.708377654540681,1.),(1.,0.708689770883327,1.)))
REPRESENTATION_ITEM('')
SURFACE()
);
#2672=(
BOUNDED_SURFACE()
B_SPLINE_SURFACE(3,2,((#200716,#200717,#200718),(#200719,#200720,#200721),
(#200722,#200723,#200724),(#200725,#200726,#200727)),.UNSPECIFIED.,.F.,
 .F.,.F.)
B_SPLINE_SURFACE_WITH_KNOTS((4,4),(3,3),(-6.42389787197661E-18,0.000511815456479792),
(0.,1.00105873159888),.UNSPECIFIED.)
GEOMETRIC_REPRESENTATION_ITEM()
RATIONAL_B_SPLINE_SURFACE(((1.,0.708394529056643,1.00061746385299),(1.,
0.708058564167205,1.00061817524628),(1.,0.707430835372362,1.0006195044389),
(1.,0.706796685880692,1.00062084722711)))
REPRESENTATION_ITEM('')
SURFACE()
);
#2673=(
BOUNDED_SURFACE()
B_SPLINE_SURFACE(3,2,((#200733,#200734,#200735),(#200736,#200737,#200738),
(#200739,#200740,#200741),(#200742,#200743,#200744)),.UNSPECIFIED.,.F.,
 .F.,.F.)
B_SPLINE_SURFACE_WITH_KNOTS((4,4),(3,3),(0.,0.000397394465448312),(0.,1.),
 .UNSPECIFIED.)
GEOMETRIC_REPRESENTATION_ITEM()
RATIONAL_B_SPLINE_SURFACE(((1.,0.705498956110746,1.),(1.,0.705821764811805,
1.),(1.,0.706461952521133,1.),(1.,0.707106781186548,1.)))
REPRESENTATION_ITEM('')
SURFACE()
);
#2674=(
BOUNDED_SURFACE()
B_SPLINE_SURFACE(3,2,((#200750,#200751,#200752),(#200753,#200754,#200755),
(#200756,#200757,#200758),(#200759,#200760,#200761)),.UNSPECIFIED.,.F.,
 .F.,.F.)
B_SPLINE_SURFACE_WITH_KNOTS((4,4),(3,3),(0.,0.000397394410828737),(0.,1.),
 .UNSPECIFIED.)
GEOMETRIC_REPRESENTATION_ITEM()
RATIONAL_B_SPLINE_SURFACE(((1.,0.708689770883323,1.),(1.,0.708376440034491,
1.),(1.,0.707750498698409,1.),(1.,0.707106781186548,1.)))
REPRESENTATION_ITEM('')
SURFACE()
);
#2675=(
BOUNDED_SURFACE()
B_SPLINE_SURFACE(3,2,((#200767,#200768,#200769),(#200770,#200771,#200772),
(#200773,#200774,#200775),(#200776,#200777,#200778)),.UNSPECIFIED.,.F.,
 .F.,.F.)
B_SPLINE_SURFACE_WITH_KNOTS((4,4),(3,3),(0.,0.000511815090126173),(0.,1.00105592270387),
 .UNSPECIFIED.)
GEOMETRIC_REPRESENTATION_ITEM()
RATIONAL_B_SPLINE_SURFACE(((1.,0.705266242716999,1.00062243213183),(1.,
0.705584085908639,1.00062176089614),(1.,0.706182089450016,1.00062049800511),
(1.,0.706797508586992,1.00061919833503)))
REPRESENTATION_ITEM('')
SURFACE()
);
#2676=(
BOUNDED_SURFACE()
B_SPLINE_SURFACE(3,2,((#200780,#200781,#200782),(#200783,#200784,#200785),
(#200786,#200787,#200788),(#200789,#200790,#200791)),.UNSPECIFIED.,.F.,
 .F.,.F.)
B_SPLINE_SURFACE_WITH_KNOTS((4,4),(3,3),(0.,0.000397394428086623),(0.,1.),
 .UNSPECIFIED.)
GEOMETRIC_REPRESENTATION_ITEM()
RATIONAL_B_SPLINE_SURFACE(((1.,0.707106781186549,1.),(1.,0.706459846759093,
1.),(1.,0.70582051073728,1.),(1.,0.705498956110743,1.)))
REPRESENTATION_ITEM('')
SURFACE()
);
#2677=(
BOUNDED_SURFACE()
B_SPLINE_SURFACE(3,2,((#200797,#200798,#200799),(#200800,#200801,#200802),
(#200803,#200804,#200805),(#200806,#200807,#200808),(#200809,#200810,#200811),
(#200812,#200813,#200814)),.UNSPECIFIED.,.F.,.F.,.F.)
B_SPLINE_SURFACE_WITH_KNOTS((4,2,4),(3,3),(-1.68051336735253E-18,0.000257953807872851,
0.000515907615745705),(0.,1.),.UNSPECIFIED.)
GEOMETRIC_REPRESENTATION_ITEM()
RATIONAL_B_SPLINE_SURFACE(((1.,0.874619707139386,1.),(1.,0.874834349678948,
1.),(1.,0.854686104157841,1.),(1.,0.79247659791508,1.),(1.,0.75088785459518,
1.),(1.,0.705585838031432,1.)))
REPRESENTATION_ITEM('')
SURFACE()
);
#2678=(
BOUNDED_SURFACE()
B_SPLINE_SURFACE(3,2,((#200820,#200821,#200822),(#200823,#200824,#200825),
(#200826,#200827,#200828),(#200829,#200830,#200831)),.UNSPECIFIED.,.F.,
 .F.,.F.)
B_SPLINE_SURFACE_WITH_KNOTS((4,4),(3,3),(0.,0.000511815437699152),(0.,1.00105881331679),
 .UNSPECIFIED.)
GEOMETRIC_REPRESENTATION_ITEM()
RATIONAL_B_SPLINE_SURFACE(((1.,0.706796661946069,1.00062089519772),(1.,
0.70743082122493,1.00061955228514),(1.,0.708058545830472,1.0006182229988),
(1.,0.708394505252429,1.00061751156218)))
REPRESENTATION_ITEM('')
SURFACE()
);
#2679=(
BOUNDED_SURFACE()
B_SPLINE_SURFACE(3,2,((#200833,#200834,#200835),(#200836,#200837,#200838),
(#200839,#200840,#200841),(#200842,#200843,#200844),(#200845,#200846,#200847),
(#200848,#200849,#200850)),.UNSPECIFIED.,.F.,.F.,.F.)
B_SPLINE_SURFACE_WITH_KNOTS((4,2,4),(3,3),(-1.89735380184963E-19,0.000256915317531259,
0.000513830635062518),(0.,1.),.UNSPECIFIED.)
GEOMETRIC_REPRESENTATION_ITEM()
RATIONAL_B_SPLINE_SURFACE(((1.,0.705585838031435,1.),(1.,0.75090243354274,
1.),(1.,0.792329530082507,1.),(1.,0.854288401594194,1.),(1.,0.874998031125134,
1.),(1.,0.874619707139387,1.)))
REPRESENTATION_ITEM('')
SURFACE()
);
#2680=(
BOUNDED_SURFACE()
B_SPLINE_SURFACE(3,2,((#200856,#200857,#200858),(#200859,#200860,#200861),
(#200862,#200863,#200864),(#200865,#200866,#200867),(#200868,#200869,#200870),
(#200871,#200872,#200873)),.UNSPECIFIED.,.F.,.F.,.F.)
B_SPLINE_SURFACE_WITH_KNOTS((4,2,4),(3,3),(0.,0.000256592814262159,0.000513185628524318),
(0.,1.),.UNSPECIFIED.)
GEOMETRIC_REPRESENTATION_ITEM()
RATIONAL_B_SPLINE_SURFACE(((1.,0.708712527163674,1.),(1.,0.753780902613273,
1.),(1.,0.794538995769612,1.),(1.,0.855070770330695,1.),(1.,0.875018427445628,
1.),(1.,0.874619707139392,1.)))
REPRESENTATION_ITEM('')
SURFACE()
);
#2681=(
BOUNDED_SURFACE()
B_SPLINE_SURFACE(3,2,((#200875,#200876,#200877),(#200878,#200879,#200880),
(#200881,#200882,#200883),(#200884,#200885,#200886)),.UNSPECIFIED.,.F.,
 .F.,.F.)
B_SPLINE_SURFACE_WITH_KNOTS((4,4),(3,3),(0.,0.000511815072430392),(0.,1.00105598365776),
 .UNSPECIFIED.)
GEOMETRIC_REPRESENTATION_ITEM()
RATIONAL_B_SPLINE_SURFACE(((1.,0.70679749073401,1.0006192341164),(1.,0.706182062146944,
1.00062053388146),(1.,0.705584062769289,1.0006217968366),(1.,0.705266224770748,
1.00062246810006)))
REPRESENTATION_ITEM('')
SURFACE()
);
#2682=(
BOUNDED_SURFACE()
B_SPLINE_SURFACE(3,2,((#200892,#200893,#200894),(#200895,#200896,#200897),
(#200898,#200899,#200900),(#200901,#200902,#200903),(#200904,#200905,#200906),
(#200907,#200908,#200909)),.UNSPECIFIED.,.F.,.F.,.F.)
B_SPLINE_SURFACE_WITH_KNOTS((4,2,4),(3,3),(0.,0.000257652232350884,0.000515304464701767),
(0.,1.),.UNSPECIFIED.)
GEOMETRIC_REPRESENTATION_ITEM()
RATIONAL_B_SPLINE_SURFACE(((1.,0.87461970713939,1.),(1.,0.874861180430969,
1.),(1.,0.855455725920519,1.),(1.,0.794699358955606,1.),(1.,0.753768977788385,
1.),(1.,0.708712527163658,1.)))
REPRESENTATION_ITEM('')
SURFACE()
);
#2683=(
BOUNDED_SURFACE()
B_SPLINE_SURFACE(3,2,((#200915,#200916,#200917),(#200918,#200919,#200920),
(#200921,#200922,#200923),(#200924,#200925,#200926)),.UNSPECIFIED.,.F.,
 .F.,.F.)
B_SPLINE_SURFACE_WITH_KNOTS((4,4),(3,3),(-6.91178884959509E-18,0.000397394373651912),
(0.,1.),.UNSPECIFIED.)
GEOMETRIC_REPRESENTATION_ITEM()
RATIONAL_B_SPLINE_SURFACE(((1.,0.707106781186545,1.),(1.,0.707752587915905,
1.),(1.,0.708377654540673,1.),(1.,0.708689770883352,1.)))
REPRESENTATION_ITEM('')
SURFACE()
);
#2684=(
BOUNDED_SURFACE()
B_SPLINE_SURFACE(3,2,((#200928,#200929,#200930),(#200931,#200932,#200933),
(#200934,#200935,#200936),(#200937,#200938,#200939)),.UNSPECIFIED.,.F.,
 .F.,.F.)
B_SPLINE_SURFACE_WITH_KNOTS((4,4),(3,3),(0.,0.000511815456479794),(0.,1.00105873160034),
 .UNSPECIFIED.)
GEOMETRIC_REPRESENTATION_ITEM()
RATIONAL_B_SPLINE_SURFACE(((1.,0.708394529056221,1.00061746385384),(1.,
0.708058564166755,1.00061817524713),(1.,0.70743083537196,1.00061950443976),
(1.,0.706796685880264,1.00062084722797)))
REPRESENTATION_ITEM('')
SURFACE()
);
#2685=(
BOUNDED_SURFACE()
B_SPLINE_SURFACE(3,2,((#200945,#200946,#200947),(#200948,#200949,#200950),
(#200951,#200952,#200953),(#200954,#200955,#200956)),.UNSPECIFIED.,.F.,
 .F.,.F.)
B_SPLINE_SURFACE_WITH_KNOTS((4,4),(3,3),(-6.50521303491303E-18,0.000397394465448303),
(0.,1.),.UNSPECIFIED.)
GEOMETRIC_REPRESENTATION_ITEM()
RATIONAL_B_SPLINE_SURFACE(((1.,0.705498956110746,1.),(1.,0.705821764811771,
1.),(1.,0.70646195252114,1.),(1.,0.707106781186545,1.)))
REPRESENTATION_ITEM('')
SURFACE()
);
#2686=(
BOUNDED_SURFACE()
B_SPLINE_SURFACE(3,2,((#200962,#200963,#200964),(#200965,#200966,#200967),
(#200968,#200969,#200970),(#200971,#200972,#200973)),.UNSPECIFIED.,.F.,
 .F.,.F.)
B_SPLINE_SURFACE_WITH_KNOTS((4,4),(3,3),(0.,0.000397394410828732),(0.,1.),
 .UNSPECIFIED.)
GEOMETRIC_REPRESENTATION_ITEM()
RATIONAL_B_SPLINE_SURFACE(((1.,0.708689770883332,1.),(1.,0.708376440034489,
1.),(1.,0.707750498698412,1.),(1.,0.707106781186548,1.)))
REPRESENTATION_ITEM('')
SURFACE()
);
#2687=(
BOUNDED_SURFACE()
B_SPLINE_SURFACE(3,2,((#200979,#200980,#200981),(#200982,#200983,#200984),
(#200985,#200986,#200987),(#200988,#200989,#200990)),.UNSPECIFIED.,.F.,
 .F.,.F.)
B_SPLINE_SURFACE_WITH_KNOTS((4,4),(3,3),(0.,0.000511815090126178),(0.,1.00105592270281),
 .UNSPECIFIED.)
GEOMETRIC_REPRESENTATION_ITEM()
RATIONAL_B_SPLINE_SURFACE(((1.,0.705266242717305,1.0006224321312),(1.,0.705584085908961,
1.00062176089551),(1.,0.70618208945032,1.00062049800448),(1.,0.706797508587304,
1.0006191983344)))
REPRESENTATION_ITEM('')
SURFACE()
);
#2688=(
BOUNDED_SURFACE()
B_SPLINE_SURFACE(3,2,((#200992,#200993,#200994),(#200995,#200996,#200997),
(#200998,#200999,#201000),(#201001,#201002,#201003)),.UNSPECIFIED.,.F.,
 .F.,.F.)
B_SPLINE_SURFACE_WITH_KNOTS((4,4),(3,3),(-6.85757874097082E-18,0.00039739442808662),
(0.,1.),.UNSPECIFIED.)
GEOMETRIC_REPRESENTATION_ITEM()
RATIONAL_B_SPLINE_SURFACE(((1.,0.707106781186548,1.),(1.,0.706459846759103,
1.),(1.,0.705820510737258,1.),(1.,0.705498956110751,1.)))
REPRESENTATION_ITEM('')
SURFACE()
);
#2689=(
BOUNDED_SURFACE()
B_SPLINE_SURFACE(3,2,((#201009,#201010,#201011),(#201012,#201013,#201014),
(#201015,#201016,#201017),(#201018,#201019,#201020),(#201021,#201022,#201023),
(#201024,#201025,#201026)),.UNSPECIFIED.,.F.,.F.,.F.)
B_SPLINE_SURFACE_WITH_KNOTS((4,2,4),(3,3),(0.,0.000257953807872855,0.00051590761574571),
(0.,1.),.UNSPECIFIED.)
GEOMETRIC_REPRESENTATION_ITEM()
RATIONAL_B_SPLINE_SURFACE(((1.,0.874619707139392,1.),(1.,0.874834349678956,
1.),(1.,0.854686104157832,1.),(1.,0.79247659791509,1.),(1.,0.750887854595159,
1.),(1.,0.70558583803143,1.)))
REPRESENTATION_ITEM('')
SURFACE()
);
#2690=(
BOUNDED_SURFACE()
B_SPLINE_SURFACE(3,2,((#201032,#201033,#201034),(#201035,#201036,#201037),
(#201038,#201039,#201040),(#201041,#201042,#201043)),.UNSPECIFIED.,.F.,
 .F.,.F.)
B_SPLINE_SURFACE_WITH_KNOTS((4,4),(3,3),(0.,0.000511815437699152),(0.,1.00105881331544),
 .UNSPECIFIED.)
GEOMETRIC_REPRESENTATION_ITEM()
RATIONAL_B_SPLINE_SURFACE(((1.,0.706796661946467,1.00062089519692),(1.,
0.707430821225345,1.00061955228435),(1.,0.708058545830854,1.000618222998),
(1.,0.708394505252849,1.00061751156139)))
REPRESENTATION_ITEM('')
SURFACE()
);
#2691=(
BOUNDED_SURFACE()
B_SPLINE_SURFACE(3,2,((#201045,#201046,#201047),(#201048,#201049,#201050),
(#201051,#201052,#201053),(#201054,#201055,#201056),(#201057,#201058,#201059),
(#201060,#201061,#201062)),.UNSPECIFIED.,.F.,.F.,.F.)
B_SPLINE_SURFACE_WITH_KNOTS((4,2,4),(3,3),(-2.71050543121376E-20,0.000256915317531259,
0.000513830635062519),(0.,1.),.UNSPECIFIED.)
GEOMETRIC_REPRESENTATION_ITEM()
RATIONAL_B_SPLINE_SURFACE(((1.,0.705585838031442,1.),(1.,0.750902433542892,
1.),(1.,0.79232953008232,1.),(1.,0.854288401594389,1.),(1.,0.874998031124987,
1.),(1.,0.874619707139392,1.)))
REPRESENTATION_ITEM('')
SURFACE()
);
#2692=(
BOUNDED_SURFACE()
B_SPLINE_SURFACE(3,2,((#201068,#201069,#201070),(#201071,#201072,#201073),
(#201074,#201075,#201076),(#201077,#201078,#201079),(#201080,#201081,#201082),
(#201083,#201084,#201085)),.UNSPECIFIED.,.F.,.F.,.F.)
B_SPLINE_SURFACE_WITH_KNOTS((4,2,4),(3,3),(-9.70360944374526E-18,0.000256592814262151,
0.000513185628524312),(0.,1.),.UNSPECIFIED.)
GEOMETRIC_REPRESENTATION_ITEM()
RATIONAL_B_SPLINE_SURFACE(((1.,0.708712527163664,1.),(1.,0.753780902613591,
1.),(1.,0.79453899576919,1.),(1.,0.855070770331123,1.),(1.,0.875018427445306,
1.),(1.,0.87461970713939,1.)))
REPRESENTATION_ITEM('')
SURFACE()
);
#2693=(
BOUNDED_SURFACE()
B_SPLINE_SURFACE(3,2,((#201087,#201088,#201089),(#201090,#201091,#201092),
(#201093,#201094,#201095),(#201096,#201097,#201098)),.UNSPECIFIED.,.F.,
 .F.,.F.)
B_SPLINE_SURFACE_WITH_KNOTS((4,4),(3,3),(0.,0.000511815072430396),(0.,1.00105598365804),
 .UNSPECIFIED.)
GEOMETRIC_REPRESENTATION_ITEM()
RATIONAL_B_SPLINE_SURFACE(((1.,0.706797490733929,1.00061923411656),(1.,
0.706182062146834,1.00062053388163),(1.,0.705584062769227,1.00062179683677),
(1.,0.705266224770692,1.00062246810023)))
REPRESENTATION_ITEM('')
SURFACE()
);
#2694=(
BOUNDED_SURFACE()
B_SPLINE_SURFACE(3,2,((#201104,#201105,#201106),(#201107,#201108,#201109),
(#201110,#201111,#201112),(#201113,#201114,#201115),(#201116,#201117,#201118),
(#201119,#201120,#201121)),.UNSPECIFIED.,.F.,.F.,.F.)
B_SPLINE_SURFACE_WITH_KNOTS((4,2,4),(3,3),(-6.36968776335234E-19,0.000257652232350877,
0.000515304464701754),(0.,1.),.UNSPECIFIED.)
GEOMETRIC_REPRESENTATION_ITEM()
RATIONAL_B_SPLINE_SURFACE(((1.,0.874619707139396,1.),(1.,0.874861180430735,
1.),(1.,0.855455725920824,1.),(1.,0.794699358955301,1.),(1.,0.753768977788632,
1.),(1.,0.708712527163662,1.)))
REPRESENTATION_ITEM('')
SURFACE()
);
#2695=(
BOUNDED_SURFACE()
B_SPLINE_SURFACE(3,2,((#201127,#201128,#201129),(#201130,#201131,#201132),
(#201133,#201134,#201135),(#201136,#201137,#201138)),.UNSPECIFIED.,.F.,
 .F.,.F.)
B_SPLINE_SURFACE_WITH_KNOTS((4,4),(3,3),(0.,0.000397394373651917),(0.,1.),
 .UNSPECIFIED.)
GEOMETRIC_REPRESENTATION_ITEM()
RATIONAL_B_SPLINE_SURFACE(((1.,0.707106781186548,1.),(1.,0.70775258791587,
1.),(1.,0.708377654540717,1.),(1.,0.708689770883313,1.)))
REPRESENTATION_ITEM('')
SURFACE()
);
#2696=(
BOUNDED_SURFACE()
B_SPLINE_SURFACE(3,2,((#201140,#201141,#201142),(#201143,#201144,#201145),
(#201146,#201147,#201148),(#201149,#201150,#201151)),.UNSPECIFIED.,.F.,
 .F.,.F.)
B_SPLINE_SURFACE_WITH_KNOTS((4,4),(3,3),(0.,0.000511815456479795),(0.,1.00105873159818),
 .UNSPECIFIED.)
GEOMETRIC_REPRESENTATION_ITEM()
RATIONAL_B_SPLINE_SURFACE(((1.,0.708394529056861,1.00061746385258),(1.,
0.708058564167389,1.00061817524587),(1.,0.70743083537258,1.00061950443849),
(1.,0.706796685880899,1.0006208472267)))
REPRESENTATION_ITEM('')
SURFACE()
);
#2697=(
BOUNDED_SURFACE()
B_SPLINE_SURFACE(3,2,((#201157,#201158,#201159),(#201160,#201161,#201162),
(#201163,#201164,#201165),(#201166,#201167,#201168)),.UNSPECIFIED.,.F.,
 .F.,.F.)
B_SPLINE_SURFACE_WITH_KNOTS((4,4),(3,3),(0.,0.000397394465448298),(0.,1.),
 .UNSPECIFIED.)
GEOMETRIC_REPRESENTATION_ITEM()
RATIONAL_B_SPLINE_SURFACE(((1.,0.70549895611077,1.),(1.,0.70582176481177,
1.),(1.,0.706461952521145,1.),(1.,0.707106781186548,1.)))
REPRESENTATION_ITEM('')
SURFACE()
);
#2698=(
BOUNDED_SURFACE()
B_SPLINE_SURFACE(3,2,((#201174,#201175,#201176),(#201177,#201178,#201179),
(#201180,#201181,#201182),(#201183,#201184,#201185)),.UNSPECIFIED.,.F.,
 .F.,.F.)
B_SPLINE_SURFACE_WITH_KNOTS((4,4),(3,3),(0.,0.00039739441082875),(0.,1.),
 .UNSPECIFIED.)
GEOMETRIC_REPRESENTATION_ITEM()
RATIONAL_B_SPLINE_SURFACE(((1.,0.708689770883323,1.),(1.,0.708376440034469,
1.),(1.,0.707750498698414,1.),(1.,0.707106781186552,1.)))
REPRESENTATION_ITEM('')
SURFACE()
);
#2699=(
BOUNDED_SURFACE()
B_SPLINE_SURFACE(3,2,((#201191,#201192,#201193),(#201194,#201195,#201196),
(#201197,#201198,#201199),(#201200,#201201,#201202)),.UNSPECIFIED.,.F.,
 .F.,.F.)
B_SPLINE_SURFACE_WITH_KNOTS((4,4),(3,3),(0.,0.000511815090126182),(0.,1.00105592270276),
 .UNSPECIFIED.)
GEOMETRIC_REPRESENTATION_ITEM()
RATIONAL_B_SPLINE_SURFACE(((1.,0.705266242717327,1.00062243213117),(1.,
0.705584085908971,1.00062176089549),(1.,0.706182089450324,1.00062049800446),
(1.,0.706797508587317,1.00061919833438)))
REPRESENTATION_ITEM('')
SURFACE()
);
#2700=(
BOUNDED_SURFACE()
B_SPLINE_SURFACE(3,2,((#201204,#201205,#201206),(#201207,#201208,#201209),
(#201210,#201211,#201212),(#201213,#201214,#201215)),.UNSPECIFIED.,.F.,
 .F.,.F.)
B_SPLINE_SURFACE_WITH_KNOTS((4,4),(3,3),(0.,0.000397394428086637),(0.,1.),
 .UNSPECIFIED.)
GEOMETRIC_REPRESENTATION_ITEM()
RATIONAL_B_SPLINE_SURFACE(((1.,0.707106781186548,1.),(1.,0.706459846759089,
1.),(1.,0.705820510737281,1.),(1.,0.705498956110758,1.)))
REPRESENTATION_ITEM('')
SURFACE()
);
#2701=(
BOUNDED_SURFACE()
B_SPLINE_SURFACE(3,2,((#201221,#201222,#201223),(#201224,#201225,#201226),
(#201227,#201228,#201229),(#201230,#201231,#201232),(#201233,#201234,#201235),
(#201236,#201237,#201238)),.UNSPECIFIED.,.F.,.F.,.F.)
B_SPLINE_SURFACE_WITH_KNOTS((4,2,4),(3,3),(0.,0.000257953807872843,0.000515907615745686),
(0.,1.),.UNSPECIFIED.)
GEOMETRIC_REPRESENTATION_ITEM()
RATIONAL_B_SPLINE_SURFACE(((1.,0.874619707139388,1.),(1.,0.874834349679259,
1.),(1.,0.854686104157437,1.),(1.,0.792476597915486,1.),(1.,0.750887854594861,
1.),(1.,0.705585838031449,1.)))
REPRESENTATION_ITEM('')
SURFACE()
);
#2702=(
BOUNDED_SURFACE()
B_SPLINE_SURFACE(3,2,((#201244,#201245,#201246),(#201247,#201248,#201249),
(#201250,#201251,#201252),(#201253,#201254,#201255)),.UNSPECIFIED.,.F.,
 .F.,.F.)
B_SPLINE_SURFACE_WITH_KNOTS((4,4),(3,3),(0.,0.000511815437699153),(0.,1.00105881331748),
 .UNSPECIFIED.)
GEOMETRIC_REPRESENTATION_ITEM()
RATIONAL_B_SPLINE_SURFACE(((1.,0.706796661945868,1.00062089519812),(1.,
0.707430821224752,1.00061955228554),(1.,0.708058545830254,1.0006182229992),
(1.,0.708394505252245,1.00061751156258)))
REPRESENTATION_ITEM('')
SURFACE()
);
#2703=(
BOUNDED_SURFACE()
B_SPLINE_SURFACE(3,2,((#201257,#201258,#201259),(#201260,#201261,#201262),
(#201263,#201264,#201265),(#201266,#201267,#201268),(#201269,#201270,#201271),
(#201272,#201273,#201274)),.UNSPECIFIED.,.F.,.F.,.F.)
B_SPLINE_SURFACE_WITH_KNOTS((4,2,4),(3,3),(0.,0.000256915317531264,0.000513830635062527),
(0.,1.),.UNSPECIFIED.)
GEOMETRIC_REPRESENTATION_ITEM()
RATIONAL_B_SPLINE_SURFACE(((1.,0.705585838031439,1.),(1.,0.750902433542536,
1.),(1.,0.79232953008279,1.),(1.,0.854288401593904,1.),(1.,0.874998031125365,
1.),(1.,0.874619707139386,1.)))
REPRESENTATION_ITEM('')
SURFACE()
);
#2704=(
BOUNDED_SURFACE()
B_SPLINE_SURFACE(3,2,((#201280,#201281,#201282),(#201283,#201284,#201285),
(#201286,#201287,#201288),(#201289,#201290,#201291),(#201292,#201293,#201294),
(#201295,#201296,#201297)),.UNSPECIFIED.,.F.,.F.,.F.)
B_SPLINE_SURFACE_WITH_KNOTS((4,2,4),(3,3),(0.,0.000256592814262156,0.000513185628524312),
(0.,1.),.UNSPECIFIED.)
GEOMETRIC_REPRESENTATION_ITEM()
RATIONAL_B_SPLINE_SURFACE(((1.,0.708712527163657,1.),(1.,0.753780902613628,
1.),(1.,0.79453899576917,1.),(1.,0.85507077033114,1.),(1.,0.875018427445298,
1.),(1.,0.87461970713939,1.)))
REPRESENTATION_ITEM('')
SURFACE()
);
#2705=(
BOUNDED_SURFACE()
B_SPLINE_SURFACE(3,2,((#201299,#201300,#201301),(#201302,#201303,#201304),
(#201305,#201306,#201307),(#201308,#201309,#201310)),.UNSPECIFIED.,.F.,
 .F.,.F.)
B_SPLINE_SURFACE_WITH_KNOTS((4,4),(3,3),(2.71050543121376E-20,0.000511815072430395),
(0.,1.00105598365867),.UNSPECIFIED.)
GEOMETRIC_REPRESENTATION_ITEM()
RATIONAL_B_SPLINE_SURFACE(((1.,0.706797490733745,1.00061923411693),(1.,
0.706182062146666,1.00062053388199),(1.,0.70558406276901,1.00062179683714),
(1.,0.705266224770511,1.0006224681006)))
REPRESENTATION_ITEM('')
SURFACE()
);
#2706=(
BOUNDED_SURFACE()
B_SPLINE_SURFACE(3,2,((#201316,#201317,#201318),(#201319,#201320,#201321),
(#201322,#201323,#201324),(#201325,#201326,#201327),(#201328,#201329,#201330),
(#201331,#201332,#201333)),.UNSPECIFIED.,.F.,.F.,.F.)
B_SPLINE_SURFACE_WITH_KNOTS((4,2,4),(3,3),(0.,0.000257652232350881,0.000515304464701761),
(0.,1.),.UNSPECIFIED.)
GEOMETRIC_REPRESENTATION_ITEM()
RATIONAL_B_SPLINE_SURFACE(((1.,0.874619707139398,1.),(1.,0.874861180431049,
1.),(1.,0.855455725920415,1.),(1.,0.794699358955707,1.),(1.,0.753768977788306,
1.),(1.,0.708712527163674,1.)))
REPRESENTATION_ITEM('')
SURFACE()
);
#2707=(
BOUNDED_SURFACE()
B_SPLINE_SURFACE(3,2,((#201339,#201340,#201341),(#201342,#201343,#201344),
(#201345,#201346,#201347),(#201348,#201349,#201350)),.UNSPECIFIED.,.F.,
 .F.,.F.)
B_SPLINE_SURFACE_WITH_KNOTS((4,4),(3,3),(0.,0.000397394373651915),(0.,1.),
 .UNSPECIFIED.)
GEOMETRIC_REPRESENTATION_ITEM()
RATIONAL_B_SPLINE_SURFACE(((1.,0.707106781186548,1.),(1.,0.707752587915894,
1.),(1.,0.708377654540696,1.),(1.,0.708689770883339,1.)))
REPRESENTATION_ITEM('')
SURFACE()
);
#2708=(
BOUNDED_SURFACE()
B_SPLINE_SURFACE(3,2,((#201352,#201353,#201354),(#201355,#201356,#201357),
(#201358,#201359,#201360),(#201361,#201362,#201363)),.UNSPECIFIED.,.F.,
 .F.,.F.)
B_SPLINE_SURFACE_WITH_KNOTS((4,4),(3,3),(0.,0.000511815456479784),(0.,1.00105873159958),
 .UNSPECIFIED.)
GEOMETRIC_REPRESENTATION_ITEM()
RATIONAL_B_SPLINE_SURFACE(((1.,0.70839452905645,1.00061746385339),(1.,0.708058564166994,
1.00061817524668),(1.,0.707430835372169,1.00061950443931),(1.,0.706796685880488,
1.00062084722752)))
REPRESENTATION_ITEM('')
SURFACE()
);
#2709=(
BOUNDED_SURFACE()
B_SPLINE_SURFACE(3,2,((#201369,#201370,#201371),(#201372,#201373,#201374),
(#201375,#201376,#201377),(#201378,#201379,#201380)),.UNSPECIFIED.,.F.,
 .F.,.F.)
B_SPLINE_SURFACE_WITH_KNOTS((4,4),(3,3),(0.,0.000397394465448314),(0.,1.),
 .UNSPECIFIED.)
GEOMETRIC_REPRESENTATION_ITEM()
RATIONAL_B_SPLINE_SURFACE(((1.,0.705498956110744,1.),(1.,0.70582176481178,
1.),(1.,0.706461952521134,1.),(1.,0.707106781186548,1.)))
REPRESENTATION_ITEM('')
SURFACE()
);
#2710=(
BOUNDED_SURFACE()
B_SPLINE_SURFACE(3,2,((#201386,#201387,#201388),(#201389,#201390,#201391),
(#201392,#201393,#201394),(#201395,#201396,#201397)),.UNSPECIFIED.,.F.,
 .F.,.F.)
B_SPLINE_SURFACE_WITH_KNOTS((4,4),(3,3),(0.,0.000397394410828745),(0.,1.),
 .UNSPECIFIED.)
GEOMETRIC_REPRESENTATION_ITEM()
RATIONAL_B_SPLINE_SURFACE(((1.,0.708689770883332,1.),(1.,0.708376440034473,
1.),(1.,0.707750498698421,1.),(1.,0.707106781186548,1.)))
REPRESENTATION_ITEM('')
SURFACE()
);
#2711=(
BOUNDED_SURFACE()
B_SPLINE_SURFACE(3,2,((#201403,#201404,#201405),(#201406,#201407,#201408),
(#201409,#201410,#201411),(#201412,#201413,#201414)),.UNSPECIFIED.,.F.,
 .F.,.F.)
B_SPLINE_SURFACE_WITH_KNOTS((4,4),(3,3),(0.,0.000511815090126174),(0.,1.00105592270135),
 .UNSPECIFIED.)
GEOMETRIC_REPRESENTATION_ITEM()
RATIONAL_B_SPLINE_SURFACE(((1.,0.705266242717712,1.00062243213034),(1.,
0.705584085909422,1.00062176089466),(1.,0.706182089450735,1.00062049800363),
(1.,0.706797508587729,1.00061919833355)))
REPRESENTATION_ITEM('')
SURFACE()
);
#2712=(
BOUNDED_SURFACE()
B_SPLINE_SURFACE(3,2,((#201416,#201417,#201418),(#201419,#201420,#201421),
(#201422,#201423,#201424),(#201425,#201426,#201427)),.UNSPECIFIED.,.F.,
 .F.,.F.)
B_SPLINE_SURFACE_WITH_KNOTS((4,4),(3,3),(0.,0.00039739442808662),(0.,1.),
 .UNSPECIFIED.)
GEOMETRIC_REPRESENTATION_ITEM()
RATIONAL_B_SPLINE_SURFACE(((1.,0.707106781186552,1.),(1.,0.706459846759089,
1.),(1.,0.705820510737278,1.),(1.,0.705498956110746,1.)))
REPRESENTATION_ITEM('')
SURFACE()
);
#2713=(
BOUNDED_SURFACE()
B_SPLINE_SURFACE(3,2,((#201433,#201434,#201435),(#201436,#201437,#201438),
(#201439,#201440,#201441),(#201442,#201443,#201444),(#201445,#201446,#201447),
(#201448,#201449,#201450)),.UNSPECIFIED.,.F.,.F.,.F.)
B_SPLINE_SURFACE_WITH_KNOTS((4,2,4),(3,3),(0.,0.000257953807872838,0.000515907615745675),
(0.,1.),.UNSPECIFIED.)
GEOMETRIC_REPRESENTATION_ITEM()
RATIONAL_B_SPLINE_SURFACE(((1.,0.874619707139393,1.),(1.,0.874834349679108,
1.),(1.,0.854686104157634,1.),(1.,0.79247659791531,1.),(1.,0.75088785459499,
1.),(1.,0.70558583803147,1.)))
REPRESENTATION_ITEM('')
SURFACE()
);
#2714=(
BOUNDED_SURFACE()
B_SPLINE_SURFACE(3,2,((#201456,#201457,#201458),(#201459,#201460,#201461),
(#201462,#201463,#201464),(#201465,#201466,#201467)),.UNSPECIFIED.,.F.,
 .F.,.F.)
B_SPLINE_SURFACE_WITH_KNOTS((4,4),(3,3),(0.,0.000511815437699151),(0.,1.00105881331552),
 .UNSPECIFIED.)
GEOMETRIC_REPRESENTATION_ITEM()
RATIONAL_B_SPLINE_SURFACE(((1.,0.706796661946441,1.00062089519697),(1.,
0.707430821225319,1.0006195522844),(1.,0.708058545830829,1.00061822299806),
(1.,0.708394505252824,1.00061751156144)))
REPRESENTATION_ITEM('')
SURFACE()
);
#2715=(
BOUNDED_SURFACE()
B_SPLINE_SURFACE(3,2,((#201469,#201470,#201471),(#201472,#201473,#201474),
(#201475,#201476,#201477),(#201478,#201479,#201480),(#201481,#201482,#201483),
(#201484,#201485,#201486)),.UNSPECIFIED.,.F.,.F.,.F.)
B_SPLINE_SURFACE_WITH_KNOTS((4,2,4),(3,3),(0.,0.000256915317531257,0.000513830635062514),
(0.,1.),.UNSPECIFIED.)
GEOMETRIC_REPRESENTATION_ITEM()
RATIONAL_B_SPLINE_SURFACE(((1.,0.705585838031445,1.),(1.,0.750902433542313,
1.),(1.,0.792329530083068,1.),(1.,0.854288401593637,1.),(1.,0.874998031125529,
1.),(1.,0.874619707139391,1.)))
REPRESENTATION_ITEM('')
SURFACE()
);
#2716=(
BOUNDED_SURFACE()
B_SPLINE_SURFACE(3,2,((#201492,#201493,#201494),(#201495,#201496,#201497),
(#201498,#201499,#201500),(#201501,#201502,#201503),(#201504,#201505,#201506),
(#201507,#201508,#201509)),.UNSPECIFIED.,.F.,.F.,.F.)
B_SPLINE_SURFACE_WITH_KNOTS((4,2,4),(3,3),(0.,0.000256592814262156,0.000513185628524311),
(0.,1.),.UNSPECIFIED.)
GEOMETRIC_REPRESENTATION_ITEM()
RATIONAL_B_SPLINE_SURFACE(((1.,0.708712527163661,1.),(1.,0.753780902613512,
1.),(1.,0.794538995769294,1.),(1.,0.855070770331016,1.),(1.,0.875018427445388,
1.),(1.,0.874619707139394,1.)))
REPRESENTATION_ITEM('')
SURFACE()
);
#2717=(
BOUNDED_SURFACE()
B_SPLINE_SURFACE(3,2,((#201511,#201512,#201513),(#201514,#201515,#201516),
(#201517,#201518,#201519),(#201520,#201521,#201522)),.UNSPECIFIED.,.F.,
 .F.,.F.)
B_SPLINE_SURFACE_WITH_KNOTS((4,4),(3,3),(2.71050543121376E-20,0.000511815072430401),
(0.,1.00105598365598),.UNSPECIFIED.)
GEOMETRIC_REPRESENTATION_ITEM()
RATIONAL_B_SPLINE_SURFACE(((1.,0.706797490734529,1.00061923411535),(1.,
0.706182062147453,1.00062053388041),(1.,0.705584062769824,1.00062179683555),
(1.,0.705266224771297,1.00062246809901)))
REPRESENTATION_ITEM('')
SURFACE()
);
#2718=(
BOUNDED_SURFACE()
B_SPLINE_SURFACE(3,2,((#201528,#201529,#201530),(#201531,#201532,#201533),
(#201534,#201535,#201536),(#201537,#201538,#201539),(#201540,#201541,#201542),
(#201543,#201544,#201545)),.UNSPECIFIED.,.F.,.F.,.F.)
B_SPLINE_SURFACE_WITH_KNOTS((4,2,4),(3,3),(0.,0.000257652232350877,0.000515304464701754),
(0.,1.),.UNSPECIFIED.)
GEOMETRIC_REPRESENTATION_ITEM()
RATIONAL_B_SPLINE_SURFACE(((1.,0.874619707139384,1.),(1.,0.874861180430375,
1.),(1.,0.855455725921361,1.),(1.,0.794699358954753,1.),(1.,0.753768977789027,
1.),(1.,0.708712527163687,1.)))
REPRESENTATION_ITEM('')
SURFACE()
);
#2719=(
BOUNDED_SURFACE()
B_SPLINE_SURFACE(3,2,((#201551,#201552,#201553),(#201554,#201555,#201556),
(#201557,#201558,#201559),(#201560,#201561,#201562)),.UNSPECIFIED.,.F.,
 .F.,.F.)
B_SPLINE_SURFACE_WITH_KNOTS((4,4),(3,3),(0.,0.000397394373651915),(0.,1.),
 .UNSPECIFIED.)
GEOMETRIC_REPRESENTATION_ITEM()
RATIONAL_B_SPLINE_SURFACE(((1.,0.707106781186548,1.),(1.,0.707752587915872,
1.),(1.,0.708377654540717,1.),(1.,0.708689770883309,1.)))
REPRESENTATION_ITEM('')
SURFACE()
);
#2720=(
BOUNDED_SURFACE()
B_SPLINE_SURFACE(3,2,((#201564,#201565,#201566),(#201567,#201568,#201569),
(#201570,#201571,#201572),(#201573,#201574,#201575)),.UNSPECIFIED.,.F.,
 .F.,.F.)
B_SPLINE_SURFACE_WITH_KNOTS((4,4),(3,3),(0.,0.000511815456479786),(0.,1.00105873159942),
 .UNSPECIFIED.)
GEOMETRIC_REPRESENTATION_ITEM()
RATIONAL_B_SPLINE_SURFACE(((1.,0.708394529056477,1.0006174638533),(1.,0.70805856416704,
1.00061817524659),(1.,0.70743083537222,1.00061950443921),(1.,0.706796685880534,
1.00062084722743)))
REPRESENTATION_ITEM('')
SURFACE()
);
#2721=(
BOUNDED_SURFACE()
B_SPLINE_SURFACE(3,2,((#201581,#201582,#201583),(#201584,#201585,#201586),
(#201587,#201588,#201589),(#201590,#201591,#201592)),.UNSPECIFIED.,.F.,
 .F.,.F.)
B_SPLINE_SURFACE_WITH_KNOTS((4,4),(3,3),(0.,0.000397394465448303),(0.,1.),
 .UNSPECIFIED.)
GEOMETRIC_REPRESENTATION_ITEM()
RATIONAL_B_SPLINE_SURFACE(((1.,0.705498956110749,1.),(1.,0.705821764811794,
1.),(1.,0.706461952521135,1.),(1.,0.707106781186552,1.)))
REPRESENTATION_ITEM('')
SURFACE()
);
#2722=(
BOUNDED_SURFACE()
B_SPLINE_SURFACE(3,2,((#201598,#201599,#201600),(#201601,#201602,#201603),
(#201604,#201605,#201606),(#201607,#201608,#201609)),.UNSPECIFIED.,.F.,
 .F.,.F.)
B_SPLINE_SURFACE_WITH_KNOTS((4,4),(3,3),(0.,0.000397394410828744),(0.,1.),
 .UNSPECIFIED.)
GEOMETRIC_REPRESENTATION_ITEM()
RATIONAL_B_SPLINE_SURFACE(((1.,0.708689770883327,1.),(1.,0.708376440034467,
1.),(1.,0.707750498698417,1.),(1.,0.707106781186553,1.)))
REPRESENTATION_ITEM('')
SURFACE()
);
#2723=(
BOUNDED_SURFACE()
B_SPLINE_SURFACE(3,2,((#201615,#201616,#201617),(#201618,#201619,#201620),
(#201621,#201622,#201623),(#201624,#201625,#201626)),.UNSPECIFIED.,.F.,
 .F.,.F.)
B_SPLINE_SURFACE_WITH_KNOTS((4,4),(3,3),(0.,0.000511815090126171),(0.,1.00105592270426),
 .UNSPECIFIED.)
GEOMETRIC_REPRESENTATION_ITEM()
RATIONAL_B_SPLINE_SURFACE(((1.,0.705266242716881,1.00062243213206),(1.,
0.70558408590855,1.00062176089637),(1.,0.706182089449876,1.00062049800534),
(1.,0.706797508586871,1.00061919833526)))
REPRESENTATION_ITEM('')
SURFACE()
);
#2724=(
BOUNDED_SURFACE()
B_SPLINE_SURFACE(3,2,((#201628,#201629,#201630),(#201631,#201632,#201633),
(#201634,#201635,#201636),(#201637,#201638,#201639)),.UNSPECIFIED.,.F.,
 .F.,.F.)
B_SPLINE_SURFACE_WITH_KNOTS((4,4),(3,3),(0.,0.000397394428086638),(0.,1.),
 .UNSPECIFIED.)
GEOMETRIC_REPRESENTATION_ITEM()
RATIONAL_B_SPLINE_SURFACE(((1.,0.707106781186542,1.),(1.,0.706459846759111,
1.),(1.,0.705820510737245,1.),(1.,0.705498956110775,1.)))
REPRESENTATION_ITEM('')
SURFACE()
);
#2725=(
BOUNDED_SURFACE()
B_SPLINE_SURFACE(3,2,((#201645,#201646,#201647),(#201648,#201649,#201650),
(#201651,#201652,#201653),(#201654,#201655,#201656),(#201657,#201658,#201659),
(#201660,#201661,#201662)),.UNSPECIFIED.,.F.,.F.,.F.)
B_SPLINE_SURFACE_WITH_KNOTS((4,2,4),(3,3),(0.,0.000257953807872846,0.000515907615745693),
(0.,1.),.UNSPECIFIED.)
GEOMETRIC_REPRESENTATION_ITEM()
RATIONAL_B_SPLINE_SURFACE(((1.,0.874619707139392,1.),(1.,0.874834349678654,
1.),(1.,0.854686104158254,1.),(1.,0.792476597914678,1.),(1.,0.750887854595472,
1.),(1.,0.705585838031445,1.)))
REPRESENTATION_ITEM('')
SURFACE()
);
#2726=(
BOUNDED_SURFACE()
B_SPLINE_SURFACE(3,2,((#201668,#201669,#201670),(#201671,#201672,#201673),
(#201674,#201675,#201676),(#201677,#201678,#201679)),.UNSPECIFIED.,.F.,
 .F.,.F.)
B_SPLINE_SURFACE_WITH_KNOTS((4,4),(3,3),(0.,0.000511815437699147),(0.,1.00105881331846),
 .UNSPECIFIED.)
GEOMETRIC_REPRESENTATION_ITEM()
RATIONAL_B_SPLINE_SURFACE(((1.,0.706796661945576,1.0006208951987),(1.,0.707430821224465,
1.00061955228611),(1.,0.708058545829957,1.00061822299977),(1.,0.708394505251969,
1.00061751156315)))
REPRESENTATION_ITEM('')
SURFACE()
);
#2727=(
BOUNDED_SURFACE()
B_SPLINE_SURFACE(3,2,((#201681,#201682,#201683),(#201684,#201685,#201686),
(#201687,#201688,#201689),(#201690,#201691,#201692),(#201693,#201694,#201695),
(#201696,#201697,#201698)),.UNSPECIFIED.,.F.,.F.,.F.)
B_SPLINE_SURFACE_WITH_KNOTS((4,2,4),(3,3),(0.,0.00025691531753127,0.00051383063506254),
(0.,1.),.UNSPECIFIED.)
GEOMETRIC_REPRESENTATION_ITEM()
RATIONAL_B_SPLINE_SURFACE(((1.,0.705585838031441,1.),(1.,0.750902433542855,
1.),(1.,0.792329530082382,1.),(1.,0.854288401594348,1.),(1.,0.874998031125036,
1.),(1.,0.874619707139405,1.)))
REPRESENTATION_ITEM('')
SURFACE()
);
#2728=(
BOUNDED_SURFACE()
B_SPLINE_SURFACE(3,2,((#201704,#201705,#201706),(#201707,#201708,#201709),
(#201710,#201711,#201712),(#201713,#201714,#201715),(#201716,#201717,#201718),
(#201719,#201720,#201721)),.UNSPECIFIED.,.F.,.F.,.F.)
B_SPLINE_SURFACE_WITH_KNOTS((4,2,4),(3,3),(-5.77337656848531E-18,0.000256592814262152,
0.00051318562852431),(0.,1.),.UNSPECIFIED.)
GEOMETRIC_REPRESENTATION_ITEM()
RATIONAL_B_SPLINE_SURFACE(((1.,0.708712527163657,1.),(1.,0.753780902613262,
1.),(1.,0.794538995769635,1.),(1.,0.855070770330661,1.),(1.,0.875018427445639,
1.),(1.,0.874619707139395,1.)))
REPRESENTATION_ITEM('')
SURFACE()
);
#2729=(
BOUNDED_SURFACE()
B_SPLINE_SURFACE(3,2,((#201723,#201724,#201725),(#201726,#201727,#201728),
(#201729,#201730,#201731),(#201732,#201733,#201734)),.UNSPECIFIED.,.F.,
 .F.,.F.)
B_SPLINE_SURFACE_WITH_KNOTS((4,4),(3,3),(0.,0.000511815072430395),(0.,1.00105598366015),
 .UNSPECIFIED.)
GEOMETRIC_REPRESENTATION_ITEM()
RATIONAL_B_SPLINE_SURFACE(((1.,0.706797490733319,1.0006192341178),(1.,0.706182062146218,
1.00062053388286),(1.,0.705584062768601,1.00062179683801),(1.,0.705266224770064,
1.00062246810147)))
REPRESENTATION_ITEM('')
SURFACE()
);
#2730=(
BOUNDED_SURFACE()
B_SPLINE_SURFACE(3,2,((#201740,#201741,#201742),(#201743,#201744,#201745),
(#201746,#201747,#201748),(#201749,#201750,#201751),(#201752,#201753,#201754),
(#201755,#201756,#201757)),.UNSPECIFIED.,.F.,.F.,.F.)
B_SPLINE_SURFACE_WITH_KNOTS((4,2,4),(3,3),(-3.36102673470506E-18,0.000257652232350881,
0.000515304464701766),(0.,1.),.UNSPECIFIED.)
GEOMETRIC_REPRESENTATION_ITEM()
RATIONAL_B_SPLINE_SURFACE(((1.,0.874619707139375,1.),(1.,0.874861180430626,
1.),(1.,0.855455725920945,1.),(1.,0.79469935895517,1.),(1.,0.753768977788711,
1.),(1.,0.708712527163638,1.)))
REPRESENTATION_ITEM('')
SURFACE()
);
#2731=(
BOUNDED_SURFACE()
B_SPLINE_SURFACE(3,2,((#201763,#201764,#201765),(#201766,#201767,#201768),
(#201769,#201770,#201771),(#201772,#201773,#201774)),.UNSPECIFIED.,.F.,
 .F.,.F.)
B_SPLINE_SURFACE_WITH_KNOTS((4,4),(3,3),(0.,0.000397394373651913),(0.,1.),
 .UNSPECIFIED.)
GEOMETRIC_REPRESENTATION_ITEM()
RATIONAL_B_SPLINE_SURFACE(((1.,0.707106781186548,1.),(1.,0.707752587915885,
1.),(1.,0.708377654540686,1.),(1.,0.708689770883335,1.)))
REPRESENTATION_ITEM('')
SURFACE()
);
#2732=(
BOUNDED_SURFACE()
B_SPLINE_SURFACE(3,2,((#201776,#201777,#201778),(#201779,#201780,#201781),
(#201782,#201783,#201784),(#201785,#201786,#201787)),.UNSPECIFIED.,.F.,
 .F.,.F.)
B_SPLINE_SURFACE_WITH_KNOTS((4,4),(3,3),(0.,0.000511815456479783),(0.,1.00105873160181),
 .UNSPECIFIED.)
GEOMETRIC_REPRESENTATION_ITEM()
RATIONAL_B_SPLINE_SURFACE(((1.,0.708394529055794,1.0006174638547),(1.,0.708058564166318,
1.00061817524799),(1.,0.707430835371533,1.00061950444062),(1.,0.706796685879833,
1.00062084722883)))
REPRESENTATION_ITEM('')
SURFACE()
);
#2733=(
BOUNDED_SURFACE()
B_SPLINE_SURFACE(3,2,((#201793,#201794,#201795),(#201796,#201797,#201798),
(#201799,#201800,#201801),(#201802,#201803,#201804)),.UNSPECIFIED.,.F.,
 .F.,.F.)
B_SPLINE_SURFACE_WITH_KNOTS((4,4),(3,3),(0.,0.000397394465448324),(0.,1.),
 .UNSPECIFIED.)
GEOMETRIC_REPRESENTATION_ITEM()
RATIONAL_B_SPLINE_SURFACE(((1.,0.705498956110748,1.),(1.,0.70582176481177,
1.),(1.,0.706461952521139,1.),(1.,0.707106781186553,1.)))
REPRESENTATION_ITEM('')
SURFACE()
);
#2734=(
BOUNDED_SURFACE()
B_SPLINE_SURFACE(3,2,((#201810,#201811,#201812),(#201813,#201814,#201815),
(#201816,#201817,#201818),(#201819,#201820,#201821)),.UNSPECIFIED.,.F.,
 .F.,.F.)
B_SPLINE_SURFACE_WITH_KNOTS((4,4),(3,3),(0.,0.000397394410828724),(0.,1.),
 .UNSPECIFIED.)
GEOMETRIC_REPRESENTATION_ITEM()
RATIONAL_B_SPLINE_SURFACE(((1.,0.708689770883328,1.),(1.,0.708376440034509,
1.),(1.,0.707750498698382,1.),(1.,0.707106781186548,1.)))
REPRESENTATION_ITEM('')
SURFACE()
);
#2735=(
BOUNDED_SURFACE()
B_SPLINE_SURFACE(3,2,((#201827,#201828,#201829),(#201830,#201831,#201832),
(#201833,#201834,#201835),(#201836,#201837,#201838)),.UNSPECIFIED.,.F.,
 .F.,.F.)
B_SPLINE_SURFACE_WITH_KNOTS((4,4),(3,3),(0.,0.000511815090126181),(0.,1.00105592270307),
 .UNSPECIFIED.)
GEOMETRIC_REPRESENTATION_ITEM()
RATIONAL_B_SPLINE_SURFACE(((1.,0.70526624271723,1.00062243213135),(1.,0.705584085908917,
1.00062176089567),(1.,0.706182089450198,1.00062049800464),(1.,0.706797508587235,
1.00061919833456)))
REPRESENTATION_ITEM('')
SURFACE()
);
#2736=(
BOUNDED_SURFACE()
B_SPLINE_SURFACE(3,2,((#201840,#201841,#201842),(#201843,#201844,#201845),
(#201846,#201847,#201848),(#201849,#201850,#201851)),.UNSPECIFIED.,.F.,
 .F.,.F.)
B_SPLINE_SURFACE_WITH_KNOTS((4,4),(3,3),(0.,0.000397394428086613),(0.,1.),
 .UNSPECIFIED.)
GEOMETRIC_REPRESENTATION_ITEM()
RATIONAL_B_SPLINE_SURFACE(((1.,0.707106781186548,1.),(1.,0.706459846759089,
1.),(1.,0.70582051073727,1.),(1.,0.705498956110753,1.)))
REPRESENTATION_ITEM('')
SURFACE()
);
#2737=(
BOUNDED_SURFACE()
B_SPLINE_SURFACE(3,2,((#201857,#201858,#201859),(#201860,#201861,#201862),
(#201863,#201864,#201865),(#201866,#201867,#201868),(#201869,#201870,#201871),
(#201872,#201873,#201874)),.UNSPECIFIED.,.F.,.F.,.F.)
B_SPLINE_SURFACE_WITH_KNOTS((4,2,4),(3,3),(0.,0.000257953807872844,0.000515907615745687),
(0.,1.),.UNSPECIFIED.)
GEOMETRIC_REPRESENTATION_ITEM()
RATIONAL_B_SPLINE_SURFACE(((1.,0.874619707139387,1.),(1.,0.874834349679082,
1.),(1.,0.854686104157689,1.),(1.,0.792476597915248,1.),(1.,0.750887854595037,
1.),(1.,0.70558583803144,1.)))
REPRESENTATION_ITEM('')
SURFACE()
);
#2738=(
BOUNDED_SURFACE()
B_SPLINE_SURFACE(3,2,((#201880,#201881,#201882),(#201883,#201884,#201885),
(#201886,#201887,#201888),(#201889,#201890,#201891)),.UNSPECIFIED.,.F.,
 .F.,.F.)
B_SPLINE_SURFACE_WITH_KNOTS((4,4),(3,3),(0.,0.000511815437699158),(0.,1.00105881331624),
 .UNSPECIFIED.)
GEOMETRIC_REPRESENTATION_ITEM()
RATIONAL_B_SPLINE_SURFACE(((1.,0.706796661946222,1.0006208951974),(1.,0.707430821225124,
1.00061955228482),(1.,0.708058545830611,1.00061822299848),(1.,0.708394505252608,
1.00061751156186)))
REPRESENTATION_ITEM('')
SURFACE()
);
#2739=(
BOUNDED_SURFACE()
B_SPLINE_SURFACE(3,2,((#201893,#201894,#201895),(#201896,#201897,#201898),
(#201899,#201900,#201901),(#201902,#201903,#201904),(#201905,#201906,#201907),
(#201908,#201909,#201910)),.UNSPECIFIED.,.F.,.F.,.F.)
B_SPLINE_SURFACE_WITH_KNOTS((4,2,4),(3,3),(0.,0.00025691531753126,0.00051383063506252),
(0.,1.),.UNSPECIFIED.)
GEOMETRIC_REPRESENTATION_ITEM()
RATIONAL_B_SPLINE_SURFACE(((1.,0.705585838031443,1.),(1.,0.750902433542485,
1.),(1.,0.792329530082859,1.),(1.,0.854288401593878,1.),(1.,0.874998031125374,
1.),(1.,0.874619707139411,1.)))
REPRESENTATION_ITEM('')
SURFACE()
);
#2740=(
BOUNDED_SURFACE()
B_SPLINE_SURFACE(3,2,((#201916,#201917,#201918),(#201919,#201920,#201921),
(#201922,#201923,#201924),(#201925,#201926,#201927),(#201928,#201929,#201930),
(#201931,#201932,#201933)),.UNSPECIFIED.,.F.,.F.,.F.)
B_SPLINE_SURFACE_WITH_KNOTS((4,2,4),(3,3),(0.,0.000256592814262158,0.000513185628524317),
(0.,1.),.UNSPECIFIED.)
GEOMETRIC_REPRESENTATION_ITEM()
RATIONAL_B_SPLINE_SURFACE(((1.,0.708712527163662,1.),(1.,0.753780902613653,
1.),(1.,0.794538995769098,1.),(1.,0.855070770331221,1.),(1.,0.875018427445238,
1.),(1.,0.874619707139383,1.)))
REPRESENTATION_ITEM('')
SURFACE()
);
#2741=(
BOUNDED_SURFACE()
B_SPLINE_SURFACE(3,2,((#201935,#201936,#201937),(#201938,#201939,#201940),
(#201941,#201942,#201943),(#201944,#201945,#201946)),.UNSPECIFIED.,.F.,
 .F.,.F.)
B_SPLINE_SURFACE_WITH_KNOTS((4,4),(3,3),(2.71050543121376E-20,0.000511815072430396),
(0.,1.00105598366068),.UNSPECIFIED.)
GEOMETRIC_REPRESENTATION_ITEM()
RATIONAL_B_SPLINE_SURFACE(((1.,0.706797490733148,1.00061923411811),(1.,
0.706182062146073,1.00062053388318),(1.,0.705584062768447,1.00062179683832),
(1.,0.705266224769915,1.00062246810179)))
REPRESENTATION_ITEM('')
SURFACE()
);
#2742=(
BOUNDED_SURFACE()
B_SPLINE_SURFACE(3,2,((#201952,#201953,#201954),(#201955,#201956,#201957),
(#201958,#201959,#201960),(#201961,#201962,#201963),(#201964,#201965,#201966),
(#201967,#201968,#201969)),.UNSPECIFIED.,.F.,.F.,.F.)
B_SPLINE_SURFACE_WITH_KNOTS((4,2,4),(3,3),(0.,0.000257652232350886,0.000515304464701772),
(0.,1.),.UNSPECIFIED.)
GEOMETRIC_REPRESENTATION_ITEM()
RATIONAL_B_SPLINE_SURFACE(((1.,0.87461970713939,1.),(1.,0.874861180430661,
1.),(1.,0.855455725920899,1.),(1.,0.794699358955201,1.),(1.,0.753768977788728,
1.),(1.,0.708712527163643,1.)))
REPRESENTATION_ITEM('')
SURFACE()
);
#2743=(
BOUNDED_SURFACE()
B_SPLINE_SURFACE(3,2,((#201975,#201976,#201977),(#201978,#201979,#201980),
(#201981,#201982,#201983),(#201984,#201985,#201986)),.UNSPECIFIED.,.F.,
 .F.,.F.)
B_SPLINE_SURFACE_WITH_KNOTS((4,4),(3,3),(0.,0.000397394373651917),(0.,1.),
 .UNSPECIFIED.)
GEOMETRIC_REPRESENTATION_ITEM()
RATIONAL_B_SPLINE_SURFACE(((1.,0.707106781186548,1.),(1.,0.70775258791592,
1.),(1.,0.708377654540679,1.),(1.,0.708689770883336,1.)))
REPRESENTATION_ITEM('')
SURFACE()
);
#2744=(
BOUNDED_SURFACE()
B_SPLINE_SURFACE(3,2,((#201988,#201989,#201990),(#201991,#201992,#201993),
(#201994,#201995,#201996),(#201997,#201998,#201999)),.UNSPECIFIED.,.F.,
 .F.,.F.)
B_SPLINE_SURFACE_WITH_KNOTS((4,4),(3,3),(0.,0.000511815456479786),(0.,1.00105873160188),
 .UNSPECIFIED.)
GEOMETRIC_REPRESENTATION_ITEM()
RATIONAL_B_SPLINE_SURFACE(((1.,0.708394529055777,1.00061746385474),(1.,
0.708058564166309,1.00061817524803),(1.,0.707430835371485,1.00061950444066),
(1.,0.706796685879812,1.00062084722887)))
REPRESENTATION_ITEM('')
SURFACE()
);
#2745=(
BOUNDED_SURFACE()
B_SPLINE_SURFACE(3,2,((#202005,#202006,#202007),(#202008,#202009,#202010),
(#202011,#202012,#202013),(#202014,#202015,#202016)),.UNSPECIFIED.,.F.,
 .F.,.F.)
B_SPLINE_SURFACE_WITH_KNOTS((4,4),(3,3),(0.,0.000397394465448299),(0.,1.),
 .UNSPECIFIED.)
GEOMETRIC_REPRESENTATION_ITEM()
RATIONAL_B_SPLINE_SURFACE(((1.,0.70549895611075,1.),(1.,0.705821764811771,
1.),(1.,0.70646195252116,1.),(1.,0.707106781186548,1.)))
REPRESENTATION_ITEM('')
SURFACE()
);
#2746=(
BOUNDED_SURFACE()
B_SPLINE_SURFACE(3,2,((#202022,#202023,#202024),(#202025,#202026,#202027),
(#202028,#202029,#202030),(#202031,#202032,#202033)),.UNSPECIFIED.,.F.,
 .F.,.F.)
B_SPLINE_SURFACE_WITH_KNOTS((4,4),(3,3),(0.,0.000397394410828727),(0.,1.),
 .UNSPECIFIED.)
GEOMETRIC_REPRESENTATION_ITEM()
RATIONAL_B_SPLINE_SURFACE(((1.,0.708689770883334,1.),(1.,0.708376440034467,
1.),(1.,0.707750498698424,1.),(1.,0.707106781186538,1.)))
REPRESENTATION_ITEM('')
SURFACE()
);
#2747=(
BOUNDED_SURFACE()
B_SPLINE_SURFACE(3,2,((#202039,#202040,#202041),(#202042,#202043,#202044),
(#202045,#202046,#202047),(#202048,#202049,#202050)),.UNSPECIFIED.,.F.,
 .F.,.F.)
B_SPLINE_SURFACE_WITH_KNOTS((4,4),(3,3),(0.,0.000511815090126184),(0.,1.00105592270359),
 .UNSPECIFIED.)
GEOMETRIC_REPRESENTATION_ITEM()
RATIONAL_B_SPLINE_SURFACE(((1.,0.705266242717073,1.00062243213166),(1.,
0.70558408590872,1.00062176089597),(1.,0.706182089450093,1.00062049800494),
(1.,0.706797508587065,1.00061919833486)))
REPRESENTATION_ITEM('')
SURFACE()
);
#2748=(
BOUNDED_SURFACE()
B_SPLINE_SURFACE(3,2,((#202052,#202053,#202054),(#202055,#202056,#202057),
(#202058,#202059,#202060),(#202061,#202062,#202063)),.UNSPECIFIED.,.F.,
 .F.,.F.)
B_SPLINE_SURFACE_WITH_KNOTS((4,4),(3,3),(0.,0.00039739442808662),(0.,1.),
 .UNSPECIFIED.)
GEOMETRIC_REPRESENTATION_ITEM()
RATIONAL_B_SPLINE_SURFACE(((1.,0.707106781186548,1.),(1.,0.706459846759105,
1.),(1.,0.705820510737281,1.),(1.,0.705498956110749,1.)))
REPRESENTATION_ITEM('')
SURFACE()
);
#2749=(
BOUNDED_SURFACE()
B_SPLINE_SURFACE(3,2,((#202069,#202070,#202071),(#202072,#202073,#202074),
(#202075,#202076,#202077),(#202078,#202079,#202080),(#202081,#202082,#202083),
(#202084,#202085,#202086)),.UNSPECIFIED.,.F.,.F.,.F.)
B_SPLINE_SURFACE_WITH_KNOTS((4,2,4),(3,3),(0.,0.000257953807872843,0.000515907615745687),
(0.,1.),.UNSPECIFIED.)
GEOMETRIC_REPRESENTATION_ITEM()
RATIONAL_B_SPLINE_SURFACE(((1.,0.874619707139391,1.),(1.,0.874834349679335,
1.),(1.,0.854686104157323,1.),(1.,0.792476597915613,1.),(1.,0.750887854594751,
1.),(1.,0.705585838031461,1.)))
REPRESENTATION_ITEM('')
SURFACE()
);
#2750=(
BOUNDED_SURFACE()
B_SPLINE_SURFACE(3,2,((#202092,#202093,#202094),(#202095,#202096,#202097),
(#202098,#202099,#202100),(#202101,#202102,#202103)),.UNSPECIFIED.,.F.,
 .F.,.F.)
B_SPLINE_SURFACE_WITH_KNOTS((4,4),(3,3),(0.,0.000511815437699148),(0.,1.00105881332022),
 .UNSPECIFIED.)
GEOMETRIC_REPRESENTATION_ITEM()
RATIONAL_B_SPLINE_SURFACE(((1.,0.706796661945066,1.00062089519973),(1.,
0.707430821223953,1.00061955228715),(1.,0.708058545829438,1.0006182230008),
(1.,0.70839450525146,1.00061751156418)))
REPRESENTATION_ITEM('')
SURFACE()
);
#2751=(
BOUNDED_SURFACE()
B_SPLINE_SURFACE(3,2,((#202105,#202106,#202107),(#202108,#202109,#202110),
(#202111,#202112,#202113),(#202114,#202115,#202116),(#202117,#202118,#202119),
(#202120,#202121,#202122)),.UNSPECIFIED.,.F.,.F.,.F.)
B_SPLINE_SURFACE_WITH_KNOTS((4,2,4),(3,3),(0.,0.00025691531753126,0.00051383063506252),
(0.,1.),.UNSPECIFIED.)
GEOMETRIC_REPRESENTATION_ITEM()
RATIONAL_B_SPLINE_SURFACE(((1.,0.705585838031456,1.),(1.,0.750902433542557,
1.),(1.,0.792329530082758,1.),(1.,0.854288401593967,1.),(1.,0.874998031125322,
1.),(1.,0.874619707139389,1.)))
REPRESENTATION_ITEM('')
SURFACE()
);
#2752=(
BOUNDED_SURFACE()
B_SPLINE_SURFACE(3,2,((#202128,#202129,#202130),(#202131,#202132,#202133),
(#202134,#202135,#202136),(#202137,#202138,#202139),(#202140,#202141,#202142),
(#202143,#202144,#202145)),.UNSPECIFIED.,.F.,.F.,.F.)
B_SPLINE_SURFACE_WITH_KNOTS((4,2,4),(3,3),(0.,0.000256592814262157,0.000513185628524313),
(0.,1.),.UNSPECIFIED.)
GEOMETRIC_REPRESENTATION_ITEM()
RATIONAL_B_SPLINE_SURFACE(((1.,0.708712527163664,1.),(1.,0.753780902613438,
1.),(1.,0.794538995769409,1.),(1.,0.855070770330893,1.),(1.,0.87501842744548,
1.),(1.,0.874619707139388,1.)))
REPRESENTATION_ITEM('')
SURFACE()
);
#2753=(
BOUNDED_SURFACE()
B_SPLINE_SURFACE(3,2,((#202147,#202148,#202149),(#202150,#202151,#202152),
(#202153,#202154,#202155),(#202156,#202157,#202158)),.UNSPECIFIED.,.F.,
 .F.,.F.)
B_SPLINE_SURFACE_WITH_KNOTS((4,4),(3,3),(0.,0.000511815072430396),(0.,1.001055983657),
 .UNSPECIFIED.)
GEOMETRIC_REPRESENTATION_ITEM()
RATIONAL_B_SPLINE_SURFACE(((1.,0.706797490734233,1.00061923411595),(1.,
0.706182062147162,1.00062053388101),(1.,0.705584062769501,1.00062179683615),
(1.,0.705266224770988,1.00062246809962)))
REPRESENTATION_ITEM('')
SURFACE()
);
#2754=(
BOUNDED_SURFACE()
B_SPLINE_SURFACE(3,2,((#202164,#202165,#202166),(#202167,#202168,#202169),
(#202170,#202171,#202172),(#202173,#202174,#202175),(#202176,#202177,#202178),
(#202179,#202180,#202181)),.UNSPECIFIED.,.F.,.F.,.F.)
B_SPLINE_SURFACE_WITH_KNOTS((4,2,4),(3,3),(-3.10352871873976E-18,0.00025765223235088,
0.000515304464701763),(0.,1.),.UNSPECIFIED.)
GEOMETRIC_REPRESENTATION_ITEM()
RATIONAL_B_SPLINE_SURFACE(((1.,0.874619707139394,1.),(1.,0.874861180430981,
1.),(1.,0.855455725920473,1.),(1.,0.794699358955668,1.),(1.,0.753768977788342,
1.),(1.,0.708712527163659,1.)))
REPRESENTATION_ITEM('')
SURFACE()
);
#2755=(
BOUNDED_SURFACE()
B_SPLINE_SURFACE(3,2,((#202187,#202188,#202189),(#202190,#202191,#202192),
(#202193,#202194,#202195),(#202196,#202197,#202198)),.UNSPECIFIED.,.F.,
 .F.,.F.)
B_SPLINE_SURFACE_WITH_KNOTS((4,4),(3,3),(2.71050543121376E-20,0.000397394373651914),
(0.,1.),.UNSPECIFIED.)
GEOMETRIC_REPRESENTATION_ITEM()
RATIONAL_B_SPLINE_SURFACE(((1.,0.707106781186538,1.),(1.,0.707752587915903,
1.),(1.,0.708377654540675,1.),(1.,0.708689770883326,1.)))
REPRESENTATION_ITEM('')
SURFACE()
);
#2756=(
BOUNDED_SURFACE()
B_SPLINE_SURFACE(3,2,((#202200,#202201,#202202),(#202203,#202204,#202205),
(#202206,#202207,#202208),(#202209,#202210,#202211)),.UNSPECIFIED.,.F.,
 .F.,.F.)
B_SPLINE_SURFACE_WITH_KNOTS((4,4),(3,3),(0.,0.000511815456479788),(0.,1.00105873159876),
 .UNSPECIFIED.)
GEOMETRIC_REPRESENTATION_ITEM()
RATIONAL_B_SPLINE_SURFACE(((1.,0.708394529056676,1.00061746385292),(1.,
0.708058564167226,1.00061817524621),(1.,0.707430835372413,1.00061950443883),
(1.,0.706796685880726,1.00062084722704)))
REPRESENTATION_ITEM('')
SURFACE()
);
#2757=(
BOUNDED_SURFACE()
B_SPLINE_SURFACE(3,2,((#202217,#202218,#202219),(#202220,#202221,#202222),
(#202223,#202224,#202225),(#202226,#202227,#202228)),.UNSPECIFIED.,.F.,
 .F.,.F.)
B_SPLINE_SURFACE_WITH_KNOTS((4,4),(3,3),(0.,0.000397394465448322),(0.,1.),
 .UNSPECIFIED.)
GEOMETRIC_REPRESENTATION_ITEM()
RATIONAL_B_SPLINE_SURFACE(((1.,0.705498956110748,1.),(1.,0.705821764811803,
1.),(1.,0.706461952521134,1.),(1.,0.707106781186529,1.)))
REPRESENTATION_ITEM('')
SURFACE()
);
#2758=(
BOUNDED_SURFACE()
B_SPLINE_SURFACE(3,2,((#202234,#202235,#202236),(#202237,#202238,#202239),
(#202240,#202241,#202242),(#202243,#202244,#202245)),.UNSPECIFIED.,.F.,
 .F.,.F.)
B_SPLINE_SURFACE_WITH_KNOTS((4,4),(3,3),(0.,0.00039739441082874),(0.,1.),
 .UNSPECIFIED.)
GEOMETRIC_REPRESENTATION_ITEM()
RATIONAL_B_SPLINE_SURFACE(((1.,0.708689770883322,1.),(1.,0.708376440034495,
1.),(1.,0.707750498698404,1.),(1.,0.707106781186548,1.)))
REPRESENTATION_ITEM('')
SURFACE()
);
#2759=(
BOUNDED_SURFACE()
B_SPLINE_SURFACE(3,2,((#202251,#202252,#202253),(#202254,#202255,#202256),
(#202257,#202258,#202259),(#202260,#202261,#202262)),.UNSPECIFIED.,.F.,
 .F.,.F.)
B_SPLINE_SURFACE_WITH_KNOTS((4,4),(3,3),(0.,0.000511815090126184),(0.,1.00105592270412),
 .UNSPECIFIED.)
GEOMETRIC_REPRESENTATION_ITEM()
RATIONAL_B_SPLINE_SURFACE(((1.,0.705266242716956,1.00062243213197),(1.,
0.705584085908522,1.00062176089629),(1.,0.706182089449954,1.00062049800525),
(1.,0.706797508586919,1.00061919833518)))
REPRESENTATION_ITEM('')
SURFACE()
);
#2760=(
BOUNDED_SURFACE()
B_SPLINE_SURFACE(3,2,((#202264,#202265,#202266),(#202267,#202268,#202269),
(#202270,#202271,#202272),(#202273,#202274,#202275)),.UNSPECIFIED.,.F.,
 .F.,.F.)
B_SPLINE_SURFACE_WITH_KNOTS((4,4),(3,3),(0.,0.000397394428086625),(0.,1.),
 .UNSPECIFIED.)
GEOMETRIC_REPRESENTATION_ITEM()
RATIONAL_B_SPLINE_SURFACE(((1.,0.707106781186548,1.),(1.,0.706459846759129,
1.),(1.,0.705820510737238,1.),(1.,0.705498956110761,1.)))
REPRESENTATION_ITEM('')
SURFACE()
);
#2761=(
BOUNDED_SURFACE()
B_SPLINE_SURFACE(3,2,((#202281,#202282,#202283),(#202284,#202285,#202286),
(#202287,#202288,#202289),(#202290,#202291,#202292),(#202293,#202294,#202295),
(#202296,#202297,#202298)),.UNSPECIFIED.,.F.,.F.,.F.)
B_SPLINE_SURFACE_WITH_KNOTS((4,2,4),(3,3),(0.,0.000257953807872846,0.000515907615745692),
(0.,1.),.UNSPECIFIED.)
GEOMETRIC_REPRESENTATION_ITEM()
RATIONAL_B_SPLINE_SURFACE(((1.,0.874619707139389,1.),(1.,0.874834349678646,
1.),(1.,0.854686104158268,1.),(1.,0.792476597914672,1.),(1.,0.75088785459547,
1.),(1.,0.705585838031423,1.)))
REPRESENTATION_ITEM('')
SURFACE()
);
#2762=(
BOUNDED_SURFACE()
B_SPLINE_SURFACE(3,2,((#202304,#202305,#202306),(#202307,#202308,#202309),
(#202310,#202311,#202312),(#202313,#202314,#202315)),.UNSPECIFIED.,.F.,
 .F.,.F.)
B_SPLINE_SURFACE_WITH_KNOTS((4,4),(3,3),(0.,0.000511815437699156),(0.,1.00105881331674),
 .UNSPECIFIED.)
GEOMETRIC_REPRESENTATION_ITEM()
RATIONAL_B_SPLINE_SURFACE(((1.,0.706796661946085,1.00062089519769),(1.,
0.707430821224981,1.00061955228511),(1.,0.708058545830442,1.00061822299877),
(1.,0.708394505252468,1.00061751156215)))
REPRESENTATION_ITEM('')
SURFACE()
);
#2763=(
BOUNDED_SURFACE()
B_SPLINE_SURFACE(3,2,((#202317,#202318,#202319),(#202320,#202321,#202322),
(#202323,#202324,#202325),(#202326,#202327,#202328),(#202329,#202330,#202331),
(#202332,#202333,#202334)),.UNSPECIFIED.,.F.,.F.,.F.)
B_SPLINE_SURFACE_WITH_KNOTS((4,2,4),(3,3),(2.71050543121376E-20,0.000256915317531266,
0.000513830635062532),(0.,1.),.UNSPECIFIED.)
GEOMETRIC_REPRESENTATION_ITEM()
RATIONAL_B_SPLINE_SURFACE(((1.,0.705585838031446,1.),(1.,0.750902433542212,
1.),(1.,0.792329530083219,1.),(1.,0.854288401593528,1.),(1.,0.874998031125645,
1.),(1.,0.874619707139392,1.)))
REPRESENTATION_ITEM('')
SURFACE()
);
#2764=(
BOUNDED_SURFACE()
B_SPLINE_SURFACE(3,2,((#202340,#202341,#202342),(#202343,#202344,#202345),
(#202346,#202347,#202348),(#202349,#202350,#202351),(#202352,#202353,#202354),
(#202355,#202356,#202357)),.UNSPECIFIED.,.F.,.F.,.F.)
B_SPLINE_SURFACE_WITH_KNOTS((4,2,4),(3,3),(-9.48676900924816E-18,0.000256592814262154,
0.000513185628524318),(0.,1.),.UNSPECIFIED.)
GEOMETRIC_REPRESENTATION_ITEM()
RATIONAL_B_SPLINE_SURFACE(((1.,0.708712527163665,1.),(1.,0.753780902613422,
1.),(1.,0.794538995769426,1.),(1.,0.855070770330873,1.),(1.,0.875018427445491,
1.),(1.,0.874619707139392,1.)))
REPRESENTATION_ITEM('')
SURFACE()
);
#2765=(
BOUNDED_SURFACE()
B_SPLINE_SURFACE(3,2,((#202359,#202360,#202361),(#202362,#202363,#202364),
(#202365,#202366,#202367),(#202368,#202369,#202370)),.UNSPECIFIED.,.F.,
 .F.,.F.)
B_SPLINE_SURFACE_WITH_KNOTS((4,4),(3,3),(0.,0.000511815072430408),(0.,1.0010559836591),
 .UNSPECIFIED.)
GEOMETRIC_REPRESENTATION_ITEM()
RATIONAL_B_SPLINE_SURFACE(((1.,0.70679749073362,1.00061923411718),(1.,0.706182062146524,
1.00062053388225),(1.,0.705584062768913,1.00062179683739),(1.,0.705266224770364,
1.00062246810085)))
REPRESENTATION_ITEM('')
SURFACE()
);
#2766=(
BOUNDED_SURFACE()
B_SPLINE_SURFACE(3,2,((#202376,#202377,#202378),(#202379,#202380,#202381),
(#202382,#202383,#202384),(#202385,#202386,#202387),(#202388,#202389,#202390),
(#202391,#202392,#202393)),.UNSPECIFIED.,.F.,.F.,.F.)
B_SPLINE_SURFACE_WITH_KNOTS((4,2,4),(3,3),(-9.40545384631175E-18,0.000257652232350876,
0.000515304464701762),(0.,1.),.UNSPECIFIED.)
GEOMETRIC_REPRESENTATION_ITEM()
RATIONAL_B_SPLINE_SURFACE(((1.,0.874619707139393,1.),(1.,0.874861180430243,
1.),(1.,0.855455725921459,1.),(1.,0.794699358954658,1.),(1.,0.753768977789092,
1.),(1.,0.70871252716366,1.)))
REPRESENTATION_ITEM('')
SURFACE()
);
#2767=(
BOUNDED_SURFACE()
B_SPLINE_SURFACE(3,2,((#202399,#202400,#202401),(#202402,#202403,#202404),
(#202405,#202406,#202407),(#202408,#202409,#202410)),.UNSPECIFIED.,.F.,
 .F.,.F.)
B_SPLINE_SURFACE_WITH_KNOTS((4,4),(3,3),(0.,0.000397394373651906),(0.,1.),
 .UNSPECIFIED.)
GEOMETRIC_REPRESENTATION_ITEM()
RATIONAL_B_SPLINE_SURFACE(((1.,0.707106781186548,1.),(1.,0.707752587915919,
1.),(1.,0.708377654540692,1.),(1.,0.708689770883306,1.)))
REPRESENTATION_ITEM('')
SURFACE()
);
#2768=(
BOUNDED_SURFACE()
B_SPLINE_SURFACE(3,2,((#202412,#202413,#202414),(#202415,#202416,#202417),
(#202418,#202419,#202420),(#202421,#202422,#202423)),.UNSPECIFIED.,.F.,
 .F.,.F.)
B_SPLINE_SURFACE_WITH_KNOTS((4,4),(3,3),(0.,0.000511815456479793),(0.,1.00105873159685),
 .UNSPECIFIED.)
GEOMETRIC_REPRESENTATION_ITEM()
RATIONAL_B_SPLINE_SURFACE(((1.,0.708394529057236,1.00061746385181),(1.,
0.708058564167794,1.00061817524509),(1.,0.707430835372963,1.00061950443771),
(1.,0.706796685881285,1.00062084722592)))
REPRESENTATION_ITEM('')
SURFACE()
);
#2769=(
BOUNDED_SURFACE()
B_SPLINE_SURFACE(3,2,((#202429,#202430,#202431),(#202432,#202433,#202434),
(#202435,#202436,#202437),(#202438,#202439,#202440)),.UNSPECIFIED.,.F.,
 .F.,.F.)
B_SPLINE_SURFACE_WITH_KNOTS((4,4),(3,3),(0.,0.000397394465448306),(0.,1.),
 .UNSPECIFIED.)
GEOMETRIC_REPRESENTATION_ITEM()
RATIONAL_B_SPLINE_SURFACE(((1.,0.705498956110745,1.),(1.,0.705821764811741,
1.),(1.,0.706461952521179,1.),(1.,0.707106781186536,1.)))
REPRESENTATION_ITEM('')
SURFACE()
);
#2770=(
BOUNDED_SURFACE()
B_SPLINE_SURFACE(3,2,((#202446,#202447,#202448),(#202449,#202450,#202451),
(#202452,#202453,#202454),(#202455,#202456,#202457)),.UNSPECIFIED.,.F.,
 .F.,.F.)
B_SPLINE_SURFACE_WITH_KNOTS((4,4),(3,3),(0.,0.00039739441082874),(0.,1.),
 .UNSPECIFIED.)
GEOMETRIC_REPRESENTATION_ITEM()
RATIONAL_B_SPLINE_SURFACE(((1.,0.708689770883326,1.),(1.,0.70837644003451,
1.),(1.,0.707750498698405,1.),(1.,0.707106781186548,1.)))
REPRESENTATION_ITEM('')
SURFACE()
);
#2771=(
BOUNDED_SURFACE()
B_SPLINE_SURFACE(3,2,((#202463,#202464,#202465),(#202466,#202467,#202468),
(#202469,#202470,#202471),(#202472,#202473,#202474)),.UNSPECIFIED.,.F.,
 .F.,.F.)
B_SPLINE_SURFACE_WITH_KNOTS((4,4),(3,3),(0.,0.000511815090126171),(0.,1.00105592270468),
 .UNSPECIFIED.)
GEOMETRIC_REPRESENTATION_ITEM()
RATIONAL_B_SPLINE_SURFACE(((1.,0.705266242716756,1.0006224321323),(1.,0.705584085908405,
1.00062176089661),(1.,0.706182089449784,1.00062049800558),(1.,0.706797508586757,
1.0006191983355)))
REPRESENTATION_ITEM('')
SURFACE()
);
#2772=(
BOUNDED_SURFACE()
B_SPLINE_SURFACE(3,2,((#202476,#202477,#202478),(#202479,#202480,#202481),
(#202482,#202483,#202484),(#202485,#202486,#202487)),.UNSPECIFIED.,.F.,
 .F.,.F.)
B_SPLINE_SURFACE_WITH_KNOTS((4,4),(3,3),(0.,0.000397394428086624),(0.,1.),
 .UNSPECIFIED.)
GEOMETRIC_REPRESENTATION_ITEM()
RATIONAL_B_SPLINE_SURFACE(((1.,0.707106781186548,1.),(1.,0.706459846759088,
1.),(1.,0.705820510737271,1.),(1.,0.705498956110742,1.)))
REPRESENTATION_ITEM('')
SURFACE()
);
#2773=(
BOUNDED_SURFACE()
B_SPLINE_SURFACE(3,2,((#202493,#202494,#202495),(#202496,#202497,#202498),
(#202499,#202500,#202501),(#202502,#202503,#202504),(#202505,#202506,#202507),
(#202508,#202509,#202510)),.UNSPECIFIED.,.F.,.F.,.F.)
B_SPLINE_SURFACE_WITH_KNOTS((4,2,4),(3,3),(0.,0.000257953807872849,0.000515907615745697),
(0.,1.),.UNSPECIFIED.)
GEOMETRIC_REPRESENTATION_ITEM()
RATIONAL_B_SPLINE_SURFACE(((1.,0.874619707139387,1.),(1.,0.874834349678404,
1.),(1.,0.854686104158593,1.),(1.,0.792476597914305,1.),(1.,0.750887854595777,
1.),(1.,0.705585838031401,1.)))
REPRESENTATION_ITEM('')
SURFACE()
);
#2774=(
BOUNDED_SURFACE()
B_SPLINE_SURFACE(3,2,((#202516,#202517,#202518),(#202519,#202520,#202521),
(#202522,#202523,#202524),(#202525,#202526,#202527)),.UNSPECIFIED.,.F.,
 .F.,.F.)
B_SPLINE_SURFACE_WITH_KNOTS((4,4),(3,3),(0.,0.000511815437699148),(0.,1.00105881331846),
 .UNSPECIFIED.)
GEOMETRIC_REPRESENTATION_ITEM()
RATIONAL_B_SPLINE_SURFACE(((1.,0.706796661945569,1.0006208951987),(1.,0.707430821224488,
1.00061955228611),(1.,0.708058545829957,1.00061822299977),(1.,0.708394505251976,
1.00061751156315)))
REPRESENTATION_ITEM('')
SURFACE()
);
#2775=(
BOUNDED_SURFACE()
B_SPLINE_SURFACE(3,2,((#202529,#202530,#202531),(#202532,#202533,#202534),
(#202535,#202536,#202537),(#202538,#202539,#202540),(#202541,#202542,#202543),
(#202544,#202545,#202546)),.UNSPECIFIED.,.F.,.F.,.F.)
B_SPLINE_SURFACE_WITH_KNOTS((4,2,4),(3,3),(0.,0.000256915317531259,0.000513830635062517),
(0.,1.),.UNSPECIFIED.)
GEOMETRIC_REPRESENTATION_ITEM()
RATIONAL_B_SPLINE_SURFACE(((1.,0.705585838031447,1.),(1.,0.750902433543016,
1.),(1.,0.792329530082168,1.),(1.,0.854288401594543,1.),(1.,0.874998031124862,
1.),(1.,0.874619707139394,1.)))
REPRESENTATION_ITEM('')
SURFACE()
);
#2776=(
BOUNDED_SURFACE()
B_SPLINE_SURFACE(3,2,((#202552,#202553,#202554),(#202555,#202556,#202557),
(#202558,#202559,#202560),(#202561,#202562,#202563),(#202564,#202565,#202566),
(#202567,#202568,#202569)),.UNSPECIFIED.,.F.,.F.,.F.)
B_SPLINE_SURFACE_WITH_KNOTS((4,2,4),(3,3),(0.,0.000256592814262157,0.000513185628524314),
(0.,1.),.UNSPECIFIED.)
GEOMETRIC_REPRESENTATION_ITEM()
RATIONAL_B_SPLINE_SURFACE(((1.,0.708712527163675,1.),(1.,0.753780902613242,
1.),(1.,0.794538995769671,1.),(1.,0.85507077033062,1.),(1.,0.875018427445703,
1.),(1.,0.874619707139387,1.)))
REPRESENTATION_ITEM('')
SURFACE()
);
#2777=(
BOUNDED_SURFACE()
B_SPLINE_SURFACE(3,2,((#202571,#202572,#202573),(#202574,#202575,#202576),
(#202577,#202578,#202579),(#202580,#202581,#202582)),.UNSPECIFIED.,.F.,
 .F.,.F.)
B_SPLINE_SURFACE_WITH_KNOTS((4,4),(3,3),(0.,0.000511815072430402),(0.,1.00105598365989),
 .UNSPECIFIED.)
GEOMETRIC_REPRESENTATION_ITEM()
RATIONAL_B_SPLINE_SURFACE(((1.,0.706797490733388,1.00061923411765),(1.,
0.70618206214629,1.00062053388271),(1.,0.70558406276869,1.00062179683786),
(1.,0.705266224770156,1.00062246810132)))
REPRESENTATION_ITEM('')
SURFACE()
);
#2778=(
BOUNDED_SURFACE()
B_SPLINE_SURFACE(3,2,((#202588,#202589,#202590),(#202591,#202592,#202593),
(#202594,#202595,#202596),(#202597,#202598,#202599),(#202600,#202601,#202602),
(#202603,#202604,#202605)),.UNSPECIFIED.,.F.,.F.,.F.)
B_SPLINE_SURFACE_WITH_KNOTS((4,2,4),(3,3),(0.,0.000257652232350882,0.000515304464701763),
(0.,1.),.UNSPECIFIED.)
GEOMETRIC_REPRESENTATION_ITEM()
RATIONAL_B_SPLINE_SURFACE(((1.,0.874619707139388,1.),(1.,0.874861180431117,
1.),(1.,0.855455725920339,1.),(1.,0.794699358955772,1.),(1.,0.753768977788269,
1.),(1.,0.70871252716366,1.)))
REPRESENTATION_ITEM('')
SURFACE()
);
#2779=(
BOUNDED_SURFACE()
B_SPLINE_SURFACE(3,2,((#202611,#202612,#202613),(#202614,#202615,#202616),
(#202617,#202618,#202619),(#202620,#202621,#202622)),.UNSPECIFIED.,.F.,
 .F.,.F.)
B_SPLINE_SURFACE_WITH_KNOTS((4,4),(3,3),(-1.47451495458029E-17,0.0003973943736519),
(0.,1.),.UNSPECIFIED.)
GEOMETRIC_REPRESENTATION_ITEM()
RATIONAL_B_SPLINE_SURFACE(((1.,0.707106781186548,1.),(1.,0.707752587915863,
1.),(1.,0.708377654540685,1.),(1.,0.708689770883324,1.)))
REPRESENTATION_ITEM('')
SURFACE()
);
#2780=(
BOUNDED_SURFACE()
B_SPLINE_SURFACE(3,2,((#202624,#202625,#202626),(#202627,#202628,#202629),
(#202630,#202631,#202632),(#202633,#202634,#202635)),.UNSPECIFIED.,.F.,
 .F.,.F.)
B_SPLINE_SURFACE_WITH_KNOTS((4,4),(3,3),(0.,0.000511815456479797),(0.,1.00105873159847),
 .UNSPECIFIED.)
GEOMETRIC_REPRESENTATION_ITEM()
RATIONAL_B_SPLINE_SURFACE(((1.,0.708394529056756,1.00061746385275),(1.,
0.708058564167281,1.00061817524604),(1.,0.707430835372509,1.00061950443866),
(1.,0.706796685880813,1.00062084722687)))
REPRESENTATION_ITEM('')
SURFACE()
);
#2781=(
BOUNDED_SURFACE()
B_SPLINE_SURFACE(3,2,((#202641,#202642,#202643),(#202644,#202645,#202646),
(#202647,#202648,#202649),(#202650,#202651,#202652)),.UNSPECIFIED.,.F.,
 .F.,.F.)
B_SPLINE_SURFACE_WITH_KNOTS((4,4),(3,3),(0.,0.000397394465448322),(0.,1.),
 .UNSPECIFIED.)
GEOMETRIC_REPRESENTATION_ITEM()
RATIONAL_B_SPLINE_SURFACE(((1.,0.705498956110752,1.),(1.,0.705821764811797,
1.),(1.,0.706461952521127,1.),(1.,0.707106781186548,1.)))
REPRESENTATION_ITEM('')
SURFACE()
);
#2782=(
BOUNDED_SURFACE()
B_SPLINE_SURFACE(3,2,((#202658,#202659,#202660),(#202661,#202662,#202663),
(#202664,#202665,#202666),(#202667,#202668,#202669)),.UNSPECIFIED.,.F.,
 .F.,.F.)
B_SPLINE_SURFACE_WITH_KNOTS((4,4),(3,3),(0.,0.000397394410828722),(0.,1.),
 .UNSPECIFIED.)
GEOMETRIC_REPRESENTATION_ITEM()
RATIONAL_B_SPLINE_SURFACE(((1.,0.708689770883299,1.),(1.,0.708376440034514,
1.),(1.,0.707750498698402,1.),(1.,0.707106781186535,1.)))
REPRESENTATION_ITEM('')
SURFACE()
);
#2783=(
BOUNDED_SURFACE()
B_SPLINE_SURFACE(3,2,((#202675,#202676,#202677),(#202678,#202679,#202680),
(#202681,#202682,#202683),(#202684,#202685,#202686)),.UNSPECIFIED.,.F.,
 .F.,.F.)
B_SPLINE_SURFACE_WITH_KNOTS((4,4),(3,3),(0.,0.000511815090126187),(0.,1.00105592270046),
 .UNSPECIFIED.)
GEOMETRIC_REPRESENTATION_ITEM()
RATIONAL_B_SPLINE_SURFACE(((1.,0.705266242718005,1.00062243212981),(1.,
0.705584085909643,1.00062176089413),(1.,0.706182089451007,1.0006204980031),
(1.,0.706797508587991,1.00061919833303)))
REPRESENTATION_ITEM('')
SURFACE()
);
#2784=(
BOUNDED_SURFACE()
B_SPLINE_SURFACE(3,2,((#202688,#202689,#202690),(#202691,#202692,#202693),
(#202694,#202695,#202696),(#202697,#202698,#202699)),.UNSPECIFIED.,.F.,
 .F.,.F.)
B_SPLINE_SURFACE_WITH_KNOTS((4,4),(3,3),(-1.47451495458029E-17,0.00039739442808661),
(0.,1.),.UNSPECIFIED.)
GEOMETRIC_REPRESENTATION_ITEM()
RATIONAL_B_SPLINE_SURFACE(((1.,0.707106781186549,1.),(1.,0.706459846759096,
1.),(1.,0.705820510737269,1.),(1.,0.705498956110752,1.)))
REPRESENTATION_ITEM('')
SURFACE()
);
#2785=(
BOUNDED_SURFACE()
B_SPLINE_SURFACE(3,2,((#202705,#202706,#202707),(#202708,#202709,#202710),
(#202711,#202712,#202713),(#202714,#202715,#202716),(#202717,#202718,#202719),
(#202720,#202721,#202722)),.UNSPECIFIED.,.F.,.F.,.F.)
B_SPLINE_SURFACE_WITH_KNOTS((4,2,4),(3,3),(0.,0.000257953807872851,0.000515907615745702),
(0.,1.),.UNSPECIFIED.)
GEOMETRIC_REPRESENTATION_ITEM()
RATIONAL_B_SPLINE_SURFACE(((1.,0.874619707139394,1.),(1.,0.874834349678836,
1.),(1.,0.85468610415798,1.),(1.,0.792476597914961,1.),(1.,0.750887854595252,
1.),(1.,0.705585838031447,1.)))
REPRESENTATION_ITEM('')
SURFACE()
);
#2786=(
BOUNDED_SURFACE()
B_SPLINE_SURFACE(3,2,((#202728,#202729,#202730),(#202731,#202732,#202733),
(#202734,#202735,#202736),(#202737,#202738,#202739)),.UNSPECIFIED.,.F.,
 .F.,.F.)
B_SPLINE_SURFACE_WITH_KNOTS((4,4),(3,3),(0.,0.000511815437699164),(0.,1.00105881331666),
 .UNSPECIFIED.)
GEOMETRIC_REPRESENTATION_ITEM()
RATIONAL_B_SPLINE_SURFACE(((1.,0.706796661946094,1.00062089519764),(1.,
0.707430821224998,1.00061955228506),(1.,0.708058545830475,1.00061822299872),
(1.,0.708394505252485,1.0006175115621)))
REPRESENTATION_ITEM('')
SURFACE()
);
#2787=(
BOUNDED_SURFACE()
B_SPLINE_SURFACE(3,2,((#202741,#202742,#202743),(#202744,#202745,#202746),
(#202747,#202748,#202749),(#202750,#202751,#202752),(#202753,#202754,#202755),
(#202756,#202757,#202758)),.UNSPECIFIED.,.F.,.F.,.F.)
B_SPLINE_SURFACE_WITH_KNOTS((4,2,4),(3,3),(0.,0.000256915317531265,0.000513830635062529),
(0.,1.),.UNSPECIFIED.)
GEOMETRIC_REPRESENTATION_ITEM()
RATIONAL_B_SPLINE_SURFACE(((1.,0.705585838031449,1.),(1.,0.750902433542386,
1.),(1.,0.792329530082973,1.),(1.,0.854288401593741,1.),(1.,0.874998031125484,
1.),(1.,0.874619707139406,1.)))
REPRESENTATION_ITEM('')
SURFACE()
);
#2788=(
BOUNDED_SURFACE()
B_SPLINE_SURFACE(3,2,((#202764,#202765,#202766),(#202767,#202768,#202769),
(#202770,#202771,#202772),(#202773,#202774,#202775),(#202776,#202777,#202778),
(#202779,#202780,#202781)),.UNSPECIFIED.,.F.,.F.,.F.)
B_SPLINE_SURFACE_WITH_KNOTS((4,2,4),(3,3),(-9.13440330319037E-18,0.000256592814262152,
0.000513185628524313),(0.,1.),.UNSPECIFIED.)
GEOMETRIC_REPRESENTATION_ITEM()
RATIONAL_B_SPLINE_SURFACE(((1.,0.708712527163635,1.),(1.,0.753780902613607,
1.),(1.,0.794538995769191,1.),(1.,0.855070770331096,1.),(1.,0.875018427445334,
1.),(1.,0.874619707139393,1.)))
REPRESENTATION_ITEM('')
SURFACE()
);
#2789=(
BOUNDED_SURFACE()
B_SPLINE_SURFACE(3,2,((#202783,#202784,#202785),(#202786,#202787,#202788),
(#202789,#202790,#202791),(#202792,#202793,#202794)),.UNSPECIFIED.,.F.,
 .F.,.F.)
B_SPLINE_SURFACE_WITH_KNOTS((4,4),(3,3),(-2.71050543121376E-20,0.000511815072430406),
(0.,1.00105598365961),.UNSPECIFIED.)
GEOMETRIC_REPRESENTATION_ITEM()
RATIONAL_B_SPLINE_SURFACE(((1.,0.706797490733471,1.00061923411748),(1.,
0.706182062146368,1.00062053388255),(1.,0.705584062768763,1.00062179683769),
(1.,0.705266224770216,1.00062246810115)))
REPRESENTATION_ITEM('')
SURFACE()
);
#2790=(
BOUNDED_SURFACE()
B_SPLINE_SURFACE(3,2,((#202800,#202801,#202802),(#202803,#202804,#202805),
(#202806,#202807,#202808),(#202809,#202810,#202811),(#202812,#202813,#202814),
(#202815,#202816,#202817)),.UNSPECIFIED.,.F.,.F.,.F.)
B_SPLINE_SURFACE_WITH_KNOTS((4,2,4),(3,3),(-5.02798757490153E-18,0.000257652232350882,
0.00051530446470177),(0.,1.),.UNSPECIFIED.)
GEOMETRIC_REPRESENTATION_ITEM()
RATIONAL_B_SPLINE_SURFACE(((1.,0.874619707139381,1.),(1.,0.87486118043123,
1.),(1.,0.855455725920156,1.),(1.,0.794699358955984,1.),(1.,0.753768977788076,
1.),(1.,0.708712527163675,1.)))
REPRESENTATION_ITEM('')
SURFACE()
);
#2791=(
BOUNDED_SURFACE()
B_SPLINE_SURFACE(3,2,((#202823,#202824,#202825),(#202826,#202827,#202828),
(#202829,#202830,#202831),(#202832,#202833,#202834)),.UNSPECIFIED.,.F.,
 .F.,.F.)
B_SPLINE_SURFACE_WITH_KNOTS((4,4),(3,3),(0.,0.000397394373651916),(0.,1.),
 .UNSPECIFIED.)
GEOMETRIC_REPRESENTATION_ITEM()
RATIONAL_B_SPLINE_SURFACE(((1.,0.707106781186535,1.),(1.,0.707752587915909,
1.),(1.,0.708377654540687,1.),(1.,0.708689770883326,1.)))
REPRESENTATION_ITEM('')
SURFACE()
);
#2792=(
BOUNDED_SURFACE()
B_SPLINE_SURFACE(3,2,((#202836,#202837,#202838),(#202839,#202840,#202841),
(#202842,#202843,#202844),(#202845,#202846,#202847)),.UNSPECIFIED.,.F.,
 .F.,.F.)
B_SPLINE_SURFACE_WITH_KNOTS((4,4),(3,3),(0.,0.00051181545647979),(0.,1.0010587315986),
 .UNSPECIFIED.)
GEOMETRIC_REPRESENTATION_ITEM()
RATIONAL_B_SPLINE_SURFACE(((1.,0.708394529056717,1.00061746385283),(1.,
0.70805856416728,1.00061817524611),(1.,0.70743083537246,1.00061950443873),
(1.,0.706796685880774,1.00062084722695)))
REPRESENTATION_ITEM('')
SURFACE()
);
#2793=(
BOUNDED_SURFACE()
B_SPLINE_SURFACE(3,2,((#202853,#202854,#202855),(#202856,#202857,#202858),
(#202859,#202860,#202861),(#202862,#202863,#202864)),.UNSPECIFIED.,.F.,
 .F.,.F.)
B_SPLINE_SURFACE_WITH_KNOTS((4,4),(3,3),(0.,0.000397394465448294),(0.,1.),
 .UNSPECIFIED.)
GEOMETRIC_REPRESENTATION_ITEM()
RATIONAL_B_SPLINE_SURFACE(((1.,0.705498956110742,1.),(1.,0.705821764811805,
1.),(1.,0.706461952521124,1.),(1.,0.70710678118656,1.)))
REPRESENTATION_ITEM('')
SURFACE()
);
#2794=(
BOUNDED_SURFACE()
B_SPLINE_SURFACE(3,2,((#202870,#202871,#202872),(#202873,#202874,#202875),
(#202876,#202877,#202878),(#202879,#202880,#202881)),.UNSPECIFIED.,.F.,
 .F.,.F.)
B_SPLINE_SURFACE_WITH_KNOTS((4,4),(3,3),(0.,0.00039739441082874),(0.,1.),
 .UNSPECIFIED.)
GEOMETRIC_REPRESENTATION_ITEM()
RATIONAL_B_SPLINE_SURFACE(((1.,0.708689770883332,1.),(1.,0.708376440034517,
1.),(1.,0.70775049869838,1.),(1.,0.707106781186548,1.)))
REPRESENTATION_ITEM('')
SURFACE()
);
#2795=(
BOUNDED_SURFACE()
B_SPLINE_SURFACE(3,2,((#202887,#202888,#202889),(#202890,#202891,#202892),
(#202893,#202894,#202895),(#202896,#202897,#202898)),.UNSPECIFIED.,.F.,
 .F.,.F.)
B_SPLINE_SURFACE_WITH_KNOTS((4,4),(3,3),(0.,0.000511815090126175),(0.,1.00105592270174),
 .UNSPECIFIED.)
GEOMETRIC_REPRESENTATION_ITEM()
RATIONAL_B_SPLINE_SURFACE(((1.,0.705266242717628,1.00062243213056),(1.,
0.705584085909269,1.00062176089488),(1.,0.706182089450612,1.00062049800385),
(1.,0.706797508587618,1.00061919833378)))
REPRESENTATION_ITEM('')
SURFACE()
);
#2796=(
BOUNDED_SURFACE()
B_SPLINE_SURFACE(3,2,((#202900,#202901,#202902),(#202903,#202904,#202905),
(#202906,#202907,#202908),(#202909,#202910,#202911)),.UNSPECIFIED.,.F.,
 .F.,.F.)
B_SPLINE_SURFACE_WITH_KNOTS((4,4),(3,3),(0.,0.000397394428086641),(0.,1.),
 .UNSPECIFIED.)
GEOMETRIC_REPRESENTATION_ITEM()
RATIONAL_B_SPLINE_SURFACE(((1.,0.707106781186532,1.),(1.,0.706459846759111,
1.),(1.,0.705820510737279,1.),(1.,0.705498956110745,1.)))
REPRESENTATION_ITEM('')
SURFACE()
);
#2797=(
BOUNDED_SURFACE()
B_SPLINE_SURFACE(3,2,((#202917,#202918,#202919),(#202920,#202921,#202922),
(#202923,#202924,#202925),(#202926,#202927,#202928),(#202929,#202930,#202931),
(#202932,#202933,#202934)),.UNSPECIFIED.,.F.,.F.,.F.)
B_SPLINE_SURFACE_WITH_KNOTS((4,2,4),(3,3),(0.,0.000257953807872849,0.000515907615745698),
(0.,1.),.UNSPECIFIED.)
GEOMETRIC_REPRESENTATION_ITEM()
RATIONAL_B_SPLINE_SURFACE(((1.,0.874619707139397,1.),(1.,0.874834349679158,
1.),(1.,0.854686104157565,1.),(1.,0.792476597915372,1.),(1.,0.750887854594947,
1.),(1.,0.705585838031446,1.)))
REPRESENTATION_ITEM('')
SURFACE()
);
#2798=(
BOUNDED_SURFACE()
B_SPLINE_SURFACE(3,2,((#202940,#202941,#202942),(#202943,#202944,#202945),
(#202946,#202947,#202948),(#202949,#202950,#202951)),.UNSPECIFIED.,.F.,
 .F.,.F.)
B_SPLINE_SURFACE_WITH_KNOTS((4,4),(3,3),(0.,0.000511815437699156),(0.,1.00105881331736),
 .UNSPECIFIED.)
GEOMETRIC_REPRESENTATION_ITEM()
RATIONAL_B_SPLINE_SURFACE(((1.,0.706796661945893,1.00062089519805),(1.,
0.707430821224857,1.00061955228547),(1.,0.708058545830205,1.00061822299913),
(1.,0.708394505252324,1.00061751156251)))
REPRESENTATION_ITEM('')
SURFACE()
);
#2799=(
BOUNDED_SURFACE()
B_SPLINE_SURFACE(3,2,((#202953,#202954,#202955),(#202956,#202957,#202958),
(#202959,#202960,#202961),(#202962,#202963,#202964),(#202965,#202966,#202967),
(#202968,#202969,#202970)),.UNSPECIFIED.,.F.,.F.,.F.)
B_SPLINE_SURFACE_WITH_KNOTS((4,2,4),(3,3),(-2.71050543121376E-20,0.000256915317531263,
0.000513830635062526),(0.,1.),.UNSPECIFIED.)
GEOMETRIC_REPRESENTATION_ITEM()
RATIONAL_B_SPLINE_SURFACE(((1.,0.705585838031448,1.),(1.,0.750902433542692,
1.),(1.,0.792329530082588,1.),(1.,0.854288401594132,1.),(1.,0.874998031125192,
1.),(1.,0.874619707139397,1.)))
REPRESENTATION_ITEM('')
SURFACE()
);
#2800=(
BOUNDED_SURFACE()
B_SPLINE_SURFACE(3,2,((#202976,#202977,#202978),(#202979,#202980,#202981),
(#202982,#202983,#202984),(#202985,#202986,#202987),(#202988,#202989,#202990),
(#202991,#202992,#202993)),.UNSPECIFIED.,.F.,.F.,.F.)
B_SPLINE_SURFACE_WITH_KNOTS((4,2,4),(3,3),(0.,0.000256592814262158,0.000513185628524316),
(0.,1.),.UNSPECIFIED.)
GEOMETRIC_REPRESENTATION_ITEM()
RATIONAL_B_SPLINE_SURFACE(((1.,0.708712527163647,1.),(1.,0.753780902613447,
1.),(1.,0.794538995769415,1.),(1.,0.855070770330899,1.),(1.,0.875018427445479,
1.),(1.,0.874619707139393,1.)))
REPRESENTATION_ITEM('')
SURFACE()
);
#2801=(
BOUNDED_SURFACE()
B_SPLINE_SURFACE(3,2,((#202995,#202996,#202997),(#202998,#202999,#203000),
(#203001,#203002,#203003),(#203004,#203005,#203006)),.UNSPECIFIED.,.F.,
 .F.,.F.)
B_SPLINE_SURFACE_WITH_KNOTS((4,4),(3,3),(0.,0.000511815072430398),(0.,1.00105598365643),
 .UNSPECIFIED.)
GEOMETRIC_REPRESENTATION_ITEM()
RATIONAL_B_SPLINE_SURFACE(((1.,0.70679749073439,1.00061923411562),(1.,0.706182062147315,
1.00062053388068),(1.,0.705584062769728,1.00062179683581),(1.,0.705266224771143,
1.00062246809928)))
REPRESENTATION_ITEM('')
SURFACE()
);
#2802=(
BOUNDED_SURFACE()
B_SPLINE_SURFACE(3,2,((#203012,#203013,#203014),(#203015,#203016,#203017),
(#203018,#203019,#203020),(#203021,#203022,#203023),(#203024,#203025,#203026),
(#203027,#203028,#203029)),.UNSPECIFIED.,.F.,.F.,.F.)
B_SPLINE_SURFACE_WITH_KNOTS((4,2,4),(3,3),(0.,0.000257652232350883,0.000515304464701767),
(0.,1.),.UNSPECIFIED.)
GEOMETRIC_REPRESENTATION_ITEM()
RATIONAL_B_SPLINE_SURFACE(((1.,0.874619707139392,1.),(1.,0.874861180430632,
1.),(1.,0.855455725920956,1.),(1.,0.794699358955172,1.),(1.,0.753768977788696,
1.),(1.,0.70871252716365,1.)))
REPRESENTATION_ITEM('')
SURFACE()
);
#2803=(
BOUNDED_SURFACE()
B_SPLINE_SURFACE(3,2,((#203035,#203036,#203037),(#203038,#203039,#203040),
(#203041,#203042,#203043),(#203044,#203045,#203046)),.UNSPECIFIED.,.F.,
 .F.,.F.)
B_SPLINE_SURFACE_WITH_KNOTS((4,4),(3,3),(0.,0.000397394373651906),(0.,1.),
 .UNSPECIFIED.)
GEOMETRIC_REPRESENTATION_ITEM()
RATIONAL_B_SPLINE_SURFACE(((1.,0.707106781186548,1.),(1.,0.707752587915907,
1.),(1.,0.70837765454067,1.),(1.,0.708689770883331,1.)))
REPRESENTATION_ITEM('')
SURFACE()
);
#2804=(
BOUNDED_SURFACE()
B_SPLINE_SURFACE(3,2,((#203048,#203049,#203050),(#203051,#203052,#203053),
(#203054,#203055,#203056),(#203057,#203058,#203059)),.UNSPECIFIED.,.F.,
 .F.,.F.)
B_SPLINE_SURFACE_WITH_KNOTS((4,4),(3,3),(-6.42389787197661E-18,0.000511815456479789),
(0.,1.00105873159726),.UNSPECIFIED.)
GEOMETRIC_REPRESENTATION_ITEM()
RATIONAL_B_SPLINE_SURFACE(((1.,0.708394529057106,1.00061746385204),(1.,
0.70805856416768,1.00061817524533),(1.,0.707430835372831,1.00061950443795),
(1.,0.706796685881154,1.00062084722616)))
REPRESENTATION_ITEM('')
SURFACE()
);
#2805=(
BOUNDED_SURFACE()
B_SPLINE_SURFACE(3,2,((#203065,#203066,#203067),(#203068,#203069,#203070),
(#203071,#203072,#203073),(#203074,#203075,#203076)),.UNSPECIFIED.,.F.,
 .F.,.F.)
B_SPLINE_SURFACE_WITH_KNOTS((4,4),(3,3),(0.,0.000397394465448304),(0.,1.),
 .UNSPECIFIED.)
GEOMETRIC_REPRESENTATION_ITEM()
RATIONAL_B_SPLINE_SURFACE(((1.,0.705498956110752,1.),(1.,0.705821764811813,
1.),(1.,0.706461952521096,1.),(1.,0.707106781186559,1.)))
REPRESENTATION_ITEM('')
SURFACE()
);
#2806=(
BOUNDED_SURFACE()
B_SPLINE_SURFACE(3,2,((#203082,#203083,#203084),(#203085,#203086,#203087),
(#203088,#203089,#203090),(#203091,#203092,#203093)),.UNSPECIFIED.,.F.,
 .F.,.F.)
B_SPLINE_SURFACE_WITH_KNOTS((4,4),(3,3),(0.,0.000397394410828728),(0.,1.),
 .UNSPECIFIED.)
GEOMETRIC_REPRESENTATION_ITEM()
RATIONAL_B_SPLINE_SURFACE(((1.,0.708689770883344,1.),(1.,0.708376440034511,
1.),(1.,0.707750498698398,1.),(1.,0.707106781186548,1.)))
REPRESENTATION_ITEM('')
SURFACE()
);
#2807=(
BOUNDED_SURFACE()
B_SPLINE_SURFACE(3,2,((#203099,#203100,#203101),(#203102,#203103,#203104),
(#203105,#203106,#203107),(#203108,#203109,#203110)),.UNSPECIFIED.,.F.,
 .F.,.F.)
B_SPLINE_SURFACE_WITH_KNOTS((4,4),(3,3),(0.,0.000511815090126177),(0.,1.00105592270118),
 .UNSPECIFIED.)
GEOMETRIC_REPRESENTATION_ITEM()
RATIONAL_B_SPLINE_SURFACE(((1.,0.705266242717771,1.00062243213024),(1.,
0.705584085909434,1.00062176089455),(1.,0.706182089450805,1.00062049800353),
(1.,0.70679750858778,1.00061919833345)))
REPRESENTATION_ITEM('')
SURFACE()
);
#2808=(
BOUNDED_SURFACE()
B_SPLINE_SURFACE(3,2,((#203112,#203113,#203114),(#203115,#203116,#203117),
(#203118,#203119,#203120),(#203121,#203122,#203123)),.UNSPECIFIED.,.F.,
 .F.,.F.)
B_SPLINE_SURFACE_WITH_KNOTS((4,4),(3,3),(0.,0.000397394428086627),(0.,1.),
 .UNSPECIFIED.)
GEOMETRIC_REPRESENTATION_ITEM()
RATIONAL_B_SPLINE_SURFACE(((1.,0.707106781186549,1.),(1.,0.706459846759132,
1.),(1.,0.705820510737241,1.),(1.,0.705498956110748,1.)))
REPRESENTATION_ITEM('')
SURFACE()
);
#2809=(
BOUNDED_SURFACE()
B_SPLINE_SURFACE(3,2,((#203129,#203130,#203131),(#203132,#203133,#203134),
(#203135,#203136,#203137),(#203138,#203139,#203140),(#203141,#203142,#203143),
(#203144,#203145,#203146)),.UNSPECIFIED.,.F.,.F.,.F.)
B_SPLINE_SURFACE_WITH_KNOTS((4,2,4),(3,3),(0.,0.000257953807872846,0.000515907615745692),
(0.,1.),.UNSPECIFIED.)
GEOMETRIC_REPRESENTATION_ITEM()
RATIONAL_B_SPLINE_SURFACE(((1.,0.874619707139383,1.),(1.,0.874834349679598,
1.),(1.,0.854686104157003,1.),(1.,0.792476597915936,1.),(1.,0.750887854594542,
1.),(1.,0.705585838031438,1.)))
REPRESENTATION_ITEM('')
SURFACE()
);
#2810=(
BOUNDED_SURFACE()
B_SPLINE_SURFACE(3,2,((#203152,#203153,#203154),(#203155,#203156,#203157),
(#203158,#203159,#203160),(#203161,#203162,#203163)),.UNSPECIFIED.,.F.,
 .F.,.F.)
B_SPLINE_SURFACE_WITH_KNOTS((4,4),(3,3),(0.,0.000511815437699146),(0.,1.00105881331538),
 .UNSPECIFIED.)
GEOMETRIC_REPRESENTATION_ITEM()
RATIONAL_B_SPLINE_SURFACE(((1.,0.706796661946483,1.00062089519689),(1.,
0.70743082122537,1.00061955228431),(1.,0.708058545830867,1.00061822299797),
(1.,0.708394505252865,1.00061751156135)))
REPRESENTATION_ITEM('')
SURFACE()
);
#2811=(
BOUNDED_SURFACE()
B_SPLINE_SURFACE(3,2,((#203165,#203166,#203167),(#203168,#203169,#203170),
(#203171,#203172,#203173),(#203174,#203175,#203176),(#203177,#203178,#203179),
(#203180,#203181,#203182)),.UNSPECIFIED.,.F.,.F.,.F.)
B_SPLINE_SURFACE_WITH_KNOTS((4,2,4),(3,3),(0.,0.000256915317531269,0.000513830635062538),
(0.,1.),.UNSPECIFIED.)
GEOMETRIC_REPRESENTATION_ITEM()
RATIONAL_B_SPLINE_SURFACE(((1.,0.705585838031449,1.),(1.,0.75090243354275,
1.),(1.,0.792329530082535,1.),(1.,0.854288401594234,1.),(1.,0.874998031125134,
1.),(1.,0.874619707139408,1.)))
REPRESENTATION_ITEM('')
SURFACE()
);
#2812=(
BOUNDED_SURFACE()
B_SPLINE_SURFACE(3,2,((#203188,#203189,#203190),(#203191,#203192,#203193),
(#203194,#203195,#203196),(#203197,#203198,#203199),(#203200,#203201,#203202),
(#203203,#203204,#203205)),.UNSPECIFIED.,.F.,.F.,.F.)
B_SPLINE_SURFACE_WITH_KNOTS((4,2,4),(3,3),(-9.7307144980574E-18,0.000256592814262153,
0.000513185628524316),(0.,1.),.UNSPECIFIED.)
GEOMETRIC_REPRESENTATION_ITEM()
RATIONAL_B_SPLINE_SURFACE(((1.,0.708712527163667,1.),(1.,0.7537809026138,
1.),(1.,0.79453899576896,1.),(1.,0.855070770331341,1.),(1.,0.875018427445144,
1.),(1.,0.874619707139388,1.)))
REPRESENTATION_ITEM('')
SURFACE()
);
#2813=(
BOUNDED_SURFACE()
B_SPLINE_SURFACE(3,2,((#203207,#203208,#203209),(#203210,#203211,#203212),
(#203213,#203214,#203215),(#203216,#203217,#203218)),.UNSPECIFIED.,.F.,
 .F.,.F.)
B_SPLINE_SURFACE_WITH_KNOTS((4,4),(3,3),(0.,0.000511815072430414),(0.,1.00105598365751),
 .UNSPECIFIED.)
GEOMETRIC_REPRESENTATION_ITEM()
RATIONAL_B_SPLINE_SURFACE(((1.,0.706797490734085,1.00061923411625),(1.,
0.70618206214702,1.00062053388131),(1.,0.705584062769344,1.00062179683645),
(1.,0.70526622477087,1.00062246809992)))
REPRESENTATION_ITEM('')
SURFACE()
);
#2814=(
BOUNDED_SURFACE()
B_SPLINE_SURFACE(3,2,((#203224,#203225,#203226),(#203227,#203228,#203229),
(#203230,#203231,#203232),(#203233,#203234,#203235),(#203236,#203237,#203238),
(#203239,#203240,#203241)),.UNSPECIFIED.,.F.,.F.,.F.)
B_SPLINE_SURFACE_WITH_KNOTS((4,2,4),(3,3),(0.,0.00025765223235089,0.00051530446470178),
(0.,1.),.UNSPECIFIED.)
GEOMETRIC_REPRESENTATION_ITEM()
RATIONAL_B_SPLINE_SURFACE(((1.,0.874619707139373,1.),(1.,0.874861180430774,
1.),(1.,0.855455725920732,1.),(1.,0.79469935895536,1.),(1.,0.75376897778856,
1.),(1.,0.708712527163633,1.)))
REPRESENTATION_ITEM('')
SURFACE()
);
#2815=(
BOUNDED_SURFACE()
B_SPLINE_SURFACE(3,2,((#203247,#203248,#203249),(#203250,#203251,#203252),
(#203253,#203254,#203255),(#203256,#203257,#203258)),.UNSPECIFIED.,.F.,
 .F.,.F.)
B_SPLINE_SURFACE_WITH_KNOTS((4,4),(3,3),(0.,0.000397394373651923),(0.,1.),
 .UNSPECIFIED.)
GEOMETRIC_REPRESENTATION_ITEM()
RATIONAL_B_SPLINE_SURFACE(((1.,0.707106781186548,1.),(1.,0.707752587915923,
1.),(1.,0.708377654540652,1.),(1.,0.708689770883338,1.)))
REPRESENTATION_ITEM('')
SURFACE()
);
#2816=(
BOUNDED_SURFACE()
B_SPLINE_SURFACE(3,2,((#203260,#203261,#203262),(#203263,#203264,#203265),
(#203266,#203267,#203268),(#203269,#203270,#203271)),.UNSPECIFIED.,.F.,
 .F.,.F.)
B_SPLINE_SURFACE_WITH_KNOTS((4,4),(3,3),(-6.42389787197661E-18,0.00051181545647979),
(0.,1.00105873159723),.UNSPECIFIED.)
GEOMETRIC_REPRESENTATION_ITEM()
RATIONAL_B_SPLINE_SURFACE(((1.,0.708394529057117,1.00061746385203),(1.,
0.708058564167685,1.00061817524531),(1.,0.707430835372828,1.00061950443793),
(1.,0.706796685881165,1.00062084722614)))
REPRESENTATION_ITEM('')
SURFACE()
);
#2817=(
BOUNDED_SURFACE()
B_SPLINE_SURFACE(3,2,((#203277,#203278,#203279),(#203280,#203281,#203282),
(#203283,#203284,#203285),(#203286,#203287,#203288)),.UNSPECIFIED.,.F.,
 .F.,.F.)
B_SPLINE_SURFACE_WITH_KNOTS((4,4),(3,3),(-1.57209315010398E-17,0.000397394465448301),
(0.,1.),.UNSPECIFIED.)
GEOMETRIC_REPRESENTATION_ITEM()
RATIONAL_B_SPLINE_SURFACE(((1.,0.705498956110757,1.),(1.,0.705821764811813,
1.),(1.,0.706461952521126,1.),(1.,0.707106781186557,1.)))
REPRESENTATION_ITEM('')
SURFACE()
);
#2818=(
BOUNDED_SURFACE()
B_SPLINE_SURFACE(3,2,((#203294,#203295,#203296),(#203297,#203298,#203299),
(#203300,#203301,#203302),(#203303,#203304,#203305)),.UNSPECIFIED.,.F.,
 .F.,.F.)
B_SPLINE_SURFACE_WITH_KNOTS((4,4),(3,3),(0.,0.000397394410828746),(0.,1.),
 .UNSPECIFIED.)
GEOMETRIC_REPRESENTATION_ITEM()
RATIONAL_B_SPLINE_SURFACE(((1.,0.708689770883336,1.),(1.,0.708376440034495,
1.),(1.,0.707750498698418,1.),(1.,0.707106781186547,1.)))
REPRESENTATION_ITEM('')
SURFACE()
);
#2819=(
BOUNDED_SURFACE()
B_SPLINE_SURFACE(3,2,((#203311,#203312,#203313),(#203314,#203315,#203316),
(#203317,#203318,#203319),(#203320,#203321,#203322)),.UNSPECIFIED.,.F.,
 .F.,.F.)
B_SPLINE_SURFACE_WITH_KNOTS((4,4),(3,3),(0.,0.000511815090126181),(0.,1.0010559227012),
 .UNSPECIFIED.)
GEOMETRIC_REPRESENTATION_ITEM()
RATIONAL_B_SPLINE_SURFACE(((1.,0.705266242717788,1.00062243213025),(1.,
0.705584085909427,1.00062176089456),(1.,0.706182089450776,1.00062049800353),
(1.,0.706797508587784,1.00061919833346)))
REPRESENTATION_ITEM('')
SURFACE()
);
#2820=(
BOUNDED_SURFACE()
B_SPLINE_SURFACE(3,2,((#203324,#203325,#203326),(#203327,#203328,#203329),
(#203330,#203331,#203332),(#203333,#203334,#203335)),.UNSPECIFIED.,.F.,
 .F.,.F.)
B_SPLINE_SURFACE_WITH_KNOTS((4,4),(3,3),(0.,0.00039739442808663),(0.,1.),
 .UNSPECIFIED.)
GEOMETRIC_REPRESENTATION_ITEM()
RATIONAL_B_SPLINE_SURFACE(((1.,0.707106781186539,1.),(1.,0.706459846759109,
1.),(1.,0.705820510737253,1.),(1.,0.705498956110755,1.)))
REPRESENTATION_ITEM('')
SURFACE()
);
#2821=(
BOUNDED_SURFACE()
B_SPLINE_SURFACE(3,2,((#203341,#203342,#203343),(#203344,#203345,#203346),
(#203347,#203348,#203349),(#203350,#203351,#203352),(#203353,#203354,#203355),
(#203356,#203357,#203358)),.UNSPECIFIED.,.F.,.F.,.F.)
B_SPLINE_SURFACE_WITH_KNOTS((4,2,4),(3,3),(0.,0.000257953807872851,0.000515907615745702),
(0.,1.),.UNSPECIFIED.)
GEOMETRIC_REPRESENTATION_ITEM()
RATIONAL_B_SPLINE_SURFACE(((1.,0.874619707139387,1.),(1.,0.874834349679411,
1.),(1.,0.854686104157238,1.),(1.,0.792476597915689,1.),(1.,0.750887854594714,
1.),(1.,0.705585838031445,1.)))
REPRESENTATION_ITEM('')
SURFACE()
);
#2822=(
BOUNDED_SURFACE()
B_SPLINE_SURFACE(3,2,((#203364,#203365,#203366),(#203367,#203368,#203369),
(#203370,#203371,#203372),(#203373,#203374,#203375)),.UNSPECIFIED.,.F.,
 .F.,.F.)
B_SPLINE_SURFACE_WITH_KNOTS((4,4),(3,3),(0.,0.000511815437699153),(0.,1.00105881331596),
 .UNSPECIFIED.)
GEOMETRIC_REPRESENTATION_ITEM()
RATIONAL_B_SPLINE_SURFACE(((1.,0.706796661946323,1.00062089519723),(1.,
0.707430821225177,1.00061955228465),(1.,0.708058545830703,1.00061822299831),
(1.,0.708394505252707,1.00061751156169)))
REPRESENTATION_ITEM('')
SURFACE()
);
#2823=(
BOUNDED_SURFACE()
B_SPLINE_SURFACE(3,2,((#203377,#203378,#203379),(#203380,#203381,#203382),
(#203383,#203384,#203385),(#203386,#203387,#203388),(#203389,#203390,#203391),
(#203392,#203393,#203394)),.UNSPECIFIED.,.F.,.F.,.F.)
B_SPLINE_SURFACE_WITH_KNOTS((4,2,4),(3,3),(0.,0.000256915317531267,0.000513830635062533),
(0.,1.),.UNSPECIFIED.)
GEOMETRIC_REPRESENTATION_ITEM()
RATIONAL_B_SPLINE_SURFACE(((1.,0.705585838031441,1.),(1.,0.750902433542965,
1.),(1.,0.792329530082225,1.),(1.,0.854288401594516,1.),(1.,0.874998031124923,
1.),(1.,0.874619707139399,1.)))
REPRESENTATION_ITEM('')
SURFACE()
);
#2824=(
BOUNDED_SURFACE()
B_SPLINE_SURFACE(3,2,((#203400,#203401,#203402),(#203403,#203404,#203405),
(#203406,#203407,#203408),(#203409,#203410,#203411),(#203412,#203413,#203414),
(#203415,#203416,#203417)),.UNSPECIFIED.,.F.,.F.,.F.)
B_SPLINE_SURFACE_WITH_KNOTS((4,2,4),(3,3),(-9.86623976961809E-18,0.000256592814262151,
0.000513185628524312),(0.,1.),.UNSPECIFIED.)
GEOMETRIC_REPRESENTATION_ITEM()
RATIONAL_B_SPLINE_SURFACE(((1.,0.708712527163664,1.),(1.,0.753780902613921,
1.),(1.,0.794538995768751,1.),(1.,0.855070770331543,1.),(1.,0.875018427444988,
1.),(1.,0.874619707139397,1.)))
REPRESENTATION_ITEM('')
SURFACE()
);
#2825=(
BOUNDED_SURFACE()
B_SPLINE_SURFACE(3,2,((#203419,#203420,#203421),(#203422,#203423,#203424),
(#203425,#203426,#203427),(#203428,#203429,#203430)),.UNSPECIFIED.,.F.,
 .F.,.F.)
B_SPLINE_SURFACE_WITH_KNOTS((4,4),(3,3),(0.,0.000511815072430393),(0.,1.00105598365616),
 .UNSPECIFIED.)
GEOMETRIC_REPRESENTATION_ITEM()
RATIONAL_B_SPLINE_SURFACE(((1.,0.706797490734472,1.00061923411546),(1.,
0.706182062147432,1.00062053388052),(1.,0.70558406276972,1.00062179683566),
(1.,0.705266224771268,1.00062246809912)))
REPRESENTATION_ITEM('')
SURFACE()
);
#2826=(
BOUNDED_SURFACE()
B_SPLINE_SURFACE(3,2,((#203436,#203437,#203438),(#203439,#203440,#203441),
(#203442,#203443,#203444),(#203445,#203446,#203447),(#203448,#203449,#203450),
(#203451,#203452,#203453)),.UNSPECIFIED.,.F.,.F.,.F.)
B_SPLINE_SURFACE_WITH_KNOTS((4,2,4),(3,3),(0.,0.000257652232350879,0.000515304464701758),
(0.,1.),.UNSPECIFIED.)
GEOMETRIC_REPRESENTATION_ITEM()
RATIONAL_B_SPLINE_SURFACE(((1.,0.874619707139378,1.),(1.,0.87486118043099,
1.),(1.,0.855455725920465,1.),(1.,0.794699358955661,1.),(1.,0.753768977788322,
1.),(1.,0.70871252716365,1.)))
REPRESENTATION_ITEM('')
SURFACE()
);
#2827=(
BOUNDED_SURFACE()
B_SPLINE_SURFACE(3,2,((#203459,#203460,#203461),(#203462,#203463,#203464),
(#203465,#203466,#203467),(#203468,#203469,#203470)),.UNSPECIFIED.,.F.,
 .F.,.F.)
B_SPLINE_SURFACE_WITH_KNOTS((4,4),(3,3),(0.,0.000397394373651913),(0.,1.),
 .UNSPECIFIED.)
GEOMETRIC_REPRESENTATION_ITEM()
RATIONAL_B_SPLINE_SURFACE(((1.,0.70710678118654,1.),(1.,0.707752587915909,
1.),(1.,0.708377654540683,1.),(1.,0.708689770883316,1.)))
REPRESENTATION_ITEM('')
SURFACE()
);
#2828=(
BOUNDED_SURFACE()
B_SPLINE_SURFACE(3,2,((#203472,#203473,#203474),(#203475,#203476,#203477),
(#203478,#203479,#203480),(#203481,#203482,#203483)),.UNSPECIFIED.,.F.,
 .F.,.F.)
B_SPLINE_SURFACE_WITH_KNOTS((4,4),(3,3),(0.,0.000511815456479786),(0.,1.00105873159848),
 .UNSPECIFIED.)
GEOMETRIC_REPRESENTATION_ITEM()
RATIONAL_B_SPLINE_SURFACE(((1.,0.708394529056752,1.00061746385276),(1.,
0.708058564167294,1.00061817524605),(1.,0.707430835372481,1.00061950443867),
(1.,0.706796685880808,1.00062084722688)))
REPRESENTATION_ITEM('')
SURFACE()
);
#2829=(
BOUNDED_SURFACE()
B_SPLINE_SURFACE(3,2,((#203489,#203490,#203491),(#203492,#203493,#203494),
(#203495,#203496,#203497),(#203498,#203499,#203500)),.UNSPECIFIED.,.F.,
 .F.,.F.)
B_SPLINE_SURFACE_WITH_KNOTS((4,4),(3,3),(0.,0.000397394465448307),(0.,1.),
 .UNSPECIFIED.)
GEOMETRIC_REPRESENTATION_ITEM()
RATIONAL_B_SPLINE_SURFACE(((1.,0.705498956110761,1.),(1.,0.705821764811792,
1.),(1.,0.706461952521129,1.),(1.,0.707106781186548,1.)))
REPRESENTATION_ITEM('')
SURFACE()
);
#2830=(
BOUNDED_SURFACE()
B_SPLINE_SURFACE(3,2,((#203506,#203507,#203508),(#203509,#203510,#203511),
(#203512,#203513,#203514),(#203515,#203516,#203517)),.UNSPECIFIED.,.F.,
 .F.,.F.)
B_SPLINE_SURFACE_WITH_KNOTS((4,4),(3,3),(0.,0.000397394410828738),(0.,1.),
 .UNSPECIFIED.)
GEOMETRIC_REPRESENTATION_ITEM()
RATIONAL_B_SPLINE_SURFACE(((1.,0.708689770883313,1.),(1.,0.708376440034526,
1.),(1.,0.707750498698415,1.),(1.,0.707106781186548,1.)))
REPRESENTATION_ITEM('')
SURFACE()
);
#2831=(
BOUNDED_SURFACE()
B_SPLINE_SURFACE(3,2,((#203523,#203524,#203525),(#203526,#203527,#203528),
(#203529,#203530,#203531),(#203532,#203533,#203534)),.UNSPECIFIED.,.F.,
 .F.,.F.)
B_SPLINE_SURFACE_WITH_KNOTS((4,4),(3,3),(0.,0.000511815090126175),(0.,1.00105592270185),
 .UNSPECIFIED.)
GEOMETRIC_REPRESENTATION_ITEM()
RATIONAL_B_SPLINE_SURFACE(((1.,0.705266242717582,1.00062243213063),(1.,
0.705584085909227,1.00062176089495),(1.,0.706182089450609,1.00062049800392),
(1.,0.70679750858758,1.00061919833384)))
REPRESENTATION_ITEM('')
SURFACE()
);
#2832=(
BOUNDED_SURFACE()
B_SPLINE_SURFACE(3,2,((#203536,#203537,#203538),(#203539,#203540,#203541),
(#203542,#203543,#203544),(#203545,#203546,#203547)),.UNSPECIFIED.,.F.,
 .F.,.F.)
B_SPLINE_SURFACE_WITH_KNOTS((4,4),(3,3),(0.,0.000397394428086637),(0.,1.),
 .UNSPECIFIED.)
GEOMETRIC_REPRESENTATION_ITEM()
RATIONAL_B_SPLINE_SURFACE(((1.,0.707106781186542,1.),(1.,0.706459846759078,
1.),(1.,0.705820510737287,1.),(1.,0.705498956110738,1.)))
REPRESENTATION_ITEM('')
SURFACE()
);
#2833=(
BOUNDED_SURFACE()
B_SPLINE_SURFACE(3,2,((#203553,#203554,#203555),(#203556,#203557,#203558),
(#203559,#203560,#203561),(#203562,#203563,#203564),(#203565,#203566,#203567),
(#203568,#203569,#203570)),.UNSPECIFIED.,.F.,.F.,.F.)
B_SPLINE_SURFACE_WITH_KNOTS((4,2,4),(3,3),(0.,0.000257953807872848,0.000515907615745695),
(0.,1.),.UNSPECIFIED.)
GEOMETRIC_REPRESENTATION_ITEM()
RATIONAL_B_SPLINE_SURFACE(((1.,0.874619707139392,1.),(1.,0.874834349678565,
1.),(1.,0.854686104158367,1.),(1.,0.792476597914559,1.),(1.,0.750887854595556,
1.),(1.,0.705585838031436,1.)))
REPRESENTATION_ITEM('')
SURFACE()
);
#2834=(
BOUNDED_SURFACE()
B_SPLINE_SURFACE(3,2,((#203576,#203577,#203578),(#203579,#203580,#203581),
(#203582,#203583,#203584),(#203585,#203586,#203587)),.UNSPECIFIED.,.F.,
 .F.,.F.)
B_SPLINE_SURFACE_WITH_KNOTS((4,4),(3,3),(0.,0.000511815437699153),(0.,1.00105881331522),
 .UNSPECIFIED.)
GEOMETRIC_REPRESENTATION_ITEM()
RATIONAL_B_SPLINE_SURFACE(((1.,0.706796661946524,1.0006208951968),(1.,0.707430821225403,
1.00061955228422),(1.,0.708058545830954,1.00061822299788),(1.,0.708394505252897,
1.00061751156126)))
REPRESENTATION_ITEM('')
SURFACE()
);
#2835=(
BOUNDED_SURFACE()
B_SPLINE_SURFACE(3,2,((#203589,#203590,#203591),(#203592,#203593,#203594),
(#203595,#203596,#203597),(#203598,#203599,#203600),(#203601,#203602,#203603),
(#203604,#203605,#203606)),.UNSPECIFIED.,.F.,.F.,.F.)
B_SPLINE_SURFACE_WITH_KNOTS((4,2,4),(3,3),(0.,0.000256915317531264,0.000513830635062528),
(0.,1.),.UNSPECIFIED.)
GEOMETRIC_REPRESENTATION_ITEM()
RATIONAL_B_SPLINE_SURFACE(((1.,0.705585838031451,1.),(1.,0.750902433543144,
1.),(1.,0.792329530082004,1.),(1.,0.854288401594724,1.),(1.,0.874998031124746,
1.),(1.,0.87461970713938,1.)))
REPRESENTATION_ITEM('')
SURFACE()
);
#2836=(
BOUNDED_SURFACE()
B_SPLINE_SURFACE(3,2,((#203612,#203613,#203614),(#203615,#203616,#203617),
(#203618,#203619,#203620),(#203621,#203622,#203623),(#203624,#203625,#203626),
(#203627,#203628,#203629)),.UNSPECIFIED.,.F.,.F.,.F.)
B_SPLINE_SURFACE_WITH_KNOTS((4,2,4),(3,3),(-5.77337656848531E-18,0.000256592814262153,
0.000513185628524311),(0.,1.),.UNSPECIFIED.)
GEOMETRIC_REPRESENTATION_ITEM()
RATIONAL_B_SPLINE_SURFACE(((1.,0.708712527163686,1.),(1.,0.753780902613222,
1.),(1.,0.794538995769662,1.),(1.,0.855070770330659,1.),(1.,0.875018427445666,
1.),(1.,0.874619707139391,1.)))
REPRESENTATION_ITEM('')
SURFACE()
);
#2837=(
BOUNDED_SURFACE()
B_SPLINE_SURFACE(3,2,((#203631,#203632,#203633),(#203634,#203635,#203636),
(#203637,#203638,#203639),(#203640,#203641,#203642)),.UNSPECIFIED.,.F.,
 .F.,.F.)
B_SPLINE_SURFACE_WITH_KNOTS((4,4),(3,3),(-6.50521303491303E-18,0.000511815072430408),
(0.,1.00105598365618),.UNSPECIFIED.)
GEOMETRIC_REPRESENTATION_ITEM()
RATIONAL_B_SPLINE_SURFACE(((1.,0.706797490734475,1.00061923411547),(1.,
0.706182062147388,1.00062053388053),(1.,0.705584062769775,1.00062179683567),
(1.,0.705266224771253,1.00062246809913)))
REPRESENTATION_ITEM('')
SURFACE()
);
#2838=(
BOUNDED_SURFACE()
B_SPLINE_SURFACE(3,2,((#203648,#203649,#203650),(#203651,#203652,#203653),
(#203654,#203655,#203656),(#203657,#203658,#203659),(#203660,#203661,#203662),
(#203663,#203664,#203665)),.UNSPECIFIED.,.F.,.F.,.F.)
B_SPLINE_SURFACE_WITH_KNOTS((4,2,4),(3,3),(0.,0.000257652232350882,0.000515304464701765),
(0.,1.),.UNSPECIFIED.)
GEOMETRIC_REPRESENTATION_ITEM()
RATIONAL_B_SPLINE_SURFACE(((1.,0.874619707139388,1.),(1.,0.874861180430391,
1.),(1.,0.855455725921296,1.),(1.,0.794699358954867,1.),(1.,0.753768977788935,
1.),(1.,0.708712527163671,1.)))
REPRESENTATION_ITEM('')
SURFACE()
);
#2839=(
BOUNDED_SURFACE()
B_SPLINE_SURFACE(3,2,((#203671,#203672,#203673),(#203674,#203675,#203676),
(#203677,#203678,#203679),(#203680,#203681,#203682)),.UNSPECIFIED.,.F.,
 .F.,.F.)
B_SPLINE_SURFACE_WITH_KNOTS((4,4),(3,3),(-6.47810798060089E-18,0.000397394373651925),
(0.,1.),.UNSPECIFIED.)
GEOMETRIC_REPRESENTATION_ITEM()
RATIONAL_B_SPLINE_SURFACE(((1.,0.707106781186548,1.),(1.,0.707752587915882,
1.),(1.,0.708377654540684,1.),(1.,0.708689770883318,1.)))
REPRESENTATION_ITEM('')
SURFACE()
);
#2840=(
BOUNDED_SURFACE()
B_SPLINE_SURFACE(3,2,((#203684,#203685,#203686),(#203687,#203688,#203689),
(#203690,#203691,#203692),(#203693,#203694,#203695)),.UNSPECIFIED.,.F.,
 .F.,.F.)
B_SPLINE_SURFACE_WITH_KNOTS((4,4),(3,3),(0.,0.000511815456479792),(0.,1.0010587315997),
 .UNSPECIFIED.)
GEOMETRIC_REPRESENTATION_ITEM()
RATIONAL_B_SPLINE_SURFACE(((1.,0.708394529056393,1.00061746385347),(1.,
0.708058564166965,1.00061817524676),(1.,0.707430835372115,1.00061950443938),
(1.,0.706796685880457,1.00062084722759)))
REPRESENTATION_ITEM('')
SURFACE()
);
#2841=(
BOUNDED_SURFACE()
B_SPLINE_SURFACE(3,2,((#203701,#203702,#203703),(#203704,#203705,#203706),
(#203707,#203708,#203709),(#203710,#203711,#203712)),.UNSPECIFIED.,.F.,
 .F.,.F.)
B_SPLINE_SURFACE_WITH_KNOTS((4,4),(3,3),(-6.50521303491303E-18,0.000397394465448295),
(0.,1.),.UNSPECIFIED.)
GEOMETRIC_REPRESENTATION_ITEM()
RATIONAL_B_SPLINE_SURFACE(((1.,0.705498956110763,1.),(1.,0.705821764811782,
1.),(1.,0.706461952521153,1.),(1.,0.707106781186548,1.)))
REPRESENTATION_ITEM('')
SURFACE()
);
#2842=(
BOUNDED_SURFACE()
B_SPLINE_SURFACE(3,2,((#203718,#203719,#203720),(#203721,#203722,#203723),
(#203724,#203725,#203726),(#203727,#203728,#203729)),.UNSPECIFIED.,.F.,
 .F.,.F.)
B_SPLINE_SURFACE_WITH_KNOTS((4,4),(3,3),(0.,0.000397394410828746),(0.,1.),
 .UNSPECIFIED.)
GEOMETRIC_REPRESENTATION_ITEM()
RATIONAL_B_SPLINE_SURFACE(((1.,0.708689770883334,1.),(1.,0.708376440034459,
1.),(1.,0.707750498698428,1.),(1.,0.707106781186548,1.)))
REPRESENTATION_ITEM('')
SURFACE()
);
#2843=(
BOUNDED_SURFACE()
B_SPLINE_SURFACE(3,2,((#203735,#203736,#203737),(#203738,#203739,#203740),
(#203741,#203742,#203743),(#203744,#203745,#203746)),.UNSPECIFIED.,.F.,
 .F.,.F.)
B_SPLINE_SURFACE_WITH_KNOTS((4,4),(3,3),(0.,0.000511815090126176),(0.,1.00105592270255),
 .UNSPECIFIED.)
GEOMETRIC_REPRESENTATION_ITEM()
RATIONAL_B_SPLINE_SURFACE(((1.,0.705266242717375,1.00062243213105),(1.,
0.705584085909053,1.00062176089536),(1.,0.706182089450385,1.00062049800433),
(1.,0.706797508587384,1.00061919833425)))
REPRESENTATION_ITEM('')
SURFACE()
);
#2844=(
BOUNDED_SURFACE()
B_SPLINE_SURFACE(3,2,((#203748,#203749,#203750),(#203751,#203752,#203753),
(#203754,#203755,#203756),(#203757,#203758,#203759)),.UNSPECIFIED.,.F.,
 .F.,.F.)
B_SPLINE_SURFACE_WITH_KNOTS((4,4),(3,3),(-7.04731412115578E-18,0.000397394428086627),
(0.,1.),.UNSPECIFIED.)
GEOMETRIC_REPRESENTATION_ITEM()
RATIONAL_B_SPLINE_SURFACE(((1.,0.707106781186552,1.),(1.,0.706459846759089,
1.),(1.,0.705820510737279,1.),(1.,0.70549895611075,1.)))
REPRESENTATION_ITEM('')
SURFACE()
);
#2845=(
BOUNDED_SURFACE()
B_SPLINE_SURFACE(3,2,((#203765,#203766,#203767),(#203768,#203769,#203770),
(#203771,#203772,#203773),(#203774,#203775,#203776),(#203777,#203778,#203779),
(#203780,#203781,#203782)),.UNSPECIFIED.,.F.,.F.,.F.)
B_SPLINE_SURFACE_WITH_KNOTS((4,2,4),(3,3),(0.,0.000257953807872837,0.000515907615745675),
(0.,1.),.UNSPECIFIED.)
GEOMETRIC_REPRESENTATION_ITEM()
RATIONAL_B_SPLINE_SURFACE(((1.,0.874619707139391,1.),(1.,0.874834349678828,
1.),(1.,0.854686104158017,1.),(1.,0.792476597914933,1.),(1.,0.750887854595276,
1.),(1.,0.705585838031441,1.)))
REPRESENTATION_ITEM('')
SURFACE()
);
#2846=(
BOUNDED_SURFACE()
B_SPLINE_SURFACE(3,2,((#203788,#203789,#203790),(#203791,#203792,#203793),
(#203794,#203795,#203796),(#203797,#203798,#203799)),.UNSPECIFIED.,.F.,
 .F.,.F.)
B_SPLINE_SURFACE_WITH_KNOTS((4,4),(3,3),(0.,0.000511815437699145),(0.,1.00105881331634),
 .UNSPECIFIED.)
GEOMETRIC_REPRESENTATION_ITEM()
RATIONAL_B_SPLINE_SURFACE(((1.,0.706796661946205,1.00062089519746),(1.,
0.707430821225054,1.00061955228488),(1.,0.708058545830615,1.00061822299854),
(1.,0.708394505252581,1.00061751156192)))
REPRESENTATION_ITEM('')
SURFACE()
);
#2847=(
BOUNDED_SURFACE()
B_SPLINE_SURFACE(3,2,((#203801,#203802,#203803),(#203804,#203805,#203806),
(#203807,#203808,#203809),(#203810,#203811,#203812),(#203813,#203814,#203815),
(#203816,#203817,#203818)),.UNSPECIFIED.,.F.,.F.,.F.)
B_SPLINE_SURFACE_WITH_KNOTS((4,2,4),(3,3),(0.,0.00025691531753126,0.00051383063506252),
(0.,1.),.UNSPECIFIED.)
GEOMETRIC_REPRESENTATION_ITEM()
RATIONAL_B_SPLINE_SURFACE(((1.,0.705585838031456,1.),(1.,0.750902433542903,
1.),(1.,0.792329530082338,1.),(1.,0.854288401594379,1.),(1.,0.874998031125013,
1.),(1.,0.874619707139406,1.)))
REPRESENTATION_ITEM('')
SURFACE()
);
#2848=(
BOUNDED_SURFACE()
B_SPLINE_SURFACE(3,2,((#203824,#203825,#203826),(#203827,#203828,#203829),
(#203830,#203831,#203832),(#203833,#203834,#203835),(#203836,#203837,#203838),
(#203839,#203840,#203841)),.UNSPECIFIED.,.F.,.F.,.F.)
B_SPLINE_SURFACE_WITH_KNOTS((4,2,4),(3,3),(-1.00559751498031E-17,0.000256592814262151,
0.000513185628524312),(0.,1.),.UNSPECIFIED.)
GEOMETRIC_REPRESENTATION_ITEM()
RATIONAL_B_SPLINE_SURFACE(((1.,0.708712527163686,1.),(1.,0.753780902613619,
1.),(1.,0.794538995769145,1.),(1.,0.855070770331154,1.),(1.,0.875018427445275,
1.),(1.,0.874619707139389,1.)))
REPRESENTATION_ITEM('')
SURFACE()
);
#2849=(
BOUNDED_SURFACE()
B_SPLINE_SURFACE(3,2,((#203843,#203844,#203845),(#203846,#203847,#203848),
(#203849,#203850,#203851),(#203852,#203853,#203854)),.UNSPECIFIED.,.F.,
 .F.,.F.)
B_SPLINE_SURFACE_WITH_KNOTS((4,4),(3,3),(0.,0.000511815072430401),(0.,1.00105598365772),
 .UNSPECIFIED.)
GEOMETRIC_REPRESENTATION_ITEM()
RATIONAL_B_SPLINE_SURFACE(((1.,0.706797490734024,1.00061923411637),(1.,
0.706182062146945,1.00062053388144),(1.,0.705584062769309,1.00062179683658),
(1.,0.705266224770789,1.00062246810004)))
REPRESENTATION_ITEM('')
SURFACE()
);
#2850=(
BOUNDED_SURFACE()
B_SPLINE_SURFACE(3,2,((#203860,#203861,#203862),(#203863,#203864,#203865),
(#203866,#203867,#203868),(#203869,#203870,#203871),(#203872,#203873,#203874),
(#203875,#203876,#203877)),.UNSPECIFIED.,.F.,.F.,.F.)
B_SPLINE_SURFACE_WITH_KNOTS((4,2,4),(3,3),(0.,0.000257652232350878,0.000515304464701757),
(0.,1.),.UNSPECIFIED.)
GEOMETRIC_REPRESENTATION_ITEM()
RATIONAL_B_SPLINE_SURFACE(((1.,0.87461970713938,1.),(1.,0.87486118043086,
1.),(1.,0.855455725920641,1.),(1.,0.794699358955482,1.),(1.,0.753768977788477,
1.),(1.,0.708712527163645,1.)))
REPRESENTATION_ITEM('')
SURFACE()
);
#2851=(
BOUNDED_SURFACE()
B_SPLINE_SURFACE(3,2,((#203883,#203884,#203885),(#203886,#203887,#203888),
(#203889,#203890,#203891),(#203892,#203893,#203894)),.UNSPECIFIED.,.F.,
 .F.,.F.)
B_SPLINE_SURFACE_WITH_KNOTS((4,4),(3,3),(0.,0.000397394373651912),(0.,1.),
 .UNSPECIFIED.)
GEOMETRIC_REPRESENTATION_ITEM()
RATIONAL_B_SPLINE_SURFACE(((1.,0.707106781186552,1.),(1.,0.707752587915898,
1.),(1.,0.708377654540669,1.),(1.,0.708689770883344,1.)))
REPRESENTATION_ITEM('')
SURFACE()
);
#2852=(
BOUNDED_SURFACE()
B_SPLINE_SURFACE(3,2,((#203896,#203897,#203898),(#203899,#203900,#203901),
(#203902,#203903,#203904),(#203905,#203906,#203907)),.UNSPECIFIED.,.F.,
 .F.,.F.)
B_SPLINE_SURFACE_WITH_KNOTS((4,4),(3,3),(0.,0.000511815456479782),(0.,1.00105873160036),
 .UNSPECIFIED.)
GEOMETRIC_REPRESENTATION_ITEM()
RATIONAL_B_SPLINE_SURFACE(((1.,0.708394529056206,1.00061746385385),(1.,
0.708058564166767,1.00061817524714),(1.,0.707430835371931,1.00061950443977),
(1.,0.706796685880258,1.00062084722798)))
REPRESENTATION_ITEM('')
SURFACE()
);
#2853=(
BOUNDED_SURFACE()
B_SPLINE_SURFACE(3,2,((#203913,#203914,#203915),(#203916,#203917,#203918),
(#203919,#203920,#203921),(#203922,#203923,#203924)),.UNSPECIFIED.,.F.,
 .F.,.F.)
B_SPLINE_SURFACE_WITH_KNOTS((4,4),(3,3),(0.,0.000397394465448309),(0.,1.),
 .UNSPECIFIED.)
GEOMETRIC_REPRESENTATION_ITEM()
RATIONAL_B_SPLINE_SURFACE(((1.,0.705498956110771,1.),(1.,0.705821764811772,
1.),(1.,0.706461952521137,1.),(1.,0.707106781186542,1.)))
REPRESENTATION_ITEM('')
SURFACE()
);
#2854=(
BOUNDED_SURFACE()
B_SPLINE_SURFACE(3,2,((#203930,#203931,#203932),(#203933,#203934,#203935),
(#203936,#203937,#203938),(#203939,#203940,#203941)),.UNSPECIFIED.,.F.,
 .F.,.F.)
B_SPLINE_SURFACE_WITH_KNOTS((4,4),(3,3),(0.,0.000397394410828738),(0.,1.),
 .UNSPECIFIED.)
GEOMETRIC_REPRESENTATION_ITEM()
RATIONAL_B_SPLINE_SURFACE(((1.,0.708689770883327,1.),(1.,0.708376440034483,
1.),(1.,0.707750498698405,1.),(1.,0.707106781186548,1.)))
REPRESENTATION_ITEM('')
SURFACE()
);
#2855=(
BOUNDED_SURFACE()
B_SPLINE_SURFACE(3,2,((#203947,#203948,#203949),(#203950,#203951,#203952),
(#203953,#203954,#203955),(#203956,#203957,#203958)),.UNSPECIFIED.,.F.,
 .F.,.F.)
B_SPLINE_SURFACE_WITH_KNOTS((4,4),(3,3),(0.,0.000511815090126174),(0.,1.00105592270161),
 .UNSPECIFIED.)
GEOMETRIC_REPRESENTATION_ITEM()
RATIONAL_B_SPLINE_SURFACE(((1.,0.705266242717667,1.00062243213049),(1.,
0.705584085909315,1.0006217608948),(1.,0.706182089450683,1.00062049800377),
(1.,0.706797508587654,1.0006191983337)))
REPRESENTATION_ITEM('')
SURFACE()
);
#2856=(
BOUNDED_SURFACE()
B_SPLINE_SURFACE(3,2,((#203960,#203961,#203962),(#203963,#203964,#203965),
(#203966,#203967,#203968),(#203969,#203970,#203971)),.UNSPECIFIED.,.F.,
 .F.,.F.)
B_SPLINE_SURFACE_WITH_KNOTS((4,4),(3,3),(0.,0.000397394428086627),(0.,1.),
 .UNSPECIFIED.)
GEOMETRIC_REPRESENTATION_ITEM()
RATIONAL_B_SPLINE_SURFACE(((1.,0.707106781186548,1.),(1.,0.706459846759099,
1.),(1.,0.705820510737275,1.),(1.,0.705498956110758,1.)))
REPRESENTATION_ITEM('')
SURFACE()
);
#2857=(
BOUNDED_SURFACE()
B_SPLINE_SURFACE(3,2,((#203977,#203978,#203979),(#203980,#203981,#203982),
(#203983,#203984,#203985),(#203986,#203987,#203988),(#203989,#203990,#203991),
(#203992,#203993,#203994)),.UNSPECIFIED.,.F.,.F.,.F.)
B_SPLINE_SURFACE_WITH_KNOTS((4,2,4),(3,3),(0.,0.00025795380787285,0.000515907615745701),
(0.,1.),.UNSPECIFIED.)
GEOMETRIC_REPRESENTATION_ITEM()
RATIONAL_B_SPLINE_SURFACE(((1.,0.874619707139387,1.),(1.,0.874834349679026,
1.),(1.,0.854686104157727,1.),(1.,0.79247659791521,1.),(1.,0.750887854595059,
1.),(1.,0.705585838031472,1.)))
REPRESENTATION_ITEM('')
SURFACE()
);
#2858=(
BOUNDED_SURFACE()
B_SPLINE_SURFACE(3,2,((#204000,#204001,#204002),(#204003,#204004,#204005),
(#204006,#204007,#204008),(#204009,#204010,#204011)),.UNSPECIFIED.,.F.,
 .F.,.F.)
B_SPLINE_SURFACE_WITH_KNOTS((4,4),(3,3),(-6.91178884959509E-18,0.000511815437699152),
(0.,1.00105881331612),.UNSPECIFIED.)
GEOMETRIC_REPRESENTATION_ITEM()
RATIONAL_B_SPLINE_SURFACE(((1.,0.706796661946268,1.00062089519732),(1.,
0.707430821225128,1.00061955228474),(1.,0.708058545830661,1.0006182229984),
(1.,0.708394505252647,1.00061751156178)))
REPRESENTATION_ITEM('')
SURFACE()
);
#2859=(
BOUNDED_SURFACE()
B_SPLINE_SURFACE(3,2,((#204013,#204014,#204015),(#204016,#204017,#204018),
(#204019,#204020,#204021),(#204022,#204023,#204024),(#204025,#204026,#204027),
(#204028,#204029,#204030)),.UNSPECIFIED.,.F.,.F.,.F.)
B_SPLINE_SURFACE_WITH_KNOTS((4,2,4),(3,3),(0.,0.000256915317531256,0.000513830635062513),
(0.,1.),.UNSPECIFIED.)
GEOMETRIC_REPRESENTATION_ITEM()
RATIONAL_B_SPLINE_SURFACE(((1.,0.705585838031416,1.),(1.,0.750902433543309,
1.),(1.,0.792329530081767,1.),(1.,0.854288401594944,1.),(1.,0.874998031124557,
1.),(1.,0.874619707139388,1.)))
REPRESENTATION_ITEM('')
SURFACE()
);
#2860=(
BOUNDED_SURFACE()
B_SPLINE_SURFACE(3,2,((#204036,#204037,#204038),(#204039,#204040,#204041),
(#204042,#204043,#204044),(#204045,#204046,#204047),(#204048,#204049,#204050),
(#204051,#204052,#204053)),.UNSPECIFIED.,.F.,.F.,.F.)
B_SPLINE_SURFACE_WITH_KNOTS((4,2,4),(3,3),(-9.86623976961809E-18,0.000256592814262151,
0.000513185628524311),(0.,1.),.UNSPECIFIED.)
GEOMETRIC_REPRESENTATION_ITEM()
RATIONAL_B_SPLINE_SURFACE(((1.,0.708712527163674,1.),(1.,0.753780902613021,
1.),(1.,0.794538995769931,1.),(1.,0.855070770330375,1.),(1.,0.875018427445861,
1.),(1.,0.874619707139398,1.)))
REPRESENTATION_ITEM('')
SURFACE()
);
#2861=(
BOUNDED_SURFACE()
B_SPLINE_SURFACE(3,2,((#204055,#204056,#204057),(#204058,#204059,#204060),
(#204061,#204062,#204063),(#204064,#204065,#204066)),.UNSPECIFIED.,.F.,
 .F.,.F.)
B_SPLINE_SURFACE_WITH_KNOTS((4,4),(3,3),(0.,0.000511815072430404),(0.,1.00105598365858),
 .UNSPECIFIED.)
GEOMETRIC_REPRESENTATION_ITEM()
RATIONAL_B_SPLINE_SURFACE(((1.,0.706797490733775,1.00061923411688),(1.,
0.706182062146654,1.00062053388194),(1.,0.705584062769082,1.00062179683708),
(1.,0.70526622477053,1.00062246810054)))
REPRESENTATION_ITEM('')
SURFACE()
);
#2862=(
BOUNDED_SURFACE()
B_SPLINE_SURFACE(3,2,((#204072,#204073,#204074),(#204075,#204076,#204077),
(#204078,#204079,#204080),(#204081,#204082,#204083),(#204084,#204085,#204086),
(#204087,#204088,#204089)),.UNSPECIFIED.,.F.,.F.,.F.)
B_SPLINE_SURFACE_WITH_KNOTS((4,2,4),(3,3),(-1.68051336735253E-18,0.000257652232350876,
0.000515304464701754),(0.,1.),.UNSPECIFIED.)
GEOMETRIC_REPRESENTATION_ITEM()
RATIONAL_B_SPLINE_SURFACE(((1.,0.874619707139403,1.),(1.,0.874861180431004,
1.),(1.,0.855455725920461,1.),(1.,0.794699358955677,1.),(1.,0.753768977788352,
1.),(1.,0.708712527163669,1.)))
REPRESENTATION_ITEM('')
SURFACE()
);
#2863=(
BOUNDED_SURFACE()
B_SPLINE_SURFACE(3,2,((#204095,#204096,#204097),(#204098,#204099,#204100),
(#204101,#204102,#204103),(#204104,#204105,#204106)),.UNSPECIFIED.,.F.,
 .F.,.F.)
B_SPLINE_SURFACE_WITH_KNOTS((4,4),(3,3),(2.71050543121376E-20,0.000397394373651921),
(0.,1.),.UNSPECIFIED.)
GEOMETRIC_REPRESENTATION_ITEM()
RATIONAL_B_SPLINE_SURFACE(((1.,0.707106781186548,1.),(1.,0.707752587915894,
1.),(1.,0.708377654540691,1.),(1.,0.708689770883335,1.)))
REPRESENTATION_ITEM('')
SURFACE()
);
#2864=(
BOUNDED_SURFACE()
B_SPLINE_SURFACE(3,2,((#204108,#204109,#204110),(#204111,#204112,#204113),
(#204114,#204115,#204116),(#204117,#204118,#204119)),.UNSPECIFIED.,.F.,
 .F.,.F.)
B_SPLINE_SURFACE_WITH_KNOTS((4,4),(3,3),(0.,0.000511815456479785),(0.,1.00105873159947),
 .UNSPECIFIED.)
GEOMETRIC_REPRESENTATION_ITEM()
RATIONAL_B_SPLINE_SURFACE(((1.,0.708394529056476,1.00061746385333),(1.,
0.708058564167017,1.00061817524662),(1.,0.707430835372211,1.00061950443924),
(1.,0.70679668588052,1.00062084722745)))
REPRESENTATION_ITEM('')
SURFACE()
);
#2865=(
BOUNDED_SURFACE()
B_SPLINE_SURFACE(3,2,((#204125,#204126,#204127),(#204128,#204129,#204130),
(#204131,#204132,#204133),(#204134,#204135,#204136)),.UNSPECIFIED.,.F.,
 .F.,.F.)
B_SPLINE_SURFACE_WITH_KNOTS((4,4),(3,3),(0.,0.00039739446544831),(0.,1.),
 .UNSPECIFIED.)
GEOMETRIC_REPRESENTATION_ITEM()
RATIONAL_B_SPLINE_SURFACE(((1.,0.705498956110746,1.),(1.,0.705821764811779,
1.),(1.,0.706461952521139,1.),(1.,0.707106781186548,1.)))
REPRESENTATION_ITEM('')
SURFACE()
);
#2866=(
BOUNDED_SURFACE()
B_SPLINE_SURFACE(3,2,((#204142,#204143,#204144),(#204145,#204146,#204147),
(#204148,#204149,#204150),(#204151,#204152,#204153)),.UNSPECIFIED.,.F.,
 .F.,.F.)
B_SPLINE_SURFACE_WITH_KNOTS((4,4),(3,3),(0.,0.000397394410828733),(0.,1.),
 .UNSPECIFIED.)
GEOMETRIC_REPRESENTATION_ITEM()
RATIONAL_B_SPLINE_SURFACE(((1.,0.708689770883331,1.),(1.,0.708376440034489,
1.),(1.,0.707750498698411,1.),(1.,0.707106781186548,1.)))
REPRESENTATION_ITEM('')
SURFACE()
);
#2867=(
BOUNDED_SURFACE()
B_SPLINE_SURFACE(3,2,((#204159,#204160,#204161),(#204162,#204163,#204164),
(#204165,#204166,#204167),(#204168,#204169,#204170)),.UNSPECIFIED.,.F.,
 .F.,.F.)
B_SPLINE_SURFACE_WITH_KNOTS((4,4),(3,3),(0.,0.000511815090126173),(0.,1.00105592270321),
 .UNSPECIFIED.)
GEOMETRIC_REPRESENTATION_ITEM()
RATIONAL_B_SPLINE_SURFACE(((1.,0.705266242717188,1.00062243213143),(1.,
0.705584085908842,1.00062176089575),(1.,0.706182089450201,1.00062049800472),
(1.,0.706797508587187,1.00061919833464)))
REPRESENTATION_ITEM('')
SURFACE()
);
#2868=(
BOUNDED_SURFACE()
B_SPLINE_SURFACE(3,2,((#204172,#204173,#204174),(#204175,#204176,#204177),
(#204178,#204179,#204180),(#204181,#204182,#204183)),.UNSPECIFIED.,.F.,
 .F.,.F.)
B_SPLINE_SURFACE_WITH_KNOTS((4,4),(3,3),(-6.85757874097082E-18,0.00039739442808662),
(0.,1.),.UNSPECIFIED.)
GEOMETRIC_REPRESENTATION_ITEM()
RATIONAL_B_SPLINE_SURFACE(((1.,0.707106781186548,1.),(1.,0.706459846759094,
1.),(1.,0.705820510737267,1.),(1.,0.705498956110752,1.)))
REPRESENTATION_ITEM('')
SURFACE()
);
#2869=(
BOUNDED_SURFACE()
B_SPLINE_SURFACE(3,2,((#204189,#204190,#204191),(#204192,#204193,#204194),
(#204195,#204196,#204197),(#204198,#204199,#204200),(#204201,#204202,#204203),
(#204204,#204205,#204206)),.UNSPECIFIED.,.F.,.F.,.F.)
B_SPLINE_SURFACE_WITH_KNOTS((4,2,4),(3,3),(0.,0.000257953807872842,0.000515907615745685),
(0.,1.),.UNSPECIFIED.)
GEOMETRIC_REPRESENTATION_ITEM()
RATIONAL_B_SPLINE_SURFACE(((1.,0.874619707139392,1.),(1.,0.874834349678954,
1.),(1.,0.854686104157838,1.),(1.,0.792476597915099,1.),(1.,0.750887854595166,
1.),(1.,0.705585838031451,1.)))
REPRESENTATION_ITEM('')
SURFACE()
);
#2870=(
BOUNDED_SURFACE()
B_SPLINE_SURFACE(3,2,((#204209,#204210,#204211),(#204212,#204213,#204214),
(#204215,#204216,#204217),(#204218,#204219,#204220)),.UNSPECIFIED.,.F.,
 .F.,.F.)
B_SPLINE_SURFACE_WITH_KNOTS((4,4),(3,3),(0.,0.000511815437699147),(0.,1.0010588133146),
 .UNSPECIFIED.)
GEOMETRIC_REPRESENTATION_ITEM()
RATIONAL_B_SPLINE_SURFACE(((1.,0.706796661946711,1.00062089519643),(1.,
0.707430821225589,1.00061955228386),(1.,0.708058545831085,1.00061822299752),
(1.,0.70839450525309,1.0006175115609)))
REPRESENTATION_ITEM('')
SURFACE()
);
#2871=(
BOUNDED_SURFACE()
B_SPLINE_SURFACE(3,2,((#204222,#204223,#204224),(#204225,#204226,#204227),
(#204228,#204229,#204230),(#204231,#204232,#204233),(#204234,#204235,#204236),
(#204237,#204238,#204239)),.UNSPECIFIED.,.F.,.F.,.F.)
B_SPLINE_SURFACE_WITH_KNOTS((4,2,4),(3,3),(0.,0.000256915317531259,0.000513830635062518),
(0.,1.),.UNSPECIFIED.)
GEOMETRIC_REPRESENTATION_ITEM()
RATIONAL_B_SPLINE_SURFACE(((1.,0.705585838031441,1.),(1.,0.750902433542931,
1.),(1.,0.79232953008227,1.),(1.,0.854288401594435,1.),(1.,0.874998031124952,
1.),(1.,0.874619707139392,1.)))
REPRESENTATION_ITEM('')
SURFACE()
);
#2872=(
BOUNDED_SURFACE()
B_SPLINE_SURFACE(3,2,((#204245,#204246,#204247),(#204248,#204249,#204250),
(#204251,#204252,#204253),(#204254,#204255,#204256),(#204257,#204258,#204259),
(#204260,#204261,#204262)),.UNSPECIFIED.,.F.,.F.,.F.)
B_SPLINE_SURFACE_WITH_KNOTS((4,2,4),(3,3),(-1.56396163381034E-17,0.000256592814262148,
0.000513185628524312),(0.,1.),.UNSPECIFIED.)
GEOMETRIC_REPRESENTATION_ITEM()
RATIONAL_B_SPLINE_SURFACE(((1.,0.708712527163647,1.),(1.,0.753780902613552,
1.),(1.,0.794538995769242,1.),(1.,0.85507077033107,1.),(1.,0.875018427445344,
1.),(1.,0.87461970713939,1.)))
REPRESENTATION_ITEM('')
SURFACE()
);
#2873=(
BOUNDED_SURFACE()
B_SPLINE_SURFACE(3,2,((#204263,#204264,#204265),(#204266,#204267,#204268),
(#204269,#204270,#204271),(#204272,#204273,#204274)),.UNSPECIFIED.,.F.,
 .F.,.F.)
B_SPLINE_SURFACE_WITH_KNOTS((4,4),(3,3),(2.71050543121376E-20,0.000511815072430402),
(0.,1.00105598365742),.UNSPECIFIED.)
GEOMETRIC_REPRESENTATION_ITEM()
RATIONAL_B_SPLINE_SURFACE(((1.,0.706797490734113,1.0006192341162),(1.,0.706182062147032,
1.00062053388126),(1.,0.705584062769394,1.0006217968364),(1.,0.705266224770875,
1.00062246809986)))
REPRESENTATION_ITEM('')
SURFACE()
);
#2874=(
BOUNDED_SURFACE()
B_SPLINE_SURFACE(3,2,((#204278,#204279,#204280),(#204281,#204282,#204283),
(#204284,#204285,#204286),(#204287,#204288,#204289),(#204290,#204291,#204292),
(#204293,#204294,#204295)),.UNSPECIFIED.,.F.,.F.,.F.)
B_SPLINE_SURFACE_WITH_KNOTS((4,2,4),(3,3),(0.,0.000257652232350872,0.000515304464701744),
(0.,1.),.UNSPECIFIED.)
GEOMETRIC_REPRESENTATION_ITEM()
RATIONAL_B_SPLINE_SURFACE(((1.,0.874619707139396,1.),(1.,0.874861180430454,
1.),(1.,0.855455725921202,1.),(1.,0.794699358954921,1.),(1.,0.753768977788908,
1.),(1.,0.708712527163673,1.)))
REPRESENTATION_ITEM('')
SURFACE()
);
#2875=(
BOUNDED_SURFACE()
B_SPLINE_SURFACE(3,2,((#204301,#204302,#204303),(#204304,#204305,#204306),
(#204307,#204308,#204309),(#204310,#204311,#204312)),.UNSPECIFIED.,.F.,
 .F.,.F.)
B_SPLINE_SURFACE_WITH_KNOTS((4,4),(3,3),(0.,0.000397394373651912),(0.,1.),
 .UNSPECIFIED.)
GEOMETRIC_REPRESENTATION_ITEM()
RATIONAL_B_SPLINE_SURFACE(((1.,0.707106781186548,1.),(1.,0.707752587915902,
1.),(1.,0.708377654540677,1.),(1.,0.708689770883331,1.)))
REPRESENTATION_ITEM('')
SURFACE()
);
#2876=(
BOUNDED_SURFACE()
B_SPLINE_SURFACE(3,2,((#204314,#204315,#204316),(#204317,#204318,#204319),
(#204320,#204321,#204322),(#204323,#204324,#204325)),.UNSPECIFIED.,.F.,
 .F.,.F.)
B_SPLINE_SURFACE_WITH_KNOTS((4,4),(3,3),(-6.42389787197661E-18,0.000511815456479786),
(0.,1.00105873159963),.UNSPECIFIED.)
GEOMETRIC_REPRESENTATION_ITEM()
RATIONAL_B_SPLINE_SURFACE(((1.,0.708394529056421,1.00061746385343),(1.,
0.708058564166972,1.00061817524672),(1.,0.707430835372151,1.00061950443934),
(1.,0.706796685880471,1.00062084722755)))
REPRESENTATION_ITEM('')
SURFACE()
);
#2877=(
BOUNDED_SURFACE()
B_SPLINE_SURFACE(3,2,((#204331,#204332,#204333),(#204334,#204335,#204336),
(#204337,#204338,#204339),(#204340,#204341,#204342)),.UNSPECIFIED.,.F.,
 .F.,.F.)
B_SPLINE_SURFACE_WITH_KNOTS((4,4),(3,3),(0.,0.000397394465448313),(0.,1.),
 .UNSPECIFIED.)
GEOMETRIC_REPRESENTATION_ITEM()
RATIONAL_B_SPLINE_SURFACE(((1.,0.705498956110752,1.),(1.,0.705821764811779,
1.),(1.,0.706461952521144,1.),(1.,0.707106781186548,1.)))
REPRESENTATION_ITEM('')
SURFACE()
);
#2878=(
BOUNDED_SURFACE()
B_SPLINE_SURFACE(3,2,((#204348,#204349,#204350),(#204351,#204352,#204353),
(#204354,#204355,#204356),(#204357,#204358,#204359)),.UNSPECIFIED.,.F.,
 .F.,.F.)
B_SPLINE_SURFACE_WITH_KNOTS((4,4),(3,3),(0.,0.000397394410828731),(0.,1.),
 .UNSPECIFIED.)
GEOMETRIC_REPRESENTATION_ITEM()
RATIONAL_B_SPLINE_SURFACE(((1.,0.708689770883323,1.),(1.,0.708376440034485,
1.),(1.,0.707750498698409,1.),(1.,0.707106781186548,1.)))
REPRESENTATION_ITEM('')
SURFACE()
);
#2879=(
BOUNDED_SURFACE()
B_SPLINE_SURFACE(3,2,((#204365,#204366,#204367),(#204368,#204369,#204370),
(#204371,#204372,#204373),(#204374,#204375,#204376)),.UNSPECIFIED.,.F.,
 .F.,.F.)
B_SPLINE_SURFACE_WITH_KNOTS((4,4),(3,3),(0.,0.000511815090126173),(0.,1.00105592270208),
 .UNSPECIFIED.)
GEOMETRIC_REPRESENTATION_ITEM()
RATIONAL_B_SPLINE_SURFACE(((1.,0.705266242717525,1.00062243213077),(1.,
0.705584085909185,1.00062176089509),(1.,0.70618208945054,1.00062049800406),
(1.,0.706797508587514,1.00061919833398)))
REPRESENTATION_ITEM('')
SURFACE()
);
#2880=(
BOUNDED_SURFACE()
B_SPLINE_SURFACE(3,2,((#204378,#204379,#204380),(#204381,#204382,#204383),
(#204384,#204385,#204386),(#204387,#204388,#204389)),.UNSPECIFIED.,.F.,
 .F.,.F.)
B_SPLINE_SURFACE_WITH_KNOTS((4,4),(3,3),(-6.88468379528295E-18,0.000397394428086624),
(0.,1.),.UNSPECIFIED.)
GEOMETRIC_REPRESENTATION_ITEM()
RATIONAL_B_SPLINE_SURFACE(((1.,0.707106781186548,1.),(1.,0.706459846759089,
1.),(1.,0.705820510737284,1.),(1.,0.705498956110758,1.)))
REPRESENTATION_ITEM('')
SURFACE()
);
#2881=(
BOUNDED_SURFACE()
B_SPLINE_SURFACE(3,2,((#204395,#204396,#204397),(#204398,#204399,#204400),
(#204401,#204402,#204403),(#204404,#204405,#204406),(#204407,#204408,#204409),
(#204410,#204411,#204412)),.UNSPECIFIED.,.F.,.F.,.F.)
B_SPLINE_SURFACE_WITH_KNOTS((4,2,4),(3,3),(-8.53809210832335E-19,0.000257953807872841,
0.000515907615745682),(0.,1.),.UNSPECIFIED.)
GEOMETRIC_REPRESENTATION_ITEM()
RATIONAL_B_SPLINE_SURFACE(((1.,0.874619707139387,1.),(1.,0.874834349679282,
1.),(1.,0.854686104157425,1.),(1.,0.792476597915532,1.),(1.,0.750887854594857,
1.),(1.,0.705585838031449,1.)))
REPRESENTATION_ITEM('')
SURFACE()
);
#2882=(
BOUNDED_SURFACE()
B_SPLINE_SURFACE(3,2,((#204418,#204419,#204420),(#204421,#204422,#204423),
(#204424,#204425,#204426),(#204427,#204428,#204429)),.UNSPECIFIED.,.F.,
 .F.,.F.)
B_SPLINE_SURFACE_WITH_KNOTS((4,4),(3,3),(0.,0.000511815437699153),(0.,1.00105881331446),
 .UNSPECIFIED.)
GEOMETRIC_REPRESENTATION_ITEM()
RATIONAL_B_SPLINE_SURFACE(((1.,0.706796661946756,1.00062089519635),(1.,
0.707430821225617,1.00061955228377),(1.,0.708058545831129,1.00061822299743),
(1.,0.708394505253124,1.00061751156081)))
REPRESENTATION_ITEM('')
SURFACE()
);
#2883=(
BOUNDED_SURFACE()
B_SPLINE_SURFACE(3,2,((#204431,#204432,#204433),(#204434,#204435,#204436),
(#204437,#204438,#204439),(#204440,#204441,#204442),(#204443,#204444,#204445),
(#204446,#204447,#204448)),.UNSPECIFIED.,.F.,.F.,.F.)
B_SPLINE_SURFACE_WITH_KNOTS((4,2,4),(3,3),(0.,0.000256915317531263,0.000513830635062527),
(0.,1.),.UNSPECIFIED.)
GEOMETRIC_REPRESENTATION_ITEM()
RATIONAL_B_SPLINE_SURFACE(((1.,0.705585838031433,1.),(1.,0.750902433542847,
1.),(1.,0.792329530082374,1.),(1.,0.85428840159432,1.),(1.,0.87499803112506,
1.),(1.,0.874619707139386,1.)))
REPRESENTATION_ITEM('')
SURFACE()
);
#2884=(
BOUNDED_SURFACE()
B_SPLINE_SURFACE(3,2,((#204454,#204455,#204456),(#204457,#204458,#204459),
(#204460,#204461,#204462),(#204463,#204464,#204465),(#204466,#204467,#204468),
(#204469,#204470,#204471)),.UNSPECIFIED.,.F.,.F.,.F.)
B_SPLINE_SURFACE_WITH_KNOTS((4,2,4),(3,3),(-9.62229428080885E-18,0.000256592814262152,
0.000513185628524313),(0.,1.),.UNSPECIFIED.)
GEOMETRIC_REPRESENTATION_ITEM()
RATIONAL_B_SPLINE_SURFACE(((1.,0.708712527163657,1.),(1.,0.753780902613763,
1.),(1.,0.794538995768959,1.),(1.,0.85507077033135,1.),(1.,0.875018427445137,
1.),(1.,0.87461970713939,1.)))
REPRESENTATION_ITEM('')
SURFACE()
);
#2885=(
BOUNDED_SURFACE()
B_SPLINE_SURFACE(3,2,((#204473,#204474,#204475),(#204476,#204477,#204478),
(#204479,#204480,#204481),(#204482,#204483,#204484)),.UNSPECIFIED.,.F.,
 .F.,.F.)
B_SPLINE_SURFACE_WITH_KNOTS((4,4),(3,3),(-6.91178884959509E-18,0.000511815072430389),
(0.,1.00105598365609),.UNSPECIFIED.)
GEOMETRIC_REPRESENTATION_ITEM()
RATIONAL_B_SPLINE_SURFACE(((1.,0.706797490734499,1.00061923411542),(1.,
0.706182062147426,1.00062053388047),(1.,0.705584062769778,1.00062179683561),
(1.,0.70526622477126,1.00062246809908)))
REPRESENTATION_ITEM('')
SURFACE()
);
#2886=(
BOUNDED_SURFACE()
B_SPLINE_SURFACE(3,2,((#204490,#204491,#204492),(#204493,#204494,#204495),
(#204496,#204497,#204498),(#204499,#204500,#204501),(#204502,#204503,#204504),
(#204505,#204506,#204507)),.UNSPECIFIED.,.F.,.F.,.F.)
B_SPLINE_SURFACE_WITH_KNOTS((4,2,4),(3,3),(-2.57498015965307E-18,0.000257652232350874,
0.000515304464701751),(0.,1.),.UNSPECIFIED.)
GEOMETRIC_REPRESENTATION_ITEM()
RATIONAL_B_SPLINE_SURFACE(((1.,0.874619707139391,1.),(1.,0.874861180430997,
1.),(1.,0.855455725920457,1.),(1.,0.794699358955682,1.),(1.,0.753768977788335,
1.),(1.,0.708712527163661,1.)))
REPRESENTATION_ITEM('')
SURFACE()
);
#2887=(
BOUNDED_SURFACE()
B_SPLINE_SURFACE(3,2,((#204513,#204514,#204515),(#204516,#204517,#204518),
(#204519,#204520,#204521),(#204522,#204523,#204524)),.UNSPECIFIED.,.F.,
 .F.,.F.)
B_SPLINE_SURFACE_WITH_KNOTS((4,4),(3,3),(-6.88468379528295E-18,0.000397394373651904),
(0.,1.),.UNSPECIFIED.)
GEOMETRIC_REPRESENTATION_ITEM()
RATIONAL_B_SPLINE_SURFACE(((1.,0.707106781186548,1.),(1.,0.707752587915922,
1.),(1.,0.708377654540658,1.),(1.,0.708689770883355,1.)))
REPRESENTATION_ITEM('')
SURFACE()
);
#2888=(
BOUNDED_SURFACE()
B_SPLINE_SURFACE(3,2,((#204526,#204527,#204528),(#204529,#204530,#204531),
(#204532,#204533,#204534),(#204535,#204536,#204537)),.UNSPECIFIED.,.F.,
 .F.,.F.)
B_SPLINE_SURFACE_WITH_KNOTS((4,4),(3,3),(0.,0.000511815456479787),(0.,1.00105873160033),
 .UNSPECIFIED.)
GEOMETRIC_REPRESENTATION_ITEM()
RATIONAL_B_SPLINE_SURFACE(((1.,0.708394529056224,1.00061746385383),(1.,
0.708058564166761,1.00061817524712),(1.,0.707430835371962,1.00061950443975),
(1.,0.70679668588027,1.00062084722796)))
REPRESENTATION_ITEM('')
SURFACE()
);
#2889=(
BOUNDED_SURFACE()
B_SPLINE_SURFACE(3,2,((#204543,#204544,#204545),(#204546,#204547,#204548),
(#204549,#204550,#204551),(#204552,#204553,#204554)),.UNSPECIFIED.,.F.,
 .F.,.F.)
B_SPLINE_SURFACE_WITH_KNOTS((4,4),(3,3),(0.,0.00039739446544831),(0.,1.),
 .UNSPECIFIED.)
GEOMETRIC_REPRESENTATION_ITEM()
RATIONAL_B_SPLINE_SURFACE(((1.,0.705498956110744,1.),(1.,0.705821764811777,
1.),(1.,0.706461952521137,1.),(1.,0.70710678118655,1.)))
REPRESENTATION_ITEM('')
SURFACE()
);
#2890=(
BOUNDED_SURFACE()
B_SPLINE_SURFACE(3,2,((#204560,#204561,#204562),(#204563,#204564,#204565),
(#204566,#204567,#204568),(#204569,#204570,#204571)),.UNSPECIFIED.,.F.,
 .F.,.F.)
B_SPLINE_SURFACE_WITH_KNOTS((4,4),(3,3),(0.,0.000397394410828739),(0.,1.),
 .UNSPECIFIED.)
GEOMETRIC_REPRESENTATION_ITEM()
RATIONAL_B_SPLINE_SURFACE(((1.,0.708689770883332,1.),(1.,0.708376440034481,
1.),(1.,0.707750498698418,1.),(1.,0.707106781186543,1.)))
REPRESENTATION_ITEM('')
SURFACE()
);
#2891=(
BOUNDED_SURFACE()
B_SPLINE_SURFACE(3,2,((#204577,#204578,#204579),(#204580,#204581,#204582),
(#204583,#204584,#204585),(#204586,#204587,#204588)),.UNSPECIFIED.,.F.,
 .F.,.F.)
B_SPLINE_SURFACE_WITH_KNOTS((4,4),(3,3),(0.,0.000511815090126177),(0.,1.00105592270103),
 .UNSPECIFIED.)
GEOMETRIC_REPRESENTATION_ITEM()
RATIONAL_B_SPLINE_SURFACE(((1.,0.705266242717828,1.00062243213015),(1.,
0.705584085909493,1.00062176089446),(1.,0.706182089450846,1.00062049800343),
(1.,0.706797508587826,1.00061919833336)))
REPRESENTATION_ITEM('')
SURFACE()
);
#2892=(
BOUNDED_SURFACE()
B_SPLINE_SURFACE(3,2,((#204590,#204591,#204592),(#204593,#204594,#204595),
(#204596,#204597,#204598),(#204599,#204600,#204601)),.UNSPECIFIED.,.F.,
 .F.,.F.)
B_SPLINE_SURFACE_WITH_KNOTS((4,4),(3,3),(0.,0.000397394428086622),(0.,1.),
 .UNSPECIFIED.)
GEOMETRIC_REPRESENTATION_ITEM()
RATIONAL_B_SPLINE_SURFACE(((1.,0.707106781186548,1.),(1.,0.706459846759115,
1.),(1.,0.705820510737262,1.),(1.,0.705498956110746,1.)))
REPRESENTATION_ITEM('')
SURFACE()
);
#2893=(
BOUNDED_SURFACE()
B_SPLINE_SURFACE(3,2,((#204607,#204608,#204609),(#204610,#204611,#204612),
(#204613,#204614,#204615),(#204616,#204617,#204618),(#204619,#204620,#204621),
(#204622,#204623,#204624)),.UNSPECIFIED.,.F.,.F.,.F.)
B_SPLINE_SURFACE_WITH_KNOTS((4,2,4),(3,3),(0.,0.000257953807872836,0.000515907615745673),
(0.,1.),.UNSPECIFIED.)
GEOMETRIC_REPRESENTATION_ITEM()
RATIONAL_B_SPLINE_SURFACE(((1.,0.874619707139392,1.),(1.,0.874834349679114,
1.),(1.,0.854686104157613,1.),(1.,0.792476597915356,1.),(1.,0.750887854594963,
1.),(1.,0.70558583803145,1.)))
REPRESENTATION_ITEM('')
SURFACE()
);
#2894=(
BOUNDED_SURFACE()
B_SPLINE_SURFACE(3,2,((#204630,#204631,#204632),(#204633,#204634,#204635),
(#204636,#204637,#204638),(#204639,#204640,#204641)),.UNSPECIFIED.,.F.,
 .F.,.F.)
B_SPLINE_SURFACE_WITH_KNOTS((4,4),(3,3),(0.,0.000511815437699158),(0.,1.00105881331778),
 .UNSPECIFIED.)
GEOMETRIC_REPRESENTATION_ITEM()
RATIONAL_B_SPLINE_SURFACE(((1.,0.70679666194578,1.0006208951983),(1.,0.707430821224659,
1.00061955228572),(1.,0.708058545830176,1.00061822299938),(1.,0.708394505252165,
1.00061751156276)))
REPRESENTATION_ITEM('')
SURFACE()
);
#2895=(
BOUNDED_SURFACE()
B_SPLINE_SURFACE(3,2,((#204643,#204644,#204645),(#204646,#204647,#204648),
(#204649,#204650,#204651),(#204652,#204653,#204654),(#204655,#204656,#204657),
(#204658,#204659,#204660)),.UNSPECIFIED.,.F.,.F.,.F.)
B_SPLINE_SURFACE_WITH_KNOTS((4,2,4),(3,3),(0.,0.000256915317531259,0.000513830635062518),
(0.,1.),.UNSPECIFIED.)
GEOMETRIC_REPRESENTATION_ITEM()
RATIONAL_B_SPLINE_SURFACE(((1.,0.70558583803145,1.),(1.,0.750902433543056,
1.),(1.,0.792329530082105,1.),(1.,0.854288401594614,1.),(1.,0.874998031124823,
1.),(1.,0.874619707139391,1.)))
REPRESENTATION_ITEM('')
SURFACE()
);
#2896=(
BOUNDED_SURFACE()
B_SPLINE_SURFACE(3,2,((#204666,#204667,#204668),(#204669,#204670,#204671),
(#204672,#204673,#204674),(#204675,#204676,#204677),(#204678,#204679,#204680),
(#204681,#204682,#204683)),.UNSPECIFIED.,.F.,.F.,.F.)
B_SPLINE_SURFACE_WITH_KNOTS((4,2,4),(3,3),(0.,0.000256592814262161,0.000513185628524321),
(0.,1.),.UNSPECIFIED.)
GEOMETRIC_REPRESENTATION_ITEM()
RATIONAL_B_SPLINE_SURFACE(((1.,0.708712527163666,1.),(1.,0.753780902613519,
1.),(1.,0.794538995769293,1.),(1.,0.855070770331016,1.),(1.,0.875018427445383,
1.),(1.,0.874619707139399,1.)))
REPRESENTATION_ITEM('')
SURFACE()
);
#2897=(
BOUNDED_SURFACE()
B_SPLINE_SURFACE(3,2,((#204685,#204686,#204687),(#204688,#204689,#204690),
(#204691,#204692,#204693),(#204694,#204695,#204696)),.UNSPECIFIED.,.F.,
 .F.,.F.)
B_SPLINE_SURFACE_WITH_KNOTS((4,4),(3,3),(0.,0.000511815072430401),(0.,1.0010559836559),
 .UNSPECIFIED.)
GEOMETRIC_REPRESENTATION_ITEM()
RATIONAL_B_SPLINE_SURFACE(((1.,0.706797490734558,1.0006192341153),(1.,0.706182062147484,
1.00062053388036),(1.,0.705584062769846,1.0006217968355),(1.,0.705266224771326,
1.00062246809896)))
REPRESENTATION_ITEM('')
SURFACE()
);
#2898=(
BOUNDED_SURFACE()
B_SPLINE_SURFACE(3,2,((#204702,#204703,#204704),(#204705,#204706,#204707),
(#204708,#204709,#204710),(#204711,#204712,#204713),(#204714,#204715,#204716),
(#204717,#204718,#204719)),.UNSPECIFIED.,.F.,.F.,.F.)
B_SPLINE_SURFACE_WITH_KNOTS((4,2,4),(3,3),(-3.40168431617327E-18,0.000257652232350873,
0.000515304464701749),(0.,1.),.UNSPECIFIED.)
GEOMETRIC_REPRESENTATION_ITEM()
RATIONAL_B_SPLINE_SURFACE(((1.,0.874619707139389,1.),(1.,0.874861180430379,
1.),(1.,0.8554557259213,1.),(1.,0.794699358954817,1.),(1.,0.753768977788956,
1.),(1.,0.70871252716369,1.)))
REPRESENTATION_ITEM('')
SURFACE()
);
#2899=(
BOUNDED_SURFACE()
B_SPLINE_SURFACE(3,2,((#204725,#204726,#204727),(#204728,#204729,#204730),
(#204731,#204732,#204733),(#204734,#204735,#204736)),.UNSPECIFIED.,.F.,
 .F.,.F.)
B_SPLINE_SURFACE_WITH_KNOTS((4,4),(3,3),(0.,0.000397394373651924),(0.,1.),
 .UNSPECIFIED.)
GEOMETRIC_REPRESENTATION_ITEM()
RATIONAL_B_SPLINE_SURFACE(((1.,0.707106781186548,1.),(1.,0.7077525879159,
1.),(1.,0.708377654540681,1.),(1.,0.708689770883329,1.)))
REPRESENTATION_ITEM('')
SURFACE()
);
#2900=(
BOUNDED_SURFACE()
B_SPLINE_SURFACE(3,2,((#204738,#204739,#204740),(#204741,#204742,#204743),
(#204744,#204745,#204746),(#204747,#204748,#204749)),.UNSPECIFIED.,.F.,
 .F.,.F.)
B_SPLINE_SURFACE_WITH_KNOTS((4,4),(3,3),(0.,0.000511815456479784),(0.,1.00105873159911),
 .UNSPECIFIED.)
GEOMETRIC_REPRESENTATION_ITEM()
RATIONAL_B_SPLINE_SURFACE(((1.,0.708394529056574,1.00061746385312),(1.,
0.708058564167126,1.00061817524641),(1.,0.707430835372308,1.00061950443903),
(1.,0.706796685880624,1.00062084722724)))
REPRESENTATION_ITEM('')
SURFACE()
);
#2901=(
BOUNDED_SURFACE()
B_SPLINE_SURFACE(3,2,((#204755,#204756,#204757),(#204758,#204759,#204760),
(#204761,#204762,#204763),(#204764,#204765,#204766)),.UNSPECIFIED.,.F.,
 .F.,.F.)
B_SPLINE_SURFACE_WITH_KNOTS((4,4),(3,3),(0.,0.000397394465448322),(0.,1.),
 .UNSPECIFIED.)
GEOMETRIC_REPRESENTATION_ITEM()
RATIONAL_B_SPLINE_SURFACE(((1.,0.705498956110755,1.),(1.,0.705821764811772,
1.),(1.,0.70646195252115,1.),(1.,0.707106781186542,1.)))
REPRESENTATION_ITEM('')
SURFACE()
);
#2902=(
BOUNDED_SURFACE()
B_SPLINE_SURFACE(3,2,((#204772,#204773,#204774),(#204775,#204776,#204777),
(#204778,#204779,#204780),(#204781,#204782,#204783)),.UNSPECIFIED.,.F.,
 .F.,.F.)
B_SPLINE_SURFACE_WITH_KNOTS((4,4),(3,3),(0.,0.00039739441082873),(0.,1.),
 .UNSPECIFIED.)
GEOMETRIC_REPRESENTATION_ITEM()
RATIONAL_B_SPLINE_SURFACE(((1.,0.708689770883327,1.),(1.,0.708376440034489,
1.),(1.,0.707750498698412,1.),(1.,0.707106781186548,1.)))
REPRESENTATION_ITEM('')
SURFACE()
);
#2903=(
BOUNDED_SURFACE()
B_SPLINE_SURFACE(3,2,((#204789,#204790,#204791),(#204792,#204793,#204794),
(#204795,#204796,#204797),(#204798,#204799,#204800)),.UNSPECIFIED.,.F.,
 .F.,.F.)
B_SPLINE_SURFACE_WITH_KNOTS((4,4),(3,3),(0.,0.000511815090126174),(0.,1.0010559227025),
 .UNSPECIFIED.)
GEOMETRIC_REPRESENTATION_ITEM()
RATIONAL_B_SPLINE_SURFACE(((1.,0.705266242717401,1.00062243213101),(1.,
0.70558408590904,1.00062176089533),(1.,0.706182089450421,1.0006204980043),
(1.,0.706797508587395,1.00061919833422)))
REPRESENTATION_ITEM('')
SURFACE()
);
#2904=(
BOUNDED_SURFACE()
B_SPLINE_SURFACE(3,2,((#204802,#204803,#204804),(#204805,#204806,#204807),
(#204808,#204809,#204810),(#204811,#204812,#204813)),.UNSPECIFIED.,.F.,
 .F.,.F.)
B_SPLINE_SURFACE_WITH_KNOTS((4,4),(3,3),(-7.58941520739853E-18,0.000397394428086626),
(0.,1.),.UNSPECIFIED.)
GEOMETRIC_REPRESENTATION_ITEM()
RATIONAL_B_SPLINE_SURFACE(((1.,0.707106781186548,1.),(1.,0.706459846759086,
1.),(1.,0.7058205107373,1.),(1.,0.705498956110753,1.)))
REPRESENTATION_ITEM('')
SURFACE()
);
#2905=(
BOUNDED_SURFACE()
B_SPLINE_SURFACE(3,2,((#204819,#204820,#204821),(#204822,#204823,#204824),
(#204825,#204826,#204827),(#204828,#204829,#204830),(#204831,#204832,#204833),
(#204834,#204835,#204836)),.UNSPECIFIED.,.F.,.F.,.F.)
B_SPLINE_SURFACE_WITH_KNOTS((4,2,4),(3,3),(0.,0.000257953807872849,0.000515907615745699),
(0.,1.),.UNSPECIFIED.)
GEOMETRIC_REPRESENTATION_ITEM()
RATIONAL_B_SPLINE_SURFACE(((1.,0.8746197071394,1.),(1.,0.874834349678804,
1.),(1.,0.854686104158048,1.),(1.,0.792476597914884,1.),(1.,0.750887854595316,
1.),(1.,0.705585838031445,1.)))
REPRESENTATION_ITEM('')
SURFACE()
);
#2906=(
BOUNDED_SURFACE()
B_SPLINE_SURFACE(3,2,((#204842,#204843,#204844),(#204845,#204846,#204847),
(#204848,#204849,#204850),(#204851,#204852,#204853)),.UNSPECIFIED.,.F.,
 .F.,.F.)
B_SPLINE_SURFACE_WITH_KNOTS((4,4),(3,3),(0.,0.000511815437699147),(0.,1.00105881331657),
 .UNSPECIFIED.)
GEOMETRIC_REPRESENTATION_ITEM()
RATIONAL_B_SPLINE_SURFACE(((1.,0.706796661946133,1.00062089519759),(1.,
0.707430821225011,1.00061955228501),(1.,0.708058545830506,1.00061822299867),
(1.,0.708394505252514,1.00061751156205)))
REPRESENTATION_ITEM('')
SURFACE()
);
#2907=(
BOUNDED_SURFACE()
B_SPLINE_SURFACE(3,2,((#204855,#204856,#204857),(#204858,#204859,#204860),
(#204861,#204862,#204863),(#204864,#204865,#204866),(#204867,#204868,#204869),
(#204870,#204871,#204872)),.UNSPECIFIED.,.F.,.F.,.F.)
B_SPLINE_SURFACE_WITH_KNOTS((4,2,4),(3,3),(0.,0.000256915317531268,0.000513830635062536),
(0.,1.),.UNSPECIFIED.)
GEOMETRIC_REPRESENTATION_ITEM()
RATIONAL_B_SPLINE_SURFACE(((1.,0.705585838031441,1.),(1.,0.750902433542207,
1.),(1.,0.792329530083274,1.),(1.,0.854288401593444,1.),(1.,0.87499803112573,
1.),(1.,0.874619707139409,1.)))
REPRESENTATION_ITEM('')
SURFACE()
);
#2908=(
BOUNDED_SURFACE()
B_SPLINE_SURFACE(3,2,((#204878,#204879,#204880),(#204881,#204882,#204883),
(#204884,#204885,#204886),(#204887,#204888,#204889),(#204890,#204891,#204892),
(#204893,#204894,#204895)),.UNSPECIFIED.,.F.,.F.,.F.)
B_SPLINE_SURFACE_WITH_KNOTS((4,2,4),(3,3),(-1.54227759036063E-17,0.000256592814262151,
0.000513185628524318),(0.,1.),.UNSPECIFIED.)
GEOMETRIC_REPRESENTATION_ITEM()
RATIONAL_B_SPLINE_SURFACE(((1.,0.708712527163657,1.),(1.,0.753780902613053,
1.),(1.,0.794538995769901,1.),(1.,0.855070770330395,1.),(1.,0.875018427445846,
1.),(1.,0.874619707139393,1.)))
REPRESENTATION_ITEM('')
SURFACE()
);
#2909=(
BOUNDED_SURFACE()
B_SPLINE_SURFACE(3,2,((#204897,#204898,#204899),(#204900,#204901,#204902),
(#204903,#204904,#204905),(#204906,#204907,#204908)),.UNSPECIFIED.,.F.,
 .F.,.F.)
B_SPLINE_SURFACE_WITH_KNOTS((4,4),(3,3),(0.,0.000511815072430394),(0.,1.00105598365931),
 .UNSPECIFIED.)
GEOMETRIC_REPRESENTATION_ITEM()
RATIONAL_B_SPLINE_SURFACE(((1.,0.706797490733558,1.00061923411731),(1.,
0.706182062146464,1.00062053388237),(1.,0.70558406276884,1.00062179683751),
(1.,0.705266224770311,1.00062246810098)))
REPRESENTATION_ITEM('')
SURFACE()
);
#2910=(
BOUNDED_SURFACE()
B_SPLINE_SURFACE(3,2,((#204914,#204915,#204916),(#204917,#204918,#204919),
(#204920,#204921,#204922),(#204923,#204924,#204925),(#204926,#204927,#204928),
(#204929,#204930,#204931)),.UNSPECIFIED.,.F.,.F.,.F.)
B_SPLINE_SURFACE_WITH_KNOTS((4,2,4),(3,3),(0.,0.000257652232350889,0.000515304464701777),
(0.,1.),.UNSPECIFIED.)
GEOMETRIC_REPRESENTATION_ITEM()
RATIONAL_B_SPLINE_SURFACE(((1.,0.874619707139377,1.),(1.,0.874861180430766,
1.),(1.,0.855455725920758,1.),(1.,0.794699358955338,1.),(1.,0.753768977788568,
1.),(1.,0.708712527163628,1.)))
REPRESENTATION_ITEM('')
SURFACE()
);
#2911=(
BOUNDED_SURFACE()
B_SPLINE_SURFACE(3,2,((#204937,#204938,#204939),(#204940,#204941,#204942),
(#204943,#204944,#204945),(#204946,#204947,#204948)),.UNSPECIFIED.,.F.,
 .F.,.F.)
B_SPLINE_SURFACE_WITH_KNOTS((4,4),(3,3),(0.,0.000397394373651908),(0.,1.),
 .UNSPECIFIED.)
GEOMETRIC_REPRESENTATION_ITEM()
RATIONAL_B_SPLINE_SURFACE(((1.,0.707106781186548,1.),(1.,0.707752587915899,
1.),(1.,0.70837765454067,1.),(1.,0.708689770883335,1.)))
REPRESENTATION_ITEM('')
SURFACE()
);
#2912=(
BOUNDED_SURFACE()
B_SPLINE_SURFACE(3,2,((#204950,#204951,#204952),(#204953,#204954,#204955),
(#204956,#204957,#204958),(#204959,#204960,#204961)),.UNSPECIFIED.,.F.,
 .F.,.F.)
B_SPLINE_SURFACE_WITH_KNOTS((4,4),(3,3),(0.,0.000511815456479795),(0.,1.00105873159874),
 .UNSPECIFIED.)
GEOMETRIC_REPRESENTATION_ITEM()
RATIONAL_B_SPLINE_SURFACE(((1.,0.708394529056711,1.00061746385291),(1.,
0.708058564167178,1.0006181752462),(1.,0.707430835372453,1.00061950443882),
(1.,0.706796685880733,1.00062084722703)))
REPRESENTATION_ITEM('')
SURFACE()
);
#2913=(
BOUNDED_SURFACE()
B_SPLINE_SURFACE(3,2,((#204967,#204968,#204969),(#204970,#204971,#204972),
(#204973,#204974,#204975),(#204976,#204977,#204978)),.UNSPECIFIED.,.F.,
 .F.,.F.)
B_SPLINE_SURFACE_WITH_KNOTS((4,4),(3,3),(0.,0.000397394465448304),(0.,1.),
 .UNSPECIFIED.)
GEOMETRIC_REPRESENTATION_ITEM()
RATIONAL_B_SPLINE_SURFACE(((1.,0.705498956110758,1.),(1.,0.705821764811759,
1.),(1.,0.706461952521154,1.),(1.,0.707106781186542,1.)))
REPRESENTATION_ITEM('')
SURFACE()
);
#2914=(
BOUNDED_SURFACE()
B_SPLINE_SURFACE(3,2,((#204984,#204985,#204986),(#204987,#204988,#204989),
(#204990,#204991,#204992),(#204993,#204994,#204995)),.UNSPECIFIED.,.F.,
 .F.,.F.)
B_SPLINE_SURFACE_WITH_KNOTS((4,4),(3,3),(0.,0.000397394410828734),(0.,1.),
 .UNSPECIFIED.)
GEOMETRIC_REPRESENTATION_ITEM()
RATIONAL_B_SPLINE_SURFACE(((1.,0.708689770883316,1.),(1.,0.708376440034496,
1.),(1.,0.707750498698412,1.),(1.,0.70710678118654,1.)))
REPRESENTATION_ITEM('')
SURFACE()
);
#2915=(
BOUNDED_SURFACE()
B_SPLINE_SURFACE(3,2,((#205001,#205002,#205003),(#205004,#205005,#205006),
(#205007,#205008,#205009),(#205010,#205011,#205012)),.UNSPECIFIED.,.F.,
 .F.,.F.)
B_SPLINE_SURFACE_WITH_KNOTS((4,4),(3,3),(0.,0.00051181509012619),(0.,1.00105592270126),
 .UNSPECIFIED.)
GEOMETRIC_REPRESENTATION_ITEM()
RATIONAL_B_SPLINE_SURFACE(((1.,0.705266242717763,1.00062243213028),(1.,
0.705584085909412,1.0006217608946),(1.,0.706182089450766,1.00062049800357),
(1.,0.706797508587757,1.0006191983335)))
REPRESENTATION_ITEM('')
SURFACE()
);
#2916=(
BOUNDED_SURFACE()
B_SPLINE_SURFACE(3,2,((#205014,#205015,#205016),(#205017,#205018,#205019),
(#205020,#205021,#205022),(#205023,#205024,#205025)),.UNSPECIFIED.,.F.,
 .F.,.F.)
B_SPLINE_SURFACE_WITH_KNOTS((4,4),(3,3),(0.,0.000397394428086627),(0.,1.),
 .UNSPECIFIED.)
GEOMETRIC_REPRESENTATION_ITEM()
RATIONAL_B_SPLINE_SURFACE(((1.,0.707106781186556,1.),(1.,0.706459846759089,
1.),(1.,0.705820510737293,1.),(1.,0.705498956110747,1.)))
REPRESENTATION_ITEM('')
SURFACE()
);
#2917=(
BOUNDED_SURFACE()
B_SPLINE_SURFACE(3,2,((#205031,#205032,#205033),(#205034,#205035,#205036),
(#205037,#205038,#205039),(#205040,#205041,#205042),(#205043,#205044,#205045),
(#205046,#205047,#205048)),.UNSPECIFIED.,.F.,.F.,.F.)
B_SPLINE_SURFACE_WITH_KNOTS((4,2,4),(3,3),(0.,0.000257953807872847,0.000515907615745694),
(0.,1.),.UNSPECIFIED.)
GEOMETRIC_REPRESENTATION_ITEM()
RATIONAL_B_SPLINE_SURFACE(((1.,0.874619707139388,1.),(1.,0.874834349679306,
1.),(1.,0.85468610415739,1.),(1.,0.792476597915524,1.),(1.,0.750887854594873,
1.),(1.,0.705585838031412,1.)))
REPRESENTATION_ITEM('')
SURFACE()
);
#2918=(
BOUNDED_SURFACE()
B_SPLINE_SURFACE(3,2,((#205054,#205055,#205056),(#205057,#205058,#205059),
(#205060,#205061,#205062),(#205063,#205064,#205065)),.UNSPECIFIED.,.F.,
 .F.,.F.)
B_SPLINE_SURFACE_WITH_KNOTS((4,4),(3,3),(0.,0.000511815437699146),(0.,1.00105881331706),
 .UNSPECIFIED.)
GEOMETRIC_REPRESENTATION_ITEM()
RATIONAL_B_SPLINE_SURFACE(((1.,0.706796661945993,1.00062089519787),(1.,
0.707430821224858,1.00061955228529),(1.,0.708058545830395,1.00061822299895),
(1.,0.708394505252372,1.00061751156233)))
REPRESENTATION_ITEM('')
SURFACE()
);
#2919=(
BOUNDED_SURFACE()
B_SPLINE_SURFACE(3,2,((#205067,#205068,#205069),(#205070,#205071,#205072),
(#205073,#205074,#205075),(#205076,#205077,#205078),(#205079,#205080,#205081),
(#205082,#205083,#205084)),.UNSPECIFIED.,.F.,.F.,.F.)
B_SPLINE_SURFACE_WITH_KNOTS((4,2,4),(3,3),(0.,0.000256915317531268,0.000513830635062537),
(0.,1.),.UNSPECIFIED.)
GEOMETRIC_REPRESENTATION_ITEM()
RATIONAL_B_SPLINE_SURFACE(((1.,0.705585838031444,1.),(1.,0.750902433542666,
1.),(1.,0.792329530082642,1.),(1.,0.854288401594098,1.),(1.,0.874998031125232,
1.),(1.,0.874619707139418,1.)))
REPRESENTATION_ITEM('')
SURFACE()
);
#2920=(
BOUNDED_SURFACE()
B_SPLINE_SURFACE(3,2,((#205090,#205091,#205092),(#205093,#205094,#205095),
(#205096,#205097,#205098),(#205099,#205100,#205101),(#205102,#205103,#205104),
(#205105,#205106,#205107)),.UNSPECIFIED.,.F.,.F.,.F.)
B_SPLINE_SURFACE_WITH_KNOTS((4,2,4),(3,3),(-9.59518922649671E-18,0.000256592814262151,
0.000513185628524311),(0.,1.),.UNSPECIFIED.)
GEOMETRIC_REPRESENTATION_ITEM()
RATIONAL_B_SPLINE_SURFACE(((1.,0.70871252716365,1.),(1.,0.753780902613946,
1.),(1.,0.794538995768726,1.),(1.,0.855070770331594,1.),(1.,0.875018427444952,
1.),(1.,0.874619707139389,1.)))
REPRESENTATION_ITEM('')
SURFACE()
);
#2921=(
BOUNDED_SURFACE()
B_SPLINE_SURFACE(3,2,((#205109,#205110,#205111),(#205112,#205113,#205114),
(#205115,#205116,#205117),(#205118,#205119,#205120)),.UNSPECIFIED.,.F.,
 .F.,.F.)
B_SPLINE_SURFACE_WITH_KNOTS((4,4),(3,3),(0.,0.000511815072430389),(0.,1.00105598365899),
 .UNSPECIFIED.)
GEOMETRIC_REPRESENTATION_ITEM()
RATIONAL_B_SPLINE_SURFACE(((1.,0.706797490733651,1.00061923411712),(1.,
0.706182062146583,1.00062053388218),(1.,0.705584062768932,1.00062179683732),
(1.,0.705266224770413,1.00062246810079)))
REPRESENTATION_ITEM('')
SURFACE()
);
#2922=(
BOUNDED_SURFACE()
B_SPLINE_SURFACE(3,2,((#205126,#205127,#205128),(#205129,#205130,#205131),
(#205132,#205133,#205134),(#205135,#205136,#205137),(#205138,#205139,#205140),
(#205141,#205142,#205143)),.UNSPECIFIED.,.F.,.F.,.F.)
B_SPLINE_SURFACE_WITH_KNOTS((4,2,4),(3,3),(-1.35525271560688E-20,0.000257652232350883,
0.000515304464701766),(0.,1.),.UNSPECIFIED.)
GEOMETRIC_REPRESENTATION_ITEM()
RATIONAL_B_SPLINE_SURFACE(((1.,0.874619707139374,1.),(1.,0.874861180430592,
1.),(1.,0.855455725921011,1.),(1.,0.794699358955083,1.),(1.,0.753768977788722,
1.),(1.,0.708712527163651,1.)))
REPRESENTATION_ITEM('')
SURFACE()
);
#2923=(
BOUNDED_SURFACE()
B_SPLINE_SURFACE(3,2,((#205149,#205150,#205151),(#205152,#205153,#205154),
(#205155,#205156,#205157),(#205158,#205159,#205160)),.UNSPECIFIED.,.F.,
 .F.,.F.)
B_SPLINE_SURFACE_WITH_KNOTS((4,4),(3,3),(-1.52601455777335E-17,0.000397394373651901),
(0.,1.),.UNSPECIFIED.)
GEOMETRIC_REPRESENTATION_ITEM()
RATIONAL_B_SPLINE_SURFACE(((1.,0.707106781186547,1.),(1.,0.707752587915871,
1.),(1.,0.708377654540695,1.),(1.,0.708689770883342,1.)))
REPRESENTATION_ITEM('')
SURFACE()
);
#2924=(
BOUNDED_SURFACE()
B_SPLINE_SURFACE(3,2,((#205162,#205163,#205164),(#205165,#205166,#205167),
(#205168,#205169,#205170),(#205171,#205172,#205173)),.UNSPECIFIED.,.F.,
 .F.,.F.)
B_SPLINE_SURFACE_WITH_KNOTS((4,4),(3,3),(0.,0.000511815456479782),(0.,1.00105873159867),
 .UNSPECIFIED.)
GEOMETRIC_REPRESENTATION_ITEM()
RATIONAL_B_SPLINE_SURFACE(((1.,0.708394529056701,1.00061746385287),(1.,
0.708058564167264,1.00061817524616),(1.,0.707430835372431,1.00061950443878),
(1.,0.706796685880745,1.00062084722699)))
REPRESENTATION_ITEM('')
SURFACE()
);
#2925=(
BOUNDED_SURFACE()
B_SPLINE_SURFACE(3,2,((#205179,#205180,#205181),(#205182,#205183,#205184),
(#205185,#205186,#205187),(#205188,#205189,#205190)),.UNSPECIFIED.,.F.,
 .F.,.F.)
B_SPLINE_SURFACE_WITH_KNOTS((4,4),(3,3),(0.,0.000397394465448317),(0.,1.),
 .UNSPECIFIED.)
GEOMETRIC_REPRESENTATION_ITEM()
RATIONAL_B_SPLINE_SURFACE(((1.,0.705498956110763,1.),(1.,0.705821764811761,
1.),(1.,0.706461952521164,1.),(1.,0.707106781186548,1.)))
REPRESENTATION_ITEM('')
SURFACE()
);
#2926=(
BOUNDED_SURFACE()
B_SPLINE_SURFACE(3,2,((#205196,#205197,#205198),(#205199,#205200,#205201),
(#205202,#205203,#205204),(#205205,#205206,#205207)),.UNSPECIFIED.,.F.,
 .F.,.F.)
B_SPLINE_SURFACE_WITH_KNOTS((4,4),(3,3),(0.,0.000397394410828733),(0.,1.),
 .UNSPECIFIED.)
GEOMETRIC_REPRESENTATION_ITEM()
RATIONAL_B_SPLINE_SURFACE(((1.,0.708689770883334,1.),(1.,0.708376440034487,
1.),(1.,0.707750498698412,1.),(1.,0.707106781186548,1.)))
REPRESENTATION_ITEM('')
SURFACE()
);
#2927=(
BOUNDED_SURFACE()
B_SPLINE_SURFACE(3,2,((#205213,#205214,#205215),(#205216,#205217,#205218),
(#205219,#205220,#205221),(#205222,#205223,#205224)),.UNSPECIFIED.,.F.,
 .F.,.F.)
B_SPLINE_SURFACE_WITH_KNOTS((4,4),(3,3),(0.,0.000511815090126187),(0.,1.00105592270036),
 .UNSPECIFIED.)
GEOMETRIC_REPRESENTATION_ITEM()
RATIONAL_B_SPLINE_SURFACE(((1.,0.705266242718023,1.00062243212976),(1.,
0.705584085909673,1.00062176089407),(1.,0.706182089451057,1.00062049800304),
(1.,0.70679750858802,1.00061919833297)))
REPRESENTATION_ITEM('')
SURFACE()
);
#2928=(
BOUNDED_SURFACE()
B_SPLINE_SURFACE(3,2,((#205226,#205227,#205228),(#205229,#205230,#205231),
(#205232,#205233,#205234),(#205235,#205236,#205237)),.UNSPECIFIED.,.F.,
 .F.,.F.)
B_SPLINE_SURFACE_WITH_KNOTS((4,4),(3,3),(0.,0.000397394428086623),(0.,1.),
 .UNSPECIFIED.)
GEOMETRIC_REPRESENTATION_ITEM()
RATIONAL_B_SPLINE_SURFACE(((1.,0.707106781186548,1.),(1.,0.706459846759091,
1.),(1.,0.705820510737279,1.),(1.,0.705498956110749,1.)))
REPRESENTATION_ITEM('')
SURFACE()
);
#2929=(
BOUNDED_SURFACE()
B_SPLINE_SURFACE(3,2,((#205243,#205244,#205245),(#205246,#205247,#205248),
(#205249,#205250,#205251),(#205252,#205253,#205254),(#205255,#205256,#205257),
(#205258,#205259,#205260)),.UNSPECIFIED.,.F.,.F.,.F.)
B_SPLINE_SURFACE_WITH_KNOTS((4,2,4),(3,3),(0.,0.000257953807872846,0.000515907615745693),
(0.,1.),.UNSPECIFIED.)
GEOMETRIC_REPRESENTATION_ITEM()
RATIONAL_B_SPLINE_SURFACE(((1.,0.874619707139391,1.),(1.,0.874834349679337,
1.),(1.,0.854686104157324,1.),(1.,0.792476597915613,1.),(1.,0.750887854594759,
1.),(1.,0.705585838031461,1.)))
REPRESENTATION_ITEM('')
SURFACE()
);
#2930=(
BOUNDED_SURFACE()
B_SPLINE_SURFACE(3,2,((#205266,#205267,#205268),(#205269,#205270,#205271),
(#205272,#205273,#205274),(#205275,#205276,#205277)),.UNSPECIFIED.,.F.,
 .F.,.F.)
B_SPLINE_SURFACE_WITH_KNOTS((4,4),(3,3),(0.,0.000511815437699162),(0.,1.00105881331649),
 .UNSPECIFIED.)
GEOMETRIC_REPRESENTATION_ITEM()
RATIONAL_B_SPLINE_SURFACE(((1.,0.706796661946159,1.00062089519754),(1.,
0.707430821225023,1.00061955228496),(1.,0.708058545830554,1.00061822299862),
(1.,0.708394505252524,1.000617511562)))
REPRESENTATION_ITEM('')
SURFACE()
);
#2931=(
BOUNDED_SURFACE()
B_SPLINE_SURFACE(3,2,((#205279,#205280,#205281),(#205282,#205283,#205284),
(#205285,#205286,#205287),(#205288,#205289,#205290),(#205291,#205292,#205293),
(#205294,#205295,#205296)),.UNSPECIFIED.,.F.,.F.,.F.)
B_SPLINE_SURFACE_WITH_KNOTS((4,2,4),(3,3),(0.,0.000256915317531264,0.000513830635062528),
(0.,1.),.UNSPECIFIED.)
GEOMETRIC_REPRESENTATION_ITEM()
RATIONAL_B_SPLINE_SURFACE(((1.,0.705585838031427,1.),(1.,0.750902433542537,
1.),(1.,0.792329530082828,1.),(1.,0.854288401593886,1.),(1.,0.874998031125381,
1.),(1.,0.874619707139383,1.)))
REPRESENTATION_ITEM('')
SURFACE()
);
#2932=(
BOUNDED_SURFACE()
B_SPLINE_SURFACE(3,2,((#205302,#205303,#205304),(#205305,#205306,#205307),
(#205308,#205309,#205310),(#205311,#205312,#205313),(#205314,#205315,#205316),
(#205317,#205318,#205319)),.UNSPECIFIED.,.F.,.F.,.F.)
B_SPLINE_SURFACE_WITH_KNOTS((4,2,4),(3,3),(-5.77337656848531E-18,0.000256592814262161,
0.000513185628524327),(0.,1.),.UNSPECIFIED.)
GEOMETRIC_REPRESENTATION_ITEM()
RATIONAL_B_SPLINE_SURFACE(((1.,0.708712527163664,1.),(1.,0.753780902613862,
1.),(1.,0.79453899576885,1.),(1.,0.855070770331452,1.),(1.,0.875018427445077,
1.),(1.,0.874619707139383,1.)))
REPRESENTATION_ITEM('')
SURFACE()
);
#2933=(
BOUNDED_SURFACE()
B_SPLINE_SURFACE(3,2,((#205321,#205322,#205323),(#205324,#205325,#205326),
(#205327,#205328,#205329),(#205330,#205331,#205332)),.UNSPECIFIED.,.F.,
 .F.,.F.)
B_SPLINE_SURFACE_WITH_KNOTS((4,4),(3,3),(0.,0.000511815072430397),(0.,1.00105598365653),
 .UNSPECIFIED.)
GEOMETRIC_REPRESENTATION_ITEM()
RATIONAL_B_SPLINE_SURFACE(((1.,0.706797490734371,1.00061923411568),(1.,
0.706182062147292,1.00062053388074),(1.,0.705584062769647,1.00062179683588),
(1.,0.705266224771127,1.00062246809934)))
REPRESENTATION_ITEM('')
SURFACE()
);
#2934=(
BOUNDED_SURFACE()
B_SPLINE_SURFACE(3,2,((#205338,#205339,#205340),(#205341,#205342,#205343),
(#205344,#205345,#205346),(#205347,#205348,#205349),(#205350,#205351,#205352),
(#205353,#205354,#205355)),.UNSPECIFIED.,.F.,.F.,.F.)
B_SPLINE_SURFACE_WITH_KNOTS((4,2,4),(3,3),(0.,0.000257652232350883,0.000515304464701766),
(0.,1.),.UNSPECIFIED.)
GEOMETRIC_REPRESENTATION_ITEM()
RATIONAL_B_SPLINE_SURFACE(((1.,0.874619707139394,1.),(1.,0.874861180431301,
1.),(1.,0.855455725920046,1.),(1.,0.794699358956096,1.),(1.,0.753768977788045,
1.),(1.,0.708712527163649,1.)))
REPRESENTATION_ITEM('')
SURFACE()
);
#2935=(
BOUNDED_SURFACE()
B_SPLINE_SURFACE(3,2,((#205361,#205362,#205363),(#205364,#205365,#205366),
(#205367,#205368,#205369),(#205370,#205371,#205372)),.UNSPECIFIED.,.F.,
 .F.,.F.)
B_SPLINE_SURFACE_WITH_KNOTS((4,4),(3,3),(0.,0.000397394373651916),(0.,1.),
 .UNSPECIFIED.)
GEOMETRIC_REPRESENTATION_ITEM()
RATIONAL_B_SPLINE_SURFACE(((1.,0.707106781186546,1.),(1.,0.707752587915909,
1.),(1.,0.708377654540654,1.),(1.,0.708689770883326,1.)))
REPRESENTATION_ITEM('')
SURFACE()
);
#2936=(
BOUNDED_SURFACE()
B_SPLINE_SURFACE(3,2,((#205374,#205375,#205376),(#205377,#205378,#205379),
(#205380,#205381,#205382),(#205383,#205384,#205385)),.UNSPECIFIED.,.F.,
 .F.,.F.)
B_SPLINE_SURFACE_WITH_KNOTS((4,4),(3,3),(0.,0.000511815456479791),(0.,1.00105873159914),
 .UNSPECIFIED.)
GEOMETRIC_REPRESENTATION_ITEM()
RATIONAL_B_SPLINE_SURFACE(((1.,0.708394529056566,1.00061746385314),(1.,
0.708058564167089,1.00061817524643),(1.,0.707430835372312,1.00061950443905),
(1.,0.706796685880615,1.00062084722726)))
REPRESENTATION_ITEM('')
SURFACE()
);
#2937=(
BOUNDED_SURFACE()
B_SPLINE_SURFACE(3,2,((#205391,#205392,#205393),(#205394,#205395,#205396),
(#205397,#205398,#205399),(#205400,#205401,#205402)),.UNSPECIFIED.,.F.,
 .F.,.F.)
B_SPLINE_SURFACE_WITH_KNOTS((4,4),(3,3),(0.,0.000397394465448314),(0.,1.),
 .UNSPECIFIED.)
GEOMETRIC_REPRESENTATION_ITEM()
RATIONAL_B_SPLINE_SURFACE(((1.,0.705498956110748,1.),(1.,0.705821764811775,
1.),(1.,0.706461952521155,1.),(1.,0.707106781186531,1.)))
REPRESENTATION_ITEM('')
SURFACE()
);
#2938=(
BOUNDED_SURFACE()
B_SPLINE_SURFACE(3,2,((#205408,#205409,#205410),(#205411,#205412,#205413),
(#205414,#205415,#205416),(#205417,#205418,#205419)),.UNSPECIFIED.,.F.,
 .F.,.F.)
B_SPLINE_SURFACE_WITH_KNOTS((4,4),(3,3),(0.,0.000397394410828728),(0.,1.),
 .UNSPECIFIED.)
GEOMETRIC_REPRESENTATION_ITEM()
RATIONAL_B_SPLINE_SURFACE(((1.,0.708689770883322,1.),(1.,0.708376440034482,
1.),(1.,0.707750498698425,1.),(1.,0.707106781186525,1.)))
REPRESENTATION_ITEM('')
SURFACE()
);
#2939=(
BOUNDED_SURFACE()
B_SPLINE_SURFACE(3,2,((#205425,#205426,#205427),(#205428,#205429,#205430),
(#205431,#205432,#205433),(#205434,#205435,#205436)),.UNSPECIFIED.,.F.,
 .F.,.F.)
B_SPLINE_SURFACE_WITH_KNOTS((4,4),(3,3),(0.,0.000511815090126179),(0.,1.00105592269913),
 .UNSPECIFIED.)
GEOMETRIC_REPRESENTATION_ITEM()
RATIONAL_B_SPLINE_SURFACE(((1.,0.705266242718401,1.00062243212903),(1.,
0.705584085910067,1.00062176089334),(1.,0.706182089451372,1.00062049800232),
(1.,0.706797508588382,1.00061919833224)))
REPRESENTATION_ITEM('')
SURFACE()
);
#2940=(
BOUNDED_SURFACE()
B_SPLINE_SURFACE(3,2,((#205438,#205439,#205440),(#205441,#205442,#205443),
(#205444,#205445,#205446),(#205447,#205448,#205449)),.UNSPECIFIED.,.F.,
 .F.,.F.)
B_SPLINE_SURFACE_WITH_KNOTS((4,4),(3,3),(0.,0.000397394428086626),(0.,1.),
 .UNSPECIFIED.)
GEOMETRIC_REPRESENTATION_ITEM()
RATIONAL_B_SPLINE_SURFACE(((1.,0.707106781186536,1.),(1.,0.706459846759119,
1.),(1.,0.705820510737292,1.),(1.,0.705498956110736,1.)))
REPRESENTATION_ITEM('')
SURFACE()
);
#2941=(
BOUNDED_SURFACE()
B_SPLINE_SURFACE(3,2,((#205455,#205456,#205457),(#205458,#205459,#205460),
(#205461,#205462,#205463),(#205464,#205465,#205466),(#205467,#205468,#205469),
(#205470,#205471,#205472)),.UNSPECIFIED.,.F.,.F.,.F.)
B_SPLINE_SURFACE_WITH_KNOTS((4,2,4),(3,3),(0.,0.000257953807872847,0.000515907615745694),
(0.,1.),.UNSPECIFIED.)
GEOMETRIC_REPRESENTATION_ITEM()
RATIONAL_B_SPLINE_SURFACE(((1.,0.874619707139395,1.),(1.,0.874834349679049,
1.),(1.,0.854686104157715,1.),(1.,0.792476597915225,1.),(1.,0.750887854595061,
1.),(1.,0.705585838031448,1.)))
REPRESENTATION_ITEM('')
SURFACE()
);
#2942=(
BOUNDED_SURFACE()
B_SPLINE_SURFACE(3,2,((#205478,#205479,#205480),(#205481,#205482,#205483),
(#205484,#205485,#205486),(#205487,#205488,#205489)),.UNSPECIFIED.,.F.,
 .F.,.F.)
B_SPLINE_SURFACE_WITH_KNOTS((4,4),(3,3),(0.,0.00051181543769915),(0.,1.00105881331433),
 .UNSPECIFIED.)
GEOMETRIC_REPRESENTATION_ITEM()
RATIONAL_B_SPLINE_SURFACE(((1.,0.706796661946792,1.00062089519627),(1.,
0.707430821225683,1.0006195522837),(1.,0.708058545831151,1.00061822299736),
(1.,0.708394505253171,1.00061751156074)))
REPRESENTATION_ITEM('')
SURFACE()
);
#2943=(
BOUNDED_SURFACE()
B_SPLINE_SURFACE(3,2,((#205491,#205492,#205493),(#205494,#205495,#205496),
(#205497,#205498,#205499),(#205500,#205501,#205502),(#205503,#205504,#205505),
(#205506,#205507,#205508)),.UNSPECIFIED.,.F.,.F.,.F.)
B_SPLINE_SURFACE_WITH_KNOTS((4,2,4),(3,3),(0.,0.000256915317531265,0.00051383063506253),
(0.,1.),.UNSPECIFIED.)
GEOMETRIC_REPRESENTATION_ITEM()
RATIONAL_B_SPLINE_SURFACE(((1.,0.705585838031436,1.),(1.,0.7509024335433,
1.),(1.,0.792329530081799,1.),(1.,0.854288401594921,1.),(1.,0.874998031124604,
1.),(1.,0.874619707139392,1.)))
REPRESENTATION_ITEM('')
SURFACE()
);
#2944=(
BOUNDED_SURFACE()
B_SPLINE_SURFACE(3,2,((#205514,#205515,#205516),(#205517,#205518,#205519),
(#205520,#205521,#205522),(#205523,#205524,#205525),(#205526,#205527,#205528),
(#205529,#205530,#205531)),.UNSPECIFIED.,.F.,.F.,.F.)
B_SPLINE_SURFACE_WITH_KNOTS((4,2,4),(3,3),(0.,0.000256592814262157,0.000513185628524315),
(0.,1.),.UNSPECIFIED.)
GEOMETRIC_REPRESENTATION_ITEM()
RATIONAL_B_SPLINE_SURFACE(((1.,0.708712527163664,1.),(1.,0.753780902613349,
1.),(1.,0.794538995769515,1.),(1.,0.855070770330789,1.),(1.,0.875018427445547,
1.),(1.,0.874619707139392,1.)))
REPRESENTATION_ITEM('')
SURFACE()
);
#2945=(
BOUNDED_SURFACE()
B_SPLINE_SURFACE(3,2,((#205533,#205534,#205535),(#205536,#205537,#205538),
(#205539,#205540,#205541),(#205542,#205543,#205544)),.UNSPECIFIED.,.F.,
 .F.,.F.)
B_SPLINE_SURFACE_WITH_KNOTS((4,4),(3,3),(0.,0.000511815072430392),(0.,1.00105598365706),
 .UNSPECIFIED.)
GEOMETRIC_REPRESENTATION_ITEM()
RATIONAL_B_SPLINE_SURFACE(((1.,0.706797490734217,1.00061923411599),(1.,
0.706182062147139,1.00062053388105),(1.,0.705584062769492,1.00062179683619),
(1.,0.705266224770975,1.00062246809965)))
REPRESENTATION_ITEM('')
SURFACE()
);
#2946=(
BOUNDED_SURFACE()
B_SPLINE_SURFACE(3,2,((#205550,#205551,#205552),(#205553,#205554,#205555),
(#205556,#205557,#205558),(#205559,#205560,#205561),(#205562,#205563,#205564),
(#205565,#205566,#205567)),.UNSPECIFIED.,.F.,.F.,.F.)
B_SPLINE_SURFACE_WITH_KNOTS((4,2,4),(3,3),(0.,0.000257652232350882,0.000515304464701764),
(0.,1.),.UNSPECIFIED.)
GEOMETRIC_REPRESENTATION_ITEM()
RATIONAL_B_SPLINE_SURFACE(((1.,0.874619707139393,1.),(1.,0.874861180431177,
1.),(1.,0.855455725920209,1.),(1.,0.794699358955939,1.),(1.,0.7537689777881,
1.),(1.,0.70871252716366,1.)))
REPRESENTATION_ITEM('')
SURFACE()
);
#2947=(
BOUNDED_SURFACE()
B_SPLINE_SURFACE(3,2,((#205573,#205574,#205575),(#205576,#205577,#205578),
(#205579,#205580,#205581),(#205582,#205583,#205584)),.UNSPECIFIED.,.F.,
 .F.,.F.)
B_SPLINE_SURFACE_WITH_KNOTS((4,4),(3,3),(-9.56808417218458E-18,0.000397394373651918),
(0.,1.),.UNSPECIFIED.)
GEOMETRIC_REPRESENTATION_ITEM()
RATIONAL_B_SPLINE_SURFACE(((1.,0.707106781186559,1.),(1.,0.707752587915889,
1.),(1.,0.708377654540676,1.),(1.,0.708689770883342,1.)))
REPRESENTATION_ITEM('')
SURFACE()
);
#2948=(
BOUNDED_SURFACE()
B_SPLINE_SURFACE(3,2,((#205586,#205587,#205588),(#205589,#205590,#205591),
(#205592,#205593,#205594),(#205595,#205596,#205597)),.UNSPECIFIED.,.F.,
 .F.,.F.)
B_SPLINE_SURFACE_WITH_KNOTS((4,4),(3,3),(0.,0.000511815456479788),(0.,1.00105873160029),
 .UNSPECIFIED.)
GEOMETRIC_REPRESENTATION_ITEM()
RATIONAL_B_SPLINE_SURFACE(((1.,0.70839452905621,1.00061746385381),(1.,0.708058564166803,
1.0006181752471),(1.,0.707430835371955,1.00061950443973),(1.,0.706796685880289,
1.00062084722794)))
REPRESENTATION_ITEM('')
SURFACE()
);
#2949=(
BOUNDED_SURFACE()
B_SPLINE_SURFACE(3,2,((#205603,#205604,#205605),(#205606,#205607,#205608),
(#205609,#205610,#205611),(#205612,#205613,#205614)),.UNSPECIFIED.,.F.,
 .F.,.F.)
B_SPLINE_SURFACE_WITH_KNOTS((4,4),(3,3),(-6.53231808922516E-18,0.000397394465448321),
(0.,1.),.UNSPECIFIED.)
GEOMETRIC_REPRESENTATION_ITEM()
RATIONAL_B_SPLINE_SURFACE(((1.,0.705498956110736,1.),(1.,0.705821764811783,
1.),(1.,0.706461952521136,1.),(1.,0.707106781186559,1.)))
REPRESENTATION_ITEM('')
SURFACE()
);
#2950=(
BOUNDED_SURFACE()
B_SPLINE_SURFACE(3,2,((#205620,#205621,#205622),(#205623,#205624,#205625),
(#205626,#205627,#205628),(#205629,#205630,#205631)),.UNSPECIFIED.,.F.,
 .F.,.F.)
B_SPLINE_SURFACE_WITH_KNOTS((4,4),(3,3),(0.,0.000397394410828731),(0.,1.),
 .UNSPECIFIED.)
GEOMETRIC_REPRESENTATION_ITEM()
RATIONAL_B_SPLINE_SURFACE(((1.,0.708689770883326,1.),(1.,0.708376440034496,
1.),(1.,0.707750498698427,1.),(1.,0.707106781186548,1.)))
REPRESENTATION_ITEM('')
SURFACE()
);
#2951=(
BOUNDED_SURFACE()
B_SPLINE_SURFACE(3,2,((#205637,#205638,#205639),(#205640,#205641,#205642),
(#205643,#205644,#205645),(#205646,#205647,#205648)),.UNSPECIFIED.,.F.,
 .F.,.F.)
B_SPLINE_SURFACE_WITH_KNOTS((4,4),(3,3),(0.,0.000511815090126171),(0.,1.0010559227001),
 .UNSPECIFIED.)
GEOMETRIC_REPRESENTATION_ITEM()
RATIONAL_B_SPLINE_SURFACE(((1.,0.705266242718086,1.0006224321296),(1.,0.705584085909776,
1.00062176089391),(1.,0.706182089451097,1.00062049800289),(1.,0.706797508588098,
1.00061919833281)))
REPRESENTATION_ITEM('')
SURFACE()
);
#2952=(
BOUNDED_SURFACE()
B_SPLINE_SURFACE(3,2,((#205650,#205651,#205652),(#205653,#205654,#205655),
(#205656,#205657,#205658),(#205659,#205660,#205661)),.UNSPECIFIED.,.F.,
 .F.,.F.)
B_SPLINE_SURFACE_WITH_KNOTS((4,4),(3,3),(0.,0.000397394428086631),(0.,1.),
 .UNSPECIFIED.)
GEOMETRIC_REPRESENTATION_ITEM()
RATIONAL_B_SPLINE_SURFACE(((1.,0.707106781186548,1.),(1.,0.706459846759102,
1.),(1.,0.70582051073727,1.),(1.,0.705498956110742,1.)))
REPRESENTATION_ITEM('')
SURFACE()
);
#2953=(
BOUNDED_SURFACE()
B_SPLINE_SURFACE(3,2,((#205667,#205668,#205669),(#205670,#205671,#205672),
(#205673,#205674,#205675),(#205676,#205677,#205678),(#205679,#205680,#205681),
(#205682,#205683,#205684)),.UNSPECIFIED.,.F.,.F.,.F.)
B_SPLINE_SURFACE_WITH_KNOTS((4,2,4),(3,3),(0.,0.000257953807872848,0.000515907615745695),
(0.,1.),.UNSPECIFIED.)
GEOMETRIC_REPRESENTATION_ITEM()
RATIONAL_B_SPLINE_SURFACE(((1.,0.874619707139383,1.),(1.,0.874834349678855,
1.),(1.,0.854686104157979,1.),(1.,0.79247659791496,1.),(1.,0.750887854595262,
1.),(1.,0.705585838031416,1.)))
REPRESENTATION_ITEM('')
SURFACE()
);
#2954=(
BOUNDED_SURFACE()
B_SPLINE_SURFACE(3,2,((#205690,#205691,#205692),(#205693,#205694,#205695),
(#205696,#205697,#205698),(#205699,#205700,#205701)),.UNSPECIFIED.,.F.,
 .F.,.F.)
B_SPLINE_SURFACE_WITH_KNOTS((4,4),(3,3),(0.,0.000511815437699153),(0.,1.00105881331625),
 .UNSPECIFIED.)
GEOMETRIC_REPRESENTATION_ITEM()
RATIONAL_B_SPLINE_SURFACE(((1.,0.706796661946227,1.0006208951974),(1.,0.707430821225108,
1.00061955228482),(1.,0.708058545830617,1.00061822299848),(1.,0.708394505252617,
1.00061751156186)))
REPRESENTATION_ITEM('')
SURFACE()
);
#2955=(
BOUNDED_SURFACE()
B_SPLINE_SURFACE(3,2,((#205703,#205704,#205705),(#205706,#205707,#205708),
(#205709,#205710,#205711),(#205712,#205713,#205714),(#205715,#205716,#205717),
(#205718,#205719,#205720)),.UNSPECIFIED.,.F.,.F.,.F.)
B_SPLINE_SURFACE_WITH_KNOTS((4,2,4),(3,3),(-9.37834879199961E-18,0.000256915317531254,
0.000513830635062517),(0.,1.),.UNSPECIFIED.)
GEOMETRIC_REPRESENTATION_ITEM()
RATIONAL_B_SPLINE_SURFACE(((1.,0.705585838031447,1.),(1.,0.750902433543063,
1.),(1.,0.79232953008209,1.),(1.,0.854288401594609,1.),(1.,0.874998031124818,
1.),(1.,0.87461970713939,1.)))
REPRESENTATION_ITEM('')
SURFACE()
);
#2956=(
BOUNDED_SURFACE()
B_SPLINE_SURFACE(3,2,((#205726,#205727,#205728),(#205729,#205730,#205731),
(#205732,#205733,#205734),(#205735,#205736,#205737),(#205738,#205739,#205740),
(#205741,#205742,#205743)),.UNSPECIFIED.,.F.,.F.,.F.)
B_SPLINE_SURFACE_WITH_KNOTS((4,2,4),(3,3),(-9.32413868337534E-18,0.000256592814262153,
0.000513185628524315),(0.,1.),.UNSPECIFIED.)
GEOMETRIC_REPRESENTATION_ITEM()
RATIONAL_B_SPLINE_SURFACE(((1.,0.708712527163675,1.),(1.,0.753780902613636,
1.),(1.,0.794538995769133,1.),(1.,0.855070770331152,1.),(1.,0.875018427445287,
1.),(1.,0.874619707139396,1.)))
REPRESENTATION_ITEM('')
SURFACE()
);
#2957=(
BOUNDED_SURFACE()
B_SPLINE_SURFACE(3,2,((#205745,#205746,#205747),(#205748,#205749,#205750),
(#205751,#205752,#205753),(#205754,#205755,#205756)),.UNSPECIFIED.,.F.,
 .F.,.F.)
B_SPLINE_SURFACE_WITH_KNOTS((4,4),(3,3),(0.,0.000511815072430401),(0.,1.00105598365716),
 .UNSPECIFIED.)
GEOMETRIC_REPRESENTATION_ITEM()
RATIONAL_B_SPLINE_SURFACE(((1.,0.706797490734188,1.00061923411604),(1.,
0.706182062147101,1.0006205338811),(1.,0.705584062769487,1.00062179683624),
(1.,0.705266224770961,1.00062246809971)))
REPRESENTATION_ITEM('')
SURFACE()
);
#2958=(
BOUNDED_SURFACE()
B_SPLINE_SURFACE(3,2,((#205762,#205763,#205764),(#205765,#205766,#205767),
(#205768,#205769,#205770),(#205771,#205772,#205773),(#205774,#205775,#205776),
(#205777,#205778,#205779)),.UNSPECIFIED.,.F.,.F.,.F.)
B_SPLINE_SURFACE_WITH_KNOTS((4,2,4),(3,3),(-9.62229428080885E-18,0.000257652232350869,
0.000515304464701747),(0.,1.),.UNSPECIFIED.)
GEOMETRIC_REPRESENTATION_ITEM()
RATIONAL_B_SPLINE_SURFACE(((1.,0.874619707139388,1.),(1.,0.87486118043047,
1.),(1.,0.855455725921216,1.),(1.,0.794699358954906,1.),(1.,0.753768977788931,
1.),(1.,0.70871252716366,1.)))
REPRESENTATION_ITEM('')
SURFACE()
);
#2959=(
BOUNDED_SURFACE()
B_SPLINE_SURFACE(3,2,((#205785,#205786,#205787),(#205788,#205789,#205790),
(#205791,#205792,#205793),(#205794,#205795,#205796)),.UNSPECIFIED.,.F.,
 .F.,.F.)
B_SPLINE_SURFACE_WITH_KNOTS((4,4),(3,3),(0.,0.000397394373651925),(0.,1.),
 .UNSPECIFIED.)
GEOMETRIC_REPRESENTATION_ITEM()
RATIONAL_B_SPLINE_SURFACE(((1.,0.707106781186548,1.),(1.,0.707752587915922,
1.),(1.,0.708377654540667,1.),(1.,0.708689770883311,1.)))
REPRESENTATION_ITEM('')
SURFACE()
);
#2960=(
BOUNDED_SURFACE()
B_SPLINE_SURFACE(3,2,((#205798,#205799,#205800),(#205801,#205802,#205803),
(#205804,#205805,#205806),(#205807,#205808,#205809)),.UNSPECIFIED.,.F.,
 .F.,.F.)
B_SPLINE_SURFACE_WITH_KNOTS((4,4),(3,3),(0.,0.000511815456479788),(0.,1.0010587316027),
 .UNSPECIFIED.)
GEOMETRIC_REPRESENTATION_ITEM()
RATIONAL_B_SPLINE_SURFACE(((1.,0.708394529055522,1.00061746385522),(1.,
0.7080585641661,1.00061817524851),(1.,0.70743083537124,1.00061950444114),
(1.,0.706796685879573,1.00062084722935)))
REPRESENTATION_ITEM('')
SURFACE()
);
#2961=(
BOUNDED_SURFACE()
B_SPLINE_SURFACE(3,2,((#205815,#205816,#205817),(#205818,#205819,#205820),
(#205821,#205822,#205823),(#205824,#205825,#205826)),.UNSPECIFIED.,.F.,
 .F.,.F.)
B_SPLINE_SURFACE_WITH_KNOTS((4,4),(3,3),(0.,0.000397394465448303),(0.,1.),
 .UNSPECIFIED.)
GEOMETRIC_REPRESENTATION_ITEM()
RATIONAL_B_SPLINE_SURFACE(((1.,0.705498956110765,1.),(1.,0.705821764811767,
1.),(1.,0.706461952521164,1.),(1.,0.707106781186548,1.)))
REPRESENTATION_ITEM('')
SURFACE()
);
#2962=(
BOUNDED_SURFACE()
B_SPLINE_SURFACE(3,2,((#205832,#205833,#205834),(#205835,#205836,#205837),
(#205838,#205839,#205840),(#205841,#205842,#205843)),.UNSPECIFIED.,.F.,
 .F.,.F.)
B_SPLINE_SURFACE_WITH_KNOTS((4,4),(3,3),(0.,0.000397394410828739),(0.,1.),
 .UNSPECIFIED.)
GEOMETRIC_REPRESENTATION_ITEM()
RATIONAL_B_SPLINE_SURFACE(((1.,0.708689770883324,1.),(1.,0.708376440034488,
1.),(1.,0.707750498698415,1.),(1.,0.707106781186548,1.)))
REPRESENTATION_ITEM('')
SURFACE()
);
#2963=(
BOUNDED_SURFACE()
B_SPLINE_SURFACE(3,2,((#205849,#205850,#205851),(#205852,#205853,#205854),
(#205855,#205856,#205857),(#205858,#205859,#205860)),.UNSPECIFIED.,.F.,
 .F.,.F.)
B_SPLINE_SURFACE_WITH_KNOTS((4,4),(3,3),(0.,0.000511815090126181),(0.,1.00105592270067),
 .UNSPECIFIED.)
GEOMETRIC_REPRESENTATION_ITEM()
RATIONAL_B_SPLINE_SURFACE(((1.,0.705266242717945,1.00062243212993),(1.,
0.705584085909577,1.00062176089425),(1.,0.70618208945095,1.00062049800322),
(1.,0.706797508587931,1.00061919833315)))
REPRESENTATION_ITEM('')
SURFACE()
);
#2964=(
BOUNDED_SURFACE()
B_SPLINE_SURFACE(3,2,((#205862,#205863,#205864),(#205865,#205866,#205867),
(#205868,#205869,#205870),(#205871,#205872,#205873)),.UNSPECIFIED.,.F.,
 .F.,.F.)
B_SPLINE_SURFACE_WITH_KNOTS((4,4),(3,3),(0.,0.00039739442808661),(0.,1.),
 .UNSPECIFIED.)
GEOMETRIC_REPRESENTATION_ITEM()
RATIONAL_B_SPLINE_SURFACE(((1.,0.707106781186548,1.),(1.,0.706459846759103,
1.),(1.,0.705820510737282,1.),(1.,0.705498956110752,1.)))
REPRESENTATION_ITEM('')
SURFACE()
);
#2965=(
BOUNDED_SURFACE()
B_SPLINE_SURFACE(3,2,((#205879,#205880,#205881),(#205882,#205883,#205884),
(#205885,#205886,#205887),(#205888,#205889,#205890),(#205891,#205892,#205893),
(#205894,#205895,#205896)),.UNSPECIFIED.,.F.,.F.,.F.)
B_SPLINE_SURFACE_WITH_KNOTS((4,2,4),(3,3),(0.,0.000257953807872847,0.000515907615745694),
(0.,1.),.UNSPECIFIED.)
GEOMETRIC_REPRESENTATION_ITEM()
RATIONAL_B_SPLINE_SURFACE(((1.,0.87461970713939,1.),(1.,0.874834349678675,
1.),(1.,0.854686104158191,1.),(1.,0.79247659791475,1.),(1.,0.750887854595405,
1.),(1.,0.705585838031447,1.)))
REPRESENTATION_ITEM('')
SURFACE()
);
#2966=(
BOUNDED_SURFACE()
B_SPLINE_SURFACE(3,2,((#205902,#205903,#205904),(#205905,#205906,#205907),
(#205908,#205909,#205910),(#205911,#205912,#205913)),.UNSPECIFIED.,.F.,
 .F.,.F.)
B_SPLINE_SURFACE_WITH_KNOTS((4,4),(3,3),(-9.64939933512099E-18,0.000511815437699153),
(0.,1.00105881331513),.UNSPECIFIED.)
GEOMETRIC_REPRESENTATION_ITEM()
RATIONAL_B_SPLINE_SURFACE(((1.,0.706796661946555,1.00062089519675),(1.,
0.707430821225458,1.00061955228417),(1.,0.708058545830927,1.00061822299783),
(1.,0.70839450525293,1.00061751156121)))
REPRESENTATION_ITEM('')
SURFACE()
);
#2967=(
BOUNDED_SURFACE()
B_SPLINE_SURFACE(3,2,((#205915,#205916,#205917),(#205918,#205919,#205920),
(#205921,#205922,#205923),(#205924,#205925,#205926),(#205927,#205928,#205929),
(#205930,#205931,#205932)),.UNSPECIFIED.,.F.,.F.,.F.)
B_SPLINE_SURFACE_WITH_KNOTS((4,2,4),(3,3),(0.,0.00025691531753127,0.000513830635062539),
(0.,1.),.UNSPECIFIED.)
GEOMETRIC_REPRESENTATION_ITEM()
RATIONAL_B_SPLINE_SURFACE(((1.,0.705585838031426,1.),(1.,0.750902433542389,
1.),(1.,0.792329530083006,1.),(1.,0.854288401593708,1.),(1.,0.87499803112553,
1.),(1.,0.874619707139387,1.)))
REPRESENTATION_ITEM('')
SURFACE()
);
#2968=(
BOUNDED_SURFACE()
B_SPLINE_SURFACE(3,2,((#205938,#205939,#205940),(#205941,#205942,#205943),
(#205944,#205945,#205946),(#205947,#205948,#205949),(#205950,#205951,#205952),
(#205953,#205954,#205955)),.UNSPECIFIED.,.F.,.F.,.F.)
B_SPLINE_SURFACE_WITH_KNOTS((4,2,4),(3,3),(0.,0.000256592814262155,0.000513185628524311),
(0.,1.),.UNSPECIFIED.)
GEOMETRIC_REPRESENTATION_ITEM()
RATIONAL_B_SPLINE_SURFACE(((1.,0.708712527163685,1.),(1.,0.753780902614243,
1.),(1.,0.794538995768276,1.),(1.,0.855070770332059,1.),(1.,0.875018427444598,
1.),(1.,0.874619707139393,1.)))
REPRESENTATION_ITEM('')
SURFACE()
);
#2969=(
BOUNDED_SURFACE()
B_SPLINE_SURFACE(3,2,((#205957,#205958,#205959),(#205960,#205961,#205962),
(#205963,#205964,#205965),(#205966,#205967,#205968)),.UNSPECIFIED.,.F.,
 .F.,.F.)
B_SPLINE_SURFACE_WITH_KNOTS((4,4),(3,3),(0.,0.000511815072430395),(0.,1.00105598365835),
 .UNSPECIFIED.)
GEOMETRIC_REPRESENTATION_ITEM()
RATIONAL_B_SPLINE_SURFACE(((1.,0.70679749073384,1.00061923411674),(1.,0.706182062146739,
1.0006205338818),(1.,0.705584062769122,1.00062179683694),(1.,0.705266224770601,
1.00062246810041)))
REPRESENTATION_ITEM('')
SURFACE()
);
#2970=(
BOUNDED_SURFACE()
B_SPLINE_SURFACE(3,2,((#205974,#205975,#205976),(#205977,#205978,#205979),
(#205980,#205981,#205982),(#205983,#205984,#205985),(#205986,#205987,#205988),
(#205989,#205990,#205991)),.UNSPECIFIED.,.F.,.F.,.F.)
B_SPLINE_SURFACE_WITH_KNOTS((4,2,4),(3,3),(0.,0.000257652232350885,0.00051530446470177),
(0.,1.),.UNSPECIFIED.)
GEOMETRIC_REPRESENTATION_ITEM()
RATIONAL_B_SPLINE_SURFACE(((1.,0.874619707139382,1.),(1.,0.874861180430943,
1.),(1.,0.855455725920536,1.),(1.,0.794699358955577,1.),(1.,0.753768977788396,
1.),(1.,0.708712527163675,1.)))
REPRESENTATION_ITEM('')
SURFACE()
);
#2971=(
BOUNDED_SURFACE()
B_SPLINE_SURFACE(3,2,((#205997,#205998,#205999),(#206000,#206001,#206002),
(#206003,#206004,#206005),(#206006,#206007,#206008)),.UNSPECIFIED.,.F.,
 .F.,.F.)
B_SPLINE_SURFACE_WITH_KNOTS((4,4),(3,3),(0.,0.000397394373651913),(0.,1.),
 .UNSPECIFIED.)
GEOMETRIC_REPRESENTATION_ITEM()
RATIONAL_B_SPLINE_SURFACE(((1.,0.707106781186548,1.),(1.,0.707752587915884,
1.),(1.,0.708377654540707,1.),(1.,0.708689770883326,1.)))
REPRESENTATION_ITEM('')
SURFACE()
);
#2972=(
BOUNDED_SURFACE()
B_SPLINE_SURFACE(3,2,((#206010,#206011,#206012),(#206013,#206014,#206015),
(#206016,#206017,#206018),(#206019,#206020,#206021)),.UNSPECIFIED.,.F.,
 .F.,.F.)
B_SPLINE_SURFACE_WITH_KNOTS((4,4),(3,3),(0.,0.000511815456479787),(0.,1.00105873159594),
 .UNSPECIFIED.)
GEOMETRIC_REPRESENTATION_ITEM()
RATIONAL_B_SPLINE_SURFACE(((1.,0.708394529057491,1.00061746385127),(1.,
0.708058564168059,1.00061817524456),(1.,0.707430835373237,1.00061950443718),
(1.,0.706796685881553,1.00062084722538)))
REPRESENTATION_ITEM('')
SURFACE()
);
#2973=(
BOUNDED_SURFACE()
B_SPLINE_SURFACE(3,2,((#206027,#206028,#206029),(#206030,#206031,#206032),
(#206033,#206034,#206035),(#206036,#206037,#206038)),.UNSPECIFIED.,.F.,
 .F.,.F.)
B_SPLINE_SURFACE_WITH_KNOTS((4,4),(3,3),(0.,0.000397394465448302),(0.,1.),
 .UNSPECIFIED.)
GEOMETRIC_REPRESENTATION_ITEM()
RATIONAL_B_SPLINE_SURFACE(((1.,0.705498956110742,1.),(1.,0.705821764811801,
1.),(1.,0.706461952521133,1.),(1.,0.707106781186548,1.)))
REPRESENTATION_ITEM('')
SURFACE()
);
#2974=(
BOUNDED_SURFACE()
B_SPLINE_SURFACE(3,2,((#206044,#206045,#206046),(#206047,#206048,#206049),
(#206050,#206051,#206052),(#206053,#206054,#206055)),.UNSPECIFIED.,.F.,
 .F.,.F.)
B_SPLINE_SURFACE_WITH_KNOTS((4,4),(3,3),(0.,0.000397394410828734),(0.,1.),
 .UNSPECIFIED.)
GEOMETRIC_REPRESENTATION_ITEM()
RATIONAL_B_SPLINE_SURFACE(((1.,0.708689770883308,1.),(1.,0.708376440034539,
1.),(1.,0.70775049869839,1.),(1.,0.707106781186548,1.)))
REPRESENTATION_ITEM('')
SURFACE()
);
#2975=(
BOUNDED_SURFACE()
B_SPLINE_SURFACE(3,2,((#206061,#206062,#206063),(#206064,#206065,#206066),
(#206067,#206068,#206069),(#206070,#206071,#206072)),.UNSPECIFIED.,.F.,
 .F.,.F.)
B_SPLINE_SURFACE_WITH_KNOTS((4,4),(3,3),(0.,0.000511815090126186),(0.,1.00105592270023),
 .UNSPECIFIED.)
GEOMETRIC_REPRESENTATION_ITEM()
RATIONAL_B_SPLINE_SURFACE(((1.,0.705266242718059,1.00062243212967),(1.,
0.705584085909722,1.00062176089399),(1.,0.706182089451054,1.00062049800296),
(1.,0.706797508588071,1.00061919833289)))
REPRESENTATION_ITEM('')
SURFACE()
);
#2976=(
BOUNDED_SURFACE()
B_SPLINE_SURFACE(3,2,((#206074,#206075,#206076),(#206077,#206078,#206079),
(#206080,#206081,#206082),(#206083,#206084,#206085)),.UNSPECIFIED.,.F.,
 .F.,.F.)
B_SPLINE_SURFACE_WITH_KNOTS((4,4),(3,3),(-5.52943107967607E-18,0.000397394428086622),
(0.,1.),.UNSPECIFIED.)
GEOMETRIC_REPRESENTATION_ITEM()
RATIONAL_B_SPLINE_SURFACE(((1.,0.707106781186548,1.),(1.,0.706459846759108,
1.),(1.,0.70582051073728,1.),(1.,0.705498956110745,1.)))
REPRESENTATION_ITEM('')
SURFACE()
);
#2977=(
BOUNDED_SURFACE()
B_SPLINE_SURFACE(3,2,((#206091,#206092,#206093),(#206094,#206095,#206096),
(#206097,#206098,#206099),(#206100,#206101,#206102),(#206103,#206104,#206105),
(#206106,#206107,#206108)),.UNSPECIFIED.,.F.,.F.,.F.)
B_SPLINE_SURFACE_WITH_KNOTS((4,2,4),(3,3),(0.,0.000257953807872851,0.000515907615745702),
(0.,1.),.UNSPECIFIED.)
GEOMETRIC_REPRESENTATION_ITEM()
RATIONAL_B_SPLINE_SURFACE(((1.,0.874619707139392,1.),(1.,0.874834349679009,
1.),(1.,0.854686104157774,1.),(1.,0.792476597915158,1.),(1.,0.750887854595105,
1.),(1.,0.705585838031436,1.)))
REPRESENTATION_ITEM('')
SURFACE()
);
#2978=(
BOUNDED_SURFACE()
B_SPLINE_SURFACE(3,2,((#206114,#206115,#206116),(#206117,#206118,#206119),
(#206120,#206121,#206122),(#206123,#206124,#206125)),.UNSPECIFIED.,.F.,
 .F.,.F.)
B_SPLINE_SURFACE_WITH_KNOTS((4,4),(3,3),(0.,0.000511815437699149),(0.,1.0010588133169),
 .UNSPECIFIED.)
GEOMETRIC_REPRESENTATION_ITEM()
RATIONAL_B_SPLINE_SURFACE(((1.,0.706796661946038,1.00062089519778),(1.,
0.707430821224916,1.0006195522852),(1.,0.708058545830393,1.00061822299886),
(1.,0.708394505252432,1.00061751156224)))
REPRESENTATION_ITEM('')
SURFACE()
);
#2979=(
BOUNDED_SURFACE()
B_SPLINE_SURFACE(3,2,((#206127,#206128,#206129),(#206130,#206131,#206132),
(#206133,#206134,#206135),(#206136,#206137,#206138),(#206139,#206140,#206141),
(#206142,#206143,#206144)),.UNSPECIFIED.,.F.,.F.,.F.)
B_SPLINE_SURFACE_WITH_KNOTS((4,2,4),(3,3),(0.,0.000256915317531261,0.000513830635062523),
(0.,1.),.UNSPECIFIED.)
GEOMETRIC_REPRESENTATION_ITEM()
RATIONAL_B_SPLINE_SURFACE(((1.,0.705585838031425,1.),(1.,0.750902433543488,
1.),(1.,0.792329530081549,1.),(1.,0.854288401595205,1.),(1.,0.874998031124371,
1.),(1.,0.874619707139389,1.)))
REPRESENTATION_ITEM('')
SURFACE()
);
#2980=(
BOUNDED_SURFACE()
B_SPLINE_SURFACE(3,2,((#206150,#206151,#206152),(#206153,#206154,#206155),
(#206156,#206157,#206158),(#206159,#206160,#206161),(#206162,#206163,#206164),
(#206165,#206166,#206167)),.UNSPECIFIED.,.F.,.F.,.F.)
B_SPLINE_SURFACE_WITH_KNOTS((4,2,4),(3,3),(0.,0.000256592814262158,0.000513185628524316),
(0.,1.),.UNSPECIFIED.)
GEOMETRIC_REPRESENTATION_ITEM()
RATIONAL_B_SPLINE_SURFACE(((1.,0.708712527163672,1.),(1.,0.753780902613422,
1.),(1.,0.794538995769399,1.),(1.,0.855070770330892,1.),(1.,0.875018427445483,
1.),(1.,0.874619707139387,1.)))
REPRESENTATION_ITEM('')
SURFACE()
);
#2981=(
BOUNDED_SURFACE()
B_SPLINE_SURFACE(3,2,((#206169,#206170,#206171),(#206172,#206173,#206174),
(#206175,#206176,#206177),(#206178,#206179,#206180)),.UNSPECIFIED.,.F.,
 .F.,.F.)
B_SPLINE_SURFACE_WITH_KNOTS((4,4),(3,3),(0.,0.000511815072430397),(0.,1.00105598366041),
 .UNSPECIFIED.)
GEOMETRIC_REPRESENTATION_ITEM()
RATIONAL_B_SPLINE_SURFACE(((1.,0.706797490733247,1.00061923411795),(1.,
0.706182062146158,1.00062053388302),(1.,0.705584062768489,1.00062179683816),
(1.,0.705266224770021,1.00062246810163)))
REPRESENTATION_ITEM('')
SURFACE()
);
#2982=(
BOUNDED_SURFACE()
B_SPLINE_SURFACE(3,2,((#206186,#206187,#206188),(#206189,#206190,#206191),
(#206192,#206193,#206194),(#206195,#206196,#206197),(#206198,#206199,#206200),
(#206201,#206202,#206203)),.UNSPECIFIED.,.F.,.F.,.F.)
B_SPLINE_SURFACE_WITH_KNOTS((4,2,4),(3,3),(0.,0.000257652232350886,0.000515304464701773),
(0.,1.),.UNSPECIFIED.)
GEOMETRIC_REPRESENTATION_ITEM()
RATIONAL_B_SPLINE_SURFACE(((1.,0.874619707139387,1.),(1.,0.874861180430777,
1.),(1.,0.85545572592079,1.),(1.,0.794699358955371,1.),(1.,0.753768977788547,
1.),(1.,0.708712527163673,1.)))
REPRESENTATION_ITEM('')
SURFACE()
);
#2983=(
BOUNDED_SURFACE()
B_SPLINE_SURFACE(3,2,((#206209,#206210,#206211),(#206212,#206213,#206214),
(#206215,#206216,#206217),(#206218,#206219,#206220)),.UNSPECIFIED.,.F.,
 .F.,.F.)
B_SPLINE_SURFACE_WITH_KNOTS((4,4),(3,3),(0.,0.000397394373651913),(0.,1.),
 .UNSPECIFIED.)
GEOMETRIC_REPRESENTATION_ITEM()
RATIONAL_B_SPLINE_SURFACE(((1.,0.707106781186536,1.),(1.,0.707752587915919,
1.),(1.,0.70837765454067,1.),(1.,0.708689770883331,1.)))
REPRESENTATION_ITEM('')
SURFACE()
);
#2984=(
BOUNDED_SURFACE()
B_SPLINE_SURFACE(3,2,((#206222,#206223,#206224),(#206225,#206226,#206227),
(#206228,#206229,#206230),(#206231,#206232,#206233)),.UNSPECIFIED.,.F.,
 .F.,.F.)
B_SPLINE_SURFACE_WITH_KNOTS((4,4),(3,3),(0.,0.000511815456479785),(0.,1.00105873159934),
 .UNSPECIFIED.)
GEOMETRIC_REPRESENTATION_ITEM()
RATIONAL_B_SPLINE_SURFACE(((1.,0.708394529056502,1.00061746385326),(1.,
0.708058564167077,1.00061817524654),(1.,0.70743083537222,1.00061950443917),
(1.,0.706796685880547,1.00062084722738)))
REPRESENTATION_ITEM('')
SURFACE()
);
#2985=(
BOUNDED_SURFACE()
B_SPLINE_SURFACE(3,2,((#206239,#206240,#206241),(#206242,#206243,#206244),
(#206245,#206246,#206247),(#206248,#206249,#206250)),.UNSPECIFIED.,.F.,
 .F.,.F.)
B_SPLINE_SURFACE_WITH_KNOTS((4,4),(3,3),(0.,0.000397394465448304),(0.,1.),
 .UNSPECIFIED.)
GEOMETRIC_REPRESENTATION_ITEM()
RATIONAL_B_SPLINE_SURFACE(((1.,0.705498956110752,1.),(1.,0.705821764811803,
1.),(1.,0.706461952521127,1.),(1.,0.707106781186548,1.)))
REPRESENTATION_ITEM('')
SURFACE()
);
#2986=(
BOUNDED_SURFACE()
B_SPLINE_SURFACE(3,2,((#206256,#206257,#206258),(#206259,#206260,#206261),
(#206262,#206263,#206264),(#206265,#206266,#206267)),.UNSPECIFIED.,.F.,
 .F.,.F.)
B_SPLINE_SURFACE_WITH_KNOTS((4,4),(3,3),(0.,0.000397394410828736),(0.,1.),
 .UNSPECIFIED.)
GEOMETRIC_REPRESENTATION_ITEM()
RATIONAL_B_SPLINE_SURFACE(((1.,0.70868977088333,1.),(1.,0.708376440034522,
1.),(1.,0.707750498698396,1.),(1.,0.707106781186548,1.)))
REPRESENTATION_ITEM('')
SURFACE()
);
#2987=(
BOUNDED_SURFACE()
B_SPLINE_SURFACE(3,2,((#206273,#206274,#206275),(#206276,#206277,#206278),
(#206279,#206280,#206281),(#206282,#206283,#206284)),.UNSPECIFIED.,.F.,
 .F.,.F.)
B_SPLINE_SURFACE_WITH_KNOTS((4,4),(3,3),(0.,0.000511815090126171),(0.,1.00105592270543),
 .UNSPECIFIED.)
GEOMETRIC_REPRESENTATION_ITEM()
RATIONAL_B_SPLINE_SURFACE(((1.,0.705266242716512,1.00062243213275),(1.,
0.705584085908209,1.00062176089706),(1.,0.706182089449527,1.00062049800603),
(1.,0.706797508586535,1.00061919833595)))
REPRESENTATION_ITEM('')
SURFACE()
);
#2988=(
BOUNDED_SURFACE()
B_SPLINE_SURFACE(3,2,((#206286,#206287,#206288),(#206289,#206290,#206291),
(#206292,#206293,#206294),(#206295,#206296,#206297)),.UNSPECIFIED.,.F.,
 .F.,.F.)
B_SPLINE_SURFACE_WITH_KNOTS((4,4),(3,3),(0.,0.000397394428086614),(0.,1.),
 .UNSPECIFIED.)
GEOMETRIC_REPRESENTATION_ITEM()
RATIONAL_B_SPLINE_SURFACE(((1.,0.707106781186548,1.),(1.,0.706459846759078,
1.),(1.,0.705820510737289,1.),(1.,0.705498956110736,1.)))
REPRESENTATION_ITEM('')
SURFACE()
);
#2989=(
BOUNDED_SURFACE()
B_SPLINE_SURFACE(3,2,((#206303,#206304,#206305),(#206306,#206307,#206308),
(#206309,#206310,#206311),(#206312,#206313,#206314),(#206315,#206316,#206317),
(#206318,#206319,#206320)),.UNSPECIFIED.,.F.,.F.,.F.)
B_SPLINE_SURFACE_WITH_KNOTS((4,2,4),(3,3),(0.,0.000257953807872845,0.00051590761574569),
(0.,1.),.UNSPECIFIED.)
GEOMETRIC_REPRESENTATION_ITEM()
RATIONAL_B_SPLINE_SURFACE(((1.,0.874619707139387,1.),(1.,0.87483434967959,
1.),(1.,0.854686104157006,1.),(1.,0.792476597915929,1.),(1.,0.750887854594532,
1.),(1.,0.705585838031438,1.)))
REPRESENTATION_ITEM('')
SURFACE()
);
#2990=(
BOUNDED_SURFACE()
B_SPLINE_SURFACE(3,2,((#206326,#206327,#206328),(#206329,#206330,#206331),
(#206332,#206333,#206334),(#206335,#206336,#206337)),.UNSPECIFIED.,.F.,
 .F.,.F.)
B_SPLINE_SURFACE_WITH_KNOTS((4,4),(3,3),(0.,0.000511815437699149),(0.,1.0010588133194),
 .UNSPECIFIED.)
GEOMETRIC_REPRESENTATION_ITEM()
RATIONAL_B_SPLINE_SURFACE(((1.,0.706796661945307,1.00062089519925),(1.,
0.707430821224188,1.00061955228667),(1.,0.708058545829719,1.00061822300032),
(1.,0.708394505251694,1.0006175115637)))
REPRESENTATION_ITEM('')
SURFACE()
);
#2991=(
BOUNDED_SURFACE()
B_SPLINE_SURFACE(3,2,((#206339,#206340,#206341),(#206342,#206343,#206344),
(#206345,#206346,#206347),(#206348,#206349,#206350),(#206351,#206352,#206353),
(#206354,#206355,#206356)),.UNSPECIFIED.,.F.,.F.,.F.)
B_SPLINE_SURFACE_WITH_KNOTS((4,2,4),(3,3),(0.,0.000256915317531267,0.000513830635062534),
(0.,1.),.UNSPECIFIED.)
GEOMETRIC_REPRESENTATION_ITEM()
RATIONAL_B_SPLINE_SURFACE(((1.,0.705585838031461,1.),(1.,0.750902433542758,
1.),(1.,0.792329530082508,1.),(1.,0.854288401594206,1.),(1.,0.874998031125127,
1.),(1.,0.8746197071394,1.)))
REPRESENTATION_ITEM('')
SURFACE()
);
#2992=(
BOUNDED_SURFACE()
B_SPLINE_SURFACE(3,2,((#206362,#206363,#206364),(#206365,#206366,#206367),
(#206368,#206369,#206370),(#206371,#206372,#206373),(#206374,#206375,#206376),
(#206377,#206378,#206379)),.UNSPECIFIED.,.F.,.F.,.F.)
B_SPLINE_SURFACE_WITH_KNOTS((4,2,4),(3,3),(0.,0.000256592814262156,0.000513185628524312),
(0.,1.),.UNSPECIFIED.)
GEOMETRIC_REPRESENTATION_ITEM()
RATIONAL_B_SPLINE_SURFACE(((1.,0.708712527163667,1.),(1.,0.753780902613713,
1.),(1.,0.794538995769065,1.),(1.,0.855070770331245,1.),(1.,0.875018427445222,
1.),(1.,0.874619707139387,1.)))
REPRESENTATION_ITEM('')
SURFACE()
);
#2993=(
BOUNDED_SURFACE()
B_SPLINE_SURFACE(3,2,((#206381,#206382,#206383),(#206384,#206385,#206386),
(#206387,#206388,#206389),(#206390,#206391,#206392)),.UNSPECIFIED.,.F.,
 .F.,.F.)
B_SPLINE_SURFACE_WITH_KNOTS((4,4),(3,3),(0.,0.000511815072430405),(0.,1.00105598366104),
 .UNSPECIFIED.)
GEOMETRIC_REPRESENTATION_ITEM()
RATIONAL_B_SPLINE_SURFACE(((1.,0.70679749073305,1.00061923411833),(1.,0.706182062145971,
1.00062053388339),(1.,0.705584062768321,1.00062179683854),(1.,0.705266224769805,
1.000622468102)))
REPRESENTATION_ITEM('')
SURFACE()
);
#2994=(
BOUNDED_SURFACE()
B_SPLINE_SURFACE(3,2,((#206398,#206399,#206400),(#206401,#206402,#206403),
(#206404,#206405,#206406),(#206407,#206408,#206409),(#206410,#206411,#206412),
(#206413,#206414,#206415)),.UNSPECIFIED.,.F.,.F.,.F.)
B_SPLINE_SURFACE_WITH_KNOTS((4,2,4),(3,3),(-2.80537312130624E-18,0.000257652232350884,
0.000515304464701771),(0.,1.),.UNSPECIFIED.)
GEOMETRIC_REPRESENTATION_ITEM()
RATIONAL_B_SPLINE_SURFACE(((1.,0.874619707139388,1.),(1.,0.874861180430588,
1.),(1.,0.855455725920997,1.),(1.,0.794699358955135,1.),(1.,0.753768977788717,
1.),(1.,0.708712527163664,1.)))
REPRESENTATION_ITEM('')
SURFACE()
);
#2995=(
BOUNDED_SURFACE()
B_SPLINE_SURFACE(3,2,((#206421,#206422,#206423),(#206424,#206425,#206426),
(#206427,#206428,#206429),(#206430,#206431,#206432)),.UNSPECIFIED.,.F.,
 .F.,.F.)
B_SPLINE_SURFACE_WITH_KNOTS((4,4),(3,3),(-7.64362531602281E-18,0.000397394373651905),
(0.,1.),.UNSPECIFIED.)
GEOMETRIC_REPRESENTATION_ITEM()
RATIONAL_B_SPLINE_SURFACE(((1.,0.707106781186548,1.),(1.,0.707752587915893,
1.),(1.,0.708377654540694,1.),(1.,0.708689770883325,1.)))
REPRESENTATION_ITEM('')
SURFACE()
);
#2996=(
BOUNDED_SURFACE()
B_SPLINE_SURFACE(3,2,((#206434,#206435,#206436),(#206437,#206438,#206439),
(#206440,#206441,#206442),(#206443,#206444,#206445)),.UNSPECIFIED.,.F.,
 .F.,.F.)
B_SPLINE_SURFACE_WITH_KNOTS((4,4),(3,3),(0.,0.000511815456479789),(0.,1.0010587316006),
 .UNSPECIFIED.)
GEOMETRIC_REPRESENTATION_ITEM()
RATIONAL_B_SPLINE_SURFACE(((1.,0.708394529056127,1.00061746385399),(1.,
0.708058564166706,1.00061817524728),(1.,0.707430835371847,1.00061950443991),
(1.,0.706796685880188,1.00062084722812)))
REPRESENTATION_ITEM('')
SURFACE()
);
#2997=(
BOUNDED_SURFACE()
B_SPLINE_SURFACE(3,2,((#206451,#206452,#206453),(#206454,#206455,#206456),
(#206457,#206458,#206459),(#206460,#206461,#206462)),.UNSPECIFIED.,.F.,
 .F.,.F.)
B_SPLINE_SURFACE_WITH_KNOTS((4,4),(3,3),(-6.50521303491303E-18,0.000397394465448314),
(0.,1.),.UNSPECIFIED.)
GEOMETRIC_REPRESENTATION_ITEM()
RATIONAL_B_SPLINE_SURFACE(((1.,0.705498956110783,1.),(1.,0.70582176481173,
1.),(1.,0.706461952521176,1.),(1.,0.707106781186546,1.)))
REPRESENTATION_ITEM('')
SURFACE()
);
#2998=(
BOUNDED_SURFACE()
B_SPLINE_SURFACE(3,2,((#206468,#206469,#206470),(#206471,#206472,#206473),
(#206474,#206475,#206476),(#206477,#206478,#206479)),.UNSPECIFIED.,.F.,
 .F.,.F.)
B_SPLINE_SURFACE_WITH_KNOTS((4,4),(3,3),(0.,0.000397394410828748),(0.,1.),
 .UNSPECIFIED.)
GEOMETRIC_REPRESENTATION_ITEM()
RATIONAL_B_SPLINE_SURFACE(((1.,0.708689770883336,1.),(1.,0.708376440034494,
1.),(1.,0.707750498698415,1.),(1.,0.707106781186548,1.)))
REPRESENTATION_ITEM('')
SURFACE()
);
#2999=(
BOUNDED_SURFACE()
B_SPLINE_SURFACE(3,2,((#206485,#206486,#206487),(#206488,#206489,#206490),
(#206491,#206492,#206493),(#206494,#206495,#206496)),.UNSPECIFIED.,.F.,
 .F.,.F.)
B_SPLINE_SURFACE_WITH_KNOTS((4,4),(3,3),(-6.42389787197661E-18,0.000511815090126191),
(0.,1.00105592270157),.UNSPECIFIED.)
GEOMETRIC_REPRESENTATION_ITEM()
RATIONAL_B_SPLINE_SURFACE(((1.,0.705266242717654,1.00062243213047),(1.,
0.705584085909314,1.00062176089479),(1.,0.706182089450723,1.00062049800376),
(1.,0.706797508587648,1.00061919833368)))
REPRESENTATION_ITEM('')
SURFACE()
);
#3000=(
BOUNDED_SURFACE()
B_SPLINE_SURFACE(3,2,((#206498,#206499,#206500),(#206501,#206502,#206503),
(#206504,#206505,#206506),(#206507,#206508,#206509)),.UNSPECIFIED.,.F.,
 .F.,.F.)
B_SPLINE_SURFACE_WITH_KNOTS((4,4),(3,3),(0.,0.000397394428086633),(0.,1.),
 .UNSPECIFIED.)
GEOMETRIC_REPRESENTATION_ITEM()
RATIONAL_B_SPLINE_SURFACE(((1.,0.707106781186556,1.),(1.,0.706459846759107,
1.),(1.,0.705820510737253,1.),(1.,0.705498956110758,1.)))
REPRESENTATION_ITEM('')
SURFACE()
);
#3001=(
BOUNDED_SURFACE()
B_SPLINE_SURFACE(3,2,((#206515,#206516,#206517),(#206518,#206519,#206520),
(#206521,#206522,#206523),(#206524,#206525,#206526),(#206527,#206528,#206529),
(#206530,#206531,#206532)),.UNSPECIFIED.,.F.,.F.,.F.)
B_SPLINE_SURFACE_WITH_KNOTS((4,2,4),(3,3),(0.,0.000257953807872838,0.000515907615745676),
(0.,1.),.UNSPECIFIED.)
GEOMETRIC_REPRESENTATION_ITEM()
RATIONAL_B_SPLINE_SURFACE(((1.,0.874619707139395,1.),(1.,0.874834349679273,
1.),(1.,0.854686104157422,1.),(1.,0.792476597915473,1.),(1.,0.750887854594883,
1.),(1.,0.705585838031443,1.)))
REPRESENTATION_ITEM('')
SURFACE()
);
#3002=(
BOUNDED_SURFACE()
B_SPLINE_SURFACE(3,2,((#206538,#206539,#206540),(#206541,#206542,#206543),
(#206544,#206545,#206546),(#206547,#206548,#206549)),.UNSPECIFIED.,.F.,
 .F.,.F.)
B_SPLINE_SURFACE_WITH_KNOTS((4,4),(3,3),(0.,0.000511815437699146),(0.,1.00105881331723),
 .UNSPECIFIED.)
GEOMETRIC_REPRESENTATION_ITEM()
RATIONAL_B_SPLINE_SURFACE(((1.,0.70679666194594,1.00062089519798),(1.,0.707430821224803,
1.0006195522854),(1.,0.70805854583036,1.00061822299905),(1.,0.70839450525233,
1.00061751156243)))
REPRESENTATION_ITEM('')
SURFACE()
);
#3003=(
BOUNDED_SURFACE()
B_SPLINE_SURFACE(3,2,((#206551,#206552,#206553),(#206554,#206555,#206556),
(#206557,#206558,#206559),(#206560,#206561,#206562),(#206563,#206564,#206565),
(#206566,#206567,#206568)),.UNSPECIFIED.,.F.,.F.,.F.)
B_SPLINE_SURFACE_WITH_KNOTS((4,2,4),(3,3),(0.,0.000256915317531265,0.00051383063506253),
(0.,1.),.UNSPECIFIED.)
GEOMETRIC_REPRESENTATION_ITEM()
RATIONAL_B_SPLINE_SURFACE(((1.,0.705585838031446,1.),(1.,0.750902433543011,
1.),(1.,0.792329530082201,1.),(1.,0.854288401594521,1.),(1.,0.874998031124925,
1.),(1.,0.874619707139403,1.)))
REPRESENTATION_ITEM('')
SURFACE()
);
#3004=(
BOUNDED_SURFACE()
B_SPLINE_SURFACE(3,2,((#206574,#206575,#206576),(#206577,#206578,#206579),
(#206580,#206581,#206582),(#206583,#206584,#206585),(#206586,#206587,#206588),
(#206589,#206590,#206591)),.UNSPECIFIED.,.F.,.F.,.F.)
B_SPLINE_SURFACE_WITH_KNOTS((4,2,4),(3,3),(0.,0.000256592814262155,0.00051318562852431),
(0.,1.),.UNSPECIFIED.)
GEOMETRIC_REPRESENTATION_ITEM()
RATIONAL_B_SPLINE_SURFACE(((1.,0.708712527163695,1.),(1.,0.753780902613568,
1.),(1.,0.794538995769177,1.),(1.,0.855070770331137,1.),(1.,0.875018427445306,
1.),(1.,0.874619707139389,1.)))
REPRESENTATION_ITEM('')
SURFACE()
);
#3005=(
BOUNDED_SURFACE()
B_SPLINE_SURFACE(3,2,((#206593,#206594,#206595),(#206596,#206597,#206598),
(#206599,#206600,#206601),(#206602,#206603,#206604)),.UNSPECIFIED.,.F.,
 .F.,.F.)
B_SPLINE_SURFACE_WITH_KNOTS((4,4),(3,3),(-2.71050543121376E-20,0.00051181507243041),
(0.,1.00105598366241),.UNSPECIFIED.)
GEOMETRIC_REPRESENTATION_ITEM()
RATIONAL_B_SPLINE_SURFACE(((1.,0.706797490732659,1.00061923411913),(1.,
0.706182062145589,1.00062053388419),(1.,0.705584062767944,1.00062179683934),
(1.,0.70526622476939,1.00062246810281)))
REPRESENTATION_ITEM('')
SURFACE()
);
#3006=(
BOUNDED_SURFACE()
B_SPLINE_SURFACE(3,2,((#206610,#206611,#206612),(#206613,#206614,#206615),
(#206616,#206617,#206618),(#206619,#206620,#206621),(#206622,#206623,#206624),
(#206625,#206626,#206627)),.UNSPECIFIED.,.F.,.F.,.F.)
B_SPLINE_SURFACE_WITH_KNOTS((4,2,4),(3,3),(-9.32413868337534E-18,0.000257652232350879,
0.000515304464701767),(0.,1.),.UNSPECIFIED.)
GEOMETRIC_REPRESENTATION_ITEM()
RATIONAL_B_SPLINE_SURFACE(((1.,0.87461970713939,1.),(1.,0.874861180430825,
1.),(1.,0.855455725920677,1.),(1.,0.794699358955439,1.),(1.,0.753768977788503,
1.),(1.,0.708712527163652,1.)))
REPRESENTATION_ITEM('')
SURFACE()
);
#3007=(
BOUNDED_SURFACE()
B_SPLINE_SURFACE(3,2,((#206633,#206634,#206635),(#206636,#206637,#206638),
(#206639,#206640,#206641),(#206642,#206643,#206644)),.UNSPECIFIED.,.F.,
 .F.,.F.)
B_SPLINE_SURFACE_WITH_KNOTS((4,4),(3,3),(0.,0.000397394373651905),(0.,1.),
 .UNSPECIFIED.)
GEOMETRIC_REPRESENTATION_ITEM()
RATIONAL_B_SPLINE_SURFACE(((1.,0.707106781186555,1.),(1.,0.707752587915883,
1.),(1.,0.708377654540676,1.),(1.,0.708689770883327,1.)))
REPRESENTATION_ITEM('')
SURFACE()
);
#3008=(
BOUNDED_SURFACE()
B_SPLINE_SURFACE(3,2,((#206646,#206647,#206648),(#206649,#206650,#206651),
(#206652,#206653,#206654),(#206655,#206656,#206657)),.UNSPECIFIED.,.F.,
 .F.,.F.)
B_SPLINE_SURFACE_WITH_KNOTS((4,4),(3,3),(0.,0.000511815456479779),(0.,1.00105873160079),
 .UNSPECIFIED.)
GEOMETRIC_REPRESENTATION_ITEM()
RATIONAL_B_SPLINE_SURFACE(((1.,0.708394529056081,1.0006174638541),(1.,0.708058564166629,
1.00061817524739),(1.,0.70743083537183,1.00061950444001),(1.,0.706796685880126,
1.00062084722823)))
REPRESENTATION_ITEM('')
SURFACE()
);
#3009=(
BOUNDED_SURFACE()
B_SPLINE_SURFACE(3,2,((#206663,#206664,#206665),(#206666,#206667,#206668),
(#206669,#206670,#206671),(#206672,#206673,#206674)),.UNSPECIFIED.,.F.,
 .F.,.F.)
B_SPLINE_SURFACE_WITH_KNOTS((4,4),(3,3),(0.,0.000397394465448301),(0.,1.),
 .UNSPECIFIED.)
GEOMETRIC_REPRESENTATION_ITEM()
RATIONAL_B_SPLINE_SURFACE(((1.,0.705498956110756,1.),(1.,0.70582176481178,
1.),(1.,0.706461952521141,1.),(1.,0.707106781186548,1.)))
REPRESENTATION_ITEM('')
SURFACE()
);
#3010=(
BOUNDED_SURFACE()
B_SPLINE_SURFACE(3,2,((#206680,#206681,#206682),(#206683,#206684,#206685),
(#206686,#206687,#206688),(#206689,#206690,#206691)),.UNSPECIFIED.,.F.,
 .F.,.F.)
B_SPLINE_SURFACE_WITH_KNOTS((4,4),(3,3),(0.,0.000397394410828731),(0.,1.),
 .UNSPECIFIED.)
GEOMETRIC_REPRESENTATION_ITEM()
RATIONAL_B_SPLINE_SURFACE(((1.,0.708689770883319,1.),(1.,0.708376440034476,
1.),(1.,0.707750498698424,1.),(1.,0.707106781186548,1.)))
REPRESENTATION_ITEM('')
SURFACE()
);
#3011=(
BOUNDED_SURFACE()
B_SPLINE_SURFACE(3,2,((#206697,#206698,#206699),(#206700,#206701,#206702),
(#206703,#206704,#206705),(#206706,#206707,#206708)),.UNSPECIFIED.,.F.,
 .F.,.F.)
B_SPLINE_SURFACE_WITH_KNOTS((4,4),(3,3),(0.,0.000511815090126184),(0.,1.00105592270507),
 .UNSPECIFIED.)
GEOMETRIC_REPRESENTATION_ITEM()
RATIONAL_B_SPLINE_SURFACE(((1.,0.705266242716637,1.00062243213253),(1.,
0.705584085908299,1.00062176089685),(1.,0.706182089449661,1.00062049800581),
(1.,0.70679750858664,1.00061919833573)))
REPRESENTATION_ITEM('')
SURFACE()
);
#3012=(
BOUNDED_SURFACE()
B_SPLINE_SURFACE(3,2,((#206710,#206711,#206712),(#206713,#206714,#206715),
(#206716,#206717,#206718),(#206719,#206720,#206721)),.UNSPECIFIED.,.F.,
 .F.,.F.)
B_SPLINE_SURFACE_WITH_KNOTS((4,4),(3,3),(0.,0.000397394428086631),(0.,1.),
 .UNSPECIFIED.)
GEOMETRIC_REPRESENTATION_ITEM()
RATIONAL_B_SPLINE_SURFACE(((1.,0.707106781186548,1.),(1.,0.706459846759093,
1.),(1.,0.705820510737288,1.),(1.,0.705498956110764,1.)))
REPRESENTATION_ITEM('')
SURFACE()
);
#3013=(
BOUNDED_SURFACE()
B_SPLINE_SURFACE(3,2,((#206727,#206728,#206729),(#206730,#206731,#206732),
(#206733,#206734,#206735),(#206736,#206737,#206738),(#206739,#206740,#206741),
(#206742,#206743,#206744)),.UNSPECIFIED.,.F.,.F.,.F.)
B_SPLINE_SURFACE_WITH_KNOTS((4,2,4),(3,3),(0.,0.000257953807872847,0.000515907615745693),
(0.,1.),.UNSPECIFIED.)
GEOMETRIC_REPRESENTATION_ITEM()
RATIONAL_B_SPLINE_SURFACE(((1.,0.874619707139398,1.),(1.,0.874834349679205,
1.),(1.,0.854686104157519,1.),(1.,0.792476597915395,1.),(1.,0.750887854594947,
1.),(1.,0.705585838031442,1.)))
REPRESENTATION_ITEM('')
SURFACE()
);
#3014=(
BOUNDED_SURFACE()
B_SPLINE_SURFACE(3,2,((#206750,#206751,#206752),(#206753,#206754,#206755),
(#206756,#206757,#206758),(#206759,#206760,#206761)),.UNSPECIFIED.,.F.,
 .F.,.F.)
B_SPLINE_SURFACE_WITH_KNOTS((4,4),(3,3),(0.,0.000511815437699154),(0.,1.00105881331611),
 .UNSPECIFIED.)
GEOMETRIC_REPRESENTATION_ITEM()
RATIONAL_B_SPLINE_SURFACE(((1.,0.706796661946269,1.00062089519732),(1.,
0.707430821225167,1.00061955228474),(1.,0.708058545830613,1.0006182229984),
(1.,0.708394505252643,1.00061751156178)))
REPRESENTATION_ITEM('')
SURFACE()
);
#3015=(
BOUNDED_SURFACE()
B_SPLINE_SURFACE(3,2,((#206763,#206764,#206765),(#206766,#206767,#206768),
(#206769,#206770,#206771),(#206772,#206773,#206774),(#206775,#206776,#206777),
(#206778,#206779,#206780)),.UNSPECIFIED.,.F.,.F.,.F.)
B_SPLINE_SURFACE_WITH_KNOTS((4,2,4),(3,3),(9.97465998686664E-18,0.000256915317531272,
0.000513830635062533),(0.,1.),.UNSPECIFIED.)
GEOMETRIC_REPRESENTATION_ITEM()
RATIONAL_B_SPLINE_SURFACE(((1.,0.705585838031435,1.),(1.,0.750902433542796,
1.),(1.,0.792329530082492,1.),(1.,0.854288401594256,1.),(1.,0.874998031125097,
1.),(1.,0.874619707139405,1.)))
REPRESENTATION_ITEM('')
SURFACE()
);
#3016=(
BOUNDED_SURFACE()
B_SPLINE_SURFACE(3,2,((#206786,#206787,#206788),(#206789,#206790,#206791),
(#206792,#206793,#206794),(#206795,#206796,#206797),(#206798,#206799,#206800),
(#206801,#206802,#206803)),.UNSPECIFIED.,.F.,.F.,.F.)
B_SPLINE_SURFACE_WITH_KNOTS((4,2,4),(3,3),(0.,0.000256592814262155,0.00051318562852431),
(0.,1.),.UNSPECIFIED.)
GEOMETRIC_REPRESENTATION_ITEM()
RATIONAL_B_SPLINE_SURFACE(((1.,0.708712527163649,1.),(1.,0.753780902613242,
1.),(1.,0.794538995769662,1.),(1.,0.855070770330658,1.),(1.,0.875018427445663,
1.),(1.,0.874619707139383,1.)))
REPRESENTATION_ITEM('')
SURFACE()
);
#3017=(
BOUNDED_SURFACE()
B_SPLINE_SURFACE(3,2,((#206805,#206806,#206807),(#206808,#206809,#206810),
(#206811,#206812,#206813),(#206814,#206815,#206816)),.UNSPECIFIED.,.F.,
 .F.,.F.)
B_SPLINE_SURFACE_WITH_KNOTS((4,4),(3,3),(2.71050543121376E-20,0.0005118150724304),
(0.,1.00105598365872),.UNSPECIFIED.)
GEOMETRIC_REPRESENTATION_ITEM()
RATIONAL_B_SPLINE_SURFACE(((1.,0.70679749073373,1.00061923411696),(1.,0.706182062146616,
1.00062053388202),(1.,0.705584062769036,1.00062179683717),(1.,0.705266224770467,
1.00062246810063)))
REPRESENTATION_ITEM('')
SURFACE()
);
#3018=(
BOUNDED_SURFACE()
B_SPLINE_SURFACE(3,2,((#206822,#206823,#206824),(#206825,#206826,#206827),
(#206828,#206829,#206830),(#206831,#206832,#206833),(#206834,#206835,#206836),
(#206837,#206838,#206839)),.UNSPECIFIED.,.F.,.F.,.F.)
B_SPLINE_SURFACE_WITH_KNOTS((4,2,4),(3,3),(-3.15773882736403E-18,0.000257652232350885,
0.000515304464701772),(0.,1.),.UNSPECIFIED.)
GEOMETRIC_REPRESENTATION_ITEM()
RATIONAL_B_SPLINE_SURFACE(((1.,0.874619707139379,1.),(1.,0.874861180430934,
1.),(1.,0.855455725920527,1.),(1.,0.794699358955577,1.),(1.,0.753768977788386,
1.),(1.,0.708712527163667,1.)))
REPRESENTATION_ITEM('')
SURFACE()
);
#3019=(
BOUNDED_SURFACE()
B_SPLINE_SURFACE(3,2,((#206845,#206846,#206847),(#206848,#206849,#206850),
(#206851,#206852,#206853),(#206854,#206855,#206856)),.UNSPECIFIED.,.F.,
 .F.,.F.)
B_SPLINE_SURFACE_WITH_KNOTS((4,4),(3,3),(0.,0.000397394373651917),(0.,1.),
 .UNSPECIFIED.)
GEOMETRIC_REPRESENTATION_ITEM()
RATIONAL_B_SPLINE_SURFACE(((1.,0.707106781186553,1.),(1.,0.707752587915892,
1.),(1.,0.708377654540686,1.),(1.,0.708689770883343,1.)))
REPRESENTATION_ITEM('')
SURFACE()
);
#3020=(
BOUNDED_SURFACE()
B_SPLINE_SURFACE(3,2,((#206858,#206859,#206860),(#206861,#206862,#206863),
(#206864,#206865,#206866),(#206867,#206868,#206869)),.UNSPECIFIED.,.F.,
 .F.,.F.)
B_SPLINE_SURFACE_WITH_KNOTS((4,4),(3,3),(0.,0.000511815456479782),(0.,1.00105873160063),
 .UNSPECIFIED.)
GEOMETRIC_REPRESENTATION_ITEM()
RATIONAL_B_SPLINE_SURFACE(((1.,0.708394529056139,1.00061746385401),(1.,
0.708058564166688,1.0006181752473),(1.,0.707430835371857,1.00061950443992),
(1.,0.70679668588018,1.00062084722814)))
REPRESENTATION_ITEM('')
SURFACE()
);
#3021=(
BOUNDED_SURFACE()
B_SPLINE_SURFACE(3,2,((#206875,#206876,#206877),(#206878,#206879,#206880),
(#206881,#206882,#206883),(#206884,#206885,#206886)),.UNSPECIFIED.,.F.,
 .F.,.F.)
B_SPLINE_SURFACE_WITH_KNOTS((4,4),(3,3),(0.,0.000397394465448316),(0.,1.),
 .UNSPECIFIED.)
GEOMETRIC_REPRESENTATION_ITEM()
RATIONAL_B_SPLINE_SURFACE(((1.,0.705498956110747,1.),(1.,0.705821764811782,
1.),(1.,0.706461952521135,1.),(1.,0.707106781186548,1.)))
REPRESENTATION_ITEM('')
SURFACE()
);
#3022=(
BOUNDED_SURFACE()
B_SPLINE_SURFACE(3,2,((#206892,#206893,#206894),(#206895,#206896,#206897),
(#206898,#206899,#206900),(#206901,#206902,#206903)),.UNSPECIFIED.,.F.,
 .F.,.F.)
B_SPLINE_SURFACE_WITH_KNOTS((4,4),(3,3),(0.,0.000397394410828751),(0.,1.),
 .UNSPECIFIED.)
GEOMETRIC_REPRESENTATION_ITEM()
RATIONAL_B_SPLINE_SURFACE(((1.,0.708689770883333,1.),(1.,0.708376440034456,
1.),(1.,0.707750498698422,1.),(1.,0.707106781186552,1.)))
REPRESENTATION_ITEM('')
SURFACE()
);
#3023=(
BOUNDED_SURFACE()
B_SPLINE_SURFACE(3,2,((#206909,#206910,#206911),(#206912,#206913,#206914),
(#206915,#206916,#206917),(#206918,#206919,#206920)),.UNSPECIFIED.,.F.,
 .F.,.F.)
B_SPLINE_SURFACE_WITH_KNOTS((4,4),(3,3),(0.,0.000511815090126177),(0.,1.00105592270027),
 .UNSPECIFIED.)
GEOMETRIC_REPRESENTATION_ITEM()
RATIONAL_B_SPLINE_SURFACE(((1.,0.70526624271804,1.0006224321297),(1.,0.70558408590973,
1.00062176089402),(1.,0.706182089451049,1.00062049800299),(1.,0.706797508588047,
1.00061919833292)))
REPRESENTATION_ITEM('')
SURFACE()
);
#3024=(
BOUNDED_SURFACE()
B_SPLINE_SURFACE(3,2,((#206922,#206923,#206924),(#206925,#206926,#206927),
(#206928,#206929,#206930),(#206931,#206932,#206933)),.UNSPECIFIED.,.F.,
 .F.,.F.)
B_SPLINE_SURFACE_WITH_KNOTS((4,4),(3,3),(-7.04731412115578E-18,0.000397394428086623),
(0.,1.),.UNSPECIFIED.)
GEOMETRIC_REPRESENTATION_ITEM()
RATIONAL_B_SPLINE_SURFACE(((1.,0.707106781186552,1.),(1.,0.706459846759081,
1.),(1.,0.705820510737286,1.),(1.,0.705498956110751,1.)))
REPRESENTATION_ITEM('')
SURFACE()
);
#3025=(
BOUNDED_SURFACE()
B_SPLINE_SURFACE(3,2,((#206939,#206940,#206941),(#206942,#206943,#206944),
(#206945,#206946,#206947),(#206948,#206949,#206950),(#206951,#206952,#206953),
(#206954,#206955,#206956)),.UNSPECIFIED.,.F.,.F.,.F.)
B_SPLINE_SURFACE_WITH_KNOTS((4,2,4),(3,3),(0.,0.000257953807872837,0.000515907615745674),
(0.,1.),.UNSPECIFIED.)
GEOMETRIC_REPRESENTATION_ITEM()
RATIONAL_B_SPLINE_SURFACE(((1.,0.874619707139392,1.),(1.,0.874834349678964,
1.),(1.,0.854686104157824,1.),(1.,0.792476597915125,1.),(1.,0.750887854595146,
1.),(1.,0.705585838031451,1.)))
REPRESENTATION_ITEM('')
SURFACE()
);
#3026=(
BOUNDED_SURFACE()
B_SPLINE_SURFACE(3,2,((#206962,#206963,#206964),(#206965,#206966,#206967),
(#206968,#206969,#206970),(#206971,#206972,#206973)),.UNSPECIFIED.,.F.,
 .F.,.F.)
B_SPLINE_SURFACE_WITH_KNOTS((4,4),(3,3),(0.,0.000511815437699147),(0.,1.00105881331747),
 .UNSPECIFIED.)
GEOMETRIC_REPRESENTATION_ITEM()
RATIONAL_B_SPLINE_SURFACE(((1.,0.706796661945872,1.00062089519812),(1.,
0.707430821224739,1.00061955228554),(1.,0.708058545830266,1.00061822299919),
(1.,0.708394505252261,1.00061751156257)))
REPRESENTATION_ITEM('')
SURFACE()
);
#3027=(
BOUNDED_SURFACE()
B_SPLINE_SURFACE(3,2,((#206975,#206976,#206977),(#206978,#206979,#206980),
(#206981,#206982,#206983),(#206984,#206985,#206986),(#206987,#206988,#206989),
(#206990,#206991,#206992)),.UNSPECIFIED.,.F.,.F.,.F.)
B_SPLINE_SURFACE_WITH_KNOTS((4,2,4),(3,3),(0.,0.00025691531753126,0.000513830635062519),
(0.,1.),.UNSPECIFIED.)
GEOMETRIC_REPRESENTATION_ITEM()
RATIONAL_B_SPLINE_SURFACE(((1.,0.705585838031444,1.),(1.,0.750902433543079,
1.),(1.,0.79232953008207,1.),(1.,0.854288401594637,1.),(1.,0.874998031124809,
1.),(1.,0.874619707139393,1.)))
REPRESENTATION_ITEM('')
SURFACE()
);
#3028=(
BOUNDED_SURFACE()
B_SPLINE_SURFACE(3,2,((#206998,#206999,#207000),(#207001,#207002,#207003),
(#207004,#207005,#207006),(#207007,#207008,#207009),(#207010,#207011,#207012),
(#207013,#207014,#207015)),.UNSPECIFIED.,.F.,.F.,.F.)
B_SPLINE_SURFACE_WITH_KNOTS((4,2,4),(3,3),(0.,0.000256592814262157,0.000513185628524314),
(0.,1.),.UNSPECIFIED.)
GEOMETRIC_REPRESENTATION_ITEM()
RATIONAL_B_SPLINE_SURFACE(((1.,0.708712527163661,1.),(1.,0.753780902613635,
1.),(1.,0.794538995769146,1.),(1.,0.855070770331154,1.),(1.,0.875018427445277,
1.),(1.,0.874619707139389,1.)))
REPRESENTATION_ITEM('')
SURFACE()
);
#3029=(
BOUNDED_SURFACE()
B_SPLINE_SURFACE(3,2,((#207017,#207018,#207019),(#207020,#207021,#207022),
(#207023,#207024,#207025),(#207026,#207027,#207028)),.UNSPECIFIED.,.F.,
 .F.,.F.)
B_SPLINE_SURFACE_WITH_KNOTS((4,4),(3,3),(2.71050543121376E-20,0.000511815072430401),
(0.,1.00105598365816),.UNSPECIFIED.)
GEOMETRIC_REPRESENTATION_ITEM()
RATIONAL_B_SPLINE_SURFACE(((1.,0.706797490733895,1.00061923411663),(1.,
0.706182062146812,1.00062053388169),(1.,0.705584062769175,1.00062179683683),
(1.,0.705266224770663,1.0006224681003)))
REPRESENTATION_ITEM('')
SURFACE()
);
#3030=(
BOUNDED_SURFACE()
B_SPLINE_SURFACE(3,2,((#207034,#207035,#207036),(#207037,#207038,#207039),
(#207040,#207041,#207042),(#207043,#207044,#207045),(#207046,#207047,#207048),
(#207049,#207050,#207051)),.UNSPECIFIED.,.F.,.F.,.F.)
B_SPLINE_SURFACE_WITH_KNOTS((4,2,4),(3,3),(-1.35525271560688E-20,0.000257652232350881,
0.000515304464701761),(0.,1.),.UNSPECIFIED.)
GEOMETRIC_REPRESENTATION_ITEM()
RATIONAL_B_SPLINE_SURFACE(((1.,0.874619707139399,1.),(1.,0.87486118043092,
1.),(1.,0.855455725920554,1.),(1.,0.794699358955568,1.),(1.,0.753768977788393,
1.),(1.,0.708712527163671,1.)))
REPRESENTATION_ITEM('')
SURFACE()
);
#3031=(
BOUNDED_SURFACE()
B_SPLINE_SURFACE(3,2,((#207057,#207058,#207059),(#207060,#207061,#207062),
(#207063,#207064,#207065),(#207066,#207067,#207068)),.UNSPECIFIED.,.F.,
 .F.,.F.)
B_SPLINE_SURFACE_WITH_KNOTS((4,4),(3,3),(0.,0.000397394373651918),(0.,1.),
 .UNSPECIFIED.)
GEOMETRIC_REPRESENTATION_ITEM()
RATIONAL_B_SPLINE_SURFACE(((1.,0.707106781186552,1.),(1.,0.707752587915896,
1.),(1.,0.708377654540672,1.),(1.,0.708689770883335,1.)))
REPRESENTATION_ITEM('')
SURFACE()
);
#3032=(
BOUNDED_SURFACE()
B_SPLINE_SURFACE(3,2,((#207070,#207071,#207072),(#207073,#207074,#207075),
(#207076,#207077,#207078),(#207079,#207080,#207081)),.UNSPECIFIED.,.F.,
 .F.,.F.)
B_SPLINE_SURFACE_WITH_KNOTS((4,4),(3,3),(0.,0.000511815456479794),(0.,1.00105873159933),
 .UNSPECIFIED.)
GEOMETRIC_REPRESENTATION_ITEM()
RATIONAL_B_SPLINE_SURFACE(((1.,0.708394529056518,1.00061746385325),(1.,
0.708058564167052,1.00061817524654),(1.,0.707430835372237,1.00061950443916),
(1.,0.706796685880559,1.00062084722737)))
REPRESENTATION_ITEM('')
SURFACE()
);
#3033=(
BOUNDED_SURFACE()
B_SPLINE_SURFACE(3,2,((#207087,#207088,#207089),(#207090,#207091,#207092),
(#207093,#207094,#207095),(#207096,#207097,#207098)),.UNSPECIFIED.,.F.,
 .F.,.F.)
B_SPLINE_SURFACE_WITH_KNOTS((4,4),(3,3),(0.,0.000397394465448303),(0.,1.),
 .UNSPECIFIED.)
GEOMETRIC_REPRESENTATION_ITEM()
RATIONAL_B_SPLINE_SURFACE(((1.,0.705498956110754,1.),(1.,0.705821764811766,
1.),(1.,0.706461952521146,1.),(1.,0.707106781186548,1.)))
REPRESENTATION_ITEM('')
SURFACE()
);
#3034=(
BOUNDED_SURFACE()
B_SPLINE_SURFACE(3,2,((#207104,#207105,#207106),(#207107,#207108,#207109),
(#207110,#207111,#207112),(#207113,#207114,#207115)),.UNSPECIFIED.,.F.,
 .F.,.F.)
B_SPLINE_SURFACE_WITH_KNOTS((4,4),(3,3),(0.,0.000397394410828732),(0.,1.),
 .UNSPECIFIED.)
GEOMETRIC_REPRESENTATION_ITEM()
RATIONAL_B_SPLINE_SURFACE(((1.,0.708689770883346,1.),(1.,0.708376440034465,
1.),(1.,0.707750498698423,1.),(1.,0.707106781186548,1.)))
REPRESENTATION_ITEM('')
SURFACE()
);
#3035=(
BOUNDED_SURFACE()
B_SPLINE_SURFACE(3,2,((#207121,#207122,#207123),(#207124,#207125,#207126),
(#207127,#207128,#207129),(#207130,#207131,#207132)),.UNSPECIFIED.,.F.,
 .F.,.F.)
B_SPLINE_SURFACE_WITH_KNOTS((4,4),(3,3),(0.,0.000511815090126172),(0.,1.00105592270163),
 .UNSPECIFIED.)
GEOMETRIC_REPRESENTATION_ITEM()
RATIONAL_B_SPLINE_SURFACE(((1.,0.705266242717656,1.0006224321305),(1.,0.705584085909297,
1.00062176089482),(1.,0.706182089450663,1.00062049800379),(1.,0.706797508587648,
1.00061919833372)))
REPRESENTATION_ITEM('')
SURFACE()
);
#3036=(
BOUNDED_SURFACE()
B_SPLINE_SURFACE(3,2,((#207134,#207135,#207136),(#207137,#207138,#207139),
(#207140,#207141,#207142),(#207143,#207144,#207145)),.UNSPECIFIED.,.F.,
 .F.,.F.)
B_SPLINE_SURFACE_WITH_KNOTS((4,4),(3,3),(0.,0.000397394428086631),(0.,1.),
 .UNSPECIFIED.)
GEOMETRIC_REPRESENTATION_ITEM()
RATIONAL_B_SPLINE_SURFACE(((1.,0.707106781186548,1.),(1.,0.706459846759101,
1.),(1.,0.705820510737274,1.),(1.,0.705498956110758,1.)))
REPRESENTATION_ITEM('')
SURFACE()
);
#3037=(
BOUNDED_SURFACE()
B_SPLINE_SURFACE(3,2,((#207151,#207152,#207153),(#207154,#207155,#207156),
(#207157,#207158,#207159),(#207160,#207161,#207162),(#207163,#207164,#207165),
(#207166,#207167,#207168)),.UNSPECIFIED.,.F.,.F.,.F.)
B_SPLINE_SURFACE_WITH_KNOTS((4,2,4),(3,3),(0.,0.000257953807872843,0.000515907615745686),
(0.,1.),.UNSPECIFIED.)
GEOMETRIC_REPRESENTATION_ITEM()
RATIONAL_B_SPLINE_SURFACE(((1.,0.874619707139387,1.),(1.,0.874834349679408,
1.),(1.,0.854686104157222,1.),(1.,0.792476597915714,1.),(1.,0.750887854594714,
1.),(1.,0.70558583803143,1.)))
REPRESENTATION_ITEM('')
SURFACE()
);
#3038=(
BOUNDED_SURFACE()
B_SPLINE_SURFACE(3,2,((#207174,#207175,#207176),(#207177,#207178,#207179),
(#207180,#207181,#207182),(#207183,#207184,#207185)),.UNSPECIFIED.,.F.,
 .F.,.F.)
B_SPLINE_SURFACE_WITH_KNOTS((4,4),(3,3),(0.,0.000511815437699148),(0.,1.00105881331484),
 .UNSPECIFIED.)
GEOMETRIC_REPRESENTATION_ITEM()
RATIONAL_B_SPLINE_SURFACE(((1.,0.706796661946642,1.00062089519658),(1.,
0.707430821225516,1.000619552284),(1.,0.708058545831031,1.00061822299766),
(1.,0.708394505253015,1.00061751156104)))
REPRESENTATION_ITEM('')
SURFACE()
);
#3039=(
BOUNDED_SURFACE()
B_SPLINE_SURFACE(3,2,((#207187,#207188,#207189),(#207190,#207191,#207192),
(#207193,#207194,#207195),(#207196,#207197,#207198),(#207199,#207200,#207201),
(#207202,#207203,#207204)),.UNSPECIFIED.,.F.,.F.,.F.)
B_SPLINE_SURFACE_WITH_KNOTS((4,2,4),(3,3),(2.71050543121376E-20,0.000256915317531269,
0.000513830635062539),(0.,1.),.UNSPECIFIED.)
GEOMETRIC_REPRESENTATION_ITEM()
RATIONAL_B_SPLINE_SURFACE(((1.,0.705585838031441,1.),(1.,0.750902433542262,
1.),(1.,0.792329530083195,1.),(1.,0.854288401593528,1.),(1.,0.874998031125646,
1.),(1.,0.874619707139414,1.)))
REPRESENTATION_ITEM('')
SURFACE()
);
#3040=(
BOUNDED_SURFACE()
B_SPLINE_SURFACE(3,2,((#207210,#207211,#207212),(#207213,#207214,#207215),
(#207216,#207217,#207218),(#207219,#207220,#207221),(#207222,#207223,#207224),
(#207225,#207226,#207227)),.UNSPECIFIED.,.F.,.F.,.F.)
B_SPLINE_SURFACE_WITH_KNOTS((4,2,4),(3,3),(-9.64939933512099E-18,0.00025659281426215,
0.000513185628524309),(0.,1.),.UNSPECIFIED.)
GEOMETRIC_REPRESENTATION_ITEM()
RATIONAL_B_SPLINE_SURFACE(((1.,0.708712527163639,1.),(1.,0.753780902613581,
1.),(1.,0.79453899576923,1.),(1.,0.855070770331076,1.),(1.,0.875018427445352,
1.),(1.,0.874619707139392,1.)))
REPRESENTATION_ITEM('')
SURFACE()
);
#3041=(
BOUNDED_SURFACE()
B_SPLINE_SURFACE(3,2,((#207229,#207230,#207231),(#207232,#207233,#207234),
(#207235,#207236,#207237),(#207238,#207239,#207240)),.UNSPECIFIED.,.F.,
 .F.,.F.)
B_SPLINE_SURFACE_WITH_KNOTS((4,4),(3,3),(0.,0.000511815072430398),(0.,1.00105598365608),
 .UNSPECIFIED.)
GEOMETRIC_REPRESENTATION_ITEM()
RATIONAL_B_SPLINE_SURFACE(((1.,0.706797490734501,1.00061923411541),(1.,
0.706182062147433,1.00062053388047),(1.,0.705584062769772,1.00062179683561),
(1.,0.705266224771265,1.00062246809907)))
REPRESENTATION_ITEM('')
SURFACE()
);
#3042=(
BOUNDED_SURFACE()
B_SPLINE_SURFACE(3,2,((#207246,#207247,#207248),(#207249,#207250,#207251),
(#207252,#207253,#207254),(#207255,#207256,#207257),(#207258,#207259,#207260),
(#207261,#207262,#207263)),.UNSPECIFIED.,.F.,.F.,.F.)
B_SPLINE_SURFACE_WITH_KNOTS((4,2,4),(3,3),(-8.53809210832335E-19,0.000257652232350883,
0.000515304464701767),(0.,1.),.UNSPECIFIED.)
GEOMETRIC_REPRESENTATION_ITEM()
RATIONAL_B_SPLINE_SURFACE(((1.,0.874619707139377,1.),(1.,0.874861180430964,
1.),(1.,0.855455725920508,1.),(1.,0.794699358955598,1.),(1.,0.753768977788379,
1.),(1.,0.708712527163652,1.)))
REPRESENTATION_ITEM('')
SURFACE()
);
#3043=(
BOUNDED_SURFACE()
B_SPLINE_SURFACE(3,2,((#207269,#207270,#207271),(#207272,#207273,#207274),
(#207275,#207276,#207277),(#207278,#207279,#207280)),.UNSPECIFIED.,.F.,
 .F.,.F.)
B_SPLINE_SURFACE_WITH_KNOTS((4,4),(3,3),(0.,0.000397394373651916),(0.,1.),
 .UNSPECIFIED.)
GEOMETRIC_REPRESENTATION_ITEM()
RATIONAL_B_SPLINE_SURFACE(((1.,0.707106781186548,1.),(1.,0.707752587915897,
1.),(1.,0.708377654540682,1.),(1.,0.708689770883335,1.)))
REPRESENTATION_ITEM('')
SURFACE()
);
#3044=(
BOUNDED_SURFACE()
B_SPLINE_SURFACE(3,2,((#207282,#207283,#207284),(#207285,#207286,#207287),
(#207288,#207289,#207290),(#207291,#207292,#207293)),.UNSPECIFIED.,.F.,
 .F.,.F.)
B_SPLINE_SURFACE_WITH_KNOTS((4,4),(3,3),(0.,0.000511815456479795),(0.,1.00105873160039),
 .UNSPECIFIED.)
GEOMETRIC_REPRESENTATION_ITEM()
RATIONAL_B_SPLINE_SURFACE(((1.,0.708394529056206,1.00061746385387),(1.,
0.708058564166753,1.00061817524716),(1.,0.70743083537193,1.00061950443978),
(1.,0.706796685880251,1.00062084722799)))
REPRESENTATION_ITEM('')
SURFACE()
);
#3045=(
BOUNDED_SURFACE()
B_SPLINE_SURFACE(3,2,((#207299,#207300,#207301),(#207302,#207303,#207304),
(#207305,#207306,#207307),(#207308,#207309,#207310)),.UNSPECIFIED.,.F.,
 .F.,.F.)
B_SPLINE_SURFACE_WITH_KNOTS((4,4),(3,3),(-6.50521303491303E-18,0.000397394465448295),
(0.,1.),.UNSPECIFIED.)
GEOMETRIC_REPRESENTATION_ITEM()
RATIONAL_B_SPLINE_SURFACE(((1.,0.705498956110765,1.),(1.,0.705821764811772,
1.),(1.,0.706461952521134,1.),(1.,0.70710678118655,1.)))
REPRESENTATION_ITEM('')
SURFACE()
);
#3046=(
BOUNDED_SURFACE()
B_SPLINE_SURFACE(3,2,((#207316,#207317,#207318),(#207319,#207320,#207321),
(#207322,#207323,#207324),(#207325,#207326,#207327)),.UNSPECIFIED.,.F.,
 .F.,.F.)
B_SPLINE_SURFACE_WITH_KNOTS((4,4),(3,3),(0.,0.000397394410828733),(0.,1.),
 .UNSPECIFIED.)
GEOMETRIC_REPRESENTATION_ITEM()
RATIONAL_B_SPLINE_SURFACE(((1.,0.708689770883334,1.),(1.,0.708376440034491,
1.),(1.,0.707750498698413,1.),(1.,0.707106781186548,1.)))
REPRESENTATION_ITEM('')
SURFACE()
);
#3047=(
BOUNDED_SURFACE()
B_SPLINE_SURFACE(3,2,((#207333,#207334,#207335),(#207336,#207337,#207338),
(#207339,#207340,#207341),(#207342,#207343,#207344)),.UNSPECIFIED.,.F.,
 .F.,.F.)
B_SPLINE_SURFACE_WITH_KNOTS((4,4),(3,3),(0.,0.000511815090126173),(0.,1.00105592270208),
 .UNSPECIFIED.)
GEOMETRIC_REPRESENTATION_ITEM()
RATIONAL_B_SPLINE_SURFACE(((1.,0.705266242717518,1.00062243213077),(1.,
0.705584085909175,1.00062176089508),(1.,0.706182089450533,1.00062049800405),
(1.,0.706797508587518,1.00061919833398)))
REPRESENTATION_ITEM('')
SURFACE()
);
#3048=(
BOUNDED_SURFACE()
B_SPLINE_SURFACE(3,2,((#207346,#207347,#207348),(#207349,#207350,#207351),
(#207352,#207353,#207354),(#207355,#207356,#207357)),.UNSPECIFIED.,.F.,
 .F.,.F.)
B_SPLINE_SURFACE_WITH_KNOTS((4,4),(3,3),(0.,0.000397394428086626),(0.,1.),
 .UNSPECIFIED.)
GEOMETRIC_REPRESENTATION_ITEM()
RATIONAL_B_SPLINE_SURFACE(((1.,0.707106781186548,1.),(1.,0.7064598467591,
1.),(1.,0.70582051073725,1.),(1.,0.705498956110749,1.)))
REPRESENTATION_ITEM('')
SURFACE()
);
#3049=(
BOUNDED_SURFACE()
B_SPLINE_SURFACE(3,2,((#207363,#207364,#207365),(#207366,#207367,#207368),
(#207369,#207370,#207371),(#207372,#207373,#207374),(#207375,#207376,#207377),
(#207378,#207379,#207380)),.UNSPECIFIED.,.F.,.F.,.F.)
B_SPLINE_SURFACE_WITH_KNOTS((4,2,4),(3,3),(0.,0.000257953807872854,0.000515907615745708),
(0.,1.),.UNSPECIFIED.)
GEOMETRIC_REPRESENTATION_ITEM()
RATIONAL_B_SPLINE_SURFACE(((1.,0.874619707139392,1.),(1.,0.874834349678953,
1.),(1.,0.854686104157836,1.),(1.,0.792476597915084,1.),(1.,0.750887854595165,
1.),(1.,0.705585838031428,1.)))
REPRESENTATION_ITEM('')
SURFACE()
);
#3050=(
BOUNDED_SURFACE()
B_SPLINE_SURFACE(3,2,((#207383,#207384,#207385),(#207386,#207387,#207388),
(#207389,#207390,#207391),(#207392,#207393,#207394)),.UNSPECIFIED.,.F.,
 .F.,.F.)
B_SPLINE_SURFACE_WITH_KNOTS((4,4),(3,3),(0.,0.000511815437699152),(0.,1.0010588133155),
 .UNSPECIFIED.)
GEOMETRIC_REPRESENTATION_ITEM()
RATIONAL_B_SPLINE_SURFACE(((1.,0.706796661946447,1.00062089519696),(1.,
0.707430821225326,1.00061955228439),(1.,0.708058545830837,1.00061822299804),
(1.,0.708394505252831,1.00061751156143)))
REPRESENTATION_ITEM('')
SURFACE()
);
#3051=(
BOUNDED_SURFACE()
B_SPLINE_SURFACE(3,2,((#207396,#207397,#207398),(#207399,#207400,#207401),
(#207402,#207403,#207404),(#207405,#207406,#207407),(#207408,#207409,#207410),
(#207411,#207412,#207413)),.UNSPECIFIED.,.F.,.F.,.F.)
B_SPLINE_SURFACE_WITH_KNOTS((4,2,4),(3,3),(0.,0.000256915317531263,0.000513830635062526),
(0.,1.),.UNSPECIFIED.)
GEOMETRIC_REPRESENTATION_ITEM()
RATIONAL_B_SPLINE_SURFACE(((1.,0.705585838031434,1.),(1.,0.750902433542931,
1.),(1.,0.792329530082276,1.),(1.,0.854288401594432,1.),(1.,0.874998031124954,
1.),(1.,0.874619707139392,1.)))
REPRESENTATION_ITEM('')
SURFACE()
);
#3052=(
BOUNDED_SURFACE()
B_SPLINE_SURFACE(3,2,((#207419,#207420,#207421),(#207422,#207423,#207424),
(#207425,#207426,#207427),(#207428,#207429,#207430),(#207431,#207432,#207433),
(#207434,#207435,#207436)),.UNSPECIFIED.,.F.,.F.,.F.)
B_SPLINE_SURFACE_WITH_KNOTS((4,2,4),(3,3),(-9.7307144980574E-18,0.000256592814262151,
0.000513185628524313),(0.,1.),.UNSPECIFIED.)
GEOMETRIC_REPRESENTATION_ITEM()
RATIONAL_B_SPLINE_SURFACE(((1.,0.708712527163666,1.),(1.,0.753780902613597,
1.),(1.,0.794538995769187,1.),(1.,0.855070770331129,1.),(1.,0.875018427445299,
1.),(1.,0.87461970713939,1.)))
REPRESENTATION_ITEM('')
SURFACE()
);
#3053=(
BOUNDED_SURFACE()
B_SPLINE_SURFACE(3,2,((#207437,#207438,#207439),(#207440,#207441,#207442),
(#207443,#207444,#207445),(#207446,#207447,#207448)),.UNSPECIFIED.,.F.,
 .F.,.F.)
B_SPLINE_SURFACE_WITH_KNOTS((4,4),(3,3),(0.,0.000511815072430396),(0.,1.00105598365805),
 .UNSPECIFIED.)
GEOMETRIC_REPRESENTATION_ITEM()
RATIONAL_B_SPLINE_SURFACE(((1.,0.706797490733928,1.00061923411657),(1.,
0.706182062146832,1.00062053388163),(1.,0.705584062769228,1.00062179683677),
(1.,0.705266224770693,1.00062246810023)))
REPRESENTATION_ITEM('')
SURFACE()
);
#3054=(
BOUNDED_SURFACE()
B_SPLINE_SURFACE(3,2,((#207452,#207453,#207454),(#207455,#207456,#207457),
(#207458,#207459,#207460),(#207461,#207462,#207463),(#207464,#207465,#207466),
(#207467,#207468,#207469)),.UNSPECIFIED.,.F.,.F.,.F.)
B_SPLINE_SURFACE_WITH_KNOTS((4,2,4),(3,3),(-6.36968776335234E-19,0.000257652232350878,
0.000515304464701757),(0.,1.),.UNSPECIFIED.)
GEOMETRIC_REPRESENTATION_ITEM()
RATIONAL_B_SPLINE_SURFACE(((1.,0.874619707139396,1.),(1.,0.874861180430738,
1.),(1.,0.855455725920818,1.),(1.,0.794699358955304,1.),(1.,0.753768977788614,
1.),(1.,0.70871252716366,1.)))
REPRESENTATION_ITEM('')
SURFACE()
);
#3055=(
BOUNDED_SURFACE()
B_SPLINE_SURFACE(3,2,((#207475,#207476,#207477),(#207478,#207479,#207480),
(#207481,#207482,#207483),(#207484,#207485,#207486)),.UNSPECIFIED.,.F.,
 .F.,.F.)
B_SPLINE_SURFACE_WITH_KNOTS((4,4),(3,3),(0.,0.000397394373651917),(0.,1.),
 .UNSPECIFIED.)
GEOMETRIC_REPRESENTATION_ITEM()
RATIONAL_B_SPLINE_SURFACE(((1.,0.707106781186548,1.),(1.,0.70775258791587,
1.),(1.,0.708377654540715,1.),(1.,0.708689770883311,1.)))
REPRESENTATION_ITEM('')
SURFACE()
);
#3056=(
BOUNDED_SURFACE()
B_SPLINE_SURFACE(3,2,((#207488,#207489,#207490),(#207491,#207492,#207493),
(#207494,#207495,#207496),(#207497,#207498,#207499)),.UNSPECIFIED.,.F.,
 .F.,.F.)
B_SPLINE_SURFACE_WITH_KNOTS((4,4),(3,3),(-6.42389787197661E-18,0.000511815456479785),
(0.,1.00105873159879),.UNSPECIFIED.)
GEOMETRIC_REPRESENTATION_ITEM()
RATIONAL_B_SPLINE_SURFACE(((1.,0.708394529056662,1.00061746385294),(1.,
0.708058564167226,1.00061817524623),(1.,0.707430835372388,1.00061950443885),
(1.,0.706796685880717,1.00062084722706)))
REPRESENTATION_ITEM('')
SURFACE()
);
#3057=(
BOUNDED_SURFACE()
B_SPLINE_SURFACE(3,2,((#207505,#207506,#207507),(#207508,#207509,#207510),
(#207511,#207512,#207513),(#207514,#207515,#207516)),.UNSPECIFIED.,.F.,
 .F.,.F.)
B_SPLINE_SURFACE_WITH_KNOTS((4,4),(3,3),(0.,0.000397394465448298),(0.,1.),
 .UNSPECIFIED.)
GEOMETRIC_REPRESENTATION_ITEM()
RATIONAL_B_SPLINE_SURFACE(((1.,0.705498956110772,1.),(1.,0.705821764811771,
1.),(1.,0.706461952521147,1.),(1.,0.707106781186547,1.)))
REPRESENTATION_ITEM('')
SURFACE()
);
#3058=(
BOUNDED_SURFACE()
B_SPLINE_SURFACE(3,2,((#207522,#207523,#207524),(#207525,#207526,#207527),
(#207528,#207529,#207530),(#207531,#207532,#207533)),.UNSPECIFIED.,.F.,
 .F.,.F.)
B_SPLINE_SURFACE_WITH_KNOTS((4,4),(3,3),(0.,0.000397394410828734),(0.,1.),
 .UNSPECIFIED.)
GEOMETRIC_REPRESENTATION_ITEM()
RATIONAL_B_SPLINE_SURFACE(((1.,0.708689770883325,1.),(1.,0.708376440034491,
1.),(1.,0.707750498698406,1.),(1.,0.707106781186545,1.)))
REPRESENTATION_ITEM('')
SURFACE()
);
#3059=(
BOUNDED_SURFACE()
B_SPLINE_SURFACE(3,2,((#207539,#207540,#207541),(#207542,#207543,#207544),
(#207545,#207546,#207547),(#207548,#207549,#207550)),.UNSPECIFIED.,.F.,
 .F.,.F.)
B_SPLINE_SURFACE_WITH_KNOTS((4,4),(3,3),(0.,0.000511815090126171),(0.,1.00105592270213),
 .UNSPECIFIED.)
GEOMETRIC_REPRESENTATION_ITEM()
RATIONAL_B_SPLINE_SURFACE(((1.,0.705266242717511,1.0006224321308),(1.,0.705584085909147,
1.00062176089511),(1.,0.706182089450526,1.00062049800408),(1.,0.706797508587502,
1.00061919833401)))
REPRESENTATION_ITEM('')
SURFACE()
);
#3060=(
BOUNDED_SURFACE()
B_SPLINE_SURFACE(3,2,((#207552,#207553,#207554),(#207555,#207556,#207557),
(#207558,#207559,#207560),(#207561,#207562,#207563)),.UNSPECIFIED.,.F.,
 .F.,.F.)
B_SPLINE_SURFACE_WITH_KNOTS((4,4),(3,3),(-6.88468379528295E-18,0.000397394428086618),
(0.,1.),.UNSPECIFIED.)
GEOMETRIC_REPRESENTATION_ITEM()
RATIONAL_B_SPLINE_SURFACE(((1.,0.707106781186545,1.),(1.,0.706459846759105,
1.),(1.,0.705820510737275,1.),(1.,0.705498956110758,1.)))
REPRESENTATION_ITEM('')
SURFACE()
);
#3061=(
BOUNDED_SURFACE()
B_SPLINE_SURFACE(3,2,((#207569,#207570,#207571),(#207572,#207573,#207574),
(#207575,#207576,#207577),(#207578,#207579,#207580),(#207581,#207582,#207583),
(#207584,#207585,#207586)),.UNSPECIFIED.,.F.,.F.,.F.)
B_SPLINE_SURFACE_WITH_KNOTS((4,2,4),(3,3),(-8.53809210832335E-19,0.000257953807872851,
0.000515907615745703),(0.,1.),.UNSPECIFIED.)
GEOMETRIC_REPRESENTATION_ITEM()
RATIONAL_B_SPLINE_SURFACE(((1.,0.874619707139387,1.),(1.,0.874834349679476,
1.),(1.,0.854686104157146,1.),(1.,0.792476597915799,1.),(1.,0.750887854594649,
1.),(1.,0.70558583803143,1.)))
REPRESENTATION_ITEM('')
SURFACE()
);
#3062=(
BOUNDED_SURFACE()
B_SPLINE_SURFACE(3,2,((#207592,#207593,#207594),(#207595,#207596,#207597),
(#207598,#207599,#207600),(#207601,#207602,#207603)),.UNSPECIFIED.,.F.,
 .F.,.F.)
B_SPLINE_SURFACE_WITH_KNOTS((4,4),(3,3),(0.,0.000511815437699152),(0.,1.00105881331394),
 .UNSPECIFIED.)
GEOMETRIC_REPRESENTATION_ITEM()
RATIONAL_B_SPLINE_SURFACE(((1.,0.706796661946908,1.00062089519604),(1.,
0.70743082122576,1.00061955228347),(1.,0.708058545831313,1.00061822299713),
(1.,0.708394505253263,1.00061751156051)))
REPRESENTATION_ITEM('')
SURFACE()
);
#3063=(
BOUNDED_SURFACE()
B_SPLINE_SURFACE(3,2,((#207605,#207606,#207607),(#207608,#207609,#207610),
(#207611,#207612,#207613),(#207614,#207615,#207616),(#207617,#207618,#207619),
(#207620,#207621,#207622)),.UNSPECIFIED.,.F.,.F.,.F.)
B_SPLINE_SURFACE_WITH_KNOTS((4,2,4),(3,3),(0.,0.000256915317531263,0.000513830635062525),
(0.,1.),.UNSPECIFIED.)
GEOMETRIC_REPRESENTATION_ITEM()
RATIONAL_B_SPLINE_SURFACE(((1.,0.705585838031452,1.),(1.,0.750902433542811,
1.),(1.,0.792329530082409,1.),(1.,0.854288401594288,1.),(1.,0.874998031125078,
1.),(1.,0.874619707139386,1.)))
REPRESENTATION_ITEM('')
SURFACE()
);
#3064=(
BOUNDED_SURFACE()
B_SPLINE_SURFACE(3,2,((#207628,#207629,#207630),(#207631,#207632,#207633),
(#207634,#207635,#207636),(#207637,#207638,#207639),(#207640,#207641,#207642),
(#207643,#207644,#207645)),.UNSPECIFIED.,.F.,.F.,.F.)
B_SPLINE_SURFACE_WITH_KNOTS((4,2,4),(3,3),(-1.0842021724855E-19,0.000256592814262156,
0.000513185628524312),(0.,1.),.UNSPECIFIED.)
GEOMETRIC_REPRESENTATION_ITEM()
RATIONAL_B_SPLINE_SURFACE(((1.,0.708712527163657,1.),(1.,0.753780902613831,
1.),(1.,0.794538995768884,1.),(1.,0.855070770331427,1.),(1.,0.875018427445074,
1.),(1.,0.874619707139396,1.)))
REPRESENTATION_ITEM('')
SURFACE()
);
#3065=(
BOUNDED_SURFACE()
B_SPLINE_SURFACE(3,2,((#207647,#207648,#207649),(#207650,#207651,#207652),
(#207653,#207654,#207655),(#207656,#207657,#207658)),.UNSPECIFIED.,.F.,
 .F.,.F.)
B_SPLINE_SURFACE_WITH_KNOTS((4,4),(3,3),(2.71050543121376E-20,0.000511815072430395),
(0.,1.00105598365712),.UNSPECIFIED.)
GEOMETRIC_REPRESENTATION_ITEM()
RATIONAL_B_SPLINE_SURFACE(((1.,0.706797490734199,1.00061923411602),(1.,
0.70618206214713,1.00062053388108),(1.,0.705584062769454,1.00062179683622),
(1.,0.705266224770955,1.00062246809969)))
REPRESENTATION_ITEM('')
SURFACE()
);
#3066=(
BOUNDED_SURFACE()
B_SPLINE_SURFACE(3,2,((#207664,#207665,#207666),(#207667,#207668,#207669),
(#207670,#207671,#207672),(#207673,#207674,#207675),(#207676,#207677,#207678),
(#207679,#207680,#207681)),.UNSPECIFIED.,.F.,.F.,.F.)
B_SPLINE_SURFACE_WITH_KNOTS((4,2,4),(3,3),(1.35525271560688E-20,0.000257652232350878,
0.000515304464701757),(0.,1.),.UNSPECIFIED.)
GEOMETRIC_REPRESENTATION_ITEM()
RATIONAL_B_SPLINE_SURFACE(((1.,0.874619707139391,1.),(1.,0.874861180431061,
1.),(1.,0.855455725920385,1.),(1.,0.794699358955754,1.),(1.,0.753768977788293,
1.),(1.,0.708712527163653,1.)))
REPRESENTATION_ITEM('')
SURFACE()
);
#3067=(
BOUNDED_SURFACE()
B_SPLINE_SURFACE(3,2,((#207687,#207688,#207689),(#207690,#207691,#207692),
(#207693,#207694,#207695),(#207696,#207697,#207698)),.UNSPECIFIED.,.F.,
 .F.,.F.)
B_SPLINE_SURFACE_WITH_KNOTS((4,4),(3,3),(0.,0.000397394373651917),(0.,1.),
 .UNSPECIFIED.)
GEOMETRIC_REPRESENTATION_ITEM()
RATIONAL_B_SPLINE_SURFACE(((1.,0.707106781186548,1.),(1.,0.707752587915895,
1.),(1.,0.708377654540701,1.),(1.,0.708689770883337,1.)))
REPRESENTATION_ITEM('')
SURFACE()
);
#3068=(
BOUNDED_SURFACE()
B_SPLINE_SURFACE(3,2,((#207700,#207701,#207702),(#207703,#207704,#207705),
(#207706,#207707,#207708),(#207709,#207710,#207711)),.UNSPECIFIED.,.F.,
 .F.,.F.)
B_SPLINE_SURFACE_WITH_KNOTS((4,4),(3,3),(0.,0.000511815456479796),(0.,1.00105873160039),
 .UNSPECIFIED.)
GEOMETRIC_REPRESENTATION_ITEM()
RATIONAL_B_SPLINE_SURFACE(((1.,0.708394529056226,1.00061746385387),(1.,
0.708058564166737,1.00061817524716),(1.,0.707430835371936,1.00061950443978),
(1.,0.70679668588025,1.00062084722799)))
REPRESENTATION_ITEM('')
SURFACE()
);
#3069=(
BOUNDED_SURFACE()
B_SPLINE_SURFACE(3,2,((#207717,#207718,#207719),(#207720,#207721,#207722),
(#207723,#207724,#207725),(#207726,#207727,#207728)),.UNSPECIFIED.,.F.,
 .F.,.F.)
B_SPLINE_SURFACE_WITH_KNOTS((4,4),(3,3),(-6.50521303491303E-18,0.000397394465448298),
(0.,1.),.UNSPECIFIED.)
GEOMETRIC_REPRESENTATION_ITEM()
RATIONAL_B_SPLINE_SURFACE(((1.,0.705498956110744,1.),(1.,0.705821764811786,
1.),(1.,0.706461952521138,1.),(1.,0.707106781186546,1.)))
REPRESENTATION_ITEM('')
SURFACE()
);
#3070=(
BOUNDED_SURFACE()
B_SPLINE_SURFACE(3,2,((#207734,#207735,#207736),(#207737,#207738,#207739),
(#207740,#207741,#207742),(#207743,#207744,#207745)),.UNSPECIFIED.,.F.,
 .F.,.F.)
B_SPLINE_SURFACE_WITH_KNOTS((4,4),(3,3),(0.,0.000397394410828756),(0.,1.),
 .UNSPECIFIED.)
GEOMETRIC_REPRESENTATION_ITEM()
RATIONAL_B_SPLINE_SURFACE(((1.,0.708689770883349,1.),(1.,0.708376440034465,
1.),(1.,0.707750498698429,1.),(1.,0.707106781186547,1.)))
REPRESENTATION_ITEM('')
SURFACE()
);
#3071=(
BOUNDED_SURFACE()
B_SPLINE_SURFACE(3,2,((#207751,#207752,#207753),(#207754,#207755,#207756),
(#207757,#207758,#207759),(#207760,#207761,#207762)),.UNSPECIFIED.,.F.,
 .F.,.F.)
B_SPLINE_SURFACE_WITH_KNOTS((4,4),(3,3),(0.,0.000511815090126185),(0.,1.00105592270233),
 .UNSPECIFIED.)
GEOMETRIC_REPRESENTATION_ITEM()
RATIONAL_B_SPLINE_SURFACE(((1.,0.705266242717445,1.00062243213092),(1.,
0.7055840859091,1.00062176089523),(1.,0.706182089450454,1.0006204980042),
(1.,0.706797508587444,1.00061919833413)))
REPRESENTATION_ITEM('')
SURFACE()
);
#3072=(
BOUNDED_SURFACE()
B_SPLINE_SURFACE(3,2,((#207764,#207765,#207766),(#207767,#207768,#207769),
(#207770,#207771,#207772),(#207773,#207774,#207775)),.UNSPECIFIED.,.F.,
 .F.,.F.)
B_SPLINE_SURFACE_WITH_KNOTS((4,4),(3,3),(0.,0.000397394428086631),(0.,1.),
 .UNSPECIFIED.)
GEOMETRIC_REPRESENTATION_ITEM()
RATIONAL_B_SPLINE_SURFACE(((1.,0.707106781186552,1.),(1.,0.706459846759088,
1.),(1.,0.705820510737275,1.),(1.,0.705498956110745,1.)))
REPRESENTATION_ITEM('')
SURFACE()
);
#3073=(
BOUNDED_SURFACE()
B_SPLINE_SURFACE(3,2,((#207781,#207782,#207783),(#207784,#207785,#207786),
(#207787,#207788,#207789),(#207790,#207791,#207792),(#207793,#207794,#207795),
(#207796,#207797,#207798)),.UNSPECIFIED.,.F.,.F.,.F.)
B_SPLINE_SURFACE_WITH_KNOTS((4,2,4),(3,3),(0.,0.000257953807872849,0.000515907615745697),
(0.,1.),.UNSPECIFIED.)
GEOMETRIC_REPRESENTATION_ITEM()
RATIONAL_B_SPLINE_SURFACE(((1.,0.874619707139393,1.),(1.,0.874834349679465,
1.),(1.,0.854686104157144,1.),(1.,0.792476597915797,1.),(1.,0.750887854594642,
1.),(1.,0.705585838031435,1.)))
REPRESENTATION_ITEM('')
SURFACE()
);
#3074=(
BOUNDED_SURFACE()
B_SPLINE_SURFACE(3,2,((#207804,#207805,#207806),(#207807,#207808,#207809),
(#207810,#207811,#207812),(#207813,#207814,#207815)),.UNSPECIFIED.,.F.,
 .F.,.F.)
B_SPLINE_SURFACE_WITH_KNOTS((4,4),(3,3),(0.,0.000511815437699151),(0.,1.00105881331716),
 .UNSPECIFIED.)
GEOMETRIC_REPRESENTATION_ITEM()
RATIONAL_B_SPLINE_SURFACE(((1.,0.706796661945962,1.00062089519794),(1.,
0.707430821224836,1.00061955228536),(1.,0.708058545830357,1.00061822299901),
(1.,0.70839450525234,1.00061751156239)))
REPRESENTATION_ITEM('')
SURFACE()
);
#3075=(
BOUNDED_SURFACE()
B_SPLINE_SURFACE(3,2,((#207817,#207818,#207819),(#207820,#207821,#207822),
(#207823,#207824,#207825),(#207826,#207827,#207828),(#207829,#207830,#207831),
(#207832,#207833,#207834)),.UNSPECIFIED.,.F.,.F.,.F.)
B_SPLINE_SURFACE_WITH_KNOTS((4,2,4),(3,3),(0.,0.000256915317531258,0.000513830635062516),
(0.,1.),.UNSPECIFIED.)
GEOMETRIC_REPRESENTATION_ITEM()
RATIONAL_B_SPLINE_SURFACE(((1.,0.705585838031428,1.),(1.,0.750902433542113,
1.),(1.,0.792329530083375,1.),(1.,0.854288401593323,1.),(1.,0.874998031125785,
1.),(1.,0.874619707139391,1.)))
REPRESENTATION_ITEM('')
SURFACE()
);
#3076=(
BOUNDED_SURFACE()
B_SPLINE_SURFACE(3,2,((#207840,#207841,#207842),(#207843,#207844,#207845),
(#207846,#207847,#207848),(#207849,#207850,#207851),(#207852,#207853,#207854),
(#207855,#207856,#207857)),.UNSPECIFIED.,.F.,.F.,.F.)
B_SPLINE_SURFACE_WITH_KNOTS((4,2,4),(3,3),(0.,0.000256592814262157,0.000513185628524314),
(0.,1.),.UNSPECIFIED.)
GEOMETRIC_REPRESENTATION_ITEM()
RATIONAL_B_SPLINE_SURFACE(((1.,0.708712527163666,1.),(1.,0.753780902613584,
1.),(1.,0.794538995769204,1.),(1.,0.855070770331107,1.),(1.,0.875018427445323,
1.),(1.,0.874619707139393,1.)))
REPRESENTATION_ITEM('')
SURFACE()
);
#3077=(
BOUNDED_SURFACE()
B_SPLINE_SURFACE(3,2,((#207859,#207860,#207861),(#207862,#207863,#207864),
(#207865,#207866,#207867),(#207868,#207869,#207870)),.UNSPECIFIED.,.F.,
 .F.,.F.)
B_SPLINE_SURFACE_WITH_KNOTS((4,4),(3,3),(2.71050543121376E-20,0.000511815072430406),
(0.,1.00105598365692),.UNSPECIFIED.)
GEOMETRIC_REPRESENTATION_ITEM()
RATIONAL_B_SPLINE_SURFACE(((1.,0.706797490734257,1.00061923411591),(1.,
0.706182062147172,1.00062053388097),(1.,0.705584062769546,1.0006217968361),
(1.,0.705266224771024,1.00062246809957)))
REPRESENTATION_ITEM('')
SURFACE()
);
#3078=(
BOUNDED_SURFACE()
B_SPLINE_SURFACE(3,2,((#207876,#207877,#207878),(#207879,#207880,#207881),
(#207882,#207883,#207884),(#207885,#207886,#207887),(#207888,#207889,#207890),
(#207891,#207892,#207893)),.UNSPECIFIED.,.F.,.F.,.F.)
B_SPLINE_SURFACE_WITH_KNOTS((4,2,4),(3,3),(-1.72117094882074E-18,0.000257652232350877,
0.000515304464701755),(0.,1.),.UNSPECIFIED.)
GEOMETRIC_REPRESENTATION_ITEM()
RATIONAL_B_SPLINE_SURFACE(((1.,0.874619707139395,1.),(1.,0.874861180430836,
1.),(1.,0.855455725920695,1.),(1.,0.794699358955469,1.),(1.,0.753768977788511,
1.),(1.,0.708712527163661,1.)))
REPRESENTATION_ITEM('')
SURFACE()
);
#3079=(
BOUNDED_SURFACE()
B_SPLINE_SURFACE(3,2,((#207899,#207900,#207901),(#207902,#207903,#207904),
(#207905,#207906,#207907),(#207908,#207909,#207910)),.UNSPECIFIED.,.F.,
 .F.,.F.)
B_SPLINE_SURFACE_WITH_KNOTS((4,4),(3,3),(0.,0.000397394373651921),(0.,1.),
 .UNSPECIFIED.)
GEOMETRIC_REPRESENTATION_ITEM()
RATIONAL_B_SPLINE_SURFACE(((1.,0.707106781186548,1.),(1.,0.707752587915898,
1.),(1.,0.70837765454066,1.),(1.,0.708689770883349,1.)))
REPRESENTATION_ITEM('')
SURFACE()
);
#3080=(
BOUNDED_SURFACE()
B_SPLINE_SURFACE(3,2,((#207912,#207913,#207914),(#207915,#207916,#207917),
(#207918,#207919,#207920),(#207921,#207922,#207923)),.UNSPECIFIED.,.F.,
 .F.,.F.)
B_SPLINE_SURFACE_WITH_KNOTS((4,4),(3,3),(-6.39679281766448E-18,0.000511815456479792),
(0.,1.00105873159887),.UNSPECIFIED.)
GEOMETRIC_REPRESENTATION_ITEM()
RATIONAL_B_SPLINE_SURFACE(((1.,0.70839452905664,1.00061746385298),(1.,0.708058564167196,
1.00061817524627),(1.,0.707430835372364,1.00061950443889),(1.,0.706796685880695,
1.0006208472271)))
REPRESENTATION_ITEM('')
SURFACE()
);
#3081=(
BOUNDED_SURFACE()
B_SPLINE_SURFACE(3,2,((#207929,#207930,#207931),(#207932,#207933,#207934),
(#207935,#207936,#207937),(#207938,#207939,#207940)),.UNSPECIFIED.,.F.,
 .F.,.F.)
B_SPLINE_SURFACE_WITH_KNOTS((4,4),(3,3),(0.,0.000397394465448321),(0.,1.),
 .UNSPECIFIED.)
GEOMETRIC_REPRESENTATION_ITEM()
RATIONAL_B_SPLINE_SURFACE(((1.,0.70549895611076,1.),(1.,0.705821764811783,
1.),(1.,0.706461952521143,1.),(1.,0.707106781186552,1.)))
REPRESENTATION_ITEM('')
SURFACE()
);
#3082=(
BOUNDED_SURFACE()
B_SPLINE_SURFACE(3,2,((#207946,#207947,#207948),(#207949,#207950,#207951),
(#207952,#207953,#207954),(#207955,#207956,#207957)),.UNSPECIFIED.,.F.,
 .F.,.F.)
B_SPLINE_SURFACE_WITH_KNOTS((4,4),(3,3),(0.,0.00039739441082874),(0.,1.),
 .UNSPECIFIED.)
GEOMETRIC_REPRESENTATION_ITEM()
RATIONAL_B_SPLINE_SURFACE(((1.,0.708689770883327,1.),(1.,0.708376440034492,
1.),(1.,0.707750498698403,1.),(1.,0.707106781186548,1.)))
REPRESENTATION_ITEM('')
SURFACE()
);
#3083=(
BOUNDED_SURFACE()
B_SPLINE_SURFACE(3,2,((#207963,#207964,#207965),(#207966,#207967,#207968),
(#207969,#207970,#207971),(#207972,#207973,#207974)),.UNSPECIFIED.,.F.,
 .F.,.F.)
B_SPLINE_SURFACE_WITH_KNOTS((4,4),(3,3),(0.,0.000511815090126179),(0.,1.00105592270391),
 .UNSPECIFIED.)
GEOMETRIC_REPRESENTATION_ITEM()
RATIONAL_B_SPLINE_SURFACE(((1.,0.705266242716965,1.00062243213185),(1.,
0.705584085908659,1.00062176089616),(1.,0.706182089449987,1.00062049800513),
(1.,0.706797508586982,1.00061919833505)))
REPRESENTATION_ITEM('')
SURFACE()
);
#3084=(
BOUNDED_SURFACE()
B_SPLINE_SURFACE(3,2,((#207976,#207977,#207978),(#207979,#207980,#207981),
(#207982,#207983,#207984),(#207985,#207986,#207987)),.UNSPECIFIED.,.F.,
 .F.,.F.)
B_SPLINE_SURFACE_WITH_KNOTS((4,4),(3,3),(0.,0.000397394428086624),(0.,1.),
 .UNSPECIFIED.)
GEOMETRIC_REPRESENTATION_ITEM()
RATIONAL_B_SPLINE_SURFACE(((1.,0.707106781186536,1.),(1.,0.70645984675908,
1.),(1.,0.705820510737281,1.),(1.,0.705498956110757,1.)))
REPRESENTATION_ITEM('')
SURFACE()
);
#3085=(
BOUNDED_SURFACE()
B_SPLINE_SURFACE(3,2,((#207993,#207994,#207995),(#207996,#207997,#207998),
(#207999,#208000,#208001),(#208002,#208003,#208004),(#208005,#208006,#208007),
(#208008,#208009,#208010)),.UNSPECIFIED.,.F.,.F.,.F.)
B_SPLINE_SURFACE_WITH_KNOTS((4,2,4),(3,3),(0.,0.00025795380787285,0.0005159076157457),
(0.,1.),.UNSPECIFIED.)
GEOMETRIC_REPRESENTATION_ITEM()
RATIONAL_B_SPLINE_SURFACE(((1.,0.874619707139398,1.),(1.,0.87483434967915,
1.),(1.,0.854686104157582,1.),(1.,0.79247659791535,1.),(1.,0.750887854594954,
1.),(1.,0.705585838031445,1.)))
REPRESENTATION_ITEM('')
SURFACE()
);
#3086=(
BOUNDED_SURFACE()
B_SPLINE_SURFACE(3,2,((#208016,#208017,#208018),(#208019,#208020,#208021),
(#208022,#208023,#208024),(#208025,#208026,#208027)),.UNSPECIFIED.,.F.,
 .F.,.F.)
B_SPLINE_SURFACE_WITH_KNOTS((4,4),(3,3),(0.,0.000511815437699155),(0.,1.00105881331727),
 .UNSPECIFIED.)
GEOMETRIC_REPRESENTATION_ITEM()
RATIONAL_B_SPLINE_SURFACE(((1.,0.70679666194593,1.000620895198),(1.,0.707430821224804,
1.00061955228542),(1.,0.708058545830307,1.00061822299907),(1.,0.708394505252306,
1.00061751156245)))
REPRESENTATION_ITEM('')
SURFACE()
);
#3087=(
BOUNDED_SURFACE()
B_SPLINE_SURFACE(3,2,((#208029,#208030,#208031),(#208032,#208033,#208034),
(#208035,#208036,#208037),(#208038,#208039,#208040),(#208041,#208042,#208043),
(#208044,#208045,#208046)),.UNSPECIFIED.,.F.,.F.,.F.)
B_SPLINE_SURFACE_WITH_KNOTS((4,2,4),(3,3),(2.71050543121376E-20,0.000256915317531261,
0.000513830635062521),(0.,1.),.UNSPECIFIED.)
GEOMETRIC_REPRESENTATION_ITEM()
RATIONAL_B_SPLINE_SURFACE(((1.,0.705585838031435,1.),(1.,0.75090243354202,
1.),(1.,0.79232953008349,1.),(1.,0.854288401593237,1.),(1.,0.874998031125857,
1.),(1.,0.874619707139389,1.)))
REPRESENTATION_ITEM('')
SURFACE()
);
#3088=(
BOUNDED_SURFACE()
B_SPLINE_SURFACE(3,2,((#208052,#208053,#208054),(#208055,#208056,#208057),
(#208058,#208059,#208060),(#208061,#208062,#208063),(#208064,#208065,#208066),
(#208067,#208068,#208069)),.UNSPECIFIED.,.F.,.F.,.F.)
B_SPLINE_SURFACE_WITH_KNOTS((4,2,4),(3,3),(0.,0.000256592814262156,0.000513185628524312),
(0.,1.),.UNSPECIFIED.)
GEOMETRIC_REPRESENTATION_ITEM()
RATIONAL_B_SPLINE_SURFACE(((1.,0.708712527163647,1.),(1.,0.753780902613735,
1.),(1.,0.79453899576901,1.),(1.,0.855070770331286,1.),(1.,0.875018427445172,
1.),(1.,0.874619707139393,1.)))
REPRESENTATION_ITEM('')
SURFACE()
);
#3089=(
BOUNDED_SURFACE()
B_SPLINE_SURFACE(3,2,((#208071,#208072,#208073),(#208074,#208075,#208076),
(#208077,#208078,#208079),(#208080,#208081,#208082)),.UNSPECIFIED.,.F.,
 .F.,.F.)
B_SPLINE_SURFACE_WITH_KNOTS((4,4),(3,3),(2.71050543121376E-20,0.000511815072430397),
(0.,1.00105598365892),.UNSPECIFIED.)
GEOMETRIC_REPRESENTATION_ITEM()
RATIONAL_B_SPLINE_SURFACE(((1.,0.706797490733671,1.00061923411708),(1.,
0.706182062146594,1.00062053388214),(1.,0.70558406276894,1.00062179683728),
(1.,0.70526622477043,1.00062246810075)))
REPRESENTATION_ITEM('')
SURFACE()
);
#3090=(
BOUNDED_SURFACE()
B_SPLINE_SURFACE(3,2,((#208088,#208089,#208090),(#208091,#208092,#208093),
(#208094,#208095,#208096),(#208097,#208098,#208099),(#208100,#208101,#208102),
(#208103,#208104,#208105)),.UNSPECIFIED.,.F.,.F.,.F.)
B_SPLINE_SURFACE_WITH_KNOTS((4,2,4),(3,3),(-3.34747420754899E-18,0.000257652232350879,
0.000515304464701761),(0.,1.),.UNSPECIFIED.)
GEOMETRIC_REPRESENTATION_ITEM()
RATIONAL_B_SPLINE_SURFACE(((1.,0.874619707139389,1.),(1.,0.874861180430669,
1.),(1.,0.855455725920945,1.),(1.,0.794699358955162,1.),(1.,0.753768977788734,
1.),(1.,0.708712527163667,1.)))
REPRESENTATION_ITEM('')
SURFACE()
);
#3091=(
BOUNDED_SURFACE()
B_SPLINE_SURFACE(3,2,((#208111,#208112,#208113),(#208114,#208115,#208116),
(#208117,#208118,#208119),(#208120,#208121,#208122)),.UNSPECIFIED.,.F.,
 .F.,.F.)
B_SPLINE_SURFACE_WITH_KNOTS((4,4),(3,3),(0.,0.000397394373651905),(0.,1.),
 .UNSPECIFIED.)
GEOMETRIC_REPRESENTATION_ITEM()
RATIONAL_B_SPLINE_SURFACE(((1.,0.707106781186542,1.),(1.,0.707752587915914,
1.),(1.,0.708377654540659,1.),(1.,0.708689770883356,1.)))
REPRESENTATION_ITEM('')
SURFACE()
);
#3092=(
BOUNDED_SURFACE()
B_SPLINE_SURFACE(3,2,((#208124,#208125,#208126),(#208127,#208128,#208129),
(#208130,#208131,#208132),(#208133,#208134,#208135)),.UNSPECIFIED.,.F.,
 .F.,.F.)
B_SPLINE_SURFACE_WITH_KNOTS((4,4),(3,3),(-6.39679281766448E-18,0.000511815456479782),
(0.,1.00105873159862),.UNSPECIFIED.)
GEOMETRIC_REPRESENTATION_ITEM()
RATIONAL_B_SPLINE_SURFACE(((1.,0.708394529056725,1.00061746385284),(1.,
0.708058564167238,1.00061817524612),(1.,0.707430835372476,1.00061950443875),
(1.,0.706796685880768,1.00062084722696)))
REPRESENTATION_ITEM('')
SURFACE()
);
#3093=(
BOUNDED_SURFACE()
B_SPLINE_SURFACE(3,2,((#208141,#208142,#208143),(#208144,#208145,#208146),
(#208147,#208148,#208149),(#208150,#208151,#208152)),.UNSPECIFIED.,.F.,
 .F.,.F.)
B_SPLINE_SURFACE_WITH_KNOTS((4,4),(3,3),(0.,0.000397394465448303),(0.,1.),
 .UNSPECIFIED.)
GEOMETRIC_REPRESENTATION_ITEM()
RATIONAL_B_SPLINE_SURFACE(((1.,0.705498956110748,1.),(1.,0.705821764811772,
1.),(1.,0.706461952521139,1.),(1.,0.707106781186553,1.)))
REPRESENTATION_ITEM('')
SURFACE()
);
#3094=(
BOUNDED_SURFACE()
B_SPLINE_SURFACE(3,2,((#208158,#208159,#208160),(#208161,#208162,#208163),
(#208164,#208165,#208166),(#208167,#208168,#208169)),.UNSPECIFIED.,.F.,
 .F.,.F.)
B_SPLINE_SURFACE_WITH_KNOTS((4,4),(3,3),(0.,0.000397394410828747),(0.,1.),
 .UNSPECIFIED.)
GEOMETRIC_REPRESENTATION_ITEM()
RATIONAL_B_SPLINE_SURFACE(((1.,0.70868977088334,1.),(1.,0.708376440034488,
1.),(1.,0.707750498698412,1.),(1.,0.707106781186555,1.)))
REPRESENTATION_ITEM('')
SURFACE()
);
#3095=(
BOUNDED_SURFACE()
B_SPLINE_SURFACE(3,2,((#208175,#208176,#208177),(#208178,#208179,#208180),
(#208181,#208182,#208183),(#208184,#208185,#208186)),.UNSPECIFIED.,.F.,
 .F.,.F.)
B_SPLINE_SURFACE_WITH_KNOTS((4,4),(3,3),(0.,0.000511815090126184),(0.,1.00105592270487),
 .UNSPECIFIED.)
GEOMETRIC_REPRESENTATION_ITEM()
RATIONAL_B_SPLINE_SURFACE(((1.,0.705266242716691,1.00062243213241),(1.,
0.705584085908343,1.00062176089673),(1.,0.706182089449713,1.00062049800569),
(1.,0.7067975085867,1.00061919833561)))
REPRESENTATION_ITEM('')
SURFACE()
);
#3096=(
BOUNDED_SURFACE()
B_SPLINE_SURFACE(3,2,((#208188,#208189,#208190),(#208191,#208192,#208193),
(#208194,#208195,#208196),(#208197,#208198,#208199)),.UNSPECIFIED.,.F.,
 .F.,.F.)
B_SPLINE_SURFACE_WITH_KNOTS((4,4),(3,3),(0.,0.000397394428086623),(0.,1.),
 .UNSPECIFIED.)
GEOMETRIC_REPRESENTATION_ITEM()
RATIONAL_B_SPLINE_SURFACE(((1.,0.707106781186548,1.),(1.,0.706459846759087,
1.),(1.,0.705820510737271,1.),(1.,0.705498956110752,1.)))
REPRESENTATION_ITEM('')
SURFACE()
);
#3097=(
BOUNDED_SURFACE()
B_SPLINE_SURFACE(3,2,((#208205,#208206,#208207),(#208208,#208209,#208210),
(#208211,#208212,#208213),(#208214,#208215,#208216),(#208217,#208218,#208219),
(#208220,#208221,#208222)),.UNSPECIFIED.,.F.,.F.,.F.)
B_SPLINE_SURFACE_WITH_KNOTS((4,2,4),(3,3),(0.,0.000257953807872843,0.000515907615745687),
(0.,1.),.UNSPECIFIED.)
GEOMETRIC_REPRESENTATION_ITEM()
RATIONAL_B_SPLINE_SURFACE(((1.,0.874619707139384,1.),(1.,0.874834349678893,
1.),(1.,0.854686104157912,1.),(1.,0.792476597915048,1.),(1.,0.750887854595206,
1.),(1.,0.705585838031446,1.)))
REPRESENTATION_ITEM('')
SURFACE()
);
#3098=(
BOUNDED_SURFACE()
B_SPLINE_SURFACE(3,2,((#208228,#208229,#208230),(#208231,#208232,#208233),
(#208234,#208235,#208236),(#208237,#208238,#208239)),.UNSPECIFIED.,.F.,
 .F.,.F.)
B_SPLINE_SURFACE_WITH_KNOTS((4,4),(3,3),(0.,0.000511815437699158),(0.,1.00105881331566),
 .UNSPECIFIED.)
GEOMETRIC_REPRESENTATION_ITEM()
RATIONAL_B_SPLINE_SURFACE(((1.,0.706796661946385,1.00062089519705),(1.,
0.70743082122529,1.00061955228448),(1.,0.708058545830781,1.00061822299813),
(1.,0.708394505252787,1.00061751156151)))
REPRESENTATION_ITEM('')
SURFACE()
);
#3099=(
BOUNDED_SURFACE()
B_SPLINE_SURFACE(3,2,((#208241,#208242,#208243),(#208244,#208245,#208246),
(#208247,#208248,#208249),(#208250,#208251,#208252),(#208253,#208254,#208255),
(#208256,#208257,#208258)),.UNSPECIFIED.,.F.,.F.,.F.)
B_SPLINE_SURFACE_WITH_KNOTS((4,2,4),(3,3),(2.71050543121376E-20,0.00025691531753126,
0.00051383063506252),(0.,1.),.UNSPECIFIED.)
GEOMETRIC_REPRESENTATION_ITEM()
RATIONAL_B_SPLINE_SURFACE(((1.,0.705585838031438,1.),(1.,0.750902433542334,
1.),(1.,0.792329530083076,1.),(1.,0.854288401593664,1.),(1.,0.874998031125545,
1.),(1.,0.874619707139391,1.)))
REPRESENTATION_ITEM('')
SURFACE()
);
#3100=(
BOUNDED_SURFACE()
B_SPLINE_SURFACE(3,2,((#208264,#208265,#208266),(#208267,#208268,#208269),
(#208270,#208271,#208272),(#208273,#208274,#208275),(#208276,#208277,#208278),
(#208279,#208280,#208281)),.UNSPECIFIED.,.F.,.F.,.F.)
B_SPLINE_SURFACE_WITH_KNOTS((4,2,4),(3,3),(0.,0.000256592814262153,0.000513185628524306),
(0.,1.),.UNSPECIFIED.)
GEOMETRIC_REPRESENTATION_ITEM()
RATIONAL_B_SPLINE_SURFACE(((1.,0.708712527163662,1.),(1.,0.753780902613821,
1.),(1.,0.794538995768888,1.),(1.,0.85507077033143,1.),(1.,0.875018427445082,
1.),(1.,0.874619707139386,1.)))
REPRESENTATION_ITEM('')
SURFACE()
);
#3101=(
BOUNDED_SURFACE()
B_SPLINE_SURFACE(3,2,((#208283,#208284,#208285),(#208286,#208287,#208288),
(#208289,#208290,#208291),(#208292,#208293,#208294)),.UNSPECIFIED.,.F.,
 .F.,.F.)
B_SPLINE_SURFACE_WITH_KNOTS((4,4),(3,3),(0.,0.000511815072430401),(0.,1.0010559836604),
 .UNSPECIFIED.)
GEOMETRIC_REPRESENTATION_ITEM()
RATIONAL_B_SPLINE_SURFACE(((1.,0.706797490733232,1.00061923411795),(1.,
0.706182062146145,1.00062053388301),(1.,0.705584062768516,1.00062179683815),
(1.,0.705266224769999,1.00062246810162)))
REPRESENTATION_ITEM('')
SURFACE()
);
#3102=(
BOUNDED_SURFACE()
B_SPLINE_SURFACE(3,2,((#208300,#208301,#208302),(#208303,#208304,#208305),
(#208306,#208307,#208308),(#208309,#208310,#208311),(#208312,#208313,#208314),
(#208315,#208316,#208317)),.UNSPECIFIED.,.F.,.F.,.F.)
B_SPLINE_SURFACE_WITH_KNOTS((4,2,4),(3,3),(0.,0.000257652232350877,0.000515304464701754),
(0.,1.),.UNSPECIFIED.)
GEOMETRIC_REPRESENTATION_ITEM()
RATIONAL_B_SPLINE_SURFACE(((1.,0.874619707139387,1.),(1.,0.874861180430517,
1.),(1.,0.855455725921104,1.),(1.,0.794699358955021,1.),(1.,0.753768977788863,
1.),(1.,0.708712527163641,1.)))
REPRESENTATION_ITEM('')
SURFACE()
);
#3103=(
BOUNDED_SURFACE()
B_SPLINE_SURFACE(3,2,((#208323,#208324,#208325),(#208326,#208327,#208328),
(#208329,#208330,#208331),(#208332,#208333,#208334)),.UNSPECIFIED.,.F.,
 .F.,.F.)
B_SPLINE_SURFACE_WITH_KNOTS((4,4),(3,3),(0.,0.000397394373651908),(0.,1.),
 .UNSPECIFIED.)
GEOMETRIC_REPRESENTATION_ITEM()
RATIONAL_B_SPLINE_SURFACE(((1.,0.707106781186556,1.),(1.,0.707752587915904,
1.),(1.,0.708377654540669,1.),(1.,0.708689770883336,1.)))
REPRESENTATION_ITEM('')
SURFACE()
);
#3104=(
BOUNDED_SURFACE()
B_SPLINE_SURFACE(3,2,((#208336,#208337,#208338),(#208339,#208340,#208341),
(#208342,#208343,#208344),(#208345,#208346,#208347)),.UNSPECIFIED.,.F.,
 .F.,.F.)
B_SPLINE_SURFACE_WITH_KNOTS((4,4),(3,3),(0.,0.000511815456479792),(0.,1.00105873160375),
 .UNSPECIFIED.)
GEOMETRIC_REPRESENTATION_ITEM()
RATIONAL_B_SPLINE_SURFACE(((1.,0.708394529055219,1.00061746385583),(1.,
0.708058564165767,1.00061817524912),(1.,0.707430835370929,1.00061950444175),
(1.,0.706796685879273,1.00062084722997)))
REPRESENTATION_ITEM('')
SURFACE()
);
#3105=(
BOUNDED_SURFACE()
B_SPLINE_SURFACE(3,2,((#208353,#208354,#208355),(#208356,#208357,#208358),
(#208359,#208360,#208361),(#208362,#208363,#208364)),.UNSPECIFIED.,.F.,
 .F.,.F.)
B_SPLINE_SURFACE_WITH_KNOTS((4,4),(3,3),(0.,0.0003973944654483),(0.,1.),
 .UNSPECIFIED.)
GEOMETRIC_REPRESENTATION_ITEM()
RATIONAL_B_SPLINE_SURFACE(((1.,0.70549895611075,1.),(1.,0.705821764811787,
1.),(1.,0.70646195252115,1.),(1.,0.707106781186548,1.)))
REPRESENTATION_ITEM('')
SURFACE()
);
#3106=(
BOUNDED_SURFACE()
B_SPLINE_SURFACE(3,2,((#208370,#208371,#208372),(#208373,#208374,#208375),
(#208376,#208377,#208378),(#208379,#208380,#208381)),.UNSPECIFIED.,.F.,
 .F.,.F.)
B_SPLINE_SURFACE_WITH_KNOTS((4,4),(3,3),(0.,0.000397394410828731),(0.,1.),
 .UNSPECIFIED.)
GEOMETRIC_REPRESENTATION_ITEM()
RATIONAL_B_SPLINE_SURFACE(((1.,0.708689770883321,1.),(1.,0.708376440034497,
1.),(1.,0.707750498698426,1.),(1.,0.707106781186538,1.)))
REPRESENTATION_ITEM('')
SURFACE()
);
#3107=(
BOUNDED_SURFACE()
B_SPLINE_SURFACE(3,2,((#208387,#208388,#208389),(#208390,#208391,#208392),
(#208393,#208394,#208395),(#208396,#208397,#208398)),.UNSPECIFIED.,.F.,
 .F.,.F.)
B_SPLINE_SURFACE_WITH_KNOTS((4,4),(3,3),(0.,0.000511815090126176),(0.,1.0010559227031),
 .UNSPECIFIED.)
GEOMETRIC_REPRESENTATION_ITEM()
RATIONAL_B_SPLINE_SURFACE(((1.,0.705266242717241,1.00062243213137),(1.,
0.705584085908851,1.00062176089569),(1.,0.70618208945024,1.00062049800466),
(1.,0.706797508587208,1.00061919833458)))
REPRESENTATION_ITEM('')
SURFACE()
);
#3108=(
BOUNDED_SURFACE()
B_SPLINE_SURFACE(3,2,((#208400,#208401,#208402),(#208403,#208404,#208405),
(#208406,#208407,#208408),(#208409,#208410,#208411)),.UNSPECIFIED.,.F.,
 .F.,.F.)
B_SPLINE_SURFACE_WITH_KNOTS((4,4),(3,3),(-1.52872506320456E-17,0.000397394428086609),
(0.,1.),.UNSPECIFIED.)
GEOMETRIC_REPRESENTATION_ITEM()
RATIONAL_B_SPLINE_SURFACE(((1.,0.707106781186549,1.),(1.,0.706459846759096,
1.),(1.,0.705820510737299,1.),(1.,0.705498956110724,1.)))
REPRESENTATION_ITEM('')
SURFACE()
);
#3109=(
BOUNDED_SURFACE()
B_SPLINE_SURFACE(3,2,((#208417,#208418,#208419),(#208420,#208421,#208422),
(#208423,#208424,#208425),(#208426,#208427,#208428),(#208429,#208430,#208431),
(#208432,#208433,#208434)),.UNSPECIFIED.,.F.,.F.,.F.)
B_SPLINE_SURFACE_WITH_KNOTS((4,2,4),(3,3),(0.,0.000257953807872847,0.000515907615745694),
(0.,1.),.UNSPECIFIED.)
GEOMETRIC_REPRESENTATION_ITEM()
RATIONAL_B_SPLINE_SURFACE(((1.,0.874619707139391,1.),(1.,0.874834349679487,
1.),(1.,0.854686104157114,1.),(1.,0.792476597915844,1.),(1.,0.75088785459459,
1.),(1.,0.705585838031461,1.)))
REPRESENTATION_ITEM('')
SURFACE()
);
#3110=(
BOUNDED_SURFACE()
B_SPLINE_SURFACE(3,2,((#208440,#208441,#208442),(#208443,#208444,#208445),
(#208446,#208447,#208448),(#208449,#208450,#208451)),.UNSPECIFIED.,.F.,
 .F.,.F.)
B_SPLINE_SURFACE_WITH_KNOTS((4,4),(3,3),(0.,0.000511815437699146),(0.,1.00105881331828),
 .UNSPECIFIED.)
GEOMETRIC_REPRESENTATION_ITEM()
RATIONAL_B_SPLINE_SURFACE(((1.,0.706796661945634,1.00062089519859),(1.,
0.707430821224513,1.00061955228601),(1.,0.708058545830029,1.00061822299966),
(1.,0.708394505252009,1.00061751156304)))
REPRESENTATION_ITEM('')
SURFACE()
);
#3111=(
BOUNDED_SURFACE()
B_SPLINE_SURFACE(3,2,((#208453,#208454,#208455),(#208456,#208457,#208458),
(#208459,#208460,#208461),(#208462,#208463,#208464),(#208465,#208466,#208467),
(#208468,#208469,#208470)),.UNSPECIFIED.,.F.,.F.,.F.)
B_SPLINE_SURFACE_WITH_KNOTS((4,2,4),(3,3),(0.,0.000256915317531259,0.000513830635062518),
(0.,1.),.UNSPECIFIED.)
GEOMETRIC_REPRESENTATION_ITEM()
RATIONAL_B_SPLINE_SURFACE(((1.,0.705585838031464,1.),(1.,0.750902433542663,
1.),(1.,0.792329530082664,1.),(1.,0.854288401594055,1.),(1.,0.874998031125273,
1.),(1.,0.874619707139395,1.)))
REPRESENTATION_ITEM('')
SURFACE()
);
#3112=(
BOUNDED_SURFACE()
B_SPLINE_SURFACE(3,2,((#208476,#208477,#208478),(#208479,#208480,#208481),
(#208482,#208483,#208484),(#208485,#208486,#208487),(#208488,#208489,#208490),
(#208491,#208492,#208493)),.UNSPECIFIED.,.F.,.F.,.F.)
B_SPLINE_SURFACE_WITH_KNOTS((4,2,4),(3,3),(0.,0.000256592814262156,0.000513185628524312),
(0.,1.),.UNSPECIFIED.)
GEOMETRIC_REPRESENTATION_ITEM()
RATIONAL_B_SPLINE_SURFACE(((1.,0.708712527163668,1.),(1.,0.753780902613508,
1.),(1.,0.794538995769307,1.),(1.,0.855070770330991,1.),(1.,0.875018427445403,
1.),(1.,0.874619707139386,1.)))
REPRESENTATION_ITEM('')
SURFACE()
);
#3113=(
BOUNDED_SURFACE()
B_SPLINE_SURFACE(3,2,((#208495,#208496,#208497),(#208498,#208499,#208500),
(#208501,#208502,#208503),(#208504,#208505,#208506)),.UNSPECIFIED.,.F.,
 .F.,.F.)
B_SPLINE_SURFACE_WITH_KNOTS((4,4),(3,3),(0.,0.000511815072430389),(0.,1.00105598366069),
 .UNSPECIFIED.)
GEOMETRIC_REPRESENTATION_ITEM()
RATIONAL_B_SPLINE_SURFACE(((1.,0.706797490733162,1.00061923411812),(1.,
0.706182062146082,1.00062053388318),(1.,0.705584062768414,1.00062179683833),
(1.,0.705266224769911,1.00062246810179)))
REPRESENTATION_ITEM('')
SURFACE()
);
#3114=(
BOUNDED_SURFACE()
B_SPLINE_SURFACE(3,2,((#208512,#208513,#208514),(#208515,#208516,#208517),
(#208518,#208519,#208520),(#208521,#208522,#208523),(#208524,#208525,#208526),
(#208527,#208528,#208529)),.UNSPECIFIED.,.F.,.F.,.F.)
B_SPLINE_SURFACE_WITH_KNOTS((4,2,4),(3,3),(0.,0.000257652232350886,0.000515304464701772),
(0.,1.),.UNSPECIFIED.)
GEOMETRIC_REPRESENTATION_ITEM()
RATIONAL_B_SPLINE_SURFACE(((1.,0.874619707139379,1.),(1.,0.874861180430367,
1.),(1.,0.855455725921303,1.),(1.,0.794699358954818,1.),(1.,0.753768977788941,
1.),(1.,0.708712527163667,1.)))
REPRESENTATION_ITEM('')
SURFACE()
);
#3115=(
BOUNDED_SURFACE()
B_SPLINE_SURFACE(3,2,((#208535,#208536,#208537),(#208538,#208539,#208540),
(#208541,#208542,#208543),(#208544,#208545,#208546)),.UNSPECIFIED.,.F.,
 .F.,.F.)
B_SPLINE_SURFACE_WITH_KNOTS((4,4),(3,3),(-1.53143556863578E-17,0.000397394373651904),
(0.,1.),.UNSPECIFIED.)
GEOMETRIC_REPRESENTATION_ITEM()
RATIONAL_B_SPLINE_SURFACE(((1.,0.707106781186548,1.),(1.,0.707752587915843,
1.),(1.,0.70837765454073,1.),(1.,0.708689770883302,1.)))
REPRESENTATION_ITEM('')
SURFACE()
);
#3116=(
BOUNDED_SURFACE()
B_SPLINE_SURFACE(3,2,((#208548,#208549,#208550),(#208551,#208552,#208553),
(#208554,#208555,#208556),(#208557,#208558,#208559)),.UNSPECIFIED.,.F.,
 .F.,.F.)
B_SPLINE_SURFACE_WITH_KNOTS((4,4),(3,3),(0.,0.000511815456479788),(0.,1.0010587315999),
 .UNSPECIFIED.)
GEOMETRIC_REPRESENTATION_ITEM()
RATIONAL_B_SPLINE_SURFACE(((1.,0.708394529056346,1.00061746385358),(1.,
0.70805856416687,1.00061817524687),(1.,0.707430835372085,1.00061950443949),
(1.,0.706796685880394,1.00062084722771)))
REPRESENTATION_ITEM('')
SURFACE()
);
#3117=(
BOUNDED_SURFACE()
B_SPLINE_SURFACE(3,2,((#208565,#208566,#208567),(#208568,#208569,#208570),
(#208571,#208572,#208573),(#208574,#208575,#208576)),.UNSPECIFIED.,.F.,
 .F.,.F.)
B_SPLINE_SURFACE_WITH_KNOTS((4,4),(3,3),(0.,0.000397394465448305),(0.,1.),
 .UNSPECIFIED.)
GEOMETRIC_REPRESENTATION_ITEM()
RATIONAL_B_SPLINE_SURFACE(((1.,0.705498956110757,1.),(1.,0.705821764811778,
1.),(1.,0.70646195252114,1.),(1.,0.707106781186556,1.)))
REPRESENTATION_ITEM('')
SURFACE()
);
#3118=(
BOUNDED_SURFACE()
B_SPLINE_SURFACE(3,2,((#208582,#208583,#208584),(#208585,#208586,#208587),
(#208588,#208589,#208590),(#208591,#208592,#208593)),.UNSPECIFIED.,.F.,
 .F.,.F.)
B_SPLINE_SURFACE_WITH_KNOTS((4,4),(3,3),(0.,0.000397394410828738),(0.,1.),
 .UNSPECIFIED.)
GEOMETRIC_REPRESENTATION_ITEM()
RATIONAL_B_SPLINE_SURFACE(((1.,0.708689770883337,1.),(1.,0.708376440034459,
1.),(1.,0.707750498698444,1.),(1.,0.707106781186536,1.)))
REPRESENTATION_ITEM('')
SURFACE()
);
#3119=(
BOUNDED_SURFACE()
B_SPLINE_SURFACE(3,2,((#208599,#208600,#208601),(#208602,#208603,#208604),
(#208605,#208606,#208607),(#208608,#208609,#208610)),.UNSPECIFIED.,.F.,
 .F.,.F.)
B_SPLINE_SURFACE_WITH_KNOTS((4,4),(3,3),(0.,0.000511815090126175),(0.,1.00105592270252),
 .UNSPECIFIED.)
GEOMETRIC_REPRESENTATION_ITEM()
RATIONAL_B_SPLINE_SURFACE(((1.,0.705266242717401,1.00062243213103),(1.,
0.705584085909057,1.00062176089535),(1.,0.70618208945039,1.00062049800432),
(1.,0.706797508587387,1.00061919833424)))
REPRESENTATION_ITEM('')
SURFACE()
);
#3120=(
BOUNDED_SURFACE()
B_SPLINE_SURFACE(3,2,((#208612,#208613,#208614),(#208615,#208616,#208617),
(#208618,#208619,#208620),(#208621,#208622,#208623)),.UNSPECIFIED.,.F.,
 .F.,.F.)
B_SPLINE_SURFACE_WITH_KNOTS((4,4),(3,3),(0.,0.000397394428086644),(0.,1.),
 .UNSPECIFIED.)
GEOMETRIC_REPRESENTATION_ITEM()
RATIONAL_B_SPLINE_SURFACE(((1.,0.707106781186536,1.),(1.,0.706459846759106,
1.),(1.,0.705820510737281,1.),(1.,0.705498956110761,1.)))
REPRESENTATION_ITEM('')
SURFACE()
);
#3121=(
BOUNDED_SURFACE()
B_SPLINE_SURFACE(3,2,((#208629,#208630,#208631),(#208632,#208633,#208634),
(#208635,#208636,#208637),(#208638,#208639,#208640),(#208641,#208642,#208643),
(#208644,#208645,#208646)),.UNSPECIFIED.,.F.,.F.,.F.)
B_SPLINE_SURFACE_WITH_KNOTS((4,2,4),(3,3),(0.,0.000257953807872846,0.000515907615745692),
(0.,1.),.UNSPECIFIED.)
GEOMETRIC_REPRESENTATION_ITEM()
RATIONAL_B_SPLINE_SURFACE(((1.,0.87461970713939,1.),(1.,0.874834349679058,
1.),(1.,0.854686104157715,1.),(1.,0.792476597915225,1.),(1.,0.750887854595065,
1.),(1.,0.705585838031458,1.)))
REPRESENTATION_ITEM('')
SURFACE()
);
#3122=(
BOUNDED_SURFACE()
B_SPLINE_SURFACE(3,2,((#208652,#208653,#208654),(#208655,#208656,#208657),
(#208658,#208659,#208660),(#208661,#208662,#208663)),.UNSPECIFIED.,.F.,
 .F.,.F.)
B_SPLINE_SURFACE_WITH_KNOTS((4,4),(3,3),(0.,0.000511815437699154),(0.,1.00105881331964),
 .UNSPECIFIED.)
GEOMETRIC_REPRESENTATION_ITEM()
RATIONAL_B_SPLINE_SURFACE(((1.,0.706796661945235,1.00062089519939),(1.,
0.707430821224115,1.00061955228681),(1.,0.708058545829616,1.00061822300046),
(1.,0.708394505251623,1.00061751156384)))
REPRESENTATION_ITEM('')
SURFACE()
);
#3123=(
BOUNDED_SURFACE()
B_SPLINE_SURFACE(3,2,((#208665,#208666,#208667),(#208668,#208669,#208670),
(#208671,#208672,#208673),(#208674,#208675,#208676),(#208677,#208678,#208679),
(#208680,#208681,#208682)),.UNSPECIFIED.,.F.,.F.,.F.)
B_SPLINE_SURFACE_WITH_KNOTS((4,2,4),(3,3),(0.,0.000256915317531264,0.000513830635062528),
(0.,1.),.UNSPECIFIED.)
GEOMETRIC_REPRESENTATION_ITEM()
RATIONAL_B_SPLINE_SURFACE(((1.,0.705585838031448,1.),(1.,0.75090243354285,
1.),(1.,0.792329530082401,1.),(1.,0.854288401594319,1.),(1.,0.874998031125059,
1.),(1.,0.874619707139403,1.)))
REPRESENTATION_ITEM('')
SURFACE()
);
#3124=(
BOUNDED_SURFACE()
B_SPLINE_SURFACE(3,2,((#208688,#208689,#208690),(#208691,#208692,#208693),
(#208694,#208695,#208696),(#208697,#208698,#208699),(#208700,#208701,#208702),
(#208703,#208704,#208705)),.UNSPECIFIED.,.F.,.F.,.F.)
B_SPLINE_SURFACE_WITH_KNOTS((4,2,4),(3,3),(-9.45966395493603E-18,0.000256592814262146,
0.000513185628524302),(0.,1.),.UNSPECIFIED.)
GEOMETRIC_REPRESENTATION_ITEM()
RATIONAL_B_SPLINE_SURFACE(((1.,0.708712527163665,1.),(1.,0.753780902613326,
1.),(1.,0.794538995769537,1.),(1.,0.855070770330762,1.),(1.,0.875018427445575,
1.),(1.,0.874619707139397,1.)))
REPRESENTATION_ITEM('')
SURFACE()
);
#3125=(
BOUNDED_SURFACE()
B_SPLINE_SURFACE(3,2,((#208707,#208708,#208709),(#208710,#208711,#208712),
(#208713,#208714,#208715),(#208716,#208717,#208718)),.UNSPECIFIED.,.F.,
 .F.,.F.)
B_SPLINE_SURFACE_WITH_KNOTS((4,4),(3,3),(0.,0.000511815072430404),(0.,1.00105598365946),
 .UNSPECIFIED.)
GEOMETRIC_REPRESENTATION_ITEM()
RATIONAL_B_SPLINE_SURFACE(((1.,0.706797490733526,1.0006192341174),(1.,0.706182062146386,
1.00062053388246),(1.,0.705584062768819,1.0006217968376),(1.,0.705266224770269,
1.00062246810107)))
REPRESENTATION_ITEM('')
SURFACE()
);
#3126=(
BOUNDED_SURFACE()
B_SPLINE_SURFACE(3,2,((#208724,#208725,#208726),(#208727,#208728,#208729),
(#208730,#208731,#208732),(#208733,#208734,#208735),(#208736,#208737,#208738),
(#208739,#208740,#208741)),.UNSPECIFIED.,.F.,.F.,.F.)
B_SPLINE_SURFACE_WITH_KNOTS((4,2,4),(3,3),(0.,0.000257652232350881,0.000515304464701762),
(0.,1.),.UNSPECIFIED.)
GEOMETRIC_REPRESENTATION_ITEM()
RATIONAL_B_SPLINE_SURFACE(((1.,0.874619707139382,1.),(1.,0.874861180430684,
1.),(1.,0.855455725920868,1.),(1.,0.794699358955249,1.),(1.,0.753768977788646,
1.),(1.,0.708712527163657,1.)))
REPRESENTATION_ITEM('')
SURFACE()
);
#3127=(
BOUNDED_SURFACE()
B_SPLINE_SURFACE(3,2,((#208747,#208748,#208749),(#208750,#208751,#208752),
(#208753,#208754,#208755),(#208756,#208757,#208758)),.UNSPECIFIED.,.F.,
 .F.,.F.)
B_SPLINE_SURFACE_WITH_KNOTS((4,4),(3,3),(0.,0.000397394373651921),(0.,1.),
 .UNSPECIFIED.)
GEOMETRIC_REPRESENTATION_ITEM()
RATIONAL_B_SPLINE_SURFACE(((1.,0.707106781186548,1.),(1.,0.707752587915883,
1.),(1.,0.708377654540729,1.),(1.,0.708689770883306,1.)))
REPRESENTATION_ITEM('')
SURFACE()
);
#3128=(
BOUNDED_SURFACE()
B_SPLINE_SURFACE(3,2,((#208760,#208761,#208762),(#208763,#208764,#208765),
(#208766,#208767,#208768),(#208769,#208770,#208771)),.UNSPECIFIED.,.F.,
 .F.,.F.)
B_SPLINE_SURFACE_WITH_KNOTS((4,4),(3,3),(-6.42389787197661E-18,0.000511815456479787),
(0.,1.00105873159917),.UNSPECIFIED.)
GEOMETRIC_REPRESENTATION_ITEM()
RATIONAL_B_SPLINE_SURFACE(((1.,0.708394529056561,1.00061746385316),(1.,
0.708058564167106,1.00061817524645),(1.,0.707430835372293,1.00061950443907),
(1.,0.706796685880606,1.00062084722728)))
REPRESENTATION_ITEM('')
SURFACE()
);
#3129=(
BOUNDED_SURFACE()
B_SPLINE_SURFACE(3,2,((#208777,#208778,#208779),(#208780,#208781,#208782),
(#208783,#208784,#208785),(#208786,#208787,#208788)),.UNSPECIFIED.,.F.,
 .F.,.F.)
B_SPLINE_SURFACE_WITH_KNOTS((4,4),(3,3),(0.,0.000397394465448318),(0.,1.),
 .UNSPECIFIED.)
GEOMETRIC_REPRESENTATION_ITEM()
RATIONAL_B_SPLINE_SURFACE(((1.,0.705498956110736,1.),(1.,0.705821764811785,
1.),(1.,0.706461952521153,1.),(1.,0.707106781186548,1.)))
REPRESENTATION_ITEM('')
SURFACE()
);
#3130=(
BOUNDED_SURFACE()
B_SPLINE_SURFACE(3,2,((#208794,#208795,#208796),(#208797,#208798,#208799),
(#208800,#208801,#208802),(#208803,#208804,#208805)),.UNSPECIFIED.,.F.,
 .F.,.F.)
B_SPLINE_SURFACE_WITH_KNOTS((4,4),(3,3),(0.,0.000397394410828749),(0.,1.),
 .UNSPECIFIED.)
GEOMETRIC_REPRESENTATION_ITEM()
RATIONAL_B_SPLINE_SURFACE(((1.,0.708689770883341,1.),(1.,0.708376440034476,
1.),(1.,0.707750498698437,1.),(1.,0.707106781186548,1.)))
REPRESENTATION_ITEM('')
SURFACE()
);
#3131=(
BOUNDED_SURFACE()
B_SPLINE_SURFACE(3,2,((#208811,#208812,#208813),(#208814,#208815,#208816),
(#208817,#208818,#208819),(#208820,#208821,#208822)),.UNSPECIFIED.,.F.,
 .F.,.F.)
B_SPLINE_SURFACE_WITH_KNOTS((4,4),(3,3),(-6.42389787197661E-18,0.000511815090126168),
(0.,1.00105592270135),.UNSPECIFIED.)
GEOMETRIC_REPRESENTATION_ITEM()
RATIONAL_B_SPLINE_SURFACE(((1.,0.705266242717731,1.00062243213034),(1.,
0.705584085909352,1.00062176089466),(1.,0.706182089450749,1.00062049800363),
(1.,0.70679750858773,1.00061919833355)))
REPRESENTATION_ITEM('')
SURFACE()
);
#3132=(
BOUNDED_SURFACE()
B_SPLINE_SURFACE(3,2,((#208824,#208825,#208826),(#208827,#208828,#208829),
(#208830,#208831,#208832),(#208833,#208834,#208835)),.UNSPECIFIED.,.F.,
 .F.,.F.)
B_SPLINE_SURFACE_WITH_KNOTS((4,4),(3,3),(-9.64939933512099E-18,0.00039739442808662),
(0.,1.),.UNSPECIFIED.)
GEOMETRIC_REPRESENTATION_ITEM()
RATIONAL_B_SPLINE_SURFACE(((1.,0.707106781186548,1.),(1.,0.70645984675908,
1.),(1.,0.705820510737268,1.),(1.,0.705498956110742,1.)))
REPRESENTATION_ITEM('')
SURFACE()
);
#3133=(
BOUNDED_SURFACE()
B_SPLINE_SURFACE(3,2,((#208841,#208842,#208843),(#208844,#208845,#208846),
(#208847,#208848,#208849),(#208850,#208851,#208852),(#208853,#208854,#208855),
(#208856,#208857,#208858)),.UNSPECIFIED.,.F.,.F.,.F.)
B_SPLINE_SURFACE_WITH_KNOTS((4,2,4),(3,3),(0.,0.00025795380787284,0.00051590761574568),
(0.,1.),.UNSPECIFIED.)
GEOMETRIC_REPRESENTATION_ITEM()
RATIONAL_B_SPLINE_SURFACE(((1.,0.874619707139388,1.),(1.,0.874834349678587,
1.),(1.,0.854686104158307,1.),(1.,0.792476597914645,1.),(1.,0.750887854595489,
1.),(1.,0.705585838031426,1.)))
REPRESENTATION_ITEM('')
SURFACE()
);
#3134=(
BOUNDED_SURFACE()
B_SPLINE_SURFACE(3,2,((#208864,#208865,#208866),(#208867,#208868,#208869),
(#208870,#208871,#208872),(#208873,#208874,#208875)),.UNSPECIFIED.,.F.,
 .F.,.F.)
B_SPLINE_SURFACE_WITH_KNOTS((4,4),(3,3),(0.,0.000511815437699152),(0.,1.00105881331964),
 .UNSPECIFIED.)
GEOMETRIC_REPRESENTATION_ITEM()
RATIONAL_B_SPLINE_SURFACE(((1.,0.706796661945223,1.00062089519939),(1.,
0.707430821224125,1.00061955228681),(1.,0.708058545829633,1.00061822300046),
(1.,0.708394505251633,1.00061751156384)))
REPRESENTATION_ITEM('')
SURFACE()
);
#3135=(
BOUNDED_SURFACE()
B_SPLINE_SURFACE(3,2,((#208877,#208878,#208879),(#208880,#208881,#208882),
(#208883,#208884,#208885),(#208886,#208887,#208888),(#208889,#208890,#208891),
(#208892,#208893,#208894)),.UNSPECIFIED.,.F.,.F.,.F.)
B_SPLINE_SURFACE_WITH_KNOTS((4,2,4),(3,3),(0.,0.000256915317531262,0.000513830635062523),
(0.,1.),.UNSPECIFIED.)
GEOMETRIC_REPRESENTATION_ITEM()
RATIONAL_B_SPLINE_SURFACE(((1.,0.705585838031437,1.),(1.,0.750902433543188,
1.),(1.,0.792329530081924,1.),(1.,0.854288401594778,1.),(1.,0.874998031124709,
1.),(1.,0.87461970713939,1.)))
REPRESENTATION_ITEM('')
SURFACE()
);
#3136=(
BOUNDED_SURFACE()
B_SPLINE_SURFACE(3,2,((#208900,#208901,#208902),(#208903,#208904,#208905),
(#208906,#208907,#208908),(#208909,#208910,#208911),(#208912,#208913,#208914),
(#208915,#208916,#208917)),.UNSPECIFIED.,.F.,.F.,.F.)
B_SPLINE_SURFACE_WITH_KNOTS((4,2,4),(3,3),(-9.32413868337534E-18,0.00025659281426215,
0.000513185628524309),(0.,1.),.UNSPECIFIED.)
GEOMETRIC_REPRESENTATION_ITEM()
RATIONAL_B_SPLINE_SURFACE(((1.,0.708712527163675,1.),(1.,0.753780902613439,
1.),(1.,0.794538995769399,1.),(1.,0.855070770330883,1.),(1.,0.875018427445492,
1.),(1.,0.874619707139387,1.)))
REPRESENTATION_ITEM('')
SURFACE()
);
#3137=(
BOUNDED_SURFACE()
B_SPLINE_SURFACE(3,2,((#208919,#208920,#208921),(#208922,#208923,#208924),
(#208925,#208926,#208927),(#208928,#208929,#208930)),.UNSPECIFIED.,.F.,
 .F.,.F.)
B_SPLINE_SURFACE_WITH_KNOTS((4,4),(3,3),(-5.09575021068187E-18,0.000511815072430393),
(0.,1.0010559836582),.UNSPECIFIED.)
GEOMETRIC_REPRESENTATION_ITEM()
RATIONAL_B_SPLINE_SURFACE(((1.,0.706797490733882,1.00061923411666),(1.,
0.7061820621468,1.00062053388172),(1.,0.705584062769178,1.00062179683686),
(1.,0.705266224770652,1.00062246810032)))
REPRESENTATION_ITEM('')
SURFACE()
);
#3138=(
BOUNDED_SURFACE()
B_SPLINE_SURFACE(3,2,((#208936,#208937,#208938),(#208939,#208940,#208941),
(#208942,#208943,#208944),(#208945,#208946,#208947),(#208948,#208949,#208950),
(#208951,#208952,#208953)),.UNSPECIFIED.,.F.,.F.,.F.)
B_SPLINE_SURFACE_WITH_KNOTS((4,2,4),(3,3),(0.,0.000257652232350884,0.000515304464701767),
(0.,1.),.UNSPECIFIED.)
GEOMETRIC_REPRESENTATION_ITEM()
RATIONAL_B_SPLINE_SURFACE(((1.,0.874619707139388,1.),(1.,0.87486118043046,
1.),(1.,0.855455725921212,1.),(1.,0.7946993589549,1.),(1.,0.753768977788974,
1.),(1.,0.708712527163625,1.)))
REPRESENTATION_ITEM('')
SURFACE()
);
#3139=(
BOUNDED_SURFACE()
B_SPLINE_SURFACE(3,2,((#208959,#208960,#208961),(#208962,#208963,#208964),
(#208965,#208966,#208967),(#208968,#208969,#208970)),.UNSPECIFIED.,.F.,
 .F.,.F.)
B_SPLINE_SURFACE_WITH_KNOTS((4,4),(3,3),(-1.47451495458029E-17,0.000397394373651904),
(0.,1.),.UNSPECIFIED.)
GEOMETRIC_REPRESENTATION_ITEM()
RATIONAL_B_SPLINE_SURFACE(((1.,0.70710678118656,1.),(1.,0.707752587915888,
1.),(1.,0.708377654540624,1.),(1.,0.708689770883349,1.)))
REPRESENTATION_ITEM('')
SURFACE()
);
#3140=(
BOUNDED_SURFACE()
B_SPLINE_SURFACE(3,2,((#208972,#208973,#208974),(#208975,#208976,#208977),
(#208978,#208979,#208980),(#208981,#208982,#208983)),.UNSPECIFIED.,.F.,
 .F.,.F.)
B_SPLINE_SURFACE_WITH_KNOTS((4,4),(3,3),(0.,0.000511815456479796),(0.,1.00105873159821),
 .UNSPECIFIED.)
GEOMETRIC_REPRESENTATION_ITEM()
RATIONAL_B_SPLINE_SURFACE(((1.,0.708394529056829,1.0006174638526),(1.,0.708058564167371,
1.00061817524589),(1.,0.707430835372575,1.00061950443851),(1.,0.706796685880887,
1.00062084722672)))
REPRESENTATION_ITEM('')
SURFACE()
);
#3141=(
BOUNDED_SURFACE()
B_SPLINE_SURFACE(3,2,((#208989,#208990,#208991),(#208992,#208993,#208994),
(#208995,#208996,#208997),(#208998,#208999,#209000)),.UNSPECIFIED.,.F.,
 .F.,.F.)
B_SPLINE_SURFACE_WITH_KNOTS((4,4),(3,3),(-6.50521303491303E-18,0.000397394465448302),
(0.,1.),.UNSPECIFIED.)
GEOMETRIC_REPRESENTATION_ITEM()
RATIONAL_B_SPLINE_SURFACE(((1.,0.705498956110765,1.),(1.,0.70582176481176,
1.),(1.,0.706461952521179,1.),(1.,0.707106781186535,1.)))
REPRESENTATION_ITEM('')
SURFACE()
);
#3142=(
BOUNDED_SURFACE()
B_SPLINE_SURFACE(3,2,((#209006,#209007,#209008),(#209009,#209010,#209011),
(#209012,#209013,#209014),(#209015,#209016,#209017)),.UNSPECIFIED.,.F.,
 .F.,.F.)
B_SPLINE_SURFACE_WITH_KNOTS((4,4),(3,3),(0.,0.000397394410828735),(0.,1.),
 .UNSPECIFIED.)
GEOMETRIC_REPRESENTATION_ITEM()
RATIONAL_B_SPLINE_SURFACE(((1.,0.708689770883313,1.),(1.,0.708376440034517,
1.),(1.,0.707750498698387,1.),(1.,0.707106781186548,1.)))
REPRESENTATION_ITEM('')
SURFACE()
);
#3143=(
BOUNDED_SURFACE()
B_SPLINE_SURFACE(3,2,((#209023,#209024,#209025),(#209026,#209027,#209028),
(#209029,#209030,#209031),(#209032,#209033,#209034)),.UNSPECIFIED.,.F.,
 .F.,.F.)
B_SPLINE_SURFACE_WITH_KNOTS((4,4),(3,3),(0.,0.000511815090126171),(0.,1.00105592270182),
 .UNSPECIFIED.)
GEOMETRIC_REPRESENTATION_ITEM()
RATIONAL_B_SPLINE_SURFACE(((1.,0.705266242717594,1.00062243213061),(1.,
0.705584085909257,1.00062176089493),(1.,0.706182089450605,1.0006204980039),
(1.,0.706797508587594,1.00061919833382)))
REPRESENTATION_ITEM('')
SURFACE()
);
#3144=(
BOUNDED_SURFACE()
B_SPLINE_SURFACE(3,2,((#209036,#209037,#209038),(#209039,#209040,#209041),
(#209042,#209043,#209044),(#209045,#209046,#209047)),.UNSPECIFIED.,.F.,
 .F.,.F.)
B_SPLINE_SURFACE_WITH_KNOTS((4,4),(3,3),(-9.64939933512099E-18,0.000397394428086625),
(0.,1.),.UNSPECIFIED.)
GEOMETRIC_REPRESENTATION_ITEM()
RATIONAL_B_SPLINE_SURFACE(((1.,0.707106781186548,1.),(1.,0.706459846759098,
1.),(1.,0.705820510737279,1.),(1.,0.705498956110752,1.)))
REPRESENTATION_ITEM('')
SURFACE()
);
#3145=(
BOUNDED_SURFACE()
B_SPLINE_SURFACE(3,2,((#209053,#209054,#209055),(#209056,#209057,#209058),
(#209059,#209060,#209061),(#209062,#209063,#209064),(#209065,#209066,#209067),
(#209068,#209069,#209070)),.UNSPECIFIED.,.F.,.F.,.F.)
B_SPLINE_SURFACE_WITH_KNOTS((4,2,4),(3,3),(0.,0.000257953807872847,0.000515907615745693),
(0.,1.),.UNSPECIFIED.)
GEOMETRIC_REPRESENTATION_ITEM()
RATIONAL_B_SPLINE_SURFACE(((1.,0.874619707139394,1.),(1.,0.87483434967884,
1.),(1.,0.85468610415798,1.),(1.,0.792476597914961,1.),(1.,0.75088785459526,
1.),(1.,0.705585838031473,1.)))
REPRESENTATION_ITEM('')
SURFACE()
);
#3146=(
BOUNDED_SURFACE()
B_SPLINE_SURFACE(3,2,((#209076,#209077,#209078),(#209079,#209080,#209081),
(#209082,#209083,#209084),(#209085,#209086,#209087)),.UNSPECIFIED.,.F.,
 .F.,.F.)
B_SPLINE_SURFACE_WITH_KNOTS((4,4),(3,3),(0.,0.000511815437699157),(0.,1.00105881331725),
 .UNSPECIFIED.)
GEOMETRIC_REPRESENTATION_ITEM()
RATIONAL_B_SPLINE_SURFACE(((1.,0.706796661945923,1.00062089519799),(1.,
0.707430821224819,1.00061955228541),(1.,0.708058545830314,1.00061822299906),
(1.,0.708394505252314,1.00061751156244)))
REPRESENTATION_ITEM('')
SURFACE()
);
#3147=(
BOUNDED_SURFACE()
B_SPLINE_SURFACE(3,2,((#209089,#209090,#209091),(#209092,#209093,#209094),
(#209095,#209096,#209097),(#209098,#209099,#209100),(#209101,#209102,#209103),
(#209104,#209105,#209106)),.UNSPECIFIED.,.F.,.F.,.F.)
B_SPLINE_SURFACE_WITH_KNOTS((4,2,4),(3,3),(2.71050543121376E-20,0.000256915317531264,
0.000513830635062527),(0.,1.),.UNSPECIFIED.)
GEOMETRIC_REPRESENTATION_ITEM()
RATIONAL_B_SPLINE_SURFACE(((1.,0.705585838031416,1.),(1.,0.750902433542516,
1.),(1.,0.792329530082844,1.),(1.,0.854288401593844,1.),(1.,0.874998031125403,
1.),(1.,0.874619707139391,1.)))
REPRESENTATION_ITEM('')
SURFACE()
);
#3148=(
BOUNDED_SURFACE()
B_SPLINE_SURFACE(3,2,((#209112,#209113,#209114),(#209115,#209116,#209117),
(#209118,#209119,#209120),(#209121,#209122,#209123),(#209124,#209125,#209126),
(#209127,#209128,#209129)),.UNSPECIFIED.,.F.,.F.,.F.)
B_SPLINE_SURFACE_WITH_KNOTS((4,2,4),(3,3),(0.,0.000256592814262161,0.000513185628524323),
(0.,1.),.UNSPECIFIED.)
GEOMETRIC_REPRESENTATION_ITEM()
RATIONAL_B_SPLINE_SURFACE(((1.,0.70871252716366,1.),(1.,0.753780902613878,
1.),(1.,0.794538995768779,1.),(1.,0.855070770331533,1.),(1.,0.875018427445003,
1.),(1.,0.874619707139393,1.)))
REPRESENTATION_ITEM('')
SURFACE()
);
#3149=(
BOUNDED_SURFACE()
B_SPLINE_SURFACE(3,2,((#209131,#209132,#209133),(#209134,#209135,#209136),
(#209137,#209138,#209139),(#209140,#209141,#209142)),.UNSPECIFIED.,.F.,
 .F.,.F.)
B_SPLINE_SURFACE_WITH_KNOTS((4,4),(3,3),(-5.06864515636973E-18,0.000511815072430401),
(0.,1.00105598365977),.UNSPECIFIED.)
GEOMETRIC_REPRESENTATION_ITEM()
RATIONAL_B_SPLINE_SURFACE(((1.,0.706797490733424,1.00061923411758),(1.,
0.706182062146334,1.00062053388264),(1.,0.705584062768699,1.00062179683778),
(1.,0.705266224770158,1.00062246810125)))
REPRESENTATION_ITEM('')
SURFACE()
);
#3150=(
BOUNDED_SURFACE()
B_SPLINE_SURFACE(3,2,((#209148,#209149,#209150),(#209151,#209152,#209153),
(#209154,#209155,#209156),(#209157,#209158,#209159),(#209160,#209161,#209162),
(#209163,#209164,#209165)),.UNSPECIFIED.,.F.,.F.,.F.)
B_SPLINE_SURFACE_WITH_KNOTS((4,2,4),(3,3),(1.35525271560688E-20,0.000257652232350885,
0.00051530446470177),(0.,1.),.UNSPECIFIED.)
GEOMETRIC_REPRESENTATION_ITEM()
RATIONAL_B_SPLINE_SURFACE(((1.,0.874619707139391,1.),(1.,0.874861180430548,
1.),(1.,0.855455725921059,1.),(1.,0.79469935895508,1.),(1.,0.753768977788768,
1.),(1.,0.708712527163675,1.)))
REPRESENTATION_ITEM('')
SURFACE()
);
#3151=(
BOUNDED_SURFACE()
B_SPLINE_SURFACE(3,2,((#209171,#209172,#209173),(#209174,#209175,#209176),
(#209177,#209178,#209179),(#209180,#209181,#209182)),.UNSPECIFIED.,.F.,
 .F.,.F.)
B_SPLINE_SURFACE_WITH_KNOTS((4,4),(3,3),(0.,0.000397394373651914),(0.,1.),
 .UNSPECIFIED.)
GEOMETRIC_REPRESENTATION_ITEM()
RATIONAL_B_SPLINE_SURFACE(((1.,0.707106781186535,1.),(1.,0.707752587915914,
1.),(1.,0.708377654540683,1.),(1.,0.708689770883326,1.)))
REPRESENTATION_ITEM('')
SURFACE()
);
#3152=(
BOUNDED_SURFACE()
B_SPLINE_SURFACE(3,2,((#209184,#209185,#209186),(#209187,#209188,#209189),
(#209190,#209191,#209192),(#209193,#209194,#209195)),.UNSPECIFIED.,.F.,
 .F.,.F.)
B_SPLINE_SURFACE_WITH_KNOTS((4,4),(3,3),(0.,0.000511815456479784),(0.,1.00105873159912),
 .UNSPECIFIED.)
GEOMETRIC_REPRESENTATION_ITEM()
RATIONAL_B_SPLINE_SURFACE(((1.,0.708394529056566,1.00061746385313),(1.,
0.708058564167135,1.00061817524642),(1.,0.707430835372306,1.00061950443904),
(1.,0.706796685880622,1.00062084722725)))
REPRESENTATION_ITEM('')
SURFACE()
);
#3153=(
BOUNDED_SURFACE()
B_SPLINE_SURFACE(3,2,((#209201,#209202,#209203),(#209204,#209205,#209206),
(#209207,#209208,#209209),(#209210,#209211,#209212)),.UNSPECIFIED.,.F.,
 .F.,.F.)
B_SPLINE_SURFACE_WITH_KNOTS((4,4),(3,3),(0.,0.000397394465448309),(0.,1.),
 .UNSPECIFIED.)
GEOMETRIC_REPRESENTATION_ITEM()
RATIONAL_B_SPLINE_SURFACE(((1.,0.705498956110767,1.),(1.,0.705821764811776,
1.),(1.,0.706461952521138,1.),(1.,0.707106781186548,1.)))
REPRESENTATION_ITEM('')
SURFACE()
);
#3154=(
BOUNDED_SURFACE()
B_SPLINE_SURFACE(3,2,((#209218,#209219,#209220),(#209221,#209222,#209223),
(#209224,#209225,#209226),(#209227,#209228,#209229)),.UNSPECIFIED.,.F.,
 .F.,.F.)
B_SPLINE_SURFACE_WITH_KNOTS((4,4),(3,3),(0.,0.000397394410828743),(0.,1.),
 .UNSPECIFIED.)
GEOMETRIC_REPRESENTATION_ITEM()
RATIONAL_B_SPLINE_SURFACE(((1.,0.708689770883332,1.),(1.,0.708376440034505,
1.),(1.,0.707750498698407,1.),(1.,0.707106781186548,1.)))
REPRESENTATION_ITEM('')
SURFACE()
);
#3155=(
BOUNDED_SURFACE()
B_SPLINE_SURFACE(3,2,((#209235,#209236,#209237),(#209238,#209239,#209240),
(#209241,#209242,#209243),(#209244,#209245,#209246)),.UNSPECIFIED.,.F.,
 .F.,.F.)
B_SPLINE_SURFACE_WITH_KNOTS((4,4),(3,3),(0.,0.000511815090126178),(0.,1.00105592270222),
 .UNSPECIFIED.)
GEOMETRIC_REPRESENTATION_ITEM()
RATIONAL_B_SPLINE_SURFACE(((1.,0.705266242717482,1.00062243213085),(1.,
0.705584085909123,1.00062176089517),(1.,0.706182089450473,1.00062049800414),
(1.,0.706797508587475,1.00061919833406)))
REPRESENTATION_ITEM('')
SURFACE()
);
#3156=(
BOUNDED_SURFACE()
B_SPLINE_SURFACE(3,2,((#209248,#209249,#209250),(#209251,#209252,#209253),
(#209254,#209255,#209256),(#209257,#209258,#209259)),.UNSPECIFIED.,.F.,
 .F.,.F.)
B_SPLINE_SURFACE_WITH_KNOTS((4,4),(3,3),(0.,0.000397394428086621),(0.,1.),
 .UNSPECIFIED.)
GEOMETRIC_REPRESENTATION_ITEM()
RATIONAL_B_SPLINE_SURFACE(((1.,0.707106781186548,1.),(1.,0.706459846759103,
1.),(1.,0.705820510737277,1.),(1.,0.705498956110743,1.)))
REPRESENTATION_ITEM('')
SURFACE()
);
#3157=(
BOUNDED_SURFACE()
B_SPLINE_SURFACE(3,2,((#209265,#209266,#209267),(#209268,#209269,#209270),
(#209271,#209272,#209273),(#209274,#209275,#209276),(#209277,#209278,#209279),
(#209280,#209281,#209282)),.UNSPECIFIED.,.F.,.F.,.F.)
B_SPLINE_SURFACE_WITH_KNOTS((4,2,4),(3,3),(-9.6900569165892E-18,0.00025795380787284,
0.00051590761574569),(0.,1.),.UNSPECIFIED.)
GEOMETRIC_REPRESENTATION_ITEM()
RATIONAL_B_SPLINE_SURFACE(((1.,0.874619707139392,1.),(1.,0.8748343496787,
1.),(1.,0.854686104158173,1.),(1.,0.792476597914769,1.),(1.,0.750887854595394,
1.),(1.,0.705585838031444,1.)))
REPRESENTATION_ITEM('')
SURFACE()
);
#3158=(
BOUNDED_SURFACE()
B_SPLINE_SURFACE(3,2,((#209288,#209289,#209290),(#209291,#209292,#209293),
(#209294,#209295,#209296),(#209297,#209298,#209299)),.UNSPECIFIED.,.F.,
 .F.,.F.)
B_SPLINE_SURFACE_WITH_KNOTS((4,4),(3,3),(0.,0.000511815437699158),(0.,1.00105881331441),
 .UNSPECIFIED.)
GEOMETRIC_REPRESENTATION_ITEM()
RATIONAL_B_SPLINE_SURFACE(((1.,0.706796661946769,1.00062089519632),(1.,
0.707430821225625,1.00061955228374),(1.,0.708058545831196,1.0006182229974),
(1.,0.708394505253119,1.00061751156078)))
REPRESENTATION_ITEM('')
SURFACE()
);
#3159=(
BOUNDED_SURFACE()
B_SPLINE_SURFACE(3,2,((#209301,#209302,#209303),(#209304,#209305,#209306),
(#209307,#209308,#209309),(#209310,#209311,#209312),(#209313,#209314,#209315),
(#209316,#209317,#209318)),.UNSPECIFIED.,.F.,.F.,.F.)
B_SPLINE_SURFACE_WITH_KNOTS((4,2,4),(3,3),(0.,0.000256915317531254,0.000513830635062507),
(0.,1.),.UNSPECIFIED.)
GEOMETRIC_REPRESENTATION_ITEM()
RATIONAL_B_SPLINE_SURFACE(((1.,0.705585838031438,1.),(1.,0.750902433543063,
1.),(1.,0.792329530082044,1.),(1.,0.854288401594628,1.),(1.,0.874998031124815,
1.),(1.,0.874619707139389,1.)))
REPRESENTATION_ITEM('')
SURFACE()
);
#3160=(
BOUNDED_SURFACE()
B_SPLINE_SURFACE(3,2,((#209324,#209325,#209326),(#209327,#209328,#209329),
(#209330,#209331,#209332),(#209333,#209334,#209335),(#209336,#209337,#209338),
(#209339,#209340,#209341)),.UNSPECIFIED.,.F.,.F.,.F.)
B_SPLINE_SURFACE_WITH_KNOTS((4,2,4),(3,3),(-8.94466792300541E-18,0.000256592814262149,
0.000513185628524306),(0.,1.),.UNSPECIFIED.)
GEOMETRIC_REPRESENTATION_ITEM()
RATIONAL_B_SPLINE_SURFACE(((1.,0.708712527163696,1.),(1.,0.753780902613059,
1.),(1.,0.794538995769904,1.),(1.,0.855070770330386,1.),(1.,0.875018427445873,
1.),(1.,0.874619707139387,1.)))
REPRESENTATION_ITEM('')
SURFACE()
);
#3161=(
BOUNDED_SURFACE()
B_SPLINE_SURFACE(3,2,((#209343,#209344,#209345),(#209346,#209347,#209348),
(#209349,#209350,#209351),(#209352,#209353,#209354)),.UNSPECIFIED.,.F.,
 .F.,.F.)
B_SPLINE_SURFACE_WITH_KNOTS((4,4),(3,3),(-5.52943107967607E-18,0.000511815072430393),
(0.,1.0010559836602),.UNSPECIFIED.)
GEOMETRIC_REPRESENTATION_ITEM()
RATIONAL_B_SPLINE_SURFACE(((1.,0.706797490733287,1.00061923411783),(1.,
0.706182062146219,1.00062053388289),(1.,0.705584062768592,1.00062179683803),
(1.,0.705266224770059,1.0006224681015)))
REPRESENTATION_ITEM('')
SURFACE()
);
#3162=(
BOUNDED_SURFACE()
B_SPLINE_SURFACE(3,2,((#209360,#209361,#209362),(#209363,#209364,#209365),
(#209366,#209367,#209368),(#209369,#209370,#209371),(#209372,#209373,#209374),
(#209375,#209376,#209377)),.UNSPECIFIED.,.F.,.F.,.F.)
B_SPLINE_SURFACE_WITH_KNOTS((4,2,4),(3,3),(1.35525271560688E-20,0.000257652232350877,
0.000515304464701754),(0.,1.),.UNSPECIFIED.)
GEOMETRIC_REPRESENTATION_ITEM()
RATIONAL_B_SPLINE_SURFACE(((1.,0.874619707139397,1.),(1.,0.874861180430313,
1.),(1.,0.855455725921391,1.),(1.,0.79469935895477,1.),(1.,0.753768977788991,
1.),(1.,0.708712527163673,1.)))
REPRESENTATION_ITEM('')
SURFACE()
);
#3163=(
BOUNDED_SURFACE()
B_SPLINE_SURFACE(3,2,((#209383,#209384,#209385),(#209386,#209387,#209388),
(#209389,#209390,#209391),(#209392,#209393,#209394)),.UNSPECIFIED.,.F.,
 .F.,.F.)
B_SPLINE_SURFACE_WITH_KNOTS((4,4),(3,3),(0.,0.000397394373651919),(0.,1.),
 .UNSPECIFIED.)
GEOMETRIC_REPRESENTATION_ITEM()
RATIONAL_B_SPLINE_SURFACE(((1.,0.707106781186559,1.),(1.,0.707752587915881,
1.),(1.,0.708377654540695,1.),(1.,0.70868977088332,1.)))
REPRESENTATION_ITEM('')
SURFACE()
);
#3164=(
BOUNDED_SURFACE()
B_SPLINE_SURFACE(3,2,((#209396,#209397,#209398),(#209399,#209400,#209401),
(#209402,#209403,#209404),(#209405,#209406,#209407)),.UNSPECIFIED.,.F.,
 .F.,.F.)
B_SPLINE_SURFACE_WITH_KNOTS((4,4),(3,3),(0.,0.000511815456479789),(0.,1.00105873160043),
 .UNSPECIFIED.)
GEOMETRIC_REPRESENTATION_ITEM()
RATIONAL_B_SPLINE_SURFACE(((1.,0.708394529056183,1.00061746385389),(1.,
0.70805856416675,1.00061817524718),(1.,0.707430835371893,1.00061950443981),
(1.,0.706796685880238,1.00062084722802)))
REPRESENTATION_ITEM('')
SURFACE()
);
#3165=(
BOUNDED_SURFACE()
B_SPLINE_SURFACE(3,2,((#209413,#209414,#209415),(#209416,#209417,#209418),
(#209419,#209420,#209421),(#209422,#209423,#209424)),.UNSPECIFIED.,.F.,
 .F.,.F.)
B_SPLINE_SURFACE_WITH_KNOTS((4,4),(3,3),(-6.50521303491303E-18,0.000397394465448301),
(0.,1.),.UNSPECIFIED.)
GEOMETRIC_REPRESENTATION_ITEM()
RATIONAL_B_SPLINE_SURFACE(((1.,0.705498956110777,1.),(1.,0.705821764811791,
1.),(1.,0.706461952521121,1.),(1.,0.707106781186559,1.)))
REPRESENTATION_ITEM('')
SURFACE()
);
#3166=(
BOUNDED_SURFACE()
B_SPLINE_SURFACE(3,2,((#209430,#209431,#209432),(#209433,#209434,#209435),
(#209436,#209437,#209438),(#209439,#209440,#209441)),.UNSPECIFIED.,.F.,
 .F.,.F.)
B_SPLINE_SURFACE_WITH_KNOTS((4,4),(3,3),(0.,0.000397394410828737),(0.,1.),
 .UNSPECIFIED.)
GEOMETRIC_REPRESENTATION_ITEM()
RATIONAL_B_SPLINE_SURFACE(((1.,0.708689770883354,1.),(1.,0.708376440034479,
1.),(1.,0.707750498698412,1.),(1.,0.707106781186548,1.)))
REPRESENTATION_ITEM('')
SURFACE()
);
#3167=(
BOUNDED_SURFACE()
B_SPLINE_SURFACE(3,2,((#209447,#209448,#209449),(#209450,#209451,#209452),
(#209453,#209454,#209455),(#209456,#209457,#209458)),.UNSPECIFIED.,.F.,
 .F.,.F.)
B_SPLINE_SURFACE_WITH_KNOTS((4,4),(3,3),(0.,0.000511815090126188),(0.,1.0010559227012),
 .UNSPECIFIED.)
GEOMETRIC_REPRESENTATION_ITEM()
RATIONAL_B_SPLINE_SURFACE(((1.,0.705266242717776,1.00062243213025),(1.,
0.705584085909439,1.00062176089456),(1.,0.706182089450786,1.00062049800353),
(1.,0.706797508587776,1.00061919833346)))
REPRESENTATION_ITEM('')
SURFACE()
);
#3168=(
BOUNDED_SURFACE()
B_SPLINE_SURFACE(3,2,((#209460,#209461,#209462),(#209463,#209464,#209465),
(#209466,#209467,#209468),(#209469,#209470,#209471)),.UNSPECIFIED.,.F.,
 .F.,.F.)
B_SPLINE_SURFACE_WITH_KNOTS((4,4),(3,3),(-1.69948690537103E-17,0.000397394428086611),
(0.,1.),.UNSPECIFIED.)
GEOMETRIC_REPRESENTATION_ITEM()
RATIONAL_B_SPLINE_SURFACE(((1.,0.707106781186546,1.),(1.,0.706459846759102,
1.),(1.,0.705820510737254,1.),(1.,0.70549895611076,1.)))
REPRESENTATION_ITEM('')
SURFACE()
);
#3169=(
BOUNDED_SURFACE()
B_SPLINE_SURFACE(3,2,((#209477,#209478,#209479),(#209480,#209481,#209482),
(#209483,#209484,#209485),(#209486,#209487,#209488),(#209489,#209490,#209491),
(#209492,#209493,#209494)),.UNSPECIFIED.,.F.,.F.,.F.)
B_SPLINE_SURFACE_WITH_KNOTS((4,2,4),(3,3),(0.,0.000257953807872847,0.000515907615745694),
(0.,1.),.UNSPECIFIED.)
GEOMETRIC_REPRESENTATION_ITEM()
RATIONAL_B_SPLINE_SURFACE(((1.,0.874619707139392,1.),(1.,0.874834349679603,
1.),(1.,0.854686104156984,1.),(1.,0.792476597915974,1.),(1.,0.750887854594486,
1.),(1.,0.705585838031442,1.)))
REPRESENTATION_ITEM('')
SURFACE()
);
#3170=(
BOUNDED_SURFACE()
B_SPLINE_SURFACE(3,2,((#209500,#209501,#209502),(#209503,#209504,#209505),
(#209506,#209507,#209508),(#209509,#209510,#209511)),.UNSPECIFIED.,.F.,
 .F.,.F.)
B_SPLINE_SURFACE_WITH_KNOTS((4,4),(3,3),(0.,0.000511815437699155),(0.,1.00105881331789),
 .UNSPECIFIED.)
GEOMETRIC_REPRESENTATION_ITEM()
RATIONAL_B_SPLINE_SURFACE(((1.,0.706796661945747,1.00062089519837),(1.,
0.707430821224615,1.00061955228579),(1.,0.708058545830165,1.00061822299944),
(1.,0.708394505252133,1.00061751156282)))
REPRESENTATION_ITEM('')
SURFACE()
);
#3171=(
BOUNDED_SURFACE()
B_SPLINE_SURFACE(3,2,((#209513,#209514,#209515),(#209516,#209517,#209518),
(#209519,#209520,#209521),(#209522,#209523,#209524),(#209525,#209526,#209527),
(#209528,#209529,#209530)),.UNSPECIFIED.,.F.,.F.,.F.)
B_SPLINE_SURFACE_WITH_KNOTS((4,2,4),(3,3),(0.,0.000256915317531267,0.000513830635062534),
(0.,1.),.UNSPECIFIED.)
GEOMETRIC_REPRESENTATION_ITEM()
RATIONAL_B_SPLINE_SURFACE(((1.,0.705585838031445,1.),(1.,0.75090243354203,
1.),(1.,0.792329530083494,1.),(1.,0.854288401593243,1.),(1.,0.874998031125855,
1.),(1.,0.874619707139413,1.)))
REPRESENTATION_ITEM('')
SURFACE()
);
#3172=(
BOUNDED_SURFACE()
B_SPLINE_SURFACE(3,2,((#209536,#209537,#209538),(#209539,#209540,#209541),
(#209542,#209543,#209544),(#209545,#209546,#209547),(#209548,#209549,#209550),
(#209551,#209552,#209553)),.UNSPECIFIED.,.F.,.F.,.F.)
B_SPLINE_SURFACE_WITH_KNOTS((4,2,4),(3,3),(-7.23704950134074E-18,0.000256592814262153,
0.000513185628524314),(0.,1.),.UNSPECIFIED.)
GEOMETRIC_REPRESENTATION_ITEM()
RATIONAL_B_SPLINE_SURFACE(((1.,0.708712527163663,1.),(1.,0.753780902613181,
1.),(1.,0.794538995769752,1.),(1.,0.855070770330559,1.),(1.,0.875018427445738,
1.),(1.,0.874619707139388,1.)))
REPRESENTATION_ITEM('')
SURFACE()
);
#3173=(
BOUNDED_SURFACE()
B_SPLINE_SURFACE(3,2,((#209555,#209556,#209557),(#209558,#209559,#209560),
(#209561,#209562,#209563),(#209564,#209565,#209566)),.UNSPECIFIED.,.F.,
 .F.,.F.)
B_SPLINE_SURFACE_WITH_KNOTS((4,4),(3,3),(0.,0.000511815072430406),(0.,1.001055983659),
 .UNSPECIFIED.)
GEOMETRIC_REPRESENTATION_ITEM()
RATIONAL_B_SPLINE_SURFACE(((1.,0.706797490733647,1.00061923411713),(1.,
0.706182062146584,1.00062053388219),(1.,0.705584062768908,1.00062179683733),
(1.,0.70526622477043,1.0006224681008)))
REPRESENTATION_ITEM('')
SURFACE()
);
#3174=(
BOUNDED_SURFACE()
B_SPLINE_SURFACE(3,2,((#209572,#209573,#209574),(#209575,#209576,#209577),
(#209578,#209579,#209580),(#209581,#209582,#209583),(#209584,#209585,#209586),
(#209587,#209588,#209589)),.UNSPECIFIED.,.F.,.F.,.F.)
B_SPLINE_SURFACE_WITH_KNOTS((4,2,4),(3,3),(0.,0.000257652232350887,0.000515304464701775),
(0.,1.),.UNSPECIFIED.)
GEOMETRIC_REPRESENTATION_ITEM()
RATIONAL_B_SPLINE_SURFACE(((1.,0.874619707139375,1.),(1.,0.874861180430142,
1.),(1.,0.8554557259216,1.),(1.,0.7946993589545,1.),(1.,0.753768977789186,
1.),(1.,0.708712527163656,1.)))
REPRESENTATION_ITEM('')
SURFACE()
);
#3175=(
BOUNDED_SURFACE()
B_SPLINE_SURFACE(3,2,((#209595,#209596,#209597),(#209598,#209599,#209600),
(#209601,#209602,#209603),(#209604,#209605,#209606)),.UNSPECIFIED.,.F.,
 .F.,.F.)
B_SPLINE_SURFACE_WITH_KNOTS((4,4),(3,3),(0.,0.000397394373651914),(0.,1.),
 .UNSPECIFIED.)
GEOMETRIC_REPRESENTATION_ITEM()
RATIONAL_B_SPLINE_SURFACE(((1.,0.707106781186558,1.),(1.,0.707752587915874,
1.),(1.,0.708377654540684,1.),(1.,0.708689770883325,1.)))
REPRESENTATION_ITEM('')
SURFACE()
);
#3176=(
BOUNDED_SURFACE()
B_SPLINE_SURFACE(3,2,((#209608,#209609,#209610),(#209611,#209612,#209613),
(#209614,#209615,#209616),(#209617,#209618,#209619)),.UNSPECIFIED.,.F.,
 .F.,.F.)
B_SPLINE_SURFACE_WITH_KNOTS((4,4),(3,3),(0.,0.000511815456479791),(0.,1.00105873160094),
 .UNSPECIFIED.)
GEOMETRIC_REPRESENTATION_ITEM()
RATIONAL_B_SPLINE_SURFACE(((1.,0.708394529056042,1.00061746385419),(1.,
0.7080585641666,1.00061817524748),(1.,0.707430835371753,1.0006195044401),
(1.,0.706796685880089,1.00062084722832)))
REPRESENTATION_ITEM('')
SURFACE()
);
#3177=(
BOUNDED_SURFACE()
B_SPLINE_SURFACE(3,2,((#209625,#209626,#209627),(#209628,#209629,#209630),
(#209631,#209632,#209633),(#209634,#209635,#209636)),.UNSPECIFIED.,.F.,
 .F.,.F.)
B_SPLINE_SURFACE_WITH_KNOTS((4,4),(3,3),(0.,0.00039739446544832),(0.,1.),
 .UNSPECIFIED.)
GEOMETRIC_REPRESENTATION_ITEM()
RATIONAL_B_SPLINE_SURFACE(((1.,0.705498956110787,1.),(1.,0.705821764811737,
1.),(1.,0.706461952521161,1.),(1.,0.707106781186548,1.)))
REPRESENTATION_ITEM('')
SURFACE()
);
#3178=(
BOUNDED_SURFACE()
B_SPLINE_SURFACE(3,2,((#209642,#209643,#209644),(#209645,#209646,#209647),
(#209648,#209649,#209650),(#209651,#209652,#209653)),.UNSPECIFIED.,.F.,
 .F.,.F.)
B_SPLINE_SURFACE_WITH_KNOTS((4,4),(3,3),(0.,0.000397394410828738),(0.,1.),
 .UNSPECIFIED.)
GEOMETRIC_REPRESENTATION_ITEM()
RATIONAL_B_SPLINE_SURFACE(((1.,0.708689770883308,1.),(1.,0.708376440034552,
1.),(1.,0.707750498698383,1.),(1.,0.707106781186548,1.)))
REPRESENTATION_ITEM('')
SURFACE()
);
#3179=(
BOUNDED_SURFACE()
B_SPLINE_SURFACE(3,2,((#209659,#209660,#209661),(#209662,#209663,#209664),
(#209665,#209666,#209667),(#209668,#209669,#209670)),.UNSPECIFIED.,.F.,
 .F.,.F.)
B_SPLINE_SURFACE_WITH_KNOTS((4,4),(3,3),(0.,0.000511815090126185),(0.,1.00105592270171),
 .UNSPECIFIED.)
GEOMETRIC_REPRESENTATION_ITEM()
RATIONAL_B_SPLINE_SURFACE(((1.,0.705266242717622,1.00062243213055),(1.,
0.705584085909267,1.00062176089486),(1.,0.706182089450651,1.00062049800383),
(1.,0.706797508587617,1.00061919833376)))
REPRESENTATION_ITEM('')
SURFACE()
);
#3180=(
BOUNDED_SURFACE()
B_SPLINE_SURFACE(3,2,((#209672,#209673,#209674),(#209675,#209676,#209677),
(#209678,#209679,#209680),(#209681,#209682,#209683)),.UNSPECIFIED.,.F.,
 .F.,.F.)
B_SPLINE_SURFACE_WITH_KNOTS((4,4),(3,3),(-7.61652026171067E-18,0.000397394428086623),
(0.,1.),.UNSPECIFIED.)
GEOMETRIC_REPRESENTATION_ITEM()
RATIONAL_B_SPLINE_SURFACE(((1.,0.707106781186548,1.),(1.,0.7064598467591,
1.),(1.,0.705820510737261,1.),(1.,0.705498956110754,1.)))
REPRESENTATION_ITEM('')
SURFACE()
);
#3181=(
BOUNDED_SURFACE()
B_SPLINE_SURFACE(3,2,((#209689,#209690,#209691),(#209692,#209693,#209694),
(#209695,#209696,#209697),(#209698,#209699,#209700),(#209701,#209702,#209703),
(#209704,#209705,#209706)),.UNSPECIFIED.,.F.,.F.,.F.)
B_SPLINE_SURFACE_WITH_KNOTS((4,2,4),(3,3),(0.,0.000257953807872849,0.000515907615745698),
(0.,1.),.UNSPECIFIED.)
GEOMETRIC_REPRESENTATION_ITEM()
RATIONAL_B_SPLINE_SURFACE(((1.,0.874619707139392,1.),(1.,0.8748343496791,
1.),(1.,0.854686104157651,1.),(1.,0.792476597915266,1.),(1.,0.750887854595039,
1.),(1.,0.705585838031425,1.)))
REPRESENTATION_ITEM('')
SURFACE()
);
#3182=(
BOUNDED_SURFACE()
B_SPLINE_SURFACE(3,2,((#209712,#209713,#209714),(#209715,#209716,#209717),
(#209718,#209719,#209720),(#209721,#209722,#209723)),.UNSPECIFIED.,.F.,
 .F.,.F.)
B_SPLINE_SURFACE_WITH_KNOTS((4,4),(3,3),(0.,0.000511815437699155),(0.,1.00105881331537),
 .UNSPECIFIED.)
GEOMETRIC_REPRESENTATION_ITEM()
RATIONAL_B_SPLINE_SURFACE(((1.,0.706796661946478,1.00062089519688),(1.,
0.707430821225356,1.00061955228431),(1.,0.708058545830873,1.00061822299797),
(1.,0.708394505252873,1.00061751156135)))
REPRESENTATION_ITEM('')
SURFACE()
);
#3183=(
BOUNDED_SURFACE()
B_SPLINE_SURFACE(3,2,((#209725,#209726,#209727),(#209728,#209729,#209730),
(#209731,#209732,#209733),(#209734,#209735,#209736),(#209737,#209738,#209739),
(#209740,#209741,#209742)),.UNSPECIFIED.,.F.,.F.,.F.)
B_SPLINE_SURFACE_WITH_KNOTS((4,2,4),(3,3),(0.,0.000256915317531255,0.00051383063506251),
(0.,1.),.UNSPECIFIED.)
GEOMETRIC_REPRESENTATION_ITEM()
RATIONAL_B_SPLINE_SURFACE(((1.,0.705585838031433,1.),(1.,0.750902433542673,
1.),(1.,0.792329530082634,1.),(1.,0.854288401594081,1.),(1.,0.874998031125218,
1.),(1.,0.874619707139388,1.)))
REPRESENTATION_ITEM('')
SURFACE()
);
#3184=(
BOUNDED_SURFACE()
B_SPLINE_SURFACE(3,2,((#209748,#209749,#209750),(#209751,#209752,#209753),
(#209754,#209755,#209756),(#209757,#209758,#209759),(#209760,#209761,#209762),
(#209763,#209764,#209765)),.UNSPECIFIED.,.F.,.F.,.F.)
B_SPLINE_SURFACE_WITH_KNOTS((4,2,4),(3,3),(-7.10152422978005E-18,0.000256592814262155,
0.000513185628524318),(0.,1.),.UNSPECIFIED.)
GEOMETRIC_REPRESENTATION_ITEM()
RATIONAL_B_SPLINE_SURFACE(((1.,0.708712527163678,1.),(1.,0.753780902613814,
1.),(1.,0.794538995768887,1.),(1.,0.855070770331403,1.),(1.,0.875018427445105,
1.),(1.,0.874619707139391,1.)))
REPRESENTATION_ITEM('')
SURFACE()
);
#3185=(
BOUNDED_SURFACE()
B_SPLINE_SURFACE(3,2,((#209767,#209768,#209769),(#209770,#209771,#209772),
(#209773,#209774,#209775),(#209776,#209777,#209778)),.UNSPECIFIED.,.F.,
 .F.,.F.)
B_SPLINE_SURFACE_WITH_KNOTS((4,4),(3,3),(0.,0.000511815072430409),(0.,1.00105598366036),
 .UNSPECIFIED.)
GEOMETRIC_REPRESENTATION_ITEM()
RATIONAL_B_SPLINE_SURFACE(((1.,0.706797490733251,1.00061923411792),(1.,
0.706182062146167,1.00062053388299),(1.,0.705584062768538,1.00062179683813),
(1.,0.70526622477001,1.0006224681016)))
REPRESENTATION_ITEM('')
SURFACE()
);
#3186=(
BOUNDED_SURFACE()
B_SPLINE_SURFACE(3,2,((#209784,#209785,#209786),(#209787,#209788,#209789),
(#209790,#209791,#209792),(#209793,#209794,#209795),(#209796,#209797,#209798),
(#209799,#209800,#209801)),.UNSPECIFIED.,.F.,.F.,.F.)
B_SPLINE_SURFACE_WITH_KNOTS((4,2,4),(3,3),(-2.99510850149121E-18,0.000257652232350881,
0.000515304464701765),(0.,1.),.UNSPECIFIED.)
GEOMETRIC_REPRESENTATION_ITEM()
RATIONAL_B_SPLINE_SURFACE(((1.,0.87461970713939,1.),(1.,0.874861180430529,
1.),(1.,0.855455725921095,1.),(1.,0.794699358955062,1.),(1.,0.75376897778881,
1.),(1.,0.708712527163653,1.)))
REPRESENTATION_ITEM('')
SURFACE()
);
#3187=(
BOUNDED_SURFACE()
B_SPLINE_SURFACE(3,2,((#209807,#209808,#209809),(#209810,#209811,#209812),
(#209813,#209814,#209815),(#209816,#209817,#209818)),.UNSPECIFIED.,.F.,
 .F.,.F.)
B_SPLINE_SURFACE_WITH_KNOTS((4,4),(3,3),(0.,0.000397394373651926),(0.,1.),
 .UNSPECIFIED.)
GEOMETRIC_REPRESENTATION_ITEM()
RATIONAL_B_SPLINE_SURFACE(((1.,0.707106781186548,1.),(1.,0.70775258791589,
1.),(1.,0.708377654540707,1.),(1.,0.708689770883312,1.)))
REPRESENTATION_ITEM('')
SURFACE()
);
#3188=(
BOUNDED_SURFACE()
B_SPLINE_SURFACE(3,2,((#209820,#209821,#209822),(#209823,#209824,#209825),
(#209826,#209827,#209828),(#209829,#209830,#209831)),.UNSPECIFIED.,.F.,
 .F.,.F.)
B_SPLINE_SURFACE_WITH_KNOTS((4,4),(3,3),(0.,0.000511815456479792),(0.,1.00105873159908),
 .UNSPECIFIED.)
GEOMETRIC_REPRESENTATION_ITEM()
RATIONAL_B_SPLINE_SURFACE(((1.,0.708394529056577,1.00061746385311),(1.,
0.708058564167112,1.0006181752464),(1.,0.707430835372313,1.00061950443902),
(1.,0.70679668588064,1.00062084722723)))
REPRESENTATION_ITEM('')
SURFACE()
);
#3189=(
BOUNDED_SURFACE()
B_SPLINE_SURFACE(3,2,((#209837,#209838,#209839),(#209840,#209841,#209842),
(#209843,#209844,#209845),(#209846,#209847,#209848)),.UNSPECIFIED.,.F.,
 .F.,.F.)
B_SPLINE_SURFACE_WITH_KNOTS((4,4),(3,3),(-6.53231808922516E-18,0.000397394465448313),
(0.,1.),.UNSPECIFIED.)
GEOMETRIC_REPRESENTATION_ITEM()
RATIONAL_B_SPLINE_SURFACE(((1.,0.705498956110761,1.),(1.,0.705821764811792,
1.),(1.,0.706461952521145,1.),(1.,0.70710678118654,1.)))
REPRESENTATION_ITEM('')
SURFACE()
);
#3190=(
BOUNDED_SURFACE()
B_SPLINE_SURFACE(3,2,((#209854,#209855,#209856),(#209857,#209858,#209859),
(#209860,#209861,#209862),(#209863,#209864,#209865)),.UNSPECIFIED.,.F.,
 .F.,.F.)
B_SPLINE_SURFACE_WITH_KNOTS((4,4),(3,3),(0.,0.000397394410828728),(0.,1.),
 .UNSPECIFIED.)
GEOMETRIC_REPRESENTATION_ITEM()
RATIONAL_B_SPLINE_SURFACE(((1.,0.708689770883319,1.),(1.,0.708376440034518,
1.),(1.,0.707750498698381,1.),(1.,0.707106781186553,1.)))
REPRESENTATION_ITEM('')
SURFACE()
);
#3191=(
BOUNDED_SURFACE()
B_SPLINE_SURFACE(3,2,((#209871,#209872,#209873),(#209874,#209875,#209876),
(#209877,#209878,#209879),(#209880,#209881,#209882)),.UNSPECIFIED.,.F.,
 .F.,.F.)
B_SPLINE_SURFACE_WITH_KNOTS((4,4),(3,3),(0.,0.000511815090126188),(0.,1.00105592270323),
 .UNSPECIFIED.)
GEOMETRIC_REPRESENTATION_ITEM()
RATIONAL_B_SPLINE_SURFACE(((1.,0.705266242717189,1.00062243213145),(1.,
0.705584085908845,1.00062176089576),(1.,0.706182089450181,1.00062049800473),
(1.,0.706797508587185,1.00061919833465)))
REPRESENTATION_ITEM('')
SURFACE()
);
#3192=(
BOUNDED_SURFACE()
B_SPLINE_SURFACE(3,2,((#209884,#209885,#209886),(#209887,#209888,#209889),
(#209890,#209891,#209892),(#209893,#209894,#209895)),.UNSPECIFIED.,.F.,
 .F.,.F.)
B_SPLINE_SURFACE_WITH_KNOTS((4,4),(3,3),(0.,0.000397394428086621),(0.,1.),
 .UNSPECIFIED.)
GEOMETRIC_REPRESENTATION_ITEM()
RATIONAL_B_SPLINE_SURFACE(((1.,0.707106781186553,1.),(1.,0.706459846759084,
1.),(1.,0.705820510737283,1.),(1.,0.705498956110755,1.)))
REPRESENTATION_ITEM('')
SURFACE()
);
#3193=(
BOUNDED_SURFACE()
B_SPLINE_SURFACE(3,2,((#209901,#209902,#209903),(#209904,#209905,#209906),
(#209907,#209908,#209909),(#209910,#209911,#209912),(#209913,#209914,#209915),
(#209916,#209917,#209918)),.UNSPECIFIED.,.F.,.F.,.F.)
B_SPLINE_SURFACE_WITH_KNOTS((4,2,4),(3,3),(-3.15773882736403E-18,0.000257953807872849,
0.0005159076157457),(0.,1.),.UNSPECIFIED.)
GEOMETRIC_REPRESENTATION_ITEM()
RATIONAL_B_SPLINE_SURFACE(((1.,0.874619707139386,1.),(1.,0.874834349679202,
1.),(1.,0.854686104157527,1.),(1.,0.792476597915401,1.),(1.,0.750887854594934,
1.),(1.,0.705585838031451,1.)))
REPRESENTATION_ITEM('')
SURFACE()
);
#3194=(
BOUNDED_SURFACE()
B_SPLINE_SURFACE(3,2,((#209924,#209925,#209926),(#209927,#209928,#209929),
(#209930,#209931,#209932),(#209933,#209934,#209935)),.UNSPECIFIED.,.F.,
 .F.,.F.)
B_SPLINE_SURFACE_WITH_KNOTS((4,4),(3,3),(0.,0.000511815437699157),(0.,1.00105881331785),
 .UNSPECIFIED.)
GEOMETRIC_REPRESENTATION_ITEM()
RATIONAL_B_SPLINE_SURFACE(((1.,0.706796661945761,1.00062089519834),(1.,
0.707430821224659,1.00061955228576),(1.,0.708058545830114,1.00061822299941),
(1.,0.70839450525216,1.00061751156279)))
REPRESENTATION_ITEM('')
SURFACE()
);
#3195=(
BOUNDED_SURFACE()
B_SPLINE_SURFACE(3,2,((#209937,#209938,#209939),(#209940,#209941,#209942),
(#209943,#209944,#209945),(#209946,#209947,#209948),(#209949,#209950,#209951),
(#209952,#209953,#209954)),.UNSPECIFIED.,.F.,.F.,.F.)
B_SPLINE_SURFACE_WITH_KNOTS((4,2,4),(3,3),(2.71050543121376E-20,0.00025691531753126,
0.00051383063506252),(0.,1.),.UNSPECIFIED.)
GEOMETRIC_REPRESENTATION_ITEM()
RATIONAL_B_SPLINE_SURFACE(((1.,0.705585838031445,1.),(1.,0.750902433542712,
1.),(1.,0.792329530082526,1.),(1.,0.854288401594204,1.),(1.,0.874998031125109,
1.),(1.,0.874619707139405,1.)))
REPRESENTATION_ITEM('')
SURFACE()
);
#3196=(
BOUNDED_SURFACE()
B_SPLINE_SURFACE(3,2,((#209960,#209961,#209962),(#209963,#209964,#209965),
(#209966,#209967,#209968),(#209969,#209970,#209971),(#209972,#209973,#209974),
(#209975,#209976,#209977)),.UNSPECIFIED.,.F.,.F.,.F.)
B_SPLINE_SURFACE_WITH_KNOTS((4,2,4),(3,3),(-5.77337656848531E-18,0.000256592814262153,
0.000513185628524312),(0.,1.),.UNSPECIFIED.)
GEOMETRIC_REPRESENTATION_ITEM()
RATIONAL_B_SPLINE_SURFACE(((1.,0.708712527163637,1.),(1.,0.753780902613617,
1.),(1.,0.794538995769177,1.),(1.,0.855070770331119,1.),(1.,0.875018427445295,
1.),(1.,0.874619707139396,1.)))
REPRESENTATION_ITEM('')
SURFACE()
);
#3197=(
BOUNDED_SURFACE()
B_SPLINE_SURFACE(3,2,((#209979,#209980,#209981),(#209982,#209983,#209984),
(#209985,#209986,#209987),(#209988,#209989,#209990)),.UNSPECIFIED.,.F.,
 .F.,.F.)
B_SPLINE_SURFACE_WITH_KNOTS((4,4),(3,3),(-7.58941520739853E-18,0.000511815072430402),
(0.,1.00105598365911),.UNSPECIFIED.)
GEOMETRIC_REPRESENTATION_ITEM()
RATIONAL_B_SPLINE_SURFACE(((1.,0.706797490733615,1.00061923411719),(1.,
0.706182062146498,1.00062053388226),(1.,0.705584062768905,1.0006217968374),
(1.,0.705266224770394,1.00062246810086)))
REPRESENTATION_ITEM('')
SURFACE()
);
#3198=(
BOUNDED_SURFACE()
B_SPLINE_SURFACE(3,2,((#209996,#209997,#209998),(#209999,#210000,#210001),
(#210002,#210003,#210004),(#210005,#210006,#210007),(#210008,#210009,#210010),
(#210011,#210012,#210013)),.UNSPECIFIED.,.F.,.F.,.F.)
B_SPLINE_SURFACE_WITH_KNOTS((4,2,4),(3,3),(-3.14418630020796E-18,0.000257652232350881,
0.000515304464701764),(0.,1.),.UNSPECIFIED.)
GEOMETRIC_REPRESENTATION_ITEM()
RATIONAL_B_SPLINE_SURFACE(((1.,0.874619707139394,1.),(1.,0.874861180431435,
1.),(1.,0.855455725919893,1.),(1.,0.794699358956221,1.),(1.,0.753768977787944,
1.),(1.,0.708712527163638,1.)))
REPRESENTATION_ITEM('')
SURFACE()
);
#3199=(
BOUNDED_SURFACE()
B_SPLINE_SURFACE(3,2,((#210019,#210020,#210021),(#210022,#210023,#210024),
(#210025,#210026,#210027),(#210028,#210029,#210030)),.UNSPECIFIED.,.F.,
 .F.,.F.)
B_SPLINE_SURFACE_WITH_KNOTS((4,4),(3,3),(-1.40675231879994E-17,0.000397394373651907),
(0.,1.),.UNSPECIFIED.)
GEOMETRIC_REPRESENTATION_ITEM()
RATIONAL_B_SPLINE_SURFACE(((1.,0.707106781186542,1.),(1.,0.707752587915892,
1.),(1.,0.708377654540694,1.),(1.,0.708689770883334,1.)))
REPRESENTATION_ITEM('')
SURFACE()
);
#3200=(
BOUNDED_SURFACE()
B_SPLINE_SURFACE(3,2,((#210032,#210033,#210034),(#210035,#210036,#210037),
(#210038,#210039,#210040),(#210041,#210042,#210043)),.UNSPECIFIED.,.F.,
 .F.,.F.)
B_SPLINE_SURFACE_WITH_KNOTS((4,4),(3,3),(-6.42389787197661E-18,0.00051181545647979),
(0.,1.00105873159698),.UNSPECIFIED.)
GEOMETRIC_REPRESENTATION_ITEM()
RATIONAL_B_SPLINE_SURFACE(((1.,0.708394529057203,1.00061746385188),(1.,
0.708058564167751,1.00061817524516),(1.,0.707430835372928,1.00061950443778),
(1.,0.70679668588125,1.00062084722599)))
REPRESENTATION_ITEM('')
SURFACE()
);
#3201=(
BOUNDED_SURFACE()
B_SPLINE_SURFACE(3,2,((#210049,#210050,#210051),(#210052,#210053,#210054),
(#210055,#210056,#210057),(#210058,#210059,#210060)),.UNSPECIFIED.,.F.,
 .F.,.F.)
B_SPLINE_SURFACE_WITH_KNOTS((4,4),(3,3),(0.,0.000397394465448308),(0.,1.),
 .UNSPECIFIED.)
GEOMETRIC_REPRESENTATION_ITEM()
RATIONAL_B_SPLINE_SURFACE(((1.,0.705498956110747,1.),(1.,0.705821764811728,
1.),(1.,0.706461952521178,1.),(1.,0.707106781186542,1.)))
REPRESENTATION_ITEM('')
SURFACE()
);
#3202=(
BOUNDED_SURFACE()
B_SPLINE_SURFACE(3,2,((#210066,#210067,#210068),(#210069,#210070,#210071),
(#210072,#210073,#210074),(#210075,#210076,#210077)),.UNSPECIFIED.,.F.,
 .F.,.F.)
B_SPLINE_SURFACE_WITH_KNOTS((4,4),(3,3),(0.,0.000397394410828749),(0.,1.),
 .UNSPECIFIED.)
GEOMETRIC_REPRESENTATION_ITEM()
RATIONAL_B_SPLINE_SURFACE(((1.,0.708689770883333,1.),(1.,0.708376440034485,
1.),(1.,0.707750498698427,1.),(1.,0.707106781186548,1.)))
REPRESENTATION_ITEM('')
SURFACE()
);
#3203=(
BOUNDED_SURFACE()
B_SPLINE_SURFACE(3,2,((#210083,#210084,#210085),(#210086,#210087,#210088),
(#210089,#210090,#210091),(#210092,#210093,#210094)),.UNSPECIFIED.,.F.,
 .F.,.F.)
B_SPLINE_SURFACE_WITH_KNOTS((4,4),(3,3),(0.,0.00051181509012617),(0.,1.00105592270455),
 .UNSPECIFIED.)
GEOMETRIC_REPRESENTATION_ITEM()
RATIONAL_B_SPLINE_SURFACE(((1.,0.705266242716791,1.00062243213223),(1.,
0.705584085908443,1.00062176089654),(1.,0.706182089449806,1.00062049800551),
(1.,0.706797508586792,1.00061919833543)))
REPRESENTATION_ITEM('')
SURFACE()
);
#3204=(
BOUNDED_SURFACE()
B_SPLINE_SURFACE(3,2,((#210096,#210097,#210098),(#210099,#210100,#210101),
(#210102,#210103,#210104),(#210105,#210106,#210107)),.UNSPECIFIED.,.F.,
 .F.,.F.)
B_SPLINE_SURFACE_WITH_KNOTS((4,4),(3,3),(0.,0.000397394428086618),(0.,1.),
 .UNSPECIFIED.)
GEOMETRIC_REPRESENTATION_ITEM()
RATIONAL_B_SPLINE_SURFACE(((1.,0.707106781186552,1.),(1.,0.706459846759076,
1.),(1.,0.705820510737295,1.),(1.,0.705498956110739,1.)))
REPRESENTATION_ITEM('')
SURFACE()
);
#3205=(
BOUNDED_SURFACE()
B_SPLINE_SURFACE(3,2,((#210113,#210114,#210115),(#210116,#210117,#210118),
(#210119,#210120,#210121),(#210122,#210123,#210124),(#210125,#210126,#210127),
(#210128,#210129,#210130)),.UNSPECIFIED.,.F.,.F.,.F.)
B_SPLINE_SURFACE_WITH_KNOTS((4,2,4),(3,3),(0.,0.000257953807872849,0.000515907615745698),
(0.,1.),.UNSPECIFIED.)
GEOMETRIC_REPRESENTATION_ITEM()
RATIONAL_B_SPLINE_SURFACE(((1.,0.874619707139397,1.),(1.,0.874834349678898,
1.),(1.,0.854686104157902,1.),(1.,0.792476597915046,1.),(1.,0.750887854595174,
1.),(1.,0.70558583803143,1.)))
REPRESENTATION_ITEM('')
SURFACE()
);
#3206=(
BOUNDED_SURFACE()
B_SPLINE_SURFACE(3,2,((#210136,#210137,#210138),(#210139,#210140,#210141),
(#210142,#210143,#210144),(#210145,#210146,#210147)),.UNSPECIFIED.,.F.,
 .F.,.F.)
B_SPLINE_SURFACE_WITH_KNOTS((4,4),(3,3),(0.,0.000511815437699145),(0.,1.0010588133135),
 .UNSPECIFIED.)
GEOMETRIC_REPRESENTATION_ITEM()
RATIONAL_B_SPLINE_SURFACE(((1.,0.706796661947034,1.00062089519579),(1.,
0.707430821225921,1.00061955228321),(1.,0.708058545831377,1.00061822299687),
(1.,0.708394505253416,1.00061751156026)))
REPRESENTATION_ITEM('')
SURFACE()
);
#3207=(
BOUNDED_SURFACE()
B_SPLINE_SURFACE(3,2,((#210149,#210150,#210151),(#210152,#210153,#210154),
(#210155,#210156,#210157),(#210158,#210159,#210160),(#210161,#210162,#210163),
(#210164,#210165,#210166)),.UNSPECIFIED.,.F.,.F.,.F.)
B_SPLINE_SURFACE_WITH_KNOTS((4,2,4),(3,3),(-6.31547765472806E-18,0.000256915317531251,
0.000513830635062508),(0.,1.),.UNSPECIFIED.)
GEOMETRIC_REPRESENTATION_ITEM()
RATIONAL_B_SPLINE_SURFACE(((1.,0.705585838031427,1.),(1.,0.750902433542642,
1.),(1.,0.792329530082651,1.),(1.,0.854288401594041,1.),(1.,0.874998031125251,
1.),(1.,0.874619707139387,1.)))
REPRESENTATION_ITEM('')
SURFACE()
);
#3208=(
BOUNDED_SURFACE()
B_SPLINE_SURFACE(3,2,((#210172,#210173,#210174),(#210175,#210176,#210177),
(#210178,#210179,#210180),(#210181,#210182,#210183),(#210184,#210185,#210186),
(#210187,#210188,#210189)),.UNSPECIFIED.,.F.,.F.,.F.)
B_SPLINE_SURFACE_WITH_KNOTS((4,2,4),(3,3),(0.,0.000256592814262157,0.000513185628524314),
(0.,1.),.UNSPECIFIED.)
GEOMETRIC_REPRESENTATION_ITEM()
RATIONAL_B_SPLINE_SURFACE(((1.,0.708712527163669,1.),(1.,0.75378090261303,
1.),(1.,0.794538995769939,1.),(1.,0.855070770330402,1.),(1.,0.875018427445837,
1.),(1.,0.874619707139389,1.)))
REPRESENTATION_ITEM('')
SURFACE()
);
#3209=(
BOUNDED_SURFACE()
B_SPLINE_SURFACE(3,2,((#210191,#210192,#210193),(#210194,#210195,#210196),
(#210197,#210198,#210199),(#210200,#210201,#210202)),.UNSPECIFIED.,.F.,
 .F.,.F.)
B_SPLINE_SURFACE_WITH_KNOTS((4,4),(3,3),(2.71050543121376E-20,0.000511815072430395),
(0.,1.00105598366028),.UNSPECIFIED.)
GEOMETRIC_REPRESENTATION_ITEM()
RATIONAL_B_SPLINE_SURFACE(((1.,0.706797490733269,1.00061923411788),(1.,
0.706182062146185,1.00062053388294),(1.,0.705584062768579,1.00062179683809),
(1.,0.705266224770014,1.00062246810155)))
REPRESENTATION_ITEM('')
SURFACE()
);
#3210=(
BOUNDED_SURFACE()
B_SPLINE_SURFACE(3,2,((#210208,#210209,#210210),(#210211,#210212,#210213),
(#210214,#210215,#210216),(#210217,#210218,#210219),(#210220,#210221,#210222),
(#210223,#210224,#210225)),.UNSPECIFIED.,.F.,.F.,.F.)
B_SPLINE_SURFACE_WITH_KNOTS((4,2,4),(3,3),(0.,0.000257652232350882,0.000515304464701763),
(0.,1.),.UNSPECIFIED.)
GEOMETRIC_REPRESENTATION_ITEM()
RATIONAL_B_SPLINE_SURFACE(((1.,0.874619707139388,1.),(1.,0.874861180430589,
1.),(1.,0.855455725921058,1.),(1.,0.794699358955073,1.),(1.,0.753768977788798,
1.),(1.,0.708712527163669,1.)))
REPRESENTATION_ITEM('')
SURFACE()
);
#3211=(
BOUNDED_SURFACE()
B_SPLINE_SURFACE(3,2,((#210231,#210232,#210233),(#210234,#210235,#210236),
(#210237,#210238,#210239),(#210240,#210241,#210242)),.UNSPECIFIED.,.F.,
 .F.,.F.)
B_SPLINE_SURFACE_WITH_KNOTS((4,4),(3,3),(0.,0.000397394373651931),(0.,1.),
 .UNSPECIFIED.)
GEOMETRIC_REPRESENTATION_ITEM()
RATIONAL_B_SPLINE_SURFACE(((1.,0.707106781186543,1.),(1.,0.707752587915884,
1.),(1.,0.708377654540689,1.),(1.,0.708689770883328,1.)))
REPRESENTATION_ITEM('')
SURFACE()
);
#3212=(
BOUNDED_SURFACE()
B_SPLINE_SURFACE(3,2,((#210244,#210245,#210246),(#210247,#210248,#210249),
(#210250,#210251,#210252),(#210253,#210254,#210255)),.UNSPECIFIED.,.F.,
 .F.,.F.)
B_SPLINE_SURFACE_WITH_KNOTS((4,4),(3,3),(0.,0.000511815456479789),(0.,1.00105873159931),
 .UNSPECIFIED.)
GEOMETRIC_REPRESENTATION_ITEM()
RATIONAL_B_SPLINE_SURFACE(((1.,0.708394529056513,1.00061746385324),(1.,
0.708058564167068,1.00061817524653),(1.,0.707430835372242,1.00061950443915),
(1.,0.706796685880566,1.00062084722736)))
REPRESENTATION_ITEM('')
SURFACE()
);
#3213=(
BOUNDED_SURFACE()
B_SPLINE_SURFACE(3,2,((#210261,#210262,#210263),(#210264,#210265,#210266),
(#210267,#210268,#210269),(#210270,#210271,#210272)),.UNSPECIFIED.,.F.,
 .F.,.F.)
B_SPLINE_SURFACE_WITH_KNOTS((4,4),(3,3),(0.,0.000397394465448298),(0.,1.),
 .UNSPECIFIED.)
GEOMETRIC_REPRESENTATION_ITEM()
RATIONAL_B_SPLINE_SURFACE(((1.,0.705498956110754,1.),(1.,0.705821764811777,
1.),(1.,0.70646195252115,1.),(1.,0.707106781186543,1.)))
REPRESENTATION_ITEM('')
SURFACE()
);
#3214=(
BOUNDED_SURFACE()
B_SPLINE_SURFACE(3,2,((#210278,#210279,#210280),(#210281,#210282,#210283),
(#210284,#210285,#210286),(#210287,#210288,#210289)),.UNSPECIFIED.,.F.,
 .F.,.F.)
B_SPLINE_SURFACE_WITH_KNOTS((4,4),(3,3),(0.,0.000397394410828728),(0.,1.),
 .UNSPECIFIED.)
GEOMETRIC_REPRESENTATION_ITEM()
RATIONAL_B_SPLINE_SURFACE(((1.,0.708689770883309,1.),(1.,0.708376440034508,
1.),(1.,0.707750498698397,1.),(1.,0.707106781186548,1.)))
REPRESENTATION_ITEM('')
SURFACE()
);
#3215=(
BOUNDED_SURFACE()
B_SPLINE_SURFACE(3,2,((#210295,#210296,#210297),(#210298,#210299,#210300),
(#210301,#210302,#210303),(#210304,#210305,#210306)),.UNSPECIFIED.,.F.,
 .F.,.F.)
B_SPLINE_SURFACE_WITH_KNOTS((4,4),(3,3),(0.,0.000511815090126182),(0.,1.00105592270654),
 .UNSPECIFIED.)
GEOMETRIC_REPRESENTATION_ITEM()
RATIONAL_B_SPLINE_SURFACE(((1.,0.705266242716211,1.0006224321334),(1.,0.705584085907866,
1.00062176089771),(1.,0.706182089449231,1.00062049800668),(1.,0.706797508586209,
1.0006191983366)))
REPRESENTATION_ITEM('')
SURFACE()
);
#3216=(
BOUNDED_SURFACE()
B_SPLINE_SURFACE(3,2,((#210308,#210309,#210310),(#210311,#210312,#210313),
(#210314,#210315,#210316),(#210317,#210318,#210319)),.UNSPECIFIED.,.F.,
 .F.,.F.)
B_SPLINE_SURFACE_WITH_KNOTS((4,4),(3,3),(0.,0.00039739442808663),(0.,1.),
 .UNSPECIFIED.)
GEOMETRIC_REPRESENTATION_ITEM()
RATIONAL_B_SPLINE_SURFACE(((1.,0.70710678118655,1.),(1.,0.706459846759094,
1.),(1.,0.705820510737275,1.),(1.,0.705498956110756,1.)))
REPRESENTATION_ITEM('')
SURFACE()
);
#3217=(
BOUNDED_SURFACE()
B_SPLINE_SURFACE(3,2,((#210325,#210326,#210327),(#210328,#210329,#210330),
(#210331,#210332,#210333),(#210334,#210335,#210336),(#210337,#210338,#210339),
(#210340,#210341,#210342)),.UNSPECIFIED.,.F.,.F.,.F.)
B_SPLINE_SURFACE_WITH_KNOTS((4,2,4),(3,3),(0.,0.000257953807872841,0.000515907615745682),
(0.,1.),.UNSPECIFIED.)
GEOMETRIC_REPRESENTATION_ITEM()
RATIONAL_B_SPLINE_SURFACE(((1.,0.874619707139387,1.),(1.,0.874834349678916,
1.),(1.,0.854686104157876,1.),(1.,0.79247659791507,1.),(1.,0.750887854595179,
1.),(1.,0.705585838031445,1.)))
REPRESENTATION_ITEM('')
SURFACE()
);
#3218=(
BOUNDED_SURFACE()
B_SPLINE_SURFACE(3,2,((#210348,#210349,#210350),(#210351,#210352,#210353),
(#210354,#210355,#210356),(#210357,#210358,#210359)),.UNSPECIFIED.,.F.,
 .F.,.F.)
B_SPLINE_SURFACE_WITH_KNOTS((4,4),(3,3),(-6.91178884959509E-18,0.000511815437699147),
(0.,1.00105881331641),.UNSPECIFIED.)
GEOMETRIC_REPRESENTATION_ITEM()
RATIONAL_B_SPLINE_SURFACE(((1.,0.70679666194618,1.00062089519749),(1.,0.707430821225043,
1.00061955228491),(1.,0.708058545830579,1.00061822299857),(1.,0.708394505252563,
1.00061751156195)))
REPRESENTATION_ITEM('')
SURFACE()
);
#3219=(
BOUNDED_SURFACE()
B_SPLINE_SURFACE(3,2,((#210361,#210362,#210363),(#210364,#210365,#210366),
(#210367,#210368,#210369),(#210370,#210371,#210372),(#210373,#210374,#210375),
(#210376,#210377,#210378)),.UNSPECIFIED.,.F.,.F.,.F.)
B_SPLINE_SURFACE_WITH_KNOTS((4,2,4),(3,3),(-2.71050543121376E-20,0.000256915317531261,
0.000513830635062522),(0.,1.),.UNSPECIFIED.)
GEOMETRIC_REPRESENTATION_ITEM()
RATIONAL_B_SPLINE_SURFACE(((1.,0.705585838031456,1.),(1.,0.750902433542761,
1.),(1.,0.792329530082443,1.),(1.,0.854288401594255,1.),(1.,0.874998031125089,
1.),(1.,0.874619707139388,1.)))
REPRESENTATION_ITEM('')
SURFACE()
);
#3220=(
BOUNDED_SURFACE()
B_SPLINE_SURFACE(3,2,((#210384,#210385,#210386),(#210387,#210388,#210389),
(#210390,#210391,#210392),(#210393,#210394,#210395),(#210396,#210397,#210398),
(#210399,#210400,#210401)),.UNSPECIFIED.,.F.,.F.,.F.)
B_SPLINE_SURFACE_WITH_KNOTS((4,2,4),(3,3),(0.,0.000256592814262156,0.000513185628524312),
(0.,1.),.UNSPECIFIED.)
GEOMETRIC_REPRESENTATION_ITEM()
RATIONAL_B_SPLINE_SURFACE(((1.,0.70871252716368,1.),(1.,0.753780902613984,
1.),(1.,0.794538995768662,1.),(1.,0.855070770331644,1.),(1.,0.875018427444918,
1.),(1.,0.874619707139392,1.)))
REPRESENTATION_ITEM('')
SURFACE()
);
#3221=(
BOUNDED_SURFACE()
B_SPLINE_SURFACE(3,2,((#210403,#210404,#210405),(#210406,#210407,#210408),
(#210409,#210410,#210411),(#210412,#210413,#210414)),.UNSPECIFIED.,.F.,
 .F.,.F.)
B_SPLINE_SURFACE_WITH_KNOTS((4,4),(3,3),(0.,0.000511815072430398),(0.,1.00105598366037),
 .UNSPECIFIED.)
GEOMETRIC_REPRESENTATION_ITEM()
RATIONAL_B_SPLINE_SURFACE(((1.,0.706797490733248,1.00061923411793),(1.,
0.706182062146152,1.000620533883),(1.,0.705584062768531,1.00062179683814),
(1.,0.705266224770001,1.00062246810161)))
REPRESENTATION_ITEM('')
SURFACE()
);
#3222=(
BOUNDED_SURFACE()
B_SPLINE_SURFACE(3,2,((#210420,#210421,#210422),(#210423,#210424,#210425),
(#210426,#210427,#210428),(#210429,#210430,#210431),(#210432,#210433,#210434),
(#210435,#210436,#210437)),.UNSPECIFIED.,.F.,.F.,.F.)
B_SPLINE_SURFACE_WITH_KNOTS((4,2,4),(3,3),(-8.26704156520197E-19,0.000257652232350878,
0.000515304464701757),(0.,1.),.UNSPECIFIED.)
GEOMETRIC_REPRESENTATION_ITEM()
RATIONAL_B_SPLINE_SURFACE(((1.,0.87461970713939,1.),(1.,0.874861180431015,
1.),(1.,0.855455725920467,1.),(1.,0.794699358955663,1.),(1.,0.753768977788366,
1.),(1.,0.708712527163666,1.)))
REPRESENTATION_ITEM('')
SURFACE()
);
#3223=(
BOUNDED_SURFACE()
B_SPLINE_SURFACE(3,2,((#210443,#210444,#210445),(#210446,#210447,#210448),
(#210449,#210450,#210451),(#210452,#210453,#210454)),.UNSPECIFIED.,.F.,
 .F.,.F.)
B_SPLINE_SURFACE_WITH_KNOTS((4,4),(3,3),(0.,0.000397394373651932),(0.,1.),
 .UNSPECIFIED.)
GEOMETRIC_REPRESENTATION_ITEM()
RATIONAL_B_SPLINE_SURFACE(((1.,0.707106781186547,1.),(1.,0.707752587915898,
1.),(1.,0.708377654540681,1.),(1.,0.708689770883335,1.)))
REPRESENTATION_ITEM('')
SURFACE()
);
#3224=(
BOUNDED_SURFACE()
B_SPLINE_SURFACE(3,2,((#210456,#210457,#210458),(#210459,#210460,#210461),
(#210462,#210463,#210464),(#210465,#210466,#210467)),.UNSPECIFIED.,.F.,
 .F.,.F.)
B_SPLINE_SURFACE_WITH_KNOTS((4,4),(3,3),(0.,0.000511815456479785),(0.,1.00105873159947),
 .UNSPECIFIED.)
GEOMETRIC_REPRESENTATION_ITEM()
RATIONAL_B_SPLINE_SURFACE(((1.,0.708394529056471,1.00061746385333),(1.,
0.708058564167021,1.00061817524662),(1.,0.70743083537221,1.00061950443924),
(1.,0.70679668588052,1.00062084722745)))
REPRESENTATION_ITEM('')
SURFACE()
);
#3225=(
BOUNDED_SURFACE()
B_SPLINE_SURFACE(3,2,((#210473,#210474,#210475),(#210476,#210477,#210478),
(#210479,#210480,#210481),(#210482,#210483,#210484)),.UNSPECIFIED.,.F.,
 .F.,.F.)
B_SPLINE_SURFACE_WITH_KNOTS((4,4),(3,3),(0.,0.000397394465448308),(0.,1.),
 .UNSPECIFIED.)
GEOMETRIC_REPRESENTATION_ITEM()
RATIONAL_B_SPLINE_SURFACE(((1.,0.705498956110727,1.),(1.,0.705821764811783,
1.),(1.,0.706461952521138,1.),(1.,0.707106781186548,1.)))
REPRESENTATION_ITEM('')
SURFACE()
);
#3226=(
BOUNDED_SURFACE()
B_SPLINE_SURFACE(3,2,((#225174,#225175,#225176),(#225177,#225178,#225179),
(#225180,#225181,#225182),(#225183,#225184,#225185)),.UNSPECIFIED.,.F.,
 .F.,.F.)
B_SPLINE_SURFACE_WITH_KNOTS((4,4),(3,3),(0.,0.00039739441082874),(0.,1.),
 .UNSPECIFIED.)
GEOMETRIC_REPRESENTATION_ITEM()
RATIONAL_B_SPLINE_SURFACE(((1.,0.708689770883314,1.),(1.,0.708376440034511,
1.),(1.,0.707750498698406,1.),(1.,0.707106781186548,1.)))
REPRESENTATION_ITEM('')
SURFACE()
);
#3227=(
BOUNDED_SURFACE()
B_SPLINE_SURFACE(3,2,((#225191,#225192,#225193),(#225194,#225195,#225196),
(#225197,#225198,#225199),(#225200,#225201,#225202)),.UNSPECIFIED.,.F.,
 .F.,.F.)
B_SPLINE_SURFACE_WITH_KNOTS((4,4),(3,3),(0.,0.000511815090126175),(0.,1.00105592270397),
 .UNSPECIFIED.)
GEOMETRIC_REPRESENTATION_ITEM()
RATIONAL_B_SPLINE_SURFACE(((1.,0.705266242716963,1.00062243213188),(1.,
0.70558408590863,1.0006217608962),(1.,0.706182089449966,1.00062049800517),
(1.,0.706797508586963,1.00061919833509)))
REPRESENTATION_ITEM('')
SURFACE()
);
#3228=(
BOUNDED_SURFACE()
B_SPLINE_SURFACE(3,2,((#225204,#225205,#225206),(#225207,#225208,#225209),
(#225210,#225211,#225212),(#225213,#225214,#225215)),.UNSPECIFIED.,.F.,
 .F.,.F.)
B_SPLINE_SURFACE_WITH_KNOTS((4,4),(3,3),(-7.07441917546792E-18,0.000397394428086617),
(0.,1.),.UNSPECIFIED.)
GEOMETRIC_REPRESENTATION_ITEM()
RATIONAL_B_SPLINE_SURFACE(((1.,0.707106781186548,1.),(1.,0.706459846759103,
1.),(1.,0.705820510737259,1.),(1.,0.705498956110752,1.)))
REPRESENTATION_ITEM('')
SURFACE()
);
#3229=(
BOUNDED_SURFACE()
B_SPLINE_SURFACE(3,2,((#225221,#225222,#225223),(#225224,#225225,#225226),
(#225227,#225228,#225229),(#225230,#225231,#225232),(#225233,#225234,#225235),
(#225236,#225237,#225238)),.UNSPECIFIED.,.F.,.F.,.F.)
B_SPLINE_SURFACE_WITH_KNOTS((4,2,4),(3,3),(9.48676900924816E-20,0.000257953807872846,
0.000515907615745692),(0.,1.),.UNSPECIFIED.)
GEOMETRIC_REPRESENTATION_ITEM()
RATIONAL_B_SPLINE_SURFACE(((1.,0.874619707139395,1.),(1.,0.874834349678943,
1.),(1.,0.854686104157858,1.),(1.,0.79247659791508,1.),(1.,0.750887854595179,
1.),(1.,0.705585838031436,1.)))
REPRESENTATION_ITEM('')
SURFACE()
);
#3230=(
BOUNDED_SURFACE()
B_SPLINE_SURFACE(3,2,((#225244,#225245,#225246),(#225247,#225248,#225249),
(#225250,#225251,#225252),(#225253,#225254,#225255)),.UNSPECIFIED.,.F.,
 .F.,.F.)
B_SPLINE_SURFACE_WITH_KNOTS((4,4),(3,3),(0.,0.000511815437699145),(0.,1.00105881331503),
 .UNSPECIFIED.)
GEOMETRIC_REPRESENTATION_ITEM()
RATIONAL_B_SPLINE_SURFACE(((1.,0.706796661946587,1.00062089519668),(1.,
0.707430821225455,1.00061955228411),(1.,0.708058545830982,1.00061822299776),
(1.,0.708394505252967,1.00061751156115)))
REPRESENTATION_ITEM('')
SURFACE()
);
#3231=(
BOUNDED_SURFACE()
B_SPLINE_SURFACE(3,2,((#225257,#225258,#225259),(#225260,#225261,#225262),
(#225263,#225264,#225265),(#225266,#225267,#225268),(#225269,#225270,#225271),
(#225272,#225273,#225274)),.UNSPECIFIED.,.F.,.F.,.F.)
B_SPLINE_SURFACE_WITH_KNOTS((4,2,4),(3,3),(-1.62630325872826E-19,0.000256915317531258,
0.000513830635062517),(0.,1.),.UNSPECIFIED.)
GEOMETRIC_REPRESENTATION_ITEM()
RATIONAL_B_SPLINE_SURFACE(((1.,0.705585838031442,1.),(1.,0.750902433542864,
1.),(1.,0.792329530082365,1.),(1.,0.854288401594348,1.),(1.,0.874998031125021,
1.),(1.,0.874619707139395,1.)))
REPRESENTATION_ITEM('')
SURFACE()
);
#3232=(
BOUNDED_SURFACE()
B_SPLINE_SURFACE(3,2,((#225280,#225281,#225282),(#225283,#225284,#225285),
(#225286,#225287,#225288),(#225289,#225290,#225291),(#225292,#225293,#225294),
(#225295,#225296,#225297)),.UNSPECIFIED.,.F.,.F.,.F.)
B_SPLINE_SURFACE_WITH_KNOTS((4,2,4),(3,3),(-2.49366499671666E-18,0.000256592814262156,
0.000513185628524314),(0.,1.),.UNSPECIFIED.)
GEOMETRIC_REPRESENTATION_ITEM()
RATIONAL_B_SPLINE_SURFACE(((1.,0.708712527163662,1.),(1.,0.753780902613589,
1.),(1.,0.794538995769203,1.),(1.,0.855070770331116,1.),(1.,0.875018427445322,
1.),(1.,0.8746197071394,1.)))
REPRESENTATION_ITEM('')
SURFACE()
);
#3233=(
BOUNDED_SURFACE()
B_SPLINE_SURFACE(3,2,((#225299,#225300,#225301),(#225302,#225303,#225304),
(#225305,#225306,#225307),(#225308,#225309,#225310)),.UNSPECIFIED.,.F.,
 .F.,.F.)
B_SPLINE_SURFACE_WITH_KNOTS((4,4),(3,3),(2.71050543121376E-20,0.000511815072430401),
(0.,1.00105598366065),.UNSPECIFIED.)
GEOMETRIC_REPRESENTATION_ITEM()
RATIONAL_B_SPLINE_SURFACE(((1.,0.706797490733166,1.00061923411809),(1.,
0.706182062146078,1.00062053388316),(1.,0.705584062768454,1.0006217968383),
(1.,0.705266224769923,1.00062246810177)))
REPRESENTATION_ITEM('')
SURFACE()
);
#3234=(
BOUNDED_SURFACE()
B_SPLINE_SURFACE(3,2,((#225316,#225317,#225318),(#225319,#225320,#225321),
(#225322,#225323,#225324),(#225325,#225326,#225327),(#225328,#225329,#225330),
(#225331,#225332,#225333)),.UNSPECIFIED.,.F.,.F.,.F.)
B_SPLINE_SURFACE_WITH_KNOTS((4,2,4),(3,3),(-9.48676900924816E-20,0.00025765223235088,
0.000515304464701759),(0.,1.),.UNSPECIFIED.)
GEOMETRIC_REPRESENTATION_ITEM()
RATIONAL_B_SPLINE_SURFACE(((1.,0.874619707139394,1.),(1.,0.874861180430754,
1.),(1.,0.855455725920805,1.),(1.,0.794699358955339,1.),(1.,0.753768977788591,
1.),(1.,0.708712527163663,1.)))
REPRESENTATION_ITEM('')
SURFACE()
);
#3235=(
BOUNDED_SURFACE()
B_SPLINE_SURFACE(3,2,((#225339,#225340,#225341),(#225342,#225343,#225344),
(#225345,#225346,#225347),(#225348,#225349,#225350)),.UNSPECIFIED.,.F.,
 .F.,.F.)
B_SPLINE_SURFACE_WITH_KNOTS((4,4),(3,3),(0.,0.000397394373651912),(0.,1.),
 .UNSPECIFIED.)
GEOMETRIC_REPRESENTATION_ITEM()
RATIONAL_B_SPLINE_SURFACE(((1.,0.707106781186548,1.),(1.,0.707752587915877,
1.),(1.,0.708377654540693,1.),(1.,0.708689770883314,1.)))
REPRESENTATION_ITEM('')
SURFACE()
);
#3236=(
BOUNDED_SURFACE()
B_SPLINE_SURFACE(3,2,((#225352,#225353,#225354),(#225355,#225356,#225357),
(#225358,#225359,#225360),(#225361,#225362,#225363)),.UNSPECIFIED.,.F.,
 .F.,.F.)
B_SPLINE_SURFACE_WITH_KNOTS((4,4),(3,3),(-5.61074624261249E-18,0.000511815456479793),
(0.,1.00105873159934),.UNSPECIFIED.)
GEOMETRIC_REPRESENTATION_ITEM()
RATIONAL_B_SPLINE_SURFACE(((1.,0.708394529056523,1.00061746385326),(1.,
0.70805856416705,1.00061817524655),(1.,0.70743083537224,1.00061950443917),
(1.,0.706796685880558,1.00062084722738)))
REPRESENTATION_ITEM('')
SURFACE()
);
#3237=(
BOUNDED_SURFACE()
B_SPLINE_SURFACE(3,2,((#225369,#225370,#225371),(#225372,#225373,#225374),
(#225375,#225376,#225377),(#225378,#225379,#225380)),.UNSPECIFIED.,.F.,
 .F.,.F.)
B_SPLINE_SURFACE_WITH_KNOTS((4,4),(3,3),(0.,0.000397394465448316),(0.,1.),
 .UNSPECIFIED.)
GEOMETRIC_REPRESENTATION_ITEM()
RATIONAL_B_SPLINE_SURFACE(((1.,0.705498956110752,1.),(1.,0.705821764811793,
1.),(1.,0.70646195252114,1.),(1.,0.707106781186548,1.)))
REPRESENTATION_ITEM('')
SURFACE()
);
#3238=(
BOUNDED_SURFACE()
B_SPLINE_SURFACE(3,2,((#240891,#240892,#240893),(#240894,#240895,#240896),
(#240897,#240898,#240899),(#240900,#240901,#240902)),.UNSPECIFIED.,.F.,
 .F.,.F.)
B_SPLINE_SURFACE_WITH_KNOTS((4,4),(3,3),(-2.71050543121376E-20,0.000397394410828744),
(0.,1.),.UNSPECIFIED.)
GEOMETRIC_REPRESENTATION_ITEM()
RATIONAL_B_SPLINE_SURFACE(((1.,0.708689770883338,1.),(1.,0.708376440034495,
1.),(1.,0.707750498698416,1.),(1.,0.707106781186545,1.)))
REPRESENTATION_ITEM('')
SURFACE()
);
#3239=(
BOUNDED_SURFACE()
B_SPLINE_SURFACE(3,2,((#240908,#240909,#240910),(#240911,#240912,#240913),
(#240914,#240915,#240916),(#240917,#240918,#240919)),.UNSPECIFIED.,.F.,
 .F.,.F.)
B_SPLINE_SURFACE_WITH_KNOTS((4,4),(3,3),(2.71050543121376E-20,0.000511815090126173),
(0.,1.00105592270292),.UNSPECIFIED.)
GEOMETRIC_REPRESENTATION_ITEM()
RATIONAL_B_SPLINE_SURFACE(((1.,0.705266242717266,1.00062243213126),(1.,
0.705584085908932,1.00062176089558),(1.,0.706182089450283,1.00062049800455),
(1.,0.706797508587271,1.00061919833447)))
REPRESENTATION_ITEM('')
SURFACE()
);
#3240=(
BOUNDED_SURFACE()
B_SPLINE_SURFACE(3,2,((#240921,#240922,#240923),(#240924,#240925,#240926),
(#240927,#240928,#240929),(#240930,#240931,#240932)),.UNSPECIFIED.,.F.,
 .F.,.F.)
B_SPLINE_SURFACE_WITH_KNOTS((4,4),(3,3),(-8.13151629364128E-20,0.00039739442808662),
(0.,1.),.UNSPECIFIED.)
GEOMETRIC_REPRESENTATION_ITEM()
RATIONAL_B_SPLINE_SURFACE(((1.,0.70710678118655,1.),(1.,0.706459846759071,
1.),(1.,0.705820510737309,1.),(1.,0.705498956110743,1.)))
REPRESENTATION_ITEM('')
SURFACE()
);
#3241=(
BOUNDED_SURFACE()
B_SPLINE_SURFACE(3,2,((#240938,#240939,#240940),(#240941,#240942,#240943),
(#240944,#240945,#240946),(#240947,#240948,#240949),(#240950,#240951,#240952),
(#240953,#240954,#240955)),.UNSPECIFIED.,.F.,.F.,.F.)
B_SPLINE_SURFACE_WITH_KNOTS((4,2,4),(3,3),(0.,0.00025795380787285,0.0005159076157457),
(0.,1.),.UNSPECIFIED.)
GEOMETRIC_REPRESENTATION_ITEM()
RATIONAL_B_SPLINE_SURFACE(((1.,0.87461970713939,1.),(1.,0.874834349679194,
1.),(1.,0.854686104157516,1.),(1.,0.792476597915439,1.),(1.,0.750887854594908,
1.),(1.,0.705585838031442,1.)))
REPRESENTATION_ITEM('')
SURFACE()
);
#3242=(
BOUNDED_SURFACE()
B_SPLINE_SURFACE(3,2,((#240961,#240962,#240963),(#240964,#240965,#240966),
(#240967,#240968,#240969),(#240970,#240971,#240972)),.UNSPECIFIED.,.F.,
 .F.,.F.)
B_SPLINE_SURFACE_WITH_KNOTS((4,4),(3,3),(8.13151629364128E-20,0.000511815437699155),
(0.,1.001058813318),.UNSPECIFIED.)
GEOMETRIC_REPRESENTATION_ITEM()
RATIONAL_B_SPLINE_SURFACE(((1.,0.706796661945717,1.00062089519843),(1.,
0.707430821224596,1.00061955228585),(1.,0.708058545830099,1.0006182229995),
(1.,0.708394505252105,1.00061751156288)))
REPRESENTATION_ITEM('')
SURFACE()
);
#3243=(
BOUNDED_SURFACE()
B_SPLINE_SURFACE(3,2,((#240974,#240975,#240976),(#240977,#240978,#240979),
(#240980,#240981,#240982),(#240983,#240984,#240985),(#240986,#240987,#240988),
(#240989,#240990,#240991)),.UNSPECIFIED.,.F.,.F.,.F.)
B_SPLINE_SURFACE_WITH_KNOTS((4,2,4),(3,3),(-1.0842021724855E-19,0.000256915317531264,
0.000513830635062529),(0.,1.),.UNSPECIFIED.)
GEOMETRIC_REPRESENTATION_ITEM()
RATIONAL_B_SPLINE_SURFACE(((1.,0.705585838031443,1.),(1.,0.750902433543475,
1.),(1.,0.792329530081552,1.),(1.,0.85428840159518,1.),(1.,0.874998031124423,
1.),(1.,0.87461970713939,1.)))
REPRESENTATION_ITEM('')
SURFACE()
);
#3244=(
BOUNDED_SURFACE()
B_SPLINE_SURFACE(3,2,((#240997,#240998,#240999),(#241000,#241001,#241002),
(#241003,#241004,#241005),(#241006,#241007,#241008),(#241009,#241010,#241011),
(#241012,#241013,#241014)),.UNSPECIFIED.,.F.,.F.,.F.)
B_SPLINE_SURFACE_WITH_KNOTS((4,2,4),(3,3),(1.0842021724855E-19,0.000256592814262158,
0.000513185628524316),(0.,1.),.UNSPECIFIED.)
GEOMETRIC_REPRESENTATION_ITEM()
RATIONAL_B_SPLINE_SURFACE(((1.,0.708712527163671,1.),(1.,0.753780902613763,
1.),(1.,0.794538995768961,1.),(1.,0.855070770331352,1.),(1.,0.875018427445139,
1.),(1.,0.874619707139394,1.)))
REPRESENTATION_ITEM('')
SURFACE()
);
#3245=(
BOUNDED_SURFACE()
B_SPLINE_SURFACE(3,2,((#241016,#241017,#241018),(#241019,#241020,#241021),
(#241022,#241023,#241024),(#241025,#241026,#241027)),.UNSPECIFIED.,.F.,
 .F.,.F.)
B_SPLINE_SURFACE_WITH_KNOTS((4,4),(3,3),(4.87890977618477E-19,0.000511815072430394),
(0.,1.00105598365812),.UNSPECIFIED.)
GEOMETRIC_REPRESENTATION_ITEM()
RATIONAL_B_SPLINE_SURFACE(((1.,0.706797490733907,1.00061923411661),(1.,
0.706182062146832,1.00062053388167),(1.,0.705584062769189,1.00062179683681),
(1.,0.705266224770674,1.00062246810027)))
REPRESENTATION_ITEM('')
SURFACE()
);
#3246=(
BOUNDED_SURFACE()
B_SPLINE_SURFACE(3,2,((#241033,#241034,#241035),(#241036,#241037,#241038),
(#241039,#241040,#241041),(#241042,#241043,#241044),(#241045,#241046,#241047),
(#241048,#241049,#241050)),.UNSPECIFIED.,.F.,.F.,.F.)
B_SPLINE_SURFACE_WITH_KNOTS((4,2,4),(3,3),(1.35525271560688E-20,0.000257652232350882,
0.000515304464701764),(0.,1.),.UNSPECIFIED.)
GEOMETRIC_REPRESENTATION_ITEM()
RATIONAL_B_SPLINE_SURFACE(((1.,0.874619707139383,1.),(1.,0.874861180430713,
1.),(1.,0.85545572592086,1.),(1.,0.794699358955259,1.),(1.,0.753768977788642,
1.),(1.,0.708712527163656,1.)))
REPRESENTATION_ITEM('')
SURFACE()
);
#3247=(
BOUNDED_SURFACE()
B_SPLINE_SURFACE(3,2,((#241056,#241057,#241058),(#241059,#241060,#241061),
(#241062,#241063,#241064),(#241065,#241066,#241067)),.UNSPECIFIED.,.F.,
 .F.,.F.)
B_SPLINE_SURFACE_WITH_KNOTS((4,4),(3,3),(8.13151629364128E-20,0.000397394373651917),
(0.,1.),.UNSPECIFIED.)
GEOMETRIC_REPRESENTATION_ITEM()
RATIONAL_B_SPLINE_SURFACE(((1.,0.707106781186548,1.),(1.,0.707752587915901,
1.),(1.,0.708377654540656,1.),(1.,0.708689770883324,1.)))
REPRESENTATION_ITEM('')
SURFACE()
);
#3248=(
BOUNDED_SURFACE()
B_SPLINE_SURFACE(3,2,((#241069,#241070,#241071),(#241072,#241073,#241074),
(#241075,#241076,#241077),(#241078,#241079,#241080)),.UNSPECIFIED.,.F.,
 .F.,.F.)
B_SPLINE_SURFACE_WITH_KNOTS((4,4),(3,3),(-2.71050543121376E-20,0.000511815456479787),
(0.,1.00105873159928),.UNSPECIFIED.)
GEOMETRIC_REPRESENTATION_ITEM()
RATIONAL_B_SPLINE_SURFACE(((1.,0.708394529056518,1.00061746385322),(1.,
0.708058564167046,1.00061817524651),(1.,0.707430835372269,1.00061950443913),
(1.,0.706796685880576,1.00062084722735)))
REPRESENTATION_ITEM('')
SURFACE()
);
#3249=(
BOUNDED_SURFACE()
B_SPLINE_SURFACE(3,2,((#241086,#241087,#241088),(#241089,#241090,#241091),
(#241092,#241093,#241094),(#241095,#241096,#241097)),.UNSPECIFIED.,.F.,
 .F.,.F.)
B_SPLINE_SURFACE_WITH_KNOTS((4,4),(3,3),(2.71050543121376E-20,0.000397394465448306),
(0.,1.),.UNSPECIFIED.)
GEOMETRIC_REPRESENTATION_ITEM()
RATIONAL_B_SPLINE_SURFACE(((1.,0.705498956110759,1.),(1.,0.70582176481179,
1.),(1.,0.706461952521145,1.),(1.,0.707106781186548,1.)))
REPRESENTATION_ITEM('')
SURFACE()
);
#3250=(
BOUNDED_SURFACE()
B_SPLINE_SURFACE(3,2,((#241103,#241104,#241105),(#241106,#241107,#241108),
(#241109,#241110,#241111),(#241112,#241113,#241114)),.UNSPECIFIED.,.F.,
 .F.,.F.)
B_SPLINE_SURFACE_WITH_KNOTS((4,4),(3,3),(0.,0.000397394410828732),(0.,1.),
 .UNSPECIFIED.)
GEOMETRIC_REPRESENTATION_ITEM()
RATIONAL_B_SPLINE_SURFACE(((1.,0.708689770883319,1.),(1.,0.70837644003452,
1.),(1.,0.70775049869839,1.),(1.,0.70710678118655,1.)))
REPRESENTATION_ITEM('')
SURFACE()
);
#3251=(
BOUNDED_SURFACE()
B_SPLINE_SURFACE(3,2,((#241120,#241121,#241122),(#241123,#241124,#241125),
(#241126,#241127,#241128),(#241129,#241130,#241131)),.UNSPECIFIED.,.F.,
 .F.,.F.)
B_SPLINE_SURFACE_WITH_KNOTS((4,4),(3,3),(1.35525271560688E-19,0.000511815090126187),
(0.,1.00105592270021),.UNSPECIFIED.)
GEOMETRIC_REPRESENTATION_ITEM()
RATIONAL_B_SPLINE_SURFACE(((1.,0.705266242718048,1.00062243212966),(1.,
0.705584085909746,1.00062176089398),(1.,0.706182089451072,1.00062049800295),
(1.,0.706797508588059,1.00061919833288)))
REPRESENTATION_ITEM('')
SURFACE()
);
#3252=(
BOUNDED_SURFACE()
B_SPLINE_SURFACE(3,2,((#241133,#241134,#241135),(#241136,#241137,#241138),
(#241139,#241140,#241141),(#241142,#241143,#241144)),.UNSPECIFIED.,.F.,
 .F.,.F.)
B_SPLINE_SURFACE_WITH_KNOTS((4,4),(3,3),(0.,0.000397394428086623),(0.,1.),
 .UNSPECIFIED.)
GEOMETRIC_REPRESENTATION_ITEM()
RATIONAL_B_SPLINE_SURFACE(((1.,0.707106781186546,1.),(1.,0.706459846759076,
1.),(1.,0.705820510737292,1.),(1.,0.705498956110753,1.)))
REPRESENTATION_ITEM('')
SURFACE()
);
#3253=(
BOUNDED_SURFACE()
B_SPLINE_SURFACE(3,2,((#241150,#241151,#241152),(#241153,#241154,#241155),
(#241156,#241157,#241158),(#241159,#241160,#241161),(#241162,#241163,#241164),
(#241165,#241166,#241167)),.UNSPECIFIED.,.F.,.F.,.F.)
B_SPLINE_SURFACE_WITH_KNOTS((4,2,4),(3,3),(0.,0.000257953807872846,0.000515907615745692),
(0.,1.),.UNSPECIFIED.)
GEOMETRIC_REPRESENTATION_ITEM()
RATIONAL_B_SPLINE_SURFACE(((1.,0.874619707139395,1.),(1.,0.874834349679043,
1.),(1.,0.854686104157736,1.),(1.,0.792476597915218,1.),(1.,0.750887854595055,
1.),(1.,0.705585838031455,1.)))
REPRESENTATION_ITEM('')
SURFACE()
);
#3254=(
BOUNDED_SURFACE()
B_SPLINE_SURFACE(3,2,((#241173,#241174,#241175),(#241176,#241177,#241178),
(#241179,#241180,#241181),(#241182,#241183,#241184)),.UNSPECIFIED.,.F.,
 .F.,.F.)
B_SPLINE_SURFACE_WITH_KNOTS((4,4),(3,3),(0.,0.000511815437699164),(0.,1.00105881331854),
 .UNSPECIFIED.)
GEOMETRIC_REPRESENTATION_ITEM()
RATIONAL_B_SPLINE_SURFACE(((1.,0.706796661945554,1.00062089519875),(1.,
0.707430821224427,1.00061955228617),(1.,0.708058545829957,1.00061822299982),
(1.,0.708394505251943,1.0006175115632)))
REPRESENTATION_ITEM('')
SURFACE()
);
#3255=(
BOUNDED_SURFACE()
B_SPLINE_SURFACE(3,2,((#241186,#241187,#241188),(#241189,#241190,#241191),
(#241192,#241193,#241194),(#241195,#241196,#241197),(#241198,#241199,#241200),
(#241201,#241202,#241203)),.UNSPECIFIED.,.F.,.F.,.F.)
B_SPLINE_SURFACE_WITH_KNOTS((4,2,4),(3,3),(0.,0.000256915317531264,0.000513830635062528),
(0.,1.),.UNSPECIFIED.)
GEOMETRIC_REPRESENTATION_ITEM()
RATIONAL_B_SPLINE_SURFACE(((1.,0.70558583803145,1.),(1.,0.75090243354219,
1.),(1.,0.792329530083307,1.),(1.,0.854288401593428,1.),(1.,0.874998031125737,
1.),(1.,0.874619707139414,1.)))
REPRESENTATION_ITEM('')
SURFACE()
);
#3256=(
BOUNDED_SURFACE()
B_SPLINE_SURFACE(3,2,((#241209,#241210,#241211),(#241212,#241213,#241214),
(#241215,#241216,#241217),(#241218,#241219,#241220),(#241221,#241222,#241223),
(#241224,#241225,#241226)),.UNSPECIFIED.,.F.,.F.,.F.)
B_SPLINE_SURFACE_WITH_KNOTS((4,2,4),(3,3),(0.,0.000256592814262154,0.000513185628524309),
(0.,1.),.UNSPECIFIED.)
GEOMETRIC_REPRESENTATION_ITEM()
RATIONAL_B_SPLINE_SURFACE(((1.,0.708712527163678,1.),(1.,0.753780902613434,
1.),(1.,0.794538995769399,1.),(1.,0.855070770330911,1.),(1.,0.875018427445479,
1.),(1.,0.874619707139399,1.)))
REPRESENTATION_ITEM('')
SURFACE()
);
#3257=(
BOUNDED_SURFACE()
B_SPLINE_SURFACE(3,2,((#241228,#241229,#241230),(#241231,#241232,#241233),
(#241234,#241235,#241236),(#241237,#241238,#241239)),.UNSPECIFIED.,.F.,
 .F.,.F.)
B_SPLINE_SURFACE_WITH_KNOTS((4,4),(3,3),(0.,0.000511815072430392),(0.,1.00105598365858),
 .UNSPECIFIED.)
GEOMETRIC_REPRESENTATION_ITEM()
RATIONAL_B_SPLINE_SURFACE(((1.,0.70679749073377,1.00061923411688),(1.,0.706182062146689,
1.00062053388194),(1.,0.705584062769055,1.00062179683708),(1.,0.705266224770533,
1.00062246810055)))
REPRESENTATION_ITEM('')
SURFACE()
);
#3258=(
BOUNDED_SURFACE()
B_SPLINE_SURFACE(3,2,((#241245,#241246,#241247),(#241248,#241249,#241250),
(#241251,#241252,#241253),(#241254,#241255,#241256),(#241257,#241258,#241259),
(#241260,#241261,#241262)),.UNSPECIFIED.,.F.,.F.,.F.)
B_SPLINE_SURFACE_WITH_KNOTS((4,2,4),(3,3),(-1.76182853028894E-18,0.000257652232350886,
0.000515304464701773),(0.,1.),.UNSPECIFIED.)
GEOMETRIC_REPRESENTATION_ITEM()
RATIONAL_B_SPLINE_SURFACE(((1.,0.87461970713938,1.),(1.,0.874861180430654,
1.),(1.,0.855455725920906,1.),(1.,0.794699358955208,1.),(1.,0.75376897778866,
1.),(1.,0.708712527163654,1.)))
REPRESENTATION_ITEM('')
SURFACE()
);
#3259=(
BOUNDED_SURFACE()
B_SPLINE_SURFACE(3,2,((#241268,#241269,#241270),(#241271,#241272,#241273),
(#241274,#241275,#241276),(#241277,#241278,#241279)),.UNSPECIFIED.,.F.,
 .F.,.F.)
B_SPLINE_SURFACE_WITH_KNOTS((4,4),(3,3),(-7.23704950134074E-18,0.000397394373651904),
(0.,1.),.UNSPECIFIED.)
GEOMETRIC_REPRESENTATION_ITEM()
RATIONAL_B_SPLINE_SURFACE(((1.,0.707106781186554,1.),(1.,0.707752587915903,
1.),(1.,0.708377654540659,1.),(1.,0.70868977088333,1.)))
REPRESENTATION_ITEM('')
SURFACE()
);
#3260=(
BOUNDED_SURFACE()
B_SPLINE_SURFACE(3,2,((#241281,#241282,#241283),(#241284,#241285,#241286),
(#241287,#241288,#241289),(#241290,#241291,#241292)),.UNSPECIFIED.,.F.,
 .F.,.F.)
B_SPLINE_SURFACE_WITH_KNOTS((4,4),(3,3),(-1.35525271560688E-19,0.000511815456479788),
(0.,1.00105873159961),.UNSPECIFIED.)
GEOMETRIC_REPRESENTATION_ITEM()
RATIONAL_B_SPLINE_SURFACE(((1.,0.708394529056427,1.00061746385341),(1.,
0.708058564166958,1.0006181752467),(1.,0.707430835372167,1.00061950443932),
(1.,0.706796685880481,1.00062084722754)))
REPRESENTATION_ITEM('')
SURFACE()
);
#3261=(
BOUNDED_SURFACE()
B_SPLINE_SURFACE(3,2,((#241298,#241299,#241300),(#241301,#241302,#241303),
(#241304,#241305,#241306),(#241307,#241308,#241309)),.UNSPECIFIED.,.F.,
 .F.,.F.)
B_SPLINE_SURFACE_WITH_KNOTS((4,4),(3,3),(-2.46655994240452E-18,0.000397394465448289),
(0.,1.),.UNSPECIFIED.)
GEOMETRIC_REPRESENTATION_ITEM()
RATIONAL_B_SPLINE_SURFACE(((1.,0.705498956110751,1.),(1.,0.705821764811789,
1.),(1.,0.706461952521142,1.),(1.,0.707106781186545,1.)))
REPRESENTATION_ITEM('')
SURFACE()
);
#3262=(
BOUNDED_SURFACE()
B_SPLINE_SURFACE(3,2,((#241315,#241316,#241317),(#241318,#241319,#241320),
(#241321,#241322,#241323),(#241324,#241325,#241326)),.UNSPECIFIED.,.F.,
 .F.,.F.)
B_SPLINE_SURFACE_WITH_KNOTS((4,4),(3,3),(-3.79470760369927E-19,0.000397394410828735),
(0.,1.),.UNSPECIFIED.)
GEOMETRIC_REPRESENTATION_ITEM()
RATIONAL_B_SPLINE_SURFACE(((1.,0.708689770883326,1.),(1.,0.708376440034481,
1.),(1.,0.707750498698415,1.),(1.,0.707106781186545,1.)))
REPRESENTATION_ITEM('')
SURFACE()
);
#3263=(
BOUNDED_SURFACE()
B_SPLINE_SURFACE(3,2,((#241332,#241333,#241334),(#241335,#241336,#241337),
(#241338,#241339,#241340),(#241341,#241342,#241343)),.UNSPECIFIED.,.F.,
 .F.,.F.)
B_SPLINE_SURFACE_WITH_KNOTS((4,4),(3,3),(0.,0.000511815090126178),(0.,1.00105592270117),
 .UNSPECIFIED.)
GEOMETRIC_REPRESENTATION_ITEM()
RATIONAL_B_SPLINE_SURFACE(((1.,0.705266242717812,1.00062243213023),(1.,
0.705584085909414,1.00062176089455),(1.,0.706182089450808,1.00062049800352),
(1.,0.70679750858778,1.00061919833345)))
REPRESENTATION_ITEM('')
SURFACE()
);
#3264=(
BOUNDED_SURFACE()
B_SPLINE_SURFACE(3,2,((#241345,#241346,#241347),(#241348,#241349,#241350),
(#241351,#241352,#241353),(#241354,#241355,#241356)),.UNSPECIFIED.,.F.,
 .F.,.F.)
B_SPLINE_SURFACE_WITH_KNOTS((4,4),(3,3),(-7.77915058758349E-18,0.000397394428086625),
(0.,1.),.UNSPECIFIED.)
GEOMETRIC_REPRESENTATION_ITEM()
RATIONAL_B_SPLINE_SURFACE(((1.,0.707106781186545,1.),(1.,0.706459846759091,
1.),(1.,0.705820510737286,1.),(1.,0.705498956110761,1.)))
REPRESENTATION_ITEM('')
SURFACE()
);
#3265=(
BOUNDED_SURFACE()
B_SPLINE_SURFACE(3,2,((#241362,#241363,#241364),(#241365,#241366,#241367),
(#241368,#241369,#241370),(#241371,#241372,#241373),(#241374,#241375,#241376),
(#241377,#241378,#241379)),.UNSPECIFIED.,.F.,.F.,.F.)
B_SPLINE_SURFACE_WITH_KNOTS((4,2,4),(3,3),(0.,0.000257953807872846,0.000515907615745691),
(0.,1.),.UNSPECIFIED.)
GEOMETRIC_REPRESENTATION_ITEM()
RATIONAL_B_SPLINE_SURFACE(((1.,0.874619707139396,1.),(1.,0.874834349678915,
1.),(1.,0.85468610415791,1.),(1.,0.792476597915036,1.),(1.,0.750887854595192,
1.),(1.,0.705585838031471,1.)))
REPRESENTATION_ITEM('')
SURFACE()
);
#3266=(
BOUNDED_SURFACE()
B_SPLINE_SURFACE(3,2,((#241385,#241386,#241387),(#241388,#241389,#241390),
(#241391,#241392,#241393),(#241394,#241395,#241396)),.UNSPECIFIED.,.F.,
 .F.,.F.)
B_SPLINE_SURFACE_WITH_KNOTS((4,4),(3,3),(-7.80625564189563E-18,0.00051181543769914),
(0.,1.00105881331477),.UNSPECIFIED.)
GEOMETRIC_REPRESENTATION_ITEM()
RATIONAL_B_SPLINE_SURFACE(((1.,0.706796661946661,1.00062089519653),(1.,
0.707430821225544,1.00061955228395),(1.,0.708058545831046,1.00061822299761),
(1.,0.708394505253034,1.00061751156099)))
REPRESENTATION_ITEM('')
SURFACE()
);
#3267=(
BOUNDED_SURFACE()
B_SPLINE_SURFACE(3,2,((#241398,#241399,#241400),(#241401,#241402,#241403),
(#241404,#241405,#241406),(#241407,#241408,#241409),(#241410,#241411,#241412),
(#241413,#241414,#241415)),.UNSPECIFIED.,.F.,.F.,.F.)
B_SPLINE_SURFACE_WITH_KNOTS((4,2,4),(3,3),(-2.71050543121376E-20,0.000256915317531264,
0.000513830635062527),(0.,1.),.UNSPECIFIED.)
GEOMETRIC_REPRESENTATION_ITEM()
RATIONAL_B_SPLINE_SURFACE(((1.,0.705585838031459,1.),(1.,0.750902433542926,
1.),(1.,0.792329530082281,1.),(1.,0.854288401594456,1.),(1.,0.874998031124951,
1.),(1.,0.874619707139397,1.)))
REPRESENTATION_ITEM('')
SURFACE()
);
#3268=(
BOUNDED_SURFACE()
B_SPLINE_SURFACE(3,2,((#241421,#241422,#241423),(#241424,#241425,#241426),
(#241427,#241428,#241429),(#241430,#241431,#241432),(#241433,#241434,#241435),
(#241436,#241437,#241438)),.UNSPECIFIED.,.F.,.F.,.F.)
B_SPLINE_SURFACE_WITH_KNOTS((4,2,4),(3,3),(-1.02999206386123E-17,0.000256592814262153,
0.000513185628524316),(0.,1.),.UNSPECIFIED.)
GEOMETRIC_REPRESENTATION_ITEM()
RATIONAL_B_SPLINE_SURFACE(((1.,0.708712527163656,1.),(1.,0.75378090261397,
1.),(1.,0.794538995768696,1.),(1.,0.855070770331603,1.),(1.,0.875018427444962,
1.),(1.,0.874619707139397,1.)))
REPRESENTATION_ITEM('')
SURFACE()
);
#3269=(
BOUNDED_SURFACE()
B_SPLINE_SURFACE(3,2,((#241440,#241441,#241442),(#241443,#241444,#241445),
(#241446,#241447,#241448),(#241449,#241450,#241451)),.UNSPECIFIED.,.F.,
 .F.,.F.)
B_SPLINE_SURFACE_WITH_KNOTS((4,4),(3,3),(2.71050543121376E-20,0.000511815072430401),
(0.,1.00105598365924),.UNSPECIFIED.)
GEOMETRIC_REPRESENTATION_ITEM()
RATIONAL_B_SPLINE_SURFACE(((1.,0.706797490733581,1.00061923411727),(1.,
0.706182062146486,1.00062053388233),(1.,0.70558406276887,1.00062179683747),
(1.,0.705266224770332,1.00062246810094)))
REPRESENTATION_ITEM('')
SURFACE()
);
#3270=(
BOUNDED_SURFACE()
B_SPLINE_SURFACE(3,2,((#241457,#241458,#241459),(#241460,#241461,#241462),
(#241463,#241464,#241465),(#241466,#241467,#241468),(#241469,#241470,#241471),
(#241472,#241473,#241474)),.UNSPECIFIED.,.F.,.F.,.F.)
B_SPLINE_SURFACE_WITH_KNOTS((4,2,4),(3,3),(-3.48299947910968E-18,0.000257652232350876,
0.000515304464701756),(0.,1.),.UNSPECIFIED.)
GEOMETRIC_REPRESENTATION_ITEM()
RATIONAL_B_SPLINE_SURFACE(((1.,0.874619707139392,1.),(1.,0.874861180430568,
1.),(1.,0.85545572592103,1.),(1.,0.794699358955112,1.),(1.,0.753768977788717,
1.),(1.,0.708712527163672,1.)))
REPRESENTATION_ITEM('')
SURFACE()
);
#3271=(
BOUNDED_SURFACE()
B_SPLINE_SURFACE(3,2,((#241480,#241481,#241482),(#241483,#241484,#241485),
(#241486,#241487,#241488),(#241489,#241490,#241491)),.UNSPECIFIED.,.F.,
 .F.,.F.)
B_SPLINE_SURFACE_WITH_KNOTS((4,4),(3,3),(0.,0.000397394373651928),(0.,1.),
 .UNSPECIFIED.)
GEOMETRIC_REPRESENTATION_ITEM()
RATIONAL_B_SPLINE_SURFACE(((1.,0.707106781186544,1.),(1.,0.707752587915889,
1.),(1.,0.708377654540682,1.),(1.,0.708689770883336,1.)))
REPRESENTATION_ITEM('')
SURFACE()
);
#3272=(
BOUNDED_SURFACE()
B_SPLINE_SURFACE(3,2,((#241493,#241494,#241495),(#241496,#241497,#241498),
(#241499,#241500,#241501),(#241502,#241503,#241504)),.UNSPECIFIED.,.F.,
 .F.,.F.)
B_SPLINE_SURFACE_WITH_KNOTS((4,4),(3,3),(0.,0.000511815456479792),(0.,1.00105873159925),
 .UNSPECIFIED.)
GEOMETRIC_REPRESENTATION_ITEM()
RATIONAL_B_SPLINE_SURFACE(((1.,0.708394529056543,1.0006174638532),(1.,0.708058564167093,
1.00061817524649),(1.,0.707430835372262,1.00061950443911),(1.,0.706796685880581,
1.00062084722733)))
REPRESENTATION_ITEM('')
SURFACE()
);
#3273=(
BOUNDED_SURFACE()
B_SPLINE_SURFACE(3,2,((#241510,#241511,#241512),(#241513,#241514,#241515),
(#241516,#241517,#241518),(#241519,#241520,#241521)),.UNSPECIFIED.,.F.,
 .F.,.F.)
B_SPLINE_SURFACE_WITH_KNOTS((4,4),(3,3),(3.79470760369927E-19,0.00039739446544831),
(0.,1.),.UNSPECIFIED.)
GEOMETRIC_REPRESENTATION_ITEM()
RATIONAL_B_SPLINE_SURFACE(((1.,0.705498956110749,1.),(1.,0.705821764811784,
1.),(1.,0.70646195252114,1.),(1.,0.707106781186547,1.)))
REPRESENTATION_ITEM('')
SURFACE()
);
#3274=(
BOUNDED_SURFACE()
B_SPLINE_SURFACE(3,2,((#241527,#241528,#241529),(#241530,#241531,#241532),
(#241533,#241534,#241535),(#241536,#241537,#241538)),.UNSPECIFIED.,.F.,
 .F.,.F.)
B_SPLINE_SURFACE_WITH_KNOTS((4,4),(3,3),(-4.87890977618477E-19,0.000397394410828753),
(0.,1.),.UNSPECIFIED.)
GEOMETRIC_REPRESENTATION_ITEM()
RATIONAL_B_SPLINE_SURFACE(((1.,0.708689770883332,1.),(1.,0.70837644003451,
1.),(1.,0.70775049869839,1.),(1.,0.707106781186553,1.)))
REPRESENTATION_ITEM('')
SURFACE()
);
#3275=(
BOUNDED_SURFACE()
B_SPLINE_SURFACE(3,2,((#241544,#241545,#241546),(#241547,#241548,#241549),
(#241550,#241551,#241552),(#241553,#241554,#241555)),.UNSPECIFIED.,.F.,
 .F.,.F.)
B_SPLINE_SURFACE_WITH_KNOTS((4,4),(3,3),(-3.22550146314438E-18,0.000511815090126175),
(0.,1.00105592270393),.UNSPECIFIED.)
GEOMETRIC_REPRESENTATION_ITEM()
RATIONAL_B_SPLINE_SURFACE(((1.,0.705266242717003,1.00062243213186),(1.,
0.705584085908612,1.00062176089618),(1.,0.706182089449985,1.00062049800514),
(1.,0.706797508586972,1.00061919833506)))
REPRESENTATION_ITEM('')
SURFACE()
);
#3276=(
BOUNDED_SURFACE()
B_SPLINE_SURFACE(3,2,((#241557,#241558,#241559),(#241560,#241561,#241562),
(#241563,#241564,#241565),(#241566,#241567,#241568)),.UNSPECIFIED.,.F.,
 .F.,.F.)
B_SPLINE_SURFACE_WITH_KNOTS((4,4),(3,3),(0.,0.000397394428086626),(0.,1.),
 .UNSPECIFIED.)
GEOMETRIC_REPRESENTATION_ITEM()
RATIONAL_B_SPLINE_SURFACE(((1.,0.707106781186545,1.),(1.,0.706459846759104,
1.),(1.,0.705820510737273,1.),(1.,0.705498956110752,1.)))
REPRESENTATION_ITEM('')
SURFACE()
);
#3277=(
BOUNDED_SURFACE()
B_SPLINE_SURFACE(3,2,((#241574,#241575,#241576),(#241577,#241578,#241579),
(#241580,#241581,#241582),(#241583,#241584,#241585),(#241586,#241587,#241588),
(#241589,#241590,#241591)),.UNSPECIFIED.,.F.,.F.,.F.)
B_SPLINE_SURFACE_WITH_KNOTS((4,2,4),(3,3),(0.,0.000257953807872851,0.000515907615745702),
(0.,1.),.UNSPECIFIED.)
GEOMETRIC_REPRESENTATION_ITEM()
RATIONAL_B_SPLINE_SURFACE(((1.,0.874619707139392,1.),(1.,0.874834349678881,
1.),(1.,0.85468610415795,1.),(1.,0.792476597914979,1.),(1.,0.750887854595268,
1.),(1.,0.705585838031435,1.)))
REPRESENTATION_ITEM('')
SURFACE()
);
#3278=(
BOUNDED_SURFACE()
B_SPLINE_SURFACE(3,2,((#241597,#241598,#241599),(#241600,#241601,#241602),
(#241603,#241604,#241605),(#241606,#241607,#241608)),.UNSPECIFIED.,.F.,
 .F.,.F.)
B_SPLINE_SURFACE_WITH_KNOTS((4,4),(3,3),(0.,0.000511815437699157),(0.,1.00105881331701),
 .UNSPECIFIED.)
GEOMETRIC_REPRESENTATION_ITEM()
RATIONAL_B_SPLINE_SURFACE(((1.,0.706796661946011,1.00062089519785),(1.,
0.707430821224864,1.00061955228527),(1.,0.708058545830404,1.00061822299893),
(1.,0.708394505252382,1.00061751156231)))
REPRESENTATION_ITEM('')
SURFACE()
);
#3279=(
BOUNDED_SURFACE()
B_SPLINE_SURFACE(3,2,((#241610,#241611,#241612),(#241613,#241614,#241615),
(#241616,#241617,#241618),(#241619,#241620,#241621),(#241622,#241623,#241624),
(#241625,#241626,#241627)),.UNSPECIFIED.,.F.,.F.,.F.)
B_SPLINE_SURFACE_WITH_KNOTS((4,2,4),(3,3),(1.62630325872826E-19,0.000256915317531262,
0.000513830635062524),(0.,1.),.UNSPECIFIED.)
GEOMETRIC_REPRESENTATION_ITEM()
RATIONAL_B_SPLINE_SURFACE(((1.,0.705585838031439,1.),(1.,0.750902433542569,
1.),(1.,0.792329530082738,1.),(1.,0.854288401593987,1.),(1.,0.874998031125295,
1.),(1.,0.8746197071394,1.)))
REPRESENTATION_ITEM('')
SURFACE()
);
#3280=(
BOUNDED_SURFACE()
B_SPLINE_SURFACE(3,2,((#241633,#241634,#241635),(#241636,#241637,#241638),
(#241639,#241640,#241641),(#241642,#241643,#241644),(#241645,#241646,#241647),
(#241648,#241649,#241650)),.UNSPECIFIED.,.F.,.F.,.F.)
B_SPLINE_SURFACE_WITH_KNOTS((4,2,4),(3,3),(-3.03576608295941E-18,0.000256592814262156,
0.000513185628524315),(0.,1.),.UNSPECIFIED.)
GEOMETRIC_REPRESENTATION_ITEM()
RATIONAL_B_SPLINE_SURFACE(((1.,0.708712527163661,1.),(1.,0.753780902613533,
1.),(1.,0.794538995769294,1.),(1.,0.855070770331017,1.),(1.,0.875018427445396,
1.),(1.,0.874619707139393,1.)))
REPRESENTATION_ITEM('')
SURFACE()
);
#3281=(
BOUNDED_SURFACE()
B_SPLINE_SURFACE(3,2,((#241652,#241653,#241654),(#241655,#241656,#241657),
(#241658,#241659,#241660),(#241661,#241662,#241663)),.UNSPECIFIED.,.F.,
 .F.,.F.)
B_SPLINE_SURFACE_WITH_KNOTS((4,4),(3,3),(0.,0.000511815072430393),(0.,1.00105598365816),
 .UNSPECIFIED.)
GEOMETRIC_REPRESENTATION_ITEM()
RATIONAL_B_SPLINE_SURFACE(((1.,0.706797490733887,1.00061923411664),(1.,
0.706182062146832,1.0006205338817),(1.,0.705584062769154,1.00062179683684),
(1.,0.705266224770657,1.0006224681003)))
REPRESENTATION_ITEM('')
SURFACE()
);
#3282=(
BOUNDED_SURFACE()
B_SPLINE_SURFACE(3,2,((#241669,#241670,#241671),(#241672,#241673,#241674),
(#241675,#241676,#241677),(#241678,#241679,#241680),(#241681,#241682,#241683),
(#241684,#241685,#241686)),.UNSPECIFIED.,.F.,.F.,.F.)
B_SPLINE_SURFACE_WITH_KNOTS((4,2,4),(3,3),(5.28548559086683E-19,0.000257652232350874,
0.000515304464701748),(0.,1.),.UNSPECIFIED.)
GEOMETRIC_REPRESENTATION_ITEM()
RATIONAL_B_SPLINE_SURFACE(((1.,0.874619707139394,1.),(1.,0.8748611804306,
1.),(1.,0.855455725921013,1.),(1.,0.794699358955116,1.),(1.,0.753768977788727,
1.),(1.,0.708712527163692,1.)))
REPRESENTATION_ITEM('')
SURFACE()
);
#3283=(
BOUNDED_SURFACE()
B_SPLINE_SURFACE(3,2,((#241692,#241693,#241694),(#241695,#241696,#241697),
(#241698,#241699,#241700),(#241701,#241702,#241703)),.UNSPECIFIED.,.F.,
 .F.,.F.)
B_SPLINE_SURFACE_WITH_KNOTS((4,4),(3,3),(0.,0.000397394373651919),(0.,1.),
 .UNSPECIFIED.)
GEOMETRIC_REPRESENTATION_ITEM()
RATIONAL_B_SPLINE_SURFACE(((1.,0.70710678118655,1.),(1.,0.707752587915875,
1.),(1.,0.708377654540735,1.),(1.,0.708689770883314,1.)))
REPRESENTATION_ITEM('')
SURFACE()
);
#3284=(
BOUNDED_SURFACE()
B_SPLINE_SURFACE(3,2,((#241705,#241706,#241707),(#241708,#241709,#241710),
(#241711,#241712,#241713),(#241714,#241715,#241716)),.UNSPECIFIED.,.F.,
 .F.,.F.)
B_SPLINE_SURFACE_WITH_KNOTS((4,4),(3,3),(0.,0.000511815456479785),(0.,1.00105873160019),
 .UNSPECIFIED.)
GEOMETRIC_REPRESENTATION_ITEM()
RATIONAL_B_SPLINE_SURFACE(((1.,0.708394529056267,1.00061746385375),(1.,
0.708058564166825,1.00061817524704),(1.,0.707430835372014,1.00061950443966),
(1.,0.706796685880295,1.00062084722788)))
REPRESENTATION_ITEM('')
SURFACE()
);
#3285=(
BOUNDED_SURFACE()
B_SPLINE_SURFACE(3,2,((#241722,#241723,#241724),(#241725,#241726,#241727),
(#241728,#241729,#241730),(#241731,#241732,#241733)),.UNSPECIFIED.,.F.,
 .F.,.F.)
B_SPLINE_SURFACE_WITH_KNOTS((4,4),(3,3),(4.87890977618477E-19,0.000397394465448305),
(0.,1.),.UNSPECIFIED.)
GEOMETRIC_REPRESENTATION_ITEM()
RATIONAL_B_SPLINE_SURFACE(((1.,0.705498956110739,1.),(1.,0.705821764811805,
1.),(1.,0.706461952521113,1.),(1.,0.707106781186559,1.)))
REPRESENTATION_ITEM('')
SURFACE()
);
#3286=(
BOUNDED_SURFACE()
B_SPLINE_SURFACE(3,2,((#241739,#241740,#241741),(#241742,#241743,#241744),
(#241745,#241746,#241747),(#241748,#241749,#241750)),.UNSPECIFIED.,.F.,
 .F.,.F.)
B_SPLINE_SURFACE_WITH_KNOTS((4,4),(3,3),(-5.96311194867027E-19,0.000397394410828722),
(0.,1.),.UNSPECIFIED.)
GEOMETRIC_REPRESENTATION_ITEM()
RATIONAL_B_SPLINE_SURFACE(((1.,0.708689770883324,1.),(1.,0.708376440034489,
1.),(1.,0.707750498698425,1.),(1.,0.707106781186535,1.)))
REPRESENTATION_ITEM('')
SURFACE()
);
#3287=(
BOUNDED_SURFACE()
B_SPLINE_SURFACE(3,2,((#241756,#241757,#241758),(#241759,#241760,#241761),
(#241762,#241763,#241764),(#241765,#241766,#241767)),.UNSPECIFIED.,.F.,
 .F.,.F.)
B_SPLINE_SURFACE_WITH_KNOTS((4,4),(3,3),(0.,0.000511815090126176),(0.,1.00105592270271),
 .UNSPECIFIED.)
GEOMETRIC_REPRESENTATION_ITEM()
RATIONAL_B_SPLINE_SURFACE(((1.,0.705266242717332,1.00062243213114),(1.,
0.705584085908974,1.00062176089545),(1.,0.706182089450373,1.00062049800442),
(1.,0.706797508587321,1.00061919833435)))
REPRESENTATION_ITEM('')
SURFACE()
);
#3288=(
BOUNDED_SURFACE()
B_SPLINE_SURFACE(3,2,((#241769,#241770,#241771),(#241772,#241773,#241774),
(#241775,#241776,#241777),(#241778,#241779,#241780)),.UNSPECIFIED.,.F.,
 .F.,.F.)
B_SPLINE_SURFACE_WITH_KNOTS((4,4),(3,3),(-8.13151629364128E-20,0.000397394428086617),
(0.,1.),.UNSPECIFIED.)
GEOMETRIC_REPRESENTATION_ITEM()
RATIONAL_B_SPLINE_SURFACE(((1.,0.707106781186563,1.),(1.,0.706459846759093,
1.),(1.,0.705820510737283,1.),(1.,0.705498956110757,1.)))
REPRESENTATION_ITEM('')
SURFACE()
);
#3289=(
BOUNDED_SURFACE()
B_SPLINE_SURFACE(3,2,((#241786,#241787,#241788),(#241789,#241790,#241791),
(#241792,#241793,#241794),(#241795,#241796,#241797),(#241798,#241799,#241800),
(#241801,#241802,#241803)),.UNSPECIFIED.,.F.,.F.,.F.)
B_SPLINE_SURFACE_WITH_KNOTS((4,2,4),(3,3),(0.,0.000257953807872855,0.00051590761574571),
(0.,1.),.UNSPECIFIED.)
GEOMETRIC_REPRESENTATION_ITEM()
RATIONAL_B_SPLINE_SURFACE(((1.,0.874619707139394,1.),(1.,0.874834349678904,
1.),(1.,0.854686104157903,1.),(1.,0.792476597915017,1.),(1.,0.750887854595213,
1.),(1.,0.705585838031453,1.)))
REPRESENTATION_ITEM('')
SURFACE()
);
#3290=(
BOUNDED_SURFACE()
B_SPLINE_SURFACE(3,2,((#241809,#241810,#241811),(#241812,#241813,#241814),
(#241815,#241816,#241817),(#241818,#241819,#241820)),.UNSPECIFIED.,.F.,
 .F.,.F.)
B_SPLINE_SURFACE_WITH_KNOTS((4,4),(3,3),(0.,0.000511815437699146),(0.,1.00105881331748),
 .UNSPECIFIED.)
GEOMETRIC_REPRESENTATION_ITEM()
RATIONAL_B_SPLINE_SURFACE(((1.,0.706796661945865,1.00062089519812),(1.,
0.707430821224745,1.00061955228554),(1.,0.708058545830274,1.0006182229992),
(1.,0.708394505252235,1.00061751156258)))
REPRESENTATION_ITEM('')
SURFACE()
);
#3291=(
BOUNDED_SURFACE()
B_SPLINE_SURFACE(3,2,((#241822,#241823,#241824),(#241825,#241826,#241827),
(#241828,#241829,#241830),(#241831,#241832,#241833),(#241834,#241835,#241836),
(#241837,#241838,#241839)),.UNSPECIFIED.,.F.,.F.,.F.)
B_SPLINE_SURFACE_WITH_KNOTS((4,2,4),(3,3),(3.52365706057789E-19,0.00025691531753126,
0.00051383063506252),(0.,1.),.UNSPECIFIED.)
GEOMETRIC_REPRESENTATION_ITEM()
RATIONAL_B_SPLINE_SURFACE(((1.,0.705585838031451,1.),(1.,0.750902433542401,
1.),(1.,0.79232953008298,1.),(1.,0.854288401593769,1.),(1.,0.874998031125475,
1.),(1.,0.874619707139399,1.)))
REPRESENTATION_ITEM('')
SURFACE()
);
#3292=(
BOUNDED_SURFACE()
B_SPLINE_SURFACE(3,2,((#241845,#241846,#241847),(#241848,#241849,#241850),
(#241851,#241852,#241853),(#241854,#241855,#241856),(#241857,#241858,#241859),
(#241860,#241861,#241862)),.UNSPECIFIED.,.F.,.F.,.F.)
B_SPLINE_SURFACE_WITH_KNOTS((4,2,4),(3,3),(-4.30970363562988E-18,0.000256592814262152,
0.000513185628524307),(0.,1.),.UNSPECIFIED.)
GEOMETRIC_REPRESENTATION_ITEM()
RATIONAL_B_SPLINE_SURFACE(((1.,0.708712527163664,1.),(1.,0.753780902613362,
1.),(1.,0.794538995769504,1.),(1.,0.855070770330797,1.),(1.,0.875018427445572,
1.),(1.,0.874619707139393,1.)))
REPRESENTATION_ITEM('')
SURFACE()
);
#3293=(
BOUNDED_SURFACE()
B_SPLINE_SURFACE(3,2,((#241864,#241865,#241866),(#241867,#241868,#241869),
(#241870,#241871,#241872),(#241873,#241874,#241875)),.UNSPECIFIED.,.F.,
 .F.,.F.)
B_SPLINE_SURFACE_WITH_KNOTS((4,4),(3,3),(5.6920614055489E-19,0.000511815072430397),
(0.,1.00105598365966),.UNSPECIFIED.)
GEOMETRIC_REPRESENTATION_ITEM()
RATIONAL_B_SPLINE_SURFACE(((1.,0.706797490733448,1.00061923411751),(1.,
0.70618206214638,1.00062053388258),(1.,0.705584062768717,1.00062179683772),
(1.,0.705266224770207,1.00062246810119)))
REPRESENTATION_ITEM('')
SURFACE()
);
#3294=(
BOUNDED_SURFACE()
B_SPLINE_SURFACE(3,2,((#241881,#241882,#241883),(#241884,#241885,#241886),
(#241887,#241888,#241889),(#241890,#241891,#241892),(#241893,#241894,#241895),
(#241896,#241897,#241898)),.UNSPECIFIED.,.F.,.F.,.F.)
B_SPLINE_SURFACE_WITH_KNOTS((4,2,4),(3,3),(-3.19839640883224E-18,0.000257652232350882,
0.000515304464701768),(0.,1.),.UNSPECIFIED.)
GEOMETRIC_REPRESENTATION_ITEM()
RATIONAL_B_SPLINE_SURFACE(((1.,0.874619707139399,1.),(1.,0.874861180430683,
1.),(1.,0.855455725920874,1.),(1.,0.794699358955272,1.),(1.,0.753768977788643,
1.),(1.,0.708712527163664,1.)))
REPRESENTATION_ITEM('')
SURFACE()
);
#3295=(
BOUNDED_SURFACE()
B_SPLINE_SURFACE(3,2,((#241904,#241905,#241906),(#241907,#241908,#241909),
(#241910,#241911,#241912),(#241913,#241914,#241915)),.UNSPECIFIED.,.F.,
 .F.,.F.)
B_SPLINE_SURFACE_WITH_KNOTS((4,4),(3,3),(0.,0.000397394373651913),(0.,1.),
 .UNSPECIFIED.)
GEOMETRIC_REPRESENTATION_ITEM()
RATIONAL_B_SPLINE_SURFACE(((1.,0.70710678118654,1.),(1.,0.707752587915903,
1.),(1.,0.708377654540674,1.),(1.,0.708689770883327,1.)))
REPRESENTATION_ITEM('')
SURFACE()
);
#3296=(
BOUNDED_SURFACE()
B_SPLINE_SURFACE(3,2,((#241917,#241918,#241919),(#241920,#241921,#241922),
(#241923,#241924,#241925),(#241926,#241927,#241928)),.UNSPECIFIED.,.F.,
 .F.,.F.)
B_SPLINE_SURFACE_WITH_KNOTS((4,4),(3,3),(0.,0.000511815456479788),(0.,1.00105873159895),
 .UNSPECIFIED.)
GEOMETRIC_REPRESENTATION_ITEM()
RATIONAL_B_SPLINE_SURFACE(((1.,0.708394529056624,1.00061746385303),(1.,
0.708058564167179,1.00061817524632),(1.,0.70743083537233,1.00061950443894),
(1.,0.706796685880683,1.00062084722715)))
REPRESENTATION_ITEM('')
SURFACE()
);
#3297=(
BOUNDED_SURFACE()
B_SPLINE_SURFACE(3,2,((#241934,#241935,#241936),(#241937,#241938,#241939),
(#241940,#241941,#241942),(#241943,#241944,#241945)),.UNSPECIFIED.,.F.,
 .F.,.F.)
B_SPLINE_SURFACE_WITH_KNOTS((4,4),(3,3),(-1.43656787854329E-18,0.000397394465448297),
(0.,1.),.UNSPECIFIED.)
GEOMETRIC_REPRESENTATION_ITEM()
RATIONAL_B_SPLINE_SURFACE(((1.,0.70549895611075,1.),(1.,0.705821764811781,
1.),(1.,0.706461952521137,1.),(1.,0.70710678118655,1.)))
REPRESENTATION_ITEM('')
SURFACE()
);
#3298=(
BOUNDED_SURFACE()
B_SPLINE_SURFACE(3,2,((#241951,#241952,#241953),(#241954,#241955,#241956),
(#241957,#241958,#241959),(#241960,#241961,#241962)),.UNSPECIFIED.,.F.,
 .F.,.F.)
B_SPLINE_SURFACE_WITH_KNOTS((4,4),(3,3),(0.,0.000397394410828738),(0.,1.),
 .UNSPECIFIED.)
GEOMETRIC_REPRESENTATION_ITEM()
RATIONAL_B_SPLINE_SURFACE(((1.,0.708689770883318,1.),(1.,0.708376440034509,
1.),(1.,0.707750498698355,1.),(1.,0.707106781186568,1.)))
REPRESENTATION_ITEM('')
SURFACE()
);
#3299=(
BOUNDED_SURFACE()
B_SPLINE_SURFACE(3,2,((#241968,#241969,#241970),(#241971,#241972,#241973),
(#241974,#241975,#241976),(#241977,#241978,#241979)),.UNSPECIFIED.,.F.,
 .F.,.F.)
B_SPLINE_SURFACE_WITH_KNOTS((4,4),(3,3),(0.,0.00051181509012617),(0.,1.00105592270631),
 .UNSPECIFIED.)
GEOMETRIC_REPRESENTATION_ITEM()
RATIONAL_B_SPLINE_SURFACE(((1.,0.705266242716285,1.00062243213326),(1.,
0.705584085907913,1.00062176089758),(1.,0.706182089449311,1.00062049800654),
(1.,0.706797508586264,1.00061919833646)))
REPRESENTATION_ITEM('')
SURFACE()
);
#3300=(
BOUNDED_SURFACE()
B_SPLINE_SURFACE(3,2,((#241981,#241982,#241983),(#241984,#241985,#241986),
(#241987,#241988,#241989),(#241990,#241991,#241992)),.UNSPECIFIED.,.F.,
 .F.,.F.)
B_SPLINE_SURFACE_WITH_KNOTS((4,4),(3,3),(0.,0.000397394428086615),(0.,1.),
 .UNSPECIFIED.)
GEOMETRIC_REPRESENTATION_ITEM()
RATIONAL_B_SPLINE_SURFACE(((1.,0.707106781186545,1.),(1.,0.706459846759086,
1.),(1.,0.70582051073728,1.),(1.,0.70549895611076,1.)))
REPRESENTATION_ITEM('')
SURFACE()
);
#3301=(
BOUNDED_SURFACE()
B_SPLINE_SURFACE(3,2,((#241998,#241999,#242000),(#242001,#242002,#242003),
(#242004,#242005,#242006),(#242007,#242008,#242009),(#242010,#242011,#242012),
(#242013,#242014,#242015)),.UNSPECIFIED.,.F.,.F.,.F.)
B_SPLINE_SURFACE_WITH_KNOTS((4,2,4),(3,3),(0.,0.000257953807872855,0.000515907615745711),
(0.,1.),.UNSPECIFIED.)
GEOMETRIC_REPRESENTATION_ITEM()
RATIONAL_B_SPLINE_SURFACE(((1.,0.87461970713939,1.),(1.,0.874834349678975,
1.),(1.,0.854686104157832,1.),(1.,0.7924765979151,1.),(1.,0.750887854595135,
1.),(1.,0.705585838031471,1.)))
REPRESENTATION_ITEM('')
SURFACE()
);
#3302=(
BOUNDED_SURFACE()
B_SPLINE_SURFACE(3,2,((#242021,#242022,#242023),(#242024,#242025,#242026),
(#242027,#242028,#242029),(#242030,#242031,#242032)),.UNSPECIFIED.,.F.,
 .F.,.F.)
B_SPLINE_SURFACE_WITH_KNOTS((4,4),(3,3),(-6.26126754610379E-18,0.000511815437699142),
(0.,1.00105881331519),.UNSPECIFIED.)
GEOMETRIC_REPRESENTATION_ITEM()
RATIONAL_B_SPLINE_SURFACE(((1.,0.70679666194653,1.00062089519678),(1.,0.707430821225431,
1.0006195522842),(1.,0.708058545830899,1.00061822299786),(1.,0.708394505252917,
1.00061751156124)))
REPRESENTATION_ITEM('')
SURFACE()
);
#3303=(
BOUNDED_SURFACE()
B_SPLINE_SURFACE(3,2,((#242034,#242035,#242036),(#242037,#242038,#242039),
(#242040,#242041,#242042),(#242043,#242044,#242045),(#242046,#242047,#242048),
(#242049,#242050,#242051)),.UNSPECIFIED.,.F.,.F.,.F.)
B_SPLINE_SURFACE_WITH_KNOTS((4,2,4),(3,3),(0.,0.000256915317531255,0.00051383063506251),
(0.,1.),.UNSPECIFIED.)
GEOMETRIC_REPRESENTATION_ITEM()
RATIONAL_B_SPLINE_SURFACE(((1.,0.705585838031438,1.),(1.,0.750902433542754,
1.),(1.,0.792329530082518,1.),(1.,0.854288401594195,1.),(1.,0.874998031125136,
1.),(1.,0.874619707139401,1.)))
REPRESENTATION_ITEM('')
SURFACE()
);
#3304=(
BOUNDED_SURFACE()
B_SPLINE_SURFACE(3,2,((#242057,#242058,#242059),(#242060,#242061,#242062),
(#242063,#242064,#242065),(#242066,#242067,#242068),(#242069,#242070,#242071),
(#242072,#242073,#242074)),.UNSPECIFIED.,.F.,.F.,.F.)
B_SPLINE_SURFACE_WITH_KNOTS((4,2,4),(3,3),(0.,0.000256592814262162,0.000513185628524325),
(0.,1.),.UNSPECIFIED.)
GEOMETRIC_REPRESENTATION_ITEM()
RATIONAL_B_SPLINE_SURFACE(((1.,0.708712527163663,1.),(1.,0.753780902613412,
1.),(1.,0.794538995769447,1.),(1.,0.855070770330856,1.),(1.,0.875018427445525,
1.),(1.,0.87461970713939,1.)))
REPRESENTATION_ITEM('')
SURFACE()
);
#3305=(
BOUNDED_SURFACE()
B_SPLINE_SURFACE(3,2,((#242076,#242077,#242078),(#242079,#242080,#242081),
(#242082,#242083,#242084),(#242085,#242086,#242087)),.UNSPECIFIED.,.F.,
 .F.,.F.)
B_SPLINE_SURFACE_WITH_KNOTS((4,4),(3,3),(-2.71050543121376E-20,0.000511815072430413),
(0.,1.00105598365856),.UNSPECIFIED.)
GEOMETRIC_REPRESENTATION_ITEM()
RATIONAL_B_SPLINE_SURFACE(((1.,0.70679749073378,1.00061923411687),(1.,0.706182062146706,
1.00062053388193),(1.,0.70558406276906,1.00062179683707),(1.,0.705266224770537,
1.00062246810054)))
REPRESENTATION_ITEM('')
SURFACE()
);
#3306=(
BOUNDED_SURFACE()
B_SPLINE_SURFACE(3,2,((#242093,#242094,#242095),(#242096,#242097,#242098),
(#242099,#242100,#242101),(#242102,#242103,#242104),(#242105,#242106,#242107),
(#242108,#242109,#242110)),.UNSPECIFIED.,.F.,.F.,.F.)
B_SPLINE_SURFACE_WITH_KNOTS((4,2,4),(3,3),(-8.13151629364128E-20,0.000257652232350874,
0.000515304464701749),(0.,1.),.UNSPECIFIED.)
GEOMETRIC_REPRESENTATION_ITEM()
RATIONAL_B_SPLINE_SURFACE(((1.,0.874619707139396,1.),(1.,0.874861180430513,
1.),(1.,0.855455725921131,1.),(1.,0.794699358954991,1.),(1.,0.753768977788884,
1.),(1.,0.708712527163653,1.)))
REPRESENTATION_ITEM('')
SURFACE()
);
#3307=(
BOUNDED_SURFACE()
B_SPLINE_SURFACE(3,2,((#242116,#242117,#242118),(#242119,#242120,#242121),
(#242122,#242123,#242124),(#242125,#242126,#242127)),.UNSPECIFIED.,.F.,
 .F.,.F.)
B_SPLINE_SURFACE_WITH_KNOTS((4,4),(3,3),(-1.04083408558608E-17,0.000397394373651904),
(0.,1.),.UNSPECIFIED.)
GEOMETRIC_REPRESENTATION_ITEM()
RATIONAL_B_SPLINE_SURFACE(((1.,0.70710678118655,1.),(1.,0.707752587915888,
1.),(1.,0.708377654540711,1.),(1.,0.708689770883332,1.)))
REPRESENTATION_ITEM('')
SURFACE()
);
#3308=(
BOUNDED_SURFACE()
B_SPLINE_SURFACE(3,2,((#242129,#242130,#242131),(#242132,#242133,#242134),
(#242135,#242136,#242137),(#242138,#242139,#242140)),.UNSPECIFIED.,.F.,
 .F.,.F.)
B_SPLINE_SURFACE_WITH_KNOTS((4,4),(3,3),(-3.6049722235143E-18,0.000511815456479789),
(0.,1.00105873159758),.UNSPECIFIED.)
GEOMETRIC_REPRESENTATION_ITEM()
RATIONAL_B_SPLINE_SURFACE(((1.,0.708394529057025,1.00061746385223),(1.,
0.708058564167564,1.00061817524552),(1.,0.70743083537276,1.00061950443814),
(1.,0.706796685881074,1.00062084722635)))
REPRESENTATION_ITEM('')
SURFACE()
);
#3309=(
BOUNDED_SURFACE()
B_SPLINE_SURFACE(3,2,((#242146,#242147,#242148),(#242149,#242150,#242151),
(#242152,#242153,#242154),(#242155,#242156,#242157)),.UNSPECIFIED.,.F.,
 .F.,.F.)
B_SPLINE_SURFACE_WITH_KNOTS((4,4),(3,3),(0.,0.000397394465448303),(0.,1.),
 .UNSPECIFIED.)
GEOMETRIC_REPRESENTATION_ITEM()
RATIONAL_B_SPLINE_SURFACE(((1.,0.705498956110737,1.),(1.,0.70582176481177,
1.),(1.,0.70646195252114,1.),(1.,0.70710678118655,1.)))
REPRESENTATION_ITEM('')
SURFACE()
);
#3310=(
BOUNDED_SURFACE()
B_SPLINE_SURFACE(3,2,((#242163,#242164,#242165),(#242166,#242167,#242168),
(#242169,#242170,#242171),(#242172,#242173,#242174)),.UNSPECIFIED.,.F.,
 .F.,.F.)
B_SPLINE_SURFACE_WITH_KNOTS((4,4),(3,3),(0.,0.000397394410828738),(0.,1.),
 .UNSPECIFIED.)
GEOMETRIC_REPRESENTATION_ITEM()
RATIONAL_B_SPLINE_SURFACE(((1.,0.708689770883326,1.),(1.,0.708376440034507,
1.),(1.,0.707750498698402,1.),(1.,0.707106781186546,1.)))
REPRESENTATION_ITEM('')
SURFACE()
);
#3311=(
BOUNDED_SURFACE()
B_SPLINE_SURFACE(3,2,((#242180,#242181,#242182),(#242183,#242184,#242185),
(#242186,#242187,#242188),(#242189,#242190,#242191)),.UNSPECIFIED.,.F.,
 .F.,.F.)
B_SPLINE_SURFACE_WITH_KNOTS((4,4),(3,3),(-1.62630325872826E-18,0.000511815090126177),
(0.,1.0010559227041),.UNSPECIFIED.)
GEOMETRIC_REPRESENTATION_ITEM()
RATIONAL_B_SPLINE_SURFACE(((1.,0.705266242716925,1.00062243213196),(1.,
0.705584085908534,1.00062176089627),(1.,0.706182089449937,1.00062049800524),
(1.,0.706797508586938,1.00061919833516)))
REPRESENTATION_ITEM('')
SURFACE()
);
#3312=(
BOUNDED_SURFACE()
B_SPLINE_SURFACE(3,2,((#242193,#242194,#242195),(#242196,#242197,#242198),
(#242199,#242200,#242201),(#242202,#242203,#242204)),.UNSPECIFIED.,.F.,
 .F.,.F.)
B_SPLINE_SURFACE_WITH_KNOTS((4,4),(3,3),(0.,0.000397394428086624),(0.,1.),
 .UNSPECIFIED.)
GEOMETRIC_REPRESENTATION_ITEM()
RATIONAL_B_SPLINE_SURFACE(((1.,0.707106781186533,1.),(1.,0.706459846759113,
1.),(1.,0.705820510737269,1.),(1.,0.705498956110716,1.)))
REPRESENTATION_ITEM('')
SURFACE()
);
#3313=(
BOUNDED_SURFACE()
B_SPLINE_SURFACE(3,2,((#242210,#242211,#242212),(#242213,#242214,#242215),
(#242216,#242217,#242218),(#242219,#242220,#242221),(#242222,#242223,#242224),
(#242225,#242226,#242227)),.UNSPECIFIED.,.F.,.F.,.F.)
B_SPLINE_SURFACE_WITH_KNOTS((4,2,4),(3,3),(0.,0.000257953807872849,0.000515907615745699),
(0.,1.),.UNSPECIFIED.)
GEOMETRIC_REPRESENTATION_ITEM()
RATIONAL_B_SPLINE_SURFACE(((1.,0.874619707139391,1.),(1.,0.874834349679018,
1.),(1.,0.854686104157772,1.),(1.,0.792476597915156,1.),(1.,0.750887854595126,
1.),(1.,0.705585838031422,1.)))
REPRESENTATION_ITEM('')
SURFACE()
);
#3314=(
BOUNDED_SURFACE()
B_SPLINE_SURFACE(3,2,((#242233,#242234,#242235),(#242236,#242237,#242238),
(#242239,#242240,#242241),(#242242,#242243,#242244)),.UNSPECIFIED.,.F.,
 .F.,.F.)
B_SPLINE_SURFACE_WITH_KNOTS((4,4),(3,3),(0.,0.000511815437699142),(0.,1.00105881331444),
 .UNSPECIFIED.)
GEOMETRIC_REPRESENTATION_ITEM()
RATIONAL_B_SPLINE_SURFACE(((1.,0.706796661946758,1.00062089519634),(1.,
0.707430821225624,1.00061955228376),(1.,0.70805854583117,1.00061822299742),
(1.,0.708394505253132,1.0006175115608)))
REPRESENTATION_ITEM('')
SURFACE()
);
#3315=(
BOUNDED_SURFACE()
B_SPLINE_SURFACE(3,2,((#242246,#242247,#242248),(#242249,#242250,#242251),
(#242252,#242253,#242254),(#242255,#242256,#242257),(#242258,#242259,#242260),
(#242261,#242262,#242263)),.UNSPECIFIED.,.F.,.F.,.F.)
B_SPLINE_SURFACE_WITH_KNOTS((4,2,4),(3,3),(2.71050543121376E-20,0.00025691531753127,
0.000513830635062539),(0.,1.),.UNSPECIFIED.)
GEOMETRIC_REPRESENTATION_ITEM()
RATIONAL_B_SPLINE_SURFACE(((1.,0.705585838031442,1.),(1.,0.750902433543051,
1.),(1.,0.792329530082094,1.),(1.,0.854288401594649,1.),(1.,0.8749980311248,
1.),(1.,0.874619707139398,1.)))
REPRESENTATION_ITEM('')
SURFACE()
);
#3316=(
BOUNDED_SURFACE()
B_SPLINE_SURFACE(3,2,((#242269,#242270,#242271),(#242272,#242273,#242274),
(#242275,#242276,#242277),(#242278,#242279,#242280),(#242281,#242282,#242283),
(#242284,#242285,#242286)),.UNSPECIFIED.,.F.,.F.,.F.)
B_SPLINE_SURFACE_WITH_KNOTS((4,2,4),(3,3),(-1.11401773222886E-17,0.000256592814262152,
0.000513185628524315),(0.,1.),.UNSPECIFIED.)
GEOMETRIC_REPRESENTATION_ITEM()
RATIONAL_B_SPLINE_SURFACE(((1.,0.708712527163676,1.),(1.,0.753780902613421,
1.),(1.,0.794538995769422,1.),(1.,0.855070770330898,1.),(1.,0.875018427445499,
1.),(1.,0.874619707139395,1.)))
REPRESENTATION_ITEM('')
SURFACE()
);
#3317=(
BOUNDED_SURFACE()
B_SPLINE_SURFACE(3,2,((#242288,#242289,#242290),(#242291,#242292,#242293),
(#242294,#242295,#242296),(#242297,#242298,#242299)),.UNSPECIFIED.,.F.,
 .F.,.F.)
B_SPLINE_SURFACE_WITH_KNOTS((4,4),(3,3),(-1.62630325872826E-19,0.000511815072430405),
(0.,1.00105598365847),.UNSPECIFIED.)
GEOMETRIC_REPRESENTATION_ITEM()
RATIONAL_B_SPLINE_SURFACE(((1.,0.706797490733806,1.00061923411681),(1.,
0.706182062146721,1.00062053388188),(1.,0.705584062769095,1.00062179683702),
(1.,0.705266224770575,1.00062246810048)))
REPRESENTATION_ITEM('')
SURFACE()
);
#3318=(
BOUNDED_SURFACE()
B_SPLINE_SURFACE(3,2,((#242305,#242306,#242307),(#242308,#242309,#242310),
(#242311,#242312,#242313),(#242314,#242315,#242316),(#242317,#242318,#242319),
(#242320,#242321,#242322)),.UNSPECIFIED.,.F.,.F.,.F.)
B_SPLINE_SURFACE_WITH_KNOTS((4,2,4),(3,3),(0.,0.000257652232350882,0.000515304464701764),
(0.,1.),.UNSPECIFIED.)
GEOMETRIC_REPRESENTATION_ITEM()
RATIONAL_B_SPLINE_SURFACE(((1.,0.874619707139392,1.),(1.,0.874861180430873,
1.),(1.,0.855455725920652,1.),(1.,0.79469935895548,1.),(1.,0.753768977788454,
1.),(1.,0.708712527163685,1.)))
REPRESENTATION_ITEM('')
SURFACE()
);
#3319=(
BOUNDED_SURFACE()
B_SPLINE_SURFACE(3,2,((#242328,#242329,#242330),(#242331,#242332,#242333),
(#242334,#242335,#242336),(#242337,#242338,#242339)),.UNSPECIFIED.,.F.,
 .F.,.F.)
B_SPLINE_SURFACE_WITH_KNOTS((4,4),(3,3),(-7.31836466427715E-19,0.000397394373651924),
(0.,1.),.UNSPECIFIED.)
GEOMETRIC_REPRESENTATION_ITEM()
RATIONAL_B_SPLINE_SURFACE(((1.,0.707106781186549,1.),(1.,0.707752587915856,
1.),(1.,0.708377654540692,1.),(1.,0.708689770883325,1.)))
REPRESENTATION_ITEM('')
SURFACE()
);
#3320=(
BOUNDED_SURFACE()
B_SPLINE_SURFACE(3,2,((#242341,#242342,#242343),(#242344,#242345,#242346),
(#242347,#242348,#242349),(#242350,#242351,#242352)),.UNSPECIFIED.,.F.,
 .F.,.F.)
B_SPLINE_SURFACE_WITH_KNOTS((4,4),(3,3),(0.,0.000511815456479794),(0.,1.00105873159879),
 .UNSPECIFIED.)
GEOMETRIC_REPRESENTATION_ITEM()
RATIONAL_B_SPLINE_SURFACE(((1.,0.708394529056662,1.00061746385294),(1.,
0.70805856416723,1.00061817524622),(1.,0.707430835372382,1.00061950443885),
(1.,0.70679668588072,1.00062084722706)))
REPRESENTATION_ITEM('')
SURFACE()
);
#3321=(
BOUNDED_SURFACE()
B_SPLINE_SURFACE(3,2,((#242358,#242359,#242360),(#242361,#242362,#242363),
(#242364,#242365,#242366),(#242367,#242368,#242369)),.UNSPECIFIED.,.F.,
 .F.,.F.)
B_SPLINE_SURFACE_WITH_KNOTS((4,4),(3,3),(-4.06575814682064E-18,0.0003973944654483),
(0.,1.),.UNSPECIFIED.)
GEOMETRIC_REPRESENTATION_ITEM()
RATIONAL_B_SPLINE_SURFACE(((1.,0.705498956110753,1.),(1.,0.705821764811809,
1.),(1.,0.706461952521118,1.),(1.,0.707106781186563,1.)))
REPRESENTATION_ITEM('')
SURFACE()
);
#3322=(
BOUNDED_SURFACE()
B_SPLINE_SURFACE(3,2,((#242375,#242376,#242377),(#242378,#242379,#242380),
(#242381,#242382,#242383),(#242384,#242385,#242386)),.UNSPECIFIED.,.F.,
 .F.,.F.)
B_SPLINE_SURFACE_WITH_KNOTS((4,4),(3,3),(0.,0.000397394410828732),(0.,1.),
 .UNSPECIFIED.)
GEOMETRIC_REPRESENTATION_ITEM()
RATIONAL_B_SPLINE_SURFACE(((1.,0.708689770883298,1.),(1.,0.708376440034519,
1.),(1.,0.707750498698387,1.),(1.,0.707106781186546,1.)))
REPRESENTATION_ITEM('')
SURFACE()
);
#3323=(
BOUNDED_SURFACE()
B_SPLINE_SURFACE(3,2,((#242392,#242393,#242394),(#242395,#242396,#242397),
(#242398,#242399,#242400),(#242401,#242402,#242403)),.UNSPECIFIED.,.F.,
 .F.,.F.)
B_SPLINE_SURFACE_WITH_KNOTS((4,4),(3,3),(-3.22550146314438E-18,0.000511815090126175),
(0.,1.00105592270367),.UNSPECIFIED.)
GEOMETRIC_REPRESENTATION_ITEM()
RATIONAL_B_SPLINE_SURFACE(((1.,0.705266242717061,1.00062243213171),(1.,
0.705584085908694,1.00062176089602),(1.,0.706182089450076,1.00062049800499),
(1.,0.70679750858705,1.00061919833491)))
REPRESENTATION_ITEM('')
SURFACE()
);
#3324=(
BOUNDED_SURFACE()
B_SPLINE_SURFACE(3,2,((#242405,#242406,#242407),(#242408,#242409,#242410),
(#242411,#242412,#242413),(#242414,#242415,#242416)),.UNSPECIFIED.,.F.,
 .F.,.F.)
B_SPLINE_SURFACE_WITH_KNOTS((4,4),(3,3),(-4.66206934168767E-18,0.000397394428086629),
(0.,1.),.UNSPECIFIED.)
GEOMETRIC_REPRESENTATION_ITEM()
RATIONAL_B_SPLINE_SURFACE(((1.,0.707106781186546,1.),(1.,0.706459846759078,
1.),(1.,0.705820510737287,1.),(1.,0.705498956110751,1.)))
REPRESENTATION_ITEM('')
SURFACE()
);
#3325=(
BOUNDED_SURFACE()
B_SPLINE_SURFACE(3,2,((#242422,#242423,#242424),(#242425,#242426,#242427),
(#242428,#242429,#242430),(#242431,#242432,#242433),(#242434,#242435,#242436),
(#242437,#242438,#242439)),.UNSPECIFIED.,.F.,.F.,.F.)
B_SPLINE_SURFACE_WITH_KNOTS((4,2,4),(3,3),(0.,0.000257953807872843,0.000515907615745686),
(0.,1.),.UNSPECIFIED.)
GEOMETRIC_REPRESENTATION_ITEM()
RATIONAL_B_SPLINE_SURFACE(((1.,0.874619707139389,1.),(1.,0.874834349678801,
1.),(1.,0.854686104158044,1.),(1.,0.792476597914911,1.),(1.,0.750887854595285,
1.),(1.,0.705585838031442,1.)))
REPRESENTATION_ITEM('')
SURFACE()
);
#3326=(
BOUNDED_SURFACE()
B_SPLINE_SURFACE(3,2,((#242445,#242446,#242447),(#242448,#242449,#242450),
(#242451,#242452,#242453),(#242454,#242455,#242456)),.UNSPECIFIED.,.F.,
 .F.,.F.)
B_SPLINE_SURFACE_WITH_KNOTS((4,4),(3,3),(-1.03812358015487E-17,0.00051181543769915),
(0.,1.00105881331573),.UNSPECIFIED.)
GEOMETRIC_REPRESENTATION_ITEM()
RATIONAL_B_SPLINE_SURFACE(((1.,0.70679666194638,1.00062089519709),(1.,0.707430821225288,
1.00061955228452),(1.,0.708058545830734,1.00061822299818),(1.,0.708394505252756,
1.00061751156156)))
REPRESENTATION_ITEM('')
SURFACE()
);
#3327=(
BOUNDED_SURFACE()
B_SPLINE_SURFACE(3,2,((#242458,#242459,#242460),(#242461,#242462,#242463),
(#242464,#242465,#242466),(#242467,#242468,#242469),(#242470,#242471,#242472),
(#242473,#242474,#242475)),.UNSPECIFIED.,.F.,.F.,.F.)
B_SPLINE_SURFACE_WITH_KNOTS((4,2,4),(3,3),(0.,0.00025691531753126,0.000513830635062521),
(0.,1.),.UNSPECIFIED.)
GEOMETRIC_REPRESENTATION_ITEM()
RATIONAL_B_SPLINE_SURFACE(((1.,0.705585838031422,1.),(1.,0.750902433542275,
1.),(1.,0.792329530083122,1.),(1.,0.854288401593586,1.),(1.,0.874998031125599,
1.),(1.,0.874619707139391,1.)))
REPRESENTATION_ITEM('')
SURFACE()
);
#3328=(
BOUNDED_SURFACE()
B_SPLINE_SURFACE(3,2,((#242481,#242482,#242483),(#242484,#242485,#242486),
(#242487,#242488,#242489),(#242490,#242491,#242492),(#242493,#242494,#242495),
(#242496,#242497,#242498)),.UNSPECIFIED.,.F.,.F.,.F.)
B_SPLINE_SURFACE_WITH_KNOTS((4,2,4),(3,3),(-2.16840434497101E-18,0.000256592814262155,
0.000513185628524311),(0.,1.),.UNSPECIFIED.)
GEOMETRIC_REPRESENTATION_ITEM()
RATIONAL_B_SPLINE_SURFACE(((1.,0.708712527163659,1.),(1.,0.753780902613598,
1.),(1.,0.794538995769182,1.),(1.,0.855070770331133,1.),(1.,0.875018427445305,
1.),(1.,0.874619707139401,1.)))
REPRESENTATION_ITEM('')
SURFACE()
);
#3329=(
BOUNDED_SURFACE()
B_SPLINE_SURFACE(3,2,((#242500,#242501,#242502),(#242503,#242504,#242505),
(#242506,#242507,#242508),(#242509,#242510,#242511)),.UNSPECIFIED.,.F.,
 .F.,.F.)
B_SPLINE_SURFACE_WITH_KNOTS((4,4),(3,3),(0.,0.000511815072430405),(0.,1.00105598365859),
 .UNSPECIFIED.)
GEOMETRIC_REPRESENTATION_ITEM()
RATIONAL_B_SPLINE_SURFACE(((1.,0.70679749073377,1.00061923411689),(1.,0.706182062146715,
1.00062053388195),(1.,0.705584062769003,1.00062179683709),(1.,0.705266224770533,
1.00062246810055)))
REPRESENTATION_ITEM('')
SURFACE()
);
#3330=(
BOUNDED_SURFACE()
B_SPLINE_SURFACE(3,2,((#242517,#242518,#242519),(#242520,#242521,#242522),
(#242523,#242524,#242525),(#242526,#242527,#242528),(#242529,#242530,#242531),
(#242532,#242533,#242534)),.UNSPECIFIED.,.F.,.F.,.F.)
B_SPLINE_SURFACE_WITH_KNOTS((4,2,4),(3,3),(4.47233396150271E-19,0.000257652232350877,
0.000515304464701754),(0.,1.),.UNSPECIFIED.)
GEOMETRIC_REPRESENTATION_ITEM()
RATIONAL_B_SPLINE_SURFACE(((1.,0.874619707139385,1.),(1.,0.874861180431084,
1.),(1.,0.855455725920359,1.),(1.,0.794699358955758,1.),(1.,0.753768977788267,
1.),(1.,0.708712527163679,1.)))
REPRESENTATION_ITEM('')
SURFACE()
);
#3331=(
BOUNDED_SURFACE()
B_SPLINE_SURFACE(3,2,((#242540,#242541,#242542),(#242543,#242544,#242545),
(#242546,#242547,#242548),(#242549,#242550,#242551)),.UNSPECIFIED.,.F.,
 .F.,.F.)
B_SPLINE_SURFACE_WITH_KNOTS((4,4),(3,3),(0.,0.000397394373651925),(0.,1.),
 .UNSPECIFIED.)
GEOMETRIC_REPRESENTATION_ITEM()
RATIONAL_B_SPLINE_SURFACE(((1.,0.707106781186536,1.),(1.,0.707752587915914,
1.),(1.,0.708377654540683,1.),(1.,0.708689770883341,1.)))
REPRESENTATION_ITEM('')
SURFACE()
);
#3332=(
BOUNDED_SURFACE()
B_SPLINE_SURFACE(3,2,((#242553,#242554,#242555),(#242556,#242557,#242558),
(#242559,#242560,#242561),(#242562,#242563,#242564)),.UNSPECIFIED.,.F.,
 .F.,.F.)
B_SPLINE_SURFACE_WITH_KNOTS((4,4),(3,3),(0.,0.000511815456479785),(0.,1.00105873159772),
 .UNSPECIFIED.)
GEOMETRIC_REPRESENTATION_ITEM()
RATIONAL_B_SPLINE_SURFACE(((1.,0.708394529056973,1.00061746385231),(1.,
0.708058564167544,1.0006181752456),(1.,0.707430835372716,1.00061950443822),
(1.,0.706796685881033,1.00062084722643)))
REPRESENTATION_ITEM('')
SURFACE()
);
#3333=(
BOUNDED_SURFACE()
B_SPLINE_SURFACE(3,2,((#242570,#242571,#242572),(#242573,#242574,#242575),
(#242576,#242577,#242578),(#242579,#242580,#242581)),.UNSPECIFIED.,.F.,
 .F.,.F.)
B_SPLINE_SURFACE_WITH_KNOTS((4,4),(3,3),(0.,0.0003973944654483),(0.,1.),
 .UNSPECIFIED.)
GEOMETRIC_REPRESENTATION_ITEM()
RATIONAL_B_SPLINE_SURFACE(((1.,0.705498956110768,1.),(1.,0.705821764811725,
1.),(1.,0.706461952521167,1.),(1.,0.707106781186562,1.)))
REPRESENTATION_ITEM('')
SURFACE()
);
#3334=(
BOUNDED_SURFACE()
B_SPLINE_SURFACE(3,2,((#242587,#242588,#242589),(#242590,#242591,#242592),
(#242593,#242594,#242595),(#242596,#242597,#242598)),.UNSPECIFIED.,.F.,
 .F.,.F.)
B_SPLINE_SURFACE_WITH_KNOTS((4,4),(3,3),(0.,0.000397394410828727),(0.,1.),
 .UNSPECIFIED.)
GEOMETRIC_REPRESENTATION_ITEM()
RATIONAL_B_SPLINE_SURFACE(((1.,0.708689770883342,1.),(1.,0.708376440034501,
1.),(1.,0.707750498698418,1.),(1.,0.707106781186535,1.)))
REPRESENTATION_ITEM('')
SURFACE()
);
#3335=(
BOUNDED_SURFACE()
B_SPLINE_SURFACE(3,2,((#242604,#242605,#242606),(#242607,#242608,#242609),
(#242610,#242611,#242612),(#242613,#242614,#242615)),.UNSPECIFIED.,.F.,
 .F.,.F.)
B_SPLINE_SURFACE_WITH_KNOTS((4,4),(3,3),(0.,0.000511815090126171),(0.,1.00105592270294),
 .UNSPECIFIED.)
GEOMETRIC_REPRESENTATION_ITEM()
RATIONAL_B_SPLINE_SURFACE(((1.,0.705266242717261,1.00062243213128),(1.,
0.70558408590891,1.00062176089559),(1.,0.706182089450261,1.00062049800456),
(1.,0.706797508587264,1.00061919833448)))
REPRESENTATION_ITEM('')
SURFACE()
);
#3336=(
BOUNDED_SURFACE()
B_SPLINE_SURFACE(3,2,((#242617,#242618,#242619),(#242620,#242621,#242622),
(#242623,#242624,#242625),(#242626,#242627,#242628)),.UNSPECIFIED.,.F.,
 .F.,.F.)
B_SPLINE_SURFACE_WITH_KNOTS((4,4),(3,3),(-5.09575021068187E-18,0.000397394428086616),
(0.,1.),.UNSPECIFIED.)
GEOMETRIC_REPRESENTATION_ITEM()
RATIONAL_B_SPLINE_SURFACE(((1.,0.707106781186535,1.),(1.,0.706459846759122,
1.),(1.,0.705820510737254,1.),(1.,0.705498956110735,1.)))
REPRESENTATION_ITEM('')
SURFACE()
);
#3337=(
BOUNDED_SURFACE()
B_SPLINE_SURFACE(3,2,((#242634,#242635,#242636),(#242637,#242638,#242639),
(#242640,#242641,#242642),(#242643,#242644,#242645),(#242646,#242647,#242648),
(#242649,#242650,#242651)),.UNSPECIFIED.,.F.,.F.,.F.)
B_SPLINE_SURFACE_WITH_KNOTS((4,2,4),(3,3),(0.,0.000257953807872844,0.000515907615745688),
(0.,1.),.UNSPECIFIED.)
GEOMETRIC_REPRESENTATION_ITEM()
RATIONAL_B_SPLINE_SURFACE(((1.,0.874619707139395,1.),(1.,0.87483434967913,
1.),(1.,0.854686104157619,1.),(1.,0.792476597915322,1.),(1.,0.750887854595009,
1.),(1.,0.705585838031439,1.)))
REPRESENTATION_ITEM('')
SURFACE()
);
#3338=(
BOUNDED_SURFACE()
B_SPLINE_SURFACE(3,2,((#242657,#242658,#242659),(#242660,#242661,#242662),
(#242663,#242664,#242665),(#242666,#242667,#242668)),.UNSPECIFIED.,.F.,
 .F.,.F.)
B_SPLINE_SURFACE_WITH_KNOTS((4,4),(3,3),(0.,0.000511815437699143),(0.,1.001058813316),
 .UNSPECIFIED.)
GEOMETRIC_REPRESENTATION_ITEM()
RATIONAL_B_SPLINE_SURFACE(((1.,0.706796661946313,1.00062089519725),(1.,
0.707430821225155,1.00061955228467),(1.,0.708058545830717,1.00061822299833),
(1.,0.708394505252681,1.00061751156171)))
REPRESENTATION_ITEM('')
SURFACE()
);
#3339=(
BOUNDED_SURFACE()
B_SPLINE_SURFACE(3,2,((#242670,#242671,#242672),(#242673,#242674,#242675),
(#242676,#242677,#242678),(#242679,#242680,#242681),(#242682,#242683,#242684),
(#242685,#242686,#242687)),.UNSPECIFIED.,.F.,.F.,.F.)
B_SPLINE_SURFACE_WITH_KNOTS((4,2,4),(3,3),(-6.50521303491303E-18,0.000256915317531246,
0.000513830635062499),(0.,1.),.UNSPECIFIED.)
GEOMETRIC_REPRESENTATION_ITEM()
RATIONAL_B_SPLINE_SURFACE(((1.,0.70558583803145,1.),(1.,0.750902433541874,
1.),(1.,0.792329530083662,1.),(1.,0.854288401593093,1.),(1.,0.874998031125971,
1.),(1.,0.874619707139399,1.)))
REPRESENTATION_ITEM('')
SURFACE()
);
#3340=(
BOUNDED_SURFACE()
B_SPLINE_SURFACE(3,2,((#242693,#242694,#242695),(#242696,#242697,#242698),
(#242699,#242700,#242701),(#242702,#242703,#242704),(#242705,#242706,#242707),
(#242708,#242709,#242710)),.UNSPECIFIED.,.F.,.F.,.F.)
B_SPLINE_SURFACE_WITH_KNOTS((4,2,4),(3,3),(-9.2970336290632E-18,0.000256592814262158,
0.000513185628524325),(0.,1.),.UNSPECIFIED.)
GEOMETRIC_REPRESENTATION_ITEM()
RATIONAL_B_SPLINE_SURFACE(((1.,0.70871252716368,1.),(1.,0.753780902613021,
1.),(1.,0.79453899576993,1.),(1.,0.855070770330385,1.),(1.,0.875018427445874,
1.),(1.,0.874619707139391,1.)))
REPRESENTATION_ITEM('')
SURFACE()
);
#3341=(
BOUNDED_SURFACE()
B_SPLINE_SURFACE(3,2,((#242712,#242713,#242714),(#242715,#242716,#242717),
(#242718,#242719,#242720),(#242721,#242722,#242723)),.UNSPECIFIED.,.F.,
 .F.,.F.)
B_SPLINE_SURFACE_WITH_KNOTS((4,4),(3,3),(-9.83913471530595E-18,0.0005118150724304),
(0.,1.00105598365781),.UNSPECIFIED.)
GEOMETRIC_REPRESENTATION_ITEM()
RATIONAL_B_SPLINE_SURFACE(((1.,0.706797490733999,1.00061923411643),(1.,
0.706182062146929,1.00062053388149),(1.,0.705584062769251,1.00062179683663),
(1.,0.705266224770772,1.00062246810009)))
REPRESENTATION_ITEM('')
SURFACE()
);
#3342=(
BOUNDED_SURFACE()
B_SPLINE_SURFACE(3,2,((#242729,#242730,#242731),(#242732,#242733,#242734),
(#242735,#242736,#242737),(#242738,#242739,#242740),(#242741,#242742,#242743),
(#242744,#242745,#242746)),.UNSPECIFIED.,.F.,.F.,.F.)
B_SPLINE_SURFACE_WITH_KNOTS((4,2,4),(3,3),(0.,0.000257652232350873,0.000515304464701747),
(0.,1.),.UNSPECIFIED.)
GEOMETRIC_REPRESENTATION_ITEM()
RATIONAL_B_SPLINE_SURFACE(((1.,0.874619707139395,1.),(1.,0.874861180430483,
1.),(1.,0.855455725921158,1.),(1.,0.794699358955009,1.),(1.,0.753768977788842,
1.),(1.,0.708712527163647,1.)))
REPRESENTATION_ITEM('')
SURFACE()
);
#3343=(
BOUNDED_SURFACE()
B_SPLINE_SURFACE(3,2,((#242752,#242753,#242754),(#242755,#242756,#242757),
(#242758,#242759,#242760),(#242761,#242762,#242763)),.UNSPECIFIED.,.F.,
 .F.,.F.)
B_SPLINE_SURFACE_WITH_KNOTS((4,4),(3,3),(-5.66495635123676E-18,0.000397394373651917),
(0.,1.),.UNSPECIFIED.)
GEOMETRIC_REPRESENTATION_ITEM()
RATIONAL_B_SPLINE_SURFACE(((1.,0.707106781186537,1.),(1.,0.707752587915902,
1.),(1.,0.70837765454068,1.),(1.,0.708689770883311,1.)))
REPRESENTATION_ITEM('')
SURFACE()
);
#3344=(
BOUNDED_SURFACE()
B_SPLINE_SURFACE(3,2,((#242765,#242766,#242767),(#242768,#242769,#242770),
(#242771,#242772,#242773),(#242774,#242775,#242776)),.UNSPECIFIED.,.F.,
 .F.,.F.)
B_SPLINE_SURFACE_WITH_KNOTS((4,4),(3,3),(0.,0.000511815456479785),(0.,1.00105873160024),
 .UNSPECIFIED.)
GEOMETRIC_REPRESENTATION_ITEM()
RATIONAL_B_SPLINE_SURFACE(((1.,0.708394529056231,1.00061746385378),(1.,
0.708058564166822,1.00061817524707),(1.,0.707430835371943,1.00061950443969),
(1.,0.706796685880296,1.00062084722791)))
REPRESENTATION_ITEM('')
SURFACE()
);
#3345=(
BOUNDED_SURFACE()
B_SPLINE_SURFACE(3,2,((#242782,#242783,#242784),(#242785,#242786,#242787),
(#242788,#242789,#242790),(#242791,#242792,#242793)),.UNSPECIFIED.,.F.,
 .F.,.F.)
B_SPLINE_SURFACE_WITH_KNOTS((4,4),(3,3),(0.,0.000397394465448315),(0.,1.),
 .UNSPECIFIED.)
GEOMETRIC_REPRESENTATION_ITEM()
RATIONAL_B_SPLINE_SURFACE(((1.,0.705498956110737,1.),(1.,0.705821764811864,
1.),(1.,0.706461952521089,1.),(1.,0.707106781186549,1.)))
REPRESENTATION_ITEM('')
SURFACE()
);
#3346=(
BOUNDED_SURFACE()
B_SPLINE_SURFACE(3,2,((#242799,#242800,#242801),(#242802,#242803,#242804),
(#242805,#242806,#242807),(#242808,#242809,#242810)),.UNSPECIFIED.,.F.,
 .F.,.F.)
B_SPLINE_SURFACE_WITH_KNOTS((4,4),(3,3),(0.,0.000397394410828729),(0.,1.),
 .UNSPECIFIED.)
GEOMETRIC_REPRESENTATION_ITEM()
RATIONAL_B_SPLINE_SURFACE(((1.,0.708689770883334,1.),(1.,0.708376440034477,
1.),(1.,0.70775049869843,1.),(1.,0.707106781186535,1.)))
REPRESENTATION_ITEM('')
SURFACE()
);
#3347=(
BOUNDED_SURFACE()
B_SPLINE_SURFACE(3,2,((#242816,#242817,#242818),(#242819,#242820,#242821),
(#242822,#242823,#242824),(#242825,#242826,#242827)),.UNSPECIFIED.,.F.,
 .F.,.F.)
B_SPLINE_SURFACE_WITH_KNOTS((4,4),(3,3),(0.,0.000511815090126169),(0.,1.00105592270366),
 .UNSPECIFIED.)
GEOMETRIC_REPRESENTATION_ITEM()
RATIONAL_B_SPLINE_SURFACE(((1.,0.705266242717034,1.0006224321317),(1.,0.705584085908732,
1.00062176089601),(1.,0.706182089450059,1.00062049800498),(1.,0.706797508587054,
1.0006191983349)))
REPRESENTATION_ITEM('')
SURFACE()
);
#3348=(
BOUNDED_SURFACE()
B_SPLINE_SURFACE(3,2,((#242829,#242830,#242831),(#242832,#242833,#242834),
(#242835,#242836,#242837),(#242838,#242839,#242840)),.UNSPECIFIED.,.F.,
 .F.,.F.)
B_SPLINE_SURFACE_WITH_KNOTS((4,4),(3,3),(-7.77915058758349E-18,0.00039739442808661),
(0.,1.),.UNSPECIFIED.)
GEOMETRIC_REPRESENTATION_ITEM()
RATIONAL_B_SPLINE_SURFACE(((1.,0.707106781186537,1.),(1.,0.706459846759104,
1.),(1.,0.70582051073728,1.),(1.,0.705498956110748,1.)))
REPRESENTATION_ITEM('')
SURFACE()
);
#3349=(
BOUNDED_SURFACE()
B_SPLINE_SURFACE(3,2,((#242846,#242847,#242848),(#242849,#242850,#242851),
(#242852,#242853,#242854),(#242855,#242856,#242857),(#242858,#242859,#242860),
(#242861,#242862,#242863)),.UNSPECIFIED.,.F.,.F.,.F.)
B_SPLINE_SURFACE_WITH_KNOTS((4,2,4),(3,3),(0.,0.000257953807872845,0.000515907615745691),
(0.,1.),.UNSPECIFIED.)
GEOMETRIC_REPRESENTATION_ITEM()
RATIONAL_B_SPLINE_SURFACE(((1.,0.874619707139393,1.),(1.,0.874834349679444,
1.),(1.,0.854686104157216,1.),(1.,0.792476597915716,1.),(1.,0.75088785459471,
1.),(1.,0.705585838031437,1.)))
REPRESENTATION_ITEM('')
SURFACE()
);
#3350=(
BOUNDED_SURFACE()
B_SPLINE_SURFACE(3,2,((#242869,#242870,#242871),(#242872,#242873,#242874),
(#242875,#242876,#242877),(#242878,#242879,#242880)),.UNSPECIFIED.,.F.,
 .F.,.F.)
B_SPLINE_SURFACE_WITH_KNOTS((4,4),(3,3),(-7.83336069620777E-18,0.000511815437699145),
(0.,1.00105881331516),.UNSPECIFIED.)
GEOMETRIC_REPRESENTATION_ITEM()
RATIONAL_B_SPLINE_SURFACE(((1.,0.706796661946547,1.00062089519676),(1.,
0.70743082122544,1.00061955228419),(1.,0.708058545830902,1.00061822299785),
(1.,0.708394505252928,1.00061751156123)))
REPRESENTATION_ITEM('')
SURFACE()
);
#3351=(
BOUNDED_SURFACE()
B_SPLINE_SURFACE(3,2,((#242882,#242883,#242884),(#242885,#242886,#242887),
(#242888,#242889,#242890),(#242891,#242892,#242893),(#242894,#242895,#242896),
(#242897,#242898,#242899)),.UNSPECIFIED.,.F.,.F.,.F.)
B_SPLINE_SURFACE_WITH_KNOTS((4,2,4),(3,3),(0.,0.000256915317531267,0.000513830635062534),
(0.,1.),.UNSPECIFIED.)
GEOMETRIC_REPRESENTATION_ITEM()
RATIONAL_B_SPLINE_SURFACE(((1.,0.705585838031457,1.),(1.,0.750902433542621,
1.),(1.,0.792329530082714,1.),(1.,0.854288401594055,1.),(1.,0.874998031125253,
1.),(1.,0.874619707139418,1.)))
REPRESENTATION_ITEM('')
SURFACE()
);
#3352=(
BOUNDED_SURFACE()
B_SPLINE_SURFACE(3,2,((#242905,#242906,#242907),(#242908,#242909,#242910),
(#242911,#242912,#242913),(#242914,#242915,#242916),(#242917,#242918,#242919),
(#242920,#242921,#242922)),.UNSPECIFIED.,.F.,.F.,.F.)
B_SPLINE_SURFACE_WITH_KNOTS((4,2,4),(3,3),(2.90024081139872E-18,0.000256592814262166,
0.000513185628524329),(0.,1.),.UNSPECIFIED.)
GEOMETRIC_REPRESENTATION_ITEM()
RATIONAL_B_SPLINE_SURFACE(((1.,0.708712527163643,1.),(1.,0.753780902613616,
1.),(1.,0.794538995769188,1.),(1.,0.855070770331141,1.),(1.,0.875018427445299,
1.),(1.,0.874619707139395,1.)))
REPRESENTATION_ITEM('')
SURFACE()
);
#3353=(
BOUNDED_SURFACE()
B_SPLINE_SURFACE(3,2,((#242924,#242925,#242926),(#242927,#242928,#242929),
(#242930,#242931,#242932),(#242933,#242934,#242935)),.UNSPECIFIED.,.F.,
 .F.,.F.)
B_SPLINE_SURFACE_WITH_KNOTS((4,4),(3,3),(0.,0.0005118150724304),(0.,1.00105598366053),
 .UNSPECIFIED.)
GEOMETRIC_REPRESENTATION_ITEM()
RATIONAL_B_SPLINE_SURFACE(((1.,0.706797490733202,1.00061923411802),(1.,
0.706182062146141,1.00062053388309),(1.,0.705584062768469,1.00062179683823),
(1.,0.705266224769957,1.0006224681017)))
REPRESENTATION_ITEM('')
SURFACE()
);
#3354=(
BOUNDED_SURFACE()
B_SPLINE_SURFACE(3,2,((#242941,#242942,#242943),(#242944,#242945,#242946),
(#242947,#242948,#242949),(#242950,#242951,#242952),(#242953,#242954,#242955),
(#242956,#242957,#242958)),.UNSPECIFIED.,.F.,.F.,.F.)
B_SPLINE_SURFACE_WITH_KNOTS((4,2,4),(3,3),(2.84603070277445E-18,0.000257652232350877,
0.000515304464701752),(0.,1.),.UNSPECIFIED.)
GEOMETRIC_REPRESENTATION_ITEM()
RATIONAL_B_SPLINE_SURFACE(((1.,0.87461970713938,1.),(1.,0.874861180430414,
1.),(1.,0.855455725921217,1.),(1.,0.794699358954895,1.),(1.,0.753768977788904,
1.),(1.,0.708712527163652,1.)))
REPRESENTATION_ITEM('')
SURFACE()
);
#3355=(
BOUNDED_SURFACE()
B_SPLINE_SURFACE(3,2,((#242964,#242965,#242966),(#242967,#242968,#242969),
(#242970,#242971,#242972),(#242973,#242974,#242975)),.UNSPECIFIED.,.F.,
 .F.,.F.)
B_SPLINE_SURFACE_WITH_KNOTS((4,4),(3,3),(-5.42101086242752E-20,0.000397394373651934),
(0.,1.),.UNSPECIFIED.)
GEOMETRIC_REPRESENTATION_ITEM()
RATIONAL_B_SPLINE_SURFACE(((1.,0.70710678118654,1.),(1.,0.707752587915909,
1.),(1.,0.708377654540641,1.),(1.,0.708689770883352,1.)))
REPRESENTATION_ITEM('')
SURFACE()
);
#3356=(
BOUNDED_SURFACE()
B_SPLINE_SURFACE(3,2,((#242977,#242978,#242979),(#242980,#242981,#242982),
(#242983,#242984,#242985),(#242986,#242987,#242988)),.UNSPECIFIED.,.F.,
 .F.,.F.)
B_SPLINE_SURFACE_WITH_KNOTS((4,4),(3,3),(-2.00577401909818E-18,0.000511815456479787),
(0.,1.00105873160032),.UNSPECIFIED.)
GEOMETRIC_REPRESENTATION_ITEM()
RATIONAL_B_SPLINE_SURFACE(((1.,0.708394529056217,1.00061746385383),(1.,
0.708058564166775,1.00061817524712),(1.,0.707430835371947,1.00061950443974),
(1.,0.70679668588027,1.00062084722796)))
REPRESENTATION_ITEM('')
SURFACE()
);
#3357=(
BOUNDED_SURFACE()
B_SPLINE_SURFACE(3,2,((#242994,#242995,#242996),(#242997,#242998,#242999),
(#243000,#243001,#243002),(#243003,#243004,#243005)),.UNSPECIFIED.,.F.,
 .F.,.F.)
B_SPLINE_SURFACE_WITH_KNOTS((4,4),(3,3),(0.,0.000397394465448307),(0.,1.),
 .UNSPECIFIED.)
GEOMETRIC_REPRESENTATION_ITEM()
RATIONAL_B_SPLINE_SURFACE(((1.,0.705498956110759,1.),(1.,0.705821764811783,
1.),(1.,0.706461952521134,1.),(1.,0.70710678118655,1.)))
REPRESENTATION_ITEM('')
SURFACE()
);
#3358=(
BOUNDED_SURFACE()
B_SPLINE_SURFACE(3,2,((#243011,#243012,#243013),(#243014,#243015,#243016),
(#243017,#243018,#243019),(#243020,#243021,#243022)),.UNSPECIFIED.,.F.,
 .F.,.F.)
B_SPLINE_SURFACE_WITH_KNOTS((4,4),(3,3),(0.,0.000397394410828732),(0.,1.),
 .UNSPECIFIED.)
GEOMETRIC_REPRESENTATION_ITEM()
RATIONAL_B_SPLINE_SURFACE(((1.,0.708689770883336,1.),(1.,0.708376440034493,
1.),(1.,0.707750498698416,1.),(1.,0.707106781186546,1.)))
REPRESENTATION_ITEM('')
SURFACE()
);
#3359=(
BOUNDED_SURFACE()
B_SPLINE_SURFACE(3,2,((#243028,#243029,#243030),(#243031,#243032,#243033),
(#243034,#243035,#243036),(#243037,#243038,#243039)),.UNSPECIFIED.,.F.,
 .F.,.F.)
B_SPLINE_SURFACE_WITH_KNOTS((4,4),(3,3),(0.,0.000511815090126173),(0.,1.00105592270393),
 .UNSPECIFIED.)
GEOMETRIC_REPRESENTATION_ITEM()
RATIONAL_B_SPLINE_SURFACE(((1.,0.705266242716976,1.00062243213186),(1.,
0.7055840859086,1.00062176089618),(1.,0.706182089450005,1.00062049800514),
(1.,0.706797508586974,1.00061919833506)))
REPRESENTATION_ITEM('')
SURFACE()
);
#3360=(
BOUNDED_SURFACE()
B_SPLINE_SURFACE(3,2,((#243041,#243042,#243043),(#243044,#243045,#243046),
(#243047,#243048,#243049),(#243050,#243051,#243052)),.UNSPECIFIED.,.F.,
 .F.,.F.)
B_SPLINE_SURFACE_WITH_KNOTS((4,4),(3,3),(-1.51246203061728E-17,0.000397394428086612),
(0.,1.),.UNSPECIFIED.)
GEOMETRIC_REPRESENTATION_ITEM()
RATIONAL_B_SPLINE_SURFACE(((1.,0.707106781186538,1.),(1.,0.706459846759089,
1.),(1.,0.705820510737279,1.),(1.,0.70549895611075,1.)))
REPRESENTATION_ITEM('')
SURFACE()
);
#3361=(
BOUNDED_SURFACE()
B_SPLINE_SURFACE(3,2,((#243058,#243059,#243060),(#243061,#243062,#243063),
(#243064,#243065,#243066),(#243067,#243068,#243069),(#243070,#243071,#243072),
(#243073,#243074,#243075)),.UNSPECIFIED.,.F.,.F.,.F.)
B_SPLINE_SURFACE_WITH_KNOTS((4,2,4),(3,3),(0.,0.000257953807872853,0.000515907615745706),
(0.,1.),.UNSPECIFIED.)
GEOMETRIC_REPRESENTATION_ITEM()
RATIONAL_B_SPLINE_SURFACE(((1.,0.874619707139391,1.),(1.,0.874834349679083,
1.),(1.,0.85468610415769,1.),(1.,0.79247659791523,1.),(1.,0.750887854595076,
1.),(1.,0.705585838031431,1.)))
REPRESENTATION_ITEM('')
SURFACE()
);
#3362=(
BOUNDED_SURFACE()
B_SPLINE_SURFACE(3,2,((#243081,#243082,#243083),(#243084,#243085,#243086),
(#243087,#243088,#243089),(#243090,#243091,#243092)),.UNSPECIFIED.,.F.,
 .F.,.F.)
B_SPLINE_SURFACE_WITH_KNOTS((4,4),(3,3),(-8.13151629364128E-20,0.00051181543769915),
(0.,1.00105881331554),.UNSPECIFIED.)
GEOMETRIC_REPRESENTATION_ITEM()
RATIONAL_B_SPLINE_SURFACE(((1.,0.706796661946445,1.00062089519698),(1.,
0.707430821225321,1.0006195522844),(1.,0.708058545830804,1.00061822299806),
(1.,0.708394505252852,1.00061751156144)))
REPRESENTATION_ITEM('')
SURFACE()
);
#3363=(
BOUNDED_SURFACE()
B_SPLINE_SURFACE(3,2,((#243094,#243095,#243096),(#243097,#243098,#243099),
(#243100,#243101,#243102),(#243103,#243104,#243105),(#243106,#243107,#243108),
(#243109,#243110,#243111)),.UNSPECIFIED.,.F.,.F.,.F.)
B_SPLINE_SURFACE_WITH_KNOTS((4,2,4),(3,3),(-1.05709711817337E-18,0.000256915317531255,
0.000513830635062511),(0.,1.),.UNSPECIFIED.)
GEOMETRIC_REPRESENTATION_ITEM()
RATIONAL_B_SPLINE_SURFACE(((1.,0.705585838031441,1.),(1.,0.750902433542587,
1.),(1.,0.792329530082719,1.),(1.,0.854288401594003,1.),(1.,0.874998031125281,
1.),(1.,0.874619707139393,1.)))
REPRESENTATION_ITEM('')
SURFACE()
);
#3364=(
BOUNDED_SURFACE()
B_SPLINE_SURFACE(3,2,((#243117,#243118,#243119),(#243120,#243121,#243122),
(#243123,#243124,#243125),(#243126,#243127,#243128),(#243129,#243130,#243131),
(#243132,#243133,#243134)),.UNSPECIFIED.,.F.,.F.,.F.)
B_SPLINE_SURFACE_WITH_KNOTS((4,2,4),(3,3),(0.,0.000256592814262157,0.000513185628524314),
(0.,1.),.UNSPECIFIED.)
GEOMETRIC_REPRESENTATION_ITEM()
RATIONAL_B_SPLINE_SURFACE(((1.,0.708712527163663,1.),(1.,0.753780902613579,
1.),(1.,0.794538995769226,1.),(1.,0.855070770331072,1.),(1.,0.875018427445355,
1.),(1.,0.874619707139399,1.)))
REPRESENTATION_ITEM('')
SURFACE()
);
#3365=(
BOUNDED_SURFACE()
B_SPLINE_SURFACE(3,2,((#243136,#243137,#243138),(#243139,#243140,#243141),
(#243142,#243143,#243144),(#243145,#243146,#243147)),.UNSPECIFIED.,.F.,
 .F.,.F.)
B_SPLINE_SURFACE_WITH_KNOTS((4,4),(3,3),(-7.83336069620777E-18,0.000511815072430394),
(0.,1.00105598366044),.UNSPECIFIED.)
GEOMETRIC_REPRESENTATION_ITEM()
RATIONAL_B_SPLINE_SURFACE(((1.,0.706797490733229,1.00061923411797),(1.,
0.706182062146136,1.00062053388303),(1.,0.705584062768512,1.00062179683818),
(1.,0.705266224769987,1.00062246810164)))
REPRESENTATION_ITEM('')
SURFACE()
);
#3366=(
BOUNDED_SURFACE()
B_SPLINE_SURFACE(3,2,((#243153,#243154,#243155),(#243156,#243157,#243158),
(#243159,#243160,#243161),(#243162,#243163,#243164),(#243165,#243166,#243167),
(#243168,#243169,#243170)),.UNSPECIFIED.,.F.,.F.,.F.)
B_SPLINE_SURFACE_WITH_KNOTS((4,2,4),(3,3),(-5.42101086242752E-20,0.000257652232350883,
0.000515304464701767),(0.,1.),.UNSPECIFIED.)
GEOMETRIC_REPRESENTATION_ITEM()
RATIONAL_B_SPLINE_SURFACE(((1.,0.874619707139392,1.),(1.,0.874861180430363,
1.),(1.,0.855455725921355,1.),(1.,0.794699358954803,1.),(1.,0.753768977788994,
1.),(1.,0.708712527163659,1.)))
REPRESENTATION_ITEM('')
SURFACE()
);
#3367=(
BOUNDED_SURFACE()
B_SPLINE_SURFACE(3,2,((#243176,#243177,#243178),(#243179,#243180,#243181),
(#243182,#243183,#243184),(#243185,#243186,#243187)),.UNSPECIFIED.,.F.,
 .F.,.F.)
B_SPLINE_SURFACE_WITH_KNOTS((4,4),(3,3),(-5.42101086242752E-20,0.000397394373651941),
(0.,1.),.UNSPECIFIED.)
GEOMETRIC_REPRESENTATION_ITEM()
RATIONAL_B_SPLINE_SURFACE(((1.,0.707106781186548,1.),(1.,0.707752587915896,
1.),(1.,0.708377654540676,1.),(1.,0.708689770883328,1.)))
REPRESENTATION_ITEM('')
SURFACE()
);
#3368=(
BOUNDED_SURFACE()
B_SPLINE_SURFACE(3,2,((#243189,#243190,#243191),(#243192,#243193,#243194),
(#243195,#243196,#243197),(#243198,#243199,#243200)),.UNSPECIFIED.,.F.,
 .F.,.F.)
B_SPLINE_SURFACE_WITH_KNOTS((4,4),(3,3),(0.,0.000511815456479789),(0.,1.00105873159835),
 .UNSPECIFIED.)
GEOMETRIC_REPRESENTATION_ITEM()
RATIONAL_B_SPLINE_SURFACE(((1.,0.708394529056799,1.00061746385268),(1.,
0.708058564167347,1.00061817524597),(1.,0.707430835372527,1.00061950443859),
(1.,0.706796685880849,1.0006208472268)))
REPRESENTATION_ITEM('')
SURFACE()
);
#3369=(
BOUNDED_SURFACE()
B_SPLINE_SURFACE(3,2,((#243206,#243207,#243208),(#243209,#243210,#243211),
(#243212,#243213,#243214),(#243215,#243216,#243217)),.UNSPECIFIED.,.F.,
 .F.,.F.)
B_SPLINE_SURFACE_WITH_KNOTS((4,4),(3,3),(0.,0.000397394465448313),(0.,1.),
 .UNSPECIFIED.)
GEOMETRIC_REPRESENTATION_ITEM()
RATIONAL_B_SPLINE_SURFACE(((1.,0.705498956110762,1.),(1.,0.705821764811743,
1.),(1.,0.706461952521185,1.),(1.,0.707106781186556,1.)))
REPRESENTATION_ITEM('')
SURFACE()
);
#3370=(
BOUNDED_SURFACE()
B_SPLINE_SURFACE(3,2,((#243223,#243224,#243225),(#243226,#243227,#243228),
(#243229,#243230,#243231),(#243232,#243233,#243234)),.UNSPECIFIED.,.F.,
 .F.,.F.)
B_SPLINE_SURFACE_WITH_KNOTS((4,4),(3,3),(3.25260651745651E-18,0.000397394410828723),
(0.,1.),.UNSPECIFIED.)
GEOMETRIC_REPRESENTATION_ITEM()
RATIONAL_B_SPLINE_SURFACE(((1.,0.708689770883334,1.),(1.,0.708376440034478,
1.),(1.,0.707750498698416,1.),(1.,0.70710678118654,1.)))
REPRESENTATION_ITEM('')
SURFACE()
);
#3371=(
BOUNDED_SURFACE()
B_SPLINE_SURFACE(3,2,((#243240,#243241,#243242),(#243243,#243244,#243245),
(#243246,#243247,#243248),(#243249,#243250,#243251)),.UNSPECIFIED.,.F.,
 .F.,.F.)
B_SPLINE_SURFACE_WITH_KNOTS((4,4),(3,3),(-5.20417042793042E-18,0.00051181509012618),
(0.,1.00105592270183),.UNSPECIFIED.)
GEOMETRIC_REPRESENTATION_ITEM()
RATIONAL_B_SPLINE_SURFACE(((1.,0.705266242717577,1.00062243213062),(1.,
0.705584085909256,1.00062176089494),(1.,0.706182089450602,1.0006204980039),
(1.,0.706797508587584,1.00061919833383)))
REPRESENTATION_ITEM('')
SURFACE()
);
#3372=(
BOUNDED_SURFACE()
B_SPLINE_SURFACE(3,2,((#243253,#243254,#243255),(#243256,#243257,#243258),
(#243259,#243260,#243261),(#243262,#243263,#243264)),.UNSPECIFIED.,.F.,
 .F.,.F.)
B_SPLINE_SURFACE_WITH_KNOTS((4,4),(3,3),(0.,0.000397394428086615),(0.,1.),
 .UNSPECIFIED.)
GEOMETRIC_REPRESENTATION_ITEM()
RATIONAL_B_SPLINE_SURFACE(((1.,0.70710678118654,1.),(1.,0.706459846759078,
1.),(1.,0.705820510737278,1.),(1.,0.705498956110748,1.)))
REPRESENTATION_ITEM('')
SURFACE()
);
#3373=(
BOUNDED_SURFACE()
B_SPLINE_SURFACE(3,2,((#243270,#243271,#243272),(#243273,#243274,#243275),
(#243276,#243277,#243278),(#243279,#243280,#243281),(#243282,#243283,#243284),
(#243285,#243286,#243287)),.UNSPECIFIED.,.F.,.F.,.F.)
B_SPLINE_SURFACE_WITH_KNOTS((4,2,4),(3,3),(0.,0.000257953807872844,0.000515907615745689),
(0.,1.),.UNSPECIFIED.)
GEOMETRIC_REPRESENTATION_ITEM()
RATIONAL_B_SPLINE_SURFACE(((1.,0.874619707139402,1.),(1.,0.874834349679007,
1.),(1.,0.854686104157788,1.),(1.,0.792476597915144,1.),(1.,0.750887854595137,
1.),(1.,0.70558583803144,1.)))
REPRESENTATION_ITEM('')
SURFACE()
);
#3374=(
BOUNDED_SURFACE()
B_SPLINE_SURFACE(3,2,((#243293,#243294,#243295),(#243296,#243297,#243298),
(#243299,#243300,#243301),(#243302,#243303,#243304)),.UNSPECIFIED.,.F.,
 .F.,.F.)
B_SPLINE_SURFACE_WITH_KNOTS((4,4),(3,3),(-7.80625564189563E-18,0.000511815437699149),
(0.,1.00105881331508),.UNSPECIFIED.)
GEOMETRIC_REPRESENTATION_ITEM()
RATIONAL_B_SPLINE_SURFACE(((1.,0.706796661946571,1.00062089519671),(1.,
0.707430821225453,1.00061955228413),(1.,0.708058545830938,1.00061822299779),
(1.,0.708394505252939,1.00061751156117)))
REPRESENTATION_ITEM('')
SURFACE()
);
#3375=(
BOUNDED_SURFACE()
B_SPLINE_SURFACE(3,2,((#243306,#243307,#243308),(#243309,#243310,#243311),
(#243312,#243313,#243314),(#243315,#243316,#243317),(#243318,#243319,#243320),
(#243321,#243322,#243323)),.UNSPECIFIED.,.F.,.F.,.F.)
B_SPLINE_SURFACE_WITH_KNOTS((4,2,4),(3,3),(-2.87313575708659E-18,0.000256915317531263,
0.000513830635062528),(0.,1.),.UNSPECIFIED.)
GEOMETRIC_REPRESENTATION_ITEM()
RATIONAL_B_SPLINE_SURFACE(((1.,0.70558583803146,1.),(1.,0.750902433542788,
1.),(1.,0.792329530082522,1.),(1.,0.854288401594226,1.),(1.,0.874998031125156,
1.),(1.,0.874619707139415,1.)))
REPRESENTATION_ITEM('')
SURFACE()
);
#3376=(
BOUNDED_SURFACE()
B_SPLINE_SURFACE(3,2,((#243329,#243330,#243331),(#243332,#243333,#243334),
(#243335,#243336,#243337),(#243338,#243339,#243340),(#243341,#243342,#243343),
(#243344,#243345,#243346)),.UNSPECIFIED.,.F.,.F.,.F.)
B_SPLINE_SURFACE_WITH_KNOTS((4,2,4),(3,3),(-2.24971950790742E-18,0.000256592814262159,
0.00051318562852432),(0.,1.),.UNSPECIFIED.)
GEOMETRIC_REPRESENTATION_ITEM()
RATIONAL_B_SPLINE_SURFACE(((1.,0.708712527163664,1.),(1.,0.753780902613397,
1.),(1.,0.794538995769452,1.),(1.,0.85507077033087,1.),(1.,0.875018427445515,
1.),(1.,0.874619707139393,1.)))
REPRESENTATION_ITEM('')
SURFACE()
);
#3377=(
BOUNDED_SURFACE()
B_SPLINE_SURFACE(3,2,((#243348,#243349,#243350),(#243351,#243352,#243353),
(#243354,#243355,#243356),(#243357,#243358,#243359)),.UNSPECIFIED.,.F.,
 .F.,.F.)
B_SPLINE_SURFACE_WITH_KNOTS((4,4),(3,3),(-7.75204553327136E-18,0.000511815072430404),
(0.,1.00105598365717),.UNSPECIFIED.)
GEOMETRIC_REPRESENTATION_ITEM()
RATIONAL_B_SPLINE_SURFACE(((1.,0.70679749073418,1.00061923411605),(1.,0.706182062147123,
1.00062053388111),(1.,0.705584062769471,1.00062179683625),(1.,0.705266224770931,
1.00062246809971)))
REPRESENTATION_ITEM('')
SURFACE()
);
#3378=(
BOUNDED_SURFACE()
B_SPLINE_SURFACE(3,2,((#243365,#243366,#243367),(#243368,#243369,#243370),
(#243371,#243372,#243373),(#243374,#243375,#243376),(#243377,#243378,#243379),
(#243380,#243381,#243382)),.UNSPECIFIED.,.F.,.F.,.F.)
B_SPLINE_SURFACE_WITH_KNOTS((4,2,4),(3,3),(0.,0.000257652232350885,0.000515304464701769),
(0.,1.),.UNSPECIFIED.)
GEOMETRIC_REPRESENTATION_ITEM()
RATIONAL_B_SPLINE_SURFACE(((1.,0.874619707139384,1.),(1.,0.874861180430819,
1.),(1.,0.855455725920674,1.),(1.,0.794699358955418,1.),(1.,0.753768977788512,
1.),(1.,0.70871252716364,1.)))
REPRESENTATION_ITEM('')
SURFACE()
);
#3379=(
BOUNDED_SURFACE()
B_SPLINE_SURFACE(3,2,((#243388,#243389,#243390),(#243391,#243392,#243393),
(#243394,#243395,#243396),(#243397,#243398,#243399)),.UNSPECIFIED.,.F.,
 .F.,.F.)
B_SPLINE_SURFACE_WITH_KNOTS((4,4),(3,3),(-8.37546178245052E-18,0.000397394373651906),
(0.,1.),.UNSPECIFIED.)
GEOMETRIC_REPRESENTATION_ITEM()
RATIONAL_B_SPLINE_SURFACE(((1.,0.707106781186549,1.),(1.,0.707752587915899,
1.),(1.,0.708377654540661,1.),(1.,0.708689770883328,1.)))
REPRESENTATION_ITEM('')
SURFACE()
);
#3380=(
BOUNDED_SURFACE()
B_SPLINE_SURFACE(3,2,((#243401,#243402,#243403),(#243404,#243405,#243406),
(#243407,#243408,#243409),(#243410,#243411,#243412)),.UNSPECIFIED.,.F.,
 .F.,.F.)
B_SPLINE_SURFACE_WITH_KNOTS((4,4),(3,3),(0.,0.000511815456479786),(0.,1.00105873159754),
 .UNSPECIFIED.)
GEOMETRIC_REPRESENTATION_ITEM()
RATIONAL_B_SPLINE_SURFACE(((1.,0.708394529057023,1.00061746385221),(1.,
0.708058564167585,1.0006181752455),(1.,0.707430835372759,1.00061950443811),
(1.,0.706796685881085,1.00062084722632)))
REPRESENTATION_ITEM('')
SURFACE()
);
#3381=(
BOUNDED_SURFACE()
B_SPLINE_SURFACE(3,2,((#243418,#243419,#243420),(#243421,#243422,#243423),
(#243424,#243425,#243426),(#243427,#243428,#243429)),.UNSPECIFIED.,.F.,
 .F.,.F.)
B_SPLINE_SURFACE_WITH_KNOTS((4,4),(3,3),(-3.25260651745651E-18,0.000397394465448296),
(0.,1.),.UNSPECIFIED.)
GEOMETRIC_REPRESENTATION_ITEM()
RATIONAL_B_SPLINE_SURFACE(((1.,0.705498956110763,1.),(1.,0.705821764811817,
1.),(1.,0.70646195252111,1.),(1.,0.707106781186561,1.)))
REPRESENTATION_ITEM('')
SURFACE()
);
#3382=(
BOUNDED_SURFACE()
B_SPLINE_SURFACE(3,2,((#243435,#243436,#243437),(#243438,#243439,#243440),
(#243441,#243442,#243443),(#243444,#243445,#243446)),.UNSPECIFIED.,.F.,
 .F.,.F.)
B_SPLINE_SURFACE_WITH_KNOTS((4,4),(3,3),(0.,0.000397394410828747),(0.,1.),
 .UNSPECIFIED.)
GEOMETRIC_REPRESENTATION_ITEM()
RATIONAL_B_SPLINE_SURFACE(((1.,0.708689770883334,1.),(1.,0.708376440034482,
1.),(1.,0.707750498698421,1.),(1.,0.707106781186548,1.)))
REPRESENTATION_ITEM('')
SURFACE()
);
#3383=(
BOUNDED_SURFACE()
B_SPLINE_SURFACE(3,2,((#243452,#243453,#243454),(#243455,#243456,#243457),
(#243458,#243459,#243460),(#243461,#243462,#243463)),.UNSPECIFIED.,.F.,
 .F.,.F.)
B_SPLINE_SURFACE_WITH_KNOTS((4,4),(3,3),(0.,0.000511815090126157),(0.,1.00105592270313),
 .UNSPECIFIED.)
GEOMETRIC_REPRESENTATION_ITEM()
RATIONAL_B_SPLINE_SURFACE(((1.,0.705266242717223,1.00062243213138),(1.,
0.705584085908876,1.0006217608957),(1.,0.706182089450213,1.00062049800467),
(1.,0.706797508587211,1.00061919833459)))
REPRESENTATION_ITEM('')
SURFACE()
);
#3384=(
BOUNDED_SURFACE()
B_SPLINE_SURFACE(3,2,((#243465,#243466,#243467),(#243468,#243469,#243470),
(#243471,#243472,#243473),(#243474,#243475,#243476)),.UNSPECIFIED.,.F.,
 .F.,.F.)
B_SPLINE_SURFACE_WITH_KNOTS((4,4),(3,3),(0.,0.000397394428086609),(0.,1.),
 .UNSPECIFIED.)
GEOMETRIC_REPRESENTATION_ITEM()
RATIONAL_B_SPLINE_SURFACE(((1.,0.707106781186544,1.),(1.,0.706459846759089,
1.),(1.,0.705820510737274,1.),(1.,0.705498956110742,1.)))
REPRESENTATION_ITEM('')
SURFACE()
);
#3385=(
BOUNDED_SURFACE()
B_SPLINE_SURFACE(3,2,((#243482,#243483,#243484),(#243485,#243486,#243487),
(#243488,#243489,#243490),(#243491,#243492,#243493),(#243494,#243495,#243496),
(#243497,#243498,#243499)),.UNSPECIFIED.,.F.,.F.,.F.)
B_SPLINE_SURFACE_WITH_KNOTS((4,2,4),(3,3),(0.,0.000257953807872844,0.000515907615745688),
(0.,1.),.UNSPECIFIED.)
GEOMETRIC_REPRESENTATION_ITEM()
RATIONAL_B_SPLINE_SURFACE(((1.,0.874619707139395,1.),(1.,0.874834349678822,
1.),(1.,0.854686104158037,1.),(1.,0.792476597914894,1.),(1.,0.750887854595317,
1.),(1.,0.705585838031437,1.)))
REPRESENTATION_ITEM('')
SURFACE()
);
#3386=(
BOUNDED_SURFACE()
B_SPLINE_SURFACE(3,2,((#243505,#243506,#243507),(#243508,#243509,#243510),
(#243511,#243512,#243513),(#243514,#243515,#243516)),.UNSPECIFIED.,.F.,
 .F.,.F.)
B_SPLINE_SURFACE_WITH_KNOTS((4,4),(3,3),(-6.7762635780344E-19,0.000511815437699156),
(0.,1.00105881331755),.UNSPECIFIED.)
GEOMETRIC_REPRESENTATION_ITEM()
RATIONAL_B_SPLINE_SURFACE(((1.,0.706796661945847,1.00062089519816),(1.,
0.707430821224722,1.00061955228558),(1.,0.708058545830208,1.00061822299924),
(1.,0.708394505252233,1.00061751156262)))
REPRESENTATION_ITEM('')
SURFACE()
);
#3387=(
BOUNDED_SURFACE()
B_SPLINE_SURFACE(3,2,((#243518,#243519,#243520),(#243521,#243522,#243523),
(#243524,#243525,#243526),(#243527,#243528,#243529),(#243530,#243531,#243532),
(#243533,#243534,#243535)),.UNSPECIFIED.,.F.,.F.,.F.)
B_SPLINE_SURFACE_WITH_KNOTS((4,2,4),(3,3),(-2.71050543121376E-20,0.000256915317531267,
0.000513830635062534),(0.,1.),.UNSPECIFIED.)
GEOMETRIC_REPRESENTATION_ITEM()
RATIONAL_B_SPLINE_SURFACE(((1.,0.705585838031452,1.),(1.,0.750902433542858,
1.),(1.,0.792329530082393,1.),(1.,0.854288401594359,1.),(1.,0.874998031125022,
1.),(1.,0.874619707139412,1.)))
REPRESENTATION_ITEM('')
SURFACE()
);
#3388=(
BOUNDED_SURFACE()
B_SPLINE_SURFACE(3,2,((#243541,#243542,#243543),(#243544,#243545,#243546),
(#243547,#243548,#243549),(#243550,#243551,#243552),(#243553,#243554,#243555),
(#243556,#243557,#243558)),.UNSPECIFIED.,.F.,.F.,.F.)
B_SPLINE_SURFACE_WITH_KNOTS((4,2,4),(3,3),(0.,0.00025659281426216,0.00051318562852432),
(0.,1.),.UNSPECIFIED.)
GEOMETRIC_REPRESENTATION_ITEM()
RATIONAL_B_SPLINE_SURFACE(((1.,0.708712527163661,1.),(1.,0.753780902613585,
1.),(1.,0.794538995769198,1.),(1.,0.855070770331121,1.),(1.,0.875018427445309,
1.),(1.,0.874619707139393,1.)))
REPRESENTATION_ITEM('')
SURFACE()
);
#3389=(
BOUNDED_SURFACE()
B_SPLINE_SURFACE(3,2,((#243560,#243561,#243562),(#243563,#243564,#243565),
(#243566,#243567,#243568),(#243569,#243570,#243571)),.UNSPECIFIED.,.F.,
 .F.,.F.)
B_SPLINE_SURFACE_WITH_KNOTS((4,4),(3,3),(5.96311194867027E-19,0.000511815072430393),
(0.,1.00105598365635),.UNSPECIFIED.)
GEOMETRIC_REPRESENTATION_ITEM()
RATIONAL_B_SPLINE_SURFACE(((1.,0.706797490734424,1.00061923411557),(1.,
0.706182062147336,1.00062053388063),(1.,0.705584062769713,1.00062179683577),
(1.,0.705266224771183,1.00062246809923)))
REPRESENTATION_ITEM('')
SURFACE()
);
#3390=(
BOUNDED_SURFACE()
B_SPLINE_SURFACE(3,2,((#243577,#243578,#243579),(#243580,#243581,#243582),
(#243583,#243584,#243585),(#243586,#243587,#243588),(#243589,#243590,#243591),
(#243592,#243593,#243594)),.UNSPECIFIED.,.F.,.F.,.F.)
B_SPLINE_SURFACE_WITH_KNOTS((4,2,4),(3,3),(0.,0.000257652232350886,0.000515304464701771),
(0.,1.),.UNSPECIFIED.)
GEOMETRIC_REPRESENTATION_ITEM()
RATIONAL_B_SPLINE_SURFACE(((1.,0.874619707139397,1.),(1.,0.874861180431091,
1.),(1.,0.85545572592034,1.),(1.,0.794699358955775,1.),(1.,0.75376897778827,
1.),(1.,0.708712527163653,1.)))
REPRESENTATION_ITEM('')
SURFACE()
);
#3391=(
BOUNDED_SURFACE()
B_SPLINE_SURFACE(3,2,((#243600,#243601,#243602),(#243603,#243604,#243605),
(#243606,#243607,#243608),(#243609,#243610,#243611)),.UNSPECIFIED.,.F.,
 .F.,.F.)
B_SPLINE_SURFACE_WITH_KNOTS((4,4),(3,3),(0.,0.000397394373651917),(0.,1.),
 .UNSPECIFIED.)
GEOMETRIC_REPRESENTATION_ITEM()
RATIONAL_B_SPLINE_SURFACE(((1.,0.707106781186548,1.),(1.,0.707752587915883,
1.),(1.,0.708377654540707,1.),(1.,0.70868977088332,1.)))
REPRESENTATION_ITEM('')
SURFACE()
);
#3392=(
BOUNDED_SURFACE()
B_SPLINE_SURFACE(3,2,((#243613,#243614,#243615),(#243616,#243617,#243618),
(#243619,#243620,#243621),(#243622,#243623,#243624)),.UNSPECIFIED.,.F.,
 .F.,.F.)
B_SPLINE_SURFACE_WITH_KNOTS((4,4),(3,3),(-8.02309607639273E-18,0.000511815456479797),
(0.,1.0010587315978),.UNSPECIFIED.)
GEOMETRIC_REPRESENTATION_ITEM()
RATIONAL_B_SPLINE_SURFACE(((1.,0.708394529056956,1.00061746385236),(1.,
0.708058564167499,1.00061817524565),(1.,0.707430835372702,1.00061950443827),
(1.,0.706796685881003,1.00062084722648)))
REPRESENTATION_ITEM('')
SURFACE()
);
#3393=(
BOUNDED_SURFACE()
B_SPLINE_SURFACE(3,2,((#243630,#243631,#243632),(#243633,#243634,#243635),
(#243636,#243637,#243638),(#243639,#243640,#243641)),.UNSPECIFIED.,.F.,
 .F.,.F.)
B_SPLINE_SURFACE_WITH_KNOTS((4,4),(3,3),(0.,0.000397394465448314),(0.,1.),
 .UNSPECIFIED.)
GEOMETRIC_REPRESENTATION_ITEM()
RATIONAL_B_SPLINE_SURFACE(((1.,0.705498956110746,1.),(1.,0.705821764811783,
1.),(1.,0.706461952521148,1.),(1.,0.707106781186544,1.)))
REPRESENTATION_ITEM('')
SURFACE()
);
#3394=(
BOUNDED_SURFACE()
B_SPLINE_SURFACE(3,2,((#243647,#243648,#243649),(#243650,#243651,#243652),
(#243653,#243654,#243655),(#243656,#243657,#243658)),.UNSPECIFIED.,.F.,
 .F.,.F.)
B_SPLINE_SURFACE_WITH_KNOTS((4,4),(3,3),(0.,0.000397394410828735),(0.,1.),
 .UNSPECIFIED.)
GEOMETRIC_REPRESENTATION_ITEM()
RATIONAL_B_SPLINE_SURFACE(((1.,0.708689770883323,1.),(1.,0.708376440034487,
1.),(1.,0.707750498698403,1.),(1.,0.707106781186548,1.)))
REPRESENTATION_ITEM('')
SURFACE()
);
#3395=(
BOUNDED_SURFACE()
B_SPLINE_SURFACE(3,2,((#243664,#243665,#243666),(#243667,#243668,#243669),
(#243670,#243671,#243672),(#243673,#243674,#243675)),.UNSPECIFIED.,.F.,
 .F.,.F.)
B_SPLINE_SURFACE_WITH_KNOTS((4,4),(3,3),(0.,0.000511815090126168),(0.,1.00105592270543),
 .UNSPECIFIED.)
GEOMETRIC_REPRESENTATION_ITEM()
RATIONAL_B_SPLINE_SURFACE(((1.,0.70526624271654,1.00062243213275),(1.,0.705584085908197,
1.00062176089706),(1.,0.706182089449555,1.00062049800603),(1.,0.706797508586535,
1.00061919833595)))
REPRESENTATION_ITEM('')
SURFACE()
);
#3396=(
BOUNDED_SURFACE()
B_SPLINE_SURFACE(3,2,((#243677,#243678,#243679),(#243680,#243681,#243682),
(#243683,#243684,#243685),(#243686,#243687,#243688)),.UNSPECIFIED.,.F.,
 .F.,.F.)
B_SPLINE_SURFACE_WITH_KNOTS((4,4),(3,3),(0.,0.000397394428086615),(0.,1.),
 .UNSPECIFIED.)
GEOMETRIC_REPRESENTATION_ITEM()
RATIONAL_B_SPLINE_SURFACE(((1.,0.707106781186548,1.),(1.,0.706459846759084,
1.),(1.,0.705820510737294,1.),(1.,0.705498956110758,1.)))
REPRESENTATION_ITEM('')
SURFACE()
);
#3397=(
BOUNDED_SURFACE()
B_SPLINE_SURFACE(3,2,((#243694,#243695,#243696),(#243697,#243698,#243699),
(#243700,#243701,#243702),(#243703,#243704,#243705),(#243706,#243707,#243708),
(#243709,#243710,#243711)),.UNSPECIFIED.,.F.,.F.,.F.)
B_SPLINE_SURFACE_WITH_KNOTS((4,2,4),(3,3),(-3.93023287525995E-19,0.000257953807872852,
0.000515907615745705),(0.,1.),.UNSPECIFIED.)
GEOMETRIC_REPRESENTATION_ITEM()
RATIONAL_B_SPLINE_SURFACE(((1.,0.874619707139391,1.),(1.,0.874834349678696,
1.),(1.,0.854686104158193,1.),(1.,0.792476597914731,1.),(1.,0.750887854595441,
1.),(1.,0.705585838031444,1.)))
REPRESENTATION_ITEM('')
SURFACE()
);
#3398=(
BOUNDED_SURFACE()
B_SPLINE_SURFACE(3,2,((#243717,#243718,#243719),(#243720,#243721,#243722),
(#243723,#243724,#243725),(#243726,#243727,#243728)),.UNSPECIFIED.,.F.,
 .F.,.F.)
B_SPLINE_SURFACE_WITH_KNOTS((4,4),(3,3),(-5.6920614055489E-19,0.000511815437699152),
(0.,1.00105881331654),.UNSPECIFIED.)
GEOMETRIC_REPRESENTATION_ITEM()
RATIONAL_B_SPLINE_SURFACE(((1.,0.706796661946145,1.00062089519757),(1.,
0.707430821225015,1.00061955228499),(1.,0.708058545830515,1.00061822299865),
(1.,0.70839450525252,1.00061751156203)))
REPRESENTATION_ITEM('')
SURFACE()
);
#3399=(
BOUNDED_SURFACE()
B_SPLINE_SURFACE(3,2,((#243730,#243731,#243732),(#243733,#243734,#243735),
(#243736,#243737,#243738),(#243739,#243740,#243741),(#243742,#243743,#243744),
(#243745,#243746,#243747)),.UNSPECIFIED.,.F.,.F.,.F.)
B_SPLINE_SURFACE_WITH_KNOTS((4,2,4),(3,3),(-2.7376104855259E-18,0.000256915317531256,
0.000513830635062514),(0.,1.),.UNSPECIFIED.)
GEOMETRIC_REPRESENTATION_ITEM()
RATIONAL_B_SPLINE_SURFACE(((1.,0.705585838031416,1.),(1.,0.750902433542311,
1.),(1.,0.792329530083129,1.),(1.,0.854288401593573,1.),(1.,0.874998031125583,
1.),(1.,0.874619707139392,1.)))
REPRESENTATION_ITEM('')
SURFACE()
);
#3400=(
BOUNDED_SURFACE()
B_SPLINE_SURFACE(3,2,((#243753,#243754,#243755),(#243756,#243757,#243758),
(#243759,#243760,#243761),(#243762,#243763,#243764),(#243765,#243766,#243767),
(#243768,#243769,#243770)),.UNSPECIFIED.,.F.,.F.,.F.)
B_SPLINE_SURFACE_WITH_KNOTS((4,2,4),(3,3),(0.,0.000256592814262159,0.000513185628524319),
(0.,1.),.UNSPECIFIED.)
GEOMETRIC_REPRESENTATION_ITEM()
RATIONAL_B_SPLINE_SURFACE(((1.,0.708712527163655,1.),(1.,0.753780902613272,
1.),(1.,0.794538995769632,1.),(1.,0.855070770330658,1.),(1.,0.875018427445671,
1.),(1.,0.874619707139395,1.)))
REPRESENTATION_ITEM('')
SURFACE()
);
#3401=(
BOUNDED_SURFACE()
B_SPLINE_SURFACE(3,2,((#243772,#243773,#243774),(#243775,#243776,#243777),
(#243778,#243779,#243780),(#243781,#243782,#243783)),.UNSPECIFIED.,.F.,
 .F.,.F.)
B_SPLINE_SURFACE_WITH_KNOTS((4,4),(3,3),(5.6920614055489E-19,0.000511815072430395),
(0.,1.00105598365956),.UNSPECIFIED.)
GEOMETRIC_REPRESENTATION_ITEM()
RATIONAL_B_SPLINE_SURFACE(((1.,0.706797490733483,1.00061923411746),(1.,
0.706182062146394,1.00062053388252),(1.,0.705584062768761,1.00062179683766),
(1.,0.705266224770235,1.00062246810113)))
REPRESENTATION_ITEM('')
SURFACE()
);
#3402=(
BOUNDED_SURFACE()
B_SPLINE_SURFACE(3,2,((#243789,#243790,#243791),(#243792,#243793,#243794),
(#243795,#243796,#243797),(#243798,#243799,#243800),(#243801,#243802,#243803),
(#243804,#243805,#243806)),.UNSPECIFIED.,.F.,.F.,.F.)
B_SPLINE_SURFACE_WITH_KNOTS((4,2,4),(3,3),(0.,0.000257652232350885,0.00051530446470177),
(0.,1.),.UNSPECIFIED.)
GEOMETRIC_REPRESENTATION_ITEM()
RATIONAL_B_SPLINE_SURFACE(((1.,0.8746197071394,1.),(1.,0.874861180430967,
1.),(1.,0.85545572592054,1.),(1.,0.794699358955578,1.),(1.,0.753768977788408,
1.),(1.,0.708712527163672,1.)))
REPRESENTATION_ITEM('')
SURFACE()
);
#3403=(
BOUNDED_SURFACE()
B_SPLINE_SURFACE(3,2,((#243812,#243813,#243814),(#243815,#243816,#243817),
(#243818,#243819,#243820),(#243821,#243822,#243823)),.UNSPECIFIED.,.F.,
 .F.,.F.)
B_SPLINE_SURFACE_WITH_KNOTS((4,4),(3,3),(-7.10152422978005E-18,0.00039739437365192),
(0.,1.),.UNSPECIFIED.)
GEOMETRIC_REPRESENTATION_ITEM()
RATIONAL_B_SPLINE_SURFACE(((1.,0.707106781186545,1.),(1.,0.707752587915908,
1.),(1.,0.708377654540671,1.),(1.,0.708689770883337,1.)))
REPRESENTATION_ITEM('')
SURFACE()
);
#3404=(
BOUNDED_SURFACE()
B_SPLINE_SURFACE(3,2,((#243825,#243826,#243827),(#243828,#243829,#243830),
(#243831,#243832,#243833),(#243834,#243835,#243836)),.UNSPECIFIED.,.F.,
 .F.,.F.)
B_SPLINE_SURFACE_WITH_KNOTS((4,4),(3,3),(0.,0.000511815456479799),(0.,1.00105873159959),
 .UNSPECIFIED.)
GEOMETRIC_REPRESENTATION_ITEM()
RATIONAL_B_SPLINE_SURFACE(((1.,0.70839452905644,1.0006174638534),(1.,0.708058564166983,
1.00061817524669),(1.,0.707430835372161,1.00061950443932),(1.,0.706796685880483,
1.00062084722753)))
REPRESENTATION_ITEM('')
SURFACE()
);
#3405=(
BOUNDED_SURFACE()
B_SPLINE_SURFACE(3,2,((#243842,#243843,#243844),(#243845,#243846,#243847),
(#243848,#243849,#243850),(#243851,#243852,#243853)),.UNSPECIFIED.,.F.,
 .F.,.F.)
B_SPLINE_SURFACE_WITH_KNOTS((4,4),(3,3),(-5.6920614055489E-18,0.000397394465448304),
(0.,1.),.UNSPECIFIED.)
GEOMETRIC_REPRESENTATION_ITEM()
RATIONAL_B_SPLINE_SURFACE(((1.,0.705498956110744,1.),(1.,0.705821764811792,
1.),(1.,0.706461952521134,1.),(1.,0.707106781186545,1.)))
REPRESENTATION_ITEM('')
SURFACE()
);
#3406=(
BOUNDED_SURFACE()
B_SPLINE_SURFACE(3,2,((#243859,#243860,#243861),(#243862,#243863,#243864),
(#243865,#243866,#243867),(#243868,#243869,#243870)),.UNSPECIFIED.,.F.,
 .F.,.F.)
B_SPLINE_SURFACE_WITH_KNOTS((4,4),(3,3),(0.,0.00039739441082873),(0.,1.),
 .UNSPECIFIED.)
GEOMETRIC_REPRESENTATION_ITEM()
RATIONAL_B_SPLINE_SURFACE(((1.,0.708689770883332,1.),(1.,0.70837644003449,
1.),(1.,0.707750498698411,1.),(1.,0.707106781186548,1.)))
REPRESENTATION_ITEM('')
SURFACE()
);
#3407=(
BOUNDED_SURFACE()
B_SPLINE_SURFACE(3,2,((#243876,#243877,#243878),(#243879,#243880,#243881),
(#243882,#243883,#243884),(#243885,#243886,#243887)),.UNSPECIFIED.,.F.,
 .F.,.F.)
B_SPLINE_SURFACE_WITH_KNOTS((4,4),(3,3),(0.,0.000511815090126174),(0.,1.00105592270389),
 .UNSPECIFIED.)
GEOMETRIC_REPRESENTATION_ITEM()
RATIONAL_B_SPLINE_SURFACE(((1.,0.70526624271697,1.00062243213183),(1.,0.705584085908647,
1.00062176089615),(1.,0.706182089450001,1.00062049800512),(1.,0.706797508586988,
1.00061919833504)))
REPRESENTATION_ITEM('')
SURFACE()
);
#3408=(
BOUNDED_SURFACE()
B_SPLINE_SURFACE(3,2,((#243889,#243890,#243891),(#243892,#243893,#243894),
(#243895,#243896,#243897),(#243898,#243899,#243900)),.UNSPECIFIED.,.F.,
 .F.,.F.)
B_SPLINE_SURFACE_WITH_KNOTS((4,4),(3,3),(-7.07441917546792E-18,0.00039739442808661),
(0.,1.),.UNSPECIFIED.)
GEOMETRIC_REPRESENTATION_ITEM()
RATIONAL_B_SPLINE_SURFACE(((1.,0.707106781186547,1.),(1.,0.706459846759101,
1.),(1.,0.705820510737253,1.),(1.,0.705498956110768,1.)))
REPRESENTATION_ITEM('')
SURFACE()
);
#3409=(
BOUNDED_SURFACE()
B_SPLINE_SURFACE(3,2,((#243906,#243907,#243908),(#243909,#243910,#243911),
(#243912,#243913,#243914),(#243915,#243916,#243917),(#243918,#243919,#243920),
(#243921,#243922,#243923)),.UNSPECIFIED.,.F.,.F.,.F.)
B_SPLINE_SURFACE_WITH_KNOTS((4,2,4),(3,3),(0.,0.000257953807872856,0.000515907615745713),
(0.,1.),.UNSPECIFIED.)
GEOMETRIC_REPRESENTATION_ITEM()
RATIONAL_B_SPLINE_SURFACE(((1.,0.874619707139396,1.),(1.,0.874834349678934,
1.),(1.,0.85468610415787,1.),(1.,0.79247659791506,1.),(1.,0.750887854595183,
1.),(1.,0.70558583803143,1.)))
REPRESENTATION_ITEM('')
SURFACE()
);
#3410=(
BOUNDED_SURFACE()
B_SPLINE_SURFACE(3,2,((#243929,#243930,#243931),(#243932,#243933,#243934),
(#243935,#243936,#243937),(#243938,#243939,#243940)),.UNSPECIFIED.,.F.,
 .F.,.F.)
B_SPLINE_SURFACE_WITH_KNOTS((4,4),(3,3),(0.,0.00051181543769915),(0.,1.00105881331475),
 .UNSPECIFIED.)
GEOMETRIC_REPRESENTATION_ITEM()
RATIONAL_B_SPLINE_SURFACE(((1.,0.706796661946667,1.00062089519652),(1.,
0.70743082122554,1.00061955228395),(1.,0.708058545831051,1.0006182229976),
(1.,0.708394505253048,1.00061751156099)))
REPRESENTATION_ITEM('')
SURFACE()
);
#3411=(
BOUNDED_SURFACE()
B_SPLINE_SURFACE(3,2,((#243942,#243943,#243944),(#243945,#243946,#243947),
(#243948,#243949,#243950),(#243951,#243952,#243953),(#243954,#243955,#243956),
(#243957,#243958,#243959)),.UNSPECIFIED.,.F.,.F.,.F.)
B_SPLINE_SURFACE_WITH_KNOTS((4,2,4),(3,3),(-2.71050543121376E-20,0.000256915317531261,
0.000513830635062521),(0.,1.),.UNSPECIFIED.)
GEOMETRIC_REPRESENTATION_ITEM()
RATIONAL_B_SPLINE_SURFACE(((1.,0.705585838031441,1.),(1.,0.750902433542888,
1.),(1.,0.792329530082332,1.),(1.,0.854288401594382,1.),(1.,0.874998031124998,
1.),(1.,0.874619707139396,1.)))
REPRESENTATION_ITEM('')
SURFACE()
);
#3412=(
BOUNDED_SURFACE()
B_SPLINE_SURFACE(3,2,((#243965,#243966,#243967),(#243968,#243969,#243970),
(#243971,#243972,#243973),(#243974,#243975,#243976),(#243977,#243978,#243979),
(#243980,#243981,#243982)),.UNSPECIFIED.,.F.,.F.,.F.)
B_SPLINE_SURFACE_WITH_KNOTS((4,2,4),(3,3),(-1.0435445910173E-17,0.000256592814262151,
0.000513185628524313),(0.,1.),.UNSPECIFIED.)
GEOMETRIC_REPRESENTATION_ITEM()
RATIONAL_B_SPLINE_SURFACE(((1.,0.70871252716368,1.),(1.,0.753780902613545,
1.),(1.,0.794538995769243,1.),(1.,0.855070770331071,1.),(1.,0.875018427445353,
1.),(1.,0.874619707139393,1.)))
REPRESENTATION_ITEM('')
SURFACE()
);
#3413=(
BOUNDED_SURFACE()
B_SPLINE_SURFACE(3,2,((#243984,#243985,#243986),(#243987,#243988,#243989),
(#243990,#243991,#243992),(#243993,#243994,#243995)),.UNSPECIFIED.,.F.,
 .F.,.F.)
B_SPLINE_SURFACE_WITH_KNOTS((4,4),(3,3),(5.6920614055489E-19,0.000511815072430399),
(0.,1.00105598365992),.UNSPECIFIED.)
GEOMETRIC_REPRESENTATION_ITEM()
RATIONAL_B_SPLINE_SURFACE(((1.,0.70679749073338,1.00061923411767),(1.,0.706182062146294,
1.00062053388273),(1.,0.70558406276866,1.00062179683787),(1.,0.705266224770139,
1.00062246810134)))
REPRESENTATION_ITEM('')
SURFACE()
);
#3414=(
BOUNDED_SURFACE()
B_SPLINE_SURFACE(3,2,((#244001,#244002,#244003),(#244004,#244005,#244006),
(#244007,#244008,#244009),(#244010,#244011,#244012),(#244013,#244014,#244015),
(#244016,#244017,#244018)),.UNSPECIFIED.,.F.,.F.,.F.)
B_SPLINE_SURFACE_WITH_KNOTS((4,2,4),(3,3),(-6.36968776335234E-19,0.000257652232350878,
0.000515304464701757),(0.,1.),.UNSPECIFIED.)
GEOMETRIC_REPRESENTATION_ITEM()
RATIONAL_B_SPLINE_SURFACE(((1.,0.874619707139393,1.),(1.,0.874861180431038,
1.),(1.,0.855455725920423,1.),(1.,0.794699358955735,1.),(1.,0.753768977788282,
1.),(1.,0.708712527163677,1.)))
REPRESENTATION_ITEM('')
SURFACE()
);
#3415=(
BOUNDED_SURFACE()
B_SPLINE_SURFACE(3,2,((#244024,#244025,#244026),(#244027,#244028,#244029),
(#244030,#244031,#244032),(#244033,#244034,#244035)),.UNSPECIFIED.,.F.,
 .F.,.F.)
B_SPLINE_SURFACE_WITH_KNOTS((4,4),(3,3),(0.,0.000397394373651921),(0.,1.),
 .UNSPECIFIED.)
GEOMETRIC_REPRESENTATION_ITEM()
RATIONAL_B_SPLINE_SURFACE(((1.,0.707106781186548,1.),(1.,0.707752587915887,
1.),(1.,0.708377654540684,1.),(1.,0.70868977088333,1.)))
REPRESENTATION_ITEM('')
SURFACE()
);
#3416=(
BOUNDED_SURFACE()
B_SPLINE_SURFACE(3,2,((#244037,#244038,#244039),(#244040,#244041,#244042),
(#244043,#244044,#244045),(#244046,#244047,#244048)),.UNSPECIFIED.,.F.,
 .F.,.F.)
B_SPLINE_SURFACE_WITH_KNOTS((4,4),(3,3),(0.,0.0005118154564798),(0.,1.0010587315969),
 .UNSPECIFIED.)
GEOMETRIC_REPRESENTATION_ITEM()
RATIONAL_B_SPLINE_SURFACE(((1.,0.708394529057217,1.00061746385183),(1.,
0.70805856416776,1.00061817524512),(1.,0.707430835372961,1.00061950443774),
(1.,0.706796685881273,1.00062084722595)))
REPRESENTATION_ITEM('')
SURFACE()
);
#3417=(
BOUNDED_SURFACE()
B_SPLINE_SURFACE(3,2,((#244054,#244055,#244056),(#244057,#244058,#244059),
(#244060,#244061,#244062),(#244063,#244064,#244065)),.UNSPECIFIED.,.F.,
 .F.,.F.)
B_SPLINE_SURFACE_WITH_KNOTS((4,4),(3,3),(-2.03287907341032E-18,0.000397394465448303),
(0.,1.),.UNSPECIFIED.)
GEOMETRIC_REPRESENTATION_ITEM()
RATIONAL_B_SPLINE_SURFACE(((1.,0.705498956110753,1.),(1.,0.705821764811784,
1.),(1.,0.706461952521139,1.),(1.,0.707106781186548,1.)))
REPRESENTATION_ITEM('')
SURFACE()
);
#3418=(
BOUNDED_SURFACE()
B_SPLINE_SURFACE(3,2,((#244071,#244072,#244073),(#244074,#244075,#244076),
(#244077,#244078,#244079),(#244080,#244081,#244082)),.UNSPECIFIED.,.F.,
 .F.,.F.)
B_SPLINE_SURFACE_WITH_KNOTS((4,4),(3,3),(0.,0.000397394410828748),(0.,1.),
 .UNSPECIFIED.)
GEOMETRIC_REPRESENTATION_ITEM()
RATIONAL_B_SPLINE_SURFACE(((1.,0.708689770883308,1.),(1.,0.708376440034495,
1.),(1.,0.707750498698405,1.),(1.,0.707106781186549,1.)))
REPRESENTATION_ITEM('')
SURFACE()
);
#3419=(
BOUNDED_SURFACE()
B_SPLINE_SURFACE(3,2,((#244088,#244089,#244090),(#244091,#244092,#244093),
(#244094,#244095,#244096),(#244097,#244098,#244099)),.UNSPECIFIED.,.F.,
 .F.,.F.)
B_SPLINE_SURFACE_WITH_KNOTS((4,4),(3,3),(0.,0.000511815090126176),(0.,1.00105592270268),
 .UNSPECIFIED.)
GEOMETRIC_REPRESENTATION_ITEM()
RATIONAL_B_SPLINE_SURFACE(((1.,0.705266242717368,1.00062243213112),(1.,
0.705584085908997,1.00062176089544),(1.,0.706182089450358,1.00062049800441),
(1.,0.706797508587342,1.00061919833433)))
REPRESENTATION_ITEM('')
SURFACE()
);
#3420=(
BOUNDED_SURFACE()
B_SPLINE_SURFACE(3,2,((#244101,#244102,#244103),(#244104,#244105,#244106),
(#244107,#244108,#244109),(#244110,#244111,#244112)),.UNSPECIFIED.,.F.,
 .F.,.F.)
B_SPLINE_SURFACE_WITH_KNOTS((4,4),(3,3),(0.,0.000397394428086627),(0.,1.),
 .UNSPECIFIED.)
GEOMETRIC_REPRESENTATION_ITEM()
RATIONAL_B_SPLINE_SURFACE(((1.,0.70710678118655,1.),(1.,0.706459846759099,
1.),(1.,0.705820510737279,1.),(1.,0.70549895611076,1.)))
REPRESENTATION_ITEM('')
SURFACE()
);
#3421=(
BOUNDED_SURFACE()
B_SPLINE_SURFACE(3,2,((#244118,#244119,#244120),(#244121,#244122,#244123),
(#244124,#244125,#244126),(#244127,#244128,#244129),(#244130,#244131,#244132),
(#244133,#244134,#244135)),.UNSPECIFIED.,.F.,.F.,.F.)
B_SPLINE_SURFACE_WITH_KNOTS((4,2,4),(3,3),(0.,0.000257953807872846,0.000515907615745692),
(0.,1.),.UNSPECIFIED.)
GEOMETRIC_REPRESENTATION_ITEM()
RATIONAL_B_SPLINE_SURFACE(((1.,0.874619707139392,1.),(1.,0.874834349678668,
1.),(1.,0.854686104158253,1.),(1.,0.792476597914677,1.),(1.,0.750887854595503,
1.),(1.,0.705585838031432,1.)))
REPRESENTATION_ITEM('')
SURFACE()
);
#3422=(
BOUNDED_SURFACE()
B_SPLINE_SURFACE(3,2,((#244141,#244142,#244143),(#244144,#244145,#244146),
(#244147,#244148,#244149),(#244150,#244151,#244152)),.UNSPECIFIED.,.F.,
 .F.,.F.)
B_SPLINE_SURFACE_WITH_KNOTS((4,4),(3,3),(-5.6920614055489E-19,0.00051181543769915),
(0.,1.0010588133166),.UNSPECIFIED.)
GEOMETRIC_REPRESENTATION_ITEM()
RATIONAL_B_SPLINE_SURFACE(((1.,0.706796661946126,1.00062089519761),(1.,
0.707430821224993,1.00061955228503),(1.,0.708058545830525,1.00061822299868),
(1.,0.708394505252487,1.00061751156206)))
REPRESENTATION_ITEM('')
SURFACE()
);
#3423=(
BOUNDED_SURFACE()
B_SPLINE_SURFACE(3,2,((#244154,#244155,#244156),(#244157,#244158,#244159),
(#244160,#244161,#244162),(#244163,#244164,#244165),(#244166,#244167,#244168),
(#244169,#244170,#244171)),.UNSPECIFIED.,.F.,.F.,.F.)
B_SPLINE_SURFACE_WITH_KNOTS((4,2,4),(3,3),(0.,0.000256915317531263,0.000513830635062526),
(0.,1.),.UNSPECIFIED.)
GEOMETRIC_REPRESENTATION_ITEM()
RATIONAL_B_SPLINE_SURFACE(((1.,0.705585838031459,1.),(1.,0.750902433542461,
1.),(1.,0.79232953008286,1.),(1.,0.854288401593831,1.),(1.,0.874998031125431,
1.),(1.,0.87461970713939,1.)))
REPRESENTATION_ITEM('')
SURFACE()
);
#3424=(
BOUNDED_SURFACE()
B_SPLINE_SURFACE(3,2,((#244177,#244178,#244179),(#244180,#244181,#244182),
(#244183,#244184,#244185),(#244186,#244187,#244188),(#244189,#244190,#244191),
(#244192,#244193,#244194)),.UNSPECIFIED.,.F.,.F.,.F.)
B_SPLINE_SURFACE_WITH_KNOTS((4,2,4),(3,3),(0.,0.000256592814262157,0.000513185628524313),
(0.,1.),.UNSPECIFIED.)
GEOMETRIC_REPRESENTATION_ITEM()
RATIONAL_B_SPLINE_SURFACE(((1.,0.708712527163657,1.),(1.,0.753780902614056,
1.),(1.,0.794538995768585,1.),(1.,0.855070770331729,1.),(1.,0.875018427444851,
1.),(1.,0.874619707139394,1.)))
REPRESENTATION_ITEM('')
SURFACE()
);
#3425=(
BOUNDED_SURFACE()
B_SPLINE_SURFACE(3,2,((#244196,#244197,#244198),(#244199,#244200,#244201),
(#244202,#244203,#244204),(#244205,#244206,#244207)),.UNSPECIFIED.,.F.,
 .F.,.F.)
B_SPLINE_SURFACE_WITH_KNOTS((4,4),(3,3),(5.96311194867027E-19,0.000511815072430393),
(0.,1.00105598365887),.UNSPECIFIED.)
GEOMETRIC_REPRESENTATION_ITEM()
RATIONAL_B_SPLINE_SURFACE(((1.,0.706797490733686,1.00061923411705),(1.,
0.706182062146616,1.00062053388211),(1.,0.70558406276894,1.00062179683726),
(1.,0.705266224770434,1.00062246810072)))
REPRESENTATION_ITEM('')
SURFACE()
);
#3426=(
BOUNDED_SURFACE()
B_SPLINE_SURFACE(3,2,((#244213,#244214,#244215),(#244216,#244217,#244218),
(#244219,#244220,#244221),(#244222,#244223,#244224),(#244225,#244226,#244227),
(#244228,#244229,#244230)),.UNSPECIFIED.,.F.,.F.,.F.)
B_SPLINE_SURFACE_WITH_KNOTS((4,2,4),(3,3),(0.,0.000257652232350883,0.000515304464701765),
(0.,1.),.UNSPECIFIED.)
GEOMETRIC_REPRESENTATION_ITEM()
RATIONAL_B_SPLINE_SURFACE(((1.,0.874619707139395,1.),(1.,0.874861180431021,
1.),(1.,0.855455725920468,1.),(1.,0.794699358955673,1.),(1.,0.753768977788341,
1.),(1.,0.708712527163671,1.)))
REPRESENTATION_ITEM('')
SURFACE()
);
#3427=(
BOUNDED_SURFACE()
B_SPLINE_SURFACE(3,2,((#244236,#244237,#244238),(#244239,#244240,#244241),
(#244242,#244243,#244244),(#244245,#244246,#244247)),.UNSPECIFIED.,.F.,
 .F.,.F.)
B_SPLINE_SURFACE_WITH_KNOTS((4,4),(3,3),(0.,0.000397394373651922),(0.,1.),
 .UNSPECIFIED.)
GEOMETRIC_REPRESENTATION_ITEM()
RATIONAL_B_SPLINE_SURFACE(((1.,0.707106781186548,1.),(1.,0.707752587915897,
1.),(1.,0.708377654540704,1.),(1.,0.708689770883339,1.)))
REPRESENTATION_ITEM('')
SURFACE()
);
#3428=(
BOUNDED_SURFACE()
B_SPLINE_SURFACE(3,2,((#244249,#244250,#244251),(#244252,#244253,#244254),
(#244255,#244256,#244257),(#244258,#244259,#244260)),.UNSPECIFIED.,.F.,
 .F.,.F.)
B_SPLINE_SURFACE_WITH_KNOTS((4,4),(3,3),(0.,0.000511815456479789),(0.,1.00105873159825),
 .UNSPECIFIED.)
GEOMETRIC_REPRESENTATION_ITEM()
RATIONAL_B_SPLINE_SURFACE(((1.,0.708394529056854,1.00061746385262),(1.,
0.708058564167349,1.00061817524591),(1.,0.707430835372582,1.00061950443853),
(1.,0.706796685880876,1.00062084722674)))
REPRESENTATION_ITEM('')
SURFACE()
);
#3429=(
BOUNDED_SURFACE()
B_SPLINE_SURFACE(3,2,((#244266,#244267,#244268),(#244269,#244270,#244271),
(#244272,#244273,#244274),(#244275,#244276,#244277)),.UNSPECIFIED.,.F.,
 .F.,.F.)
B_SPLINE_SURFACE_WITH_KNOTS((4,4),(3,3),(0.,0.000397394465448316),(0.,1.),
 .UNSPECIFIED.)
GEOMETRIC_REPRESENTATION_ITEM()
RATIONAL_B_SPLINE_SURFACE(((1.,0.705498956110759,1.),(1.,0.705821764811766,
1.),(1.,0.706461952521144,1.),(1.,0.707106781186546,1.)))
REPRESENTATION_ITEM('')
SURFACE()
);
#3430=(
BOUNDED_SURFACE()
B_SPLINE_SURFACE(3,2,((#244283,#244284,#244285),(#244286,#244287,#244288),
(#244289,#244290,#244291),(#244292,#244293,#244294)),.UNSPECIFIED.,.F.,
 .F.,.F.)
B_SPLINE_SURFACE_WITH_KNOTS((4,4),(3,3),(0.,0.000397394410828743),(0.,1.),
 .UNSPECIFIED.)
GEOMETRIC_REPRESENTATION_ITEM()
RATIONAL_B_SPLINE_SURFACE(((1.,0.708689770883332,1.),(1.,0.70837644003449,
1.),(1.,0.707750498698407,1.),(1.,0.707106781186551,1.)))
REPRESENTATION_ITEM('')
SURFACE()
);
#3431=(
BOUNDED_SURFACE()
B_SPLINE_SURFACE(3,2,((#244300,#244301,#244302),(#244303,#244304,#244305),
(#244306,#244307,#244308),(#244309,#244310,#244311)),.UNSPECIFIED.,.F.,
 .F.,.F.)
B_SPLINE_SURFACE_WITH_KNOTS((4,4),(3,3),(0.,0.000511815090126169),(0.,1.00105592270137),
 .UNSPECIFIED.)
GEOMETRIC_REPRESENTATION_ITEM()
RATIONAL_B_SPLINE_SURFACE(((1.,0.705266242717729,1.00062243213035),(1.,
0.70558408590941,1.00062176089466),(1.,0.706182089450716,1.00062049800363),
(1.,0.706797508587726,1.00061919833356)))
REPRESENTATION_ITEM('')
SURFACE()
);
#3432=(
BOUNDED_SURFACE()
B_SPLINE_SURFACE(3,2,((#244313,#244314,#244315),(#244316,#244317,#244318),
(#244319,#244320,#244321),(#244322,#244323,#244324)),.UNSPECIFIED.,.F.,
 .F.,.F.)
B_SPLINE_SURFACE_WITH_KNOTS((4,4),(3,3),(0.,0.00039739442808661),(0.,1.),
 .UNSPECIFIED.)
GEOMETRIC_REPRESENTATION_ITEM()
RATIONAL_B_SPLINE_SURFACE(((1.,0.707106781186552,1.),(1.,0.70645984675909,
1.),(1.,0.705820510737272,1.),(1.,0.705498956110746,1.)))
REPRESENTATION_ITEM('')
SURFACE()
);
#3433=(
BOUNDED_SURFACE()
B_SPLINE_SURFACE(3,2,((#244330,#244331,#244332),(#244333,#244334,#244335),
(#244336,#244337,#244338),(#244339,#244340,#244341),(#244342,#244343,#244344),
(#244345,#244346,#244347)),.UNSPECIFIED.,.F.,.F.,.F.)
B_SPLINE_SURFACE_WITH_KNOTS((4,2,4),(3,3),(0.,0.000257953807872836,0.000515907615745672),
(0.,1.),.UNSPECIFIED.)
GEOMETRIC_REPRESENTATION_ITEM()
RATIONAL_B_SPLINE_SURFACE(((1.,0.874619707139391,1.),(1.,0.874834349679291,
1.),(1.,0.854686104157408,1.),(1.,0.792476597915517,1.),(1.,0.750887854594871,
1.),(1.,0.705585838031449,1.)))
REPRESENTATION_ITEM('')
SURFACE()
);
#3434=(
BOUNDED_SURFACE()
B_SPLINE_SURFACE(3,2,((#244353,#244354,#244355),(#244356,#244357,#244358),
(#244359,#244360,#244361),(#244362,#244363,#244364)),.UNSPECIFIED.,.F.,
 .F.,.F.)
B_SPLINE_SURFACE_WITH_KNOTS((4,4),(3,3),(0.,0.00051181543769915),(0.,1.00105881331569),
 .UNSPECIFIED.)
GEOMETRIC_REPRESENTATION_ITEM()
RATIONAL_B_SPLINE_SURFACE(((1.,0.706796661946389,1.00062089519707),(1.,
0.707430821225278,1.00061955228449),(1.,0.708058545830776,1.00061822299815),
(1.,0.708394505252776,1.00061751156153)))
REPRESENTATION_ITEM('')
SURFACE()
);
#3435=(
BOUNDED_SURFACE()
B_SPLINE_SURFACE(3,2,((#244366,#244367,#244368),(#244369,#244370,#244371),
(#244372,#244373,#244374),(#244375,#244376,#244377),(#244378,#244379,#244380),
(#244381,#244382,#244383)),.UNSPECIFIED.,.F.,.F.,.F.)
B_SPLINE_SURFACE_WITH_KNOTS((4,2,4),(3,3),(0.,0.000256915317531256,0.000513830635062512),
(0.,1.),.UNSPECIFIED.)
GEOMETRIC_REPRESENTATION_ITEM()
RATIONAL_B_SPLINE_SURFACE(((1.,0.705585838031447,1.),(1.,0.750902433541732,
1.),(1.,0.792329530083833,1.),(1.,0.854288401592882,1.),(1.,0.874998031126119,
1.),(1.,0.874619707139395,1.)))
REPRESENTATION_ITEM('')
SURFACE()
);
#3436=(
BOUNDED_SURFACE()
B_SPLINE_SURFACE(3,2,((#244389,#244390,#244391),(#244392,#244393,#244394),
(#244395,#244396,#244397),(#244398,#244399,#244400),(#244401,#244402,#244403),
(#244404,#244405,#244406)),.UNSPECIFIED.,.F.,.F.,.F.)
B_SPLINE_SURFACE_WITH_KNOTS((4,2,4),(3,3),(-2.5207700510288E-18,0.000256592814262155,
0.000513185628524313),(0.,1.),.UNSPECIFIED.)
GEOMETRIC_REPRESENTATION_ITEM()
RATIONAL_B_SPLINE_SURFACE(((1.,0.70871252716366,1.),(1.,0.753780902613132,
1.),(1.,0.794538995769815,1.),(1.,0.855070770330497,1.),(1.,0.875018427445787,
1.),(1.,0.874619707139398,1.)))
REPRESENTATION_ITEM('')
SURFACE()
);
#3437=(
BOUNDED_SURFACE()
B_SPLINE_SURFACE(3,2,((#244408,#244409,#244410),(#244411,#244412,#244413),
(#244414,#244415,#244416),(#244417,#244418,#244419)),.UNSPECIFIED.,.F.,
 .F.,.F.)
B_SPLINE_SURFACE_WITH_KNOTS((4,4),(3,3),(5.96311194867027E-19,0.000511815072430402),
(0.,1.00105598365777),.UNSPECIFIED.)
GEOMETRIC_REPRESENTATION_ITEM()
RATIONAL_B_SPLINE_SURFACE(((1.,0.706797490734009,1.0006192341164),(1.,0.706182062146925,
1.00062053388146),(1.,0.705584062769296,1.0006217968366),(1.,0.705266224770765,
1.00062246810007)))
REPRESENTATION_ITEM('')
SURFACE()
);
#3438=(
BOUNDED_SURFACE()
B_SPLINE_SURFACE(3,2,((#244425,#244426,#244427),(#244428,#244429,#244430),
(#244431,#244432,#244433),(#244434,#244435,#244436),(#244437,#244438,#244439),
(#244440,#244441,#244442)),.UNSPECIFIED.,.F.,.F.,.F.)
B_SPLINE_SURFACE_WITH_KNOTS((4,2,4),(3,3),(0.,0.00025765223235088,0.00051530446470176),
(0.,1.),.UNSPECIFIED.)
GEOMETRIC_REPRESENTATION_ITEM()
RATIONAL_B_SPLINE_SURFACE(((1.,0.874619707139393,1.),(1.,0.874861180430485,
1.),(1.,0.8554557259212,1.),(1.,0.794699358954937,1.),(1.,0.753768977788887,
1.),(1.,0.708712527163683,1.)))
REPRESENTATION_ITEM('')
SURFACE()
);
#3439=(
BOUNDED_SURFACE()
B_SPLINE_SURFACE(3,2,((#244448,#244449,#244450),(#244451,#244452,#244453),
(#244454,#244455,#244456),(#244457,#244458,#244459)),.UNSPECIFIED.,.F.,
 .F.,.F.)
B_SPLINE_SURFACE_WITH_KNOTS((4,4),(3,3),(0.,0.000397394373651921),(0.,1.),
 .UNSPECIFIED.)
GEOMETRIC_REPRESENTATION_ITEM()
RATIONAL_B_SPLINE_SURFACE(((1.,0.707106781186548,1.),(1.,0.70775258791588,
1.),(1.,0.708377654540694,1.),(1.,0.70868977088333,1.)))
REPRESENTATION_ITEM('')
SURFACE()
);
#3440=(
BOUNDED_SURFACE()
B_SPLINE_SURFACE(3,2,((#244461,#244462,#244463),(#244464,#244465,#244466),
(#244467,#244468,#244469),(#244470,#244471,#244472)),.UNSPECIFIED.,.F.,
 .F.,.F.)
B_SPLINE_SURFACE_WITH_KNOTS((4,4),(3,3),(0.,0.000511815456479791),(0.,1.00105873159742),
 .UNSPECIFIED.)
GEOMETRIC_REPRESENTATION_ITEM()
RATIONAL_B_SPLINE_SURFACE(((1.,0.708394529057083,1.00061746385214),(1.,
0.708058564167601,1.00061817524542),(1.,0.707430835372811,1.00061950443804),
(1.,0.70679668588112,1.00062084722625)))
REPRESENTATION_ITEM('')
SURFACE()
);
#3441=(
BOUNDED_SURFACE()
B_SPLINE_SURFACE(3,2,((#244478,#244479,#244480),(#244481,#244482,#244483),
(#244484,#244485,#244486),(#244487,#244488,#244489)),.UNSPECIFIED.,.F.,
 .F.,.F.)
B_SPLINE_SURFACE_WITH_KNOTS((4,4),(3,3),(0.,0.000397394465448304),(0.,1.),
 .UNSPECIFIED.)
GEOMETRIC_REPRESENTATION_ITEM()
RATIONAL_B_SPLINE_SURFACE(((1.,0.705498956110762,1.),(1.,0.705821764811753,
1.),(1.,0.706461952521157,1.),(1.,0.707106781186548,1.)))
REPRESENTATION_ITEM('')
SURFACE()
);
#3442=(
BOUNDED_SURFACE()
B_SPLINE_SURFACE(3,2,((#244495,#244496,#244497),(#244498,#244499,#244500),
(#244501,#244502,#244503),(#244504,#244505,#244506)),.UNSPECIFIED.,.F.,
 .F.,.F.)
B_SPLINE_SURFACE_WITH_KNOTS((4,4),(3,3),(0.,0.000397394410828741),(0.,1.),
 .UNSPECIFIED.)
GEOMETRIC_REPRESENTATION_ITEM()
RATIONAL_B_SPLINE_SURFACE(((1.,0.708689770883328,1.),(1.,0.708376440034484,
1.),(1.,0.7077504986984,1.),(1.,0.707106781186561,1.)))
REPRESENTATION_ITEM('')
SURFACE()
);
#3443=(
BOUNDED_SURFACE()
B_SPLINE_SURFACE(3,2,((#244512,#244513,#244514),(#244515,#244516,#244517),
(#244518,#244519,#244520),(#244521,#244522,#244523)),.UNSPECIFIED.,.F.,
 .F.,.F.)
B_SPLINE_SURFACE_WITH_KNOTS((4,4),(3,3),(0.,0.000511815090126166),(0.,1.00105592270446),
 .UNSPECIFIED.)
GEOMETRIC_REPRESENTATION_ITEM()
RATIONAL_B_SPLINE_SURFACE(((1.,0.705266242716819,1.00062243213217),(1.,
0.705584085908485,1.00062176089648),(1.,0.706182089449831,1.00062049800545),
(1.,0.706797508586823,1.00061919833537)))
REPRESENTATION_ITEM('')
SURFACE()
);
#3444=(
BOUNDED_SURFACE()
B_SPLINE_SURFACE(3,2,((#244525,#244526,#244527),(#244528,#244529,#244530),
(#244531,#244532,#244533),(#244534,#244535,#244536)),.UNSPECIFIED.,.F.,
 .F.,.F.)
B_SPLINE_SURFACE_WITH_KNOTS((4,4),(3,3),(5.6920614055489E-19,0.000397394428086632),
(0.,1.),.UNSPECIFIED.)
GEOMETRIC_REPRESENTATION_ITEM()
RATIONAL_B_SPLINE_SURFACE(((1.,0.707106781186555,1.),(1.,0.706459846759096,
1.),(1.,0.705820510737272,1.),(1.,0.705498956110754,1.)))
REPRESENTATION_ITEM('')
SURFACE()
);
#3445=(
BOUNDED_SURFACE()
B_SPLINE_SURFACE(3,2,((#244542,#244543,#244544),(#244545,#244546,#244547),
(#244548,#244549,#244550),(#244551,#244552,#244553),(#244554,#244555,#244556),
(#244557,#244558,#244559)),.UNSPECIFIED.,.F.,.F.,.F.)
B_SPLINE_SURFACE_WITH_KNOTS((4,2,4),(3,3),(0.,0.000257953807872845,0.00051590761574569),
(0.,1.),.UNSPECIFIED.)
GEOMETRIC_REPRESENTATION_ITEM()
RATIONAL_B_SPLINE_SURFACE(((1.,0.874619707139396,1.),(1.,0.874834349679282,
1.),(1.,0.854686104157417,1.),(1.,0.792476597915543,1.),(1.,0.750887854594793,
1.),(1.,0.705585838031461,1.)))
REPRESENTATION_ITEM('')
SURFACE()
);
#3446=(
BOUNDED_SURFACE()
B_SPLINE_SURFACE(3,2,((#244565,#244566,#244567),(#244568,#244569,#244570),
(#244571,#244572,#244573),(#244574,#244575,#244576)),.UNSPECIFIED.,.F.,
 .F.,.F.)
B_SPLINE_SURFACE_WITH_KNOTS((4,4),(3,3),(0.,0.000511815437699145),(0.,1.00105881331729),
 .UNSPECIFIED.)
GEOMETRIC_REPRESENTATION_ITEM()
RATIONAL_B_SPLINE_SURFACE(((1.,0.706796661945924,1.00062089519801),(1.,
0.707430821224786,1.00061955228543),(1.,0.708058545830317,1.00061822299909),
(1.,0.708394505252299,1.00061751156247)))
REPRESENTATION_ITEM('')
SURFACE()
);
#3447=(
BOUNDED_SURFACE()
B_SPLINE_SURFACE(3,2,((#244578,#244579,#244580),(#244581,#244582,#244583),
(#244584,#244585,#244586),(#244587,#244588,#244589),(#244590,#244591,#244592),
(#244593,#244594,#244595)),.UNSPECIFIED.,.F.,.F.,.F.)
B_SPLINE_SURFACE_WITH_KNOTS((4,2,4),(3,3),(0.,0.00025691531753127,0.00051383063506254),
(0.,1.),.UNSPECIFIED.)
GEOMETRIC_REPRESENTATION_ITEM()
RATIONAL_B_SPLINE_SURFACE(((1.,0.705585838031444,1.),(1.,0.75090243354346,
1.),(1.,0.792329530081589,1.),(1.,0.854288401595151,1.),(1.,0.874998031124432,
1.),(1.,0.87461970713941,1.)))
REPRESENTATION_ITEM('')
SURFACE()
);
#3448=(
BOUNDED_SURFACE()
B_SPLINE_SURFACE(3,2,((#244601,#244602,#244603),(#244604,#244605,#244606),
(#244607,#244608,#244609),(#244610,#244611,#244612),(#244613,#244614,#244615),
(#244616,#244617,#244618)),.UNSPECIFIED.,.F.,.F.,.F.)
B_SPLINE_SURFACE_WITH_KNOTS((4,2,4),(3,3),(-3.95733792957209E-18,0.000256592814262154,
0.000513185628524312),(0.,1.),.UNSPECIFIED.)
GEOMETRIC_REPRESENTATION_ITEM()
RATIONAL_B_SPLINE_SURFACE(((1.,0.708712527163665,1.),(1.,0.753780902613942,
1.),(1.,0.794538995768714,1.),(1.,0.855070770331582,1.),(1.,0.875018427444968,
1.),(1.,0.874619707139392,1.)))
REPRESENTATION_ITEM('')
SURFACE()
);
#3449=(
BOUNDED_SURFACE()
B_SPLINE_SURFACE(3,2,((#244620,#244621,#244622),(#244623,#244624,#244625),
(#244626,#244627,#244628),(#244629,#244630,#244631)),.UNSPECIFIED.,.F.,
 .F.,.F.)
B_SPLINE_SURFACE_WITH_KNOTS((4,4),(3,3),(5.6920614055489E-19,0.000511815072430398),
(0.,1.00105598366039),.UNSPECIFIED.)
GEOMETRIC_REPRESENTATION_ITEM()
RATIONAL_B_SPLINE_SURFACE(((1.,0.706797490733239,1.00061923411794),(1.,
0.706182062146141,1.00062053388301),(1.,0.705584062768533,1.00062179683815),
(1.,0.70526622476999,1.00062246810162)))
REPRESENTATION_ITEM('')
SURFACE()
);
#3450=(
BOUNDED_SURFACE()
B_SPLINE_SURFACE(3,2,((#244637,#244638,#244639),(#244640,#244641,#244642),
(#244643,#244644,#244645),(#244646,#244647,#244648),(#244649,#244650,#244651),
(#244652,#244653,#244654)),.UNSPECIFIED.,.F.,.F.,.F.)
B_SPLINE_SURFACE_WITH_KNOTS((4,2,4),(3,3),(-3.42878937048541E-18,0.000257652232350883,
0.000515304464701769),(0.,1.),.UNSPECIFIED.)
GEOMETRIC_REPRESENTATION_ITEM()
RATIONAL_B_SPLINE_SURFACE(((1.,0.874619707139372,1.),(1.,0.874861180430602,
1.),(1.,0.855455725920989,1.),(1.,0.794699358955127,1.),(1.,0.753768977788718,
1.),(1.,0.70871252716366,1.)))
REPRESENTATION_ITEM('')
SURFACE()
);
#3451=(
BOUNDED_SURFACE()
B_SPLINE_SURFACE(3,2,((#244660,#244661,#244662),(#244663,#244664,#244665),
(#244666,#244667,#244668),(#244669,#244670,#244671)),.UNSPECIFIED.,.F.,
 .F.,.F.)
B_SPLINE_SURFACE_WITH_KNOTS((4,4),(3,3),(0.,0.000397394373651921),(0.,1.),
 .UNSPECIFIED.)
GEOMETRIC_REPRESENTATION_ITEM()
RATIONAL_B_SPLINE_SURFACE(((1.,0.70710678118654,1.),(1.,0.707752587915911,
1.),(1.,0.70837765454067,1.),(1.,0.708689770883334,1.)))
REPRESENTATION_ITEM('')
SURFACE()
);
#3452=(
BOUNDED_SURFACE()
B_SPLINE_SURFACE(3,2,((#244673,#244674,#244675),(#244676,#244677,#244678),
(#244679,#244680,#244681),(#244682,#244683,#244684)),.UNSPECIFIED.,.F.,
 .F.,.F.)
B_SPLINE_SURFACE_WITH_KNOTS((4,4),(3,3),(-1.59919820441612E-18,0.000511815456479788),
(0.,1.00105873159859),.UNSPECIFIED.)
GEOMETRIC_REPRESENTATION_ITEM()
RATIONAL_B_SPLINE_SURFACE(((1.,0.708394529056712,1.00061746385282),(1.,
0.708058564167312,1.00061817524611),(1.,0.70743083537244,1.00061950443873),
(1.,0.70679668588077,1.00062084722694)))
REPRESENTATION_ITEM('')
SURFACE()
);
#3453=(
BOUNDED_SURFACE()
B_SPLINE_SURFACE(3,2,((#244690,#244691,#244692),(#244693,#244694,#244695),
(#244696,#244697,#244698),(#244699,#244700,#244701)),.UNSPECIFIED.,.F.,
 .F.,.F.)
B_SPLINE_SURFACE_WITH_KNOTS((4,4),(3,3),(0.,0.000397394465448327),(0.,1.),
 .UNSPECIFIED.)
GEOMETRIC_REPRESENTATION_ITEM()
RATIONAL_B_SPLINE_SURFACE(((1.,0.705498956110748,1.),(1.,0.705821764811772,
1.),(1.,0.706461952521144,1.),(1.,0.707106781186546,1.)))
REPRESENTATION_ITEM('')
SURFACE()
);
#3454=(
BOUNDED_SURFACE()
B_SPLINE_SURFACE(3,2,((#244707,#244708,#244709),(#244710,#244711,#244712),
(#244713,#244714,#244715),(#244716,#244717,#244718)),.UNSPECIFIED.,.F.,
 .F.,.F.)
B_SPLINE_SURFACE_WITH_KNOTS((4,4),(3,3),(0.,0.000397394410828723),(0.,1.),
 .UNSPECIFIED.)
GEOMETRIC_REPRESENTATION_ITEM()
RATIONAL_B_SPLINE_SURFACE(((1.,0.708689770883336,1.),(1.,0.70837644003447,
1.),(1.,0.707750498698429,1.),(1.,0.707106781186541,1.)))
REPRESENTATION_ITEM('')
SURFACE()
);
#3455=(
BOUNDED_SURFACE()
B_SPLINE_SURFACE(3,2,((#244724,#244725,#244726),(#244727,#244728,#244729),
(#244730,#244731,#244732),(#244733,#244734,#244735)),.UNSPECIFIED.,.F.,
 .F.,.F.)
B_SPLINE_SURFACE_WITH_KNOTS((4,4),(3,3),(-4.01154803819637E-18,0.000511815090126176),
(0.,1.00105592270494),.UNSPECIFIED.)
GEOMETRIC_REPRESENTATION_ITEM()
RATIONAL_B_SPLINE_SURFACE(((1.,0.705266242716679,1.00062243213246),(1.,
0.705584085908372,1.00062176089677),(1.,0.706182089449679,1.00062049800574),
(1.,0.70679750858668,1.00061919833566)))
REPRESENTATION_ITEM('')
SURFACE()
);
#3456=(
BOUNDED_SURFACE()
B_SPLINE_SURFACE(3,2,((#244737,#244738,#244739),(#244740,#244741,#244742),
(#244743,#244744,#244745),(#244746,#244747,#244748)),.UNSPECIFIED.,.F.,
 .F.,.F.)
B_SPLINE_SURFACE_WITH_KNOTS((4,4),(3,3),(0.,0.000397394428086601),(0.,1.),
 .UNSPECIFIED.)
GEOMETRIC_REPRESENTATION_ITEM()
RATIONAL_B_SPLINE_SURFACE(((1.,0.707106781186548,1.),(1.,0.706459846759071,
1.),(1.,0.705820510737329,1.),(1.,0.70549895611073,1.)))
REPRESENTATION_ITEM('')
SURFACE()
);
#3457=(
BOUNDED_SURFACE()
B_SPLINE_SURFACE(3,2,((#244754,#244755,#244756),(#244757,#244758,#244759),
(#244760,#244761,#244762),(#244763,#244764,#244765),(#244766,#244767,#244768),
(#244769,#244770,#244771)),.UNSPECIFIED.,.F.,.F.,.F.)
B_SPLINE_SURFACE_WITH_KNOTS((4,2,4),(3,3),(0.,0.000257953807872844,0.000515907615745688),
(0.,1.),.UNSPECIFIED.)
GEOMETRIC_REPRESENTATION_ITEM()
RATIONAL_B_SPLINE_SURFACE(((1.,0.874619707139391,1.),(1.,0.874834349679489,
1.),(1.,0.854686104157156,1.),(1.,0.792476597915762,1.),(1.,0.750887854594684,
1.),(1.,0.705585838031417,1.)))
REPRESENTATION_ITEM('')
SURFACE()
);
#3458=(
BOUNDED_SURFACE()
B_SPLINE_SURFACE(3,2,((#244777,#244778,#244779),(#244780,#244781,#244782),
(#244783,#244784,#244785),(#244786,#244787,#244788)),.UNSPECIFIED.,.F.,
 .F.,.F.)
B_SPLINE_SURFACE_WITH_KNOTS((4,4),(3,3),(-5.6920614055489E-19,0.00051181543769916),
(0.,1.00105881331573),.UNSPECIFIED.)
GEOMETRIC_REPRESENTATION_ITEM()
RATIONAL_B_SPLINE_SURFACE(((1.,0.706796661946382,1.0006208951971),(1.,0.707430821225235,
1.00061955228452),(1.,0.708058545830781,1.00061822299818),(1.,0.708394505252767,
1.00061751156156)))
REPRESENTATION_ITEM('')
SURFACE()
);
#3459=(
BOUNDED_SURFACE()
B_SPLINE_SURFACE(3,2,((#244790,#244791,#244792),(#244793,#244794,#244795),
(#244796,#244797,#244798),(#244799,#244800,#244801),(#244802,#244803,#244804),
(#244805,#244806,#244807)),.UNSPECIFIED.,.F.,.F.,.F.)
B_SPLINE_SURFACE_WITH_KNOTS((4,2,4),(3,3),(-3.52365706057789E-19,0.000256915317531259,
0.000513830635062519),(0.,1.),.UNSPECIFIED.)
GEOMETRIC_REPRESENTATION_ITEM()
RATIONAL_B_SPLINE_SURFACE(((1.,0.705585838031437,1.),(1.,0.750902433542628,
1.),(1.,0.792329530082712,1.),(1.,0.854288401594017,1.),(1.,0.874998031125283,
1.),(1.,0.87461970713941,1.)))
REPRESENTATION_ITEM('')
SURFACE()
);
#3460=(
BOUNDED_SURFACE()
B_SPLINE_SURFACE(3,2,((#244813,#244814,#244815),(#244816,#244817,#244818),
(#244819,#244820,#244821),(#244822,#244823,#244824),(#244825,#244826,#244827),
(#244828,#244829,#244830)),.UNSPECIFIED.,.F.,.F.,.F.)
B_SPLINE_SURFACE_WITH_KNOTS((4,2,4),(3,3),(0.,0.000256592814262159,0.000513185628524318),
(0.,1.),.UNSPECIFIED.)
GEOMETRIC_REPRESENTATION_ITEM()
RATIONAL_B_SPLINE_SURFACE(((1.,0.708712527163661,1.),(1.,0.753780902613338,
1.),(1.,0.794538995769515,1.),(1.,0.855070770330818,1.),(1.,0.875018427445545,
1.),(1.,0.874619707139392,1.)))
REPRESENTATION_ITEM('')
SURFACE()
);
#3461=(
BOUNDED_SURFACE()
B_SPLINE_SURFACE(3,2,((#244832,#244833,#244834),(#244835,#244836,#244837),
(#244838,#244839,#244840),(#244841,#244842,#244843)),.UNSPECIFIED.,.F.,
 .F.,.F.)
B_SPLINE_SURFACE_WITH_KNOTS((4,4),(3,3),(-2.71050543121376E-20,0.000511815072430398),
(0.,1.00105598365999),.UNSPECIFIED.)
GEOMETRIC_REPRESENTATION_ITEM()
RATIONAL_B_SPLINE_SURFACE(((1.,0.706797490733357,1.00061923411771),(1.,
0.706182062146283,1.00062053388277),(1.,0.705584062768626,1.00062179683791),
(1.,0.705266224770118,1.00062246810138)))
REPRESENTATION_ITEM('')
SURFACE()
);
#3462=(
BOUNDED_SURFACE()
B_SPLINE_SURFACE(3,2,((#244849,#244850,#244851),(#244852,#244853,#244854),
(#244855,#244856,#244857),(#244858,#244859,#244860),(#244861,#244862,#244863),
(#244864,#244865,#244866)),.UNSPECIFIED.,.F.,.F.,.F.)
B_SPLINE_SURFACE_WITH_KNOTS((4,2,4),(3,3),(0.,0.000257652232350886,0.000515304464701772),
(0.,1.),.UNSPECIFIED.)
GEOMETRIC_REPRESENTATION_ITEM()
RATIONAL_B_SPLINE_SURFACE(((1.,0.874619707139399,1.),(1.,0.874861180430627,
1.),(1.,0.855455725920946,1.),(1.,0.794699358955181,1.),(1.,0.753768977788717,
1.),(1.,0.70871252716364,1.)))
REPRESENTATION_ITEM('')
SURFACE()
);
#3463=(
BOUNDED_SURFACE()
B_SPLINE_SURFACE(3,2,((#244872,#244873,#244874),(#244875,#244876,#244877),
(#244878,#244879,#244880),(#244881,#244882,#244883)),.UNSPECIFIED.,.F.,
 .F.,.F.)
B_SPLINE_SURFACE_WITH_KNOTS((4,4),(3,3),(-6.50521303491303E-19,0.000397394373651923),
(0.,1.),.UNSPECIFIED.)
GEOMETRIC_REPRESENTATION_ITEM()
RATIONAL_B_SPLINE_SURFACE(((1.,0.707106781186546,1.),(1.,0.707752587915898,
1.),(1.,0.708377654540671,1.),(1.,0.708689770883336,1.)))
REPRESENTATION_ITEM('')
SURFACE()
);
#3464=(
BOUNDED_SURFACE()
B_SPLINE_SURFACE(3,2,((#244885,#244886,#244887),(#244888,#244889,#244890),
(#244891,#244892,#244893),(#244894,#244895,#244896)),.UNSPECIFIED.,.F.,
 .F.,.F.)
B_SPLINE_SURFACE_WITH_KNOTS((4,4),(3,3),(0.,0.000511815456479791),(0.,1.00105873160122),
 .UNSPECIFIED.)
GEOMETRIC_REPRESENTATION_ITEM()
RATIONAL_B_SPLINE_SURFACE(((1.,0.708394529055968,1.00061746385436),(1.,
0.708058564166503,1.00061817524765),(1.,0.707430835371682,1.00061950444027),
(1.,0.706796685880003,1.00062084722849)))
REPRESENTATION_ITEM('')
SURFACE()
);
#3465=(
BOUNDED_SURFACE()
B_SPLINE_SURFACE(3,2,((#244902,#244903,#244904),(#244905,#244906,#244907),
(#244908,#244909,#244910),(#244911,#244912,#244913)),.UNSPECIFIED.,.F.,
 .F.,.F.)
B_SPLINE_SURFACE_WITH_KNOTS((4,4),(3,3),(0.,0.0003973944654483),(0.,1.),
 .UNSPECIFIED.)
GEOMETRIC_REPRESENTATION_ITEM()
RATIONAL_B_SPLINE_SURFACE(((1.,0.705498956110742,1.),(1.,0.70582176481179,
1.),(1.,0.70646195252114,1.),(1.,0.707106781186547,1.)))
REPRESENTATION_ITEM('')
SURFACE()
);
#3466=(
BOUNDED_SURFACE()
B_SPLINE_SURFACE(3,2,((#244919,#244920,#244921),(#244922,#244923,#244924),
(#244925,#244926,#244927),(#244928,#244929,#244930)),.UNSPECIFIED.,.F.,
 .F.,.F.)
B_SPLINE_SURFACE_WITH_KNOTS((4,4),(3,3),(0.,0.000397394410828726),(0.,1.),
 .UNSPECIFIED.)
GEOMETRIC_REPRESENTATION_ITEM()
RATIONAL_B_SPLINE_SURFACE(((1.,0.708689770883339,1.),(1.,0.708376440034475,
1.),(1.,0.707750498698421,1.),(1.,0.707106781186549,1.)))
REPRESENTATION_ITEM('')
SURFACE()
);
#3467=(
BOUNDED_SURFACE()
B_SPLINE_SURFACE(3,2,((#244936,#244937,#244938),(#244939,#244940,#244941),
(#244942,#244943,#244944),(#244945,#244946,#244947)),.UNSPECIFIED.,.F.,
 .F.,.F.)
B_SPLINE_SURFACE_WITH_KNOTS((4,4),(3,3),(-3.22550146314438E-18,0.00051181509012618),
(0.,1.00105592270442),.UNSPECIFIED.)
GEOMETRIC_REPRESENTATION_ITEM()
RATIONAL_B_SPLINE_SURFACE(((1.,0.705266242716829,1.00062243213215),(1.,
0.70558408590849,1.00062176089647),(1.,0.706182089449834,1.00062049800543),
(1.,0.706797508586832,1.00061919833535)))
REPRESENTATION_ITEM('')
SURFACE()
);
#3468=(
BOUNDED_SURFACE()
B_SPLINE_SURFACE(3,2,((#244949,#244950,#244951),(#244952,#244953,#244954),
(#244955,#244956,#244957),(#244958,#244959,#244960)),.UNSPECIFIED.,.F.,
 .F.,.F.)
B_SPLINE_SURFACE_WITH_KNOTS((4,4),(3,3),(0.,0.00039739442808661),(0.,1.),
 .UNSPECIFIED.)
GEOMETRIC_REPRESENTATION_ITEM()
RATIONAL_B_SPLINE_SURFACE(((1.,0.70710678118654,1.),(1.,0.706459846759122,
1.),(1.,0.705820510737254,1.),(1.,0.705498956110749,1.)))
REPRESENTATION_ITEM('')
SURFACE()
);
#3469=(
BOUNDED_SURFACE()
B_SPLINE_SURFACE(3,2,((#244966,#244967,#244968),(#244969,#244970,#244971),
(#244972,#244973,#244974),(#244975,#244976,#244977),(#244978,#244979,#244980),
(#244981,#244982,#244983)),.UNSPECIFIED.,.F.,.F.,.F.)
B_SPLINE_SURFACE_WITH_KNOTS((4,2,4),(3,3),(0.,0.000257953807872843,0.000515907615745687),
(0.,1.),.UNSPECIFIED.)
GEOMETRIC_REPRESENTATION_ITEM()
RATIONAL_B_SPLINE_SURFACE(((1.,0.874619707139395,1.),(1.,0.874834349679314,
1.),(1.,0.854686104157372,1.),(1.,0.792476597915575,1.),(1.,0.750887854594771,
1.),(1.,0.705585838031435,1.)))
REPRESENTATION_ITEM('')
SURFACE()
);
#3470=(
BOUNDED_SURFACE()
B_SPLINE_SURFACE(3,2,((#244989,#244990,#244991),(#244992,#244993,#244994),
(#244995,#244996,#244997),(#244998,#244999,#245000)),.UNSPECIFIED.,.F.,
 .F.,.F.)
B_SPLINE_SURFACE_WITH_KNOTS((4,4),(3,3),(-5.6920614055489E-19,0.000511815437699148),
(0.,1.00105881331991),.UNSPECIFIED.)
GEOMETRIC_REPRESENTATION_ITEM()
RATIONAL_B_SPLINE_SURFACE(((1.,0.706796661945167,1.00062089519955),(1.,
0.707430821224023,1.00061955228697),(1.,0.70805854582955,1.00061822300062),
(1.,0.708394505251536,1.000617511564)))
REPRESENTATION_ITEM('')
SURFACE()
);
#3471=(
BOUNDED_SURFACE()
B_SPLINE_SURFACE(3,2,((#245002,#245003,#245004),(#245005,#245006,#245007),
(#245008,#245009,#245010),(#245011,#245012,#245013),(#245014,#245015,#245016),
(#245017,#245018,#245019)),.UNSPECIFIED.,.F.,.F.,.F.)
B_SPLINE_SURFACE_WITH_KNOTS((4,2,4),(3,3),(0.,0.000256915317531256,0.000513830635062513),
(0.,1.),.UNSPECIFIED.)
GEOMETRIC_REPRESENTATION_ITEM()
RATIONAL_B_SPLINE_SURFACE(((1.,0.705585838031439,1.),(1.,0.75090243354274,
1.),(1.,0.792329530082544,1.),(1.,0.854288401594183,1.),(1.,0.874998031125163,
1.),(1.,0.874619707139398,1.)))
REPRESENTATION_ITEM('')
SURFACE()
);
#3472=(
BOUNDED_SURFACE()
B_SPLINE_SURFACE(3,2,((#245025,#245026,#245027),(#245028,#245029,#245030),
(#245031,#245032,#245033),(#245034,#245035,#245036),(#245037,#245038,#245039),
(#245040,#245041,#245042)),.UNSPECIFIED.,.F.,.F.,.F.)
B_SPLINE_SURFACE_WITH_KNOTS((4,2,4),(3,3),(0.,0.000256592814262157,0.000513185628524315),
(0.,1.),.UNSPECIFIED.)
GEOMETRIC_REPRESENTATION_ITEM()
RATIONAL_B_SPLINE_SURFACE(((1.,0.708712527163663,1.),(1.,0.75378090261347,
1.),(1.,0.794538995769367,1.),(1.,0.855070770330937,1.),(1.,0.875018427445453,
1.),(1.,0.874619707139386,1.)))
REPRESENTATION_ITEM('')
SURFACE()
);
#3473=(
BOUNDED_SURFACE()
B_SPLINE_SURFACE(3,2,((#245044,#245045,#245046),(#245047,#245048,#245049),
(#245050,#245051,#245052),(#245053,#245054,#245055)),.UNSPECIFIED.,.F.,
 .F.,.F.)
B_SPLINE_SURFACE_WITH_KNOTS((4,4),(3,3),(0.,0.000511815072430399),(0.,1.0010559836589),
 .UNSPECIFIED.)
GEOMETRIC_REPRESENTATION_ITEM()
RATIONAL_B_SPLINE_SURFACE(((1.,0.706797490733676,1.00061923411707),(1.,
0.706182062146617,1.00062053388213),(1.,0.705584062768934,1.00062179683727),
(1.,0.705266224770433,1.00062246810074)))
REPRESENTATION_ITEM('')
SURFACE()
);
#3474=(
BOUNDED_SURFACE()
B_SPLINE_SURFACE(3,2,((#245061,#245062,#245063),(#245064,#245065,#245066),
(#245067,#245068,#245069),(#245070,#245071,#245072),(#245073,#245074,#245075),
(#245076,#245077,#245078)),.UNSPECIFIED.,.F.,.F.,.F.)
B_SPLINE_SURFACE_WITH_KNOTS((4,2,4),(3,3),(-3.1712913545201E-18,0.000257652232350882,
0.000515304464701766),(0.,1.),.UNSPECIFIED.)
GEOMETRIC_REPRESENTATION_ITEM()
RATIONAL_B_SPLINE_SURFACE(((1.,0.874619707139392,1.),(1.,0.874861180430489,
1.),(1.,0.855455725921166,1.),(1.,0.794699358954979,1.),(1.,0.75376897778886,
1.),(1.,0.708712527163655,1.)))
REPRESENTATION_ITEM('')
SURFACE()
);
#3475=(
BOUNDED_SURFACE()
B_SPLINE_SURFACE(3,2,((#245084,#245085,#245086),(#245087,#245088,#245089),
(#245090,#245091,#245092),(#245093,#245094,#245095)),.UNSPECIFIED.,.F.,
 .F.,.F.)
B_SPLINE_SURFACE_WITH_KNOTS((4,4),(3,3),(2.71050543121376E-20,0.000397394373651917),
(0.,1.),.UNSPECIFIED.)
GEOMETRIC_REPRESENTATION_ITEM()
RATIONAL_B_SPLINE_SURFACE(((1.,0.707106781186545,1.),(1.,0.707752587915855,
1.),(1.,0.70837765454072,1.),(1.,0.708689770883334,1.)))
REPRESENTATION_ITEM('')
SURFACE()
);
#3476=(
BOUNDED_SURFACE()
B_SPLINE_SURFACE(3,2,((#245097,#245098,#245099),(#245100,#245101,#245102),
(#245103,#245104,#245105),(#245106,#245107,#245108)),.UNSPECIFIED.,.F.,
 .F.,.F.)
B_SPLINE_SURFACE_WITH_KNOTS((4,4),(3,3),(0.,0.000511815456479795),(0.,1.00105873159796),
 .UNSPECIFIED.)
GEOMETRIC_REPRESENTATION_ITEM()
RATIONAL_B_SPLINE_SURFACE(((1.,0.708394529056934,1.00061746385245),(1.,
0.708058564167418,1.00061817524574),(1.,0.707430835372665,1.00061950443836),
(1.,0.706796685880961,1.00062084722657)))
REPRESENTATION_ITEM('')
SURFACE()
);
#3477=(
BOUNDED_SURFACE()
B_SPLINE_SURFACE(3,2,((#245114,#245115,#245116),(#245117,#245118,#245119),
(#245120,#245121,#245122),(#245123,#245124,#245125)),.UNSPECIFIED.,.F.,
 .F.,.F.)
B_SPLINE_SURFACE_WITH_KNOTS((4,4),(3,3),(0.,0.000397394465448323),(0.,1.),
 .UNSPECIFIED.)
GEOMETRIC_REPRESENTATION_ITEM()
RATIONAL_B_SPLINE_SURFACE(((1.,0.705498956110748,1.),(1.,0.705821764811774,
1.),(1.,0.706461952521149,1.),(1.,0.707106781186538,1.)))
REPRESENTATION_ITEM('')
SURFACE()
);
#3478=(
BOUNDED_SURFACE()
B_SPLINE_SURFACE(3,2,((#245131,#245132,#245133),(#245134,#245135,#245136),
(#245137,#245138,#245139),(#245140,#245141,#245142)),.UNSPECIFIED.,.F.,
 .F.,.F.)
B_SPLINE_SURFACE_WITH_KNOTS((4,4),(3,3),(0.,0.000397394410828735),(0.,1.),
 .UNSPECIFIED.)
GEOMETRIC_REPRESENTATION_ITEM()
RATIONAL_B_SPLINE_SURFACE(((1.,0.708689770883322,1.),(1.,0.708376440034484,
1.),(1.,0.707750498698409,1.),(1.,0.70710678118656,1.)))
REPRESENTATION_ITEM('')
SURFACE()
);
#3479=(
BOUNDED_SURFACE()
B_SPLINE_SURFACE(3,2,((#245148,#245149,#245150),(#245151,#245152,#245153),
(#245154,#245155,#245156),(#245157,#245158,#245159)),.UNSPECIFIED.,.F.,
 .F.,.F.)
B_SPLINE_SURFACE_WITH_KNOTS((4,4),(3,3),(0.,0.000511815090126181),(0.,1.00105592270304),
 .UNSPECIFIED.)
GEOMETRIC_REPRESENTATION_ITEM()
RATIONAL_B_SPLINE_SURFACE(((1.,0.705266242717251,1.00062243213133),(1.,
0.705584085908867,1.00062176089565),(1.,0.706182089450269,1.00062049800462),
(1.,0.706797508587227,1.00061919833454)))
REPRESENTATION_ITEM('')
SURFACE()
);
#3480=(
BOUNDED_SURFACE()
B_SPLINE_SURFACE(3,2,((#245161,#245162,#245163),(#245164,#245165,#245166),
(#245167,#245168,#245169),(#245170,#245171,#245172)),.UNSPECIFIED.,.F.,
 .F.,.F.)
B_SPLINE_SURFACE_WITH_KNOTS((4,4),(3,3),(0.,0.000397394428086618),(0.,1.),
 .UNSPECIFIED.)
GEOMETRIC_REPRESENTATION_ITEM()
RATIONAL_B_SPLINE_SURFACE(((1.,0.707106781186571,1.),(1.,0.706459846759077,
1.),(1.,0.705820510737271,1.),(1.,0.705498956110762,1.)))
REPRESENTATION_ITEM('')
SURFACE()
);
#3481=(
BOUNDED_SURFACE()
B_SPLINE_SURFACE(3,2,((#245178,#245179,#245180),(#245181,#245182,#245183),
(#245184,#245185,#245186),(#245187,#245188,#245189),(#245190,#245191,#245192),
(#245193,#245194,#245195)),.UNSPECIFIED.,.F.,.F.,.F.)
B_SPLINE_SURFACE_WITH_KNOTS((4,2,4),(3,3),(5.01443504774546E-19,0.000257953807872845,
0.00051590761574569),(0.,1.),.UNSPECIFIED.)
GEOMETRIC_REPRESENTATION_ITEM()
RATIONAL_B_SPLINE_SURFACE(((1.,0.874619707139404,1.),(1.,0.874834349678571,
1.),(1.,0.854686104158358,1.),(1.,0.792476597914571,1.),(1.,0.750887854595536,
1.),(1.,0.705585838031444,1.)))
REPRESENTATION_ITEM('')
SURFACE()
);
#3482=(
BOUNDED_SURFACE()
B_SPLINE_SURFACE(3,2,((#245201,#245202,#245203),(#245204,#245205,#245206),
(#245207,#245208,#245209),(#245210,#245211,#245212)),.UNSPECIFIED.,.F.,
 .F.,.F.)
B_SPLINE_SURFACE_WITH_KNOTS((4,4),(3,3),(0.,0.000511815437699152),(0.,1.00105881331367),
 .UNSPECIFIED.)
GEOMETRIC_REPRESENTATION_ITEM()
RATIONAL_B_SPLINE_SURFACE(((1.,0.706796661946975,1.00062089519589),(1.,
0.707430821225895,1.00061955228331),(1.,0.708058545831334,1.00061822299697),
(1.,0.708394505253363,1.00061751156035)))
REPRESENTATION_ITEM('')
SURFACE()
);
#3483=(
BOUNDED_SURFACE()
B_SPLINE_SURFACE(3,2,((#245214,#245215,#245216),(#245217,#245218,#245219),
(#245220,#245221,#245222),(#245223,#245224,#245225),(#245226,#245227,#245228),
(#245229,#245230,#245231)),.UNSPECIFIED.,.F.,.F.,.F.)
B_SPLINE_SURFACE_WITH_KNOTS((4,2,4),(3,3),(-2.84603070277445E-18,0.000256915317531263,
0.000513830635062529),(0.,1.),.UNSPECIFIED.)
GEOMETRIC_REPRESENTATION_ITEM()
RATIONAL_B_SPLINE_SURFACE(((1.,0.705585838031451,1.),(1.,0.750902433542774,
1.),(1.,0.792329530082481,1.),(1.,0.854288401594243,1.),(1.,0.87499803112512,
1.),(1.,0.874619707139395,1.)))
REPRESENTATION_ITEM('')
SURFACE()
);
#3484=(
BOUNDED_SURFACE()
B_SPLINE_SURFACE(3,2,((#245237,#245238,#245239),(#245240,#245241,#245242),
(#245243,#245244,#245245),(#245246,#245247,#245248),(#245249,#245250,#245251),
(#245252,#245253,#245254)),.UNSPECIFIED.,.F.,.F.,.F.)
B_SPLINE_SURFACE_WITH_KNOTS((4,2,4),(3,3),(-1.09233368877915E-17,0.000256592814262153,
0.000513185628524316),(0.,1.),.UNSPECIFIED.)
GEOMETRIC_REPRESENTATION_ITEM()
RATIONAL_B_SPLINE_SURFACE(((1.,0.708712527163668,1.),(1.,0.753780902613415,
1.),(1.,0.794538995769434,1.),(1.,0.855070770330872,1.),(1.,0.875018427445518,
1.),(1.,0.874619707139395,1.)))
REPRESENTATION_ITEM('')
SURFACE()
);
#3485=(
BOUNDED_SURFACE()
B_SPLINE_SURFACE(3,2,((#245256,#245257,#245258),(#245259,#245260,#245261),
(#245262,#245263,#245264),(#245265,#245266,#245267)),.UNSPECIFIED.,.F.,
 .F.,.F.)
B_SPLINE_SURFACE_WITH_KNOTS((4,4),(3,3),(0.,0.000511815072430409),(0.,1.0010559836586),
 .UNSPECIFIED.)
GEOMETRIC_REPRESENTATION_ITEM()
RATIONAL_B_SPLINE_SURFACE(((1.,0.706797490733765,1.00061923411689),(1.,
0.706182062146697,1.00062053388195),(1.,0.705584062769033,1.00062179683709),
(1.,0.705266224770523,1.00062246810056)))
REPRESENTATION_ITEM('')
SURFACE()
);
#3486=(
BOUNDED_SURFACE()
B_SPLINE_SURFACE(3,2,((#245273,#245274,#245275),(#245276,#245277,#245278),
(#245279,#245280,#245281),(#245282,#245283,#245284),(#245285,#245286,#245287),
(#245288,#245289,#245290)),.UNSPECIFIED.,.F.,.F.,.F.)
B_SPLINE_SURFACE_WITH_KNOTS((4,2,4),(3,3),(-9.52742659071637E-18,0.000257652232350881,
0.000515304464701771),(0.,1.),.UNSPECIFIED.)
GEOMETRIC_REPRESENTATION_ITEM()
RATIONAL_B_SPLINE_SURFACE(((1.,0.874619707139396,1.),(1.,0.874861180430588,
1.),(1.,0.855455725921017,1.),(1.,0.794699358955082,1.),(1.,0.753768977788791,
1.),(1.,0.70871252716365,1.)))
REPRESENTATION_ITEM('')
SURFACE()
);
#3487=(
BOUNDED_SURFACE()
B_SPLINE_SURFACE(3,2,((#245296,#245297,#245298),(#245299,#245300,#245301),
(#245302,#245303,#245304),(#245305,#245306,#245307)),.UNSPECIFIED.,.F.,
 .F.,.F.)
B_SPLINE_SURFACE_WITH_KNOTS((4,4),(3,3),(-5.96311194867027E-19,0.000397394373651909),
(0.,1.),.UNSPECIFIED.)
GEOMETRIC_REPRESENTATION_ITEM()
RATIONAL_B_SPLINE_SURFACE(((1.,0.707106781186546,1.),(1.,0.707752587915895,
1.),(1.,0.708377654540719,1.),(1.,0.70868977088333,1.)))
REPRESENTATION_ITEM('')
SURFACE()
);
#3488=(
BOUNDED_SURFACE()
B_SPLINE_SURFACE(3,2,((#245309,#245310,#245311),(#245312,#245313,#245314),
(#245315,#245316,#245317),(#245318,#245319,#245320)),.UNSPECIFIED.,.F.,
 .F.,.F.)
B_SPLINE_SURFACE_WITH_KNOTS((4,4),(3,3),(0.,0.000511815456479797),(0.,1.00105873159678),
 .UNSPECIFIED.)
GEOMETRIC_REPRESENTATION_ITEM()
RATIONAL_B_SPLINE_SURFACE(((1.,0.708394529057283,1.00061746385176),(1.,
0.70805856416776,1.00061817524505),(1.,0.707430835373029,1.00061950443767),
(1.,0.706796685881307,1.00062084722587)))
REPRESENTATION_ITEM('')
SURFACE()
);
#3489=(
BOUNDED_SURFACE()
B_SPLINE_SURFACE(3,2,((#245326,#245327,#245328),(#245329,#245330,#245331),
(#245332,#245333,#245334),(#245335,#245336,#245337)),.UNSPECIFIED.,.F.,
 .F.,.F.)
B_SPLINE_SURFACE_WITH_KNOTS((4,4),(3,3),(0.,0.00039739446544831),(0.,1.),
 .UNSPECIFIED.)
GEOMETRIC_REPRESENTATION_ITEM()
RATIONAL_B_SPLINE_SURFACE(((1.,0.705498956110735,1.),(1.,0.705821764811779,
1.),(1.,0.70646195252112,1.),(1.,0.707106781186562,1.)))
REPRESENTATION_ITEM('')
SURFACE()
);
#3490=(
BOUNDED_SURFACE()
B_SPLINE_SURFACE(3,2,((#245343,#245344,#245345),(#245346,#245347,#245348),
(#245349,#245350,#245351),(#245352,#245353,#245354)),.UNSPECIFIED.,.F.,
 .F.,.F.)
B_SPLINE_SURFACE_WITH_KNOTS((4,4),(3,3),(0.,0.000397394410828739),(0.,1.),
 .UNSPECIFIED.)
GEOMETRIC_REPRESENTATION_ITEM()
RATIONAL_B_SPLINE_SURFACE(((1.,0.708689770883341,1.),(1.,0.708376440034489,
1.),(1.,0.70775049869842,1.),(1.,0.707106781186549,1.)))
REPRESENTATION_ITEM('')
SURFACE()
);
#3491=(
BOUNDED_SURFACE()
B_SPLINE_SURFACE(3,2,((#245360,#245361,#245362),(#245363,#245364,#245365),
(#245366,#245367,#245368),(#245369,#245370,#245371)),.UNSPECIFIED.,.F.,
 .F.,.F.)
B_SPLINE_SURFACE_WITH_KNOTS((4,4),(3,3),(-1.59919820441612E-18,0.000511815090126168),
(0.,1.00105592270431),.UNSPECIFIED.)
GEOMETRIC_REPRESENTATION_ITEM()
RATIONAL_B_SPLINE_SURFACE(((1.,0.705266242716864,1.00062243213208),(1.,
0.705584085908508,1.0006217608964),(1.,0.706182089449863,1.00062049800537),
(1.,0.706797508586865,1.00061919833529)))
REPRESENTATION_ITEM('')
SURFACE()
);
#3492=(
BOUNDED_SURFACE()
B_SPLINE_SURFACE(3,2,((#245373,#245374,#245375),(#245376,#245377,#245378),
(#245379,#245380,#245381),(#245382,#245383,#245384)),.UNSPECIFIED.,.F.,
 .F.,.F.)
B_SPLINE_SURFACE_WITH_KNOTS((4,4),(3,3),(0.,0.00039739442808662),(0.,1.),
 .UNSPECIFIED.)
GEOMETRIC_REPRESENTATION_ITEM()
RATIONAL_B_SPLINE_SURFACE(((1.,0.707106781186562,1.),(1.,0.706459846759107,
1.),(1.,0.705820510737251,1.),(1.,0.705498956110768,1.)))
REPRESENTATION_ITEM('')
SURFACE()
);
#3493=(
BOUNDED_SURFACE()
B_SPLINE_SURFACE(3,2,((#245390,#245391,#245392),(#245393,#245394,#245395),
(#245396,#245397,#245398),(#245399,#245400,#245401),(#245402,#245403,#245404),
(#245405,#245406,#245407)),.UNSPECIFIED.,.F.,.F.,.F.)
B_SPLINE_SURFACE_WITH_KNOTS((4,2,4),(3,3),(0.,0.000257953807872846,0.000515907615745693),
(0.,1.),.UNSPECIFIED.)
GEOMETRIC_REPRESENTATION_ITEM()
RATIONAL_B_SPLINE_SURFACE(((1.,0.874619707139391,1.),(1.,0.874834349679018,
1.),(1.,0.854686104157766,1.),(1.,0.792476597915161,1.),(1.,0.75088785459512,
1.),(1.,0.705585838031422,1.)))
REPRESENTATION_ITEM('')
SURFACE()
);
#3494=(
BOUNDED_SURFACE()
B_SPLINE_SURFACE(3,2,((#245413,#245414,#245415),(#245416,#245417,#245418),
(#245419,#245420,#245421),(#245422,#245423,#245424)),.UNSPECIFIED.,.F.,
 .F.,.F.)
B_SPLINE_SURFACE_WITH_KNOTS((4,4),(3,3),(-5.42101086242752E-20,0.000511815437699146),
(0.,1.00105881331879),.UNSPECIFIED.)
GEOMETRIC_REPRESENTATION_ITEM()
RATIONAL_B_SPLINE_SURFACE(((1.,0.706796661945487,1.00062089519889),(1.,
0.707430821224365,1.00061955228631),(1.,0.708058545829886,1.00061822299996),
(1.,0.708394505251882,1.00061751156334)))
REPRESENTATION_ITEM('')
SURFACE()
);
#3495=(
BOUNDED_SURFACE()
B_SPLINE_SURFACE(3,2,((#245426,#245427,#245428),(#245429,#245430,#245431),
(#245432,#245433,#245434),(#245435,#245436,#245437),(#245438,#245439,#245440),
(#245441,#245442,#245443)),.UNSPECIFIED.,.F.,.F.,.F.)
B_SPLINE_SURFACE_WITH_KNOTS((4,2,4),(3,3),(0.,0.000256915317531259,0.000513830635062518),
(0.,1.),.UNSPECIFIED.)
GEOMETRIC_REPRESENTATION_ITEM()
RATIONAL_B_SPLINE_SURFACE(((1.,0.705585838031442,1.),(1.,0.750902433542966,
1.),(1.,0.792329530082241,1.),(1.,0.854288401594463,1.),(1.,0.874998031124932,
1.),(1.,0.874619707139397,1.)))
REPRESENTATION_ITEM('')
SURFACE()
);
#3496=(
BOUNDED_SURFACE()
B_SPLINE_SURFACE(3,2,((#245449,#245450,#245451),(#245452,#245453,#245454),
(#245455,#245456,#245457),(#245458,#245459,#245460),(#245461,#245462,#245463),
(#245464,#245465,#245466)),.UNSPECIFIED.,.F.,.F.,.F.)
B_SPLINE_SURFACE_WITH_KNOTS((4,2,4),(3,3),(-1.05709711817337E-18,0.000256592814262156,
0.000513185628524313),(0.,1.),.UNSPECIFIED.)
GEOMETRIC_REPRESENTATION_ITEM()
RATIONAL_B_SPLINE_SURFACE(((1.,0.708712527163677,1.),(1.,0.753780902613637,
1.),(1.,0.79453899576914,1.),(1.,0.855070770331177,1.),(1.,0.875018427445286,
1.),(1.,0.874619707139395,1.)))
REPRESENTATION_ITEM('')
SURFACE()
);
#3497=(
BOUNDED_SURFACE()
B_SPLINE_SURFACE(3,2,((#245468,#245469,#245470),(#245471,#245472,#245473),
(#245474,#245475,#245476),(#245477,#245478,#245479)),.UNSPECIFIED.,.F.,
 .F.,.F.)
B_SPLINE_SURFACE_WITH_KNOTS((4,4),(3,3),(-1.35525271560688E-19,0.000511815072430405),
(0.,1.00105598365711),.UNSPECIFIED.)
GEOMETRIC_REPRESENTATION_ITEM()
RATIONAL_B_SPLINE_SURFACE(((1.,0.706797490734201,1.00061923411602),(1.,
0.706182062147124,1.00062053388108),(1.,0.705584062769492,1.00062179683622),
(1.,0.705266224770974,1.00062246809968)))
REPRESENTATION_ITEM('')
SURFACE()
);
#3498=(
BOUNDED_SURFACE()
B_SPLINE_SURFACE(3,2,((#245485,#245486,#245487),(#245488,#245489,#245490),
(#245491,#245492,#245493),(#245494,#245495,#245496),(#245497,#245498,#245499),
(#245500,#245501,#245502)),.UNSPECIFIED.,.F.,.F.,.F.)
B_SPLINE_SURFACE_WITH_KNOTS((4,2,4),(3,3),(0.,0.000257652232350885,0.00051530446470177),
(0.,1.),.UNSPECIFIED.)
GEOMETRIC_REPRESENTATION_ITEM()
RATIONAL_B_SPLINE_SURFACE(((1.,0.874619707139392,1.),(1.,0.874861180429708,
1.),(1.,0.855455725922225,1.),(1.,0.794699358953907,1.),(1.,0.753768977789676,
1.),(1.,0.70871252716366,1.)))
REPRESENTATION_ITEM('')
SURFACE()
);
#3499=(
BOUNDED_SURFACE()
B_SPLINE_SURFACE(3,2,((#245508,#245509,#245510),(#245511,#245512,#245513),
(#245514,#245515,#245516),(#245517,#245518,#245519)),.UNSPECIFIED.,.F.,
 .F.,.F.)
B_SPLINE_SURFACE_WITH_KNOTS((4,4),(3,3),(-1.5748036555352E-17,0.000397394373651906),
(0.,1.),.UNSPECIFIED.)
GEOMETRIC_REPRESENTATION_ITEM()
RATIONAL_B_SPLINE_SURFACE(((1.,0.707106781186546,1.),(1.,0.70775258791588,
1.),(1.,0.708377654540694,1.),(1.,0.708689770883323,1.)))
REPRESENTATION_ITEM('')
SURFACE()
);
#3500=(
BOUNDED_SURFACE()
B_SPLINE_SURFACE(3,2,((#245521,#245522,#245523),(#245524,#245525,#245526),
(#245527,#245528,#245529),(#245530,#245531,#245532)),.UNSPECIFIED.,.F.,
 .F.,.F.)
B_SPLINE_SURFACE_WITH_KNOTS((4,4),(3,3),(0.,0.000511815456479801),(0.,1.00105873159925),
 .UNSPECIFIED.)
GEOMETRIC_REPRESENTATION_ITEM()
RATIONAL_B_SPLINE_SURFACE(((1.,0.708394529056526,1.00061746385321),(1.,
0.708058564167044,1.0006181752465),(1.,0.707430835372304,1.00061950443912),
(1.,0.706796685880582,1.00062084722733)))
REPRESENTATION_ITEM('')
SURFACE()
);
#3501=(
BOUNDED_SURFACE()
B_SPLINE_SURFACE(3,2,((#245538,#245539,#245540),(#245541,#245542,#245543),
(#245544,#245545,#245546),(#245547,#245548,#245549)),.UNSPECIFIED.,.F.,
 .F.,.F.)
B_SPLINE_SURFACE_WITH_KNOTS((4,4),(3,3),(0.,0.000397394465448322),(0.,1.),
 .UNSPECIFIED.)
GEOMETRIC_REPRESENTATION_ITEM()
RATIONAL_B_SPLINE_SURFACE(((1.,0.705498956110752,1.),(1.,0.705821764811804,
1.),(1.,0.70646195252111,1.),(1.,0.707106781186559,1.)))
REPRESENTATION_ITEM('')
SURFACE()
);
#3502=(
BOUNDED_SURFACE()
B_SPLINE_SURFACE(3,2,((#245555,#245556,#245557),(#245558,#245559,#245560),
(#245561,#245562,#245563),(#245564,#245565,#245566)),.UNSPECIFIED.,.F.,
 .F.,.F.)
B_SPLINE_SURFACE_WITH_KNOTS((4,4),(3,3),(0.,0.00039739441082872),(0.,1.),
 .UNSPECIFIED.)
GEOMETRIC_REPRESENTATION_ITEM()
RATIONAL_B_SPLINE_SURFACE(((1.,0.708689770883314,1.),(1.,0.708376440034513,
1.),(1.,0.70775049869841,1.),(1.,0.707106781186537,1.)))
REPRESENTATION_ITEM('')
SURFACE()
);
#3503=(
BOUNDED_SURFACE()
B_SPLINE_SURFACE(3,2,((#245572,#245573,#245574),(#245575,#245576,#245577),
(#245578,#245579,#245580),(#245581,#245582,#245583)),.UNSPECIFIED.,.F.,
 .F.,.F.)
B_SPLINE_SURFACE_WITH_KNOTS((4,4),(3,3),(0.,0.000511815090126186),(0.,1.00105592270166),
 .UNSPECIFIED.)
GEOMETRIC_REPRESENTATION_ITEM()
RATIONAL_B_SPLINE_SURFACE(((1.,0.705266242717654,1.00062243213052),(1.,
0.705584085909304,1.00062176089484),(1.,0.706182089450655,1.00062049800381),
(1.,0.706797508587642,1.00061919833373)))
REPRESENTATION_ITEM('')
SURFACE()
);
#3504=(
BOUNDED_SURFACE()
B_SPLINE_SURFACE(3,2,((#245585,#245586,#245587),(#245588,#245589,#245590),
(#245591,#245592,#245593),(#245594,#245595,#245596)),.UNSPECIFIED.,.F.,
 .F.,.F.)
B_SPLINE_SURFACE_WITH_KNOTS((4,4),(3,3),(-1.458251921993E-17,0.000397394428086608),
(0.,1.),.UNSPECIFIED.)
GEOMETRIC_REPRESENTATION_ITEM()
RATIONAL_B_SPLINE_SURFACE(((1.,0.707106781186551,1.),(1.,0.70645984675909,
1.),(1.,0.705820510737285,1.),(1.,0.705498956110753,1.)))
REPRESENTATION_ITEM('')
SURFACE()
);
#3505=(
BOUNDED_SURFACE()
B_SPLINE_SURFACE(3,2,((#245602,#245603,#245604),(#245605,#245606,#245607),
(#245608,#245609,#245610),(#245611,#245612,#245613),(#245614,#245615,#245616),
(#245617,#245618,#245619)),.UNSPECIFIED.,.F.,.F.,.F.)
B_SPLINE_SURFACE_WITH_KNOTS((4,2,4),(3,3),(0.,0.00025795380787285,0.000515907615745699),
(0.,1.),.UNSPECIFIED.)
GEOMETRIC_REPRESENTATION_ITEM()
RATIONAL_B_SPLINE_SURFACE(((1.,0.874619707139398,1.),(1.,0.874834349678536,
1.),(1.,0.854686104158402,1.),(1.,0.792476597914546,1.),(1.,0.7508878545956,
1.),(1.,0.705585838031444,1.)))
REPRESENTATION_ITEM('')
SURFACE()
);
#3506=(
BOUNDED_SURFACE()
B_SPLINE_SURFACE(3,2,((#245625,#245626,#245627),(#245628,#245629,#245630),
(#245631,#245632,#245633),(#245634,#245635,#245636)),.UNSPECIFIED.,.F.,
 .F.,.F.)
B_SPLINE_SURFACE_WITH_KNOTS((4,4),(3,3),(-5.6920614055489E-19,0.000511815437699162),
(0.,1.00105881331531),.UNSPECIFIED.)
GEOMETRIC_REPRESENTATION_ITEM()
RATIONAL_B_SPLINE_SURFACE(((1.,0.706796661946493,1.00062089519685),(1.,
0.707430821225386,1.00061955228427),(1.,0.708058545830895,1.00061822299793),
(1.,0.70839450525288,1.00061751156131)))
REPRESENTATION_ITEM('')
SURFACE()
);
#3507=(
BOUNDED_SURFACE()
B_SPLINE_SURFACE(3,2,((#245638,#245639,#245640),(#245641,#245642,#245643),
(#245644,#245645,#245646),(#245647,#245648,#245649),(#245650,#245651,#245652),
(#245653,#245654,#245655)),.UNSPECIFIED.,.F.,.F.,.F.)
B_SPLINE_SURFACE_WITH_KNOTS((4,2,4),(3,3),(0.,0.000256915317531261,0.000513830635062522),
(0.,1.),.UNSPECIFIED.)
GEOMETRIC_REPRESENTATION_ITEM()
RATIONAL_B_SPLINE_SURFACE(((1.,0.705585838031423,1.),(1.,0.750902433542322,
1.),(1.,0.792329530083111,1.),(1.,0.854288401593614,1.),(1.,0.874998031125594,
1.),(1.,0.874619707139391,1.)))
REPRESENTATION_ITEM('')
SURFACE()
);
#3508=(
BOUNDED_SURFACE()
B_SPLINE_SURFACE(3,2,((#245661,#245662,#245663),(#245664,#245665,#245666),
(#245667,#245668,#245669),(#245670,#245671,#245672),(#245673,#245674,#245675),
(#245676,#245677,#245678)),.UNSPECIFIED.,.F.,.F.,.F.)
B_SPLINE_SURFACE_WITH_KNOTS((4,2,4),(3,3),(-9.86623976961809E-18,0.000256592814262149,
0.000513185628524309),(0.,1.),.UNSPECIFIED.)
GEOMETRIC_REPRESENTATION_ITEM()
RATIONAL_B_SPLINE_SURFACE(((1.,0.708712527163638,1.),(1.,0.753780902613253,
1.),(1.,0.794538995769658,1.),(1.,0.855070770330655,1.),(1.,0.875018427445672,
1.),(1.,0.874619707139396,1.)))
REPRESENTATION_ITEM('')
SURFACE()
);
#3509=(
BOUNDED_SURFACE()
B_SPLINE_SURFACE(3,2,((#245680,#245681,#245682),(#245683,#245684,#245685),
(#245686,#245687,#245688),(#245689,#245690,#245691)),.UNSPECIFIED.,.F.,
 .F.,.F.)
B_SPLINE_SURFACE_WITH_KNOTS((4,4),(3,3),(5.42101086242752E-19,0.000511815072430404),
(0.,1.00105598366058),.UNSPECIFIED.)
GEOMETRIC_REPRESENTATION_ITEM()
RATIONAL_B_SPLINE_SURFACE(((1.,0.706797490733183,1.00061923411805),(1.,
0.706182062146105,1.00062053388312),(1.,0.705584062768457,1.00062179683826),
(1.,0.705266224769939,1.00062246810173)))
REPRESENTATION_ITEM('')
SURFACE()
);
#3510=(
BOUNDED_SURFACE()
B_SPLINE_SURFACE(3,2,((#245697,#245698,#245699),(#245700,#245701,#245702),
(#245703,#245704,#245705),(#245706,#245707,#245708),(#245709,#245710,#245711),
(#245712,#245713,#245714)),.UNSPECIFIED.,.F.,.F.,.F.)
B_SPLINE_SURFACE_WITH_KNOTS((4,2,4),(3,3),(-5.16351284646221E-18,0.000257652232350889,
0.000515304464701783),(0.,1.),.UNSPECIFIED.)
GEOMETRIC_REPRESENTATION_ITEM()
RATIONAL_B_SPLINE_SURFACE(((1.,0.874619707139395,1.),(1.,0.874861180431115,
1.),(1.,0.855455725920305,1.),(1.,0.794699358955837,1.),(1.,0.753768977788197,
1.),(1.,0.708712527163675,1.)))
REPRESENTATION_ITEM('')
SURFACE()
);
#3511=(
BOUNDED_SURFACE()
B_SPLINE_SURFACE(3,2,((#245720,#245721,#245722),(#245723,#245724,#245725),
(#245726,#245727,#245728),(#245729,#245730,#245731)),.UNSPECIFIED.,.F.,
 .F.,.F.)
B_SPLINE_SURFACE_WITH_KNOTS((4,4),(3,3),(0.,0.000397394373651917),(0.,1.),
 .UNSPECIFIED.)
GEOMETRIC_REPRESENTATION_ITEM()
RATIONAL_B_SPLINE_SURFACE(((1.,0.707106781186532,1.),(1.,0.707752587915907,
1.),(1.,0.708377654540682,1.),(1.,0.708689770883325,1.)))
REPRESENTATION_ITEM('')
SURFACE()
);
#3512=(
BOUNDED_SURFACE()
B_SPLINE_SURFACE(3,2,((#245733,#245734,#245735),(#245736,#245737,#245738),
(#245739,#245740,#245741),(#245742,#245743,#245744)),.UNSPECIFIED.,.F.,
 .F.,.F.)
B_SPLINE_SURFACE_WITH_KNOTS((4,4),(3,3),(-2.41234983378025E-18,0.000511815456479792),
(0.,1.00105873159715),.UNSPECIFIED.)
GEOMETRIC_REPRESENTATION_ITEM()
RATIONAL_B_SPLINE_SURFACE(((1.,0.708394529057139,1.00061746385198),(1.,
0.708058564167716,1.00061817524526),(1.,0.707430835372875,1.00061950443788),
(1.,0.706796685881197,1.00062084722609)))
REPRESENTATION_ITEM('')
SURFACE()
);
#3513=(
BOUNDED_SURFACE()
B_SPLINE_SURFACE(3,2,((#245750,#245751,#245752),(#245753,#245754,#245755),
(#245756,#245757,#245758),(#245759,#245760,#245761)),.UNSPECIFIED.,.F.,
 .F.,.F.)
B_SPLINE_SURFACE_WITH_KNOTS((4,4),(3,3),(-2.84603070277445E-18,0.000397394465448296),
(0.,1.),.UNSPECIFIED.)
GEOMETRIC_REPRESENTATION_ITEM()
RATIONAL_B_SPLINE_SURFACE(((1.,0.705498956110741,1.),(1.,0.70582176481181,
1.),(1.,0.706461952521106,1.),(1.,0.707106781186558,1.)))
REPRESENTATION_ITEM('')
SURFACE()
);
#3514=(
BOUNDED_SURFACE()
B_SPLINE_SURFACE(3,2,((#245767,#245768,#245769),(#245770,#245771,#245772),
(#245773,#245774,#245775),(#245776,#245777,#245778)),.UNSPECIFIED.,.F.,
 .F.,.F.)
B_SPLINE_SURFACE_WITH_KNOTS((4,4),(3,3),(0.,0.000397394410828738),(0.,1.),
 .UNSPECIFIED.)
GEOMETRIC_REPRESENTATION_ITEM()
RATIONAL_B_SPLINE_SURFACE(((1.,0.708689770883334,1.),(1.,0.708376440034488,
1.),(1.,0.707750498698412,1.),(1.,0.70710678118655,1.)))
REPRESENTATION_ITEM('')
SURFACE()
);
#3515=(
BOUNDED_SURFACE()
B_SPLINE_SURFACE(3,2,((#245784,#245785,#245786),(#245787,#245788,#245789),
(#245790,#245791,#245792),(#245793,#245794,#245795)),.UNSPECIFIED.,.F.,
 .F.,.F.)
B_SPLINE_SURFACE_WITH_KNOTS((4,4),(3,3),(0.,0.000511815090126173),(0.,1.00105592270469),
 .UNSPECIFIED.)
GEOMETRIC_REPRESENTATION_ITEM()
RATIONAL_B_SPLINE_SURFACE(((1.,0.70526624271676,1.00062243213231),(1.,0.705584085908403,
1.00062176089662),(1.,0.706182089449747,1.00062049800559),(1.,0.706797508586756,
1.00061919833551)))
REPRESENTATION_ITEM('')
SURFACE()
);
#3516=(
BOUNDED_SURFACE()
B_SPLINE_SURFACE(3,2,((#245797,#245798,#245799),(#245800,#245801,#245802),
(#245803,#245804,#245805),(#245806,#245807,#245808)),.UNSPECIFIED.,.F.,
 .F.,.F.)
B_SPLINE_SURFACE_WITH_KNOTS((4,4),(3,3),(5.96311194867027E-19,0.000397394428086636),
(0.,1.),.UNSPECIFIED.)
GEOMETRIC_REPRESENTATION_ITEM()
RATIONAL_B_SPLINE_SURFACE(((1.,0.70710678118655,1.),(1.,0.706459846759095,
1.),(1.,0.705820510737291,1.),(1.,0.705498956110747,1.)))
REPRESENTATION_ITEM('')
SURFACE()
);
#3517=(
BOUNDED_SURFACE()
B_SPLINE_SURFACE(3,2,((#245814,#245815,#245816),(#245817,#245818,#245819),
(#245820,#245821,#245822),(#245823,#245824,#245825),(#245826,#245827,#245828),
(#245829,#245830,#245831)),.UNSPECIFIED.,.F.,.F.,.F.)
B_SPLINE_SURFACE_WITH_KNOTS((4,2,4),(3,3),(5.14996031930615E-19,0.000257953807872846,
0.000515907615745692),(0.,1.),.UNSPECIFIED.)
GEOMETRIC_REPRESENTATION_ITEM()
RATIONAL_B_SPLINE_SURFACE(((1.,0.874619707139401,1.),(1.,0.874834349679141,
1.),(1.,0.854686104157596,1.),(1.,0.792476597915346,1.),(1.,0.750887854594966,
1.),(1.,0.705585838031443,1.)))
REPRESENTATION_ITEM('')
SURFACE()
);
#3518=(
BOUNDED_SURFACE()
B_SPLINE_SURFACE(3,2,((#245837,#245838,#245839),(#245840,#245841,#245842),
(#245843,#245844,#245845),(#245846,#245847,#245848)),.UNSPECIFIED.,.F.,
 .F.,.F.)
B_SPLINE_SURFACE_WITH_KNOTS((4,4),(3,3),(0.,0.000511815437699156),(0.,1.00105881331562),
 .UNSPECIFIED.)
GEOMETRIC_REPRESENTATION_ITEM()
RATIONAL_B_SPLINE_SURFACE(((1.,0.706796661946404,1.00062089519703),(1.,
0.707430821225336,1.00061955228445),(1.,0.70805854583075,1.00061822299811),
(1.,0.708394505252815,1.00061751156149)))
REPRESENTATION_ITEM('')
SURFACE()
);
#3519=(
BOUNDED_SURFACE()
B_SPLINE_SURFACE(3,2,((#245850,#245851,#245852),(#245853,#245854,#245855),
(#245856,#245857,#245858),(#245859,#245860,#245861),(#245862,#245863,#245864),
(#245865,#245866,#245867)),.UNSPECIFIED.,.F.,.F.,.F.)
B_SPLINE_SURFACE_WITH_KNOTS((4,2,4),(3,3),(-2.71050543121376E-20,0.000256915317531265,
0.00051383063506253),(0.,1.),.UNSPECIFIED.)
GEOMETRIC_REPRESENTATION_ITEM()
RATIONAL_B_SPLINE_SURFACE(((1.,0.705585838031445,1.),(1.,0.750902433542657,
1.),(1.,0.792329530082642,1.),(1.,0.854288401594088,1.),(1.,0.87499803112522,
1.),(1.,0.874619707139401,1.)))
REPRESENTATION_ITEM('')
SURFACE()
);
#3520=(
BOUNDED_SURFACE()
B_SPLINE_SURFACE(3,2,((#245873,#245874,#245875),(#245876,#245877,#245878),
(#245879,#245880,#245881),(#245882,#245883,#245884),(#245885,#245886,#245887),
(#245888,#245889,#245890)),.UNSPECIFIED.,.F.,.F.,.F.)
B_SPLINE_SURFACE_WITH_KNOTS((4,2,4),(3,3),(1.43656787854329E-18,0.000256592814262158,
0.000513185628524315),(0.,1.),.UNSPECIFIED.)
GEOMETRIC_REPRESENTATION_ITEM()
RATIONAL_B_SPLINE_SURFACE(((1.,0.70871252716365,1.),(1.,0.753780902613447,
1.),(1.,0.794538995769409,1.),(1.,0.855070770330912,1.),(1.,0.875018427445475,
1.),(1.,0.874619707139396,1.)))
REPRESENTATION_ITEM('')
SURFACE()
);
#3521=(
BOUNDED_SURFACE()
B_SPLINE_SURFACE(3,2,((#245892,#245893,#245894),(#245895,#245896,#245897),
(#245898,#245899,#245900),(#245901,#245902,#245903)),.UNSPECIFIED.,.F.,
 .F.,.F.)
B_SPLINE_SURFACE_WITH_KNOTS((4,4),(3,3),(5.96311194867027E-19,0.000511815072430399),
(0.,1.00105598365885),.UNSPECIFIED.)
GEOMETRIC_REPRESENTATION_ITEM()
RATIONAL_B_SPLINE_SURFACE(((1.,0.706797490733679,1.00061923411704),(1.,
0.706182062146613,1.0006205338821),(1.,0.705584062769007,1.00062179683724),
(1.,0.705266224770429,1.00062246810071)))
REPRESENTATION_ITEM('')
SURFACE()
);
#3522=(
BOUNDED_SURFACE()
B_SPLINE_SURFACE(3,2,((#245909,#245910,#245911),(#245912,#245913,#245914),
(#245915,#245916,#245917),(#245918,#245919,#245920),(#245921,#245922,#245923),
(#245924,#245925,#245926)),.UNSPECIFIED.,.F.,.F.,.F.)
B_SPLINE_SURFACE_WITH_KNOTS((4,2,4),(3,3),(0.,0.00025765223235089,0.00051530446470178),
(0.,1.),.UNSPECIFIED.)
GEOMETRIC_REPRESENTATION_ITEM()
RATIONAL_B_SPLINE_SURFACE(((1.,0.874619707139387,1.),(1.,0.874861180430702,
1.),(1.,0.855455725920869,1.),(1.,0.794699358955257,1.),(1.,0.753768977788647,
1.),(1.,0.708712527163647,1.)))
REPRESENTATION_ITEM('')
SURFACE()
);
#3523=(
BOUNDED_SURFACE()
B_SPLINE_SURFACE(3,2,((#245932,#245933,#245934),(#245935,#245936,#245937),
(#245938,#245939,#245940),(#245941,#245942,#245943)),.UNSPECIFIED.,.F.,
 .F.,.F.)
B_SPLINE_SURFACE_WITH_KNOTS((4,4),(3,3),(0.,0.000397394373651909),(0.,1.),
 .UNSPECIFIED.)
GEOMETRIC_REPRESENTATION_ITEM()
RATIONAL_B_SPLINE_SURFACE(((1.,0.707106781186545,1.),(1.,0.707752587915893,
1.),(1.,0.70837765454068,1.),(1.,0.70868977088333,1.)))
REPRESENTATION_ITEM('')
SURFACE()
);
#3524=(
BOUNDED_SURFACE()
B_SPLINE_SURFACE(3,2,((#245945,#245946,#245947),(#245948,#245949,#245950),
(#245951,#245952,#245953),(#245954,#245955,#245956)),.UNSPECIFIED.,.F.,
 .F.,.F.)
B_SPLINE_SURFACE_WITH_KNOTS((4,4),(3,3),(-5.61074624261249E-18,0.000511815456479791),
(0.,1.00105873159595),.UNSPECIFIED.)
GEOMETRIC_REPRESENTATION_ITEM()
RATIONAL_B_SPLINE_SURFACE(((1.,0.708394529057486,1.00061746385128),(1.,
0.708058564168047,1.00061817524457),(1.,0.707430835373218,1.00061950443718),
(1.,0.706796685881535,1.00062084722539)))
REPRESENTATION_ITEM('')
SURFACE()
);
#3525=(
BOUNDED_SURFACE()
B_SPLINE_SURFACE(3,2,((#245962,#245963,#245964),(#245965,#245966,#245967),
(#245968,#245969,#245970),(#245971,#245972,#245973)),.UNSPECIFIED.,.F.,
 .F.,.F.)
B_SPLINE_SURFACE_WITH_KNOTS((4,4),(3,3),(0.,0.000397394465448306),(0.,1.),
 .UNSPECIFIED.)
GEOMETRIC_REPRESENTATION_ITEM()
RATIONAL_B_SPLINE_SURFACE(((1.,0.70549895611075,1.),(1.,0.705821764811804,
1.),(1.,0.706461952521105,1.),(1.,0.707106781186556,1.)))
REPRESENTATION_ITEM('')
SURFACE()
);
#3526=(
BOUNDED_SURFACE()
B_SPLINE_SURFACE(3,2,((#245979,#245980,#245981),(#245982,#245983,#245984),
(#245985,#245986,#245987),(#245988,#245989,#245990)),.UNSPECIFIED.,.F.,
 .F.,.F.)
B_SPLINE_SURFACE_WITH_KNOTS((4,4),(3,3),(-6.23416249179165E-19,0.000397394410828727),
(0.,1.),.UNSPECIFIED.)
GEOMETRIC_REPRESENTATION_ITEM()
RATIONAL_B_SPLINE_SURFACE(((1.,0.70868977088335,1.),(1.,0.708376440034487,
1.),(1.,0.707750498698414,1.),(1.,0.707106781186542,1.)))
REPRESENTATION_ITEM('')
SURFACE()
);
#3527=(
BOUNDED_SURFACE()
B_SPLINE_SURFACE(3,2,((#245996,#245997,#245998),(#245999,#246000,#246001),
(#246002,#246003,#246004),(#246005,#246006,#246007)),.UNSPECIFIED.,.F.,
 .F.,.F.)
B_SPLINE_SURFACE_WITH_KNOTS((4,4),(3,3),(0.,0.000511815090126179),(0.,1.00105592270077),
 .UNSPECIFIED.)
GEOMETRIC_REPRESENTATION_ITEM()
RATIONAL_B_SPLINE_SURFACE(((1.,0.705266242717907,1.00062243212999),(1.,
0.705584085909567,1.00062176089431),(1.,0.706182089450896,1.00062049800328),
(1.,0.706797508587904,1.00061919833321)))
REPRESENTATION_ITEM('')
SURFACE()
);
#3528=(
BOUNDED_SURFACE()
B_SPLINE_SURFACE(3,2,((#246009,#246010,#246011),(#246012,#246013,#246014),
(#246015,#246016,#246017),(#246018,#246019,#246020)),.UNSPECIFIED.,.F.,
 .F.,.F.)
B_SPLINE_SURFACE_WITH_KNOTS((4,4),(3,3),(0.,0.000397394428086625),(0.,1.),
 .UNSPECIFIED.)
GEOMETRIC_REPRESENTATION_ITEM()
RATIONAL_B_SPLINE_SURFACE(((1.,0.70710678118656,1.),(1.,0.706459846759085,
1.),(1.,0.705820510737268,1.),(1.,0.70549895611075,1.)))
REPRESENTATION_ITEM('')
SURFACE()
);
#3529=(
BOUNDED_SURFACE()
B_SPLINE_SURFACE(3,2,((#246026,#246027,#246028),(#246029,#246030,#246031),
(#246032,#246033,#246034),(#246035,#246036,#246037),(#246038,#246039,#246040),
(#246041,#246042,#246043)),.UNSPECIFIED.,.F.,.F.,.F.)
B_SPLINE_SURFACE_WITH_KNOTS((4,2,4),(3,3),(0.,0.000257953807872843,0.000515907615745687),
(0.,1.),.UNSPECIFIED.)
GEOMETRIC_REPRESENTATION_ITEM()
RATIONAL_B_SPLINE_SURFACE(((1.,0.87461970713939,1.),(1.,0.874834349679608,
1.),(1.,0.854686104156984,1.),(1.,0.792476597915946,1.),(1.,0.750887854594552,
1.),(1.,0.705585838031425,1.)))
REPRESENTATION_ITEM('')
SURFACE()
);
#3530=(
BOUNDED_SURFACE()
B_SPLINE_SURFACE(3,2,((#246049,#246050,#246051),(#246052,#246053,#246054),
(#246055,#246056,#246057),(#246058,#246059,#246060)),.UNSPECIFIED.,.F.,
 .F.,.F.)
B_SPLINE_SURFACE_WITH_KNOTS((4,4),(3,3),(0.,0.000511815437699149),(0.,1.00105881331542),
 .UNSPECIFIED.)
GEOMETRIC_REPRESENTATION_ITEM()
RATIONAL_B_SPLINE_SURFACE(((1.,0.706796661946474,1.00062089519691),(1.,
0.707430821225348,1.00061955228434),(1.,0.708058545830872,1.00061822299799),
(1.,0.708394505252856,1.00061751156138)))
REPRESENTATION_ITEM('')
SURFACE()
);
#3531=(
BOUNDED_SURFACE()
B_SPLINE_SURFACE(3,2,((#246062,#246063,#246064),(#246065,#246066,#246067),
(#246068,#246069,#246070),(#246071,#246072,#246073),(#246074,#246075,#246076),
(#246077,#246078,#246079)),.UNSPECIFIED.,.F.,.F.,.F.)
B_SPLINE_SURFACE_WITH_KNOTS((4,2,4),(3,3),(0.,0.000256915317531268,0.000513830635062537),
(0.,1.),.UNSPECIFIED.)
GEOMETRIC_REPRESENTATION_ITEM()
RATIONAL_B_SPLINE_SURFACE(((1.,0.705585838031453,1.),(1.,0.75090243354269,
1.),(1.,0.792329530082585,1.),(1.,0.85428840159416,1.),(1.,0.874998031125199,
1.),(1.,0.874619707139421,1.)))
REPRESENTATION_ITEM('')
SURFACE()
);
#3532=(
BOUNDED_SURFACE()
B_SPLINE_SURFACE(3,2,((#246085,#246086,#246087),(#246088,#246089,#246090),
(#246091,#246092,#246093),(#246094,#246095,#246096),(#246097,#246098,#246099),
(#246100,#246101,#246102)),.UNSPECIFIED.,.F.,.F.,.F.)
B_SPLINE_SURFACE_WITH_KNOTS((4,2,4),(3,3),(-1.40946282423116E-17,0.000256592814262149,
0.000513185628524313),(0.,1.),.UNSPECIFIED.)
GEOMETRIC_REPRESENTATION_ITEM()
RATIONAL_B_SPLINE_SURFACE(((1.,0.708712527163669,1.),(1.,0.753780902613169,
1.),(1.,0.794538995769778,1.),(1.,0.855070770330537,1.),(1.,0.875018427445752,
1.),(1.,0.874619707139392,1.)))
REPRESENTATION_ITEM('')
SURFACE()
);
#3533=(
BOUNDED_SURFACE()
B_SPLINE_SURFACE(3,2,((#246104,#246105,#246106),(#246107,#246108,#246109),
(#246110,#246111,#246112),(#246113,#246114,#246115)),.UNSPECIFIED.,.F.,
 .F.,.F.)
B_SPLINE_SURFACE_WITH_KNOTS((4,4),(3,3),(0.,0.000511815072430413),(0.,1.00105598365874),
 .UNSPECIFIED.)
GEOMETRIC_REPRESENTATION_ITEM()
RATIONAL_B_SPLINE_SURFACE(((1.,0.706797490733722,1.00061923411697),(1.,
0.706182062146645,1.00062053388204),(1.,0.705584062768979,1.00062179683718),
(1.,0.705266224770506,1.00062246810064)))
REPRESENTATION_ITEM('')
SURFACE()
);
#3534=(
BOUNDED_SURFACE()
B_SPLINE_SURFACE(3,2,((#246121,#246122,#246123),(#246124,#246125,#246126),
(#246127,#246128,#246129),(#246130,#246131,#246132),(#246133,#246134,#246135),
(#246136,#246137,#246138)),.UNSPECIFIED.,.F.,.F.,.F.)
B_SPLINE_SURFACE_WITH_KNOTS((4,2,4),(3,3),(0.,0.000257652232350891,0.000515304464701781),
(0.,1.),.UNSPECIFIED.)
GEOMETRIC_REPRESENTATION_ITEM()
RATIONAL_B_SPLINE_SURFACE(((1.,0.874619707139378,1.),(1.,0.87486118043044,
1.),(1.,0.85545572592119,1.),(1.,0.794699358954915,1.),(1.,0.75376897778887,
1.),(1.,0.708712527163644,1.)))
REPRESENTATION_ITEM('')
SURFACE()
);
#3535=(
BOUNDED_SURFACE()
B_SPLINE_SURFACE(3,2,((#246144,#246145,#246146),(#246147,#246148,#246149),
(#246150,#246151,#246152),(#246153,#246154,#246155)),.UNSPECIFIED.,.F.,
 .F.,.F.)
B_SPLINE_SURFACE_WITH_KNOTS((4,4),(3,3),(-5.42101086242752E-20,0.000397394373651921),
(0.,1.),.UNSPECIFIED.)
GEOMETRIC_REPRESENTATION_ITEM()
RATIONAL_B_SPLINE_SURFACE(((1.,0.707106781186562,1.),(1.,0.707752587915892,
1.),(1.,0.708377654540671,1.),(1.,0.708689770883324,1.)))
REPRESENTATION_ITEM('')
SURFACE()
);
#3536=(
BOUNDED_SURFACE()
B_SPLINE_SURFACE(3,2,((#246157,#246158,#246159),(#246160,#246161,#246162),
(#246163,#246164,#246165),(#246166,#246167,#246168)),.UNSPECIFIED.,.F.,
 .F.,.F.)
B_SPLINE_SURFACE_WITH_KNOTS((4,4),(3,3),(-5.63785129692462E-18,0.000511815456479789),
(0.,1.00105873159701),.UNSPECIFIED.)
GEOMETRIC_REPRESENTATION_ITEM()
RATIONAL_B_SPLINE_SURFACE(((1.,0.708394529057188,1.0006174638519),(1.,0.708058564167717,
1.00061817524519),(1.,0.70743083537295,1.0006195044378),(1.,0.706796685881218,
1.00062084722601)))
REPRESENTATION_ITEM('')
SURFACE()
);
#3537=(
BOUNDED_SURFACE()
B_SPLINE_SURFACE(3,2,((#246174,#246175,#246176),(#246177,#246178,#246179),
(#246180,#246181,#246182),(#246183,#246184,#246185)),.UNSPECIFIED.,.F.,
 .F.,.F.)
B_SPLINE_SURFACE_WITH_KNOTS((4,4),(3,3),(-1.38777878078145E-17,0.000397394465448301),
(0.,1.),.UNSPECIFIED.)
GEOMETRIC_REPRESENTATION_ITEM()
RATIONAL_B_SPLINE_SURFACE(((1.,0.705498956110756,1.),(1.,0.705821764811832,
1.),(1.,0.706461952521107,1.),(1.,0.707106781186571,1.)))
REPRESENTATION_ITEM('')
SURFACE()
);
#3538=(
BOUNDED_SURFACE()
B_SPLINE_SURFACE(3,2,((#246191,#246192,#246193),(#246194,#246195,#246196),
(#246197,#246198,#246199),(#246200,#246201,#246202)),.UNSPECIFIED.,.F.,
 .F.,.F.)
B_SPLINE_SURFACE_WITH_KNOTS((4,4),(3,3),(-4.87890977618477E-19,0.000397394410828747),
(0.,1.),.UNSPECIFIED.)
GEOMETRIC_REPRESENTATION_ITEM()
RATIONAL_B_SPLINE_SURFACE(((1.,0.708689770883332,1.),(1.,0.708376440034503,
1.),(1.,0.707750498698384,1.),(1.,0.707106781186558,1.)))
REPRESENTATION_ITEM('')
SURFACE()
);
#3539=(
BOUNDED_SURFACE()
B_SPLINE_SURFACE(3,2,((#246208,#246209,#246210),(#246211,#246212,#246213),
(#246214,#246215,#246216),(#246217,#246218,#246219)),.UNSPECIFIED.,.F.,
 .F.,.F.)
B_SPLINE_SURFACE_WITH_KNOTS((4,4),(3,3),(0.,0.000511815090126181),(0.,1.00105592270224),
 .UNSPECIFIED.)
GEOMETRIC_REPRESENTATION_ITEM()
RATIONAL_B_SPLINE_SURFACE(((1.,0.705266242717473,1.00062243213086),(1.,
0.705584085909101,1.00062176089518),(1.,0.706182089450503,1.00062049800415),
(1.,0.706797508587471,1.00061919833407)))
REPRESENTATION_ITEM('')
SURFACE()
);
#3540=(
BOUNDED_SURFACE()
B_SPLINE_SURFACE(3,2,((#246221,#246222,#246223),(#246224,#246225,#246226),
(#246227,#246228,#246229),(#246230,#246231,#246232)),.UNSPECIFIED.,.F.,
 .F.,.F.)
B_SPLINE_SURFACE_WITH_KNOTS((4,4),(3,3),(0.,0.000397394428086631),(0.,1.),
 .UNSPECIFIED.)
GEOMETRIC_REPRESENTATION_ITEM()
RATIONAL_B_SPLINE_SURFACE(((1.,0.70710678118655,1.),(1.,0.706459846759093,
1.),(1.,0.705820510737295,1.),(1.,0.705498956110744,1.)))
REPRESENTATION_ITEM('')
SURFACE()
);
#3541=(
BOUNDED_SURFACE()
B_SPLINE_SURFACE(3,2,((#246238,#246239,#246240),(#246241,#246242,#246243),
(#246244,#246245,#246246),(#246247,#246248,#246249),(#246250,#246251,#246252),
(#246253,#246254,#246255)),.UNSPECIFIED.,.F.,.F.,.F.)
B_SPLINE_SURFACE_WITH_KNOTS((4,2,4),(3,3),(0.,0.000257953807872851,0.000515907615745702),
(0.,1.),.UNSPECIFIED.)
GEOMETRIC_REPRESENTATION_ITEM()
RATIONAL_B_SPLINE_SURFACE(((1.,0.874619707139391,1.),(1.,0.874834349679692,
1.),(1.,0.85468610415687,1.),(1.,0.792476597916061,1.),(1.,0.750887854594425,
1.),(1.,0.705585838031435,1.)))
REPRESENTATION_ITEM('')
SURFACE()
);
#3542=(
BOUNDED_SURFACE()
B_SPLINE_SURFACE(3,2,((#246261,#246262,#246263),(#246264,#246265,#246266),
(#246267,#246268,#246269),(#246270,#246271,#246272)),.UNSPECIFIED.,.F.,
 .F.,.F.)
B_SPLINE_SURFACE_WITH_KNOTS((4,4),(3,3),(0.,0.000511815437699153),(0.,1.00105881331651),
 .UNSPECIFIED.)
GEOMETRIC_REPRESENTATION_ITEM()
RATIONAL_B_SPLINE_SURFACE(((1.,0.706796661946155,1.00062089519755),(1.,
0.707430821225017,1.00061955228497),(1.,0.708058545830544,1.00061822299863),
(1.,0.708394505252542,1.00061751156201)))
REPRESENTATION_ITEM('')
SURFACE()
);
#3543=(
BOUNDED_SURFACE()
B_SPLINE_SURFACE(3,2,((#246274,#246275,#246276),(#246277,#246278,#246279),
(#246280,#246281,#246282),(#246283,#246284,#246285),(#246286,#246287,#246288),
(#246289,#246290,#246291)),.UNSPECIFIED.,.F.,.F.,.F.)
B_SPLINE_SURFACE_WITH_KNOTS((4,2,4),(3,3),(1.35525271560688E-18,0.000256915317531269,
0.000513830635062536),(0.,1.),.UNSPECIFIED.)
GEOMETRIC_REPRESENTATION_ITEM()
RATIONAL_B_SPLINE_SURFACE(((1.,0.705585838031444,1.),(1.,0.750902433542528,
1.),(1.,0.792329530082818,1.),(1.,0.854288401593931,1.),(1.,0.87499803112536,
1.),(1.,0.874619707139404,1.)))
REPRESENTATION_ITEM('')
SURFACE()
);
#3544=(
BOUNDED_SURFACE()
B_SPLINE_SURFACE(3,2,((#246297,#246298,#246299),(#246300,#246301,#246302),
(#246303,#246304,#246305),(#246306,#246307,#246308),(#246309,#246310,#246311),
(#246312,#246313,#246314)),.UNSPECIFIED.,.F.,.F.,.F.)
B_SPLINE_SURFACE_WITH_KNOTS((4,2,4),(3,3),(-1.33627917758838E-17,0.000256592814262148,
0.00051318562852431),(0.,1.),.UNSPECIFIED.)
GEOMETRIC_REPRESENTATION_ITEM()
RATIONAL_B_SPLINE_SURFACE(((1.,0.708712527163659,1.),(1.,0.753780902613647,
1.),(1.,0.794538995769118,1.),(1.,0.855070770331176,1.),(1.,0.875018427445279,
1.),(1.,0.874619707139401,1.)))
REPRESENTATION_ITEM('')
SURFACE()
);
#3545=(
BOUNDED_SURFACE()
B_SPLINE_SURFACE(3,2,((#246316,#246317,#246318),(#246319,#246320,#246321),
(#246322,#246323,#246324),(#246325,#246326,#246327)),.UNSPECIFIED.,.F.,
 .F.,.F.)
B_SPLINE_SURFACE_WITH_KNOTS((4,4),(3,3),(0.,0.000511815072430395),(0.,1.00105598365649),
 .UNSPECIFIED.)
GEOMETRIC_REPRESENTATION_ITEM()
RATIONAL_B_SPLINE_SURFACE(((1.,0.706797490734372,1.00061923411566),(1.,
0.706182062147344,1.00062053388071),(1.,0.705584062769602,1.00062179683585),
(1.,0.705266224771175,1.00062246809932)))
REPRESENTATION_ITEM('')
SURFACE()
);
#3546=(
BOUNDED_SURFACE()
B_SPLINE_SURFACE(3,2,((#246333,#246334,#246335),(#246336,#246337,#246338),
(#246339,#246340,#246341),(#246342,#246343,#246344),(#246345,#246346,#246347),
(#246348,#246349,#246350)),.UNSPECIFIED.,.F.,.F.,.F.)
B_SPLINE_SURFACE_WITH_KNOTS((4,2,4),(3,3),(0.,0.000257652232350881,0.000515304464701762),
(0.,1.),.UNSPECIFIED.)
GEOMETRIC_REPRESENTATION_ITEM()
RATIONAL_B_SPLINE_SURFACE(((1.,0.874619707139381,1.),(1.,0.874861180430671,
1.),(1.,0.855455725920884,1.),(1.,0.794699358955244,1.),(1.,0.75376897778864,
1.),(1.,0.708712527163656,1.)))
REPRESENTATION_ITEM('')
SURFACE()
);
#3547=(
BOUNDED_SURFACE()
B_SPLINE_SURFACE(3,2,((#246356,#246357,#246358),(#246359,#246360,#246361),
(#246362,#246363,#246364),(#246365,#246366,#246367)),.UNSPECIFIED.,.F.,
 .F.,.F.)
B_SPLINE_SURFACE_WITH_KNOTS((4,4),(3,3),(0.,0.000397394373651913),(0.,1.),
 .UNSPECIFIED.)
GEOMETRIC_REPRESENTATION_ITEM()
RATIONAL_B_SPLINE_SURFACE(((1.,0.707106781186537,1.),(1.,0.707752587915933,
1.),(1.,0.708377654540649,1.),(1.,0.708689770883327,1.)))
REPRESENTATION_ITEM('')
SURFACE()
);
#3548=(
BOUNDED_SURFACE()
B_SPLINE_SURFACE(3,2,((#246369,#246370,#246371),(#246372,#246373,#246374),
(#246375,#246376,#246377),(#246378,#246379,#246380)),.UNSPECIFIED.,.F.,
 .F.,.F.)
B_SPLINE_SURFACE_WITH_KNOTS((4,4),(3,3),(0.,0.000511815456479784),(0.,1.00105873159913),
 .UNSPECIFIED.)
GEOMETRIC_REPRESENTATION_ITEM()
RATIONAL_B_SPLINE_SURFACE(((1.,0.708394529056561,1.00061746385314),(1.,
0.708058564167131,1.00061817524643),(1.,0.707430835372305,1.00061950443905),
(1.,0.706796685880607,1.00062084722726)))
REPRESENTATION_ITEM('')
SURFACE()
);
#3549=(
BOUNDED_SURFACE()
B_SPLINE_SURFACE(3,2,((#246386,#246387,#246388),(#246389,#246390,#246391),
(#246392,#246393,#246394),(#246395,#246396,#246397)),.UNSPECIFIED.,.F.,
 .F.,.F.)
B_SPLINE_SURFACE_WITH_KNOTS((4,4),(3,3),(8.13151629364128E-20,0.000397394465448307),
(0.,1.),.UNSPECIFIED.)
GEOMETRIC_REPRESENTATION_ITEM()
RATIONAL_B_SPLINE_SURFACE(((1.,0.70549895611076,1.),(1.,0.7058217648118,
1.),(1.,0.706461952521123,1.),(1.,0.707106781186563,1.)))
REPRESENTATION_ITEM('')
SURFACE()
);
#3550=(
BOUNDED_SURFACE()
B_SPLINE_SURFACE(3,2,((#246403,#246404,#246405),(#246406,#246407,#246408),
(#246409,#246410,#246411),(#246412,#246413,#246414)),.UNSPECIFIED.,.F.,
 .F.,.F.)
B_SPLINE_SURFACE_WITH_KNOTS((4,4),(3,3),(-3.79470760369927E-19,0.000397394410828737),
(0.,1.),.UNSPECIFIED.)
GEOMETRIC_REPRESENTATION_ITEM()
RATIONAL_B_SPLINE_SURFACE(((1.,0.708689770883314,1.),(1.,0.708376440034537,
1.),(1.,0.707750498698401,1.),(1.,0.70710678118655,1.)))
REPRESENTATION_ITEM('')
SURFACE()
);
#3551=(
BOUNDED_SURFACE()
B_SPLINE_SURFACE(3,2,((#246420,#246421,#246422),(#246423,#246424,#246425),
(#246426,#246427,#246428),(#246429,#246430,#246431)),.UNSPECIFIED.,.F.,
 .F.,.F.)
B_SPLINE_SURFACE_WITH_KNOTS((4,4),(3,3),(0.,0.000511815090126176),(0.,1.00105592270117),
 .UNSPECIFIED.)
GEOMETRIC_REPRESENTATION_ITEM()
RATIONAL_B_SPLINE_SURFACE(((1.,0.705266242717781,1.00062243213023),(1.,
0.705584085909421,1.00062176089455),(1.,0.706182089450807,1.00062049800352),
(1.,0.706797508587779,1.00061919833345)))
REPRESENTATION_ITEM('')
SURFACE()
);
#3552=(
BOUNDED_SURFACE()
B_SPLINE_SURFACE(3,2,((#246433,#246434,#246435),(#246436,#246437,#246438),
(#246439,#246440,#246441),(#246442,#246443,#246444)),.UNSPECIFIED.,.F.,
 .F.,.F.)
B_SPLINE_SURFACE_WITH_KNOTS((4,4),(3,3),(0.,0.000397394428086637),(0.,1.),
 .UNSPECIFIED.)
GEOMETRIC_REPRESENTATION_ITEM()
RATIONAL_B_SPLINE_SURFACE(((1.,0.707106781186535,1.),(1.,0.706459846759099,
1.),(1.,0.705820510737271,1.),(1.,0.705498956110739,1.)))
REPRESENTATION_ITEM('')
SURFACE()
);
#3553=(
BOUNDED_SURFACE()
B_SPLINE_SURFACE(3,2,((#246450,#246451,#246452),(#246453,#246454,#246455),
(#246456,#246457,#246458),(#246459,#246460,#246461),(#246462,#246463,#246464),
(#246465,#246466,#246467)),.UNSPECIFIED.,.F.,.F.,.F.)
B_SPLINE_SURFACE_WITH_KNOTS((4,2,4),(3,3),(0.,0.000257953807872846,0.000515907615745692),
(0.,1.),.UNSPECIFIED.)
GEOMETRIC_REPRESENTATION_ITEM()
RATIONAL_B_SPLINE_SURFACE(((1.,0.874619707139395,1.),(1.,0.874834349679225,
1.),(1.,0.854686104157495,1.),(1.,0.792476597915437,1.),(1.,0.750887854594915,
1.),(1.,0.705585838031433,1.)))
REPRESENTATION_ITEM('')
SURFACE()
);
#3554=(
BOUNDED_SURFACE()
B_SPLINE_SURFACE(3,2,((#246473,#246474,#246475),(#246476,#246477,#246478),
(#246479,#246480,#246481),(#246482,#246483,#246484)),.UNSPECIFIED.,.F.,
 .F.,.F.)
B_SPLINE_SURFACE_WITH_KNOTS((4,4),(3,3),(0.,0.00051181543769915),(0.,1.00105881331661),
 .UNSPECIFIED.)
GEOMETRIC_REPRESENTATION_ITEM()
RATIONAL_B_SPLINE_SURFACE(((1.,0.706796661946118,1.00062089519761),(1.,
0.707430821224989,1.00061955228504),(1.,0.708058545830539,1.00061822299869),
(1.,0.708394505252492,1.00061751156207)))
REPRESENTATION_ITEM('')
SURFACE()
);
#3555=(
BOUNDED_SURFACE()
B_SPLINE_SURFACE(3,2,((#246486,#246487,#246488),(#246489,#246490,#246491),
(#246492,#246493,#246494),(#246495,#246496,#246497),(#246498,#246499,#246500),
(#246501,#246502,#246503)),.UNSPECIFIED.,.F.,.F.,.F.)
B_SPLINE_SURFACE_WITH_KNOTS((4,2,4),(3,3),(1.19262238973405E-18,0.000256915317531265,
0.000513830635062528),(0.,1.),.UNSPECIFIED.)
GEOMETRIC_REPRESENTATION_ITEM()
RATIONAL_B_SPLINE_SURFACE(((1.,0.705585838031449,1.),(1.,0.750902433542299,
1.),(1.,0.792329530083107,1.),(1.,0.854288401593629,1.),(1.,0.874998031125559,
1.),(1.,0.874619707139395,1.)))
REPRESENTATION_ITEM('')
SURFACE()
);
#3556=(
BOUNDED_SURFACE()
B_SPLINE_SURFACE(3,2,((#246509,#246510,#246511),(#246512,#246513,#246514),
(#246515,#246516,#246517),(#246518,#246519,#246520),(#246521,#246522,#246523),
(#246524,#246525,#246526)),.UNSPECIFIED.,.F.,.F.,.F.)
B_SPLINE_SURFACE_WITH_KNOTS((4,2,4),(3,3),(-4.41812385287843E-18,0.000256592814262153,
0.00051318562852431),(0.,1.),.UNSPECIFIED.)
GEOMETRIC_REPRESENTATION_ITEM()
RATIONAL_B_SPLINE_SURFACE(((1.,0.708712527163687,1.),(1.,0.753780902613256,
1.),(1.,0.79453899576962,1.),(1.,0.855070770330703,1.),(1.,0.875018427445644,
1.),(1.,0.874619707139394,1.)))
REPRESENTATION_ITEM('')
SURFACE()
);
#3557=(
BOUNDED_SURFACE()
B_SPLINE_SURFACE(3,2,((#246528,#246529,#246530),(#246531,#246532,#246533),
(#246534,#246535,#246536),(#246537,#246538,#246539)),.UNSPECIFIED.,.F.,
 .F.,.F.)
B_SPLINE_SURFACE_WITH_KNOTS((4,4),(3,3),(-6.64073830647371E-18,0.000511815072430408),
(0.,1.00105598365564),.UNSPECIFIED.)
GEOMETRIC_REPRESENTATION_ITEM()
RATIONAL_B_SPLINE_SURFACE(((1.,0.70679749073463,1.00061923411516),(1.,0.706182062147569,
1.00062053388021),(1.,0.705584062769927,1.00062179683535),(1.,0.70526622477141,
1.00062246809881)))
REPRESENTATION_ITEM('')
SURFACE()
);
#3558=(
BOUNDED_SURFACE()
B_SPLINE_SURFACE(3,2,((#246545,#246546,#246547),(#246548,#246549,#246550),
(#246551,#246552,#246553),(#246554,#246555,#246556),(#246557,#246558,#246559),
(#246560,#246561,#246562)),.UNSPECIFIED.,.F.,.F.,.F.)
B_SPLINE_SURFACE_WITH_KNOTS((4,2,4),(3,3),(0.,0.00025765223235088,0.00051530446470176),
(0.,1.),.UNSPECIFIED.)
GEOMETRIC_REPRESENTATION_ITEM()
RATIONAL_B_SPLINE_SURFACE(((1.,0.874619707139391,1.),(1.,0.874861180429929,
1.),(1.,0.85545572592193,1.),(1.,0.794699358954205,1.),(1.,0.753768977789438,
1.),(1.,0.708712527163671,1.)))
REPRESENTATION_ITEM('')
SURFACE()
);
#3559=(
BOUNDED_SURFACE()
B_SPLINE_SURFACE(3,2,((#246568,#246569,#246570),(#246571,#246572,#246573),
(#246574,#246575,#246576),(#246577,#246578,#246579)),.UNSPECIFIED.,.F.,
 .F.,.F.)
B_SPLINE_SURFACE_WITH_KNOTS((4,4),(3,3),(-6.64073830647371E-18,0.000397394373651924),
(0.,1.),.UNSPECIFIED.)
GEOMETRIC_REPRESENTATION_ITEM()
RATIONAL_B_SPLINE_SURFACE(((1.,0.707106781186545,1.),(1.,0.707752587915891,
1.),(1.,0.708377654540681,1.),(1.,0.708689770883316,1.)))
REPRESENTATION_ITEM('')
SURFACE()
);
#3560=(
BOUNDED_SURFACE()
B_SPLINE_SURFACE(3,2,((#246581,#246582,#246583),(#246584,#246585,#246586),
(#246587,#246588,#246589),(#246590,#246591,#246592)),.UNSPECIFIED.,.F.,
 .F.,.F.)
B_SPLINE_SURFACE_WITH_KNOTS((4,4),(3,3),(3.22550146314438E-18,0.000511815456479793),
(0.,1.00105873160129),.UNSPECIFIED.)
GEOMETRIC_REPRESENTATION_ITEM()
RATIONAL_B_SPLINE_SURFACE(((1.,0.708394529055928,1.0006174638544),(1.,0.708058564166499,
1.00061817524769),(1.,0.707430835371648,1.00061950444031),(1.,0.706796685879989,
1.00062084722853)))
REPRESENTATION_ITEM('')
SURFACE()
);
#3561=(
BOUNDED_SURFACE()
B_SPLINE_SURFACE(3,2,((#246598,#246599,#246600),(#246601,#246602,#246603),
(#246604,#246605,#246606),(#246607,#246608,#246609)),.UNSPECIFIED.,.F.,
 .F.,.F.)
B_SPLINE_SURFACE_WITH_KNOTS((4,4),(3,3),(-6.96599895821937E-18,0.000397394465448294),
(0.,1.),.UNSPECIFIED.)
GEOMETRIC_REPRESENTATION_ITEM()
RATIONAL_B_SPLINE_SURFACE(((1.,0.705498956110761,1.),(1.,0.705821764811777,
1.),(1.,0.706461952521158,1.),(1.,0.707106781186545,1.)))
REPRESENTATION_ITEM('')
SURFACE()
);
#3562=(
BOUNDED_SURFACE()
B_SPLINE_SURFACE(3,2,((#246615,#246616,#246617),(#246618,#246619,#246620),
(#246621,#246622,#246623),(#246624,#246625,#246626)),.UNSPECIFIED.,.F.,
 .F.,.F.)
B_SPLINE_SURFACE_WITH_KNOTS((4,4),(3,3),(0.,0.000397394410828746),(0.,1.),
 .UNSPECIFIED.)
GEOMETRIC_REPRESENTATION_ITEM()
RATIONAL_B_SPLINE_SURFACE(((1.,0.708689770883335,1.),(1.,0.708376440034449,
1.),(1.,0.70775049869843,1.),(1.,0.707106781186545,1.)))
REPRESENTATION_ITEM('')
SURFACE()
);
#3563=(
BOUNDED_SURFACE()
B_SPLINE_SURFACE(3,2,((#246632,#246633,#246634),(#246635,#246636,#246637),
(#246638,#246639,#246640),(#246641,#246642,#246643)),.UNSPECIFIED.,.F.,
 .F.,.F.)
B_SPLINE_SURFACE_WITH_KNOTS((4,4),(3,3),(1.35525271560688E-19,0.000511815090126177),
(0.,1.00105592270336),.UNSPECIFIED.)
GEOMETRIC_REPRESENTATION_ITEM()
RATIONAL_B_SPLINE_SURFACE(((1.,0.705266242717142,1.00062243213152),(1.,
0.705584085908801,1.00062176089584),(1.,0.70618208945015,1.00062049800481),
(1.,0.706797508587144,1.00061919833473)))
REPRESENTATION_ITEM('')
SURFACE()
);
#3564=(
BOUNDED_SURFACE()
B_SPLINE_SURFACE(3,2,((#246645,#246646,#246647),(#246648,#246649,#246650),
(#246651,#246652,#246653),(#246654,#246655,#246656)),.UNSPECIFIED.,.F.,
 .F.,.F.)
B_SPLINE_SURFACE_WITH_KNOTS((4,4),(3,3),(-7.26415455565288E-18,0.000397394428086627),
(0.,1.),.UNSPECIFIED.)
GEOMETRIC_REPRESENTATION_ITEM()
RATIONAL_B_SPLINE_SURFACE(((1.,0.707106781186549,1.),(1.,0.70645984675907,
1.),(1.,0.705820510737295,1.),(1.,0.705498956110751,1.)))
REPRESENTATION_ITEM('')
SURFACE()
);
#3565=(
BOUNDED_SURFACE()
B_SPLINE_SURFACE(3,2,((#246662,#246663,#246664),(#246665,#246666,#246667),
(#246668,#246669,#246670),(#246671,#246672,#246673),(#246674,#246675,#246676),
(#246677,#246678,#246679)),.UNSPECIFIED.,.F.,.F.,.F.)
B_SPLINE_SURFACE_WITH_KNOTS((4,2,4),(3,3),(5.14996031930615E-19,0.000257953807872838,
0.000515907615745675),(0.,1.),.UNSPECIFIED.)
GEOMETRIC_REPRESENTATION_ITEM()
RATIONAL_B_SPLINE_SURFACE(((1.,0.874619707139394,1.),(1.,0.874834349678729,
1.),(1.,0.854686104158156,1.),(1.,0.792476597914813,1.),(1.,0.750887854595356,
1.),(1.,0.705585838031451,1.)))
REPRESENTATION_ITEM('')
SURFACE()
);
#3566=(
BOUNDED_SURFACE()
B_SPLINE_SURFACE(3,2,((#246685,#246686,#246687),(#246688,#246689,#246690),
(#246691,#246692,#246693),(#246694,#246695,#246696)),.UNSPECIFIED.,.F.,
 .F.,.F.)
B_SPLINE_SURFACE_WITH_KNOTS((4,4),(3,3),(0.,0.000511815437699148),(0.,1.00105881331611),
 .UNSPECIFIED.)
GEOMETRIC_REPRESENTATION_ITEM()
RATIONAL_B_SPLINE_SURFACE(((1.,0.706796661946273,1.00062089519732),(1.,
0.707430821225126,1.00061955228474),(1.,0.708058545830682,1.0006182229984),
(1.,0.708394505252651,1.00061751156178)))
REPRESENTATION_ITEM('')
SURFACE()
);
#3567=(
BOUNDED_SURFACE()
B_SPLINE_SURFACE(3,2,((#246698,#246699,#246700),(#246701,#246702,#246703),
(#246704,#246705,#246706),(#246707,#246708,#246709),(#246710,#246711,#246712),
(#246713,#246714,#246715)),.UNSPECIFIED.,.F.,.F.,.F.)
B_SPLINE_SURFACE_WITH_KNOTS((4,2,4),(3,3),(0.,0.00025691531753126,0.00051383063506252),
(0.,1.),.UNSPECIFIED.)
GEOMETRIC_REPRESENTATION_ITEM()
RATIONAL_B_SPLINE_SURFACE(((1.,0.705585838031466,1.),(1.,0.75090243354285,
1.),(1.,0.792329530082371,1.),(1.,0.854288401594364,1.),(1.,0.874998031125017,
1.),(1.,0.874619707139408,1.)))
REPRESENTATION_ITEM('')
SURFACE()
);
#3568=(
BOUNDED_SURFACE()
B_SPLINE_SURFACE(3,2,((#246721,#246722,#246723),(#246724,#246725,#246726),
(#246727,#246728,#246729),(#246730,#246731,#246732),(#246733,#246734,#246735),
(#246736,#246737,#246738)),.UNSPECIFIED.,.F.,.F.,.F.)
B_SPLINE_SURFACE_WITH_KNOTS((4,2,4),(3,3),(-1.07607065619186E-17,0.000256592814262151,
0.000513185628524313),(0.,1.),.UNSPECIFIED.)
GEOMETRIC_REPRESENTATION_ITEM()
RATIONAL_B_SPLINE_SURFACE(((1.,0.708712527163685,1.),(1.,0.753780902613632,
1.),(1.,0.794538995769127,1.),(1.,0.855070770331165,1.),(1.,0.875018427445278,
1.),(1.,0.874619707139394,1.)))
REPRESENTATION_ITEM('')
SURFACE()
);
#3569=(
BOUNDED_SURFACE()
B_SPLINE_SURFACE(3,2,((#246740,#246741,#246742),(#246743,#246744,#246745),
(#246746,#246747,#246748),(#246749,#246750,#246751)),.UNSPECIFIED.,.F.,
 .F.,.F.)
B_SPLINE_SURFACE_WITH_KNOTS((4,4),(3,3),(0.,0.000511815072430402),(0.,1.00105598365829),
 .UNSPECIFIED.)
GEOMETRIC_REPRESENTATION_ITEM()
RATIONAL_B_SPLINE_SURFACE(((1.,0.706797490733853,1.00061923411671),(1.,
0.70618206214678,1.00062053388177),(1.,0.705584062769139,1.00062179683691),
(1.,0.705266224770619,1.00062246810038)))
REPRESENTATION_ITEM('')
SURFACE()
);
#3570=(
BOUNDED_SURFACE()
B_SPLINE_SURFACE(3,2,((#246757,#246758,#246759),(#246760,#246761,#246762),
(#246763,#246764,#246765),(#246766,#246767,#246768),(#246769,#246770,#246771),
(#246772,#246773,#246774)),.UNSPECIFIED.,.F.,.F.,.F.)
B_SPLINE_SURFACE_WITH_KNOTS((4,2,4),(3,3),(0.,0.000257652232350876,0.000515304464701751),
(0.,1.),.UNSPECIFIED.)
GEOMETRIC_REPRESENTATION_ITEM()
RATIONAL_B_SPLINE_SURFACE(((1.,0.874619707139385,1.),(1.,0.874861180430971,
1.),(1.,0.855455725920496,1.),(1.,0.794699358955617,1.),(1.,0.753768977788383,
1.),(1.,0.708712527163647,1.)))
REPRESENTATION_ITEM('')
SURFACE()
);
#3571=(
BOUNDED_SURFACE()
B_SPLINE_SURFACE(3,2,((#246780,#246781,#246782),(#246783,#246784,#246785),
(#246786,#246787,#246788),(#246789,#246790,#246791)),.UNSPECIFIED.,.F.,
 .F.,.F.)
B_SPLINE_SURFACE_WITH_KNOTS((4,4),(3,3),(0.,0.000397394373651911),(0.,1.),
 .UNSPECIFIED.)
GEOMETRIC_REPRESENTATION_ITEM()
RATIONAL_B_SPLINE_SURFACE(((1.,0.707106781186554,1.),(1.,0.707752587915894,
1.),(1.,0.708377654540672,1.),(1.,0.708689770883338,1.)))
REPRESENTATION_ITEM('')
SURFACE()
);
#3572=(
BOUNDED_SURFACE()
B_SPLINE_SURFACE(3,2,((#246793,#246794,#246795),(#246796,#246797,#246798),
(#246799,#246800,#246801),(#246802,#246803,#246804)),.UNSPECIFIED.,.F.,
 .F.,.F.)
B_SPLINE_SURFACE_WITH_KNOTS((4,4),(3,3),(-2.54787510534094E-18,0.000511815456479783),
(0.,1.00105873160091),.UNSPECIFIED.)
GEOMETRIC_REPRESENTATION_ITEM()
RATIONAL_B_SPLINE_SURFACE(((1.,0.708394529056051,1.00061746385417),(1.,
0.708058564166611,1.00061817524746),(1.,0.707430835371771,1.00061950444008),
(1.,0.706796685880101,1.0006208472283)))
REPRESENTATION_ITEM('')
SURFACE()
);
#3573=(
BOUNDED_SURFACE()
B_SPLINE_SURFACE(3,2,((#246810,#246811,#246812),(#246813,#246814,#246815),
(#246816,#246817,#246818),(#246819,#246820,#246821)),.UNSPECIFIED.,.F.,
 .F.,.F.)
B_SPLINE_SURFACE_WITH_KNOTS((4,4),(3,3),(0.,0.00039739446544831),(0.,1.),
 .UNSPECIFIED.)
GEOMETRIC_REPRESENTATION_ITEM()
RATIONAL_B_SPLINE_SURFACE(((1.,0.70549895611077,1.),(1.,0.705821764811747,
1.),(1.,0.706461952521146,1.),(1.,0.707106781186554,1.)))
REPRESENTATION_ITEM('')
SURFACE()
);
#3574=(
BOUNDED_SURFACE()
B_SPLINE_SURFACE(3,2,((#246827,#246828,#246829),(#246830,#246831,#246832),
(#246833,#246834,#246835),(#246836,#246837,#246838)),.UNSPECIFIED.,.F.,
 .F.,.F.)
B_SPLINE_SURFACE_WITH_KNOTS((4,4),(3,3),(-2.71050543121376E-20,0.000397394410828737),
(0.,1.),.UNSPECIFIED.)
GEOMETRIC_REPRESENTATION_ITEM()
RATIONAL_B_SPLINE_SURFACE(((1.,0.708689770883326,1.),(1.,0.708376440034482,
1.),(1.,0.707750498698405,1.),(1.,0.707106781186548,1.)))
REPRESENTATION_ITEM('')
SURFACE()
);
#3575=(
BOUNDED_SURFACE()
B_SPLINE_SURFACE(3,2,((#246844,#246845,#246846),(#246847,#246848,#246849),
(#246850,#246851,#246852),(#246853,#246854,#246855)),.UNSPECIFIED.,.F.,
 .F.,.F.)
B_SPLINE_SURFACE_WITH_KNOTS((4,4),(3,3),(2.71050543121376E-20,0.000511815090126173),
(0.,1.00105592270303),.UNSPECIFIED.)
GEOMETRIC_REPRESENTATION_ITEM()
RATIONAL_B_SPLINE_SURFACE(((1.,0.705266242717242,1.00062243213133),(1.,
0.705584085908911,1.00062176089565),(1.,0.706182089450249,1.00062049800462),
(1.,0.70679750858724,1.00061919833454)))
REPRESENTATION_ITEM('')
SURFACE()
);
#3576=(
BOUNDED_SURFACE()
B_SPLINE_SURFACE(3,2,((#246857,#246858,#246859),(#246860,#246861,#246862),
(#246863,#246864,#246865),(#246866,#246867,#246868)),.UNSPECIFIED.,.F.,
 .F.,.F.)
B_SPLINE_SURFACE_WITH_KNOTS((4,4),(3,3),(-8.13151629364128E-20,0.000397394428086625),
(0.,1.),.UNSPECIFIED.)
GEOMETRIC_REPRESENTATION_ITEM()
RATIONAL_B_SPLINE_SURFACE(((1.,0.707106781186548,1.),(1.,0.706459846759093,
1.),(1.,0.70582051073728,1.),(1.,0.705498956110757,1.)))
REPRESENTATION_ITEM('')
SURFACE()
);
#3577=(
BOUNDED_SURFACE()
B_SPLINE_SURFACE(3,2,((#246874,#246875,#246876),(#246877,#246878,#246879),
(#246880,#246881,#246882),(#246883,#246884,#246885),(#246886,#246887,#246888),
(#246889,#246890,#246891)),.UNSPECIFIED.,.F.,.F.,.F.)
B_SPLINE_SURFACE_WITH_KNOTS((4,2,4),(3,3),(0.,0.00025795380787285,0.000515907615745701),
(0.,1.),.UNSPECIFIED.)
GEOMETRIC_REPRESENTATION_ITEM()
RATIONAL_B_SPLINE_SURFACE(((1.,0.874619707139389,1.),(1.,0.874834349678911,
1.),(1.,0.854686104157886,1.),(1.,0.792476597915053,1.),(1.,0.750887854595184,
1.),(1.,0.705585838031474,1.)))
REPRESENTATION_ITEM('')
SURFACE()
);
#3578=(
BOUNDED_SURFACE()
B_SPLINE_SURFACE(3,2,((#246897,#246898,#246899),(#246900,#246901,#246902),
(#246903,#246904,#246905),(#246906,#246907,#246908)),.UNSPECIFIED.,.F.,
 .F.,.F.)
B_SPLINE_SURFACE_WITH_KNOTS((4,4),(3,3),(-7.04731412115578E-18,0.000511815437699152),
(0.,1.00105881331506),.UNSPECIFIED.)
GEOMETRIC_REPRESENTATION_ITEM()
RATIONAL_B_SPLINE_SURFACE(((1.,0.706796661946578,1.0006208951967),(1.,0.707430821225437,
1.00061955228412),(1.,0.708058545830975,1.00061822299778),(1.,0.708394505252952,
1.00061751156116)))
REPRESENTATION_ITEM('')
SURFACE()
);
#3579=(
BOUNDED_SURFACE()
B_SPLINE_SURFACE(3,2,((#246910,#246911,#246912),(#246913,#246914,#246915),
(#246916,#246917,#246918),(#246919,#246920,#246921),(#246922,#246923,#246924),
(#246925,#246926,#246927)),.UNSPECIFIED.,.F.,.F.,.F.)
B_SPLINE_SURFACE_WITH_KNOTS((4,2,4),(3,3),(1.89735380184963E-19,0.000256915317531257,
0.000513830635062515),(0.,1.),.UNSPECIFIED.)
GEOMETRIC_REPRESENTATION_ITEM()
RATIONAL_B_SPLINE_SURFACE(((1.,0.705585838031421,1.),(1.,0.750902433543199,
1.),(1.,0.792329530081917,1.),(1.,0.854288401594789,1.),(1.,0.874998031124692,
1.),(1.,0.87461970713939,1.)))
REPRESENTATION_ITEM('')
SURFACE()
);
#3580=(
BOUNDED_SURFACE()
B_SPLINE_SURFACE(3,2,((#246933,#246934,#246935),(#246936,#246937,#246938),
(#246939,#246940,#246941),(#246942,#246943,#246944),(#246945,#246946,#246947),
(#246948,#246949,#246950)),.UNSPECIFIED.,.F.,.F.,.F.)
B_SPLINE_SURFACE_WITH_KNOTS((4,2,4),(3,3),(-1.07878116162308E-17,0.000256592814262151,
0.000513185628524312),(0.,1.),.UNSPECIFIED.)
GEOMETRIC_REPRESENTATION_ITEM()
RATIONAL_B_SPLINE_SURFACE(((1.,0.708712527163674,1.),(1.,0.753780902612964,
1.),(1.,0.794538995770014,1.),(1.,0.855070770330296,1.),(1.,0.875018427445928,
1.),(1.,0.874619707139402,1.)))
REPRESENTATION_ITEM('')
SURFACE()
);
#3581=(
BOUNDED_SURFACE()
B_SPLINE_SURFACE(3,2,((#246952,#246953,#246954),(#246955,#246956,#246957),
(#246958,#246959,#246960),(#246961,#246962,#246963)),.UNSPECIFIED.,.F.,
 .F.,.F.)
B_SPLINE_SURFACE_WITH_KNOTS((4,4),(3,3),(4.87890977618477E-19,0.000511815072430404),
(0.,1.00105598365881),.UNSPECIFIED.)
GEOMETRIC_REPRESENTATION_ITEM()
RATIONAL_B_SPLINE_SURFACE(((1.,0.706797490733706,1.00061923411701),(1.,
0.706182062146592,1.00062053388208),(1.,0.705584062769001,1.00062179683722),
(1.,0.70526622477046,1.00062246810068)))
REPRESENTATION_ITEM('')
SURFACE()
);
#3582=(
BOUNDED_SURFACE()
B_SPLINE_SURFACE(3,2,((#246969,#246970,#246971),(#246972,#246973,#246974),
(#246975,#246976,#246977),(#246978,#246979,#246980),(#246981,#246982,#246983),
(#246984,#246985,#246986)),.UNSPECIFIED.,.F.,.F.,.F.)
B_SPLINE_SURFACE_WITH_KNOTS((4,2,4),(3,3),(-2.24971950790742E-18,0.000257652232350876,
0.000515304464701754),(0.,1.),.UNSPECIFIED.)
GEOMETRIC_REPRESENTATION_ITEM()
RATIONAL_B_SPLINE_SURFACE(((1.,0.874619707139394,1.),(1.,0.874861180430937,
1.),(1.,0.855455725920569,1.),(1.,0.794699358955574,1.),(1.,0.753768977788433,
1.),(1.,0.708712527163671,1.)))
REPRESENTATION_ITEM('')
SURFACE()
);
#3583=(
BOUNDED_SURFACE()
B_SPLINE_SURFACE(3,2,((#246992,#246993,#246994),(#246995,#246996,#246997),
(#246998,#246999,#247000),(#247001,#247002,#247003)),.UNSPECIFIED.,.F.,
 .F.,.F.)
B_SPLINE_SURFACE_WITH_KNOTS((4,4),(3,3),(1.0842021724855E-19,0.000397394373651918),
(0.,1.),.UNSPECIFIED.)
GEOMETRIC_REPRESENTATION_ITEM()
RATIONAL_B_SPLINE_SURFACE(((1.,0.707106781186548,1.),(1.,0.707752587915899,
1.),(1.,0.708377654540685,1.),(1.,0.708689770883336,1.)))
REPRESENTATION_ITEM('')
SURFACE()
);
#3584=(
BOUNDED_SURFACE()
B_SPLINE_SURFACE(3,2,((#247005,#247006,#247007),(#247008,#247009,#247010),
(#247011,#247012,#247013),(#247014,#247015,#247016)),.UNSPECIFIED.,.F.,
 .F.,.F.)
B_SPLINE_SURFACE_WITH_KNOTS((4,4),(3,3),(-2.43945488809238E-18,0.000511815456479785),
(0.,1.00105873160026),.UNSPECIFIED.)
GEOMETRIC_REPRESENTATION_ITEM()
RATIONAL_B_SPLINE_SURFACE(((1.,0.708394529056247,1.00061746385379),(1.,
0.708058564166769,1.00061817524708),(1.,0.707430835371989,1.00061950443971),
(1.,0.706796685880284,1.00062084722792)))
REPRESENTATION_ITEM('')
SURFACE()
);
#3585=(
BOUNDED_SURFACE()
B_SPLINE_SURFACE(3,2,((#247022,#247023,#247024),(#247025,#247026,#247027),
(#247028,#247029,#247030),(#247031,#247032,#247033)),.UNSPECIFIED.,.F.,
 .F.,.F.)
B_SPLINE_SURFACE_WITH_KNOTS((4,4),(3,3),(2.71050543121376E-20,0.00039739446544831),
(0.,1.),.UNSPECIFIED.)
GEOMETRIC_REPRESENTATION_ITEM()
RATIONAL_B_SPLINE_SURFACE(((1.,0.705498956110749,1.),(1.,0.705821764811765,
1.),(1.,0.706461952521142,1.),(1.,0.707106781186548,1.)))
REPRESENTATION_ITEM('')
SURFACE()
);
#3586=(
BOUNDED_SURFACE()
B_SPLINE_SURFACE(3,2,((#247039,#247040,#247041),(#247042,#247043,#247044),
(#247045,#247046,#247047),(#247048,#247049,#247050)),.UNSPECIFIED.,.F.,
 .F.,.F.)
B_SPLINE_SURFACE_WITH_KNOTS((4,4),(3,3),(0.,0.000397394410828733),(0.,1.),
 .UNSPECIFIED.)
GEOMETRIC_REPRESENTATION_ITEM()
RATIONAL_B_SPLINE_SURFACE(((1.,0.708689770883331,1.),(1.,0.70837644003449,
1.),(1.,0.707750498698411,1.),(1.,0.707106781186548,1.)))
REPRESENTATION_ITEM('')
SURFACE()
);
#3587=(
BOUNDED_SURFACE()
B_SPLINE_SURFACE(3,2,((#247056,#247057,#247058),(#247059,#247060,#247061),
(#247062,#247063,#247064),(#247065,#247066,#247067)),.UNSPECIFIED.,.F.,
 .F.,.F.)
B_SPLINE_SURFACE_WITH_KNOTS((4,4),(3,3),(0.,0.000511815090126173),(0.,1.00105592270359),
 .UNSPECIFIED.)
GEOMETRIC_REPRESENTATION_ITEM()
RATIONAL_B_SPLINE_SURFACE(((1.,0.705266242717076,1.00062243213166),(1.,
0.705584085908736,1.00062176089597),(1.,0.70618208945009,1.00062049800494),
(1.,0.706797508587075,1.00061919833486)))
REPRESENTATION_ITEM('')
SURFACE()
);
#3588=(
BOUNDED_SURFACE()
B_SPLINE_SURFACE(3,2,((#247069,#247070,#247071),(#247072,#247073,#247074),
(#247075,#247076,#247077),(#247078,#247079,#247080)),.UNSPECIFIED.,.F.,
 .F.,.F.)
B_SPLINE_SURFACE_WITH_KNOTS((4,4),(3,3),(-7.07441917546792E-18,0.00039739442808662),
(0.,1.),.UNSPECIFIED.)
GEOMETRIC_REPRESENTATION_ITEM()
RATIONAL_B_SPLINE_SURFACE(((1.,0.707106781186548,1.),(1.,0.706459846759096,
1.),(1.,0.705820510737264,1.),(1.,0.705498956110752,1.)))
REPRESENTATION_ITEM('')
SURFACE()
);
#3589=(
BOUNDED_SURFACE()
B_SPLINE_SURFACE(3,2,((#247086,#247087,#247088),(#247089,#247090,#247091),
(#247092,#247093,#247094),(#247095,#247096,#247097),(#247098,#247099,#247100),
(#247101,#247102,#247103)),.UNSPECIFIED.,.F.,.F.,.F.)
B_SPLINE_SURFACE_WITH_KNOTS((4,2,4),(3,3),(-9.48676900924816E-20,0.000257953807872841,
0.000515907615745682),(0.,1.),.UNSPECIFIED.)
GEOMETRIC_REPRESENTATION_ITEM()
RATIONAL_B_SPLINE_SURFACE(((1.,0.874619707139395,1.),(1.,0.874834349678826,
1.),(1.,0.854686104158014,1.),(1.,0.792476597914929,1.),(1.,0.750887854595294,
1.),(1.,0.70558583803145,1.)))
REPRESENTATION_ITEM('')
SURFACE()
);
#3590=(
BOUNDED_SURFACE()
B_SPLINE_SURFACE(3,2,((#247106,#247107,#247108),(#247109,#247110,#247111),
(#247112,#247113,#247114),(#247115,#247116,#247117)),.UNSPECIFIED.,.F.,
 .F.,.F.)
B_SPLINE_SURFACE_WITH_KNOTS((4,4),(3,3),(0.,0.000511815437699145),(0.,1.00105881331498),
 .UNSPECIFIED.)
GEOMETRIC_REPRESENTATION_ITEM()
RATIONAL_B_SPLINE_SURFACE(((1.,0.706796661946602,1.00062089519665),(1.,
0.707430821225483,1.00061955228408),(1.,0.708058545830975,1.00061822299773),
(1.,0.708394505252982,1.00061751156112)))
REPRESENTATION_ITEM('')
SURFACE()
);
#3591=(
BOUNDED_SURFACE()
B_SPLINE_SURFACE(3,2,((#247119,#247120,#247121),(#247122,#247123,#247124),
(#247125,#247126,#247127),(#247128,#247129,#247130),(#247131,#247132,#247133),
(#247134,#247135,#247136)),.UNSPECIFIED.,.F.,.F.,.F.)
B_SPLINE_SURFACE_WITH_KNOTS((4,2,4),(3,3),(1.62630325872826E-19,0.00025691531753126,
0.00051383063506252),(0.,1.),.UNSPECIFIED.)
GEOMETRIC_REPRESENTATION_ITEM()
RATIONAL_B_SPLINE_SURFACE(((1.,0.705585838031442,1.),(1.,0.750902433542864,
1.),(1.,0.792329530082364,1.),(1.,0.854288401594348,1.),(1.,0.874998031125022,
1.),(1.,0.874619707139395,1.)))
REPRESENTATION_ITEM('')
SURFACE()
);
#3592=(
BOUNDED_SURFACE()
B_SPLINE_SURFACE(3,2,((#247142,#247143,#247144),(#247145,#247146,#247147),
(#247148,#247149,#247150),(#247151,#247152,#247153),(#247154,#247155,#247156),
(#247157,#247158,#247159)),.UNSPECIFIED.,.F.,.F.,.F.)
B_SPLINE_SURFACE_WITH_KNOTS((4,2,4),(3,3),(-1.32814766129474E-17,0.000256592814262149,
0.000513185628524311),(0.,1.),.UNSPECIFIED.)
GEOMETRIC_REPRESENTATION_ITEM()
RATIONAL_B_SPLINE_SURFACE(((1.,0.708712527163647,1.),(1.,0.75378090261363,
1.),(1.,0.794538995769148,1.),(1.,0.855070770331167,1.),(1.,0.87501842744528,
1.),(1.,0.874619707139394,1.)))
REPRESENTATION_ITEM('')
SURFACE()
);
#3593=(
BOUNDED_SURFACE()
B_SPLINE_SURFACE(3,2,((#247160,#247161,#247162),(#247163,#247164,#247165),
(#247166,#247167,#247168),(#247169,#247170,#247171)),.UNSPECIFIED.,.F.,
 .F.,.F.)
B_SPLINE_SURFACE_WITH_KNOTS((4,4),(3,3),(2.71050543121376E-20,0.000511815072430403),
(0.,1.0010559836588),.UNSPECIFIED.)
GEOMETRIC_REPRESENTATION_ITEM()
RATIONAL_B_SPLINE_SURFACE(((1.,0.706797490733709,1.00061923411701),(1.,
0.706182062146628,1.00062053388207),(1.,0.70558406276899,1.00062179683721),
(1.,0.705266224770469,1.00062246810067)))
REPRESENTATION_ITEM('')
SURFACE()
);
#3594=(
BOUNDED_SURFACE()
B_SPLINE_SURFACE(3,2,((#247175,#247176,#247177),(#247178,#247179,#247180),
(#247181,#247182,#247183),(#247184,#247185,#247186),(#247187,#247188,#247189),
(#247190,#247191,#247192)),.UNSPECIFIED.,.F.,.F.,.F.)
B_SPLINE_SURFACE_WITH_KNOTS((4,2,4),(3,3),(8.13151629364128E-20,0.000257652232350873,
0.000515304464701745),(0.,1.),.UNSPECIFIED.)
GEOMETRIC_REPRESENTATION_ITEM()
RATIONAL_B_SPLINE_SURFACE(((1.,0.8746197071394,1.),(1.,0.874861180430503,
1.),(1.,0.855455725921145,1.),(1.,0.79469935895498,1.),(1.,0.753768977788861,
1.),(1.,0.708712527163669,1.)))
REPRESENTATION_ITEM('')
SURFACE()
);
#3595=(
BOUNDED_SURFACE()
B_SPLINE_SURFACE(3,2,((#247198,#247199,#247200),(#247201,#247202,#247203),
(#247204,#247205,#247206),(#247207,#247208,#247209)),.UNSPECIFIED.,.F.,
 .F.,.F.)
B_SPLINE_SURFACE_WITH_KNOTS((4,4),(3,3),(0.,0.00039739437365191),(0.,1.),
 .UNSPECIFIED.)
GEOMETRIC_REPRESENTATION_ITEM()
RATIONAL_B_SPLINE_SURFACE(((1.,0.707106781186548,1.),(1.,0.707752587915901,
1.),(1.,0.708377654540677,1.),(1.,0.708689770883331,1.)))
REPRESENTATION_ITEM('')
SURFACE()
);
#3596=(
BOUNDED_SURFACE()
B_SPLINE_SURFACE(3,2,((#247211,#247212,#247213),(#247214,#247215,#247216),
(#247217,#247218,#247219),(#247220,#247221,#247222)),.UNSPECIFIED.,.F.,
 .F.,.F.)
B_SPLINE_SURFACE_WITH_KNOTS((4,4),(3,3),(-5.61074624261249E-18,0.000511815456479785),
(0.,1.00105873159895),.UNSPECIFIED.)
GEOMETRIC_REPRESENTATION_ITEM()
RATIONAL_B_SPLINE_SURFACE(((1.,0.70839452905662,1.00061746385303),(1.,0.708058564167168,
1.00061817524632),(1.,0.707430835372348,1.00061950443894),(1.,0.706796685880671,
1.00062084722715)))
REPRESENTATION_ITEM('')
SURFACE()
);
#3597=(
BOUNDED_SURFACE()
B_SPLINE_SURFACE(3,2,((#247228,#247229,#247230),(#247231,#247232,#247233),
(#247234,#247235,#247236),(#247237,#247238,#247239)),.UNSPECIFIED.,.F.,
 .F.,.F.)
B_SPLINE_SURFACE_WITH_KNOTS((4,4),(3,3),(0.,0.000397394465448314),(0.,1.),
 .UNSPECIFIED.)
GEOMETRIC_REPRESENTATION_ITEM()
RATIONAL_B_SPLINE_SURFACE(((1.,0.705498956110752,1.),(1.,0.705821764811787,
1.),(1.,0.706461952521144,1.),(1.,0.707106781186548,1.)))
REPRESENTATION_ITEM('')
SURFACE()
);
#3598=(
BOUNDED_SURFACE()
B_SPLINE_SURFACE(3,2,((#247245,#247246,#247247),(#247248,#247249,#247250),
(#247251,#247252,#247253),(#247254,#247255,#247256)),.UNSPECIFIED.,.F.,
 .F.,.F.)
B_SPLINE_SURFACE_WITH_KNOTS((4,4),(3,3),(2.71050543121376E-20,0.000397394410828732),
(0.,1.),.UNSPECIFIED.)
GEOMETRIC_REPRESENTATION_ITEM()
RATIONAL_B_SPLINE_SURFACE(((1.,0.708689770883327,1.),(1.,0.708376440034475,
1.),(1.,0.707750498698411,1.),(1.,0.707106781186548,1.)))
REPRESENTATION_ITEM('')
SURFACE()
);
#3599=(
BOUNDED_SURFACE()
B_SPLINE_SURFACE(3,2,((#247262,#247263,#247264),(#247265,#247266,#247267),
(#247268,#247269,#247270),(#247271,#247272,#247273)),.UNSPECIFIED.,.F.,
 .F.,.F.)
B_SPLINE_SURFACE_WITH_KNOTS((4,4),(3,3),(-2.71050543121376E-20,0.000511815090126174),
(0.,1.00105592270086),.UNSPECIFIED.)
GEOMETRIC_REPRESENTATION_ITEM()
RATIONAL_B_SPLINE_SURFACE(((1.,0.705266242717886,1.00062243213005),(1.,
0.705584085909542,1.00062176089437),(1.,0.706182089450896,1.00062049800334),
(1.,0.706797508587876,1.00061919833326)))
REPRESENTATION_ITEM('')
SURFACE()
);
#3600=(
BOUNDED_SURFACE()
B_SPLINE_SURFACE(3,2,((#247275,#247276,#247277),(#247278,#247279,#247280),
(#247281,#247282,#247283),(#247284,#247285,#247286)),.UNSPECIFIED.,.F.,
 .F.,.F.)
B_SPLINE_SURFACE_WITH_KNOTS((4,4),(3,3),(-7.02020906684364E-18,0.000397394428086623),
(0.,1.),.UNSPECIFIED.)
GEOMETRIC_REPRESENTATION_ITEM()
RATIONAL_B_SPLINE_SURFACE(((1.,0.707106781186548,1.),(1.,0.706459846759084,
1.),(1.,0.705820510737286,1.),(1.,0.705498956110757,1.)))
REPRESENTATION_ITEM('')
SURFACE()
);
#3601=(
BOUNDED_SURFACE()
B_SPLINE_SURFACE(3,2,((#247292,#247293,#247294),(#247295,#247296,#247297),
(#247298,#247299,#247300),(#247301,#247302,#247303),(#247304,#247305,#247306),
(#247307,#247308,#247309)),.UNSPECIFIED.,.F.,.F.,.F.)
B_SPLINE_SURFACE_WITH_KNOTS((4,2,4),(3,3),(-8.53809210832335E-19,0.000257953807872841,
0.000515907615745684),(0.,1.),.UNSPECIFIED.)
GEOMETRIC_REPRESENTATION_ITEM()
RATIONAL_B_SPLINE_SURFACE(((1.,0.87461970713939,1.),(1.,0.874834349679068,
1.),(1.,0.854686104157704,1.),(1.,0.792476597915263,1.),(1.,0.750887854595055,
1.),(1.,0.705585838031452,1.)))
REPRESENTATION_ITEM('')
SURFACE()
);
#3602=(
BOUNDED_SURFACE()
B_SPLINE_SURFACE(3,2,((#247315,#247316,#247317),(#247318,#247319,#247320),
(#247321,#247322,#247323),(#247324,#247325,#247326)),.UNSPECIFIED.,.F.,
 .F.,.F.)
B_SPLINE_SURFACE_WITH_KNOTS((4,4),(3,3),(-1.0842021724855E-19,0.000511815437699153),
(0.,1.00105881331538),.UNSPECIFIED.)
GEOMETRIC_REPRESENTATION_ITEM()
RATIONAL_B_SPLINE_SURFACE(((1.,0.706796661946481,1.00062089519689),(1.,
0.707430821225356,1.00061955228431),(1.,0.708058545830853,1.00061822299797),
(1.,0.708394505252858,1.00061751156135)))
REPRESENTATION_ITEM('')
SURFACE()
);
#3603=(
BOUNDED_SURFACE()
B_SPLINE_SURFACE(3,2,((#247328,#247329,#247330),(#247331,#247332,#247333),
(#247334,#247335,#247336),(#247337,#247338,#247339),(#247340,#247341,#247342),
(#247343,#247344,#247345)),.UNSPECIFIED.,.F.,.F.,.F.)
B_SPLINE_SURFACE_WITH_KNOTS((4,2,4),(3,3),(1.0842021724855E-19,0.000256915317531263,
0.000513830635062526),(0.,1.),.UNSPECIFIED.)
GEOMETRIC_REPRESENTATION_ITEM()
RATIONAL_B_SPLINE_SURFACE(((1.,0.70558583803143,1.),(1.,0.750902433542735,
1.),(1.,0.792329530082518,1.),(1.,0.854288401594187,1.),(1.,0.874998031125162,
1.),(1.,0.874619707139389,1.)))
REPRESENTATION_ITEM('')
SURFACE()
);
#3604=(
BOUNDED_SURFACE()
B_SPLINE_SURFACE(3,2,((#247351,#247352,#247353),(#247354,#247355,#247356),
(#247357,#247358,#247359),(#247360,#247361,#247362),(#247363,#247364,#247365),
(#247366,#247367,#247368)),.UNSPECIFIED.,.F.,.F.,.F.)
B_SPLINE_SURFACE_WITH_KNOTS((4,2,4),(3,3),(-1.04625509644851E-17,0.00025659281426215,
0.000513185628524311),(0.,1.),.UNSPECIFIED.)
GEOMETRIC_REPRESENTATION_ITEM()
RATIONAL_B_SPLINE_SURFACE(((1.,0.708712527163659,1.),(1.,0.753780902613745,
1.),(1.,0.794538995768978,1.),(1.,0.855070770331331,1.),(1.,0.875018427445157,
1.),(1.,0.874619707139395,1.)))
REPRESENTATION_ITEM('')
SURFACE()
);
#3605=(
BOUNDED_SURFACE()
B_SPLINE_SURFACE(3,2,((#247370,#247371,#247372),(#247373,#247374,#247375),
(#247376,#247377,#247378),(#247379,#247380,#247381)),.UNSPECIFIED.,.F.,
 .F.,.F.)
B_SPLINE_SURFACE_WITH_KNOTS((4,4),(3,3),(-7.61652026171067E-18,0.00051181507243039),
(0.,1.00105598365716),.UNSPECIFIED.)
GEOMETRIC_REPRESENTATION_ITEM()
RATIONAL_B_SPLINE_SURFACE(((1.,0.706797490734189,1.00061923411605),(1.,
0.7061820621471,1.00062053388111),(1.,0.705584062769466,1.00062179683625),
(1.,0.705266224770944,1.00062246809971)))
REPRESENTATION_ITEM('')
SURFACE()
);
#3606=(
BOUNDED_SURFACE()
B_SPLINE_SURFACE(3,2,((#247387,#247388,#247389),(#247390,#247391,#247392),
(#247393,#247394,#247395),(#247396,#247397,#247398),(#247399,#247400,#247401),
(#247402,#247403,#247404)),.UNSPECIFIED.,.F.,.F.,.F.)
B_SPLINE_SURFACE_WITH_KNOTS((4,2,4),(3,3),(-2.62919026827735E-18,0.000257652232350876,
0.000515304464701754),(0.,1.),.UNSPECIFIED.)
GEOMETRIC_REPRESENTATION_ITEM()
RATIONAL_B_SPLINE_SURFACE(((1.,0.874619707139396,1.),(1.,0.874861180430993,
1.),(1.,0.855455725920489,1.),(1.,0.794699358955656,1.),(1.,0.753768977788361,
1.),(1.,0.708712527163659,1.)))
REPRESENTATION_ITEM('')
SURFACE()
);
#3607=(
BOUNDED_SURFACE()
B_SPLINE_SURFACE(3,2,((#247410,#247411,#247412),(#247413,#247414,#247415),
(#247416,#247417,#247418),(#247419,#247420,#247421)),.UNSPECIFIED.,.F.,
 .F.,.F.)
B_SPLINE_SURFACE_WITH_KNOTS((4,4),(3,3),(-7.18283939271647E-18,0.000397394373651905),
(0.,1.),.UNSPECIFIED.)
GEOMETRIC_REPRESENTATION_ITEM()
RATIONAL_B_SPLINE_SURFACE(((1.,0.707106781186548,1.),(1.,0.707752587915914,
1.),(1.,0.70837765454066,1.),(1.,0.708689770883359,1.)))
REPRESENTATION_ITEM('')
SURFACE()
);
#3608=(
BOUNDED_SURFACE()
B_SPLINE_SURFACE(3,2,((#247423,#247424,#247425),(#247426,#247427,#247428),
(#247429,#247430,#247431),(#247432,#247433,#247434)),.UNSPECIFIED.,.F.,
 .F.,.F.)
B_SPLINE_SURFACE_WITH_KNOTS((4,4),(3,3),(5.42101086242752E-20,0.000511815456479787),
(0.,1.00105873159955),.UNSPECIFIED.)
GEOMETRIC_REPRESENTATION_ITEM()
RATIONAL_B_SPLINE_SURFACE(((1.,0.708394529056452,1.00061746385338),(1.,
0.708058564166979,1.00061817524667),(1.,0.707430835372198,1.00061950443929),
(1.,0.706796685880492,1.0006208472275)))
REPRESENTATION_ITEM('')
SURFACE()
);
#3609=(
BOUNDED_SURFACE()
B_SPLINE_SURFACE(3,2,((#247440,#247441,#247442),(#247443,#247444,#247445),
(#247446,#247447,#247448),(#247449,#247450,#247451)),.UNSPECIFIED.,.F.,
 .F.,.F.)
B_SPLINE_SURFACE_WITH_KNOTS((4,4),(3,3),(-2.71050543121376E-20,0.00039739446544831),
(0.,1.),.UNSPECIFIED.)
GEOMETRIC_REPRESENTATION_ITEM()
RATIONAL_B_SPLINE_SURFACE(((1.,0.705498956110745,1.),(1.,0.705821764811779,
1.),(1.,0.706461952521128,1.),(1.,0.70710678118655,1.)))
REPRESENTATION_ITEM('')
SURFACE()
);
#3610=(
BOUNDED_SURFACE()
B_SPLINE_SURFACE(3,2,((#247457,#247458,#247459),(#247460,#247461,#247462),
(#247463,#247464,#247465),(#247466,#247467,#247468)),.UNSPECIFIED.,.F.,
 .F.,.F.)
B_SPLINE_SURFACE_WITH_KNOTS((4,4),(3,3),(0.,0.00039739441082874),(0.,1.),
 .UNSPECIFIED.)
GEOMETRIC_REPRESENTATION_ITEM()
RATIONAL_B_SPLINE_SURFACE(((1.,0.708689770883333,1.),(1.,0.708376440034488,
1.),(1.,0.707750498698412,1.),(1.,0.70710678118655,1.)))
REPRESENTATION_ITEM('')
SURFACE()
);
#3611=(
BOUNDED_SURFACE()
B_SPLINE_SURFACE(3,2,((#247474,#247475,#247476),(#247477,#247478,#247479),
(#247480,#247481,#247482),(#247483,#247484,#247485)),.UNSPECIFIED.,.F.,
 .F.,.F.)
B_SPLINE_SURFACE_WITH_KNOTS((4,4),(3,3),(-1.35525271560688E-19,0.000511815090126177),
(0.,1.00105592270234),.UNSPECIFIED.)
GEOMETRIC_REPRESENTATION_ITEM()
RATIONAL_B_SPLINE_SURFACE(((1.,0.70526624271744,1.00062243213092),(1.,0.705584085909104,
1.00062176089524),(1.,0.706182089450463,1.0006204980042),(1.,0.70679750858744,
1.00061919833413)))
REPRESENTATION_ITEM('')
SURFACE()
);
#3612=(
BOUNDED_SURFACE()
B_SPLINE_SURFACE(3,2,((#247487,#247488,#247489),(#247490,#247491,#247492),
(#247493,#247494,#247495),(#247496,#247497,#247498)),.UNSPECIFIED.,.F.,
 .F.,.F.)
B_SPLINE_SURFACE_WITH_KNOTS((4,4),(3,3),(0.,0.000397394428086621),(0.,1.),
 .UNSPECIFIED.)
GEOMETRIC_REPRESENTATION_ITEM()
RATIONAL_B_SPLINE_SURFACE(((1.,0.707106781186545,1.),(1.,0.706459846759102,
1.),(1.,0.705820510737278,1.),(1.,0.705498956110747,1.)))
REPRESENTATION_ITEM('')
SURFACE()
);
#3613=(
BOUNDED_SURFACE()
B_SPLINE_SURFACE(3,2,((#247504,#247505,#247506),(#247507,#247508,#247509),
(#247510,#247511,#247512),(#247513,#247514,#247515),(#247516,#247517,#247518),
(#247519,#247520,#247521)),.UNSPECIFIED.,.F.,.F.,.F.)
B_SPLINE_SURFACE_WITH_KNOTS((4,2,4),(3,3),(0.,0.000257953807872835,0.000515907615745671),
(0.,1.),.UNSPECIFIED.)
GEOMETRIC_REPRESENTATION_ITEM()
RATIONAL_B_SPLINE_SURFACE(((1.,0.874619707139395,1.),(1.,0.874834349678973,
1.),(1.,0.854686104157817,1.),(1.,0.792476597915156,1.),(1.,0.750887854595112,
1.),(1.,0.705585838031439,1.)))
REPRESENTATION_ITEM('')
SURFACE()
);
#3614=(
BOUNDED_SURFACE()
B_SPLINE_SURFACE(3,2,((#247527,#247528,#247529),(#247530,#247531,#247532),
(#247533,#247534,#247535),(#247536,#247537,#247538)),.UNSPECIFIED.,.F.,
 .F.,.F.)
B_SPLINE_SURFACE_WITH_KNOTS((4,4),(3,3),(0.,0.000511815437699155),(0.,1.0010588133155),
 .UNSPECIFIED.)
GEOMETRIC_REPRESENTATION_ITEM()
RATIONAL_B_SPLINE_SURFACE(((1.,0.706796661946457,1.00062089519696),(1.,
0.707430821225312,1.00061955228438),(1.,0.708058545830853,1.00061822299804),
(1.,0.708394505252833,1.00061751156142)))
REPRESENTATION_ITEM('')
SURFACE()
);
#3615=(
BOUNDED_SURFACE()
B_SPLINE_SURFACE(3,2,((#247540,#247541,#247542),(#247543,#247544,#247545),
(#247546,#247547,#247548),(#247549,#247550,#247551),(#247552,#247553,#247554),
(#247555,#247556,#247557)),.UNSPECIFIED.,.F.,.F.,.F.)
B_SPLINE_SURFACE_WITH_KNOTS((4,2,4),(3,3),(0.,0.00025691531753126,0.00051383063506252),
(0.,1.),.UNSPECIFIED.)
GEOMETRIC_REPRESENTATION_ITEM()
RATIONAL_B_SPLINE_SURFACE(((1.,0.705585838031444,1.),(1.,0.750902433542275,
1.),(1.,0.792329530083157,1.),(1.,0.854288401593573,1.),(1.,0.87499803112561,
1.),(1.,0.874619707139394,1.)))
REPRESENTATION_ITEM('')
SURFACE()
);
#3616=(
BOUNDED_SURFACE()
B_SPLINE_SURFACE(3,2,((#247563,#247564,#247565),(#247566,#247567,#247568),
(#247569,#247570,#247571),(#247572,#247573,#247574),(#247575,#247576,#247577),
(#247578,#247579,#247580)),.UNSPECIFIED.,.F.,.F.,.F.)
B_SPLINE_SURFACE_WITH_KNOTS((4,2,4),(3,3),(0.,0.000256592814262163,0.000513185628524326),
(0.,1.),.UNSPECIFIED.)
GEOMETRIC_REPRESENTATION_ITEM()
RATIONAL_B_SPLINE_SURFACE(((1.,0.708712527163656,1.),(1.,0.7537809026137,
1.),(1.,0.794538995769058,1.),(1.,0.855070770331249,1.),(1.,0.875018427445215,
1.),(1.,0.874619707139403,1.)))
REPRESENTATION_ITEM('')
SURFACE()
);
#3617=(
BOUNDED_SURFACE()
B_SPLINE_SURFACE(3,2,((#247582,#247583,#247584),(#247585,#247586,#247587),
(#247588,#247589,#247590),(#247591,#247592,#247593)),.UNSPECIFIED.,.F.,
 .F.,.F.)
B_SPLINE_SURFACE_WITH_KNOTS((4,4),(3,3),(0.,0.0005118150724304),(0.,1.00105598365535),
 .UNSPECIFIED.)
GEOMETRIC_REPRESENTATION_ITEM()
RATIONAL_B_SPLINE_SURFACE(((1.,0.706797490734715,1.00061923411498),(1.,
0.706182062147634,1.00062053388004),(1.,0.705584062770011,1.00062179683518),
(1.,0.705266224771485,1.00062246809864)))
REPRESENTATION_ITEM('')
SURFACE()
);
#3618=(
BOUNDED_SURFACE()
B_SPLINE_SURFACE(3,2,((#247599,#247600,#247601),(#247602,#247603,#247604),
(#247605,#247606,#247607),(#247608,#247609,#247610),(#247611,#247612,#247613),
(#247614,#247615,#247616)),.UNSPECIFIED.,.F.,.F.,.F.)
B_SPLINE_SURFACE_WITH_KNOTS((4,2,4),(3,3),(-3.46944695195361E-18,0.000257652232350873,
0.00051530446470175),(0.,1.),.UNSPECIFIED.)
GEOMETRIC_REPRESENTATION_ITEM()
RATIONAL_B_SPLINE_SURFACE(((1.,0.874619707139393,1.),(1.,0.874861180430414,
1.),(1.,0.855455725921246,1.),(1.,0.794699358954878,1.),(1.,0.753768977788917,
1.),(1.,0.708712527163685,1.)))
REPRESENTATION_ITEM('')
SURFACE()
);
#3619=(
BOUNDED_SURFACE()
B_SPLINE_SURFACE(3,2,((#247622,#247623,#247624),(#247625,#247626,#247627),
(#247628,#247629,#247630),(#247631,#247632,#247633)),.UNSPECIFIED.,.F.,
 .F.,.F.)
B_SPLINE_SURFACE_WITH_KNOTS((4,4),(3,3),(0.,0.000397394373651924),(0.,1.),
 .UNSPECIFIED.)
GEOMETRIC_REPRESENTATION_ITEM()
RATIONAL_B_SPLINE_SURFACE(((1.,0.70710678118655,1.),(1.,0.707752587915898,
1.),(1.,0.708377654540676,1.),(1.,0.708689770883331,1.)))
REPRESENTATION_ITEM('')
SURFACE()
);
#3620=(
BOUNDED_SURFACE()
B_SPLINE_SURFACE(3,2,((#247635,#247636,#247637),(#247638,#247639,#247640),
(#247641,#247642,#247643),(#247644,#247645,#247646)),.UNSPECIFIED.,.F.,
 .F.,.F.)
B_SPLINE_SURFACE_WITH_KNOTS((4,4),(3,3),(-3.06287113727155E-18,0.000511815456479783),
(0.,1.00105873159907),.UNSPECIFIED.)
GEOMETRIC_REPRESENTATION_ITEM()
RATIONAL_B_SPLINE_SURFACE(((1.,0.708394529056585,1.0006174638531),(1.,0.708058564167109,
1.00061817524639),(1.,0.707430835372329,1.00061950443901),(1.,0.706796685880633,
1.00062084722722)))
REPRESENTATION_ITEM('')
SURFACE()
);
#3621=(
BOUNDED_SURFACE()
B_SPLINE_SURFACE(3,2,((#247652,#247653,#247654),(#247655,#247656,#247657),
(#247658,#247659,#247660),(#247661,#247662,#247663)),.UNSPECIFIED.,.F.,
 .F.,.F.)
B_SPLINE_SURFACE_WITH_KNOTS((4,4),(3,3),(0.,0.000397394465448322),(0.,1.),
 .UNSPECIFIED.)
GEOMETRIC_REPRESENTATION_ITEM()
RATIONAL_B_SPLINE_SURFACE(((1.,0.705498956110758,1.),(1.,0.705821764811796,
1.),(1.,0.706461952521131,1.),(1.,0.707106781186554,1.)))
REPRESENTATION_ITEM('')
SURFACE()
);
#3622=(
BOUNDED_SURFACE()
B_SPLINE_SURFACE(3,2,((#247669,#247670,#247671),(#247672,#247673,#247674),
(#247675,#247676,#247677),(#247678,#247679,#247680)),.UNSPECIFIED.,.F.,
 .F.,.F.)
B_SPLINE_SURFACE_WITH_KNOTS((4,4),(3,3),(3.79470760369927E-19,0.000397394410828729),
(0.,1.),.UNSPECIFIED.)
GEOMETRIC_REPRESENTATION_ITEM()
RATIONAL_B_SPLINE_SURFACE(((1.,0.708689770883329,1.),(1.,0.708376440034479,
1.),(1.,0.707750498698412,1.),(1.,0.70710678118655,1.)))
REPRESENTATION_ITEM('')
SURFACE()
);
#3623=(
BOUNDED_SURFACE()
B_SPLINE_SURFACE(3,2,((#247686,#247687,#247688),(#247689,#247690,#247691),
(#247692,#247693,#247694),(#247695,#247696,#247697)),.UNSPECIFIED.,.F.,
 .F.,.F.)
B_SPLINE_SURFACE_WITH_KNOTS((4,4),(3,3),(0.,0.000511815090126172),(0.,1.00105592270453),
 .UNSPECIFIED.)
GEOMETRIC_REPRESENTATION_ITEM()
RATIONAL_B_SPLINE_SURFACE(((1.,0.705266242716804,1.00062243213221),(1.,
0.705584085908435,1.00062176089653),(1.,0.706182089449835,1.0006204980055),
(1.,0.706797508586802,1.00061919833542)))
REPRESENTATION_ITEM('')
SURFACE()
);
#3624=(
BOUNDED_SURFACE()
B_SPLINE_SURFACE(3,2,((#247699,#247700,#247701),(#247702,#247703,#247704),
(#247705,#247706,#247707),(#247708,#247709,#247710)),.UNSPECIFIED.,.F.,
 .F.,.F.)
B_SPLINE_SURFACE_WITH_KNOTS((4,4),(3,3),(-7.80625564189563E-18,0.000397394428086628),
(0.,1.),.UNSPECIFIED.)
GEOMETRIC_REPRESENTATION_ITEM()
RATIONAL_B_SPLINE_SURFACE(((1.,0.70710678118655,1.),(1.,0.70645984675907,
1.),(1.,0.705820510737293,1.),(1.,0.705498956110754,1.)))
REPRESENTATION_ITEM('')
SURFACE()
);
#3625=(
BOUNDED_SURFACE()
B_SPLINE_SURFACE(3,2,((#247716,#247717,#247718),(#247719,#247720,#247721),
(#247722,#247723,#247724),(#247725,#247726,#247727),(#247728,#247729,#247730),
(#247731,#247732,#247733)),.UNSPECIFIED.,.F.,.F.,.F.)
B_SPLINE_SURFACE_WITH_KNOTS((4,2,4),(3,3),(0.,0.00025795380787285,0.000515907615745699),
(0.,1.),.UNSPECIFIED.)
GEOMETRIC_REPRESENTATION_ITEM()
RATIONAL_B_SPLINE_SURFACE(((1.,0.874619707139402,1.),(1.,0.874834349679344,
1.),(1.,0.854686104157338,1.),(1.,0.792476597915597,1.),(1.,0.750887854594773,
1.),(1.,0.705585838031445,1.)))
REPRESENTATION_ITEM('')
SURFACE()
);
#3626=(
BOUNDED_SURFACE()
B_SPLINE_SURFACE(3,2,((#247739,#247740,#247741),(#247742,#247743,#247744),
(#247745,#247746,#247747),(#247748,#247749,#247750)),.UNSPECIFIED.,.F.,
 .F.,.F.)
B_SPLINE_SURFACE_WITH_KNOTS((4,4),(3,3),(-8.13151629364128E-20,0.000511815437699148),
(0.,1.00105881331685),.UNSPECIFIED.)
GEOMETRIC_REPRESENTATION_ITEM()
RATIONAL_B_SPLINE_SURFACE(((1.,0.706796661946055,1.00062089519775),(1.,
0.707430821224927,1.00061955228517),(1.,0.708058545830431,1.00061822299883),
(1.,0.708394505252429,1.00061751156221)))
REPRESENTATION_ITEM('')
SURFACE()
);
#3627=(
BOUNDED_SURFACE()
B_SPLINE_SURFACE(3,2,((#247752,#247753,#247754),(#247755,#247756,#247757),
(#247758,#247759,#247760),(#247761,#247762,#247763),(#247764,#247765,#247766),
(#247767,#247768,#247769)),.UNSPECIFIED.,.F.,.F.,.F.)
B_SPLINE_SURFACE_WITH_KNOTS((4,2,4),(3,3),(5.42101086242752E-20,0.00025691531753127,
0.000513830635062541),(0.,1.),.UNSPECIFIED.)
GEOMETRIC_REPRESENTATION_ITEM()
RATIONAL_B_SPLINE_SURFACE(((1.,0.705585838031452,1.),(1.,0.750902433542135,
1.),(1.,0.792329530083361,1.),(1.,0.85428840159336,1.),(1.,0.874998031125796,
1.),(1.,0.874619707139413,1.)))
REPRESENTATION_ITEM('')
SURFACE()
);
#3628=(
BOUNDED_SURFACE()
B_SPLINE_SURFACE(3,2,((#247775,#247776,#247777),(#247778,#247779,#247780),
(#247781,#247782,#247783),(#247784,#247785,#247786),(#247787,#247788,#247789),
(#247790,#247791,#247792)),.UNSPECIFIED.,.F.,.F.,.F.)
B_SPLINE_SURFACE_WITH_KNOTS((4,2,4),(3,3),(-1.33085816672596E-17,0.000256592814262153,
0.000513185628524318),(0.,1.),.UNSPECIFIED.)
GEOMETRIC_REPRESENTATION_ITEM()
RATIONAL_B_SPLINE_SURFACE(((1.,0.708712527163657,1.),(1.,0.753780902613274,
1.),(1.,0.794538995769617,1.),(1.,0.855070770330683,1.),(1.,0.875018427445638,
1.),(1.,0.874619707139398,1.)))
REPRESENTATION_ITEM('')
SURFACE()
);
#3629=(
BOUNDED_SURFACE()
B_SPLINE_SURFACE(3,2,((#247794,#247795,#247796),(#247797,#247798,#247799),
(#247800,#247801,#247802),(#247803,#247804,#247805)),.UNSPECIFIED.,.F.,
 .F.,.F.)
B_SPLINE_SURFACE_WITH_KNOTS((4,4),(3,3),(0.,0.000511815072430392),(0.,1.00105598365709),
 .UNSPECIFIED.)
GEOMETRIC_REPRESENTATION_ITEM()
RATIONAL_B_SPLINE_SURFACE(((1.,0.706797490734206,1.000619234116),(1.,0.706182062147127,
1.00062053388107),(1.,0.705584062769492,1.0006217968362),(1.,0.705266224770968,
1.00062246809967)))
REPRESENTATION_ITEM('')
SURFACE()
);
#3630=(
BOUNDED_SURFACE()
B_SPLINE_SURFACE(3,2,((#247811,#247812,#247813),(#247814,#247815,#247816),
(#247817,#247818,#247819),(#247820,#247821,#247822),(#247823,#247824,#247825),
(#247826,#247827,#247828)),.UNSPECIFIED.,.F.,.F.,.F.)
B_SPLINE_SURFACE_WITH_KNOTS((4,2,4),(3,3),(0.,0.000257652232350887,0.000515304464701773),
(0.,1.),.UNSPECIFIED.)
GEOMETRIC_REPRESENTATION_ITEM()
RATIONAL_B_SPLINE_SURFACE(((1.,0.87461970713938,1.),(1.,0.874861180430769,
1.),(1.,0.855455725920777,1.),(1.,0.794699358955329,1.),(1.,0.753768977788596,
1.),(1.,0.708712527163624,1.)))
REPRESENTATION_ITEM('')
SURFACE()
);
#3631=(
BOUNDED_SURFACE()
B_SPLINE_SURFACE(3,2,((#247834,#247835,#247836),(#247837,#247838,#247839),
(#247840,#247841,#247842),(#247843,#247844,#247845)),.UNSPECIFIED.,.F.,
 .F.,.F.)
B_SPLINE_SURFACE_WITH_KNOTS((4,4),(3,3),(0.,0.000397394373651907),(0.,1.),
 .UNSPECIFIED.)
GEOMETRIC_REPRESENTATION_ITEM()
RATIONAL_B_SPLINE_SURFACE(((1.,0.707106781186545,1.),(1.,0.707752587915894,
1.),(1.,0.708377654540684,1.),(1.,0.708689770883333,1.)))
REPRESENTATION_ITEM('')
SURFACE()
);
#3632=(
BOUNDED_SURFACE()
B_SPLINE_SURFACE(3,2,((#247847,#247848,#247849),(#247850,#247851,#247852),
(#247853,#247854,#247855),(#247856,#247857,#247858)),.UNSPECIFIED.,.F.,
 .F.,.F.)
B_SPLINE_SURFACE_WITH_KNOTS((4,4),(3,3),(0.,0.000511815456479797),(0.,1.00105873160002),
 .UNSPECIFIED.)
GEOMETRIC_REPRESENTATION_ITEM()
RATIONAL_B_SPLINE_SURFACE(((1.,0.708394529056337,1.00061746385365),(1.,
0.708058564166813,1.00061817524694),(1.,0.707430835372066,1.00061950443957),
(1.,0.706796685880356,1.00062084722778)))
REPRESENTATION_ITEM('')
SURFACE()
);
#3633=(
BOUNDED_SURFACE()
B_SPLINE_SURFACE(3,2,((#247864,#247865,#247866),(#247867,#247868,#247869),
(#247870,#247871,#247872),(#247873,#247874,#247875)),.UNSPECIFIED.,.F.,
 .F.,.F.)
B_SPLINE_SURFACE_WITH_KNOTS((4,4),(3,3),(-3.52365706057789E-19,0.000397394465448304),
(0.,1.),.UNSPECIFIED.)
GEOMETRIC_REPRESENTATION_ITEM()
RATIONAL_B_SPLINE_SURFACE(((1.,0.705498956110757,1.),(1.,0.705821764811772,
1.),(1.,0.706461952521142,1.),(1.,0.707106781186548,1.)))
REPRESENTATION_ITEM('')
SURFACE()
);
#3634=(
BOUNDED_SURFACE()
B_SPLINE_SURFACE(3,2,((#247881,#247882,#247883),(#247884,#247885,#247886),
(#247887,#247888,#247889),(#247890,#247891,#247892)),.UNSPECIFIED.,.F.,
 .F.,.F.)
B_SPLINE_SURFACE_WITH_KNOTS((4,4),(3,3),(4.87890977618477E-19,0.000397394410828734),
(0.,1.),.UNSPECIFIED.)
GEOMETRIC_REPRESENTATION_ITEM()
RATIONAL_B_SPLINE_SURFACE(((1.,0.708689770883329,1.),(1.,0.708376440034481,
1.),(1.,0.707750498698425,1.),(1.,0.707106781186533,1.)))
REPRESENTATION_ITEM('')
SURFACE()
);
#3635=(
BOUNDED_SURFACE()
B_SPLINE_SURFACE(3,2,((#247898,#247899,#247900),(#247901,#247902,#247903),
(#247904,#247905,#247906),(#247907,#247908,#247909)),.UNSPECIFIED.,.F.,
 .F.,.F.)
B_SPLINE_SURFACE_WITH_KNOTS((4,4),(3,3),(3.19839640883224E-18,0.000511815090126191),
(0.,1.00105592270058),.UNSPECIFIED.)
GEOMETRIC_REPRESENTATION_ITEM()
RATIONAL_B_SPLINE_SURFACE(((1.,0.705266242717954,1.00062243212989),(1.,
0.705584085909609,1.0006217608942),(1.,0.706182089450989,1.00062049800317),
(1.,0.706797508587958,1.0006191983331)))
REPRESENTATION_ITEM('')
SURFACE()
);
#3636=(
BOUNDED_SURFACE()
B_SPLINE_SURFACE(3,2,((#247911,#247912,#247913),(#247914,#247915,#247916),
(#247917,#247918,#247919),(#247920,#247921,#247922)),.UNSPECIFIED.,.F.,
 .F.,.F.)
B_SPLINE_SURFACE_WITH_KNOTS((4,4),(3,3),(0.,0.00039739442808663),(0.,1.),
 .UNSPECIFIED.)
GEOMETRIC_REPRESENTATION_ITEM()
RATIONAL_B_SPLINE_SURFACE(((1.,0.70710678118655,1.),(1.,0.706459846759083,
1.),(1.,0.705820510737299,1.),(1.,0.705498956110753,1.)))
REPRESENTATION_ITEM('')
SURFACE()
);
#3637=(
BOUNDED_SURFACE()
B_SPLINE_SURFACE(3,2,((#247928,#247929,#247930),(#247931,#247932,#247933),
(#247934,#247935,#247936),(#247937,#247938,#247939),(#247940,#247941,#247942),
(#247943,#247944,#247945)),.UNSPECIFIED.,.F.,.F.,.F.)
B_SPLINE_SURFACE_WITH_KNOTS((4,2,4),(3,3),(0.,0.000257953807872844,0.000515907615745688),
(0.,1.),.UNSPECIFIED.)
GEOMETRIC_REPRESENTATION_ITEM()
RATIONAL_B_SPLINE_SURFACE(((1.,0.874619707139388,1.),(1.,0.874834349679326,
1.),(1.,0.854686104157358,1.),(1.,0.79247659791558,1.),(1.,0.750887854594821,
1.),(1.,0.705585838031413,1.)))
REPRESENTATION_ITEM('')
SURFACE()
);
#3638=(
BOUNDED_SURFACE()
B_SPLINE_SURFACE(3,2,((#247951,#247952,#247953),(#247954,#247955,#247956),
(#247957,#247958,#247959),(#247960,#247961,#247962)),.UNSPECIFIED.,.F.,
 .F.,.F.)
B_SPLINE_SURFACE_WITH_KNOTS((4,4),(3,3),(0.,0.000511815437699147),(0.,1.00105881331661),
 .UNSPECIFIED.)
GEOMETRIC_REPRESENTATION_ITEM()
RATIONAL_B_SPLINE_SURFACE(((1.,0.706796661946126,1.00062089519761),(1.,
0.707430821224989,1.00061955228503),(1.,0.708058545830522,1.00061822299869),
(1.,0.708394505252503,1.00061751156207)))
REPRESENTATION_ITEM('')
SURFACE()
);
#3639=(
BOUNDED_SURFACE()
B_SPLINE_SURFACE(3,2,((#247964,#247965,#247966),(#247967,#247968,#247969),
(#247970,#247971,#247972),(#247973,#247974,#247975),(#247976,#247977,#247978),
(#247979,#247980,#247981)),.UNSPECIFIED.,.F.,.F.,.F.)
B_SPLINE_SURFACE_WITH_KNOTS((4,2,4),(3,3),(-1.35525271560688E-19,0.000256915317531268,
0.000513830635062535),(0.,1.),.UNSPECIFIED.)
GEOMETRIC_REPRESENTATION_ITEM()
RATIONAL_B_SPLINE_SURFACE(((1.,0.705585838031459,1.),(1.,0.750902433542557,
1.),(1.,0.792329530082764,1.),(1.,0.854288401593981,1.),(1.,0.874998031125318,
1.),(1.,0.87461970713942,1.)))
REPRESENTATION_ITEM('')
SURFACE()
);
#3640=(
BOUNDED_SURFACE()
B_SPLINE_SURFACE(3,2,((#247987,#247988,#247989),(#247990,#247991,#247992),
(#247993,#247994,#247995),(#247996,#247997,#247998),(#247999,#248000,#248001),
(#248002,#248003,#248004)),.UNSPECIFIED.,.F.,.F.,.F.)
B_SPLINE_SURFACE_WITH_KNOTS((4,2,4),(3,3),(-1.05438661274215E-17,0.000256592814262151,
0.000513185628524312),(0.,1.),.UNSPECIFIED.)
GEOMETRIC_REPRESENTATION_ITEM()
RATIONAL_B_SPLINE_SURFACE(((1.,0.708712527163662,1.),(1.,0.753780902614111,
1.),(1.,0.79453899576847,1.),(1.,0.855070770331844,1.),(1.,0.875018427444773,
1.),(1.,0.874619707139394,1.)))
REPRESENTATION_ITEM('')
SURFACE()
);
#3641=(
BOUNDED_SURFACE()
B_SPLINE_SURFACE(3,2,((#248006,#248007,#248008),(#248009,#248010,#248011),
(#248012,#248013,#248014),(#248015,#248016,#248017)),.UNSPECIFIED.,.F.,
 .F.,.F.)
B_SPLINE_SURFACE_WITH_KNOTS((4,4),(3,3),(-5.42101086242752E-20,0.000511815072430393),
(0.,1.00105598365896),.UNSPECIFIED.)
GEOMETRIC_REPRESENTATION_ITEM()
RATIONAL_B_SPLINE_SURFACE(((1.,0.706797490733667,1.0006192341171),(1.,0.706182062146547,
1.00062053388216),(1.,0.705584062768983,1.0006217968373),(1.,0.70526622477041,
1.00062246810077)))
REPRESENTATION_ITEM('')
SURFACE()
);
#3642=(
BOUNDED_SURFACE()
B_SPLINE_SURFACE(3,2,((#248023,#248024,#248025),(#248026,#248027,#248028),
(#248029,#248030,#248031),(#248032,#248033,#248034),(#248035,#248036,#248037),
(#248038,#248039,#248040)),.UNSPECIFIED.,.F.,.F.,.F.)
B_SPLINE_SURFACE_WITH_KNOTS((4,2,4),(3,3),(-5.28548559086683E-19,0.000257652232350884,
0.000515304464701769),(0.,1.),.UNSPECIFIED.)
GEOMETRIC_REPRESENTATION_ITEM()
RATIONAL_B_SPLINE_SURFACE(((1.,0.87461970713938,1.),(1.,0.874861180430975,
1.),(1.,0.855455725920509,1.),(1.,0.794699358955589,1.),(1.,0.753768977788371,
1.),(1.,0.708712527163643,1.)))
REPRESENTATION_ITEM('')
SURFACE()
);
#3643=(
BOUNDED_SURFACE()
B_SPLINE_SURFACE(3,2,((#248046,#248047,#248048),(#248049,#248050,#248051),
(#248052,#248053,#248054),(#248055,#248056,#248057)),.UNSPECIFIED.,.F.,
 .F.,.F.)
B_SPLINE_SURFACE_WITH_KNOTS((4,4),(3,3),(-1.56938264467277E-17,0.000397394373651899),
(0.,1.),.UNSPECIFIED.)
GEOMETRIC_REPRESENTATION_ITEM()
RATIONAL_B_SPLINE_SURFACE(((1.,0.707106781186553,1.),(1.,0.707752587915868,
1.),(1.,0.708377654540695,1.),(1.,0.708689770883335,1.)))
REPRESENTATION_ITEM('')
SURFACE()
);
#3644=(
BOUNDED_SURFACE()
B_SPLINE_SURFACE(3,2,((#248059,#248060,#248061),(#248062,#248063,#248064),
(#248065,#248066,#248067),(#248068,#248069,#248070)),.UNSPECIFIED.,.F.,
 .F.,.F.)
B_SPLINE_SURFACE_WITH_KNOTS((4,4),(3,3),(-4.06575814682064E-19,0.000511815456479783),
(0.,1.0010587315981),.UNSPECIFIED.)
GEOMETRIC_REPRESENTATION_ITEM()
RATIONAL_B_SPLINE_SURFACE(((1.,0.708394529056873,1.00061746385253),(1.,
0.708058564167432,1.00061817524582),(1.,0.707430835372599,1.00061950443844),
(1.,0.706796685880911,1.00062084722665)))
REPRESENTATION_ITEM('')
SURFACE()
);
#3645=(
BOUNDED_SURFACE()
B_SPLINE_SURFACE(3,2,((#248076,#248077,#248078),(#248079,#248080,#248081),
(#248082,#248083,#248084),(#248085,#248086,#248087)),.UNSPECIFIED.,.F.,
 .F.,.F.)
B_SPLINE_SURFACE_WITH_KNOTS((4,4),(3,3),(-5.14996031930615E-19,0.000397394465448316),
(0.,1.),.UNSPECIFIED.)
GEOMETRIC_REPRESENTATION_ITEM()
RATIONAL_B_SPLINE_SURFACE(((1.,0.705498956110749,1.),(1.,0.705821764811784,
1.),(1.,0.70646195252115,1.),(1.,0.707106781186545,1.)))
REPRESENTATION_ITEM('')
SURFACE()
);
#3646=(
BOUNDED_SURFACE()
B_SPLINE_SURFACE(3,2,((#248093,#248094,#248095),(#248096,#248097,#248098),
(#248099,#248100,#248101),(#248102,#248103,#248104)),.UNSPECIFIED.,.F.,
 .F.,.F.)
B_SPLINE_SURFACE_WITH_KNOTS((4,4),(3,3),(5.96311194867027E-19,0.000397394410828733),
(0.,1.),.UNSPECIFIED.)
GEOMETRIC_REPRESENTATION_ITEM()
RATIONAL_B_SPLINE_SURFACE(((1.,0.708689770883335,1.),(1.,0.70837644003448,
1.),(1.,0.707750498698401,1.),(1.,0.70710678118655,1.)))
REPRESENTATION_ITEM('')
SURFACE()
);
#3647=(
BOUNDED_SURFACE()
B_SPLINE_SURFACE(3,2,((#248110,#248111,#248112),(#248113,#248114,#248115),
(#248116,#248117,#248118),(#248119,#248120,#248121)),.UNSPECIFIED.,.F.,
 .F.,.F.)
B_SPLINE_SURFACE_WITH_KNOTS((4,4),(3,3),(0.,0.000511815090126191),(0.,1.00105592270065),
 .UNSPECIFIED.)
GEOMETRIC_REPRESENTATION_ITEM()
RATIONAL_B_SPLINE_SURFACE(((1.,0.705266242717941,1.00062243212992),(1.,
0.705584085909598,1.00062176089424),(1.,0.706182089450967,1.00062049800321),
(1.,0.706797508587938,1.00061919833314)))
REPRESENTATION_ITEM('')
SURFACE()
);
#3648=(
BOUNDED_SURFACE()
B_SPLINE_SURFACE(3,2,((#248123,#248124,#248125),(#248126,#248127,#248128),
(#248129,#248130,#248131),(#248132,#248133,#248134)),.UNSPECIFIED.,.F.,
 .F.,.F.)
B_SPLINE_SURFACE_WITH_KNOTS((4,4),(3,3),(0.,0.000397394428086623),(0.,1.),
 .UNSPECIFIED.)
GEOMETRIC_REPRESENTATION_ITEM()
RATIONAL_B_SPLINE_SURFACE(((1.,0.70710678118655,1.),(1.,0.706459846759068,
1.),(1.,0.705820510737312,1.),(1.,0.70549895611075,1.)))
REPRESENTATION_ITEM('')
SURFACE()
);
#3649=(
BOUNDED_SURFACE()
B_SPLINE_SURFACE(3,2,((#248140,#248141,#248142),(#248143,#248144,#248145),
(#248146,#248147,#248148),(#248149,#248150,#248151),(#248152,#248153,#248154),
(#248155,#248156,#248157)),.UNSPECIFIED.,.F.,.F.,.F.)
B_SPLINE_SURFACE_WITH_KNOTS((4,2,4),(3,3),(0.,0.000257953807872843,0.000515907615745686),
(0.,1.),.UNSPECIFIED.)
GEOMETRIC_REPRESENTATION_ITEM()
RATIONAL_B_SPLINE_SURFACE(((1.,0.874619707139393,1.),(1.,0.874834349680018,
1.),(1.,0.85468610415643,1.),(1.,0.792476597916507,1.),(1.,0.750887854594091,
1.),(1.,0.705585838031455,1.)))
REPRESENTATION_ITEM('')
SURFACE()
);
#3650=(
BOUNDED_SURFACE()
B_SPLINE_SURFACE(3,2,((#248163,#248164,#248165),(#248166,#248167,#248168),
(#248169,#248170,#248171),(#248172,#248173,#248174)),.UNSPECIFIED.,.F.,
 .F.,.F.)
B_SPLINE_SURFACE_WITH_KNOTS((4,4),(3,3),(-8.13151629364128E-20,0.000511815437699164),
(0.,1.00105881331608),.UNSPECIFIED.)
GEOMETRIC_REPRESENTATION_ITEM()
RATIONAL_B_SPLINE_SURFACE(((1.,0.706796661946281,1.0006208951973),(1.,0.707430821225167,
1.00061955228472),(1.,0.70805854583067,1.00061822299838),(1.,0.708394505252657,
1.00061751156176)))
REPRESENTATION_ITEM('')
SURFACE()
);
#3651=(
BOUNDED_SURFACE()
B_SPLINE_SURFACE(3,2,((#248176,#248177,#248178),(#248179,#248180,#248181),
(#248182,#248183,#248184),(#248185,#248186,#248187),(#248188,#248189,#248190),
(#248191,#248192,#248193)),.UNSPECIFIED.,.F.,.F.,.F.)
B_SPLINE_SURFACE_WITH_KNOTS((4,2,4),(3,3),(-3.25260651745651E-19,0.000256915317531264,
0.000513830635062529),(0.,1.),.UNSPECIFIED.)
GEOMETRIC_REPRESENTATION_ITEM()
RATIONAL_B_SPLINE_SURFACE(((1.,0.70558583803144,1.),(1.,0.750902433542234,
1.),(1.,0.792329530083195,1.),(1.,0.854288401593536,1.),(1.,0.874998031125647,
1.),(1.,0.874619707139385,1.)))
REPRESENTATION_ITEM('')
SURFACE()
);
#3652=(
BOUNDED_SURFACE()
B_SPLINE_SURFACE(3,2,((#248199,#248200,#248201),(#248202,#248203,#248204),
(#248205,#248206,#248207),(#248208,#248209,#248210),(#248211,#248212,#248213),
(#248214,#248215,#248216)),.UNSPECIFIED.,.F.,.F.,.F.)
B_SPLINE_SURFACE_WITH_KNOTS((4,2,4),(3,3),(-3.6049722235143E-18,0.000256592814262163,
0.00051318562852433),(0.,1.),.UNSPECIFIED.)
GEOMETRIC_REPRESENTATION_ITEM()
RATIONAL_B_SPLINE_SURFACE(((1.,0.708712527163664,1.),(1.,0.753780902613515,
1.),(1.,0.794538995769305,1.),(1.,0.855070770331,1.),(1.,0.875018427445427,
1.),(1.,0.87461970713939,1.)))
REPRESENTATION_ITEM('')
SURFACE()
);
#3653=(
BOUNDED_SURFACE()
B_SPLINE_SURFACE(3,2,((#248218,#248219,#248220),(#248221,#248222,#248223),
(#248224,#248225,#248226),(#248227,#248228,#248229)),.UNSPECIFIED.,.F.,
 .F.,.F.)
B_SPLINE_SURFACE_WITH_KNOTS((4,4),(3,3),(-5.6920614055489E-19,0.000511815072430396),
(0.,1.00105598365828),.UNSPECIFIED.)
GEOMETRIC_REPRESENTATION_ITEM()
RATIONAL_B_SPLINE_SURFACE(((1.,0.706797490733857,1.0006192341167),(1.,0.706182062146763,
1.00062053388177),(1.,0.70558406276914,1.00062179683691),(1.,0.705266224770631,
1.00062246810037)))
REPRESENTATION_ITEM('')
SURFACE()
);
#3654=(
BOUNDED_SURFACE()
B_SPLINE_SURFACE(3,2,((#248235,#248236,#248237),(#248238,#248239,#248240),
(#248241,#248242,#248243),(#248244,#248245,#248246),(#248247,#248248,#248249),
(#248250,#248251,#248252)),.UNSPECIFIED.,.F.,.F.,.F.)
B_SPLINE_SURFACE_WITH_KNOTS((4,2,4),(3,3),(0.,0.000257652232350883,0.000515304464701766),
(0.,1.),.UNSPECIFIED.)
GEOMETRIC_REPRESENTATION_ITEM()
RATIONAL_B_SPLINE_SURFACE(((1.,0.874619707139399,1.),(1.,0.874861180430963,
1.),(1.,0.855455725920514,1.),(1.,0.794699358955633,1.),(1.,0.753768977788405,
1.),(1.,0.708712527163651,1.)))
REPRESENTATION_ITEM('')
SURFACE()
);
#3655=(
BOUNDED_SURFACE()
B_SPLINE_SURFACE(3,2,((#248258,#248259,#248260),(#248261,#248262,#248263),
(#248264,#248265,#248266),(#248267,#248268,#248269)),.UNSPECIFIED.,.F.,
 .F.,.F.)
B_SPLINE_SURFACE_WITH_KNOTS((4,4),(3,3),(0.,0.000397394373651917),(0.,1.),
 .UNSPECIFIED.)
GEOMETRIC_REPRESENTATION_ITEM()
RATIONAL_B_SPLINE_SURFACE(((1.,0.707106781186535,1.),(1.,0.707752587915927,
1.),(1.,0.708377654540653,1.),(1.,0.708689770883321,1.)))
REPRESENTATION_ITEM('')
SURFACE()
);
#3656=(
BOUNDED_SURFACE()
B_SPLINE_SURFACE(3,2,((#248271,#248272,#248273),(#248274,#248275,#248276),
(#248277,#248278,#248279),(#248280,#248281,#248282)),.UNSPECIFIED.,.F.,
 .F.,.F.)
B_SPLINE_SURFACE_WITH_KNOTS((4,4),(3,3),(0.,0.000511815456479791),(0.,1.00105873159918),
 .UNSPECIFIED.)
GEOMETRIC_REPRESENTATION_ITEM()
RATIONAL_B_SPLINE_SURFACE(((1.,0.708394529056554,1.00061746385316),(1.,
0.708058564167108,1.00061817524645),(1.,0.707430835372274,1.00061950443907),
(1.,0.70679668588061,1.00062084722729)))
REPRESENTATION_ITEM('')
SURFACE()
);
#3657=(
BOUNDED_SURFACE()
B_SPLINE_SURFACE(3,2,((#248288,#248289,#248290),(#248291,#248292,#248293),
(#248294,#248295,#248296),(#248297,#248298,#248299)),.UNSPECIFIED.,.F.,
 .F.,.F.)
B_SPLINE_SURFACE_WITH_KNOTS((4,4),(3,3),(-6.23416249179165E-19,0.000397394465448315),
(0.,1.),.UNSPECIFIED.)
GEOMETRIC_REPRESENTATION_ITEM()
RATIONAL_B_SPLINE_SURFACE(((1.,0.70549895611076,1.),(1.,0.705821764811773,
1.),(1.,0.706461952521134,1.),(1.,0.707106781186545,1.)))
REPRESENTATION_ITEM('')
SURFACE()
);
#3658=(
BOUNDED_SURFACE()
B_SPLINE_SURFACE(3,2,((#248305,#248306,#248307),(#248308,#248309,#248310),
(#248311,#248312,#248313),(#248314,#248315,#248316)),.UNSPECIFIED.,.F.,
 .F.,.F.)
B_SPLINE_SURFACE_WITH_KNOTS((4,4),(3,3),(0.,0.000397394410828731),(0.,1.),
 .UNSPECIFIED.)
GEOMETRIC_REPRESENTATION_ITEM()
RATIONAL_B_SPLINE_SURFACE(((1.,0.708689770883323,1.),(1.,0.708376440034482,
1.),(1.,0.707750498698435,1.),(1.,0.707106781186543,1.)))
REPRESENTATION_ITEM('')
SURFACE()
);
#3659=(
BOUNDED_SURFACE()
B_SPLINE_SURFACE(3,2,((#248322,#248323,#248324),(#248325,#248326,#248327),
(#248328,#248329,#248330),(#248331,#248332,#248333)),.UNSPECIFIED.,.F.,
 .F.,.F.)
B_SPLINE_SURFACE_WITH_KNOTS((4,4),(3,3),(0.,0.000511815090126181),(0.,1.00105592270032),
 .UNSPECIFIED.)
GEOMETRIC_REPRESENTATION_ITEM()
RATIONAL_B_SPLINE_SURFACE(((1.,0.705266242718053,1.00062243212973),(1.,
0.705584085909701,1.00062176089404),(1.,0.706182089451028,1.00062049800302),
(1.,0.706797508588036,1.00061919833294)))
REPRESENTATION_ITEM('')
SURFACE()
);
#3660=(
BOUNDED_SURFACE()
B_SPLINE_SURFACE(3,2,((#248335,#248336,#248337),(#248338,#248339,#248340),
(#248341,#248342,#248343),(#248344,#248345,#248346)),.UNSPECIFIED.,.F.,
 .F.,.F.)
B_SPLINE_SURFACE_WITH_KNOTS((4,4),(3,3),(0.,0.000397394428086633),(0.,1.),
 .UNSPECIFIED.)
GEOMETRIC_REPRESENTATION_ITEM()
RATIONAL_B_SPLINE_SURFACE(((1.,0.707106781186539,1.),(1.,0.706459846759122,
1.),(1.,0.705820510737294,1.),(1.,0.705498956110738,1.)))
REPRESENTATION_ITEM('')
SURFACE()
);
#3661=(
BOUNDED_SURFACE()
B_SPLINE_SURFACE(3,2,((#248352,#248353,#248354),(#248355,#248356,#248357),
(#248358,#248359,#248360),(#248361,#248362,#248363),(#248364,#248365,#248366),
(#248367,#248368,#248369)),.UNSPECIFIED.,.F.,.F.,.F.)
B_SPLINE_SURFACE_WITH_KNOTS((4,2,4),(3,3),(0.,0.000257953807872844,0.000515907615745689),
(0.,1.),.UNSPECIFIED.)
GEOMETRIC_REPRESENTATION_ITEM()
RATIONAL_B_SPLINE_SURFACE(((1.,0.874619707139397,1.),(1.,0.874834349679094,
1.),(1.,0.854686104157672,1.),(1.,0.792476597915231,1.),(1.,0.750887854595069,
1.),(1.,0.705585838031445,1.)))
REPRESENTATION_ITEM('')
SURFACE()
);
#3662=(
BOUNDED_SURFACE()
B_SPLINE_SURFACE(3,2,((#248375,#248376,#248377),(#248378,#248379,#248380),
(#248381,#248382,#248383),(#248384,#248385,#248386)),.UNSPECIFIED.,.F.,
 .F.,.F.)
B_SPLINE_SURFACE_WITH_KNOTS((4,4),(3,3),(5.6920614055489E-19,0.000511815437699151),
(0.,1.00105881331661),.UNSPECIFIED.)
GEOMETRIC_REPRESENTATION_ITEM()
RATIONAL_B_SPLINE_SURFACE(((1.,0.706796661946126,1.00062089519761),(1.,
0.707430821224996,1.00061955228503),(1.,0.708058545830506,1.00061822299869),
(1.,0.708394505252508,1.00061751156207)))
REPRESENTATION_ITEM('')
SURFACE()
);
#3663=(
BOUNDED_SURFACE()
B_SPLINE_SURFACE(3,2,((#248388,#248389,#248390),(#248391,#248392,#248393),
(#248394,#248395,#248396),(#248397,#248398,#248399),(#248400,#248401,#248402),
(#248403,#248404,#248405)),.UNSPECIFIED.,.F.,.F.,.F.)
B_SPLINE_SURFACE_WITH_KNOTS((4,2,4),(3,3),(0.,0.000256915317531267,0.000513830635062533),
(0.,1.),.UNSPECIFIED.)
GEOMETRIC_REPRESENTATION_ITEM()
RATIONAL_B_SPLINE_SURFACE(((1.,0.705585838031428,1.),(1.,0.750902433542297,
1.),(1.,0.792329530083163,1.),(1.,0.854288401593562,1.),(1.,0.874998031125636,
1.),(1.,0.874619707139394,1.)))
REPRESENTATION_ITEM('')
SURFACE()
);
#3664=(
BOUNDED_SURFACE()
B_SPLINE_SURFACE(3,2,((#248411,#248412,#248413),(#248414,#248415,#248416),
(#248417,#248418,#248419),(#248420,#248421,#248422),(#248423,#248424,#248425),
(#248426,#248427,#248428)),.UNSPECIFIED.,.F.,.F.,.F.)
B_SPLINE_SURFACE_WITH_KNOTS((4,2,4),(3,3),(-7.31836466427715E-19,0.000256592814262155,
0.000513185628524311),(0.,1.),.UNSPECIFIED.)
GEOMETRIC_REPRESENTATION_ITEM()
RATIONAL_B_SPLINE_SURFACE(((1.,0.708712527163665,1.),(1.,0.753780902613352,
1.),(1.,0.794538995769519,1.),(1.,0.855070770330792,1.),(1.,0.875018427445553,
1.),(1.,0.874619707139396,1.)))
REPRESENTATION_ITEM('')
SURFACE()
);
#3665=(
BOUNDED_SURFACE()
B_SPLINE_SURFACE(3,2,((#248430,#248431,#248432),(#248433,#248434,#248435),
(#248436,#248437,#248438),(#248439,#248440,#248441)),.UNSPECIFIED.,.F.,
 .F.,.F.)
B_SPLINE_SURFACE_WITH_KNOTS((4,4),(3,3),(0.,0.000511815072430391),(0.,1.00105598365643),
 .UNSPECIFIED.)
GEOMETRIC_REPRESENTATION_ITEM()
RATIONAL_B_SPLINE_SURFACE(((1.,0.706797490734398,1.00061923411562),(1.,
0.706182062147312,1.00062053388068),(1.,0.705584062769681,1.00062179683582),
(1.,0.705266224771159,1.00062246809928)))
REPRESENTATION_ITEM('')
SURFACE()
);
#3666=(
BOUNDED_SURFACE()
B_SPLINE_SURFACE(3,2,((#248447,#248448,#248449),(#248450,#248451,#248452),
(#248453,#248454,#248455),(#248456,#248457,#248458),(#248459,#248460,#248461),
(#248462,#248463,#248464)),.UNSPECIFIED.,.F.,.F.,.F.)
B_SPLINE_SURFACE_WITH_KNOTS((4,2,4),(3,3),(0.,0.000257652232350891,0.000515304464701781),
(0.,1.),.UNSPECIFIED.)
GEOMETRIC_REPRESENTATION_ITEM()
RATIONAL_B_SPLINE_SURFACE(((1.,0.874619707139387,1.),(1.,0.874861180430548,
1.),(1.,0.855455725921075,1.),(1.,0.794699358955069,1.),(1.,0.75376897778878,
1.),(1.,0.70871252716364,1.)))
REPRESENTATION_ITEM('')
SURFACE()
);
#3667=(
BOUNDED_SURFACE()
B_SPLINE_SURFACE(3,2,((#248470,#248471,#248472),(#248473,#248474,#248475),
(#248476,#248477,#248478),(#248479,#248480,#248481)),.UNSPECIFIED.,.F.,
 .F.,.F.)
B_SPLINE_SURFACE_WITH_KNOTS((4,4),(3,3),(-9.26992857475106E-18,0.000397394373651915),
(0.,1.),.UNSPECIFIED.)
GEOMETRIC_REPRESENTATION_ITEM()
RATIONAL_B_SPLINE_SURFACE(((1.,0.707106781186556,1.),(1.,0.707752587915886,
1.),(1.,0.708377654540688,1.),(1.,0.708689770883341,1.)))
REPRESENTATION_ITEM('')
SURFACE()
);
#3668=(
BOUNDED_SURFACE()
B_SPLINE_SURFACE(3,2,((#248483,#248484,#248485),(#248486,#248487,#248488),
(#248489,#248490,#248491),(#248492,#248493,#248494)),.UNSPECIFIED.,.F.,
 .F.,.F.)
B_SPLINE_SURFACE_WITH_KNOTS((4,4),(3,3),(0.,0.000511815456479786),(0.,1.00105873160137),
 .UNSPECIFIED.)
GEOMETRIC_REPRESENTATION_ITEM()
RATIONAL_B_SPLINE_SURFACE(((1.,0.708394529055883,1.00061746385444),(1.,
0.708058564166512,1.00061817524773),(1.,0.707430835371623,1.00061950444036),
(1.,0.706796685879971,1.00062084722857)))
REPRESENTATION_ITEM('')
SURFACE()
);
#3669=(
BOUNDED_SURFACE()
B_SPLINE_SURFACE(3,2,((#248500,#248501,#248502),(#248503,#248504,#248505),
(#248506,#248507,#248508),(#248509,#248510,#248511)),.UNSPECIFIED.,.F.,
 .F.,.F.)
B_SPLINE_SURFACE_WITH_KNOTS((4,4),(3,3),(-4.06575814682064E-18,0.000397394465448322),
(0.,1.),.UNSPECIFIED.)
GEOMETRIC_REPRESENTATION_ITEM()
RATIONAL_B_SPLINE_SURFACE(((1.,0.705498956110734,1.),(1.,0.70582176481179,
1.),(1.,0.706461952521119,1.),(1.,0.707106781186556,1.)))
REPRESENTATION_ITEM('')
SURFACE()
);
#3670=(
BOUNDED_SURFACE()
B_SPLINE_SURFACE(3,2,((#248517,#248518,#248519),(#248520,#248521,#248522),
(#248523,#248524,#248525),(#248526,#248527,#248528)),.UNSPECIFIED.,.F.,
 .F.,.F.)
B_SPLINE_SURFACE_WITH_KNOTS((4,4),(3,3),(0.,0.000397394410828732),(0.,1.),
 .UNSPECIFIED.)
GEOMETRIC_REPRESENTATION_ITEM()
RATIONAL_B_SPLINE_SURFACE(((1.,0.708689770883327,1.),(1.,0.708376440034498,
1.),(1.,0.707750498698427,1.),(1.,0.707106781186549,1.)))
REPRESENTATION_ITEM('')
SURFACE()
);
#3671=(
BOUNDED_SURFACE()
B_SPLINE_SURFACE(3,2,((#248534,#248535,#248536),(#248537,#248538,#248539),
(#248540,#248541,#248542),(#248543,#248544,#248545)),.UNSPECIFIED.,.F.,
 .F.,.F.)
B_SPLINE_SURFACE_WITH_KNOTS((4,4),(3,3),(-1.59919820441612E-18,0.000511815090126176),
(0.,1.00105592270011),.UNSPECIFIED.)
GEOMETRIC_REPRESENTATION_ITEM()
RATIONAL_B_SPLINE_SURFACE(((1.,0.705266242718087,1.0006224321296),(1.,0.705584085909776,
1.00062176089392),(1.,0.706182089451103,1.00062049800289),(1.,0.706797508588096,
1.00061919833282)))
REPRESENTATION_ITEM('')
SURFACE()
);
#3672=(
BOUNDED_SURFACE()
B_SPLINE_SURFACE(3,2,((#248547,#248548,#248549),(#248550,#248551,#248552),
(#248553,#248554,#248555),(#248556,#248557,#248558)),.UNSPECIFIED.,.F.,
 .F.,.F.)
B_SPLINE_SURFACE_WITH_KNOTS((4,4),(3,3),(0.,0.000397394428086635),(0.,1.),
 .UNSPECIFIED.)
GEOMETRIC_REPRESENTATION_ITEM()
RATIONAL_B_SPLINE_SURFACE(((1.,0.707106781186549,1.),(1.,0.706459846759078,
1.),(1.,0.705820510737299,1.),(1.,0.705498956110743,1.)))
REPRESENTATION_ITEM('')
SURFACE()
);
#3673=(
BOUNDED_SURFACE()
B_SPLINE_SURFACE(3,2,((#248564,#248565,#248566),(#248567,#248568,#248569),
(#248570,#248571,#248572),(#248573,#248574,#248575),(#248576,#248577,#248578),
(#248579,#248580,#248581)),.UNSPECIFIED.,.F.,.F.,.F.)
B_SPLINE_SURFACE_WITH_KNOTS((4,2,4),(3,3),(0.,0.000257953807872847,0.000515907615745694),
(0.,1.),.UNSPECIFIED.)
GEOMETRIC_REPRESENTATION_ITEM()
RATIONAL_B_SPLINE_SURFACE(((1.,0.874619707139385,1.),(1.,0.874834349678975,
1.),(1.,0.854686104157834,1.),(1.,0.792476597915104,1.),(1.,0.750887854595155,
1.),(1.,0.705585838031417,1.)))
REPRESENTATION_ITEM('')
SURFACE()
);
#3674=(
BOUNDED_SURFACE()
B_SPLINE_SURFACE(3,2,((#248587,#248588,#248589),(#248590,#248591,#248592),
(#248593,#248594,#248595),(#248596,#248597,#248598)),.UNSPECIFIED.,.F.,
 .F.,.F.)
B_SPLINE_SURFACE_WITH_KNOTS((4,4),(3,3),(0.,0.000511815437699152),(0.,1.00105881331622),
 .UNSPECIFIED.)
GEOMETRIC_REPRESENTATION_ITEM()
RATIONAL_B_SPLINE_SURFACE(((1.,0.706796661946239,1.00062089519738),(1.,
0.707430821225126,1.0006195522848),(1.,0.708058545830628,1.00061822299846),
(1.,0.708394505252628,1.00061751156184)))
REPRESENTATION_ITEM('')
SURFACE()
);
#3675=(
BOUNDED_SURFACE()
B_SPLINE_SURFACE(3,2,((#248600,#248601,#248602),(#248603,#248604,#248605),
(#248606,#248607,#248608),(#248609,#248610,#248611),(#248612,#248613,#248614),
(#248615,#248616,#248617)),.UNSPECIFIED.,.F.,.F.,.F.)
B_SPLINE_SURFACE_WITH_KNOTS((4,2,4),(3,3),(-8.6465123255719E-18,0.000256915317531255,
0.000513830635062519),(0.,1.),.UNSPECIFIED.)
GEOMETRIC_REPRESENTATION_ITEM()
RATIONAL_B_SPLINE_SURFACE(((1.,0.70558583803142,1.),(1.,0.750902433543074,
1.),(1.,0.792329530082077,1.),(1.,0.854288401594625,1.),(1.,0.874998031124799,
1.),(1.,0.874619707139392,1.)))
REPRESENTATION_ITEM('')
SURFACE()
);
#3676=(
BOUNDED_SURFACE()
B_SPLINE_SURFACE(3,2,((#248623,#248624,#248625),(#248626,#248627,#248628),
(#248629,#248630,#248631),(#248632,#248633,#248634),(#248635,#248636,#248637),
(#248638,#248639,#248640)),.UNSPECIFIED.,.F.,.F.,.F.)
B_SPLINE_SURFACE_WITH_KNOTS((4,2,4),(3,3),(-8.59230221694762E-18,0.000256592814262153,
0.000513185628524315),(0.,1.),.UNSPECIFIED.)
GEOMETRIC_REPRESENTATION_ITEM()
RATIONAL_B_SPLINE_SURFACE(((1.,0.708712527163675,1.),(1.,0.753780902613455,
1.),(1.,0.794538995769379,1.),(1.,0.855070770330912,1.),(1.,0.87501842744547,
1.),(1.,0.874619707139402,1.)))
REPRESENTATION_ITEM('')
SURFACE()
);
#3677=(
BOUNDED_SURFACE()
B_SPLINE_SURFACE(3,2,((#248642,#248643,#248644),(#248645,#248646,#248647),
(#248648,#248649,#248650),(#248651,#248652,#248653)),.UNSPECIFIED.,.F.,
 .F.,.F.)
B_SPLINE_SURFACE_WITH_KNOTS((4,4),(3,3),(0.,0.000511815072430396),(0.,1.00105598365749),
 .UNSPECIFIED.)
GEOMETRIC_REPRESENTATION_ITEM()
RATIONAL_B_SPLINE_SURFACE(((1.,0.706797490734088,1.00061923411624),(1.,
0.706182062147,1.0006205338813),(1.,0.705584062769387,1.00062179683644),
(1.,0.705266224770861,1.00062246809991)))
REPRESENTATION_ITEM('')
SURFACE()
);
#3678=(
BOUNDED_SURFACE()
B_SPLINE_SURFACE(3,2,((#248659,#248660,#248661),(#248662,#248663,#248664),
(#248665,#248666,#248667),(#248668,#248669,#248670),(#248671,#248672,#248673),
(#248674,#248675,#248676)),.UNSPECIFIED.,.F.,.F.,.F.)
B_SPLINE_SURFACE_WITH_KNOTS((4,2,4),(3,3),(-9.81202966099382E-18,0.000257652232350868,
0.000515304464701747),(0.,1.),.UNSPECIFIED.)
GEOMETRIC_REPRESENTATION_ITEM()
RATIONAL_B_SPLINE_SURFACE(((1.,0.874619707139399,1.),(1.,0.874861180430778,
1.),(1.,0.855455725920788,1.),(1.,0.794699358955341,1.),(1.,0.753768977788617,
1.),(1.,0.708712527163659,1.)))
REPRESENTATION_ITEM('')
SURFACE()
);
#3679=(
BOUNDED_SURFACE()
B_SPLINE_SURFACE(3,2,((#248682,#248683,#248684),(#248685,#248686,#248687),
(#248688,#248689,#248690),(#248691,#248692,#248693)),.UNSPECIFIED.,.F.,
 .F.,.F.)
B_SPLINE_SURFACE_WITH_KNOTS((4,4),(3,3),(5.96311194867027E-19,0.00039739437365192),
(0.,1.),.UNSPECIFIED.)
GEOMETRIC_REPRESENTATION_ITEM()
RATIONAL_B_SPLINE_SURFACE(((1.,0.707106781186546,1.),(1.,0.707752587915923,
1.),(1.,0.708377654540663,1.),(1.,0.708689770883323,1.)))
REPRESENTATION_ITEM('')
SURFACE()
);
#3680=(
BOUNDED_SURFACE()
B_SPLINE_SURFACE(3,2,((#248695,#248696,#248697),(#248698,#248699,#248700),
(#248701,#248702,#248703),(#248704,#248705,#248706)),.UNSPECIFIED.,.F.,
 .F.,.F.)
B_SPLINE_SURFACE_WITH_KNOTS((4,4),(3,3),(-1.62630325872826E-18,0.000511815456479784),
(0.,1.00105873160343),.UNSPECIFIED.)
GEOMETRIC_REPRESENTATION_ITEM()
RATIONAL_B_SPLINE_SURFACE(((1.,0.708394529055308,1.00061746385565),(1.,
0.708058564165876,1.00061817524894),(1.,0.707430835371038,1.00061950444157),
(1.,0.706796685879357,1.00062084722978)))
REPRESENTATION_ITEM('')
SURFACE()
);
#3681=(
BOUNDED_SURFACE()
B_SPLINE_SURFACE(3,2,((#248712,#248713,#248714),(#248715,#248716,#248717),
(#248718,#248719,#248720),(#248721,#248722,#248723)),.UNSPECIFIED.,.F.,
 .F.,.F.)
B_SPLINE_SURFACE_WITH_KNOTS((4,4),(3,3),(0.,0.0003973944654483),(0.,1.),
 .UNSPECIFIED.)
GEOMETRIC_REPRESENTATION_ITEM()
RATIONAL_B_SPLINE_SURFACE(((1.,0.705498956110752,1.),(1.,0.705821764811786,
1.),(1.,0.706461952521135,1.),(1.,0.707106781186546,1.)))
REPRESENTATION_ITEM('')
SURFACE()
);
#3682=(
BOUNDED_SURFACE()
B_SPLINE_SURFACE(3,2,((#248729,#248730,#248731),(#248732,#248733,#248734),
(#248735,#248736,#248737),(#248738,#248739,#248740)),.UNSPECIFIED.,.F.,
 .F.,.F.)
B_SPLINE_SURFACE_WITH_KNOTS((4,4),(3,3),(0.,0.00039739441082874),(0.,1.),
 .UNSPECIFIED.)
GEOMETRIC_REPRESENTATION_ITEM()
RATIONAL_B_SPLINE_SURFACE(((1.,0.708689770883324,1.),(1.,0.708376440034465,
1.),(1.,0.70775049869842,1.),(1.,0.707106781186549,1.)))
REPRESENTATION_ITEM('')
SURFACE()
);
#3683=(
BOUNDED_SURFACE()
B_SPLINE_SURFACE(3,2,((#248746,#248747,#248748),(#248749,#248750,#248751),
(#248752,#248753,#248754),(#248755,#248756,#248757)),.UNSPECIFIED.,.F.,
 .F.,.F.)
B_SPLINE_SURFACE_WITH_KNOTS((4,4),(3,3),(3.19839640883224E-18,0.000511815090126186),
(0.,1.00105592270213),.UNSPECIFIED.)
GEOMETRIC_REPRESENTATION_ITEM()
RATIONAL_B_SPLINE_SURFACE(((1.,0.705266242717516,1.0006224321308),(1.,0.705584085909153,
1.00062176089511),(1.,0.706182089450503,1.00062049800408),(1.,0.706797508587505,
1.00061919833401)))
REPRESENTATION_ITEM('')
SURFACE()
);
#3684=(
BOUNDED_SURFACE()
B_SPLINE_SURFACE(3,2,((#248759,#248760,#248761),(#248762,#248763,#248764),
(#248765,#248766,#248767),(#248768,#248769,#248770)),.UNSPECIFIED.,.F.,
 .F.,.F.)
B_SPLINE_SURFACE_WITH_KNOTS((4,4),(3,3),(-5.96311194867027E-19,0.000397394428086614),
(0.,1.),.UNSPECIFIED.)
GEOMETRIC_REPRESENTATION_ITEM()
RATIONAL_B_SPLINE_SURFACE(((1.,0.707106781186549,1.),(1.,0.70645984675909,
1.),(1.,0.705820510737294,1.),(1.,0.705498956110753,1.)))
REPRESENTATION_ITEM('')
SURFACE()
);
#3685=(
BOUNDED_SURFACE()
B_SPLINE_SURFACE(3,2,((#248776,#248777,#248778),(#248779,#248780,#248781),
(#248782,#248783,#248784),(#248785,#248786,#248787),(#248788,#248789,#248790),
(#248791,#248792,#248793)),.UNSPECIFIED.,.F.,.F.,.F.)
B_SPLINE_SURFACE_WITH_KNOTS((4,2,4),(3,3),(0.,0.000257953807872847,0.000515907615745694),
(0.,1.),.UNSPECIFIED.)
GEOMETRIC_REPRESENTATION_ITEM()
RATIONAL_B_SPLINE_SURFACE(((1.,0.874619707139392,1.),(1.,0.874834349678804,
1.),(1.,0.854686104158036,1.),(1.,0.792476597914902,1.),(1.,0.750887854595278,
1.),(1.,0.705585838031443,1.)))
REPRESENTATION_ITEM('')
SURFACE()
);
#3686=(
BOUNDED_SURFACE()
B_SPLINE_SURFACE(3,2,((#248799,#248800,#248801),(#248802,#248803,#248804),
(#248805,#248806,#248807),(#248808,#248809,#248810)),.UNSPECIFIED.,.F.,
 .F.,.F.)
B_SPLINE_SURFACE_WITH_KNOTS((4,4),(3,3),(-9.21571846612679E-18,0.000511815437699153),
(0.,1.00105881331631),.UNSPECIFIED.)
GEOMETRIC_REPRESENTATION_ITEM()
RATIONAL_B_SPLINE_SURFACE(((1.,0.706796661946213,1.00062089519743),(1.,
0.707430821225091,1.00061955228486),(1.,0.708058545830576,1.00061822299851),
(1.,0.70839450525259,1.00061751156189)))
REPRESENTATION_ITEM('')
SURFACE()
);
#3687=(
BOUNDED_SURFACE()
B_SPLINE_SURFACE(3,2,((#248812,#248813,#248814),(#248815,#248816,#248817),
(#248818,#248819,#248820),(#248821,#248822,#248823),(#248824,#248825,#248826),
(#248827,#248828,#248829)),.UNSPECIFIED.,.F.,.F.,.F.)
B_SPLINE_SURFACE_WITH_KNOTS((4,2,4),(3,3),(0.,0.000256915317531268,0.000513830635062536),
(0.,1.),.UNSPECIFIED.)
GEOMETRIC_REPRESENTATION_ITEM()
RATIONAL_B_SPLINE_SURFACE(((1.,0.705585838031433,1.),(1.,0.750902433542739,
1.),(1.,0.792329530082555,1.),(1.,0.854288401594177,1.),(1.,0.874998031125162,
1.),(1.,0.874619707139394,1.)))
REPRESENTATION_ITEM('')
SURFACE()
);
#3688=(
BOUNDED_SURFACE()
B_SPLINE_SURFACE(3,2,((#248835,#248836,#248837),(#248838,#248839,#248840),
(#248841,#248842,#248843),(#248844,#248845,#248846),(#248847,#248848,#248849),
(#248850,#248851,#248852)),.UNSPECIFIED.,.F.,.F.,.F.)
B_SPLINE_SURFACE_WITH_KNOTS((4,2,4),(3,3),(-1.43656787854329E-18,0.000256592814262153,
0.000513185628524308),(0.,1.),.UNSPECIFIED.)
GEOMETRIC_REPRESENTATION_ITEM()
RATIONAL_B_SPLINE_SURFACE(((1.,0.708712527163662,1.),(1.,0.75378090261378,
1.),(1.,0.794538995768932,1.),(1.,0.855070770331388,1.),(1.,0.87501842744511,
1.),(1.,0.874619707139403,1.)))
REPRESENTATION_ITEM('')
SURFACE()
);
#3689=(
BOUNDED_SURFACE()
B_SPLINE_SURFACE(3,2,((#248854,#248855,#248856),(#248857,#248858,#248859),
(#248860,#248861,#248862),(#248863,#248864,#248865)),.UNSPECIFIED.,.F.,
 .F.,.F.)
B_SPLINE_SURFACE_WITH_KNOTS((4,4),(3,3),(0.,0.000511815072430396),(0.,1.00105598365732),
 .UNSPECIFIED.)
GEOMETRIC_REPRESENTATION_ITEM()
RATIONAL_B_SPLINE_SURFACE(((1.,0.706797490734141,1.00061923411614),(1.,
0.706182062147035,1.0006205338812),(1.,0.705584062769417,1.00062179683634),
(1.,0.705266224770904,1.0006224680998)))
REPRESENTATION_ITEM('')
SURFACE()
);
#3690=(
BOUNDED_SURFACE()
B_SPLINE_SURFACE(3,2,((#248871,#248872,#248873),(#248874,#248875,#248876),
(#248877,#248878,#248879),(#248880,#248881,#248882),(#248883,#248884,#248885),
(#248886,#248887,#248888)),.UNSPECIFIED.,.F.,.F.,.F.)
B_SPLINE_SURFACE_WITH_KNOTS((4,2,4),(3,3),(-5.14996031930615E-19,0.00025765223235089,
0.000515304464701781),(0.,1.),.UNSPECIFIED.)
GEOMETRIC_REPRESENTATION_ITEM()
RATIONAL_B_SPLINE_SURFACE(((1.,0.874619707139388,1.),(1.,0.874861180431065,
1.),(1.,0.855455725920387,1.),(1.,0.794699358955754,1.),(1.,0.753768977788268,
1.),(1.,0.708712527163674,1.)))
REPRESENTATION_ITEM('')
SURFACE()
);
#3691=(
BOUNDED_SURFACE()
B_SPLINE_SURFACE(3,2,((#248894,#248895,#248896),(#248897,#248898,#248899),
(#248900,#248901,#248902),(#248903,#248904,#248905)),.UNSPECIFIED.,.F.,
 .F.,.F.)
B_SPLINE_SURFACE_WITH_KNOTS((4,4),(3,3),(0.,0.000397394373651913),(0.,1.),
 .UNSPECIFIED.)
GEOMETRIC_REPRESENTATION_ITEM()
RATIONAL_B_SPLINE_SURFACE(((1.,0.707106781186546,1.),(1.,0.707752587915897,
1.),(1.,0.708377654540679,1.),(1.,0.708689770883326,1.)))
REPRESENTATION_ITEM('')
SURFACE()
);
#3692=(
BOUNDED_SURFACE()
B_SPLINE_SURFACE(3,2,((#248907,#248908,#248909),(#248910,#248911,#248912),
(#248913,#248914,#248915),(#248916,#248917,#248918)),.UNSPECIFIED.,.F.,
 .F.,.F.)
B_SPLINE_SURFACE_WITH_KNOTS((4,4),(3,3),(0.,0.000511815456479785),(0.,1.00105873159871),
 .UNSPECIFIED.)
GEOMETRIC_REPRESENTATION_ITEM()
RATIONAL_B_SPLINE_SURFACE(((1.,0.708394529056685,1.00061746385289),(1.,
0.708058564167261,1.00061817524618),(1.,0.70743083537241,1.0006195044388),
(1.,0.706796685880754,1.00062084722701)))
REPRESENTATION_ITEM('')
SURFACE()
);
#3693=(
BOUNDED_SURFACE()
B_SPLINE_SURFACE(3,2,((#248924,#248925,#248926),(#248927,#248928,#248929),
(#248930,#248931,#248932),(#248933,#248934,#248935)),.UNSPECIFIED.,.F.,
 .F.,.F.)
B_SPLINE_SURFACE_WITH_KNOTS((4,4),(3,3),(0.,0.000397394465448299),(0.,1.),
 .UNSPECIFIED.)
GEOMETRIC_REPRESENTATION_ITEM()
RATIONAL_B_SPLINE_SURFACE(((1.,0.705498956110716,1.),(1.,0.705821764811794,
1.),(1.,0.706461952521151,1.),(1.,0.707106781186533,1.)))
REPRESENTATION_ITEM('')
SURFACE()
);
#3694=(
BOUNDED_SURFACE()
B_SPLINE_SURFACE(3,2,((#248941,#248942,#248943),(#248944,#248945,#248946),
(#248947,#248948,#248949),(#248950,#248951,#248952)),.UNSPECIFIED.,.F.,
 .F.,.F.)
B_SPLINE_SURFACE_WITH_KNOTS((4,4),(3,3),(0.,0.000397394410828737),(0.,1.),
 .UNSPECIFIED.)
GEOMETRIC_REPRESENTATION_ITEM()
RATIONAL_B_SPLINE_SURFACE(((1.,0.708689770883333,1.),(1.,0.708376440034488,
1.),(1.,0.7077504986984,1.),(1.,0.70710678118656,1.)))
REPRESENTATION_ITEM('')
SURFACE()
);
#3695=(
BOUNDED_SURFACE()
B_SPLINE_SURFACE(3,2,((#248958,#248959,#248960),(#248961,#248962,#248963),
(#248964,#248965,#248966),(#248967,#248968,#248969)),.UNSPECIFIED.,.F.,
 .F.,.F.)
B_SPLINE_SURFACE_WITH_KNOTS((4,4),(3,3),(0.,0.00051181509012619),(0.,1.00105592269933),
 .UNSPECIFIED.)
GEOMETRIC_REPRESENTATION_ITEM()
RATIONAL_B_SPLINE_SURFACE(((1.,0.705266242718325,1.00062243212914),(1.,
0.705584085909984,1.00062176089346),(1.,0.70618208945133,1.00062049800243),
(1.,0.706797508588325,1.00061919833236)))
REPRESENTATION_ITEM('')
SURFACE()
);
#3696=(
BOUNDED_SURFACE()
B_SPLINE_SURFACE(3,2,((#248971,#248972,#248973),(#248974,#248975,#248976),
(#248977,#248978,#248979),(#248980,#248981,#248982)),.UNSPECIFIED.,.F.,
 .F.,.F.)
B_SPLINE_SURFACE_WITH_KNOTS((4,4),(3,3),(-6.26126754610379E-18,0.000397394428086626),
(0.,1.),.UNSPECIFIED.)
GEOMETRIC_REPRESENTATION_ITEM()
RATIONAL_B_SPLINE_SURFACE(((1.,0.707106781186549,1.),(1.,0.706459846759093,
1.),(1.,0.705820510737289,1.),(1.,0.705498956110746,1.)))
REPRESENTATION_ITEM('')
SURFACE()
);
#3697=(
BOUNDED_SURFACE()
B_SPLINE_SURFACE(3,2,((#248988,#248989,#248990),(#248991,#248992,#248993),
(#248994,#248995,#248996),(#248997,#248998,#248999),(#249000,#249001,#249002),
(#249003,#249004,#249005)),.UNSPECIFIED.,.F.,.F.,.F.)
B_SPLINE_SURFACE_WITH_KNOTS((4,2,4),(3,3),(0.,0.000257953807872849,0.000515907615745697),
(0.,1.),.UNSPECIFIED.)
GEOMETRIC_REPRESENTATION_ITEM()
RATIONAL_B_SPLINE_SURFACE(((1.,0.874619707139393,1.),(1.,0.874834349679035,
1.),(1.,0.854686104157749,1.),(1.,0.792476597915191,1.),(1.,0.750887854595084,
1.),(1.,0.705585838031438,1.)))
REPRESENTATION_ITEM('')
SURFACE()
);
#3698=(
BOUNDED_SURFACE()
B_SPLINE_SURFACE(3,2,((#249011,#249012,#249013),(#249014,#249015,#249016),
(#249017,#249018,#249019),(#249020,#249021,#249022)),.UNSPECIFIED.,.F.,
 .F.,.F.)
B_SPLINE_SURFACE_WITH_KNOTS((4,4),(3,3),(0.,0.00051181543769915),(0.,1.00105881331638),
 .UNSPECIFIED.)
GEOMETRIC_REPRESENTATION_ITEM()
RATIONAL_B_SPLINE_SURFACE(((1.,0.706796661946193,1.00062089519747),(1.,
0.707430821225081,1.0006195522849),(1.,0.708058545830556,1.00061822299855),
(1.,0.708394505252586,1.00061751156193)))
REPRESENTATION_ITEM('')
SURFACE()
);
#3699=(
BOUNDED_SURFACE()
B_SPLINE_SURFACE(3,2,((#249024,#249025,#249026),(#249027,#249028,#249029),
(#249030,#249031,#249032),(#249033,#249034,#249035),(#249036,#249037,#249038),
(#249039,#249040,#249041)),.UNSPECIFIED.,.F.,.F.,.F.)
B_SPLINE_SURFACE_WITH_KNOTS((4,2,4),(3,3),(2.90024081139872E-18,0.000256915317531264,
0.000513830635062526),(0.,1.),.UNSPECIFIED.)
GEOMETRIC_REPRESENTATION_ITEM()
RATIONAL_B_SPLINE_SURFACE(((1.,0.705585838031437,1.),(1.,0.750902433543791,
1.),(1.,0.792329530081131,1.),(1.,0.854288401595599,1.),(1.,0.874998031124076,
1.),(1.,0.874619707139391,1.)))
REPRESENTATION_ITEM('')
SURFACE()
);
#3700=(
BOUNDED_SURFACE()
B_SPLINE_SURFACE(3,2,((#249047,#249048,#249049),(#249050,#249051,#249052),
(#249053,#249054,#249055),(#249056,#249057,#249058),(#249059,#249060,#249061),
(#249062,#249063,#249064)),.UNSPECIFIED.,.F.,.F.,.F.)
B_SPLINE_SURFACE_WITH_KNOTS((4,2,4),(3,3),(0.,0.000256592814262157,0.000513185628524314),
(0.,1.),.UNSPECIFIED.)
GEOMETRIC_REPRESENTATION_ITEM()
RATIONAL_B_SPLINE_SURFACE(((1.,0.708712527163633,1.),(1.,0.753780902613117,
1.),(1.,0.794538995769877,1.),(1.,0.855070770330416,1.),(1.,0.875018427445846,
1.),(1.,0.874619707139403,1.)))
REPRESENTATION_ITEM('')
SURFACE()
);
#3701=(
BOUNDED_SURFACE()
B_SPLINE_SURFACE(3,2,((#249066,#249067,#249068),(#249069,#249070,#249071),
(#249072,#249073,#249074),(#249075,#249076,#249077)),.UNSPECIFIED.,.F.,
 .F.,.F.)
B_SPLINE_SURFACE_WITH_KNOTS((4,4),(3,3),(0.,0.000511815072430398),(0.,1.00105598365789),
 .UNSPECIFIED.)
GEOMETRIC_REPRESENTATION_ITEM()
RATIONAL_B_SPLINE_SURFACE(((1.,0.706797490733974,1.00061923411647),(1.,
0.706182062146914,1.00062053388153),(1.,0.705584062769252,1.00062179683667),
(1.,0.705266224770738,1.00062246810014)))
REPRESENTATION_ITEM('')
SURFACE()
);
#3702=(
BOUNDED_SURFACE()
B_SPLINE_SURFACE(3,2,((#249083,#249084,#249085),(#249086,#249087,#249088),
(#249089,#249090,#249091),(#249092,#249093,#249094),(#249095,#249096,#249097),
(#249098,#249099,#249100)),.UNSPECIFIED.,.F.,.F.,.F.)
B_SPLINE_SURFACE_WITH_KNOTS((4,2,4),(3,3),(0.,0.000257652232350886,0.000515304464701772),
(0.,1.),.UNSPECIFIED.)
GEOMETRIC_REPRESENTATION_ITEM()
RATIONAL_B_SPLINE_SURFACE(((1.,0.874619707139397,1.),(1.,0.874861180430422,
1.),(1.,0.855455725921253,1.),(1.,0.794699358954883,1.),(1.,0.753768977788929,
1.),(1.,0.708712527163669,1.)))
REPRESENTATION_ITEM('')
SURFACE()
);
#3703=(
BOUNDED_SURFACE()
B_SPLINE_SURFACE(3,2,((#249106,#249107,#249108),(#249109,#249110,#249111),
(#249112,#249113,#249114),(#249115,#249116,#249117)),.UNSPECIFIED.,.F.,
 .F.,.F.)
B_SPLINE_SURFACE_WITH_KNOTS((4,4),(3,3),(0.,0.000397394373651908),(0.,1.),
 .UNSPECIFIED.)
GEOMETRIC_REPRESENTATION_ITEM()
RATIONAL_B_SPLINE_SURFACE(((1.,0.707106781186546,1.),(1.,0.707752587915901,
1.),(1.,0.708377654540672,1.),(1.,0.708689770883331,1.)))
REPRESENTATION_ITEM('')
SURFACE()
);
#3704=(
BOUNDED_SURFACE()
B_SPLINE_SURFACE(3,2,((#249119,#249120,#249121),(#249122,#249123,#249124),
(#249125,#249126,#249127),(#249128,#249129,#249130)),.UNSPECIFIED.,.F.,
 .F.,.F.)
B_SPLINE_SURFACE_WITH_KNOTS((4,4),(3,3),(0.,0.000511815456479783),(0.,1.00105873160032),
 .UNSPECIFIED.)
GEOMETRIC_REPRESENTATION_ITEM()
RATIONAL_B_SPLINE_SURFACE(((1.,0.708394529056214,1.00061746385383),(1.,
0.70805856416676,1.00061817524712),(1.,0.707430835371966,1.00061950443974),
(1.,0.706796685880259,1.00062084722795)))
REPRESENTATION_ITEM('')
SURFACE()
);
#3705=(
BOUNDED_SURFACE()
B_SPLINE_SURFACE(3,2,((#249136,#249137,#249138),(#249139,#249140,#249141),
(#249142,#249143,#249144),(#249145,#249146,#249147)),.UNSPECIFIED.,.F.,
 .F.,.F.)
B_SPLINE_SURFACE_WITH_KNOTS((4,4),(3,3),(0.,0.000397394465448303),(0.,1.),
 .UNSPECIFIED.)
GEOMETRIC_REPRESENTATION_ITEM()
RATIONAL_B_SPLINE_SURFACE(((1.,0.705498956110751,1.),(1.,0.705821764811794,
1.),(1.,0.706461952521126,1.),(1.,0.707106781186546,1.)))
REPRESENTATION_ITEM('')
SURFACE()
);
#3706=(
BOUNDED_SURFACE()
B_SPLINE_SURFACE(3,2,((#249153,#249154,#249155),(#249156,#249157,#249158),
(#249159,#249160,#249161),(#249162,#249163,#249164)),.UNSPECIFIED.,.F.,
 .F.,.F.)
B_SPLINE_SURFACE_WITH_KNOTS((4,4),(3,3),(0.,0.000397394410828739),(0.,1.),
 .UNSPECIFIED.)
GEOMETRIC_REPRESENTATION_ITEM()
RATIONAL_B_SPLINE_SURFACE(((1.,0.708689770883341,1.),(1.,0.708376440034498,
1.),(1.,0.707750498698416,1.),(1.,0.70710678118655,1.)))
REPRESENTATION_ITEM('')
SURFACE()
);
#3707=(
BOUNDED_SURFACE()
B_SPLINE_SURFACE(3,2,((#249170,#249171,#249172),(#249173,#249174,#249175),
(#249176,#249177,#249178),(#249179,#249180,#249181)),.UNSPECIFIED.,.F.,
 .F.,.F.)
B_SPLINE_SURFACE_WITH_KNOTS((4,4),(3,3),(-4.06575814682064E-19,0.000511815090126176),
(0.,1.00105592270253),.UNSPECIFIED.)
GEOMETRIC_REPRESENTATION_ITEM()
RATIONAL_B_SPLINE_SURFACE(((1.,0.705266242717368,1.00062243213103),(1.,
0.705584085909073,1.00062176089535),(1.,0.706182089450375,1.00062049800432),
(1.,0.706797508587387,1.00061919833424)))
REPRESENTATION_ITEM('')
SURFACE()
);
#3708=(
BOUNDED_SURFACE()
B_SPLINE_SURFACE(3,2,((#249183,#249184,#249185),(#249186,#249187,#249188),
(#249189,#249190,#249191),(#249192,#249193,#249194)),.UNSPECIFIED.,.F.,
 .F.,.F.)
B_SPLINE_SURFACE_WITH_KNOTS((4,4),(3,3),(-5.42101086242752E-20,0.000397394428086623),
(0.,1.),.UNSPECIFIED.)
GEOMETRIC_REPRESENTATION_ITEM()
RATIONAL_B_SPLINE_SURFACE(((1.,0.707106781186549,1.),(1.,0.706459846759087,
1.),(1.,0.705820510737284,1.),(1.,0.705498956110736,1.)))
REPRESENTATION_ITEM('')
SURFACE()
);
#3709=(
BOUNDED_SURFACE()
B_SPLINE_SURFACE(3,2,((#249200,#249201,#249202),(#249203,#249204,#249205),
(#249206,#249207,#249208),(#249209,#249210,#249211),(#249212,#249213,#249214),
(#249215,#249216,#249217)),.UNSPECIFIED.,.F.,.F.,.F.)
B_SPLINE_SURFACE_WITH_KNOTS((4,2,4),(3,3),(0.,0.000257953807872845,0.00051590761574569),
(0.,1.),.UNSPECIFIED.)
GEOMETRIC_REPRESENTATION_ITEM()
RATIONAL_B_SPLINE_SURFACE(((1.,0.874619707139394,1.),(1.,0.874834349679555,
1.),(1.,0.854686104157056,1.),(1.,0.792476597915864,1.),(1.,0.750887854594591,
1.),(1.,0.705585838031442,1.)))
REPRESENTATION_ITEM('')
SURFACE()
);
#3710=(
BOUNDED_SURFACE()
B_SPLINE_SURFACE(3,2,((#249223,#249224,#249225),(#249226,#249227,#249228),
(#249229,#249230,#249231),(#249232,#249233,#249234)),.UNSPECIFIED.,.F.,
 .F.,.F.)
B_SPLINE_SURFACE_WITH_KNOTS((4,4),(3,3),(0.,0.00051181543769915),(0.,1.00105881331787),
 .UNSPECIFIED.)
GEOMETRIC_REPRESENTATION_ITEM()
RATIONAL_B_SPLINE_SURFACE(((1.,0.706796661945757,1.00062089519835),(1.,
0.707430821224658,1.00061955228577),(1.,0.708058545830111,1.00061822299943),
(1.,0.708394505252165,1.00061751156281)))
REPRESENTATION_ITEM('')
SURFACE()
);
#3711=(
BOUNDED_SURFACE()
B_SPLINE_SURFACE(3,2,((#249236,#249237,#249238),(#249239,#249240,#249241),
(#249242,#249243,#249244),(#249245,#249246,#249247),(#249248,#249249,#249250),
(#249251,#249252,#249253)),.UNSPECIFIED.,.F.,.F.,.F.)
B_SPLINE_SURFACE_WITH_KNOTS((4,2,4),(3,3),(0.,0.000256915317531267,0.000513830635062535),
(0.,1.),.UNSPECIFIED.)
GEOMETRIC_REPRESENTATION_ITEM()
RATIONAL_B_SPLINE_SURFACE(((1.,0.705585838031432,1.),(1.,0.750902433542741,
1.),(1.,0.792329530082537,1.),(1.,0.854288401594207,1.),(1.,0.874998031125139,
1.),(1.,0.874619707139396,1.)))
REPRESENTATION_ITEM('')
SURFACE()
);
#3712=(
BOUNDED_SURFACE()
B_SPLINE_SURFACE(3,2,((#249259,#249260,#249261),(#249262,#249263,#249264),
(#249265,#249266,#249267),(#249268,#249269,#249270),(#249271,#249272,#249273),
(#249274,#249275,#249276)),.UNSPECIFIED.,.F.,.F.,.F.)
B_SPLINE_SURFACE_WITH_KNOTS((4,2,4),(3,3),(-2.87313575708659E-18,0.000256592814262152,
0.000513185628524308),(0.,1.),.UNSPECIFIED.)
GEOMETRIC_REPRESENTATION_ITEM()
RATIONAL_B_SPLINE_SURFACE(((1.,0.708712527163668,1.),(1.,0.753780902614103,
1.),(1.,0.79453899576851,1.),(1.,0.855070770331806,1.),(1.,0.875018427444798,
1.),(1.,0.874619707139392,1.)))
REPRESENTATION_ITEM('')
SURFACE()
);
#3713=(
BOUNDED_SURFACE()
B_SPLINE_SURFACE(3,2,((#249278,#249279,#249280),(#249281,#249282,#249283),
(#249284,#249285,#249286),(#249287,#249288,#249289)),.UNSPECIFIED.,.F.,
 .F.,.F.)
B_SPLINE_SURFACE_WITH_KNOTS((4,4),(3,3),(0.,0.000511815072430403),(0.,1.00105598365859),
 .UNSPECIFIED.)
GEOMETRIC_REPRESENTATION_ITEM()
RATIONAL_B_SPLINE_SURFACE(((1.,0.706797490733767,1.00061923411689),(1.,
0.706182062146727,1.00062053388195),(1.,0.705584062769004,1.00062179683709),
(1.,0.705266224770526,1.00062246810056)))
REPRESENTATION_ITEM('')
SURFACE()
);
#3714=(
BOUNDED_SURFACE()
B_SPLINE_SURFACE(3,2,((#249295,#249296,#249297),(#249298,#249299,#249300),
(#249301,#249302,#249303),(#249304,#249305,#249306),(#249307,#249308,#249309),
(#249310,#249311,#249312)),.UNSPECIFIED.,.F.,.F.,.F.)
B_SPLINE_SURFACE_WITH_KNOTS((4,2,4),(3,3),(-2.87313575708659E-18,0.000257652232350883,
0.000515304464701769),(0.,1.),.UNSPECIFIED.)
GEOMETRIC_REPRESENTATION_ITEM()
RATIONAL_B_SPLINE_SURFACE(((1.,0.874619707139394,1.),(1.,0.874861180430723,
1.),(1.,0.85545572592083,1.),(1.,0.794699358955305,1.),(1.,0.753768977788583,
1.),(1.,0.708712527163669,1.)))
REPRESENTATION_ITEM('')
SURFACE()
);
#3715=(
BOUNDED_SURFACE()
B_SPLINE_SURFACE(3,2,((#249318,#249319,#249320),(#249321,#249322,#249323),
(#249324,#249325,#249326),(#249327,#249328,#249329)),.UNSPECIFIED.,.F.,
 .F.,.F.)
B_SPLINE_SURFACE_WITH_KNOTS((4,4),(3,3),(-7.86046575051991E-18,0.000397394373651897),
(0.,1.),.UNSPECIFIED.)
GEOMETRIC_REPRESENTATION_ITEM()
RATIONAL_B_SPLINE_SURFACE(((1.,0.707106781186546,1.),(1.,0.707752587915903,
1.),(1.,0.708377654540693,1.),(1.,0.708689770883325,1.)))
REPRESENTATION_ITEM('')
SURFACE()
);
#3716=(
BOUNDED_SURFACE()
B_SPLINE_SURFACE(3,2,((#249331,#249332,#249333),(#249334,#249335,#249336),
(#249337,#249338,#249339),(#249340,#249341,#249342)),.UNSPECIFIED.,.F.,
 .F.,.F.)
B_SPLINE_SURFACE_WITH_KNOTS((4,4),(3,3),(0.,0.000511815456479783),(0.,1.00105873160118),
 .UNSPECIFIED.)
GEOMETRIC_REPRESENTATION_ITEM()
RATIONAL_B_SPLINE_SURFACE(((1.,0.708394529055962,1.00061746385433),(1.,
0.708058564166525,1.00061817524762),(1.,0.707430835371686,1.00061950444025),
(1.,0.706796685880017,1.00062084722846)))
REPRESENTATION_ITEM('')
SURFACE()
);
#3717=(
BOUNDED_SURFACE()
B_SPLINE_SURFACE(3,2,((#249348,#249349,#249350),(#249351,#249352,#249353),
(#249354,#249355,#249356),(#249357,#249358,#249359)),.UNSPECIFIED.,.F.,
 .F.,.F.)
B_SPLINE_SURFACE_WITH_KNOTS((4,4),(3,3),(-6.09863722023096E-18,0.000397394465448312),
(0.,1.),.UNSPECIFIED.)
GEOMETRIC_REPRESENTATION_ITEM()
RATIONAL_B_SPLINE_SURFACE(((1.,0.705498956110748,1.),(1.,0.705821764811799,
1.),(1.,0.706461952521121,1.),(1.,0.707106781186555,1.)))
REPRESENTATION_ITEM('')
SURFACE()
);
#3718=(
BOUNDED_SURFACE()
B_SPLINE_SURFACE(3,2,((#249365,#249366,#249367),(#249368,#249369,#249370),
(#249371,#249372,#249373),(#249374,#249375,#249376)),.UNSPECIFIED.,.F.,
 .F.,.F.)
B_SPLINE_SURFACE_WITH_KNOTS((4,4),(3,3),(0.,0.000397394410828749),(0.,1.),
 .UNSPECIFIED.)
GEOMETRIC_REPRESENTATION_ITEM()
RATIONAL_B_SPLINE_SURFACE(((1.,0.708689770883337,1.),(1.,0.708376440034518,
1.),(1.,0.707750498698402,1.),(1.,0.707106781186549,1.)))
REPRESENTATION_ITEM('')
SURFACE()
);
#3719=(
BOUNDED_SURFACE()
B_SPLINE_SURFACE(3,2,((#249382,#249383,#249384),(#249385,#249386,#249387),
(#249388,#249389,#249390),(#249391,#249392,#249393)),.UNSPECIFIED.,.F.,
 .F.,.F.)
B_SPLINE_SURFACE_WITH_KNOTS((4,4),(3,3),(-5.23127548224256E-18,0.000511815090126196),
(0.,1.00105592270209),.UNSPECIFIED.)
GEOMETRIC_REPRESENTATION_ITEM()
RATIONAL_B_SPLINE_SURFACE(((1.,0.705266242717518,1.00062243213078),(1.,
0.705584085909157,1.00062176089509),(1.,0.706182089450553,1.00062049800406),
(1.,0.706797508587506,1.00061919833399)))
REPRESENTATION_ITEM('')
SURFACE()
);
#3720=(
BOUNDED_SURFACE()
B_SPLINE_SURFACE(3,2,((#249395,#249396,#249397),(#249398,#249399,#249400),
(#249401,#249402,#249403),(#249404,#249405,#249406)),.UNSPECIFIED.,.F.,
 .F.,.F.)
B_SPLINE_SURFACE_WITH_KNOTS((4,4),(3,3),(-5.6920614055489E-19,0.000397394428086642),
(0.,1.),.UNSPECIFIED.)
GEOMETRIC_REPRESENTATION_ITEM()
RATIONAL_B_SPLINE_SURFACE(((1.,0.707106781186549,1.),(1.,0.706459846759097,
1.),(1.,0.705820510737282,1.),(1.,0.705498956110751,1.)))
REPRESENTATION_ITEM('')
SURFACE()
);
#3721=(
BOUNDED_SURFACE()
B_SPLINE_SURFACE(3,2,((#249412,#249413,#249414),(#249415,#249416,#249417),
(#249418,#249419,#249420),(#249421,#249422,#249423),(#249424,#249425,#249426),
(#249427,#249428,#249429)),.UNSPECIFIED.,.F.,.F.,.F.)
B_SPLINE_SURFACE_WITH_KNOTS((4,2,4),(3,3),(0.,0.000257953807872837,0.000515907615745674),
(0.,1.),.UNSPECIFIED.)
GEOMETRIC_REPRESENTATION_ITEM()
RATIONAL_B_SPLINE_SURFACE(((1.,0.874619707139396,1.),(1.,0.87483434967922,
1.),(1.,0.854686104157491,1.),(1.,0.792476597915446,1.),(1.,0.750887854594912,
1.),(1.,0.705585838031434,1.)))
REPRESENTATION_ITEM('')
SURFACE()
);
#3722=(
BOUNDED_SURFACE()
B_SPLINE_SURFACE(3,2,((#249435,#249436,#249437),(#249438,#249439,#249440),
(#249441,#249442,#249443),(#249444,#249445,#249446)),.UNSPECIFIED.,.F.,
 .F.,.F.)
B_SPLINE_SURFACE_WITH_KNOTS((4,4),(3,3),(0.,0.00051181543769915),(0.,1.00105881331998),
 .UNSPECIFIED.)
GEOMETRIC_REPRESENTATION_ITEM()
RATIONAL_B_SPLINE_SURFACE(((1.,0.706796661945137,1.00062089519959),(1.,
0.707430821224013,1.00061955228701),(1.,0.708058545829528,1.00061822300066),
(1.,0.708394505251531,1.00061751156404)))
REPRESENTATION_ITEM('')
SURFACE()
);
#3723=(
BOUNDED_SURFACE()
B_SPLINE_SURFACE(3,2,((#249448,#249449,#249450),(#249451,#249452,#249453),
(#249454,#249455,#249456),(#249457,#249458,#249459),(#249460,#249461,#249462),
(#249463,#249464,#249465)),.UNSPECIFIED.,.F.,.F.,.F.)
B_SPLINE_SURFACE_WITH_KNOTS((4,2,4),(3,3),(0.,0.000256915317531263,0.000513830635062527),
(0.,1.),.UNSPECIFIED.)
GEOMETRIC_REPRESENTATION_ITEM()
RATIONAL_B_SPLINE_SURFACE(((1.,0.705585838031439,1.),(1.,0.750902433542964,
1.),(1.,0.792329530082284,1.),(1.,0.854288401594488,1.),(1.,0.874998031124956,
1.),(1.,0.874619707139399,1.)))
REPRESENTATION_ITEM('')
SURFACE()
);
#3724=(
BOUNDED_SURFACE()
B_SPLINE_SURFACE(3,2,((#249471,#249472,#249473),(#249474,#249475,#249476),
(#249477,#249478,#249479),(#249480,#249481,#249482),(#249483,#249484,#249485),
(#249486,#249487,#249488)),.UNSPECIFIED.,.F.,.F.,.F.)
B_SPLINE_SURFACE_WITH_KNOTS((4,2,4),(3,3),(-1.81603863891322E-18,0.000256592814262153,
0.000513185628524309),(0.,1.),.UNSPECIFIED.)
GEOMETRIC_REPRESENTATION_ITEM()
RATIONAL_B_SPLINE_SURFACE(((1.,0.708712527163673,1.),(1.,0.753780902614018,
1.),(1.,0.794538995768624,1.),(1.,0.855070770331673,1.),(1.,0.875018427444898,
1.),(1.,0.8746197071394,1.)))
REPRESENTATION_ITEM('')
SURFACE()
);
#3725=(
BOUNDED_SURFACE()
B_SPLINE_SURFACE(3,2,((#249490,#249491,#249492),(#249493,#249494,#249495),
(#249496,#249497,#249498),(#249499,#249500,#249501)),.UNSPECIFIED.,.F.,
 .F.,.F.)
B_SPLINE_SURFACE_WITH_KNOTS((4,4),(3,3),(-2.71050543121376E-20,0.00051181507243041),
(0.,1.00105598366023),.UNSPECIFIED.)
GEOMETRIC_REPRESENTATION_ITEM()
RATIONAL_B_SPLINE_SURFACE(((1.,0.706797490733287,1.00061923411785),(1.,
0.706182062146206,1.00062053388291),(1.,0.705584062768565,1.00062179683806),
(1.,0.705266224770061,1.00062246810152)))
REPRESENTATION_ITEM('')
SURFACE()
);
#3726=(
BOUNDED_SURFACE()
B_SPLINE_SURFACE(3,2,((#249507,#249508,#249509),(#249510,#249511,#249512),
(#249513,#249514,#249515),(#249516,#249517,#249518),(#249519,#249520,#249521),
(#249522,#249523,#249524)),.UNSPECIFIED.,.F.,.F.,.F.)
B_SPLINE_SURFACE_WITH_KNOTS((4,2,4),(3,3),(-9.5138740635603E-18,0.000257652232350882,
0.000515304464701774),(0.,1.),.UNSPECIFIED.)
GEOMETRIC_REPRESENTATION_ITEM()
RATIONAL_B_SPLINE_SURFACE(((1.,0.874619707139393,1.),(1.,0.87486118043118,
1.),(1.,0.855455725920206,1.),(1.,0.794699358955927,1.),(1.,0.753768977788158,
1.),(1.,0.708712527163641,1.)))
REPRESENTATION_ITEM('')
SURFACE()
);
#3727=(
BOUNDED_SURFACE()
B_SPLINE_SURFACE(3,2,((#249530,#249531,#249532),(#249533,#249534,#249535),
(#249536,#249537,#249538),(#249539,#249540,#249541)),.UNSPECIFIED.,.F.,
 .F.,.F.)
B_SPLINE_SURFACE_WITH_KNOTS((4,4),(3,3),(0.,0.000397394373651898),(0.,1.),
 .UNSPECIFIED.)
GEOMETRIC_REPRESENTATION_ITEM()
RATIONAL_B_SPLINE_SURFACE(((1.,0.707106781186546,1.),(1.,0.707752587915892,
1.),(1.,0.708377654540671,1.),(1.,0.708689770883326,1.)))
REPRESENTATION_ITEM('')
SURFACE()
);
#3728=(
BOUNDED_SURFACE()
B_SPLINE_SURFACE(3,2,((#249543,#249544,#249545),(#249546,#249547,#249548),
(#249549,#249550,#249551),(#249552,#249553,#249554)),.UNSPECIFIED.,.F.,
 .F.,.F.)
B_SPLINE_SURFACE_WITH_KNOTS((4,4),(3,3),(0.,0.000511815456479774),(0.,1.00105873160096),
 .UNSPECIFIED.)
GEOMETRIC_REPRESENTATION_ITEM()
RATIONAL_B_SPLINE_SURFACE(((1.,0.70839452905603,1.0006174638542),(1.,0.708058564166566,
1.00061817524749),(1.,0.707430835371767,1.00061950444012),(1.,0.70679668588009,
1.00062084722833)))
REPRESENTATION_ITEM('')
SURFACE()
);
#3729=(
BOUNDED_SURFACE()
B_SPLINE_SURFACE(3,2,((#249560,#249561,#249562),(#249563,#249564,#249565),
(#249566,#249567,#249568),(#249569,#249570,#249571)),.UNSPECIFIED.,.F.,
 .F.,.F.)
B_SPLINE_SURFACE_WITH_KNOTS((4,4),(3,3),(0.,0.000397394465448298),(0.,1.),
 .UNSPECIFIED.)
GEOMETRIC_REPRESENTATION_ITEM()
RATIONAL_B_SPLINE_SURFACE(((1.,0.705498956110755,1.),(1.,0.705821764811781,
1.),(1.,0.706461952521135,1.),(1.,0.707106781186546,1.)))
REPRESENTATION_ITEM('')
SURFACE()
);
#3730=(
BOUNDED_SURFACE()
B_SPLINE_SURFACE(3,2,((#249577,#249578,#249579),(#249580,#249581,#249582),
(#249583,#249584,#249585),(#249586,#249587,#249588)),.UNSPECIFIED.,.F.,
 .F.,.F.)
B_SPLINE_SURFACE_WITH_KNOTS((4,4),(3,3),(-3.25260651745651E-18,0.000397394410828732),
(0.,1.),.UNSPECIFIED.)
GEOMETRIC_REPRESENTATION_ITEM()
RATIONAL_B_SPLINE_SURFACE(((1.,0.708689770883298,1.),(1.,0.708376440034509,
1.),(1.,0.707750498698393,1.),(1.,0.707106781186555,1.)))
REPRESENTATION_ITEM('')
SURFACE()
);
#3731=(
BOUNDED_SURFACE()
B_SPLINE_SURFACE(3,2,((#249594,#249595,#249596),(#249597,#249598,#249599),
(#249600,#249601,#249602),(#249603,#249604,#249605)),.UNSPECIFIED.,.F.,
 .F.,.F.)
B_SPLINE_SURFACE_WITH_KNOTS((4,4),(3,3),(0.,0.000511815090126188),(0.,1.00105592270402),
 .UNSPECIFIED.)
GEOMETRIC_REPRESENTATION_ITEM()
RATIONAL_B_SPLINE_SURFACE(((1.,0.705266242716956,1.00062243213192),(1.,
0.705584085908583,1.00062176089623),(1.,0.706182089449988,1.0006204980052),
(1.,0.706797508586943,1.00061919833512)))
REPRESENTATION_ITEM('')
SURFACE()
);
#3732=(
BOUNDED_SURFACE()
B_SPLINE_SURFACE(3,2,((#249607,#249608,#249609),(#249610,#249611,#249612),
(#249613,#249614,#249615),(#249616,#249617,#249618)),.UNSPECIFIED.,.F.,
 .F.,.F.)
B_SPLINE_SURFACE_WITH_KNOTS((4,4),(3,3),(0.,0.000397394428086639),(0.,1.),
 .UNSPECIFIED.)
GEOMETRIC_REPRESENTATION_ITEM()
RATIONAL_B_SPLINE_SURFACE(((1.,0.707106781186549,1.),(1.,0.706459846759092,
1.),(1.,0.705820510737292,1.),(1.,0.705498956110755,1.)))
REPRESENTATION_ITEM('')
SURFACE()
);
#3733=(
BOUNDED_SURFACE()
B_SPLINE_SURFACE(3,2,((#249624,#249625,#249626),(#249627,#249628,#249629),
(#249630,#249631,#249632),(#249633,#249634,#249635),(#249636,#249637,#249638),
(#249639,#249640,#249641)),.UNSPECIFIED.,.F.,.F.,.F.)
B_SPLINE_SURFACE_WITH_KNOTS((4,2,4),(3,3),(0.,0.000257953807872845,0.00051590761574569),
(0.,1.),.UNSPECIFIED.)
GEOMETRIC_REPRESENTATION_ITEM()
RATIONAL_B_SPLINE_SURFACE(((1.,0.874619707139393,1.),(1.,0.874834349679431,
1.),(1.,0.85468610415722,1.),(1.,0.792476597915739,1.),(1.,0.750887854594666,
1.),(1.,0.705585838031452,1.)))
REPRESENTATION_ITEM('')
SURFACE()
);
#3734=(
BOUNDED_SURFACE()
B_SPLINE_SURFACE(3,2,((#249647,#249648,#249649),(#249650,#249651,#249652),
(#249653,#249654,#249655),(#249656,#249657,#249658)),.UNSPECIFIED.,.F.,
 .F.,.F.)
B_SPLINE_SURFACE_WITH_KNOTS((4,4),(3,3),(0.,0.000511815437699155),(0.,1.00105881331839),
 .UNSPECIFIED.)
GEOMETRIC_REPRESENTATION_ITEM()
RATIONAL_B_SPLINE_SURFACE(((1.,0.706796661945596,1.00062089519866),(1.,
0.707430821224483,1.00061955228608),(1.,0.708058545829982,1.00061822299973),
(1.,0.708394505251979,1.00061751156311)))
REPRESENTATION_ITEM('')
SURFACE()
);
#3735=(
BOUNDED_SURFACE()
B_SPLINE_SURFACE(3,2,((#249660,#249661,#249662),(#249663,#249664,#249665),
(#249666,#249667,#249668),(#249669,#249670,#249671),(#249672,#249673,#249674),
(#249675,#249676,#249677)),.UNSPECIFIED.,.F.,.F.,.F.)
B_SPLINE_SURFACE_WITH_KNOTS((4,2,4),(3,3),(2.90024081139872E-18,0.00025691531753127,
0.000513830635062537),(0.,1.),.UNSPECIFIED.)
GEOMETRIC_REPRESENTATION_ITEM()
RATIONAL_B_SPLINE_SURFACE(((1.,0.70558583803146,1.),(1.,0.75090243354268,
1.),(1.,0.792329530082599,1.),(1.,0.854288401594135,1.),(1.,0.874998031125191,
1.),(1.,0.874619707139406,1.)))
REPRESENTATION_ITEM('')
SURFACE()
);
#3736=(
BOUNDED_SURFACE()
B_SPLINE_SURFACE(3,2,((#249683,#249684,#249685),(#249686,#249687,#249688),
(#249689,#249690,#249691),(#249692,#249693,#249694),(#249695,#249696,#249697),
(#249698,#249699,#249700)),.UNSPECIFIED.,.F.,.F.,.F.)
B_SPLINE_SURFACE_WITH_KNOTS((4,2,4),(3,3),(-3.95733792957209E-18,0.000256592814262151,
0.000513185628524305),(0.,1.),.UNSPECIFIED.)
GEOMETRIC_REPRESENTATION_ITEM()
RATIONAL_B_SPLINE_SURFACE(((1.,0.708712527163649,1.),(1.,0.753780902613286,
1.),(1.,0.794538995769611,1.),(1.,0.855070770330693,1.),(1.,0.87501842744564,
1.),(1.,0.874619707139394,1.)))
REPRESENTATION_ITEM('')
SURFACE()
);
#3737=(
BOUNDED_SURFACE()
B_SPLINE_SURFACE(3,2,((#249702,#249703,#249704),(#249705,#249706,#249707),
(#249708,#249709,#249710),(#249711,#249712,#249713)),.UNSPECIFIED.,.F.,
 .F.,.F.)
B_SPLINE_SURFACE_WITH_KNOTS((4,4),(3,3),(2.71050543121376E-20,0.000511815072430399),
(0.,1.00105598365803),.UNSPECIFIED.)
GEOMETRIC_REPRESENTATION_ITEM()
RATIONAL_B_SPLINE_SURFACE(((1.,0.706797490733933,1.00061923411655),(1.,
0.70618206214684,1.00062053388162),(1.,0.705584062769212,1.00062179683676),
(1.,0.705266224770693,1.00062246810022)))
REPRESENTATION_ITEM('')
SURFACE()
);
#3738=(
BOUNDED_SURFACE()
B_SPLINE_SURFACE(3,2,((#249719,#249720,#249721),(#249722,#249723,#249724),
(#249725,#249726,#249727),(#249728,#249729,#249730),(#249731,#249732,#249733),
(#249734,#249735,#249736)),.UNSPECIFIED.,.F.,.F.,.F.)
B_SPLINE_SURFACE_WITH_KNOTS((4,2,4),(3,3),(-3.21194893598831E-18,0.000257652232350884,
0.000515304464701772),(0.,1.),.UNSPECIFIED.)
GEOMETRIC_REPRESENTATION_ITEM()
RATIONAL_B_SPLINE_SURFACE(((1.,0.874619707139385,1.),(1.,0.87486118043075,
1.),(1.,0.855455725920803,1.),(1.,0.794699358955335,1.),(1.,0.753768977788572,
1.),(1.,0.708712527163662,1.)))
REPRESENTATION_ITEM('')
SURFACE()
);
#3739=(
BOUNDED_SURFACE()
B_SPLINE_SURFACE(3,2,((#249742,#249743,#249744),(#249745,#249746,#249747),
(#249748,#249749,#249750),(#249751,#249752,#249753)),.UNSPECIFIED.,.F.,
 .F.,.F.)
B_SPLINE_SURFACE_WITH_KNOTS((4,4),(3,3),(5.96311194867027E-19,0.000397394373651915),
(0.,1.),.UNSPECIFIED.)
GEOMETRIC_REPRESENTATION_ITEM()
RATIONAL_B_SPLINE_SURFACE(((1.,0.707106781186546,1.),(1.,0.707752587915887,
1.),(1.,0.708377654540691,1.),(1.,0.708689770883333,1.)))
REPRESENTATION_ITEM('')
SURFACE()
);
#3740=(
BOUNDED_SURFACE()
B_SPLINE_SURFACE(3,2,((#249755,#249756,#249757),(#249758,#249759,#249760),
(#249761,#249762,#249763),(#249764,#249765,#249766)),.UNSPECIFIED.,.F.,
 .F.,.F.)
B_SPLINE_SURFACE_WITH_KNOTS((4,4),(3,3),(-1.59919820441612E-18,0.000511815456479778),
(0.,1.00105873160197),.UNSPECIFIED.)
GEOMETRIC_REPRESENTATION_ITEM()
RATIONAL_B_SPLINE_SURFACE(((1.,0.708394529055743,1.00061746385479),(1.,
0.708058564166312,1.00061817524808),(1.,0.707430835371452,1.00061950444071),
(1.,0.706796685879791,1.00062084722892)))
REPRESENTATION_ITEM('')
SURFACE()
);
#3741=(
BOUNDED_SURFACE()
B_SPLINE_SURFACE(3,2,((#249772,#249773,#249774),(#249775,#249776,#249777),
(#249778,#249779,#249780),(#249781,#249782,#249783)),.UNSPECIFIED.,.F.,
 .F.,.F.)
B_SPLINE_SURFACE_WITH_KNOTS((4,4),(3,3),(3.27971157176865E-18,0.000397394465448314),
(0.,1.),.UNSPECIFIED.)
GEOMETRIC_REPRESENTATION_ITEM()
RATIONAL_B_SPLINE_SURFACE(((1.,0.705498956110724,1.),(1.,0.705821764811811,
1.),(1.,0.706461952521113,1.),(1.,0.70710678118654,1.)))
REPRESENTATION_ITEM('')
SURFACE()
);
#3742=(
BOUNDED_SURFACE()
B_SPLINE_SURFACE(3,2,((#249789,#249790,#249791),(#249792,#249793,#249794),
(#249795,#249796,#249797),(#249798,#249799,#249800)),.UNSPECIFIED.,.F.,
 .F.,.F.)
B_SPLINE_SURFACE_WITH_KNOTS((4,4),(3,3),(0.,0.000397394410828754),(0.,1.),
 .UNSPECIFIED.)
GEOMETRIC_REPRESENTATION_ITEM()
RATIONAL_B_SPLINE_SURFACE(((1.,0.708689770883333,1.),(1.,0.708376440034482,
1.),(1.,0.707750498698425,1.),(1.,0.707106781186548,1.)))
REPRESENTATION_ITEM('')
SURFACE()
);
#3743=(
BOUNDED_SURFACE()
B_SPLINE_SURFACE(3,2,((#249806,#249807,#249808),(#249809,#249810,#249811),
(#249812,#249813,#249814),(#249815,#249816,#249817)),.UNSPECIFIED.,.F.,
 .F.,.F.)
B_SPLINE_SURFACE_WITH_KNOTS((4,4),(3,3),(0.,0.000511815090126182),(0.,1.00105592270073),
 .UNSPECIFIED.)
GEOMETRIC_REPRESENTATION_ITEM()
RATIONAL_B_SPLINE_SURFACE(((1.,0.705266242717918,1.00062243212997),(1.,
0.705584085909569,1.00062176089429),(1.,0.706182089450925,1.00062049800326),
(1.,0.706797508587914,1.00061919833318)))
REPRESENTATION_ITEM('')
SURFACE()
);
#3744=(
BOUNDED_SURFACE()
B_SPLINE_SURFACE(3,2,((#249819,#249820,#249821),(#249822,#249823,#249824),
(#249825,#249826,#249827),(#249828,#249829,#249830)),.UNSPECIFIED.,.F.,
 .F.,.F.)
B_SPLINE_SURFACE_WITH_KNOTS((4,4),(3,3),(-7.26415455565288E-18,0.000397394428086632),
(0.,1.),.UNSPECIFIED.)
GEOMETRIC_REPRESENTATION_ITEM()
RATIONAL_B_SPLINE_SURFACE(((1.,0.707106781186548,1.),(1.,0.706459846759083,
1.),(1.,0.705820510737279,1.),(1.,0.705498956110751,1.)))
REPRESENTATION_ITEM('')
SURFACE()
);
#3745=(
BOUNDED_SURFACE()
B_SPLINE_SURFACE(3,2,((#249836,#249837,#249838),(#249839,#249840,#249841),
(#249842,#249843,#249844),(#249845,#249846,#249847),(#249848,#249849,#249850),
(#249851,#249852,#249853)),.UNSPECIFIED.,.F.,.F.,.F.)
B_SPLINE_SURFACE_WITH_KNOTS((4,2,4),(3,3),(0.,0.00025795380787284,0.00051590761574568),
(0.,1.),.UNSPECIFIED.)
GEOMETRIC_REPRESENTATION_ITEM()
RATIONAL_B_SPLINE_SURFACE(((1.,0.874619707139393,1.),(1.,0.874834349678958,
1.),(1.,0.854686104157849,1.),(1.,0.792476597915072,1.),(1.,0.750887854595184,
1.),(1.,0.705585838031448,1.)))
REPRESENTATION_ITEM('')
SURFACE()
);
#3746=(
BOUNDED_SURFACE()
B_SPLINE_SURFACE(3,2,((#249859,#249860,#249861),(#249862,#249863,#249864),
(#249865,#249866,#249867),(#249868,#249869,#249870)),.UNSPECIFIED.,.F.,
 .F.,.F.)
B_SPLINE_SURFACE_WITH_KNOTS((4,4),(3,3),(5.96311194867027E-19,0.000511815437699145),
(0.,1.00105881331926),.UNSPECIFIED.)
GEOMETRIC_REPRESENTATION_ITEM()
RATIONAL_B_SPLINE_SURFACE(((1.,0.706796661945347,1.00062089519917),(1.,
0.707430821224218,1.00061955228658),(1.,0.708058545829726,1.00061822300024),
(1.,0.708394505251735,1.00061751156362)))
REPRESENTATION_ITEM('')
SURFACE()
);
#3747=(
BOUNDED_SURFACE()
B_SPLINE_SURFACE(3,2,((#249872,#249873,#249874),(#249875,#249876,#249877),
(#249878,#249879,#249880),(#249881,#249882,#249883),(#249884,#249885,#249886),
(#249887,#249888,#249889)),.UNSPECIFIED.,.F.,.F.,.F.)
B_SPLINE_SURFACE_WITH_KNOTS((4,2,4),(3,3),(0.,0.000256915317531259,0.000513830635062518),
(0.,1.),.UNSPECIFIED.)
GEOMETRIC_REPRESENTATION_ITEM()
RATIONAL_B_SPLINE_SURFACE(((1.,0.705585838031445,1.),(1.,0.750902433542064,
1.),(1.,0.792329530083464,1.),(1.,0.854288401593278,1.),(1.,0.874998031125833,
1.),(1.,0.874619707139395,1.)))
REPRESENTATION_ITEM('')
SURFACE()
);
#3748=(
BOUNDED_SURFACE()
B_SPLINE_SURFACE(3,2,((#249895,#249896,#249897),(#249898,#249899,#249900),
(#249901,#249902,#249903),(#249904,#249905,#249906),(#249907,#249908,#249909),
(#249910,#249911,#249912)),.UNSPECIFIED.,.F.,.F.,.F.)
B_SPLINE_SURFACE_WITH_KNOTS((4,2,4),(3,3),(-3.52365706057789E-19,0.000256592814262156,
0.000513185628524312),(0.,1.),.UNSPECIFIED.)
GEOMETRIC_REPRESENTATION_ITEM()
RATIONAL_B_SPLINE_SURFACE(((1.,0.708712527163661,1.),(1.,0.753780902613628,
1.),(1.,0.794538995769124,1.),(1.,0.85507077033118,1.),(1.,0.875018427445262,
1.),(1.,0.874619707139395,1.)))
REPRESENTATION_ITEM('')
SURFACE()
);
#3749=(
BOUNDED_SURFACE()
B_SPLINE_SURFACE(3,2,((#249914,#249915,#249916),(#249917,#249918,#249919),
(#249920,#249921,#249922),(#249923,#249924,#249925)),.UNSPECIFIED.,.F.,
 .F.,.F.)
B_SPLINE_SURFACE_WITH_KNOTS((4,4),(3,3),(-5.42101086242752E-19,0.000511815072430401),
(0.,1.00105598365713),.UNSPECIFIED.)
GEOMETRIC_REPRESENTATION_ITEM()
RATIONAL_B_SPLINE_SURFACE(((1.,0.706797490734198,1.00061923411603),(1.,
0.706182062147102,1.00062053388109),(1.,0.705584062769515,1.00062179683623),
(1.,0.705266224770947,1.00062246809969)))
REPRESENTATION_ITEM('')
SURFACE()
);
#3750=(
BOUNDED_SURFACE()
B_SPLINE_SURFACE(3,2,((#249931,#249932,#249933),(#249934,#249935,#249936),
(#249937,#249938,#249939),(#249940,#249941,#249942),(#249943,#249944,#249945),
(#249946,#249947,#249948)),.UNSPECIFIED.,.F.,.F.,.F.)
B_SPLINE_SURFACE_WITH_KNOTS((4,2,4),(3,3),(-1.35525271560688E-20,0.00025765223235088,
0.00051530446470176),(0.,1.),.UNSPECIFIED.)
GEOMETRIC_REPRESENTATION_ITEM()
RATIONAL_B_SPLINE_SURFACE(((1.,0.874619707139398,1.),(1.,0.874861180431335,
1.),(1.,0.855455725920025,1.),(1.,0.794699358956114,1.),(1.,0.753768977787991,
1.),(1.,0.708712527163669,1.)))
REPRESENTATION_ITEM('')
SURFACE()
);
#3751=(
BOUNDED_SURFACE()
B_SPLINE_SURFACE(3,2,((#249954,#249955,#249956),(#249957,#249958,#249959),
(#249960,#249961,#249962),(#249963,#249964,#249965)),.UNSPECIFIED.,.F.,
 .F.,.F.)
B_SPLINE_SURFACE_WITH_KNOTS((4,4),(3,3),(0.,0.000397394373651909),(0.,1.),
 .UNSPECIFIED.)
GEOMETRIC_REPRESENTATION_ITEM()
RATIONAL_B_SPLINE_SURFACE(((1.,0.707106781186548,1.),(1.,0.707752587915889,
1.),(1.,0.708377654540692,1.),(1.,0.708689770883327,1.)))
REPRESENTATION_ITEM('')
SURFACE()
);
#3752=(
BOUNDED_SURFACE()
B_SPLINE_SURFACE(3,2,((#249967,#249968,#249969),(#249970,#249971,#249972),
(#249973,#249974,#249975),(#249976,#249977,#249978)),.UNSPECIFIED.,.F.,
 .F.,.F.)
B_SPLINE_SURFACE_WITH_KNOTS((4,4),(3,3),(0.,0.000511815456479789),(0.,1.00105873159976),
 .UNSPECIFIED.)
GEOMETRIC_REPRESENTATION_ITEM()
RATIONAL_B_SPLINE_SURFACE(((1.,0.708394529056382,1.0006174638535),(1.,0.708058564166943,
1.00061817524679),(1.,0.707430835372111,1.00061950443941),(1.,0.706796685880434,
1.00062084722763)))
REPRESENTATION_ITEM('')
SURFACE()
);
#3753=(
BOUNDED_SURFACE()
B_SPLINE_SURFACE(3,2,((#249984,#249985,#249986),(#249987,#249988,#249989),
(#249990,#249991,#249992),(#249993,#249994,#249995)),.UNSPECIFIED.,.F.,
 .F.,.F.)
B_SPLINE_SURFACE_WITH_KNOTS((4,4),(3,3),(0.,0.000397394465448301),(0.,1.),
 .UNSPECIFIED.)
GEOMETRIC_REPRESENTATION_ITEM()
RATIONAL_B_SPLINE_SURFACE(((1.,0.705498956110754,1.),(1.,0.705821764811775,
1.),(1.,0.706461952521147,1.),(1.,0.707106781186548,1.)))
REPRESENTATION_ITEM('')
SURFACE()
);
#3754=(
BOUNDED_SURFACE()
B_SPLINE_SURFACE(3,2,((#250001,#250002,#250003),(#250004,#250005,#250006),
(#250007,#250008,#250009),(#250010,#250011,#250012)),.UNSPECIFIED.,.F.,
 .F.,.F.)
B_SPLINE_SURFACE_WITH_KNOTS((4,4),(3,3),(0.,0.000397394410828734),(0.,1.),
 .UNSPECIFIED.)
GEOMETRIC_REPRESENTATION_ITEM()
RATIONAL_B_SPLINE_SURFACE(((1.,0.708689770883327,1.),(1.,0.708376440034502,
1.),(1.,0.707750498698397,1.),(1.,0.707106781186547,1.)))
REPRESENTATION_ITEM('')
SURFACE()
);
#3755=(
BOUNDED_SURFACE()
B_SPLINE_SURFACE(3,2,((#250018,#250019,#250020),(#250021,#250022,#250023),
(#250024,#250025,#250026),(#250027,#250028,#250029)),.UNSPECIFIED.,.F.,
 .F.,.F.)
B_SPLINE_SURFACE_WITH_KNOTS((4,4),(3,3),(0.,0.000511815090126177),(0.,1.00105592270346),
 .UNSPECIFIED.)
GEOMETRIC_REPRESENTATION_ITEM()
RATIONAL_B_SPLINE_SURFACE(((1.,0.705266242717117,1.00062243213158),(1.,
0.705584085908778,1.0006217608959),(1.,0.70618208945012,1.00062049800487),
(1.,0.706797508587112,1.00061919833479)))
REPRESENTATION_ITEM('')
SURFACE()
);
#3756=(
BOUNDED_SURFACE()
B_SPLINE_SURFACE(3,2,((#250031,#250032,#250033),(#250034,#250035,#250036),
(#250037,#250038,#250039),(#250040,#250041,#250042)),.UNSPECIFIED.,.F.,
 .F.,.F.)
B_SPLINE_SURFACE_WITH_KNOTS((4,4),(3,3),(0.,0.000397394428086637),(0.,1.),
 .UNSPECIFIED.)
GEOMETRIC_REPRESENTATION_ITEM()
RATIONAL_B_SPLINE_SURFACE(((1.,0.707106781186545,1.),(1.,0.706459846759095,
1.),(1.,0.705820510737284,1.),(1.,0.705498956110773,1.)))
REPRESENTATION_ITEM('')
SURFACE()
);
#3757=(
BOUNDED_SURFACE()
B_SPLINE_SURFACE(3,2,((#250048,#250049,#250050),(#250051,#250052,#250053),
(#250054,#250055,#250056),(#250057,#250058,#250059),(#250060,#250061,#250062),
(#250063,#250064,#250065)),.UNSPECIFIED.,.F.,.F.,.F.)
B_SPLINE_SURFACE_WITH_KNOTS((4,2,4),(3,3),(-1.35525271560688E-18,0.000257953807872841,
0.000515907615745683),(0.,1.),.UNSPECIFIED.)
GEOMETRIC_REPRESENTATION_ITEM()
RATIONAL_B_SPLINE_SURFACE(((1.,0.874619707139388,1.),(1.,0.874834349678696,
1.),(1.,0.85468610415819,1.),(1.,0.792476597914758,1.),(1.,0.750887854595417,
1.),(1.,0.705585838031446,1.)))
REPRESENTATION_ITEM('')
SURFACE()
);
#3758=(
BOUNDED_SURFACE()
B_SPLINE_SURFACE(3,2,((#250071,#250072,#250073),(#250074,#250075,#250076),
(#250077,#250078,#250079),(#250080,#250081,#250082)),.UNSPECIFIED.,.F.,
 .F.,.F.)
B_SPLINE_SURFACE_WITH_KNOTS((4,4),(3,3),(5.6920614055489E-19,0.000511815437699149),
(0.,1.00105881331655),.UNSPECIFIED.)
GEOMETRIC_REPRESENTATION_ITEM()
RATIONAL_B_SPLINE_SURFACE(((1.,0.706796661946143,1.00062089519758),(1.,
0.707430821225016,1.000619552285),(1.,0.708058545830524,1.00061822299866),
(1.,0.708394505252519,1.00061751156204)))
REPRESENTATION_ITEM('')
SURFACE()
);
#3759=(
BOUNDED_SURFACE()
B_SPLINE_SURFACE(3,2,((#250084,#250085,#250086),(#250087,#250088,#250089),
(#250090,#250091,#250092),(#250093,#250094,#250095),(#250096,#250097,#250098),
(#250099,#250100,#250101)),.UNSPECIFIED.,.F.,.F.,.F.)
B_SPLINE_SURFACE_WITH_KNOTS((4,2,4),(3,3),(2.71050543121376E-20,0.00025691531753127,
0.00051383063506254),(0.,1.),.UNSPECIFIED.)
GEOMETRIC_REPRESENTATION_ITEM()
RATIONAL_B_SPLINE_SURFACE(((1.,0.705585838031444,1.),(1.,0.750902433542877,
1.),(1.,0.792329530082359,1.),(1.,0.854288401594373,1.),(1.,0.87499803112502,
1.),(1.,0.874619707139415,1.)))
REPRESENTATION_ITEM('')
SURFACE()
);
#3760=(
BOUNDED_SURFACE()
B_SPLINE_SURFACE(3,2,((#250107,#250108,#250109),(#250110,#250111,#250112),
(#250113,#250114,#250115),(#250116,#250117,#250118),(#250119,#250120,#250121),
(#250122,#250123,#250124)),.UNSPECIFIED.,.F.,.F.,.F.)
B_SPLINE_SURFACE_WITH_KNOTS((4,2,4),(3,3),(-1.00017650411788E-17,0.000256592814262149,
0.000513185628524308),(0.,1.),.UNSPECIFIED.)
GEOMETRIC_REPRESENTATION_ITEM()
RATIONAL_B_SPLINE_SURFACE(((1.,0.708712527163658,1.),(1.,0.753780902613446,
1.),(1.,0.794538995769375,1.),(1.,0.855070770330916,1.),(1.,0.875018427445467,
1.),(1.,0.874619707139404,1.)))
REPRESENTATION_ITEM('')
SURFACE()
);
#3761=(
BOUNDED_SURFACE()
B_SPLINE_SURFACE(3,2,((#250126,#250127,#250128),(#250129,#250130,#250131),
(#250132,#250133,#250134),(#250135,#250136,#250137)),.UNSPECIFIED.,.F.,
 .F.,.F.)
B_SPLINE_SURFACE_WITH_KNOTS((4,4),(3,3),(-5.96311194867027E-19,0.000511815072430398),
(0.,1.00105598365647),.UNSPECIFIED.)
GEOMETRIC_REPRESENTATION_ITEM()
RATIONAL_B_SPLINE_SURFACE(((1.,0.706797490734389,1.00061923411564),(1.,
0.706182062147284,1.0006205338807),(1.,0.705584062769693,1.00062179683584),
(1.,0.705266224771152,1.0006224680993)))
REPRESENTATION_ITEM('')
SURFACE()
);
#3762=(
BOUNDED_SURFACE()
B_SPLINE_SURFACE(3,2,((#250143,#250144,#250145),(#250146,#250147,#250148),
(#250149,#250150,#250151),(#250152,#250153,#250154),(#250155,#250156,#250157),
(#250158,#250159,#250160)),.UNSPECIFIED.,.F.,.F.,.F.)
B_SPLINE_SURFACE_WITH_KNOTS((4,2,4),(3,3),(-8.53809210832335E-19,0.000257652232350881,
0.000515304464701762),(0.,1.),.UNSPECIFIED.)
GEOMETRIC_REPRESENTATION_ITEM()
RATIONAL_B_SPLINE_SURFACE(((1.,0.874619707139382,1.),(1.,0.874861180431399,
1.),(1.,0.85545572591994,1.),(1.,0.794699358956173,1.),(1.,0.753768977787953,
1.),(1.,0.708712527163656,1.)))
REPRESENTATION_ITEM('')
SURFACE()
);
#3763=(
BOUNDED_SURFACE()
B_SPLINE_SURFACE(3,2,((#250166,#250167,#250168),(#250169,#250170,#250171),
(#250172,#250173,#250174),(#250175,#250176,#250177)),.UNSPECIFIED.,.F.,
 .F.,.F.)
B_SPLINE_SURFACE_WITH_KNOTS((4,4),(3,3),(0.,0.000397394373651905),(0.,1.),
 .UNSPECIFIED.)
GEOMETRIC_REPRESENTATION_ITEM()
RATIONAL_B_SPLINE_SURFACE(((1.,0.707106781186545,1.),(1.,0.707752587915898,
1.),(1.,0.708377654540682,1.),(1.,0.70868977088332,1.)))
REPRESENTATION_ITEM('')
SURFACE()
);
#3764=(
BOUNDED_SURFACE()
B_SPLINE_SURFACE(3,2,((#250179,#250180,#250181),(#250182,#250183,#250184),
(#250185,#250186,#250187),(#250188,#250189,#250190)),.UNSPECIFIED.,.F.,
 .F.,.F.)
B_SPLINE_SURFACE_WITH_KNOTS((4,4),(3,3),(0.,0.00051181545647979),(0.,1.00105873159952),
 .UNSPECIFIED.)
GEOMETRIC_REPRESENTATION_ITEM()
RATIONAL_B_SPLINE_SURFACE(((1.,0.708394529056458,1.00061746385336),(1.,
0.708058564167018,1.00061817524665),(1.,0.707430835372176,1.00061950443927),
(1.,0.706796685880504,1.00062084722749)))
REPRESENTATION_ITEM('')
SURFACE()
);
#3765=(
BOUNDED_SURFACE()
B_SPLINE_SURFACE(3,2,((#250196,#250197,#250198),(#250199,#250200,#250201),
(#250202,#250203,#250204),(#250205,#250206,#250207)),.UNSPECIFIED.,.F.,
 .F.,.F.)
B_SPLINE_SURFACE_WITH_KNOTS((4,4),(3,3),(-5.6920614055489E-18,0.000397394465448292),
(0.,1.),.UNSPECIFIED.)
GEOMETRIC_REPRESENTATION_ITEM()
RATIONAL_B_SPLINE_SURFACE(((1.,0.705498956110746,1.),(1.,0.70582176481177,
1.),(1.,0.706461952521135,1.),(1.,0.70710678118655,1.)))
REPRESENTATION_ITEM('')
SURFACE()
);
#3766=(
BOUNDED_SURFACE()
B_SPLINE_SURFACE(3,2,((#250213,#250214,#250215),(#250216,#250217,#250218),
(#250219,#250220,#250221),(#250222,#250223,#250224)),.UNSPECIFIED.,.F.,
 .F.,.F.)
B_SPLINE_SURFACE_WITH_KNOTS((4,4),(3,3),(0.,0.000397394410828736),(0.,1.),
 .UNSPECIFIED.)
GEOMETRIC_REPRESENTATION_ITEM()
RATIONAL_B_SPLINE_SURFACE(((1.,0.708689770883334,1.),(1.,0.708376440034502,
1.),(1.,0.707750498698403,1.),(1.,0.707106781186548,1.)))
REPRESENTATION_ITEM('')
SURFACE()
);
#3767=(
BOUNDED_SURFACE()
B_SPLINE_SURFACE(3,2,((#250230,#250231,#250232),(#250233,#250234,#250235),
(#250236,#250237,#250238),(#250239,#250240,#250241)),.UNSPECIFIED.,.F.,
 .F.,.F.)
B_SPLINE_SURFACE_WITH_KNOTS((4,4),(3,3),(0.,0.000511815090126177),(0.,1.00105592270128),
 .UNSPECIFIED.)
GEOMETRIC_REPRESENTATION_ITEM()
RATIONAL_B_SPLINE_SURFACE(((1.,0.70526624271777,1.00062243213029),(1.,0.705584085909375,
1.00062176089461),(1.,0.706182089450778,1.00062049800358),(1.,0.706797508587752,
1.00061919833351)))
REPRESENTATION_ITEM('')
SURFACE()
);
#3768=(
BOUNDED_SURFACE()
B_SPLINE_SURFACE(3,2,((#250243,#250244,#250245),(#250246,#250247,#250248),
(#250249,#250250,#250251),(#250252,#250253,#250254)),.UNSPECIFIED.,.F.,
 .F.,.F.)
B_SPLINE_SURFACE_WITH_KNOTS((4,4),(3,3),(0.,0.000397394428086634),(0.,1.),
 .UNSPECIFIED.)
GEOMETRIC_REPRESENTATION_ITEM()
RATIONAL_B_SPLINE_SURFACE(((1.,0.707106781186548,1.),(1.,0.706459846759077,
1.),(1.,0.705820510737296,1.),(1.,0.705498956110732,1.)))
REPRESENTATION_ITEM('')
SURFACE()
);
#3769=(
BOUNDED_SURFACE()
B_SPLINE_SURFACE(3,2,((#250260,#250261,#250262),(#250263,#250264,#250265),
(#250266,#250267,#250268),(#250269,#250270,#250271),(#250272,#250273,#250274),
(#250275,#250276,#250277)),.UNSPECIFIED.,.F.,.F.,.F.)
B_SPLINE_SURFACE_WITH_KNOTS((4,2,4),(3,3),(0.,0.000257953807872852,0.000515907615745705),
(0.,1.),.UNSPECIFIED.)
GEOMETRIC_REPRESENTATION_ITEM()
RATIONAL_B_SPLINE_SURFACE(((1.,0.874619707139393,1.),(1.,0.874834349679286,
1.),(1.,0.854686104157385,1.),(1.,0.792476597915547,1.),(1.,0.750887854594819,
1.),(1.,0.705585838031429,1.)))
REPRESENTATION_ITEM('')
SURFACE()
);
#3770=(
BOUNDED_SURFACE()
B_SPLINE_SURFACE(3,2,((#250280,#250281,#250282),(#250283,#250284,#250285),
(#250286,#250287,#250288),(#250289,#250290,#250291)),.UNSPECIFIED.,.F.,
 .F.,.F.)
B_SPLINE_SURFACE_WITH_KNOTS((4,4),(3,3),(0.,0.000511815437699153),(0.,1.00105881331696),
 .UNSPECIFIED.)
GEOMETRIC_REPRESENTATION_ITEM()
RATIONAL_B_SPLINE_SURFACE(((1.,0.706796661946019,1.00062089519782),(1.,
0.70743082122491,1.00061955228524),(1.,0.708058545830392,1.0006182229989),
(1.,0.708394505252405,1.00061751156228)))
REPRESENTATION_ITEM('')
SURFACE()
);
#3771=(
BOUNDED_SURFACE()
B_SPLINE_SURFACE(3,2,((#250293,#250294,#250295),(#250296,#250297,#250298),
(#250299,#250300,#250301),(#250302,#250303,#250304),(#250305,#250306,#250307),
(#250308,#250309,#250310)),.UNSPECIFIED.,.F.,.F.,.F.)
B_SPLINE_SURFACE_WITH_KNOTS((4,2,4),(3,3),(0.,0.000256915317531262,0.000513830635062524),
(0.,1.),.UNSPECIFIED.)
GEOMETRIC_REPRESENTATION_ITEM()
RATIONAL_B_SPLINE_SURFACE(((1.,0.705585838031438,1.),(1.,0.750902433542942,
1.),(1.,0.792329530082252,1.),(1.,0.854288401594462,1.),(1.,0.874998031124935,
1.),(1.,0.874619707139393,1.)))
REPRESENTATION_ITEM('')
SURFACE()
);
#3772=(
BOUNDED_SURFACE()
B_SPLINE_SURFACE(3,2,((#250316,#250317,#250318),(#250319,#250320,#250321),
(#250322,#250323,#250324),(#250325,#250326,#250327),(#250328,#250329,#250330),
(#250331,#250332,#250333)),.UNSPECIFIED.,.F.,.F.,.F.)
B_SPLINE_SURFACE_WITH_KNOTS((4,2,4),(3,3),(-1.0435445910173E-17,0.000256592814262151,
0.000513185628524312),(0.,1.),.UNSPECIFIED.)
GEOMETRIC_REPRESENTATION_ITEM()
RATIONAL_B_SPLINE_SURFACE(((1.,0.708712527163666,1.),(1.,0.753780902613587,
1.),(1.,0.794538995769213,1.),(1.,0.855070770331108,1.),(1.,0.87501842744534,
1.),(1.,0.874619707139389,1.)))
REPRESENTATION_ITEM('')
SURFACE()
);
#3773=(
BOUNDED_SURFACE()
B_SPLINE_SURFACE(3,2,((#250334,#250335,#250336),(#250337,#250338,#250339),
(#250340,#250341,#250342),(#250343,#250344,#250345)),.UNSPECIFIED.,.F.,
 .F.,.F.)
B_SPLINE_SURFACE_WITH_KNOTS((4,4),(3,3),(-5.96311194867027E-19,0.000511815072430392),
(0.,1.00105598365949),.UNSPECIFIED.)
GEOMETRIC_REPRESENTATION_ITEM()
RATIONAL_B_SPLINE_SURFACE(((1.,0.706797490733506,1.00061923411741),(1.,
0.706182062146417,1.00062053388248),(1.,0.705584062768799,1.00062179683762),
(1.,0.705266224770268,1.00062246810108)))
REPRESENTATION_ITEM('')
SURFACE()
);
#3774=(
BOUNDED_SURFACE()
B_SPLINE_SURFACE(3,2,((#250349,#250350,#250351),(#250352,#250353,#250354),
(#250355,#250356,#250357),(#250358,#250359,#250360),(#250361,#250362,#250363),
(#250364,#250365,#250366)),.UNSPECIFIED.,.F.,.F.,.F.)
B_SPLINE_SURFACE_WITH_KNOTS((4,2,4),(3,3),(-6.36968776335234E-19,0.000257652232350878,
0.000515304464701756),(0.,1.),.UNSPECIFIED.)
GEOMETRIC_REPRESENTATION_ITEM()
RATIONAL_B_SPLINE_SURFACE(((1.,0.874619707139395,1.),(1.,0.874861180430727,
1.),(1.,0.855455725920841,1.),(1.,0.794699358955299,1.),(1.,0.753768977788615,
1.),(1.,0.708712527163659,1.)))
REPRESENTATION_ITEM('')
SURFACE()
);
#3775=(
BOUNDED_SURFACE()
B_SPLINE_SURFACE(3,2,((#250372,#250373,#250374),(#250375,#250376,#250377),
(#250378,#250379,#250380),(#250381,#250382,#250383)),.UNSPECIFIED.,.F.,
 .F.,.F.)
B_SPLINE_SURFACE_WITH_KNOTS((4,4),(3,3),(0.,0.000397394373651911),(0.,1.),
 .UNSPECIFIED.)
GEOMETRIC_REPRESENTATION_ITEM()
RATIONAL_B_SPLINE_SURFACE(((1.,0.707106781186548,1.),(1.,0.707752587915892,
1.),(1.,0.708377654540693,1.),(1.,0.708689770883328,1.)))
REPRESENTATION_ITEM('')
SURFACE()
);
#3776=(
BOUNDED_SURFACE()
B_SPLINE_SURFACE(3,2,((#250385,#250386,#250387),(#250388,#250389,#250390),
(#250391,#250392,#250393),(#250394,#250395,#250396)),.UNSPECIFIED.,.F.,
 .F.,.F.)
B_SPLINE_SURFACE_WITH_KNOTS((4,4),(3,3),(-5.61074624261249E-18,0.00051181545647978),
(0.,1.00105873160076),.UNSPECIFIED.)
GEOMETRIC_REPRESENTATION_ITEM()
RATIONAL_B_SPLINE_SURFACE(((1.,0.708394529056089,1.00061746385409),(1.,
0.70805856416664,1.00061817524738),(1.,0.70743083537182,1.00061950444),
(1.,0.70679668588014,1.00062084722821)))
REPRESENTATION_ITEM('')
SURFACE()
);
#3777=(
BOUNDED_SURFACE()
B_SPLINE_SURFACE(3,2,((#250402,#250403,#250404),(#250405,#250406,#250407),
(#250408,#250409,#250410),(#250411,#250412,#250413)),.UNSPECIFIED.,.F.,
 .F.,.F.)
B_SPLINE_SURFACE_WITH_KNOTS((4,4),(3,3),(-2.03287907341032E-18,0.000397394465448296),
(0.,1.),.UNSPECIFIED.)
GEOMETRIC_REPRESENTATION_ITEM()
RATIONAL_B_SPLINE_SURFACE(((1.,0.705498956110755,1.),(1.,0.70582176481177,
1.),(1.,0.706461952521151,1.),(1.,0.707106781186548,1.)))
REPRESENTATION_ITEM('')
SURFACE()
);
#3778=(
BOUNDED_SURFACE()
B_SPLINE_SURFACE(3,2,((#250419,#250420,#250421),(#250422,#250423,#250424),
(#250425,#250426,#250427),(#250428,#250429,#250430)),.UNSPECIFIED.,.F.,
 .F.,.F.)
B_SPLINE_SURFACE_WITH_KNOTS((4,4),(3,3),(0.,0.000397394410828736),(0.,1.),
 .UNSPECIFIED.)
GEOMETRIC_REPRESENTATION_ITEM()
RATIONAL_B_SPLINE_SURFACE(((1.,0.708689770883325,1.),(1.,0.708376440034479,
1.),(1.,0.707750498698413,1.),(1.,0.707106781186545,1.)))
REPRESENTATION_ITEM('')
SURFACE()
);
#3779=(
BOUNDED_SURFACE()
B_SPLINE_SURFACE(3,2,((#250436,#250437,#250438),(#250439,#250440,#250441),
(#250442,#250443,#250444),(#250445,#250446,#250447)),.UNSPECIFIED.,.F.,
 .F.,.F.)
B_SPLINE_SURFACE_WITH_KNOTS((4,4),(3,3),(0.,0.000511815090126176),(0.,1.00105592270094),
 .UNSPECIFIED.)
GEOMETRIC_REPRESENTATION_ITEM()
RATIONAL_B_SPLINE_SURFACE(((1.,0.705266242717862,1.00062243213009),(1.,
0.705584085909489,1.00062176089441),(1.,0.706182089450879,1.00062049800338),
(1.,0.706797508587852,1.00061919833331)))
REPRESENTATION_ITEM('')
SURFACE()
);
#3780=(
BOUNDED_SURFACE()
B_SPLINE_SURFACE(3,2,((#250449,#250450,#250451),(#250452,#250453,#250454),
(#250455,#250456,#250457),(#250458,#250459,#250460)),.UNSPECIFIED.,.F.,
 .F.,.F.)
B_SPLINE_SURFACE_WITH_KNOTS((4,4),(3,3),(-7.12862928409219E-18,0.000397394428086624),
(0.,1.),.UNSPECIFIED.)
GEOMETRIC_REPRESENTATION_ITEM()
RATIONAL_B_SPLINE_SURFACE(((1.,0.707106781186548,1.),(1.,0.7064598467591,
1.),(1.,0.705820510737274,1.),(1.,0.705498956110758,1.)))
REPRESENTATION_ITEM('')
SURFACE()
);
#3781=(
BOUNDED_SURFACE()
B_SPLINE_SURFACE(3,2,((#250466,#250467,#250468),(#250469,#250470,#250471),
(#250472,#250473,#250474),(#250475,#250476,#250477),(#250478,#250479,#250480),
(#250481,#250482,#250483)),.UNSPECIFIED.,.F.,.F.,.F.)
B_SPLINE_SURFACE_WITH_KNOTS((4,2,4),(3,3),(-8.53809210832335E-19,0.000257953807872848,
0.000515907615745697),(0.,1.),.UNSPECIFIED.)
GEOMETRIC_REPRESENTATION_ITEM()
RATIONAL_B_SPLINE_SURFACE(((1.,0.874619707139389,1.),(1.,0.874834349679475,
1.),(1.,0.854686104157152,1.),(1.,0.792476597915786,1.),(1.,0.750887854594648,
1.),(1.,0.705585838031442,1.)))
REPRESENTATION_ITEM('')
SURFACE()
);
#3782=(
BOUNDED_SURFACE()
B_SPLINE_SURFACE(3,2,((#250489,#250490,#250491),(#250492,#250493,#250494),
(#250495,#250496,#250497),(#250498,#250499,#250500)),.UNSPECIFIED.,.F.,
 .F.,.F.)
B_SPLINE_SURFACE_WITH_KNOTS((4,4),(3,3),(5.96311194867027E-19,0.00051181543769915),
(0.,1.00105881331694),.UNSPECIFIED.)
GEOMETRIC_REPRESENTATION_ITEM()
RATIONAL_B_SPLINE_SURFACE(((1.,0.70679666194603,1.0006208951978),(1.,0.707430821224897,
1.00061955228523),(1.,0.708058545830418,1.00061822299888),(1.,0.708394505252403,
1.00061751156226)))
REPRESENTATION_ITEM('')
SURFACE()
);
#3783=(
BOUNDED_SURFACE()
B_SPLINE_SURFACE(3,2,((#250502,#250503,#250504),(#250505,#250506,#250507),
(#250508,#250509,#250510),(#250511,#250512,#250513),(#250514,#250515,#250516),
(#250517,#250518,#250519)),.UNSPECIFIED.,.F.,.F.,.F.)
B_SPLINE_SURFACE_WITH_KNOTS((4,2,4),(3,3),(0.,0.000256915317531264,0.000513830635062528),
(0.,1.),.UNSPECIFIED.)
GEOMETRIC_REPRESENTATION_ITEM()
RATIONAL_B_SPLINE_SURFACE(((1.,0.705585838031432,1.),(1.,0.750902433542905,
1.),(1.,0.792329530082297,1.),(1.,0.854288401594434,1.),(1.,0.874998031124962,
1.),(1.,0.874619707139388,1.)))
REPRESENTATION_ITEM('')
SURFACE()
);
#3784=(
BOUNDED_SURFACE()
B_SPLINE_SURFACE(3,2,((#250525,#250526,#250527),(#250528,#250529,#250530),
(#250531,#250532,#250533),(#250534,#250535,#250536),(#250537,#250538,#250539),
(#250540,#250541,#250542)),.UNSPECIFIED.,.F.,.F.,.F.)
B_SPLINE_SURFACE_WITH_KNOTS((4,2,4),(3,3),(-2.62919026827735E-18,0.000256592814262154,
0.000513185628524311),(0.,1.),.UNSPECIFIED.)
GEOMETRIC_REPRESENTATION_ITEM()
RATIONAL_B_SPLINE_SURFACE(((1.,0.708712527163643,1.),(1.,0.753780902613486,
1.),(1.,0.79453899576934,1.),(1.,0.855070770330976,1.),(1.,0.875018427445422,
1.),(1.,0.874619707139395,1.)))
REPRESENTATION_ITEM('')
SURFACE()
);
#3785=(
BOUNDED_SURFACE()
B_SPLINE_SURFACE(3,2,((#250544,#250545,#250546),(#250547,#250548,#250549),
(#250550,#250551,#250552),(#250553,#250554,#250555)),.UNSPECIFIED.,.F.,
 .F.,.F.)
B_SPLINE_SURFACE_WITH_KNOTS((4,4),(3,3),(-5.42101086242752E-19,0.000511815072430395),
(0.,1.00105598365927),.UNSPECIFIED.)
GEOMETRIC_REPRESENTATION_ITEM()
RATIONAL_B_SPLINE_SURFACE(((1.,0.706797490733568,1.00061923411729),(1.,
0.706182062146479,1.00062053388235),(1.,0.705584062768855,1.00062179683749),
(1.,0.705266224770321,1.00062246810096)))
REPRESENTATION_ITEM('')
SURFACE()
);
#3786=(
BOUNDED_SURFACE()
B_SPLINE_SURFACE(3,2,((#250561,#250562,#250563),(#250564,#250565,#250566),
(#250567,#250568,#250569),(#250570,#250571,#250572),(#250573,#250574,#250575),
(#250576,#250577,#250578)),.UNSPECIFIED.,.F.,.F.,.F.)
B_SPLINE_SURFACE_WITH_KNOTS((4,2,4),(3,3),(1.35525271560688E-20,0.000257652232350878,
0.000515304464701755),(0.,1.),.UNSPECIFIED.)
GEOMETRIC_REPRESENTATION_ITEM()
RATIONAL_B_SPLINE_SURFACE(((1.,0.874619707139397,1.),(1.,0.874861180430768,
1.),(1.,0.855455725920795,1.),(1.,0.794699358955348,1.),(1.,0.753768977788566,
1.),(1.,0.708712527163672,1.)))
REPRESENTATION_ITEM('')
SURFACE()
);
#3787=(
BOUNDED_SURFACE()
B_SPLINE_SURFACE(3,2,((#250584,#250585,#250586),(#250587,#250588,#250589),
(#250590,#250591,#250592),(#250593,#250594,#250595)),.UNSPECIFIED.,.F.,
 .F.,.F.)
B_SPLINE_SURFACE_WITH_KNOTS((4,4),(3,3),(0.,0.000397394373651909),(0.,1.),
 .UNSPECIFIED.)
GEOMETRIC_REPRESENTATION_ITEM()
RATIONAL_B_SPLINE_SURFACE(((1.,0.707106781186548,1.),(1.,0.707752587915876,
1.),(1.,0.708377654540709,1.),(1.,0.708689770883337,1.)))
REPRESENTATION_ITEM('')
SURFACE()
);
#3788=(
BOUNDED_SURFACE()
B_SPLINE_SURFACE(3,2,((#250597,#250598,#250599),(#250600,#250601,#250602),
(#250603,#250604,#250605),(#250606,#250607,#250608)),.UNSPECIFIED.,.F.,
 .F.,.F.)
B_SPLINE_SURFACE_WITH_KNOTS((4,4),(3,3),(0.,0.000511815456479791),(0.,1.00105873160053),
 .UNSPECIFIED.)
GEOMETRIC_REPRESENTATION_ITEM()
RATIONAL_B_SPLINE_SURFACE(((1.,0.708394529056164,1.00061746385395),(1.,
0.708058564166729,1.00061817524724),(1.,0.707430835371884,1.00061950443987),
(1.,0.706796685880206,1.00062084722808)))
REPRESENTATION_ITEM('')
SURFACE()
);
#3789=(
BOUNDED_SURFACE()
B_SPLINE_SURFACE(3,2,((#250614,#250615,#250616),(#250617,#250618,#250619),
(#250620,#250621,#250622),(#250623,#250624,#250625)),.UNSPECIFIED.,.F.,
 .F.,.F.)
B_SPLINE_SURFACE_WITH_KNOTS((4,4),(3,3),(-7.72494047895922E-18,0.000397394465448296),
(0.,1.),.UNSPECIFIED.)
GEOMETRIC_REPRESENTATION_ITEM()
RATIONAL_B_SPLINE_SURFACE(((1.,0.705498956110744,1.),(1.,0.705821764811781,
1.),(1.,0.706461952521132,1.),(1.,0.707106781186548,1.)))
REPRESENTATION_ITEM('')
SURFACE()
);
#3790=(
BOUNDED_SURFACE()
B_SPLINE_SURFACE(3,2,((#250631,#250632,#250633),(#250634,#250635,#250636),
(#250637,#250638,#250639),(#250640,#250641,#250642)),.UNSPECIFIED.,.F.,
 .F.,.F.)
B_SPLINE_SURFACE_WITH_KNOTS((4,4),(3,3),(0.,0.000397394410828758),(0.,1.),
 .UNSPECIFIED.)
GEOMETRIC_REPRESENTATION_ITEM()
RATIONAL_B_SPLINE_SURFACE(((1.,0.708689770883337,1.),(1.,0.708376440034474,
1.),(1.,0.707750498698435,1.),(1.,0.707106781186543,1.)))
REPRESENTATION_ITEM('')
SURFACE()
);
#3791=(
BOUNDED_SURFACE()
B_SPLINE_SURFACE(3,2,((#250648,#250649,#250650),(#250651,#250652,#250653),
(#250654,#250655,#250656),(#250657,#250658,#250659)),.UNSPECIFIED.,.F.,
 .F.,.F.)
B_SPLINE_SURFACE_WITH_KNOTS((4,4),(3,3),(0.,0.000511815090126189),(0.,1.0010559227023),
 .UNSPECIFIED.)
GEOMETRIC_REPRESENTATION_ITEM()
RATIONAL_B_SPLINE_SURFACE(((1.,0.705266242717454,1.0006224321309),(1.,0.705584085909081,
1.00062176089521),(1.,0.706182089450486,1.00062049800418),(1.,0.706797508587448,
1.00061919833411)))
REPRESENTATION_ITEM('')
SURFACE()
);
#3792=(
BOUNDED_SURFACE()
B_SPLINE_SURFACE(3,2,((#250661,#250662,#250663),(#250664,#250665,#250666),
(#250667,#250668,#250669),(#250670,#250671,#250672)),.UNSPECIFIED.,.F.,
 .F.,.F.)
B_SPLINE_SURFACE_WITH_KNOTS((4,4),(3,3),(0.,0.000397394428086637),(0.,1.),
 .UNSPECIFIED.)
GEOMETRIC_REPRESENTATION_ITEM()
RATIONAL_B_SPLINE_SURFACE(((1.,0.707106781186548,1.),(1.,0.706459846759098,
1.),(1.,0.705820510737255,1.),(1.,0.705498956110766,1.)))
REPRESENTATION_ITEM('')
SURFACE()
);
#3793=(
BOUNDED_SURFACE()
B_SPLINE_SURFACE(3,2,((#250678,#250679,#250680),(#250681,#250682,#250683),
(#250684,#250685,#250686),(#250687,#250688,#250689),(#250690,#250691,#250692),
(#250693,#250694,#250695)),.UNSPECIFIED.,.F.,.F.,.F.)
B_SPLINE_SURFACE_WITH_KNOTS((4,2,4),(3,3),(0.,0.000257953807872852,0.000515907615745703),
(0.,1.),.UNSPECIFIED.)
GEOMETRIC_REPRESENTATION_ITEM()
RATIONAL_B_SPLINE_SURFACE(((1.,0.874619707139395,1.),(1.,0.874834349679212,
1.),(1.,0.854686104157491,1.),(1.,0.792476597915442,1.),(1.,0.750887854594872,
1.),(1.,0.705585838031449,1.)))
REPRESENTATION_ITEM('')
SURFACE()
);
#3794=(
BOUNDED_SURFACE()
B_SPLINE_SURFACE(3,2,((#250701,#250702,#250703),(#250704,#250705,#250706),
(#250707,#250708,#250709),(#250710,#250711,#250712)),.UNSPECIFIED.,.F.,
 .F.,.F.)
B_SPLINE_SURFACE_WITH_KNOTS((4,4),(3,3),(0.,0.00051181543769915),(0.,1.00105881331692),
 .UNSPECIFIED.)
GEOMETRIC_REPRESENTATION_ITEM()
RATIONAL_B_SPLINE_SURFACE(((1.,0.706796661946038,1.00062089519779),(1.,
0.707430821224895,1.00061955228521),(1.,0.708058545830441,1.00061822299887),
(1.,0.708394505252425,1.00061751156225)))
REPRESENTATION_ITEM('')
SURFACE()
);
#3795=(
BOUNDED_SURFACE()
B_SPLINE_SURFACE(3,2,((#250714,#250715,#250716),(#250717,#250718,#250719),
(#250720,#250721,#250722),(#250723,#250724,#250725),(#250726,#250727,#250728),
(#250729,#250730,#250731)),.UNSPECIFIED.,.F.,.F.,.F.)
B_SPLINE_SURFACE_WITH_KNOTS((4,2,4),(3,3),(0.,0.000256915317531259,0.000513830635062518),
(0.,1.),.UNSPECIFIED.)
GEOMETRIC_REPRESENTATION_ITEM()
RATIONAL_B_SPLINE_SURFACE(((1.,0.705585838031427,1.),(1.,0.750902433542276,
1.),(1.,0.792329530083153,1.),(1.,0.85428840159355,1.),(1.,0.874998031125595,
1.),(1.,0.874619707139398,1.)))
REPRESENTATION_ITEM('')
SURFACE()
);
#3796=(
BOUNDED_SURFACE()
B_SPLINE_SURFACE(3,2,((#250737,#250738,#250739),(#250740,#250741,#250742),
(#250743,#250744,#250745),(#250746,#250747,#250748),(#250749,#250750,#250751),
(#250752,#250753,#250754)),.UNSPECIFIED.,.F.,.F.,.F.)
B_SPLINE_SURFACE_WITH_KNOTS((4,2,4),(3,3),(0.,0.000256592814262156,0.000513185628524313),
(0.,1.),.UNSPECIFIED.)
GEOMETRIC_REPRESENTATION_ITEM()
RATIONAL_B_SPLINE_SURFACE(((1.,0.708712527163666,1.),(1.,0.753780902613626,
1.),(1.,0.794538995769145,1.),(1.,0.855070770331172,1.),(1.,0.875018427445286,
1.),(1.,0.874619707139399,1.)))
REPRESENTATION_ITEM('')
SURFACE()
);
#3797=(
BOUNDED_SURFACE()
B_SPLINE_SURFACE(3,2,((#250756,#250757,#250758),(#250759,#250760,#250761),
(#250762,#250763,#250764),(#250765,#250766,#250767)),.UNSPECIFIED.,.F.,
 .F.,.F.)
B_SPLINE_SURFACE_WITH_KNOTS((4,4),(3,3),(-5.42101086242752E-19,0.000511815072430406),
(0.,1.00105598365709),.UNSPECIFIED.)
GEOMETRIC_REPRESENTATION_ITEM()
RATIONAL_B_SPLINE_SURFACE(((1.,0.706797490734208,1.000619234116),(1.,0.706182062147114,
1.00062053388107),(1.,0.705584062769522,1.0006217968362),(1.,0.705266224770962,
1.00062246809967)))
REPRESENTATION_ITEM('')
SURFACE()
);
#3798=(
BOUNDED_SURFACE()
B_SPLINE_SURFACE(3,2,((#250773,#250774,#250775),(#250776,#250777,#250778),
(#250779,#250780,#250781),(#250782,#250783,#250784),(#250785,#250786,#250787),
(#250788,#250789,#250790)),.UNSPECIFIED.,.F.,.F.,.F.)
B_SPLINE_SURFACE_WITH_KNOTS((4,2,4),(3,3),(-1.77538105744501E-18,0.000257652232350876,
0.000515304464701753),(0.,1.),.UNSPECIFIED.)
GEOMETRIC_REPRESENTATION_ITEM()
RATIONAL_B_SPLINE_SURFACE(((1.,0.874619707139395,1.),(1.,0.874861180430488,
1.),(1.,0.85545572592118,1.),(1.,0.794699358954985,1.),(1.,0.753768977788849,
1.),(1.,0.708712527163682,1.)))
REPRESENTATION_ITEM('')
SURFACE()
);
#3799=(
BOUNDED_SURFACE()
B_SPLINE_SURFACE(3,2,((#250796,#250797,#250798),(#250799,#250800,#250801),
(#250802,#250803,#250804),(#250805,#250806,#250807)),.UNSPECIFIED.,.F.,
 .F.,.F.)
B_SPLINE_SURFACE_WITH_KNOTS((4,4),(3,3),(0.,0.000397394373651913),(0.,1.),
 .UNSPECIFIED.)
GEOMETRIC_REPRESENTATION_ITEM()
RATIONAL_B_SPLINE_SURFACE(((1.,0.707106781186552,1.),(1.,0.707752587915901,
1.),(1.,0.70837765454067,1.),(1.,0.708689770883329,1.)))
REPRESENTATION_ITEM('')
SURFACE()
);
#3800=(
BOUNDED_SURFACE()
B_SPLINE_SURFACE(3,2,((#250809,#250810,#250811),(#250812,#250813,#250814),
(#250815,#250816,#250817),(#250818,#250819,#250820)),.UNSPECIFIED.,.F.,
 .F.,.F.)
B_SPLINE_SURFACE_WITH_KNOTS((4,4),(3,3),(-5.20417042793042E-18,0.000511815456479787),
(0.,1.0010587315994),.UNSPECIFIED.)
GEOMETRIC_REPRESENTATION_ITEM()
RATIONAL_B_SPLINE_SURFACE(((1.,0.708394529056482,1.00061746385329),(1.,
0.708058564167038,1.00061817524658),(1.,0.707430835372215,1.0006195044392),
(1.,0.706796685880545,1.00062084722741)))
REPRESENTATION_ITEM('')
SURFACE()
);
#3801=(
BOUNDED_SURFACE()
B_SPLINE_SURFACE(3,2,((#250826,#250827,#250828),(#250829,#250830,#250831),
(#250832,#250833,#250834),(#250835,#250836,#250837)),.UNSPECIFIED.,.F.,
 .F.,.F.)
B_SPLINE_SURFACE_WITH_KNOTS((4,4),(3,3),(0.,0.00039739446544832),(0.,1.),
 .UNSPECIFIED.)
GEOMETRIC_REPRESENTATION_ITEM()
RATIONAL_B_SPLINE_SURFACE(((1.,0.705498956110773,1.),(1.,0.705821764811761,
1.),(1.,0.706461952521155,1.),(1.,0.707106781186548,1.)))
REPRESENTATION_ITEM('')
SURFACE()
);
#3802=(
BOUNDED_SURFACE()
B_SPLINE_SURFACE(3,2,((#250843,#250844,#250845),(#250846,#250847,#250848),
(#250849,#250850,#250851),(#250852,#250853,#250854)),.UNSPECIFIED.,.F.,
 .F.,.F.)
B_SPLINE_SURFACE_WITH_KNOTS((4,4),(3,3),(0.,0.000397394410828742),(0.,1.),
 .UNSPECIFIED.)
GEOMETRIC_REPRESENTATION_ITEM()
RATIONAL_B_SPLINE_SURFACE(((1.,0.708689770883327,1.),(1.,0.708376440034486,
1.),(1.,0.707750498698416,1.),(1.,0.70710678118654,1.)))
REPRESENTATION_ITEM('')
SURFACE()
);
#3803=(
BOUNDED_SURFACE()
B_SPLINE_SURFACE(3,2,((#250860,#250861,#250862),(#250863,#250864,#250865),
(#250866,#250867,#250868),(#250869,#250870,#250871)),.UNSPECIFIED.,.F.,
 .F.,.F.)
B_SPLINE_SURFACE_WITH_KNOTS((4,4),(3,3),(0.,0.000511815090126184),(0.,1.00105592270038),
 .UNSPECIFIED.)
GEOMETRIC_REPRESENTATION_ITEM()
RATIONAL_B_SPLINE_SURFACE(((1.,0.705266242718023,1.00062243212977),(1.,
0.705584085909628,1.00062176089409),(1.,0.706182089451054,1.00062049800306),
(1.,0.706797508588024,1.00061919833298)))
REPRESENTATION_ITEM('')
SURFACE()
);
#3804=(
BOUNDED_SURFACE()
B_SPLINE_SURFACE(3,2,((#250873,#250874,#250875),(#250876,#250877,#250878),
(#250879,#250880,#250881),(#250882,#250883,#250884)),.UNSPECIFIED.,.F.,
 .F.,.F.)
B_SPLINE_SURFACE_WITH_KNOTS((4,4),(3,3),(-5.96311194867027E-19,0.000397394428086628),
(0.,1.),.UNSPECIFIED.)
GEOMETRIC_REPRESENTATION_ITEM()
RATIONAL_B_SPLINE_SURFACE(((1.,0.70710678118654,1.),(1.,0.706459846759098,
1.),(1.,0.705820510737268,1.),(1.,0.705498956110756,1.)))
REPRESENTATION_ITEM('')
SURFACE()
);
#3805=(
BOUNDED_SURFACE()
B_SPLINE_SURFACE(3,2,((#250890,#250891,#250892),(#250893,#250894,#250895),
(#250896,#250897,#250898),(#250899,#250900,#250901),(#250902,#250903,#250904),
(#250905,#250906,#250907)),.UNSPECIFIED.,.F.,.F.,.F.)
B_SPLINE_SURFACE_WITH_KNOTS((4,2,4),(3,3),(0.,0.00025795380787285,0.000515907615745701),
(0.,1.),.UNSPECIFIED.)
GEOMETRIC_REPRESENTATION_ITEM()
RATIONAL_B_SPLINE_SURFACE(((1.,0.874619707139394,1.),(1.,0.874834349679145,
1.),(1.,0.854686104157602,1.),(1.,0.792476597915341,1.),(1.,0.750887854594964,
1.),(1.,0.705585838031464,1.)))
REPRESENTATION_ITEM('')
SURFACE()
);
#3806=(
BOUNDED_SURFACE()
B_SPLINE_SURFACE(3,2,((#250913,#250914,#250915),(#250916,#250917,#250918),
(#250919,#250920,#250921),(#250922,#250923,#250924)),.UNSPECIFIED.,.F.,
 .F.,.F.)
B_SPLINE_SURFACE_WITH_KNOTS((4,4),(3,3),(0.,0.000511815437699155),(0.,1.00105881331637),
 .UNSPECIFIED.)
GEOMETRIC_REPRESENTATION_ITEM()
RATIONAL_B_SPLINE_SURFACE(((1.,0.706796661946191,1.00062089519747),(1.,
0.707430821225076,1.00061955228489),(1.,0.708058545830567,1.00061822299855),
(1.,0.708394505252572,1.00061751156193)))
REPRESENTATION_ITEM('')
SURFACE()
);
#3807=(
BOUNDED_SURFACE()
B_SPLINE_SURFACE(3,2,((#250926,#250927,#250928),(#250929,#250930,#250931),
(#250932,#250933,#250934),(#250935,#250936,#250937),(#250938,#250939,#250940),
(#250941,#250942,#250943)),.UNSPECIFIED.,.F.,.F.,.F.)
B_SPLINE_SURFACE_WITH_KNOTS((4,2,4),(3,3),(2.71050543121376E-20,0.000256915317531261,
0.000513830635062521),(0.,1.),.UNSPECIFIED.)
GEOMETRIC_REPRESENTATION_ITEM()
RATIONAL_B_SPLINE_SURFACE(((1.,0.705585838031446,1.),(1.,0.750902433542993,
1.),(1.,0.792329530082176,1.),(1.,0.854288401594561,1.),(1.,0.87499803112487,
1.),(1.,0.874619707139384,1.)))
REPRESENTATION_ITEM('')
SURFACE()
);
#3808=(
BOUNDED_SURFACE()
B_SPLINE_SURFACE(3,2,((#250949,#250950,#250951),(#250952,#250953,#250954),
(#250955,#250956,#250957),(#250958,#250959,#250960),(#250961,#250962,#250963),
(#250964,#250965,#250966)),.UNSPECIFIED.,.F.,.F.,.F.)
B_SPLINE_SURFACE_WITH_KNOTS((4,2,4),(3,3),(-2.5207700510288E-18,0.000256592814262154,
0.000513185628524311),(0.,1.),.UNSPECIFIED.)
GEOMETRIC_REPRESENTATION_ITEM()
RATIONAL_B_SPLINE_SURFACE(((1.,0.708712527163663,1.),(1.,0.753780902613565,
1.),(1.,0.794538995769234,1.),(1.,0.85507077033108,1.),(1.,0.87501842744533,
1.),(1.,0.874619707139398,1.)))
REPRESENTATION_ITEM('')
SURFACE()
);
#3809=(
BOUNDED_SURFACE()
B_SPLINE_SURFACE(3,2,((#250968,#250969,#250970),(#250971,#250972,#250973),
(#250974,#250975,#250976),(#250977,#250978,#250979)),.UNSPECIFIED.,.F.,
 .F.,.F.)
B_SPLINE_SURFACE_WITH_KNOTS((4,4),(3,3),(-5.6920614055489E-19,0.000511815072430393),
(0.,1.00105598365897),.UNSPECIFIED.)
GEOMETRIC_REPRESENTATION_ITEM()
RATIONAL_B_SPLINE_SURFACE(((1.,0.706797490733658,1.00061923411711),(1.,
0.706182062146592,1.00062053388217),(1.,0.705584062768913,1.00062179683731),
(1.,0.705266224770416,1.00062246810078)))
REPRESENTATION_ITEM('')
SURFACE()
);
#3810=(
BOUNDED_SURFACE()
B_SPLINE_SURFACE(3,2,((#250985,#250986,#250987),(#250988,#250989,#250990),
(#250991,#250992,#250993),(#250994,#250995,#250996),(#250997,#250998,#250999),
(#251000,#251001,#251002)),.UNSPECIFIED.,.F.,.F.,.F.)
B_SPLINE_SURFACE_WITH_KNOTS((4,2,4),(3,3),(-3.41523684332934E-18,0.000257652232350878,
0.00051530446470176),(0.,1.),.UNSPECIFIED.)
GEOMETRIC_REPRESENTATION_ITEM()
RATIONAL_B_SPLINE_SURFACE(((1.,0.874619707139395,1.),(1.,0.874861180430739,
1.),(1.,0.855455725920833,1.),(1.,0.794699358955319,1.),(1.,0.753768977788611,
1.),(1.,0.708712527163663,1.)))
REPRESENTATION_ITEM('')
SURFACE()
);
#3811=(
BOUNDED_SURFACE()
B_SPLINE_SURFACE(3,2,((#251008,#251009,#251010),(#251011,#251012,#251013),
(#251014,#251015,#251016),(#251017,#251018,#251019)),.UNSPECIFIED.,.F.,
 .F.,.F.)
B_SPLINE_SURFACE_WITH_KNOTS((4,4),(3,3),(0.,0.000397394373651901),(0.,1.),
 .UNSPECIFIED.)
GEOMETRIC_REPRESENTATION_ITEM()
RATIONAL_B_SPLINE_SURFACE(((1.,0.707106781186549,1.),(1.,0.707752587915924,
1.),(1.,0.70837765454066,1.),(1.,0.708689770883335,1.)))
REPRESENTATION_ITEM('')
SURFACE()
);
#3812=(
BOUNDED_SURFACE()
B_SPLINE_SURFACE(3,2,((#251021,#251022,#251023),(#251024,#251025,#251026),
(#251027,#251028,#251029),(#251030,#251031,#251032)),.UNSPECIFIED.,.F.,
 .F.,.F.)
B_SPLINE_SURFACE_WITH_KNOTS((4,4),(3,3),(-5.61074624261249E-18,0.000511815456479779),
(0.,1.00105873160044),.UNSPECIFIED.)
GEOMETRIC_REPRESENTATION_ITEM()
RATIONAL_B_SPLINE_SURFACE(((1.,0.708394529056196,1.0006174638539),(1.,0.708058564166725,
1.00061817524719),(1.,0.707430835371925,1.00061950443981),(1.,0.706796685880237,
1.00062084722802)))
REPRESENTATION_ITEM('')
SURFACE()
);
#3813=(
BOUNDED_SURFACE()
B_SPLINE_SURFACE(3,2,((#251038,#251039,#251040),(#251041,#251042,#251043),
(#251044,#251045,#251046),(#251047,#251048,#251049)),.UNSPECIFIED.,.F.,
 .F.,.F.)
B_SPLINE_SURFACE_WITH_KNOTS((4,4),(3,3),(0.,0.000397394465448301),(0.,1.),
 .UNSPECIFIED.)
GEOMETRIC_REPRESENTATION_ITEM()
RATIONAL_B_SPLINE_SURFACE(((1.,0.705498956110749,1.),(1.,0.70582176481179,
1.),(1.,0.706461952521136,1.),(1.,0.707106781186549,1.)))
REPRESENTATION_ITEM('')
SURFACE()
);
#3814=(
BOUNDED_SURFACE()
B_SPLINE_SURFACE(3,2,((#251055,#251056,#251057),(#251058,#251059,#251060),
(#251061,#251062,#251063),(#251064,#251065,#251066)),.UNSPECIFIED.,.F.,
 .F.,.F.)
B_SPLINE_SURFACE_WITH_KNOTS((4,4),(3,3),(0.,0.000397394410828748),(0.,1.),
 .UNSPECIFIED.)
GEOMETRIC_REPRESENTATION_ITEM()
RATIONAL_B_SPLINE_SURFACE(((1.,0.708689770883332,1.),(1.,0.708376440034477,
1.),(1.,0.707750498698426,1.),(1.,0.707106781186546,1.)))
REPRESENTATION_ITEM('')
SURFACE()
);
#3815=(
BOUNDED_SURFACE()
B_SPLINE_SURFACE(3,2,((#251072,#251073,#251074),(#251075,#251076,#251077),
(#251078,#251079,#251080),(#251081,#251082,#251083)),.UNSPECIFIED.,.F.,
 .F.,.F.)
B_SPLINE_SURFACE_WITH_KNOTS((4,4),(3,3),(3.19839640883224E-18,0.00051181509012619),
(0.,1.00105592270332),.UNSPECIFIED.)
GEOMETRIC_REPRESENTATION_ITEM()
RATIONAL_B_SPLINE_SURFACE(((1.,0.705266242717177,1.0006224321315),(1.,0.705584085908736,
1.00062176089582),(1.,0.706182089450218,1.00062049800479),(1.,0.706797508587152,
1.00061919833471)))
REPRESENTATION_ITEM('')
SURFACE()
);
#3816=(
BOUNDED_SURFACE()
B_SPLINE_SURFACE(3,2,((#251085,#251086,#251087),(#251088,#251089,#251090),
(#251091,#251092,#251093),(#251094,#251095,#251096)),.UNSPECIFIED.,.F.,
 .F.,.F.)
B_SPLINE_SURFACE_WITH_KNOTS((4,4),(3,3),(0.,0.000397394428086631),(0.,1.),
 .UNSPECIFIED.)
GEOMETRIC_REPRESENTATION_ITEM()
RATIONAL_B_SPLINE_SURFACE(((1.,0.707106781186546,1.),(1.,0.706459846759087,
1.),(1.,0.705820510737286,1.),(1.,0.705498956110744,1.)))
REPRESENTATION_ITEM('')
SURFACE()
);
#3817=(
BOUNDED_SURFACE()
B_SPLINE_SURFACE(3,2,((#251102,#251103,#251104),(#251105,#251106,#251107),
(#251108,#251109,#251110),(#251111,#251112,#251113),(#251114,#251115,#251116),
(#251117,#251118,#251119)),.UNSPECIFIED.,.F.,.F.,.F.)
B_SPLINE_SURFACE_WITH_KNOTS((4,2,4),(3,3),(0.,0.000257953807872843,0.000515907615745686),
(0.,1.),.UNSPECIFIED.)
GEOMETRIC_REPRESENTATION_ITEM()
RATIONAL_B_SPLINE_SURFACE(((1.,0.874619707139386,1.),(1.,0.874834349679186,
1.),(1.,0.854686104157541,1.),(1.,0.792476597915398,1.),(1.,0.750887854594977,
1.),(1.,0.705585838031422,1.)))
REPRESENTATION_ITEM('')
SURFACE()
);
#3818=(
BOUNDED_SURFACE()
B_SPLINE_SURFACE(3,2,((#251125,#251126,#251127),(#251128,#251129,#251130),
(#251131,#251132,#251133),(#251134,#251135,#251136)),.UNSPECIFIED.,.F.,
 .F.,.F.)
B_SPLINE_SURFACE_WITH_KNOTS((4,4),(3,3),(5.6920614055489E-19,0.000511815437699156),
(0.,1.00105881331822),.UNSPECIFIED.)
GEOMETRIC_REPRESENTATION_ITEM()
RATIONAL_B_SPLINE_SURFACE(((1.,0.706796661945643,1.00062089519855),(1.,
0.707430821224538,1.00061955228597),(1.,0.708058545830045,1.00061822299963),
(1.,0.708394505252033,1.00061751156301)))
REPRESENTATION_ITEM('')
SURFACE()
);
#3819=(
BOUNDED_SURFACE()
B_SPLINE_SURFACE(3,2,((#251138,#251139,#251140),(#251141,#251142,#251143),
(#251144,#251145,#251146),(#251147,#251148,#251149),(#251150,#251151,#251152),
(#251153,#251154,#251155)),.UNSPECIFIED.,.F.,.F.,.F.)
B_SPLINE_SURFACE_WITH_KNOTS((4,2,4),(3,3),(2.71050543121376E-20,0.000256915317531261,
0.000513830635062521),(0.,1.),.UNSPECIFIED.)
GEOMETRIC_REPRESENTATION_ITEM()
RATIONAL_B_SPLINE_SURFACE(((1.,0.705585838031431,1.),(1.,0.750902433543086,
1.),(1.,0.792329530082085,1.),(1.,0.854288401594642,1.),(1.,0.874998031124819,
1.),(1.,0.874619707139387,1.)))
REPRESENTATION_ITEM('')
SURFACE()
);
#3820=(
BOUNDED_SURFACE()
B_SPLINE_SURFACE(3,2,((#251161,#251162,#251163),(#251164,#251165,#251166),
(#251167,#251168,#251169),(#251170,#251171,#251172),(#251173,#251174,#251175),
(#251176,#251177,#251178)),.UNSPECIFIED.,.F.,.F.,.F.)
B_SPLINE_SURFACE_WITH_KNOTS((4,2,4),(3,3),(-2.54787510534094E-18,0.000256592814262151,
0.000513185628524304),(0.,1.),.UNSPECIFIED.)
GEOMETRIC_REPRESENTATION_ITEM()
RATIONAL_B_SPLINE_SURFACE(((1.,0.70871252716367,1.),(1.,0.75378090261397,
1.),(1.,0.7945389957687,1.),(1.,0.855070770331624,1.),(1.,0.875018427444944,
1.),(1.,0.874619707139394,1.)))
REPRESENTATION_ITEM('')
SURFACE()
);
#3821=(
BOUNDED_SURFACE()
B_SPLINE_SURFACE(3,2,((#251180,#251181,#251182),(#251183,#251184,#251185),
(#251186,#251187,#251188),(#251189,#251190,#251191)),.UNSPECIFIED.,.F.,
 .F.,.F.)
B_SPLINE_SURFACE_WITH_KNOTS((4,4),(3,3),(-8.13151629364128E-20,0.000511815072430399),
(0.,1.00105598366107),.UNSPECIFIED.)
GEOMETRIC_REPRESENTATION_ITEM()
RATIONAL_B_SPLINE_SURFACE(((1.,0.706797490733043,1.00061923411834),(1.,
0.706182062145961,1.00062053388341),(1.,0.705584062768314,1.00062179683855),
(1.,0.705266224769801,1.00062246810202)))
REPRESENTATION_ITEM('')
SURFACE()
);
#3822=(
BOUNDED_SURFACE()
B_SPLINE_SURFACE(3,2,((#251197,#251198,#251199),(#251200,#251201,#251202),
(#251203,#251204,#251205),(#251206,#251207,#251208),(#251209,#251210,#251211),
(#251212,#251213,#251214)),.UNSPECIFIED.,.F.,.F.,.F.)
B_SPLINE_SURFACE_WITH_KNOTS((4,2,4),(3,3),(0.,0.000257652232350877,0.000515304464701754),
(0.,1.),.UNSPECIFIED.)
GEOMETRIC_REPRESENTATION_ITEM()
RATIONAL_B_SPLINE_SURFACE(((1.,0.874619707139387,1.),(1.,0.874861180430411,
1.),(1.,0.855455725921276,1.),(1.,0.794699358954857,1.),(1.,0.753768977788948,
1.),(1.,0.708712527163661,1.)))
REPRESENTATION_ITEM('')
SURFACE()
);
#3823=(
BOUNDED_SURFACE()
B_SPLINE_SURFACE(3,2,((#251220,#251221,#251222),(#251223,#251224,#251225),
(#251226,#251227,#251228),(#251229,#251230,#251231)),.UNSPECIFIED.,.F.,
 .F.,.F.)
B_SPLINE_SURFACE_WITH_KNOTS((4,4),(3,3),(5.96311194867027E-19,0.000397394373651902),
(0.,1.),.UNSPECIFIED.)
GEOMETRIC_REPRESENTATION_ITEM()
RATIONAL_B_SPLINE_SURFACE(((1.,0.707106781186558,1.),(1.,0.707752587915892,
1.),(1.,0.708377654540708,1.),(1.,0.708689770883314,1.)))
REPRESENTATION_ITEM('')
SURFACE()
);
#3824=(
BOUNDED_SURFACE()
B_SPLINE_SURFACE(3,2,((#251233,#251234,#251235),(#251236,#251237,#251238),
(#251239,#251240,#251241),(#251242,#251243,#251244)),.UNSPECIFIED.,.F.,
 .F.,.F.)
B_SPLINE_SURFACE_WITH_KNOTS((4,4),(3,3),(0.,0.000511815456479788),(0.,1.001058731602),
 .UNSPECIFIED.)
GEOMETRIC_REPRESENTATION_ITEM()
RATIONAL_B_SPLINE_SURFACE(((1.,0.708394529055739,1.00061746385481),(1.,
0.708058564166243,1.0006181752481),(1.,0.707430835371497,1.00061950444072),
(1.,0.706796685879771,1.00062084722894)))
REPRESENTATION_ITEM('')
SURFACE()
);
#3825=(
BOUNDED_SURFACE()
B_SPLINE_SURFACE(3,2,((#251250,#251251,#251252),(#251253,#251254,#251255),
(#251256,#251257,#251258),(#251259,#251260,#251261)),.UNSPECIFIED.,.F.,
 .F.,.F.)
B_SPLINE_SURFACE_WITH_KNOTS((4,4),(3,3),(-4.33680868994202E-19,0.000397394465448297),
(0.,1.),.UNSPECIFIED.)
GEOMETRIC_REPRESENTATION_ITEM()
RATIONAL_B_SPLINE_SURFACE(((1.,0.705498956110758,1.),(1.,0.705821764811795,
1.),(1.,0.706461952521142,1.),(1.,0.707106781186557,1.)))
REPRESENTATION_ITEM('')
SURFACE()
);
#3826=(
BOUNDED_SURFACE()
B_SPLINE_SURFACE(3,2,((#251267,#251268,#251269),(#251270,#251271,#251272),
(#251273,#251274,#251275),(#251276,#251277,#251278)),.UNSPECIFIED.,.F.,
 .F.,.F.)
B_SPLINE_SURFACE_WITH_KNOTS((4,4),(3,3),(0.,0.000397394410828731),(0.,1.),
 .UNSPECIFIED.)
GEOMETRIC_REPRESENTATION_ITEM()
RATIONAL_B_SPLINE_SURFACE(((1.,0.708689770883321,1.),(1.,0.708376440034491,
1.),(1.,0.707750498698422,1.),(1.,0.707106781186546,1.)))
REPRESENTATION_ITEM('')
SURFACE()
);
#3827=(
BOUNDED_SURFACE()
B_SPLINE_SURFACE(3,2,((#251284,#251285,#251286),(#251287,#251288,#251289),
(#251290,#251291,#251292),(#251293,#251294,#251295)),.UNSPECIFIED.,.F.,
 .F.,.F.)
B_SPLINE_SURFACE_WITH_KNOTS((4,4),(3,3),(1.19262238973405E-18,0.000511815090126183),
(0.,1.00105592270195),.UNSPECIFIED.)
GEOMETRIC_REPRESENTATION_ITEM()
RATIONAL_B_SPLINE_SURFACE(((1.,0.705266242717556,1.00062243213069),(1.,
0.705584085909223,1.00062176089501),(1.,0.706182089450549,1.00062049800398),
(1.,0.706797508587564,1.0006191983339)))
REPRESENTATION_ITEM('')
SURFACE()
);
#3828=(
BOUNDED_SURFACE()
B_SPLINE_SURFACE(3,2,((#251297,#251298,#251299),(#251300,#251301,#251302),
(#251303,#251304,#251305),(#251306,#251307,#251308)),.UNSPECIFIED.,.F.,
 .F.,.F.)
B_SPLINE_SURFACE_WITH_KNOTS((4,4),(3,3),(-1.57209315010398E-17,0.000397394428086616),
(0.,1.),.UNSPECIFIED.)
GEOMETRIC_REPRESENTATION_ITEM()
RATIONAL_B_SPLINE_SURFACE(((1.,0.707106781186557,1.),(1.,0.70645984675906,
1.),(1.,0.705820510737312,1.),(1.,0.705498956110748,1.)))
REPRESENTATION_ITEM('')
SURFACE()
);
#3829=(
BOUNDED_SURFACE()
B_SPLINE_SURFACE(3,2,((#251314,#251315,#251316),(#251317,#251318,#251319),
(#251320,#251321,#251322),(#251323,#251324,#251325),(#251326,#251327,#251328),
(#251329,#251330,#251331)),.UNSPECIFIED.,.F.,.F.,.F.)
B_SPLINE_SURFACE_WITH_KNOTS((4,2,4),(3,3),(0.,0.000257953807872847,0.000515907615745694),
(0.,1.),.UNSPECIFIED.)
GEOMETRIC_REPRESENTATION_ITEM()
RATIONAL_B_SPLINE_SURFACE(((1.,0.874619707139392,1.),(1.,0.874834349679668,
1.),(1.,0.854686104156887,1.),(1.,0.792476597916051,1.),(1.,0.750887854594419,
1.),(1.,0.705585838031433,1.)))
REPRESENTATION_ITEM('')
SURFACE()
);
#3830=(
BOUNDED_SURFACE()
B_SPLINE_SURFACE(3,2,((#251337,#251338,#251339),(#251340,#251341,#251342),
(#251343,#251344,#251345),(#251346,#251347,#251348)),.UNSPECIFIED.,.F.,
 .F.,.F.)
B_SPLINE_SURFACE_WITH_KNOTS((4,4),(3,3),(5.6920614055489E-19,0.000511815437699143),
(0.,1.00105881331806),.UNSPECIFIED.)
GEOMETRIC_REPRESENTATION_ITEM()
RATIONAL_B_SPLINE_SURFACE(((1.,0.706796661945705,1.00062089519846),(1.,
0.707430821224546,1.00061955228588),(1.,0.708058545830125,1.00061822299954),
(1.,0.708394505252067,1.00061751156292)))
REPRESENTATION_ITEM('')
SURFACE()
);
#3831=(
BOUNDED_SURFACE()
B_SPLINE_SURFACE(3,2,((#251350,#251351,#251352),(#251353,#251354,#251355),
(#251356,#251357,#251358),(#251359,#251360,#251361),(#251362,#251363,#251364),
(#251365,#251366,#251367)),.UNSPECIFIED.,.F.,.F.,.F.)
B_SPLINE_SURFACE_WITH_KNOTS((4,2,4),(3,3),(0.,0.000256915317531259,0.000513830635062519),
(0.,1.),.UNSPECIFIED.)
GEOMETRIC_REPRESENTATION_ITEM()
RATIONAL_B_SPLINE_SURFACE(((1.,0.705585838031461,1.),(1.,0.750902433542499,
1.),(1.,0.79232953008284,1.),(1.,0.854288401593916,1.),(1.,0.874998031125362,
1.),(1.,0.874619707139391,1.)))
REPRESENTATION_ITEM('')
SURFACE()
);
#3832=(
BOUNDED_SURFACE()
B_SPLINE_SURFACE(3,2,((#251373,#251374,#251375),(#251376,#251377,#251378),
(#251379,#251380,#251381),(#251382,#251383,#251384),(#251385,#251386,#251387),
(#251388,#251389,#251390)),.UNSPECIFIED.,.F.,.F.,.F.)
B_SPLINE_SURFACE_WITH_KNOTS((4,2,4),(3,3),(-3.52365706057789E-19,0.000256592814262155,
0.00051318562852431),(0.,1.),.UNSPECIFIED.)
GEOMETRIC_REPRESENTATION_ITEM()
RATIONAL_B_SPLINE_SURFACE(((1.,0.708712527163665,1.),(1.,0.753780902613458,
1.),(1.,0.794538995769382,1.),(1.,0.855070770330922,1.),(1.,0.875018427445469,
1.),(1.,0.874619707139403,1.)))
REPRESENTATION_ITEM('')
SURFACE()
);
#3833=(
BOUNDED_SURFACE()
B_SPLINE_SURFACE(3,2,((#251392,#251393,#251394),(#251395,#251396,#251397),
(#251398,#251399,#251400),(#251401,#251402,#251403)),.UNSPECIFIED.,.F.,
 .F.,.F.)
B_SPLINE_SURFACE_WITH_KNOTS((4,4),(3,3),(0.,0.000511815072430388),(0.,1.0010559836583),
 .UNSPECIFIED.)
GEOMETRIC_REPRESENTATION_ITEM()
RATIONAL_B_SPLINE_SURFACE(((1.,0.706797490733863,1.00061923411672),(1.,
0.706182062146757,1.00062053388178),(1.,0.705584062769147,1.00062179683692),
(1.,0.70526622477061,1.00062246810038)))
REPRESENTATION_ITEM('')
SURFACE()
);
#3834=(
BOUNDED_SURFACE()
B_SPLINE_SURFACE(3,2,((#251409,#251410,#251411),(#251412,#251413,#251414),
(#251415,#251416,#251417),(#251418,#251419,#251420),(#251421,#251422,#251423),
(#251424,#251425,#251426)),.UNSPECIFIED.,.F.,.F.,.F.)
B_SPLINE_SURFACE_WITH_KNOTS((4,2,4),(3,3),(0.,0.000257652232350886,0.000515304464701772),
(0.,1.),.UNSPECIFIED.)
GEOMETRIC_REPRESENTATION_ITEM()
RATIONAL_B_SPLINE_SURFACE(((1.,0.874619707139385,1.),(1.,0.874861180430413,
1.),(1.,0.855455725921248,1.),(1.,0.794699358954868,1.),(1.,0.753768977788925,
1.),(1.,0.708712527163669,1.)))
REPRESENTATION_ITEM('')
SURFACE()
);
#3835=(
BOUNDED_SURFACE()
B_SPLINE_SURFACE(3,2,((#251432,#251433,#251434),(#251435,#251436,#251437),
(#251438,#251439,#251440),(#251441,#251442,#251443)),.UNSPECIFIED.,.F.,
 .F.,.F.)
B_SPLINE_SURFACE_WITH_KNOTS((4,4),(3,3),(-1.5748036555352E-17,0.000397394373651903),
(0.,1.),.UNSPECIFIED.)
GEOMETRIC_REPRESENTATION_ITEM()
RATIONAL_B_SPLINE_SURFACE(((1.,0.70710678118655,1.),(1.,0.70775258791589,
1.),(1.,0.70837765454068,1.),(1.,0.708689770883327,1.)))
REPRESENTATION_ITEM('')
SURFACE()
);
#3836=(
BOUNDED_SURFACE()
B_SPLINE_SURFACE(3,2,((#251445,#251446,#251447),(#251448,#251449,#251450),
(#251451,#251452,#251453),(#251454,#251455,#251456)),.UNSPECIFIED.,.F.,
 .F.,.F.)
B_SPLINE_SURFACE_WITH_KNOTS((4,4),(3,3),(-3.79470760369927E-19,0.000511815456479784),
(0.,1.00105873159937),.UNSPECIFIED.)
GEOMETRIC_REPRESENTATION_ITEM()
RATIONAL_B_SPLINE_SURFACE(((1.,0.708394529056501,1.00061746385327),(1.,
0.708058564167041,1.00061817524656),(1.,0.707430835372212,1.00061950443918),
(1.,0.70679668588055,1.0006208472274)))
REPRESENTATION_ITEM('')
SURFACE()
);
#3837=(
BOUNDED_SURFACE()
B_SPLINE_SURFACE(3,2,((#251462,#251463,#251464),(#251465,#251466,#251467),
(#251468,#251469,#251470),(#251471,#251472,#251473)),.UNSPECIFIED.,.F.,
 .F.,.F.)
B_SPLINE_SURFACE_WITH_KNOTS((4,4),(3,3),(-1.21972744404619E-18,0.000397394465448303),
(0.,1.),.UNSPECIFIED.)
GEOMETRIC_REPRESENTATION_ITEM()
RATIONAL_B_SPLINE_SURFACE(((1.,0.705498956110749,1.),(1.,0.705821764811809,
1.),(1.,0.70646195252111,1.),(1.,0.707106781186557,1.)))
REPRESENTATION_ITEM('')
SURFACE()
);
#3838=(
BOUNDED_SURFACE()
B_SPLINE_SURFACE(3,2,((#251479,#251480,#251481),(#251482,#251483,#251484),
(#251485,#251486,#251487),(#251488,#251489,#251490)),.UNSPECIFIED.,.F.,
 .F.,.F.)
B_SPLINE_SURFACE_WITH_KNOTS((4,4),(3,3),(0.,0.00039739441082874),(0.,1.),
 .UNSPECIFIED.)
GEOMETRIC_REPRESENTATION_ITEM()
RATIONAL_B_SPLINE_SURFACE(((1.,0.708689770883337,1.),(1.,0.708376440034467,
1.),(1.,0.70775049869843,1.),(1.,0.707106781186535,1.)))
REPRESENTATION_ITEM('')
SURFACE()
);
#3839=(
BOUNDED_SURFACE()
B_SPLINE_SURFACE(3,2,((#251496,#251497,#251498),(#251499,#251500,#251501),
(#251502,#251503,#251504),(#251505,#251506,#251507)),.UNSPECIFIED.,.F.,
 .F.,.F.)
B_SPLINE_SURFACE_WITH_KNOTS((4,4),(3,3),(0.,0.00051181509012618),(0.,1.00105592270322),
 .UNSPECIFIED.)
GEOMETRIC_REPRESENTATION_ITEM()
RATIONAL_B_SPLINE_SURFACE(((1.,0.705266242717196,1.00062243213144),(1.,
0.705584085908844,1.00062176089576),(1.,0.706182089450187,1.00062049800472),
(1.,0.706797508587171,1.00061919833465)))
REPRESENTATION_ITEM('')
SURFACE()
);
#3840=(
BOUNDED_SURFACE()
B_SPLINE_SURFACE(3,2,((#251509,#251510,#251511),(#251512,#251513,#251514),
(#251515,#251516,#251517),(#251518,#251519,#251520)),.UNSPECIFIED.,.F.,
 .F.,.F.)
B_SPLINE_SURFACE_WITH_KNOTS((4,4),(3,3),(0.,0.000397394428086653),(0.,1.),
 .UNSPECIFIED.)
GEOMETRIC_REPRESENTATION_ITEM()
RATIONAL_B_SPLINE_SURFACE(((1.,0.707106781186551,1.),(1.,0.706459846759095,
1.),(1.,0.705820510737328,1.),(1.,0.705498956110736,1.)))
REPRESENTATION_ITEM('')
SURFACE()
);
#3841=(
BOUNDED_SURFACE()
B_SPLINE_SURFACE(3,2,((#251526,#251527,#251528),(#251529,#251530,#251531),
(#251532,#251533,#251534),(#251535,#251536,#251537),(#251538,#251539,#251540),
(#251541,#251542,#251543)),.UNSPECIFIED.,.F.,.F.,.F.)
B_SPLINE_SURFACE_WITH_KNOTS((4,2,4),(3,3),(-5.14996031930615E-19,0.000257953807872846,
0.000515907615745692),(0.,1.),.UNSPECIFIED.)
GEOMETRIC_REPRESENTATION_ITEM()
RATIONAL_B_SPLINE_SURFACE(((1.,0.874619707139391,1.),(1.,0.874834349679085,
1.),(1.,0.854686104157701,1.),(1.,0.79247659791524,1.),(1.,0.75088785459503,
1.),(1.,0.705585838031485,1.)))
REPRESENTATION_ITEM('')
SURFACE()
);
#3842=(
BOUNDED_SURFACE()
B_SPLINE_SURFACE(3,2,((#251549,#251550,#251551),(#251552,#251553,#251554),
(#251555,#251556,#251557),(#251558,#251559,#251560)),.UNSPECIFIED.,.F.,
 .F.,.F.)
B_SPLINE_SURFACE_WITH_KNOTS((4,4),(3,3),(0.,0.000511815437699156),(0.,1.00105881331948),
 .UNSPECIFIED.)
GEOMETRIC_REPRESENTATION_ITEM()
RATIONAL_B_SPLINE_SURFACE(((1.,0.706796661945281,1.0006208951993),(1.,0.707430821224171,
1.00061955228671),(1.,0.708058545829648,1.00061822300037),(1.,0.708394505251669,
1.00061751156375)))
REPRESENTATION_ITEM('')
SURFACE()
);
#3843=(
BOUNDED_SURFACE()
B_SPLINE_SURFACE(3,2,((#251562,#251563,#251564),(#251565,#251566,#251567),
(#251568,#251569,#251570),(#251571,#251572,#251573),(#251574,#251575,#251576),
(#251577,#251578,#251579)),.UNSPECIFIED.,.F.,.F.,.F.)
B_SPLINE_SURFACE_WITH_KNOTS((4,2,4),(3,3),(2.87313575708659E-18,0.000256915317531265,
0.000513830635062527),(0.,1.),.UNSPECIFIED.)
GEOMETRIC_REPRESENTATION_ITEM()
RATIONAL_B_SPLINE_SURFACE(((1.,0.705585838031446,1.),(1.,0.750902433542731,
1.),(1.,0.792329530082549,1.),(1.,0.85428840159417,1.),(1.,0.874998031125167,
1.),(1.,0.874619707139405,1.)))
REPRESENTATION_ITEM('')
SURFACE()
);
#3844=(
BOUNDED_SURFACE()
B_SPLINE_SURFACE(3,2,((#251585,#251586,#251587),(#251588,#251589,#251590),
(#251591,#251592,#251593),(#251594,#251595,#251596),(#251597,#251598,#251599),
(#251600,#251601,#251602)),.UNSPECIFIED.,.F.,.F.,.F.)
B_SPLINE_SURFACE_WITH_KNOTS((4,2,4),(3,3),(-1.08962318334793E-17,0.000256592814262147,
0.000513185628524304),(0.,1.),.UNSPECIFIED.)
GEOMETRIC_REPRESENTATION_ITEM()
RATIONAL_B_SPLINE_SURFACE(((1.,0.708712527163664,1.),(1.,0.753780902613837,
1.),(1.,0.794538995768865,1.),(1.,0.855070770331436,1.),(1.,0.875018427445072,
1.),(1.,0.874619707139397,1.)))
REPRESENTATION_ITEM('')
SURFACE()
);
#3845=(
BOUNDED_SURFACE()
B_SPLINE_SURFACE(3,2,((#251604,#251605,#251606),(#251607,#251608,#251609),
(#251610,#251611,#251612),(#251613,#251614,#251615)),.UNSPECIFIED.,.F.,
 .F.,.F.)
B_SPLINE_SURFACE_WITH_KNOTS((4,4),(3,3),(0.,0.000511815072430403),(0.,1.0010559836591),
 .UNSPECIFIED.)
GEOMETRIC_REPRESENTATION_ITEM()
RATIONAL_B_SPLINE_SURFACE(((1.,0.706797490733619,1.00061923411719),(1.,
0.706182062146509,1.00062053388225),(1.,0.70558406276892,1.00062179683739),
(1.,0.705266224770374,1.00062246810086)))
REPRESENTATION_ITEM('')
SURFACE()
);
#3846=(
BOUNDED_SURFACE()
B_SPLINE_SURFACE(3,2,((#251621,#251622,#251623),(#251624,#251625,#251626),
(#251627,#251628,#251629),(#251630,#251631,#251632),(#251633,#251634,#251635),
(#251636,#251637,#251638)),.UNSPECIFIED.,.F.,.F.,.F.)
B_SPLINE_SURFACE_WITH_KNOTS((4,2,4),(3,3),(0.,0.000257652232350878,0.000515304464701757),
(0.,1.),.UNSPECIFIED.)
GEOMETRIC_REPRESENTATION_ITEM()
RATIONAL_B_SPLINE_SURFACE(((1.,0.874619707139383,1.),(1.,0.874861180430538,
1.),(1.,0.855455725921087,1.),(1.,0.794699358955036,1.),(1.,0.753768977788808,
1.),(1.,0.708712527163679,1.)))
REPRESENTATION_ITEM('')
SURFACE()
);
#3847=(
BOUNDED_SURFACE()
B_SPLINE_SURFACE(3,2,((#251644,#251645,#251646),(#251647,#251648,#251649),
(#251650,#251651,#251652),(#251653,#251654,#251655)),.UNSPECIFIED.,.F.,
 .F.,.F.)
B_SPLINE_SURFACE_WITH_KNOTS((4,4),(3,3),(5.96311194867027E-19,0.000397394373651916),
(0.,1.),.UNSPECIFIED.)
GEOMETRIC_REPRESENTATION_ITEM()
RATIONAL_B_SPLINE_SURFACE(((1.,0.707106781186549,1.),(1.,0.70775258791589,
1.),(1.,0.708377654540699,1.),(1.,0.708689770883332,1.)))
REPRESENTATION_ITEM('')
SURFACE()
);
#3848=(
BOUNDED_SURFACE()
B_SPLINE_SURFACE(3,2,((#251657,#251658,#251659),(#251660,#251661,#251662),
(#251663,#251664,#251665),(#251666,#251667,#251668)),.UNSPECIFIED.,.F.,
 .F.,.F.)
B_SPLINE_SURFACE_WITH_KNOTS((4,4),(3,3),(-5.61074624261249E-18,0.000511815456479781),
(0.,1.00105873159944),.UNSPECIFIED.)
GEOMETRIC_REPRESENTATION_ITEM()
RATIONAL_B_SPLINE_SURFACE(((1.,0.708394529056449,1.00061746385331),(1.,
0.70805856416707,1.0006181752466),(1.,0.707430835372197,1.00061950443923),
(1.,0.706796685880541,1.00062084722744)))
REPRESENTATION_ITEM('')
SURFACE()
);
#3849=(
BOUNDED_SURFACE()
B_SPLINE_SURFACE(3,2,((#251674,#251675,#251676),(#251677,#251678,#251679),
(#251680,#251681,#251682),(#251683,#251684,#251685)),.UNSPECIFIED.,.F.,
 .F.,.F.)
B_SPLINE_SURFACE_WITH_KNOTS((4,4),(3,3),(0.,0.000397394465448315),(0.,1.),
 .UNSPECIFIED.)
GEOMETRIC_REPRESENTATION_ITEM()
RATIONAL_B_SPLINE_SURFACE(((1.,0.705498956110738,1.),(1.,0.7058217648118,
1.),(1.,0.706461952521122,1.),(1.,0.70710678118656,1.)))
REPRESENTATION_ITEM('')
SURFACE()
);
#3850=(
BOUNDED_SURFACE()
B_SPLINE_SURFACE(3,2,((#251691,#251692,#251693),(#251694,#251695,#251696),
(#251697,#251698,#251699),(#251700,#251701,#251702)),.UNSPECIFIED.,.F.,
 .F.,.F.)
B_SPLINE_SURFACE_WITH_KNOTS((4,4),(3,3),(0.,0.000397394410828751),(0.,1.),
 .UNSPECIFIED.)
GEOMETRIC_REPRESENTATION_ITEM()
RATIONAL_B_SPLINE_SURFACE(((1.,0.708689770883341,1.),(1.,0.708376440034478,
1.),(1.,0.707750498698437,1.),(1.,0.707106781186546,1.)))
REPRESENTATION_ITEM('')
SURFACE()
);
#3851=(
BOUNDED_SURFACE()
B_SPLINE_SURFACE(3,2,((#251708,#251709,#251710),(#251711,#251712,#251713),
(#251714,#251715,#251716),(#251717,#251718,#251719)),.UNSPECIFIED.,.F.,
 .F.,.F.)
B_SPLINE_SURFACE_WITH_KNOTS((4,4),(3,3),(-5.61074624261249E-18,0.000511815090126171),
(0.,1.00105592270005),.UNSPECIFIED.)
GEOMETRIC_REPRESENTATION_ITEM()
RATIONAL_B_SPLINE_SURFACE(((1.,0.705266242718099,1.00062243212957),(1.,
0.70558408590981,1.00062176089389),(1.,0.706182089451058,1.00062049800286),
(1.,0.706797508588123,1.00061919833279)))
REPRESENTATION_ITEM('')
SURFACE()
);
#3852=(
BOUNDED_SURFACE()
B_SPLINE_SURFACE(3,2,((#251721,#251722,#251723),(#251724,#251725,#251726),
(#251727,#251728,#251729),(#251730,#251731,#251732)),.UNSPECIFIED.,.F.,
 .F.,.F.)
B_SPLINE_SURFACE_WITH_KNOTS((4,4),(3,3),(-9.9475549325545E-18,0.000397394428086624),
(0.,1.),.UNSPECIFIED.)
GEOMETRIC_REPRESENTATION_ITEM()
RATIONAL_B_SPLINE_SURFACE(((1.,0.707106781186546,1.),(1.,0.706459846759125,
1.),(1.,0.705820510737227,1.),(1.,0.705498956110741,1.)))
REPRESENTATION_ITEM('')
SURFACE()
);
#3853=(
BOUNDED_SURFACE()
B_SPLINE_SURFACE(3,2,((#251738,#251739,#251740),(#251741,#251742,#251743),
(#251744,#251745,#251746),(#251747,#251748,#251749),(#251750,#251751,#251752),
(#251753,#251754,#251755)),.UNSPECIFIED.,.F.,.F.,.F.)
B_SPLINE_SURFACE_WITH_KNOTS((4,2,4),(3,3),(0.,0.000257953807872842,0.000515907615745685),
(0.,1.),.UNSPECIFIED.)
GEOMETRIC_REPRESENTATION_ITEM()
RATIONAL_B_SPLINE_SURFACE(((1.,0.87461970713939,1.),(1.,0.874834349679033,
1.),(1.,0.854686104157721,1.),(1.,0.792476597915213,1.),(1.,0.750887854595099,
1.),(1.,0.70558583803142,1.)))
REPRESENTATION_ITEM('')
SURFACE()
);
#3854=(
BOUNDED_SURFACE()
B_SPLINE_SURFACE(3,2,((#251761,#251762,#251763),(#251764,#251765,#251766),
(#251767,#251768,#251769),(#251770,#251771,#251772)),.UNSPECIFIED.,.F.,
 .F.,.F.)
B_SPLINE_SURFACE_WITH_KNOTS((4,4),(3,3),(0.,0.000511815437699156),(0.,1.0010588133186),
 .UNSPECIFIED.)
GEOMETRIC_REPRESENTATION_ITEM()
RATIONAL_B_SPLINE_SURFACE(((1.,0.70679666194554,1.00062089519878),(1.,0.707430821224428,
1.0006195522862),(1.,0.708058545829939,1.00061822299985),(1.,0.708394505251935,
1.00061751156323)))
REPRESENTATION_ITEM('')
SURFACE()
);
#3855=(
BOUNDED_SURFACE()
B_SPLINE_SURFACE(3,2,((#251774,#251775,#251776),(#251777,#251778,#251779),
(#251780,#251781,#251782),(#251783,#251784,#251785),(#251786,#251787,#251788),
(#251789,#251790,#251791)),.UNSPECIFIED.,.F.,.F.,.F.)
B_SPLINE_SURFACE_WITH_KNOTS((4,2,4),(3,3),(0.,0.000256915317531261,0.000513830635062522),
(0.,1.),.UNSPECIFIED.)
GEOMETRIC_REPRESENTATION_ITEM()
RATIONAL_B_SPLINE_SURFACE(((1.,0.705585838031441,1.),(1.,0.75090243354325,
1.),(1.,0.792329530081844,1.),(1.,0.854288401594898,1.),(1.,0.874998031124623,
1.),(1.,0.874619707139392,1.)))
REPRESENTATION_ITEM('')
SURFACE()
);
#3856=(
BOUNDED_SURFACE()
B_SPLINE_SURFACE(3,2,((#251797,#251798,#251799),(#251800,#251801,#251802),
(#251803,#251804,#251805),(#251806,#251807,#251808),(#251809,#251810,#251811),
(#251812,#251813,#251814)),.UNSPECIFIED.,.F.,.F.,.F.)
B_SPLINE_SURFACE_WITH_KNOTS((4,2,4),(3,3),(-1.00559751498031E-17,0.00025659281426215,
0.00051318562852431),(0.,1.),.UNSPECIFIED.)
GEOMETRIC_REPRESENTATION_ITEM()
RATIONAL_B_SPLINE_SURFACE(((1.,0.708712527163675,1.),(1.,0.753780902613865,
1.),(1.,0.79453899576883,1.),(1.,0.85507077033146,1.),(1.,0.875018427445065,
1.),(1.,0.874619707139397,1.)))
REPRESENTATION_ITEM('')
SURFACE()
);
#3857=(
BOUNDED_SURFACE()
B_SPLINE_SURFACE(3,2,((#251816,#251817,#251818),(#251819,#251820,#251821),
(#251822,#251823,#251824),(#251825,#251826,#251827)),.UNSPECIFIED.,.F.,
 .F.,.F.)
B_SPLINE_SURFACE_WITH_KNOTS((4,4),(3,3),(-5.23127548224256E-18,0.000511815072430389),
(0.,1.00105598365557),.UNSPECIFIED.)
GEOMETRIC_REPRESENTATION_ITEM()
RATIONAL_B_SPLINE_SURFACE(((1.,0.706797490734655,1.00061923411511),(1.,
0.706182062147555,1.00062053388017),(1.,0.705584062769966,1.00062179683531),
(1.,0.705266224771429,1.00062246809877)))
REPRESENTATION_ITEM('')
SURFACE()
);
#3858=(
BOUNDED_SURFACE()
B_SPLINE_SURFACE(3,2,((#251833,#251834,#251835),(#251836,#251837,#251838),
(#251839,#251840,#251841),(#251842,#251843,#251844),(#251845,#251846,#251847),
(#251848,#251849,#251850)),.UNSPECIFIED.,.F.,.F.,.F.)
B_SPLINE_SURFACE_WITH_KNOTS((4,2,4),(3,3),(0.,0.00025765223235088,0.00051530446470176),
(0.,1.),.UNSPECIFIED.)
GEOMETRIC_REPRESENTATION_ITEM()
RATIONAL_B_SPLINE_SURFACE(((1.,0.874619707139389,1.),(1.,0.874861180430388,
1.),(1.,0.8554557259213,1.),(1.,0.794699358954825,1.),(1.,0.753768977788989,
1.),(1.,0.708712527163643,1.)))
REPRESENTATION_ITEM('')
SURFACE()
);
#3859=(
BOUNDED_SURFACE()
B_SPLINE_SURFACE(3,2,((#251856,#251857,#251858),(#251859,#251860,#251861),
(#251862,#251863,#251864),(#251865,#251866,#251867)),.UNSPECIFIED.,.F.,
 .F.,.F.)
B_SPLINE_SURFACE_WITH_KNOTS((4,4),(3,3),(-1.46096242742422E-17,0.0003973943736519),
(0.,1.),.UNSPECIFIED.)
GEOMETRIC_REPRESENTATION_ITEM()
RATIONAL_B_SPLINE_SURFACE(((1.,0.707106781186549,1.),(1.,0.707752587915898,
1.),(1.,0.708377654540658,1.),(1.,0.708689770883325,1.)))
REPRESENTATION_ITEM('')
SURFACE()
);
#3860=(
BOUNDED_SURFACE()
B_SPLINE_SURFACE(3,2,((#251869,#251870,#251871),(#251872,#251873,#251874),
(#251875,#251876,#251877),(#251878,#251879,#251880)),.UNSPECIFIED.,.F.,
 .F.,.F.)
B_SPLINE_SURFACE_WITH_KNOTS((4,4),(3,3),(0.,0.000511815456479792),(0.,1.0010587315979),
 .UNSPECIFIED.)
GEOMETRIC_REPRESENTATION_ITEM()
RATIONAL_B_SPLINE_SURFACE(((1.,0.708394529056921,1.00061746385242),(1.,
0.708058564167515,1.00061817524571),(1.,0.7074308353726,1.00061950443833),
(1.,0.70679668588098,1.00062084722653)))
REPRESENTATION_ITEM('')
SURFACE()
);
#3861=(
BOUNDED_SURFACE()
B_SPLINE_SURFACE(3,2,((#251886,#251887,#251888),(#251889,#251890,#251891),
(#251892,#251893,#251894),(#251895,#251896,#251897)),.UNSPECIFIED.,.F.,
 .F.,.F.)
B_SPLINE_SURFACE_WITH_KNOTS((4,4),(3,3),(-4.06575814682064E-18,0.000397394465448297),
(0.,1.),.UNSPECIFIED.)
GEOMETRIC_REPRESENTATION_ITEM()
RATIONAL_B_SPLINE_SURFACE(((1.,0.705498956110766,1.),(1.,0.705821764811788,
1.),(1.,0.706461952521129,1.),(1.,0.707106781186549,1.)))
REPRESENTATION_ITEM('')
SURFACE()
);
#3862=(
BOUNDED_SURFACE()
B_SPLINE_SURFACE(3,2,((#251903,#251904,#251905),(#251906,#251907,#251908),
(#251909,#251910,#251911),(#251912,#251913,#251914)),.UNSPECIFIED.,.F.,
 .F.,.F.)
B_SPLINE_SURFACE_WITH_KNOTS((4,4),(3,3),(0.,0.000397394410828736),(0.,1.),
 .UNSPECIFIED.)
GEOMETRIC_REPRESENTATION_ITEM()
RATIONAL_B_SPLINE_SURFACE(((1.,0.708689770883297,1.),(1.,0.708376440034533,
1.),(1.,0.707750498698387,1.),(1.,0.707106781186545,1.)))
REPRESENTATION_ITEM('')
SURFACE()
);
#3863=(
BOUNDED_SURFACE()
B_SPLINE_SURFACE(3,2,((#251920,#251921,#251922),(#251923,#251924,#251925),
(#251926,#251927,#251928),(#251929,#251930,#251931)),.UNSPECIFIED.,.F.,
 .F.,.F.)
B_SPLINE_SURFACE_WITH_KNOTS((4,4),(3,3),(0.,0.000511815090126174),(0.,1.00105592270111),
 .UNSPECIFIED.)
GEOMETRIC_REPRESENTATION_ITEM()
RATIONAL_B_SPLINE_SURFACE(((1.,0.705266242717813,1.0006224321302),(1.,0.705584085909436,
1.00062176089451),(1.,0.706182089450826,1.00062049800348),(1.,0.706797508587798,
1.00061919833341)))
REPRESENTATION_ITEM('')
SURFACE()
);
#3864=(
BOUNDED_SURFACE()
B_SPLINE_SURFACE(3,2,((#251933,#251934,#251935),(#251936,#251937,#251938),
(#251939,#251940,#251941),(#251942,#251943,#251944)),.UNSPECIFIED.,.F.,
 .F.,.F.)
B_SPLINE_SURFACE_WITH_KNOTS((4,4),(3,3),(-1.05167610731094E-17,0.000397394428086628),
(0.,1.),.UNSPECIFIED.)
GEOMETRIC_REPRESENTATION_ITEM()
RATIONAL_B_SPLINE_SURFACE(((1.,0.707106781186545,1.),(1.,0.706459846759091,
1.),(1.,0.705820510737279,1.),(1.,0.705498956110751,1.)))
REPRESENTATION_ITEM('')
SURFACE()
);
#3865=(
BOUNDED_SURFACE()
B_SPLINE_SURFACE(3,2,((#251950,#251951,#251952),(#251953,#251954,#251955),
(#251956,#251957,#251958),(#251959,#251960,#251961),(#251962,#251963,#251964),
(#251965,#251966,#251967)),.UNSPECIFIED.,.F.,.F.,.F.)
B_SPLINE_SURFACE_WITH_KNOTS((4,2,4),(3,3),(0.,0.000257953807872849,0.000515907615745697),
(0.,1.),.UNSPECIFIED.)
GEOMETRIC_REPRESENTATION_ITEM()
RATIONAL_B_SPLINE_SURFACE(((1.,0.874619707139396,1.),(1.,0.874834349678808,
1.),(1.,0.854686104158024,1.),(1.,0.792476597914919,1.),(1.,0.750887854595303,
1.),(1.,0.705585838031442,1.)))
REPRESENTATION_ITEM('')
SURFACE()
);
#3866=(
BOUNDED_SURFACE()
B_SPLINE_SURFACE(3,2,((#251973,#251974,#251975),(#251976,#251977,#251978),
(#251979,#251980,#251981),(#251982,#251983,#251984)),.UNSPECIFIED.,.F.,
 .F.,.F.)
B_SPLINE_SURFACE_WITH_KNOTS((4,4),(3,3),(5.6920614055489E-19,0.000511815437699157),
(0.,1.00105881331715),.UNSPECIFIED.)
GEOMETRIC_REPRESENTATION_ITEM()
RATIONAL_B_SPLINE_SURFACE(((1.,0.706796661945948,1.00062089519793),(1.,
0.70743082122483,1.00061955228535),(1.,0.708058545830374,1.00061822299901),
(1.,0.708394505252341,1.00061751156239)))
REPRESENTATION_ITEM('')
SURFACE()
);
#3867=(
BOUNDED_SURFACE()
B_SPLINE_SURFACE(3,2,((#251986,#251987,#251988),(#251989,#251990,#251991),
(#251992,#251993,#251994),(#251995,#251996,#251997),(#251998,#251999,#252000),
(#252001,#252002,#252003)),.UNSPECIFIED.,.F.,.F.,.F.)
B_SPLINE_SURFACE_WITH_KNOTS((4,2,4),(3,3),(2.71050543121376E-20,0.000256915317531263,
0.000513830635062525),(0.,1.),.UNSPECIFIED.)
GEOMETRIC_REPRESENTATION_ITEM()
RATIONAL_B_SPLINE_SURFACE(((1.,0.705585838031425,1.),(1.,0.750902433542554,
1.),(1.,0.792329530082784,1.),(1.,0.854288401593908,1.),(1.,0.87499803112535,
1.),(1.,0.874619707139389,1.)))
REPRESENTATION_ITEM('')
SURFACE()
);
#3868=(
BOUNDED_SURFACE()
B_SPLINE_SURFACE(3,2,((#252009,#252010,#252011),(#252012,#252013,#252014),
(#252015,#252016,#252017),(#252018,#252019,#252020),(#252021,#252022,#252023),
(#252024,#252025,#252026)),.UNSPECIFIED.,.F.,.F.,.F.)
B_SPLINE_SURFACE_WITH_KNOTS((4,2,4),(3,3),(-2.16840434497101E-18,0.000256592814262163,
0.000513185628524328),(0.,1.),.UNSPECIFIED.)
GEOMETRIC_REPRESENTATION_ITEM()
RATIONAL_B_SPLINE_SURFACE(((1.,0.708712527163658,1.),(1.,0.753780902613584,
1.),(1.,0.794538995769163,1.),(1.,0.855070770331154,1.),(1.,0.875018427445297,
1.),(1.,0.874619707139398,1.)))
REPRESENTATION_ITEM('')
SURFACE()
);
#3869=(
BOUNDED_SURFACE()
B_SPLINE_SURFACE(3,2,((#252028,#252029,#252030),(#252031,#252032,#252033),
(#252034,#252035,#252036),(#252037,#252038,#252039)),.UNSPECIFIED.,.F.,
 .F.,.F.)
B_SPLINE_SURFACE_WITH_KNOTS((4,4),(3,3),(-5.80048162279745E-18,0.000511815072430405),
(0.,1.00105598365882),.UNSPECIFIED.)
GEOMETRIC_REPRESENTATION_ITEM()
RATIONAL_B_SPLINE_SURFACE(((1.,0.706797490733704,1.00061923411702),(1.,
0.706182062146584,1.00062053388208),(1.,0.705584062769038,1.00062179683722),
(1.,0.705266224770424,1.00062246810069)))
REPRESENTATION_ITEM('')
SURFACE()
);
#3870=(
BOUNDED_SURFACE()
B_SPLINE_SURFACE(3,2,((#252045,#252046,#252047),(#252048,#252049,#252050),
(#252051,#252052,#252053),(#252054,#252055,#252056),(#252057,#252058,#252059),
(#252060,#252061,#252062)),.UNSPECIFIED.,.F.,.F.,.F.)
B_SPLINE_SURFACE_WITH_KNOTS((4,2,4),(3,3),(1.35525271560688E-20,0.000257652232350883,
0.000515304464701766),(0.,1.),.UNSPECIFIED.)
GEOMETRIC_REPRESENTATION_ITEM()
RATIONAL_B_SPLINE_SURFACE(((1.,0.874619707139396,1.),(1.,0.874861180430779,
1.),(1.,0.855455725920777,1.),(1.,0.794699358955354,1.),(1.,0.753768977788557,
1.),(1.,0.708712527163675,1.)))
REPRESENTATION_ITEM('')
SURFACE()
);
#3871=(
BOUNDED_SURFACE()
B_SPLINE_SURFACE(3,2,((#252068,#252069,#252070),(#252071,#252072,#252073),
(#252074,#252075,#252076),(#252077,#252078,#252079)),.UNSPECIFIED.,.F.,
 .F.,.F.)
B_SPLINE_SURFACE_WITH_KNOTS((4,4),(3,3),(0.,0.000397394373651912),(0.,1.),
 .UNSPECIFIED.)
GEOMETRIC_REPRESENTATION_ITEM()
RATIONAL_B_SPLINE_SURFACE(((1.,0.707106781186537,1.),(1.,0.707752587915915,
1.),(1.,0.708377654540671,1.),(1.,0.708689770883328,1.)))
REPRESENTATION_ITEM('')
SURFACE()
);
#3872=(
BOUNDED_SURFACE()
B_SPLINE_SURFACE(3,2,((#252081,#252082,#252083),(#252084,#252085,#252086),
(#252087,#252088,#252089),(#252090,#252091,#252092)),.UNSPECIFIED.,.F.,
 .F.,.F.)
B_SPLINE_SURFACE_WITH_KNOTS((4,4),(3,3),(0.,0.000511815456479782),(0.,1.00105873159953),
 .UNSPECIFIED.)
GEOMETRIC_REPRESENTATION_ITEM()
RATIONAL_B_SPLINE_SURFACE(((1.,0.708394529056449,1.00061746385337),(1.,
0.708058564167009,1.00061817524665),(1.,0.707430835372194,1.00061950443928),
(1.,0.706796685880505,1.00062084722749)))
REPRESENTATION_ITEM('')
SURFACE()
);
#3873=(
BOUNDED_SURFACE()
B_SPLINE_SURFACE(3,2,((#252098,#252099,#252100),(#252101,#252102,#252103),
(#252104,#252105,#252106),(#252107,#252108,#252109)),.UNSPECIFIED.,.F.,
 .F.,.F.)
B_SPLINE_SURFACE_WITH_KNOTS((4,4),(3,3),(0.,0.000397394465448306),(0.,1.),
 .UNSPECIFIED.)
GEOMETRIC_REPRESENTATION_ITEM()
RATIONAL_B_SPLINE_SURFACE(((1.,0.705498956110769,1.),(1.,0.705821764811784,
1.),(1.,0.70646195252113,1.),(1.,0.70710678118655,1.)))
REPRESENTATION_ITEM('')
SURFACE()
);
#3874=(
BOUNDED_SURFACE()
B_SPLINE_SURFACE(3,2,((#252115,#252116,#252117),(#252118,#252119,#252120),
(#252121,#252122,#252123),(#252124,#252125,#252126)),.UNSPECIFIED.,.F.,
 .F.,.F.)
B_SPLINE_SURFACE_WITH_KNOTS((4,4),(3,3),(0.,0.000397394410828744),(0.,1.),
 .UNSPECIFIED.)
GEOMETRIC_REPRESENTATION_ITEM()
RATIONAL_B_SPLINE_SURFACE(((1.,0.708689770883331,1.),(1.,0.708376440034484,
1.),(1.,0.707750498698425,1.),(1.,0.707106781186545,1.)))
REPRESENTATION_ITEM('')
SURFACE()
);
#3875=(
BOUNDED_SURFACE()
B_SPLINE_SURFACE(3,2,((#252132,#252133,#252134),(#252135,#252136,#252137),
(#252138,#252139,#252140),(#252141,#252142,#252143)),.UNSPECIFIED.,.F.,
 .F.,.F.)
B_SPLINE_SURFACE_WITH_KNOTS((4,4),(3,3),(0.,0.000511815090126181),(0.,1.00105592270294),
 .UNSPECIFIED.)
GEOMETRIC_REPRESENTATION_ITEM()
RATIONAL_B_SPLINE_SURFACE(((1.,0.70526624271726,1.00062243213127),(1.,0.705584085908922,
1.00062176089559),(1.,0.706182089450262,1.00062049800456),(1.,0.706797508587264,
1.00061919833448)))
REPRESENTATION_ITEM('')
SURFACE()
);
#3876=(
BOUNDED_SURFACE()
B_SPLINE_SURFACE(3,2,((#252145,#252146,#252147),(#252148,#252149,#252150),
(#252151,#252152,#252153),(#252154,#252155,#252156)),.UNSPECIFIED.,.F.,
 .F.,.F.)
B_SPLINE_SURFACE_WITH_KNOTS((4,4),(3,3),(-6.50521303491303E-19,0.000397394428086628),
(0.,1.),.UNSPECIFIED.)
GEOMETRIC_REPRESENTATION_ITEM()
RATIONAL_B_SPLINE_SURFACE(((1.,0.707106781186545,1.),(1.,0.706459846759103,
1.),(1.,0.705820510737279,1.),(1.,0.705498956110742,1.)))
REPRESENTATION_ITEM('')
SURFACE()
);
#3877=(
BOUNDED_SURFACE()
B_SPLINE_SURFACE(3,2,((#252162,#252163,#252164),(#252165,#252166,#252167),
(#252168,#252169,#252170),(#252171,#252172,#252173),(#252174,#252175,#252176),
(#252177,#252178,#252179)),.UNSPECIFIED.,.F.,.F.,.F.)
B_SPLINE_SURFACE_WITH_KNOTS((4,2,4),(3,3),(-1.03947883287048E-17,0.000257953807872844,
0.000515907615745698),(0.,1.),.UNSPECIFIED.)
GEOMETRIC_REPRESENTATION_ITEM()
RATIONAL_B_SPLINE_SURFACE(((1.,0.874619707139394,1.),(1.,0.874834349678638,
1.),(1.,0.85468610415827,1.),(1.,0.792476597914672,1.),(1.,0.750887854595475,
1.),(1.,0.705585838031437,1.)))
REPRESENTATION_ITEM('')
SURFACE()
);
#3878=(
BOUNDED_SURFACE()
B_SPLINE_SURFACE(3,2,((#252185,#252186,#252187),(#252188,#252189,#252190),
(#252191,#252192,#252193),(#252194,#252195,#252196)),.UNSPECIFIED.,.F.,
 .F.,.F.)
B_SPLINE_SURFACE_WITH_KNOTS((4,4),(3,3),(0.,0.000511815437699158),(0.,1.00105881331704),
 .UNSPECIFIED.)
GEOMETRIC_REPRESENTATION_ITEM()
RATIONAL_B_SPLINE_SURFACE(((1.,0.706796661945995,1.00062089519786),(1.,
0.707430821224872,1.00061955228528),(1.,0.70805854583039,1.00061822299894),
(1.,0.708394505252366,1.00061751156232)))
REPRESENTATION_ITEM('')
SURFACE()
);
#3879=(
BOUNDED_SURFACE()
B_SPLINE_SURFACE(3,2,((#252198,#252199,#252200),(#252201,#252202,#252203),
(#252204,#252205,#252206),(#252207,#252208,#252209),(#252210,#252211,#252212),
(#252213,#252214,#252215)),.UNSPECIFIED.,.F.,.F.,.F.)
B_SPLINE_SURFACE_WITH_KNOTS((4,2,4),(3,3),(-1.43656787854329E-18,0.000256915317531251,
0.000513830635062504),(0.,1.),.UNSPECIFIED.)
GEOMETRIC_REPRESENTATION_ITEM()
RATIONAL_B_SPLINE_SURFACE(((1.,0.705585838031439,1.),(1.,0.750902433542744,
1.),(1.,0.792329530082503,1.),(1.,0.854288401594159,1.),(1.,0.874998031125173,
1.),(1.,0.874619707139391,1.)))
REPRESENTATION_ITEM('')
SURFACE()
);
#3880=(
BOUNDED_SURFACE()
B_SPLINE_SURFACE(3,2,((#252221,#252222,#252223),(#252224,#252225,#252226),
(#252227,#252228,#252229),(#252230,#252231,#252232),(#252233,#252234,#252235),
(#252236,#252237,#252238)),.UNSPECIFIED.,.F.,.F.,.F.)
B_SPLINE_SURFACE_WITH_KNOTS((4,2,4),(3,3),(-1.14654379740342E-17,0.000256592814262148,
0.000513185628524307),(0.,1.),.UNSPECIFIED.)
GEOMETRIC_REPRESENTATION_ITEM()
RATIONAL_B_SPLINE_SURFACE(((1.,0.708712527163693,1.),(1.,0.753780902613078,
1.),(1.,0.794538995769877,1.),(1.,0.855070770330416,1.),(1.,0.875018427445857,
1.),(1.,0.874619707139392,1.)))
REPRESENTATION_ITEM('')
SURFACE()
);
#3881=(
BOUNDED_SURFACE()
B_SPLINE_SURFACE(3,2,((#252240,#252241,#252242),(#252243,#252244,#252245),
(#252246,#252247,#252248),(#252249,#252250,#252251)),.UNSPECIFIED.,.F.,
 .F.,.F.)
B_SPLINE_SURFACE_WITH_KNOTS((4,4),(3,3),(-6.26126754610379E-18,0.000511815072430392),
(0.,1.00105598366083),.UNSPECIFIED.)
GEOMETRIC_REPRESENTATION_ITEM()
RATIONAL_B_SPLINE_SURFACE(((1.,0.706797490733103,1.0006192341182),(1.,0.706182062146034,
1.00062053388327),(1.,0.705584062768406,1.00062179683841),(1.,0.705266224769873,
1.00062246810188)))
REPRESENTATION_ITEM('')
SURFACE()
);
#3882=(
BOUNDED_SURFACE()
B_SPLINE_SURFACE(3,2,((#252257,#252258,#252259),(#252260,#252261,#252262),
(#252263,#252264,#252265),(#252266,#252267,#252268),(#252269,#252270,#252271),
(#252272,#252273,#252274)),.UNSPECIFIED.,.F.,.F.,.F.)
B_SPLINE_SURFACE_WITH_KNOTS((4,2,4),(3,3),(-5.42101086242752E-20,0.000257652232350875,
0.00051530446470175),(0.,1.),.UNSPECIFIED.)
GEOMETRIC_REPRESENTATION_ITEM()
RATIONAL_B_SPLINE_SURFACE(((1.,0.874619707139402,1.),(1.,0.874861180430557,
1.),(1.,0.855455725921085,1.),(1.,0.794699358955079,1.),(1.,0.753768977788781,
1.),(1.,0.708712527163674,1.)))
REPRESENTATION_ITEM('')
SURFACE()
);
#3883=(
BOUNDED_SURFACE()
B_SPLINE_SURFACE(3,2,((#252280,#252281,#252282),(#252283,#252284,#252285),
(#252286,#252287,#252288),(#252289,#252290,#252291)),.UNSPECIFIED.,.F.,
 .F.,.F.)
B_SPLINE_SURFACE_WITH_KNOTS((4,4),(3,3),(0.,0.000397394373651914),(0.,1.),
 .UNSPECIFIED.)
GEOMETRIC_REPRESENTATION_ITEM()
RATIONAL_B_SPLINE_SURFACE(((1.,0.70710678118655,1.),(1.,0.707752587915891,
1.),(1.,0.708377654540695,1.),(1.,0.708689770883321,1.)))
REPRESENTATION_ITEM('')
SURFACE()
);
#3884=(
BOUNDED_SURFACE()
B_SPLINE_SURFACE(3,2,((#252293,#252294,#252295),(#252296,#252297,#252298),
(#252299,#252300,#252301),(#252302,#252303,#252304)),.UNSPECIFIED.,.F.,
 .F.,.F.)
B_SPLINE_SURFACE_WITH_KNOTS((4,4),(3,3),(0.,0.000511815456479786),(0.,1.00105873160046),
 .UNSPECIFIED.)
GEOMETRIC_REPRESENTATION_ITEM()
RATIONAL_B_SPLINE_SURFACE(((1.,0.708394529056175,1.00061746385391),(1.,
0.708058564166742,1.0006181752472),(1.,0.707430835371885,1.00061950443983),
(1.,0.70679668588023,1.00062084722804)))
REPRESENTATION_ITEM('')
SURFACE()
);
#3885=(
BOUNDED_SURFACE()
B_SPLINE_SURFACE(3,2,((#252310,#252311,#252312),(#252313,#252314,#252315),
(#252316,#252317,#252318),(#252319,#252320,#252321)),.UNSPECIFIED.,.F.,
 .F.,.F.)
B_SPLINE_SURFACE_WITH_KNOTS((4,4),(3,3),(-7.31836466427715E-18,0.0003973944654483),
(0.,1.),.UNSPECIFIED.)
GEOMETRIC_REPRESENTATION_ITEM()
RATIONAL_B_SPLINE_SURFACE(((1.,0.705498956110778,1.),(1.,0.705821764811775,
1.),(1.,0.706461952521157,1.),(1.,0.70710678118655,1.)))
REPRESENTATION_ITEM('')
SURFACE()
);
#3886=(
BOUNDED_SURFACE()
B_SPLINE_SURFACE(3,2,((#252327,#252328,#252329),(#252330,#252331,#252332),
(#252333,#252334,#252335),(#252336,#252337,#252338)),.UNSPECIFIED.,.F.,
 .F.,.F.)
B_SPLINE_SURFACE_WITH_KNOTS((4,4),(3,3),(5.96311194867027E-19,0.000397394410828737),
(0.,1.),.UNSPECIFIED.)
GEOMETRIC_REPRESENTATION_ITEM()
RATIONAL_B_SPLINE_SURFACE(((1.,0.708689770883353,1.),(1.,0.70837644003448,
1.),(1.,0.707750498698424,1.),(1.,0.707106781186537,1.)))
REPRESENTATION_ITEM('')
SURFACE()
);
#3887=(
BOUNDED_SURFACE()
B_SPLINE_SURFACE(3,2,((#252344,#252345,#252346),(#252347,#252348,#252349),
(#252350,#252351,#252352),(#252353,#252354,#252355)),.UNSPECIFIED.,.F.,
 .F.,.F.)
B_SPLINE_SURFACE_WITH_KNOTS((4,4),(3,3),(0.,0.000511815090126187),(0.,1.00105592270198),
 .UNSPECIFIED.)
GEOMETRIC_REPRESENTATION_ITEM()
RATIONAL_B_SPLINE_SURFACE(((1.,0.705266242717543,1.00062243213071),(1.,
0.705584085909212,1.00062176089503),(1.,0.706182089450554,1.000620498004),
(1.,0.706797508587552,1.00061919833392)))
REPRESENTATION_ITEM('')
SURFACE()
);
#3888=(
BOUNDED_SURFACE()
B_SPLINE_SURFACE(3,2,((#252357,#252358,#252359),(#252360,#252361,#252362),
(#252363,#252364,#252365),(#252366,#252367,#252368)),.UNSPECIFIED.,.F.,
 .F.,.F.)
B_SPLINE_SURFACE_WITH_KNOTS((4,4),(3,3),(-1.75098650856409E-17,0.000397394428086613),
(0.,1.),.UNSPECIFIED.)
GEOMETRIC_REPRESENTATION_ITEM()
RATIONAL_B_SPLINE_SURFACE(((1.,0.707106781186552,1.),(1.,0.706459846759093,
1.),(1.,0.705820510737281,1.),(1.,0.705498956110746,1.)))
REPRESENTATION_ITEM('')
SURFACE()
);
#3889=(
BOUNDED_SURFACE()
B_SPLINE_SURFACE(3,2,((#252374,#252375,#252376),(#252377,#252378,#252379),
(#252380,#252381,#252382),(#252383,#252384,#252385),(#252386,#252387,#252388),
(#252389,#252390,#252391)),.UNSPECIFIED.,.F.,.F.,.F.)
B_SPLINE_SURFACE_WITH_KNOTS((4,2,4),(3,3),(0.,0.00025795380787285,0.0005159076157457),
(0.,1.),.UNSPECIFIED.)
GEOMETRIC_REPRESENTATION_ITEM()
RATIONAL_B_SPLINE_SURFACE(((1.,0.874619707139391,1.),(1.,0.874834349679644,
1.),(1.,0.854686104156943,1.),(1.,0.792476597916,1.),(1.,0.750887854594491,
1.),(1.,0.705585838031437,1.)))
REPRESENTATION_ITEM('')
SURFACE()
);
#3890=(
BOUNDED_SURFACE()
B_SPLINE_SURFACE(3,2,((#252397,#252398,#252399),(#252400,#252401,#252402),
(#252403,#252404,#252405),(#252406,#252407,#252408)),.UNSPECIFIED.,.F.,
 .F.,.F.)
B_SPLINE_SURFACE_WITH_KNOTS((4,4),(3,3),(0.,0.000511815437699156),(0.,1.00105881331732),
 .UNSPECIFIED.)
GEOMETRIC_REPRESENTATION_ITEM()
RATIONAL_B_SPLINE_SURFACE(((1.,0.706796661945905,1.00062089519803),(1.,
0.707430821224792,1.00061955228545),(1.,0.708058545830336,1.0006182229991),
(1.,0.708394505252305,1.00061751156248)))
REPRESENTATION_ITEM('')
SURFACE()
);
#3891=(
BOUNDED_SURFACE()
B_SPLINE_SURFACE(3,2,((#252410,#252411,#252412),(#252413,#252414,#252415),
(#252416,#252417,#252418),(#252419,#252420,#252421),(#252422,#252423,#252424),
(#252425,#252426,#252427)),.UNSPECIFIED.,.F.,.F.,.F.)
B_SPLINE_SURFACE_WITH_KNOTS((4,2,4),(3,3),(0.,0.000256915317531267,0.000513830635062535),
(0.,1.),.UNSPECIFIED.)
GEOMETRIC_REPRESENTATION_ITEM()
RATIONAL_B_SPLINE_SURFACE(((1.,0.70558583803144,1.),(1.,0.750902433541966,
1.),(1.,0.792329530083573,1.),(1.,0.854288401593169,1.),(1.,0.874998031125916,
1.),(1.,0.874619707139415,1.)))
REPRESENTATION_ITEM('')
SURFACE()
);
#3892=(
BOUNDED_SURFACE()
B_SPLINE_SURFACE(3,2,((#252433,#252434,#252435),(#252436,#252437,#252438),
(#252439,#252440,#252441),(#252442,#252443,#252444),(#252445,#252446,#252447),
(#252448,#252449,#252450)),.UNSPECIFIED.,.F.,.F.,.F.)
B_SPLINE_SURFACE_WITH_KNOTS((4,2,4),(3,3),(-4.68917439599981E-18,0.000256592814262156,
0.000513185628524317),(0.,1.),.UNSPECIFIED.)
GEOMETRIC_REPRESENTATION_ITEM()
RATIONAL_B_SPLINE_SURFACE(((1.,0.70871252716367,1.),(1.,0.753780902613218,
1.),(1.,0.794538995769711,1.),(1.,0.855070770330604,1.),(1.,0.87501842744571,
1.),(1.,0.874619707139392,1.)))
REPRESENTATION_ITEM('')
SURFACE()
);
#3893=(
BOUNDED_SURFACE()
B_SPLINE_SURFACE(3,2,((#252452,#252453,#252454),(#252455,#252456,#252457),
(#252458,#252459,#252460),(#252461,#252462,#252463)),.UNSPECIFIED.,.F.,
 .F.,.F.)
B_SPLINE_SURFACE_WITH_KNOTS((4,4),(3,3),(0.,0.000511815072430404),(0.,1.00105598365879),
 .UNSPECIFIED.)
GEOMETRIC_REPRESENTATION_ITEM()
RATIONAL_B_SPLINE_SURFACE(((1.,0.706797490733712,1.000619234117),(1.,0.706182062146633,
1.00062053388207),(1.,0.705584062768981,1.00062179683721),(1.,0.705266224770493,
1.00062246810067)))
REPRESENTATION_ITEM('')
SURFACE()
);
#3894=(
BOUNDED_SURFACE()
B_SPLINE_SURFACE(3,2,((#252469,#252470,#252471),(#252472,#252473,#252474),
(#252475,#252476,#252477),(#252478,#252479,#252480),(#252481,#252482,#252483),
(#252484,#252485,#252486)),.UNSPECIFIED.,.F.,.F.,.F.)
B_SPLINE_SURFACE_WITH_KNOTS((4,2,4),(3,3),(0.,0.000257652232350885,0.000515304464701769),
(0.,1.),.UNSPECIFIED.)
GEOMETRIC_REPRESENTATION_ITEM()
RATIONAL_B_SPLINE_SURFACE(((1.,0.87461970713938,1.),(1.,0.874861180430577,
1.),(1.,0.855455725921031,1.),(1.,0.794699358955064,1.),(1.,0.753768977788782,
1.),(1.,0.708712527163652,1.)))
REPRESENTATION_ITEM('')
SURFACE()
);
#3895=(
BOUNDED_SURFACE()
B_SPLINE_SURFACE(3,2,((#252492,#252493,#252494),(#252495,#252496,#252497),
(#252498,#252499,#252500),(#252501,#252502,#252503)),.UNSPECIFIED.,.F.,
 .F.,.F.)
B_SPLINE_SURFACE_WITH_KNOTS((4,4),(3,3),(0.,0.000397394373651918),(0.,1.),
 .UNSPECIFIED.)
GEOMETRIC_REPRESENTATION_ITEM()
RATIONAL_B_SPLINE_SURFACE(((1.,0.707106781186561,1.),(1.,0.707752587915879,
1.),(1.,0.708377654540666,1.),(1.,0.708689770883339,1.)))
REPRESENTATION_ITEM('')
SURFACE()
);
#3896=(
BOUNDED_SURFACE()
B_SPLINE_SURFACE(3,2,((#252505,#252506,#252507),(#252508,#252509,#252510),
(#252511,#252512,#252513),(#252514,#252515,#252516)),.UNSPECIFIED.,.F.,
 .F.,.F.)
B_SPLINE_SURFACE_WITH_KNOTS((4,4),(3,3),(0.,0.000511815456479793),(0.,1.00105873159869),
 .UNSPECIFIED.)
GEOMETRIC_REPRESENTATION_ITEM()
RATIONAL_B_SPLINE_SURFACE(((1.,0.708394529056689,1.00061746385288),(1.,
0.70805856416725,1.00061817524616),(1.,0.707430835372447,1.00061950443879),
(1.,0.706796685880741,1.000620847227)))
REPRESENTATION_ITEM('')
SURFACE()
);
#3897=(
BOUNDED_SURFACE()
B_SPLINE_SURFACE(3,2,((#252522,#252523,#252524),(#252525,#252526,#252527),
(#252528,#252529,#252530),(#252531,#252532,#252533)),.UNSPECIFIED.,.F.,
 .F.,.F.)
B_SPLINE_SURFACE_WITH_KNOTS((4,4),(3,3),(-5.96311194867027E-19,0.00039739446544832),
(0.,1.),.UNSPECIFIED.)
GEOMETRIC_REPRESENTATION_ITEM()
RATIONAL_B_SPLINE_SURFACE(((1.,0.705498956110792,1.),(1.,0.705821764811748,
1.),(1.,0.706461952521157,1.),(1.,0.70710678118655,1.)))
REPRESENTATION_ITEM('')
SURFACE()
);
#3898=(
BOUNDED_SURFACE()
B_SPLINE_SURFACE(3,2,((#252539,#252540,#252541),(#252542,#252543,#252544),
(#252545,#252546,#252547),(#252548,#252549,#252550)),.UNSPECIFIED.,.F.,
 .F.,.F.)
B_SPLINE_SURFACE_WITH_KNOTS((4,4),(3,3),(4.87890977618477E-19,0.000397394410828737),
(0.,1.),.UNSPECIFIED.)
GEOMETRIC_REPRESENTATION_ITEM()
RATIONAL_B_SPLINE_SURFACE(((1.,0.708689770883312,1.),(1.,0.708376440034555,
1.),(1.,0.707750498698384,1.),(1.,0.707106781186545,1.)))
REPRESENTATION_ITEM('')
SURFACE()
);
#3899=(
BOUNDED_SURFACE()
B_SPLINE_SURFACE(3,2,((#252556,#252557,#252558),(#252559,#252560,#252561),
(#252562,#252563,#252564),(#252565,#252566,#252567)),.UNSPECIFIED.,.F.,
 .F.,.F.)
B_SPLINE_SURFACE_WITH_KNOTS((4,4),(3,3),(0.,0.000511815090126186),(0.,1.00105592270295),
 .UNSPECIFIED.)
GEOMETRIC_REPRESENTATION_ITEM()
RATIONAL_B_SPLINE_SURFACE(((1.,0.705266242717264,1.00062243213128),(1.,
0.705584085908904,1.0006217608956),(1.,0.706182089450258,1.00062049800456),
(1.,0.706797508587261,1.00061919833449)))
REPRESENTATION_ITEM('')
SURFACE()
);
#3900=(
BOUNDED_SURFACE()
B_SPLINE_SURFACE(3,2,((#252569,#252570,#252571),(#252572,#252573,#252574),
(#252575,#252576,#252577),(#252578,#252579,#252580)),.UNSPECIFIED.,.F.,
 .F.,.F.)
B_SPLINE_SURFACE_WITH_KNOTS((4,4),(3,3),(-7.83336069620777E-18,0.000397394428086622),
(0.,1.),.UNSPECIFIED.)
GEOMETRIC_REPRESENTATION_ITEM()
RATIONAL_B_SPLINE_SURFACE(((1.,0.707106781186536,1.),(1.,0.70645984675912,
1.),(1.,0.705820510737251,1.),(1.,0.70549895611074,1.)))
REPRESENTATION_ITEM('')
SURFACE()
);
#3901=(
BOUNDED_SURFACE()
B_SPLINE_SURFACE(3,2,((#252586,#252587,#252588),(#252589,#252590,#252591),
(#252592,#252593,#252594),(#252595,#252596,#252597),(#252598,#252599,#252600),
(#252601,#252602,#252603)),.UNSPECIFIED.,.F.,.F.,.F.)
B_SPLINE_SURFACE_WITH_KNOTS((4,2,4),(3,3),(0.,0.000257953807872848,0.000515907615745697),
(0.,1.),.UNSPECIFIED.)
GEOMETRIC_REPRESENTATION_ITEM()
RATIONAL_B_SPLINE_SURFACE(((1.,0.874619707139394,1.),(1.,0.874834349679261,
1.),(1.,0.854686104157444,1.),(1.,0.792476597915463,1.),(1.,0.75088785459489,
1.),(1.,0.705585838031425,1.)))
REPRESENTATION_ITEM('')
SURFACE()
);
#3902=(
BOUNDED_SURFACE()
B_SPLINE_SURFACE(3,2,((#252609,#252610,#252611),(#252612,#252613,#252614),
(#252615,#252616,#252617),(#252618,#252619,#252620)),.UNSPECIFIED.,.F.,
 .F.,.F.)
B_SPLINE_SURFACE_WITH_KNOTS((4,4),(3,3),(0.,0.000511815437699154),(0.,1.00105881331701),
 .UNSPECIFIED.)
GEOMETRIC_REPRESENTATION_ITEM()
RATIONAL_B_SPLINE_SURFACE(((1.,0.706796661945988,1.00062089519784),(1.,
0.707430821224899,1.00061955228526),(1.,0.708058545830382,1.00061822299892),
(1.,0.708394505252395,1.0006175115623)))
REPRESENTATION_ITEM('')
SURFACE()
);
#3903=(
BOUNDED_SURFACE()
B_SPLINE_SURFACE(3,2,((#252622,#252623,#252624),(#252625,#252626,#252627),
(#252628,#252629,#252630),(#252631,#252632,#252633),(#252634,#252635,#252636),
(#252637,#252638,#252639)),.UNSPECIFIED.,.F.,.F.,.F.)
B_SPLINE_SURFACE_WITH_KNOTS((4,2,4),(3,3),(-1.35525271560688E-18,0.000256915317531253,
0.000513830635062508),(0.,1.),.UNSPECIFIED.)
GEOMETRIC_REPRESENTATION_ITEM()
RATIONAL_B_SPLINE_SURFACE(((1.,0.705585838031429,1.),(1.,0.750902433542525,
1.),(1.,0.792329530082822,1.),(1.,0.854288401593897,1.),(1.,0.874998031125356,
1.),(1.,0.87461970713939,1.)))
REPRESENTATION_ITEM('')
SURFACE()
);
#3904=(
BOUNDED_SURFACE()
B_SPLINE_SURFACE(3,2,((#252645,#252646,#252647),(#252648,#252649,#252650),
(#252651,#252652,#252653),(#252654,#252655,#252656),(#252657,#252658,#252659),
(#252660,#252661,#252662)),.UNSPECIFIED.,.F.,.F.,.F.)
B_SPLINE_SURFACE_WITH_KNOTS((4,2,4),(3,3),(-5.06864515636973E-18,0.000256592814262158,
0.00051318562852432),(0.,1.),.UNSPECIFIED.)
GEOMETRIC_REPRESENTATION_ITEM()
RATIONAL_B_SPLINE_SURFACE(((1.,0.708712527163671,1.),(1.,0.753780902613968,
1.),(1.,0.794538995768688,1.),(1.,0.855070770331595,1.),(1.,0.87501842744497,
1.),(1.,0.874619707139396,1.)))
REPRESENTATION_ITEM('')
SURFACE()
);
#3905=(
BOUNDED_SURFACE()
B_SPLINE_SURFACE(3,2,((#252664,#252665,#252666),(#252667,#252668,#252669),
(#252670,#252671,#252672),(#252673,#252674,#252675)),.UNSPECIFIED.,.F.,
 .F.,.F.)
B_SPLINE_SURFACE_WITH_KNOTS((4,4),(3,3),(0.,0.000511815072430407),(0.,1.0010559836599),
 .UNSPECIFIED.)
GEOMETRIC_REPRESENTATION_ITEM()
RATIONAL_B_SPLINE_SURFACE(((1.,0.706797490733387,1.00061923411766),(1.,
0.706182062146288,1.00062053388272),(1.,0.705584062768689,1.00062179683786),
(1.,0.705266224770146,1.00062246810133)))
REPRESENTATION_ITEM('')
SURFACE()
);
#3906=(
BOUNDED_SURFACE()
B_SPLINE_SURFACE(3,2,((#252681,#252682,#252683),(#252684,#252685,#252686),
(#252687,#252688,#252689),(#252690,#252691,#252692),(#252693,#252694,#252695),
(#252696,#252697,#252698)),.UNSPECIFIED.,.F.,.F.,.F.)
B_SPLINE_SURFACE_WITH_KNOTS((4,2,4),(3,3),(-3.06287113727155E-18,0.000257652232350878,
0.000515304464701758),(0.,1.),.UNSPECIFIED.)
GEOMETRIC_REPRESENTATION_ITEM()
RATIONAL_B_SPLINE_SURFACE(((1.,0.874619707139395,1.),(1.,0.874861180430859,
1.),(1.,0.85545572592067,1.),(1.,0.794699358955482,1.),(1.,0.753768977788507,
1.),(1.,0.708712527163654,1.)))
REPRESENTATION_ITEM('')
SURFACE()
);
#3907=(
BOUNDED_SURFACE()
B_SPLINE_SURFACE(3,2,((#252704,#252705,#252706),(#252707,#252708,#252709),
(#252710,#252711,#252712),(#252713,#252714,#252715)),.UNSPECIFIED.,.F.,
 .F.,.F.)
B_SPLINE_SURFACE_WITH_KNOTS((4,4),(3,3),(0.,0.000397394373651927),(0.,1.),
 .UNSPECIFIED.)
GEOMETRIC_REPRESENTATION_ITEM()
RATIONAL_B_SPLINE_SURFACE(((1.,0.707106781186541,1.),(1.,0.707752587915892,
1.),(1.,0.708377654540697,1.),(1.,0.708689770883313,1.)))
REPRESENTATION_ITEM('')
SURFACE()
);
#3908=(
BOUNDED_SURFACE()
B_SPLINE_SURFACE(3,2,((#252717,#252718,#252719),(#252720,#252721,#252722),
(#252723,#252724,#252725),(#252726,#252727,#252728)),.UNSPECIFIED.,.F.,
 .F.,.F.)
B_SPLINE_SURFACE_WITH_KNOTS((4,4),(3,3),(0.,0.000511815456479792),(0.,1.0010587316),
 .UNSPECIFIED.)
GEOMETRIC_REPRESENTATION_ITEM()
RATIONAL_B_SPLINE_SURFACE(((1.,0.708394529056316,1.00061746385364),(1.,
0.708058564166859,1.00061817524693),(1.,0.707430835372039,1.00061950443955),
(1.,0.706796685880368,1.00062084722776)))
REPRESENTATION_ITEM('')
SURFACE()
);
#3909=(
BOUNDED_SURFACE()
B_SPLINE_SURFACE(3,2,((#252734,#252735,#252736),(#252737,#252738,#252739),
(#252740,#252741,#252742),(#252743,#252744,#252745)),.UNSPECIFIED.,.F.,
 .F.,.F.)
B_SPLINE_SURFACE_WITH_KNOTS((4,4),(3,3),(-6.20705743747951E-18,0.000397394465448313),
(0.,1.),.UNSPECIFIED.)
GEOMETRIC_REPRESENTATION_ITEM()
RATIONAL_B_SPLINE_SURFACE(((1.,0.705498956110768,1.),(1.,0.705821764811784,
1.),(1.,0.706461952521158,1.),(1.,0.707106781186533,1.)))
REPRESENTATION_ITEM('')
SURFACE()
);
#3910=(
BOUNDED_SURFACE()
B_SPLINE_SURFACE(3,2,((#252751,#252752,#252753),(#252754,#252755,#252756),
(#252757,#252758,#252759),(#252760,#252761,#252762)),.UNSPECIFIED.,.F.,
 .F.,.F.)
B_SPLINE_SURFACE_WITH_KNOTS((4,4),(3,3),(3.52365706057789E-19,0.000397394410828728),
(0.,1.),.UNSPECIFIED.)
GEOMETRIC_REPRESENTATION_ITEM()
RATIONAL_B_SPLINE_SURFACE(((1.,0.708689770883317,1.),(1.,0.708376440034512,
1.),(1.,0.707750498698386,1.),(1.,0.707106781186551,1.)))
REPRESENTATION_ITEM('')
SURFACE()
);
#3911=(
BOUNDED_SURFACE()
B_SPLINE_SURFACE(3,2,((#252768,#252769,#252770),(#252771,#252772,#252773),
(#252774,#252775,#252776),(#252777,#252778,#252779)),.UNSPECIFIED.,.F.,
 .F.,.F.)
B_SPLINE_SURFACE_WITH_KNOTS((4,4),(3,3),(0.,0.000511815090126187),(0.,1.00105592270218),
 .UNSPECIFIED.)
GEOMETRIC_REPRESENTATION_ITEM()
RATIONAL_B_SPLINE_SURFACE(((1.,0.705266242717496,1.00062243213083),(1.,
0.705584085909148,1.00062176089515),(1.,0.706182089450495,1.00062049800412),
(1.,0.70679750858749,1.00061919833404)))
REPRESENTATION_ITEM('')
SURFACE()
);
#3912=(
BOUNDED_SURFACE()
B_SPLINE_SURFACE(3,2,((#252781,#252782,#252783),(#252784,#252785,#252786),
(#252787,#252788,#252789),(#252790,#252791,#252792)),.UNSPECIFIED.,.F.,
 .F.,.F.)
B_SPLINE_SURFACE_WITH_KNOTS((4,4),(3,3),(0.,0.00039739442808662),(0.,1.),
 .UNSPECIFIED.)
GEOMETRIC_REPRESENTATION_ITEM()
RATIONAL_B_SPLINE_SURFACE(((1.,0.707106781186551,1.),(1.,0.706459846759092,
1.),(1.,0.705820510737283,1.),(1.,0.705498956110754,1.)))
REPRESENTATION_ITEM('')
SURFACE()
);
#3913=(
BOUNDED_SURFACE()
B_SPLINE_SURFACE(3,2,((#252798,#252799,#252800),(#252801,#252802,#252803),
(#252804,#252805,#252806),(#252807,#252808,#252809),(#252810,#252811,#252812),
(#252813,#252814,#252815)),.UNSPECIFIED.,.F.,.F.,.F.)
B_SPLINE_SURFACE_WITH_KNOTS((4,2,4),(3,3),(-3.27971157176865E-18,0.00025795380787285,
0.000515907615745704),(0.,1.),.UNSPECIFIED.)
GEOMETRIC_REPRESENTATION_ITEM()
RATIONAL_B_SPLINE_SURFACE(((1.,0.874619707139389,1.),(1.,0.874834349679203,
1.),(1.,0.854686104157534,1.),(1.,0.792476597915407,1.),(1.,0.750887854594928,
1.),(1.,0.705585838031446,1.)))
REPRESENTATION_ITEM('')
SURFACE()
);
#3914=(
BOUNDED_SURFACE()
B_SPLINE_SURFACE(3,2,((#252821,#252822,#252823),(#252824,#252825,#252826),
(#252827,#252828,#252829),(#252830,#252831,#252832)),.UNSPECIFIED.,.F.,
 .F.,.F.)
B_SPLINE_SURFACE_WITH_KNOTS((4,4),(3,3),(0.,0.000511815437699159),(0.,1.00105881331807),
 .UNSPECIFIED.)
GEOMETRIC_REPRESENTATION_ITEM()
RATIONAL_B_SPLINE_SURFACE(((1.,0.706796661945702,1.00062089519847),(1.,
0.707430821224571,1.00061955228589),(1.,0.70805854583007,1.00061822299954),
(1.,0.708394505252093,1.00061751156292)))
REPRESENTATION_ITEM('')
SURFACE()
);
#3915=(
BOUNDED_SURFACE()
B_SPLINE_SURFACE(3,2,((#252834,#252835,#252836),(#252837,#252838,#252839),
(#252840,#252841,#252842),(#252843,#252844,#252845),(#252846,#252847,#252848),
(#252849,#252850,#252851)),.UNSPECIFIED.,.F.,.F.,.F.)
B_SPLINE_SURFACE_WITH_KNOTS((4,2,4),(3,3),(-1.13841228110978E-18,0.00025691531753126,
0.000513830635062521),(0.,1.),.UNSPECIFIED.)
GEOMETRIC_REPRESENTATION_ITEM()
RATIONAL_B_SPLINE_SURFACE(((1.,0.705585838031441,1.),(1.,0.750902433542694,
1.),(1.,0.792329530082573,1.),(1.,0.854288401594117,1.),(1.,0.87499803112519,
1.),(1.,0.874619707139408,1.)))
REPRESENTATION_ITEM('')
SURFACE()
);
#3916=(
BOUNDED_SURFACE()
B_SPLINE_SURFACE(3,2,((#252857,#252858,#252859),(#252860,#252861,#252862),
(#252863,#252864,#252865),(#252866,#252867,#252868),(#252869,#252870,#252871),
(#252872,#252873,#252874)),.UNSPECIFIED.,.F.,.F.,.F.)
B_SPLINE_SURFACE_WITH_KNOTS((4,2,4),(3,3),(-2.0870891820346E-18,0.000256592814262156,
0.000513185628524313),(0.,1.),.UNSPECIFIED.)
GEOMETRIC_REPRESENTATION_ITEM()
RATIONAL_B_SPLINE_SURFACE(((1.,0.708712527163635,1.),(1.,0.753780902613681,
1.),(1.,0.794538995769107,1.),(1.,0.855070770331192,1.),(1.,0.875018427445252,
1.),(1.,0.874619707139401,1.)))
REPRESENTATION_ITEM('')
SURFACE()
);
#3917=(
BOUNDED_SURFACE()
B_SPLINE_SURFACE(3,2,((#252876,#252877,#252878),(#252879,#252880,#252881),
(#252882,#252883,#252884),(#252885,#252886,#252887)),.UNSPECIFIED.,.F.,
 .F.,.F.)
B_SPLINE_SURFACE_WITH_KNOTS((4,4),(3,3),(-7.77915058758349E-18,0.0005118150724304),
(0.,1.00105598365789),.UNSPECIFIED.)
GEOMETRIC_REPRESENTATION_ITEM()
RATIONAL_B_SPLINE_SURFACE(((1.,0.706797490733977,1.00061923411647),(1.,
0.706182062146854,1.00062053388153),(1.,0.705584062769277,1.00062179683667),
(1.,0.705266224770748,1.00062246810014)))
REPRESENTATION_ITEM('')
SURFACE()
);
#3918=(
BOUNDED_SURFACE()
B_SPLINE_SURFACE(3,2,((#252893,#252894,#252895),(#252896,#252897,#252898),
(#252899,#252900,#252901),(#252902,#252903,#252904),(#252905,#252906,#252907),
(#252908,#252909,#252910)),.UNSPECIFIED.,.F.,.F.,.F.)
B_SPLINE_SURFACE_WITH_KNOTS((4,2,4),(3,3),(-3.21194893598831E-18,0.000257652232350879,
0.000515304464701761),(0.,1.),.UNSPECIFIED.)
GEOMETRIC_REPRESENTATION_ITEM()
RATIONAL_B_SPLINE_SURFACE(((1.,0.874619707139399,1.),(1.,0.874861180430952,
1.),(1.,0.855455725920543,1.),(1.,0.794699358955585,1.),(1.,0.753768977788435,
1.),(1.,0.708712527163638,1.)))
REPRESENTATION_ITEM('')
SURFACE()
);
#3919=(
BOUNDED_SURFACE()
B_SPLINE_SURFACE(3,2,((#252916,#252917,#252918),(#252919,#252920,#252921),
(#252922,#252923,#252924),(#252925,#252926,#252927)),.UNSPECIFIED.,.F.,
 .F.,.F.)
B_SPLINE_SURFACE_WITH_KNOTS((4,4),(3,3),(-1.44740990026815E-17,0.000397394373651909),
(0.,1.),.UNSPECIFIED.)
GEOMETRIC_REPRESENTATION_ITEM()
RATIONAL_B_SPLINE_SURFACE(((1.,0.707106781186544,1.),(1.,0.70775258791589,
1.),(1.,0.708377654540694,1.),(1.,0.708689770883335,1.)))
REPRESENTATION_ITEM('')
SURFACE()
);
#3920=(
BOUNDED_SURFACE()
B_SPLINE_SURFACE(3,2,((#252929,#252930,#252931),(#252932,#252933,#252934),
(#252935,#252936,#252937),(#252938,#252939,#252940)),.UNSPECIFIED.,.F.,
 .F.,.F.)
B_SPLINE_SURFACE_WITH_KNOTS((4,4),(3,3),(-6.42389787197661E-18,0.000511815456479789),
(0.,1.00105873159907),.UNSPECIFIED.)
GEOMETRIC_REPRESENTATION_ITEM()
RATIONAL_B_SPLINE_SURFACE(((1.,0.708394529056584,1.0006174638531),(1.,0.708058564167148,
1.00061817524639),(1.,0.707430835372308,1.00061950443901),(1.,0.706796685880638,
1.00062084722722)))
REPRESENTATION_ITEM('')
SURFACE()
);
#3921=(
BOUNDED_SURFACE()
B_SPLINE_SURFACE(3,2,((#252946,#252947,#252948),(#252949,#252950,#252951),
(#252952,#252953,#252954),(#252955,#252956,#252957)),.UNSPECIFIED.,.F.,
 .F.,.F.)
B_SPLINE_SURFACE_WITH_KNOTS((4,4),(3,3),(-3.79470760369927E-19,0.000397394465448309),
(0.,1.),.UNSPECIFIED.)
GEOMETRIC_REPRESENTATION_ITEM()
RATIONAL_B_SPLINE_SURFACE(((1.,0.705498956110748,1.),(1.,0.705821764811732,
1.),(1.,0.706461952521157,1.),(1.,0.707106781186544,1.)))
REPRESENTATION_ITEM('')
SURFACE()
);
#3922=(
BOUNDED_SURFACE()
B_SPLINE_SURFACE(3,2,((#252963,#252964,#252965),(#252966,#252967,#252968),
(#252969,#252970,#252971),(#252972,#252973,#252974)),.UNSPECIFIED.,.F.,
 .F.,.F.)
B_SPLINE_SURFACE_WITH_KNOTS((4,4),(3,3),(0.,0.000397394410828749),(0.,1.),
 .UNSPECIFIED.)
GEOMETRIC_REPRESENTATION_ITEM()
RATIONAL_B_SPLINE_SURFACE(((1.,0.70868977088334,1.),(1.,0.708376440034472,
1.),(1.,0.707750498698436,1.),(1.,0.707106781186546,1.)))
REPRESENTATION_ITEM('')
SURFACE()
);
#3923=(
BOUNDED_SURFACE()
B_SPLINE_SURFACE(3,2,((#252980,#252981,#252982),(#252983,#252984,#252985),
(#252986,#252987,#252988),(#252989,#252990,#252991)),.UNSPECIFIED.,.F.,
 .F.,.F.)
B_SPLINE_SURFACE_WITH_KNOTS((4,4),(3,3),(-1.35525271560688E-19,0.000511815090126169),
(0.,1.00105592270159),.UNSPECIFIED.)
GEOMETRIC_REPRESENTATION_ITEM()
RATIONAL_B_SPLINE_SURFACE(((1.,0.705266242717656,1.00062243213048),(1.,
0.705584085909313,1.0006217608948),(1.,0.706182089450677,1.00062049800377),
(1.,0.706797508587662,1.00061919833369)))
REPRESENTATION_ITEM('')
SURFACE()
);
#3924=(
BOUNDED_SURFACE()
B_SPLINE_SURFACE(3,2,((#252993,#252994,#252995),(#252996,#252997,#252998),
(#252999,#253000,#253001),(#253002,#253003,#253004)),.UNSPECIFIED.,.F.,
 .F.,.F.)
B_SPLINE_SURFACE_WITH_KNOTS((4,4),(3,3),(0.,0.000397394428086617),(0.,1.),
 .UNSPECIFIED.)
GEOMETRIC_REPRESENTATION_ITEM()
RATIONAL_B_SPLINE_SURFACE(((1.,0.707106781186545,1.),(1.,0.706459846759076,
1.),(1.,0.705820510737292,1.),(1.,0.705498956110732,1.)))
REPRESENTATION_ITEM('')
SURFACE()
);
#3925=(
BOUNDED_SURFACE()
B_SPLINE_SURFACE(3,2,((#253010,#253011,#253012),(#253013,#253014,#253015),
(#253016,#253017,#253018),(#253019,#253020,#253021),(#253022,#253023,#253024),
(#253025,#253026,#253027)),.UNSPECIFIED.,.F.,.F.,.F.)
B_SPLINE_SURFACE_WITH_KNOTS((4,2,4),(3,3),(-5.14996031930615E-19,0.000257953807872849,
0.000515907615745698),(0.,1.),.UNSPECIFIED.)
GEOMETRIC_REPRESENTATION_ITEM()
RATIONAL_B_SPLINE_SURFACE(((1.,0.874619707139401,1.),(1.,0.874834349678968,
1.),(1.,0.85468610415782,1.),(1.,0.792476597915128,1.),(1.,0.750887854595128,
1.),(1.,0.70558583803143,1.)))
REPRESENTATION_ITEM('')
SURFACE()
);
#3926=(
BOUNDED_SURFACE()
B_SPLINE_SURFACE(3,2,((#253033,#253034,#253035),(#253036,#253037,#253038),
(#253039,#253040,#253041),(#253042,#253043,#253044)),.UNSPECIFIED.,.F.,
 .F.,.F.)
B_SPLINE_SURFACE_WITH_KNOTS((4,4),(3,3),(-8.13151629364128E-20,0.000511815437699142),
(0.,1.00105881331387),.UNSPECIFIED.)
GEOMETRIC_REPRESENTATION_ITEM()
RATIONAL_B_SPLINE_SURFACE(((1.,0.706796661946928,1.000620895196),(1.,0.707430821225802,
1.00061955228343),(1.,0.708058545831284,1.00061822299709),(1.,0.708394505253304,
1.00061751156047)))
REPRESENTATION_ITEM('')
SURFACE()
);
#3927=(
BOUNDED_SURFACE()
B_SPLINE_SURFACE(3,2,((#253046,#253047,#253048),(#253049,#253050,#253051),
(#253052,#253053,#253054),(#253055,#253056,#253057),(#253058,#253059,#253060),
(#253061,#253062,#253063)),.UNSPECIFIED.,.F.,.F.,.F.)
B_SPLINE_SURFACE_WITH_KNOTS((4,2,4),(3,3),(-4.49943901581484E-18,0.000256915317531251,
0.000513830635062507),(0.,1.),.UNSPECIFIED.)
GEOMETRIC_REPRESENTATION_ITEM()
RATIONAL_B_SPLINE_SURFACE(((1.,0.705585838031437,1.),(1.,0.750902433542874,
1.),(1.,0.79232953008234,1.),(1.,0.854288401594352,1.),(1.,0.874998031125028,
1.),(1.,0.874619707139391,1.)))
REPRESENTATION_ITEM('')
SURFACE()
);
#3928=(
BOUNDED_SURFACE()
B_SPLINE_SURFACE(3,2,((#253069,#253070,#253071),(#253072,#253073,#253074),
(#253075,#253076,#253077),(#253078,#253079,#253080),(#253081,#253082,#253083),
(#253084,#253085,#253086)),.UNSPECIFIED.,.F.,.F.,.F.)
B_SPLINE_SURFACE_WITH_KNOTS((4,2,4),(3,3),(-3.25260651745651E-19,0.000256592814262156,
0.000513185628524313),(0.,1.),.UNSPECIFIED.)
GEOMETRIC_REPRESENTATION_ITEM()
RATIONAL_B_SPLINE_SURFACE(((1.,0.708712527163664,1.),(1.,0.753780902612852,
1.),(1.,0.794538995770168,1.),(1.,0.855070770330182,1.),(1.,0.875018427446005,
1.),(1.,0.874619707139394,1.)))
REPRESENTATION_ITEM('')
SURFACE()
);
#3929=(
BOUNDED_SURFACE()
B_SPLINE_SURFACE(3,2,((#253088,#253089,#253090),(#253091,#253092,#253093),
(#253094,#253095,#253096),(#253097,#253098,#253099)),.UNSPECIFIED.,.F.,
 .F.,.F.)
B_SPLINE_SURFACE_WITH_KNOTS((4,4),(3,3),(2.71050543121376E-20,0.000511815072430397),
(0.,1.00105598365838),.UNSPECIFIED.)
GEOMETRIC_REPRESENTATION_ITEM()
RATIONAL_B_SPLINE_SURFACE(((1.,0.706797490733823,1.00061923411676),(1.,
0.706182062146751,1.00062053388183),(1.,0.705584062769127,1.00062179683697),
(1.,0.70526622477057,1.00062246810043)))
REPRESENTATION_ITEM('')
SURFACE()
);
#3930=(
BOUNDED_SURFACE()
B_SPLINE_SURFACE(3,2,((#253105,#253106,#253107),(#253108,#253109,#253110),
(#253111,#253112,#253113),(#253114,#253115,#253116),(#253117,#253118,#253119),
(#253120,#253121,#253122)),.UNSPECIFIED.,.F.,.F.,.F.)
B_SPLINE_SURFACE_WITH_KNOTS((4,2,4),(3,3),(0.,0.000257652232350884,0.000515304464701769),
(0.,1.),.UNSPECIFIED.)
GEOMETRIC_REPRESENTATION_ITEM()
RATIONAL_B_SPLINE_SURFACE(((1.,0.874619707139393,1.),(1.,0.874861180430782,
1.),(1.,0.85545572592081,1.),(1.,0.794699358955333,1.),(1.,0.753768977788603,
1.),(1.,0.708712527163673,1.)))
REPRESENTATION_ITEM('')
SURFACE()
);
#3931=(
BOUNDED_SURFACE()
B_SPLINE_SURFACE(3,2,((#253128,#253129,#253130),(#253131,#253132,#253133),
(#253134,#253135,#253136),(#253137,#253138,#253139)),.UNSPECIFIED.,.F.,
 .F.,.F.)
B_SPLINE_SURFACE_WITH_KNOTS((4,4),(3,3),(0.,0.000397394373651932),(0.,1.),
 .UNSPECIFIED.)
GEOMETRIC_REPRESENTATION_ITEM()
RATIONAL_B_SPLINE_SURFACE(((1.,0.707106781186545,1.),(1.,0.707752587915885,
1.),(1.,0.708377654540695,1.),(1.,0.70868977088333,1.)))
REPRESENTATION_ITEM('')
SURFACE()
);
#3932=(
BOUNDED_SURFACE()
B_SPLINE_SURFACE(3,2,((#253141,#253142,#253143),(#253144,#253145,#253146),
(#253147,#253148,#253149),(#253150,#253151,#253152)),.UNSPECIFIED.,.F.,
 .F.,.F.)
B_SPLINE_SURFACE_WITH_KNOTS((4,4),(3,3),(1.35525271560688E-19,0.000511815456479789),
(0.,1.00105873159949),.UNSPECIFIED.)
GEOMETRIC_REPRESENTATION_ITEM()
RATIONAL_B_SPLINE_SURFACE(((1.,0.708394529056461,1.00061746385335),(1.,
0.708058564166996,1.00061817524664),(1.,0.707430835372202,1.00061950443926),
(1.,0.70679668588051,1.00062084722747)))
REPRESENTATION_ITEM('')
SURFACE()
);
#3933=(
BOUNDED_SURFACE()
B_SPLINE_SURFACE(3,2,((#253158,#253159,#253160),(#253161,#253162,#253163),
(#253164,#253165,#253166),(#253167,#253168,#253169)),.UNSPECIFIED.,.F.,
 .F.,.F.)
B_SPLINE_SURFACE_WITH_KNOTS((4,4),(3,3),(0.,0.000397394465448298),(0.,1.),
 .UNSPECIFIED.)
GEOMETRIC_REPRESENTATION_ITEM()
RATIONAL_B_SPLINE_SURFACE(((1.,0.705498956110754,1.),(1.,0.705821764811776,
1.),(1.,0.706461952521147,1.),(1.,0.707106781186545,1.)))
REPRESENTATION_ITEM('')
SURFACE()
);
#3934=(
BOUNDED_SURFACE()
B_SPLINE_SURFACE(3,2,((#253175,#253176,#253177),(#253178,#253179,#253180),
(#253181,#253182,#253183),(#253184,#253185,#253186)),.UNSPECIFIED.,.F.,
 .F.,.F.)
B_SPLINE_SURFACE_WITH_KNOTS((4,4),(3,3),(2.71050543121376E-20,0.000397394410828729),
(0.,1.),.UNSPECIFIED.)
GEOMETRIC_REPRESENTATION_ITEM()
RATIONAL_B_SPLINE_SURFACE(((1.,0.70868977088331,1.),(1.,0.708376440034508,
1.),(1.,0.707750498698394,1.),(1.,0.707106781186548,1.)))
REPRESENTATION_ITEM('')
SURFACE()
);
#3935=(
BOUNDED_SURFACE()
B_SPLINE_SURFACE(3,2,((#253192,#253193,#253194),(#253195,#253196,#253197),
(#253198,#253199,#253200),(#253201,#253202,#253203)),.UNSPECIFIED.,.F.,
 .F.,.F.)
B_SPLINE_SURFACE_WITH_KNOTS((4,4),(3,3),(-2.71050543121376E-20,0.000511815090126182),
(0.,1.00105592270603),.UNSPECIFIED.)
GEOMETRIC_REPRESENTATION_ITEM()
RATIONAL_B_SPLINE_SURFACE(((1.,0.705266242716357,1.0006224321331),(1.,0.705584085908022,
1.00062176089741),(1.,0.706182089449371,1.00062049800638),(1.,0.706797508586361,
1.0006191983363)))
REPRESENTATION_ITEM('')
SURFACE()
);
#3936=(
BOUNDED_SURFACE()
B_SPLINE_SURFACE(3,2,((#253205,#253206,#253207),(#253208,#253209,#253210),
(#253211,#253212,#253213),(#253214,#253215,#253216)),.UNSPECIFIED.,.F.,
 .F.,.F.)
B_SPLINE_SURFACE_WITH_KNOTS((4,4),(3,3),(1.0842021724855E-19,0.00039739442808663),
(0.,1.),.UNSPECIFIED.)
GEOMETRIC_REPRESENTATION_ITEM()
RATIONAL_B_SPLINE_SURFACE(((1.,0.70710678118655,1.),(1.,0.706459846759098,
1.),(1.,0.705820510737275,1.),(1.,0.705498956110757,1.)))
REPRESENTATION_ITEM('')
SURFACE()
);
#3937=(
BOUNDED_SURFACE()
B_SPLINE_SURFACE(3,2,((#253222,#253223,#253224),(#253225,#253226,#253227),
(#253228,#253229,#253230),(#253231,#253232,#253233),(#253234,#253235,#253236),
(#253237,#253238,#253239)),.UNSPECIFIED.,.F.,.F.,.F.)
B_SPLINE_SURFACE_WITH_KNOTS((4,2,4),(3,3),(0.,0.00025795380787284,0.00051590761574568),
(0.,1.),.UNSPECIFIED.)
GEOMETRIC_REPRESENTATION_ITEM()
RATIONAL_B_SPLINE_SURFACE(((1.,0.87461970713939,1.),(1.,0.874834349678797,
1.),(1.,0.854686104158041,1.),(1.,0.792476597914909,1.),(1.,0.750887854595297,
1.),(1.,0.705585838031443,1.)))
REPRESENTATION_ITEM('')
SURFACE()
);
#3938=(
BOUNDED_SURFACE()
B_SPLINE_SURFACE(3,2,((#253245,#253246,#253247),(#253248,#253249,#253250),
(#253251,#253252,#253253),(#253254,#253255,#253256)),.UNSPECIFIED.,.F.,
 .F.,.F.)
B_SPLINE_SURFACE_WITH_KNOTS((4,4),(3,3),(-7.23704950134074E-18,0.000511815437699144),
(0.,1.00105881331707),.UNSPECIFIED.)
GEOMETRIC_REPRESENTATION_ITEM()
RATIONAL_B_SPLINE_SURFACE(((1.,0.706796661945989,1.00062089519788),(1.,
0.70743082122485,1.0006195522853),(1.,0.708058545830382,1.00061822299896),
(1.,0.708394505252367,1.00061751156234)))
REPRESENTATION_ITEM('')
SURFACE()
);
#3939=(
BOUNDED_SURFACE()
B_SPLINE_SURFACE(3,2,((#253258,#253259,#253260),(#253261,#253262,#253263),
(#253264,#253265,#253266),(#253267,#253268,#253269),(#253270,#253271,#253272),
(#253273,#253274,#253275)),.UNSPECIFIED.,.F.,.F.,.F.)
B_SPLINE_SURFACE_WITH_KNOTS((4,2,4),(3,3),(-2.43945488809238E-19,0.00025691531753126,
0.00051383063506252),(0.,1.),.UNSPECIFIED.)
GEOMETRIC_REPRESENTATION_ITEM()
RATIONAL_B_SPLINE_SURFACE(((1.,0.705585838031451,1.),(1.,0.750902433542877,
1.),(1.,0.792329530082299,1.),(1.,0.854288401594406,1.),(1.,0.874998031124972,
1.),(1.,0.874619707139391,1.)))
REPRESENTATION_ITEM('')
SURFACE()
);
#3940=(
BOUNDED_SURFACE()
B_SPLINE_SURFACE(3,2,((#253281,#253282,#253283),(#253284,#253285,#253286),
(#253287,#253288,#253289),(#253290,#253291,#253292),(#253293,#253294,#253295),
(#253296,#253297,#253298)),.UNSPECIFIED.,.F.,.F.,.F.)
B_SPLINE_SURFACE_WITH_KNOTS((4,2,4),(3,3),(1.89735380184963E-19,0.000256592814262156,
0.000513185628524311),(0.,1.),.UNSPECIFIED.)
GEOMETRIC_REPRESENTATION_ITEM()
RATIONAL_B_SPLINE_SURFACE(((1.,0.708712527163678,1.),(1.,0.753780902613698,
1.),(1.,0.794538995769049,1.),(1.,0.855070770331267,1.),(1.,0.875018427445209,
1.),(1.,0.874619707139396,1.)))
REPRESENTATION_ITEM('')
SURFACE()
);
#3941=(
BOUNDED_SURFACE()
B_SPLINE_SURFACE(3,2,((#253300,#253301,#253302),(#253303,#253304,#253305),
(#253306,#253307,#253308),(#253309,#253310,#253311)),.UNSPECIFIED.,.F.,
 .F.,.F.)
B_SPLINE_SURFACE_WITH_KNOTS((4,4),(3,3),(-4.87890977618477E-19,0.000511815072430402),
(0.,1.001055983659),.UNSPECIFIED.)
GEOMETRIC_REPRESENTATION_ITEM()
RATIONAL_B_SPLINE_SURFACE(((1.,0.706797490733651,1.00061923411713),(1.,
0.706182062146538,1.00062053388219),(1.,0.705584062768948,1.00062179683733),
(1.,0.705266224770404,1.0006224681008)))
REPRESENTATION_ITEM('')
SURFACE()
);
#3942=(
BOUNDED_SURFACE()
B_SPLINE_SURFACE(3,2,((#253317,#253318,#253319),(#253320,#253321,#253322),
(#253323,#253324,#253325),(#253326,#253327,#253328),(#253329,#253330,#253331),
(#253332,#253333,#253334)),.UNSPECIFIED.,.F.,.F.,.F.)
B_SPLINE_SURFACE_WITH_KNOTS((4,2,4),(3,3),(-3.11708124589583E-19,0.00025765223235088,
0.00051530446470176),(0.,1.),.UNSPECIFIED.)
GEOMETRIC_REPRESENTATION_ITEM()
RATIONAL_B_SPLINE_SURFACE(((1.,0.874619707139394,1.),(1.,0.874861180430961,
1.),(1.,0.855455725920548,1.),(1.,0.794699358955591,1.),(1.,0.75376897778842,
1.),(1.,0.70871252716367,1.)))
REPRESENTATION_ITEM('')
SURFACE()
);
#3943=(
BOUNDED_SURFACE()
B_SPLINE_SURFACE(3,2,((#253340,#253341,#253342),(#253343,#253344,#253345),
(#253346,#253347,#253348),(#253349,#253350,#253351)),.UNSPECIFIED.,.F.,
 .F.,.F.)
B_SPLINE_SURFACE_WITH_KNOTS((4,4),(3,3),(-8.13151629364128E-20,0.000397394373651932),
(0.,1.),.UNSPECIFIED.)
GEOMETRIC_REPRESENTATION_ITEM()
RATIONAL_B_SPLINE_SURFACE(((1.,0.707106781186547,1.),(1.,0.707752587915892,
1.),(1.,0.708377654540687,1.),(1.,0.708689770883334,1.)))
REPRESENTATION_ITEM('')
SURFACE()
);
#3944=(
BOUNDED_SURFACE()
B_SPLINE_SURFACE(3,2,((#253353,#253354,#253355),(#253356,#253357,#253358),
(#253359,#253360,#253361),(#253362,#253363,#253364)),.UNSPECIFIED.,.F.,
 .F.,.F.)
B_SPLINE_SURFACE_WITH_KNOTS((4,4),(3,3),(2.71050543121376E-20,0.000511815456479785),
(0.,1.00105873159858),.UNSPECIFIED.)
GEOMETRIC_REPRESENTATION_ITEM()
RATIONAL_B_SPLINE_SURFACE(((1.,0.708394529056732,1.00061746385281),(1.,
0.708058564167282,1.0006181752461),(1.,0.707430835372459,1.00061950443872),
(1.,0.706796685880782,1.00062084722693)))
REPRESENTATION_ITEM('')
SURFACE()
);
#3945=(
BOUNDED_SURFACE()
B_SPLINE_SURFACE(3,2,((#253370,#253371,#253372),(#253373,#253374,#253375),
(#253376,#253377,#253378),(#253379,#253380,#253381)),.UNSPECIFIED.,.F.,
 .F.,.F.)
B_SPLINE_SURFACE_WITH_KNOTS((4,4),(3,3),(-2.71050543121376E-20,0.000397394465448309),
(0.,1.),.UNSPECIFIED.)
GEOMETRIC_REPRESENTATION_ITEM()
RATIONAL_B_SPLINE_SURFACE(((1.,0.705498956110728,1.),(1.,0.705821764811776,
1.),(1.,0.706461952521145,1.),(1.,0.707106781186548,1.)))
REPRESENTATION_ITEM('')
SURFACE()
);
#3946=(
BOUNDED_SURFACE()
B_SPLINE_SURFACE(2,2,((#253474,#253475,#253476),(#253477,#253478,#253479),
(#253480,#253481,#253482)),.UNSPECIFIED.,.F.,.F.,.F.)
B_SPLINE_SURFACE_WITH_KNOTS((3,3),(3,3),(-1.5707963267949,0.),(-0.314644728766082,
0.610865238198018),.UNSPECIFIED.)
GEOMETRIC_REPRESENTATION_ITEM()
RATIONAL_B_SPLINE_SURFACE(((1.,0.894826028883616,1.),(0.707106781186549,
0.632737553005835,0.707106781186549),(1.,0.894826028883616,1.)))
REPRESENTATION_ITEM('')
SURFACE()
);
#3947=(
BOUNDED_SURFACE()
B_SPLINE_SURFACE(2,2,((#253491,#253492,#253493),(#253494,#253495,#253496),
(#253497,#253498,#253499)),.UNSPECIFIED.,.F.,.F.,.F.)
B_SPLINE_SURFACE_WITH_KNOTS((3,3),(3,3),(-1.5707963267949,0.),(-0.610865238198018,
0.314644728766082),.UNSPECIFIED.)
GEOMETRIC_REPRESENTATION_ITEM()
RATIONAL_B_SPLINE_SURFACE(((1.,0.894826028883616,1.),(0.707106781186549,
0.632737553005836,0.707106781186549),(1.,0.894826028883616,1.)))
REPRESENTATION_ITEM('')
SURFACE()
);
#3948=(
BOUNDED_SURFACE()
B_SPLINE_SURFACE(2,2,((#253508,#253509,#253510),(#253511,#253512,#253513),
(#253514,#253515,#253516)),.UNSPECIFIED.,.F.,.F.,.F.)
B_SPLINE_SURFACE_WITH_KNOTS((3,3),(3,3),(-1.5707963267949,0.),(-0.462754983482051,
0.462754983482052),.UNSPECIFIED.)
GEOMETRIC_REPRESENTATION_ITEM()
RATIONAL_B_SPLINE_SURFACE(((1.,0.894826028883615,1.),(0.707106781186545,
0.632737553005831,0.707106781186545),(1.,0.894826028883615,1.)))
REPRESENTATION_ITEM('')
SURFACE()
);
#3949=(
BOUNDED_SURFACE()
B_SPLINE_SURFACE(2,2,((#253531,#253532,#253533),(#253534,#253535,#253536),
(#253537,#253538,#253539)),.UNSPECIFIED.,.F.,.F.,.F.)
B_SPLINE_SURFACE_WITH_KNOTS((3,3),(3,3),(-1.5707963267949,0.),(-0.462754983482049,
0.46275498348205),.UNSPECIFIED.)
GEOMETRIC_REPRESENTATION_ITEM()
RATIONAL_B_SPLINE_SURFACE(((1.,0.894826028883616,1.),(0.707106781186543,
0.63273755300583,0.707106781186543),(1.,0.894826028883616,1.)))
REPRESENTATION_ITEM('')
SURFACE()
);
#3950=(
BOUNDED_SURFACE()
B_SPLINE_SURFACE(3,1,((#254918,#254919),(#254920,#254921),(#254922,#254923),
(#254924,#254925)),.UNSPECIFIED.,.F.,.F.,.F.)
B_SPLINE_SURFACE_WITH_KNOTS((4,4),(2,2),(0.,1.),(0.,1.),.UNSPECIFIED.)
GEOMETRIC_REPRESENTATION_ITEM()
RATIONAL_B_SPLINE_SURFACE(((1.,1.),(0.948102323621204,0.987087872581763),
(0.948102323621204,0.987087872581763),(1.,1.)))
REPRESENTATION_ITEM('')
SURFACE()
);
#3951=(
BOUNDED_SURFACE()
B_SPLINE_SURFACE(3,2,((#255695,#255696,#255697),(#255698,#255699,#255700),
(#255701,#255702,#255703),(#255704,#255705,#255706)),.UNSPECIFIED.,.F.,
 .F.,.F.)
B_SPLINE_SURFACE_WITH_KNOTS((4,4),(3,3),(-3.46944695195361E-18,0.00108749691872869),
(0.827141149879304,1.),.UNSPECIFIED.)
GEOMETRIC_REPRESENTATION_ITEM()
RATIONAL_B_SPLINE_SURFACE(((0.969924731391313,0.981819748290195,1.),(0.969924599712626,
0.981819668691515,1.),(0.969814841303219,0.981753320638693,1.),(0.969600878752829,
0.981623982042481,1.)))
REPRESENTATION_ITEM('')
SURFACE()
);
#3952=(
BOUNDED_SURFACE()
B_SPLINE_SURFACE(3,2,((#255790,#255791,#255792),(#255793,#255794,#255795),
(#255796,#255797,#255798),(#255799,#255800,#255801)),.UNSPECIFIED.,.F.,
 .F.,.F.)
B_SPLINE_SURFACE_WITH_KNOTS((4,4),(3,3),(0.,0.00108749691872869),(0.,0.172858850120678),
 .UNSPECIFIED.)
GEOMETRIC_REPRESENTATION_ITEM()
RATIONAL_B_SPLINE_SURFACE(((1.,0.981819748290197,0.969924731391315),(1.,
0.981819668691517,0.969924599712628),(1.,0.981753320638695,0.969814841303222),
(1.,0.981623982042483,0.969600878752832)))
REPRESENTATION_ITEM('')
SURFACE()
);
#3953=(
BOUNDED_SURFACE()
B_SPLINE_SURFACE(3,2,((#255884,#255885,#255886),(#255887,#255888,#255889),
(#255890,#255891,#255892),(#255893,#255894,#255895)),.UNSPECIFIED.,.F.,
 .F.,.F.)
B_SPLINE_SURFACE_WITH_KNOTS((4,4),(3,3),(0.,0.00108749691872869),(0.827141149879317,
1.),.UNSPECIFIED.)
GEOMETRIC_REPRESENTATION_ITEM()
RATIONAL_B_SPLINE_SURFACE(((0.969924731391315,0.981819748290196,1.),(0.969924599712627,
0.981819668691516,1.),(0.969814841303221,0.981753320638695,1.),(0.969600878752831,
0.981623982042482,1.)))
REPRESENTATION_ITEM('')
SURFACE()
);
#3954=(
BOUNDED_SURFACE()
B_SPLINE_SURFACE(3,2,((#255942,#255943,#255944),(#255945,#255946,#255947),
(#255948,#255949,#255950),(#255951,#255952,#255953)),.UNSPECIFIED.,.F.,
 .F.,.F.)
B_SPLINE_SURFACE_WITH_KNOTS((4,4),(3,3),(-3.46944695195361E-18,0.0010874969187287),
(0.,0.172858850120678),.UNSPECIFIED.)
GEOMETRIC_REPRESENTATION_ITEM()
RATIONAL_B_SPLINE_SURFACE(((1.,0.981819748290197,0.969924731391316),(1.,
0.981819668691517,0.969924599712629),(1.,0.981753320638695,0.969814841303222),
(1.,0.981623982042483,0.969600878752832)))
REPRESENTATION_ITEM('')
SURFACE()
);
#3955=(
BOUNDED_SURFACE()
B_SPLINE_SURFACE(3,2,((#256036,#256037,#256038),(#256039,#256040,#256041),
(#256042,#256043,#256044),(#256045,#256046,#256047)),.UNSPECIFIED.,.F.,
 .F.,.F.)
B_SPLINE_SURFACE_WITH_KNOTS((4,4),(3,3),(0.,0.00108749691872869),(0.82714114987934,
1.),.UNSPECIFIED.)
GEOMETRIC_REPRESENTATION_ITEM()
RATIONAL_B_SPLINE_SURFACE(((0.969924731391318,0.981819748290198,1.),(0.969924599712631,
0.981819668691519,1.),(0.969814841303224,0.981753320638697,1.),(0.969600878752834,
0.981623982042484,1.)))
REPRESENTATION_ITEM('')
SURFACE()
);
#3956=(
BOUNDED_SURFACE()
B_SPLINE_SURFACE(3,2,((#256130,#256131,#256132),(#256133,#256134,#256135),
(#256136,#256137,#256138),(#256139,#256140,#256141)),.UNSPECIFIED.,.F.,
 .F.,.F.)
B_SPLINE_SURFACE_WITH_KNOTS((4,4),(3,3),(-3.03576608295941E-18,0.00108749691872869),
(0.,0.172858850120729),.UNSPECIFIED.)
GEOMETRIC_REPRESENTATION_ITEM()
RATIONAL_B_SPLINE_SURFACE(((1.,0.981819748290191,0.969924731391308),(1.,
0.981819668691511,0.969924599712621),(1.,0.98175332063869,0.969814841303215),
(1.,0.981623982042477,0.969600878752825)))
REPRESENTATION_ITEM('')
SURFACE()
);
#3957=(
BOUNDED_SURFACE()
B_SPLINE_SURFACE(3,2,((#256154,#256155,#256156),(#256157,#256158,#256159),
(#256160,#256161,#256162),(#256163,#256164,#256165)),.UNSPECIFIED.,.F.,
 .F.,.F.)
B_SPLINE_SURFACE_WITH_KNOTS((4,4),(3,3),(0.,0.0010874969187287),(0.,0.172858850120729),
 .UNSPECIFIED.)
GEOMETRIC_REPRESENTATION_ITEM()
RATIONAL_B_SPLINE_SURFACE(((1.,0.981819748290191,0.969924731391308),(1.,
0.981819668691512,0.969924599712622),(1.,0.98175332063869,0.969814841303215),
(1.,0.981623982042477,0.969600878752825)))
REPRESENTATION_ITEM('')
SURFACE()
);
#3958=(
BOUNDED_SURFACE()
B_SPLINE_SURFACE(3,2,((#256178,#256179,#256180),(#256181,#256182,#256183),
(#256184,#256185,#256186),(#256187,#256188,#256189)),.UNSPECIFIED.,.F.,
 .F.,.F.)
B_SPLINE_SURFACE_WITH_KNOTS((4,4),(3,3),(0.,0.00108749691872868),(0.827141149879317,
1.),.UNSPECIFIED.)
GEOMETRIC_REPRESENTATION_ITEM()
RATIONAL_B_SPLINE_SURFACE(((0.969924731391315,0.981819748290196,1.),(0.969924599712628,
0.981819668691516,1.),(0.969814841303221,0.981753320638694,1.),(0.969600878752831,
0.981623982042482,1.)))
REPRESENTATION_ITEM('')
SURFACE()
);
#3959=(
BOUNDED_SURFACE()
B_SPLINE_SURFACE(2,2,((#256202,#256203,#256204),(#256205,#256206,#256207),
(#256208,#256209,#256210)),.UNSPECIFIED.,.F.,.F.,.F.)
B_SPLINE_SURFACE_WITH_KNOTS((3,3),(3,3),(-1.5707963267949,0.),(0.959931088596877,
1.88544105556098),.UNSPECIFIED.)
GEOMETRIC_REPRESENTATION_ITEM()
RATIONAL_B_SPLINE_SURFACE(((1.,0.894826028883615,1.),(0.707106781186545,
0.632737553005832,0.707106781186545),(1.,0.894826028883615,1.)))
REPRESENTATION_ITEM('')
SURFACE()
);
#3960=(
BOUNDED_SURFACE()
B_SPLINE_SURFACE(2,2,((#256219,#256220,#256221),(#256222,#256223,#256224),
(#256225,#256226,#256227)),.UNSPECIFIED.,.F.,.F.,.F.)
B_SPLINE_SURFACE_WITH_KNOTS((3,3),(3,3),(-1.5707963267949,0.),(1.25615159802882,
2.18166156499291),.UNSPECIFIED.)
GEOMETRIC_REPRESENTATION_ITEM()
RATIONAL_B_SPLINE_SURFACE(((1.,0.894826028883616,1.),(0.707106781186542,
0.632737553005829,0.707106781186542),(1.,0.894826028883616,1.)))
REPRESENTATION_ITEM('')
SURFACE()
);
#3961=(
BOUNDED_SURFACE()
B_SPLINE_SURFACE(3,2,((#256229,#256230,#256231),(#256232,#256233,#256234),
(#256235,#256236,#256237),(#256238,#256239,#256240),(#256241,#256242,#256243),
(#256244,#256245,#256246),(#256247,#256248,#256249),(#256250,#256251,#256252),
(#256253,#256254,#256255),(#256256,#256257,#256258),(#256259,#256260,#256261),
(#256262,#256263,#256264),(#256265,#256266,#256267),(#256268,#256269,#256270)),
 .UNSPECIFIED.,.F.,.F.,.F.)
B_SPLINE_SURFACE_WITH_KNOTS((4,2,2,2,2,2,4),(3,3),(0.00306933855977502,
0.00495218666169259,0.00683503476361015,0.00871788286552771,0.0106007309674453,
0.0143664271712804,0.0181321233751155),(0.,1.),.UNSPECIFIED.)
GEOMETRIC_REPRESENTATION_ITEM()
RATIONAL_B_SPLINE_SURFACE(((1.,0.707106781186548,1.),(1.,0.733011584422493,
1.),(1.,0.756757437792392,1.),(1.,0.800574796194754,1.),(1.,0.820645929370482,
1.),(1.,0.857475616581832,1.),(1.,0.874266151416803,1.),(1.,0.904559499542173,
1.),(1.,0.917975383131884,1.),(1.,0.953491353960086,1.),(1.,0.970901198269013,
1.),(1.,0.994190014771706,1.),(1.,1.00000947743974,1.),(1.,1.,1.)))
REPRESENTATION_ITEM('')
SURFACE()
);
#3962=(
BOUNDED_SURFACE()
B_SPLINE_SURFACE(3,2,((#256374,#256375,#256376),(#256377,#256378,#256379),
(#256380,#256381,#256382),(#256383,#256384,#256385),(#256386,#256387,#256388),
(#256389,#256390,#256391),(#256392,#256393,#256394),(#256395,#256396,#256397),
(#256398,#256399,#256400),(#256401,#256402,#256403),(#256404,#256405,#256406),
(#256407,#256408,#256409),(#256410,#256411,#256412),(#256413,#256414,#256415)),
 .UNSPECIFIED.,.F.,.F.,.F.)
B_SPLINE_SURFACE_WITH_KNOTS((4,2,2,2,2,2,4),(3,3),(0.00306933855977502,
0.00495218666169259,0.00683503476361015,0.00871788286552771,0.0106007309674453,
0.0143664271712804,0.0181321233751155),(0.,1.),.UNSPECIFIED.)
GEOMETRIC_REPRESENTATION_ITEM()
RATIONAL_B_SPLINE_SURFACE(((1.,0.707106781186548,1.),(1.,0.733011584422493,
1.),(1.,0.756757437792392,1.),(1.,0.800574796194754,1.),(1.,0.820645929370482,
1.),(1.,0.857475616581832,1.),(1.,0.874266151416803,1.),(1.,0.904559499542173,
1.),(1.,0.917975383131884,1.),(1.,0.953491353960086,1.),(1.,0.970901198269013,
1.),(1.,0.994190014771706,1.),(1.,1.00000947743974,1.),(1.,1.,1.)))
REPRESENTATION_ITEM('')
SURFACE()
);
#3963=(
BOUNDED_SURFACE()
B_SPLINE_SURFACE(3,2,((#256420,#256421,#256422),(#256423,#256424,#256425),
(#256426,#256427,#256428),(#256429,#256430,#256431),(#256432,#256433,#256434),
(#256435,#256436,#256437),(#256438,#256439,#256440),(#256441,#256442,#256443),
(#256444,#256445,#256446),(#256447,#256448,#256449),(#256450,#256451,#256452),
(#256453,#256454,#256455),(#256456,#256457,#256458),(#256459,#256460,#256461)),
 .UNSPECIFIED.,.F.,.F.,.F.)
B_SPLINE_SURFACE_WITH_KNOTS((4,2,2,2,2,2,4),(3,3),(0.003069338559775,0.00495218666169257,
0.00683503476361014,0.00871788286552772,0.0106007309674453,0.0143664271712804,
0.0181321233751156),(0.,1.),.UNSPECIFIED.)
GEOMETRIC_REPRESENTATION_ITEM()
RATIONAL_B_SPLINE_SURFACE(((1.,0.70710678118655,1.),(1.,0.73301158442153,
1.),(1.,0.756757437793674,1.),(1.,0.800574796193468,1.),(1.,0.82064592936982,
1.),(1.,0.85747561658249,1.),(1.,0.874266151415543,1.),(1.,0.904559499543433,
1.),(1.,0.917975383132164,1.),(1.,0.953491353959532,1.),(1.,0.970901198269014,
1.),(1.,0.994190014771708,1.),(1.,1.00000947743974,1.),(1.,1.,1.)))
REPRESENTATION_ITEM('')
SURFACE()
);
#3964=(
BOUNDED_SURFACE()
B_SPLINE_SURFACE(3,2,((#256565,#256566,#256567),(#256568,#256569,#256570),
(#256571,#256572,#256573),(#256574,#256575,#256576),(#256577,#256578,#256579),
(#256580,#256581,#256582),(#256583,#256584,#256585),(#256586,#256587,#256588),
(#256589,#256590,#256591),(#256592,#256593,#256594),(#256595,#256596,#256597),
(#256598,#256599,#256600),(#256601,#256602,#256603),(#256604,#256605,#256606)),
 .UNSPECIFIED.,.F.,.F.,.F.)
B_SPLINE_SURFACE_WITH_KNOTS((4,2,2,2,2,2,4),(3,3),(0.003069338559775,0.00495218666169257,
0.00683503476361014,0.00871788286552772,0.0106007309674453,0.0143664271712804,
0.0181321233751156),(0.,1.),.UNSPECIFIED.)
GEOMETRIC_REPRESENTATION_ITEM()
RATIONAL_B_SPLINE_SURFACE(((1.,0.70710678118655,1.),(1.,0.73301158442153,
1.),(1.,0.756757437793674,1.),(1.,0.800574796193468,1.),(1.,0.82064592936982,
1.),(1.,0.85747561658249,1.),(1.,0.874266151415543,1.),(1.,0.904559499543433,
1.),(1.,0.917975383132164,1.),(1.,0.953491353959532,1.),(1.,0.970901198269014,
1.),(1.,0.994190014771708,1.),(1.,1.00000947743974,1.),(1.,1.,1.)))
REPRESENTATION_ITEM('')
SURFACE()
);
#3965=(
BOUNDED_SURFACE()
B_SPLINE_SURFACE(3,2,((#256612,#256613,#256614),(#256615,#256616,#256617),
(#256618,#256619,#256620),(#256621,#256622,#256623),(#256624,#256625,#256626),
(#256627,#256628,#256629),(#256630,#256631,#256632),(#256633,#256634,#256635),
(#256636,#256637,#256638),(#256639,#256640,#256641),(#256642,#256643,#256644),
(#256645,#256646,#256647),(#256648,#256649,#256650),(#256651,#256652,#256653)),
 .UNSPECIFIED.,.F.,.F.,.F.)
B_SPLINE_SURFACE_WITH_KNOTS((4,2,2,2,2,2,4),(3,3),(0.00306933855977502,
0.00495218666169259,0.00683503476361016,0.00871788286552773,0.0106007309674453,
0.0143664271712804,0.0181321233751156),(0.,1.),.UNSPECIFIED.)
GEOMETRIC_REPRESENTATION_ITEM()
RATIONAL_B_SPLINE_SURFACE(((1.,0.70710678118655,1.),(1.,0.73301158442153,
1.),(1.,0.756757437793674,1.),(1.,0.800574796193468,1.),(1.,0.820645929369924,
1.),(1.,0.857475616582386,1.),(1.,0.874266151416033,1.),(1.,0.904559499542943,
1.),(1.,0.917975383132164,1.),(1.,0.953491353959532,1.),(1.,0.970901198268875,
1.),(1.,0.994190014771847,1.),(1.,1.00000947743964,1.),(1.,1.,1.)))
REPRESENTATION_ITEM('')
SURFACE()
);
#3966=(
BOUNDED_SURFACE()
B_SPLINE_SURFACE(3,2,((#256757,#256758,#256759),(#256760,#256761,#256762),
(#256763,#256764,#256765),(#256766,#256767,#256768),(#256769,#256770,#256771),
(#256772,#256773,#256774),(#256775,#256776,#256777),(#256778,#256779,#256780),
(#256781,#256782,#256783),(#256784,#256785,#256786),(#256787,#256788,#256789),
(#256790,#256791,#256792),(#256793,#256794,#256795),(#256796,#256797,#256798)),
 .UNSPECIFIED.,.F.,.F.,.F.)
B_SPLINE_SURFACE_WITH_KNOTS((4,2,2,2,2,2,4),(3,3),(0.00306933855977502,
0.00495218666169259,0.00683503476361016,0.00871788286552773,0.0106007309674453,
0.0143664271712804,0.0181321233751156),(0.,1.),.UNSPECIFIED.)
GEOMETRIC_REPRESENTATION_ITEM()
RATIONAL_B_SPLINE_SURFACE(((1.,0.70710678118655,1.),(1.,0.73301158442153,
1.),(1.,0.756757437793674,1.),(1.,0.800574796193468,1.),(1.,0.820645929369924,
1.),(1.,0.857475616582386,1.),(1.,0.874266151416033,1.),(1.,0.904559499542943,
1.),(1.,0.917975383132164,1.),(1.,0.953491353959532,1.),(1.,0.970901198268875,
1.),(1.,0.994190014771847,1.),(1.,1.00000947743964,1.),(1.,1.,1.)))
REPRESENTATION_ITEM('')
SURFACE()
);
#3967=(
BOUNDED_SURFACE()
B_SPLINE_SURFACE(3,2,((#256801,#256802,#256803),(#256804,#256805,#256806),
(#256807,#256808,#256809),(#256810,#256811,#256812),(#256813,#256814,#256815),
(#256816,#256817,#256818),(#256819,#256820,#256821),(#256822,#256823,#256824),
(#256825,#256826,#256827),(#256828,#256829,#256830),(#256831,#256832,#256833),
(#256834,#256835,#256836),(#256837,#256838,#256839),(#256840,#256841,#256842)),
 .UNSPECIFIED.,.F.,.F.,.F.)
B_SPLINE_SURFACE_WITH_KNOTS((4,2,2,2,2,2,4),(3,3),(0.0165800150464154,0.0218443656748581,
0.0271029672948129,0.0376201705347225,0.048137373774632,0.0533959753945868,
0.0586603260230295),(0.,1.00000574900849),.UNSPECIFIED.)
GEOMETRIC_REPRESENTATION_ITEM()
RATIONAL_B_SPLINE_SURFACE(((1.,0.746871247280354,1.0000029104787),(1.,0.745462351055241,
1.00000292667821),(1.,0.744212008056876,1.00000294105467),(1.,0.742063457964921,
1.00000296575874),(1.,0.741161631619667,1.00000297612795),(1.,0.738982445187317,
1.00000300118428),(1.,0.738228768574483,1.00000300985006),(1.,0.738231075589957,
1.00000300982354),(1.,0.738986907486423,1.00000300113297),(1.,0.741166319133875,
1.00000297607406),(1.,0.742067724836351,1.00000296570968),(1.,0.744213991604145,
1.00000294103187),(1.,0.745461255089228,1.00000292669081),(1.,0.746871250867751,
1.00000291047865)))
REPRESENTATION_ITEM('')
SURFACE()
);
#3968=(
BOUNDED_SURFACE()
B_SPLINE_SURFACE(3,2,((#257652,#257653,#257654),(#257655,#257656,#257657),
(#257658,#257659,#257660),(#257661,#257662,#257663),(#257664,#257665,#257666),
(#257667,#257668,#257669),(#257670,#257671,#257672),(#257673,#257674,#257675),
(#257676,#257677,#257678),(#257679,#257680,#257681),(#257682,#257683,#257684),
(#257685,#257686,#257687),(#257688,#257689,#257690),(#257691,#257692,#257693),
(#257694,#257695,#257696),(#257697,#257698,#257699),(#257700,#257701,#257702),
(#257703,#257704,#257705),(#257706,#257707,#257708),(#257709,#257710,#257711),
(#257712,#257713,#257714),(#257715,#257716,#257717)),.UNSPECIFIED.,.F.,
 .F.,.F.)
B_SPLINE_SURFACE_WITH_KNOTS((4,2,2,2,2,2,2,2,2,2,4),(3,3),(0.00948259018043931,
0.0103154262700519,0.0111482623596645,0.0119810984492771,0.0123975164940833,
0.0128139345388896,0.0136467706285022,0.0144796067181148,0.0148960247629211,
0.0153124428077274,0.01614527889734),(0.,1.),.UNSPECIFIED.)
GEOMETRIC_REPRESENTATION_ITEM()
RATIONAL_B_SPLINE_SURFACE(((1.,0.748955720789,1.),(1.,0.760172974879871,
1.),(1.,0.771047258289343,1.),(1.,0.792164805631483,1.),(1.,0.80250638759394,
1.),(1.,0.821938683277389,1.),(1.,0.831055189778017,1.),(1.,0.843821930267136,
1.),(1.,0.847925078305043,1.),(1.,0.855808932317141,1.),(1.,0.859614300419405,
1.),(1.,0.870277583221261,1.),(1.,0.876401549840479,1.),(1.,0.886526706071859,
1.),(1.,0.890548210266271,1.),(1.,0.894400461302912,1.),(1.,0.895338782452369,
1.),(1.,0.896497135067161,1.),(1.,0.896712673869112,1.),(1.,0.89622893258817,
1.),(1.,0.894438559265301,1.),(1.,0.891217425172869,1.)))
REPRESENTATION_ITEM('')
SURFACE()
);
#3969=(
BOUNDED_SURFACE()
B_SPLINE_SURFACE(3,2,((#257892,#257893,#257894),(#257895,#257896,#257897),
(#257898,#257899,#257900),(#257901,#257902,#257903),(#257904,#257905,#257906),
(#257907,#257908,#257909),(#257910,#257911,#257912),(#257913,#257914,#257915),
(#257916,#257917,#257918),(#257919,#257920,#257921),(#257922,#257923,#257924),
(#257925,#257926,#257927),(#257928,#257929,#257930),(#257931,#257932,#257933),
(#257934,#257935,#257936),(#257937,#257938,#257939),(#257940,#257941,#257942),
(#257943,#257944,#257945),(#257946,#257947,#257948),(#257949,#257950,#257951)),
 .UNSPECIFIED.,.F.,.F.,.F.)
B_SPLINE_SURFACE_WITH_KNOTS((4,2,2,2,2,2,2,2,2,4),(3,3),(0.0112764198461947,
0.0121119087584978,0.0125296532146494,0.012947397670801,0.0137828865831041,
0.0146183754954072,0.0154538644077104,0.0162893533200135,0.0171248422323166,
0.0179603311446198),(0.,1.),.UNSPECIFIED.)
GEOMETRIC_REPRESENTATION_ITEM()
RATIONAL_B_SPLINE_SURFACE(((1.,0.89121897909325,1.),(1.,0.894429433227244,
1.),(1.,0.896207982264178,1.),(1.,0.896714045563393,1.),(1.,0.896515267970691,
1.),(1.,0.895381325101059,1.),(1.,0.894455556169836,1.),(1.,0.890656783919795,
1.),(1.,0.886687750370936,1.),(1.,0.876609320012727,1.),(1.,0.870508986223097,
1.),(1.,0.856349909354098,1.),(1.,0.84841920915651,1.),(1.,0.831316008677178,
1.),(1.,0.822011223917002,1.),(1.,0.8025589034124,1.),(1.,0.792407582621121,
1.),(1.,0.771230982137234,1.),(1.,0.760139004795012,1.),(1.,0.748955720789,
1.)))
REPRESENTATION_ITEM('')
SURFACE()
);
#3970=(
BOUNDED_SURFACE()
B_SPLINE_SURFACE(3,2,((#258120,#258121,#258122),(#258123,#258124,#258125),
(#258126,#258127,#258128),(#258129,#258130,#258131),(#258132,#258133,#258134),
(#258135,#258136,#258137),(#258138,#258139,#258140),(#258141,#258142,#258143),
(#258144,#258145,#258146),(#258147,#258148,#258149),(#258150,#258151,#258152),
(#258153,#258154,#258155),(#258156,#258157,#258158),(#258159,#258160,#258161),
(#258162,#258163,#258164),(#258165,#258166,#258167),(#258168,#258169,#258170),
(#258171,#258172,#258173),(#258174,#258175,#258176),(#258177,#258178,#258179),
(#258180,#258181,#258182),(#258183,#258184,#258185)),.UNSPECIFIED.,.F.,
 .F.,.F.)
B_SPLINE_SURFACE_WITH_KNOTS((4,2,2,2,2,2,2,2,2,2,4),(3,3),(0.0094825901804395,
0.0103154262700525,0.0111482623596655,0.0119810984492784,0.0123975164940849,
0.0128139345388914,0.0136467706285044,0.0144796067181174,0.0148960247629239,
0.0153124428077303,0.0161452788973433),(0.,1.),.UNSPECIFIED.)
GEOMETRIC_REPRESENTATION_ITEM()
RATIONAL_B_SPLINE_SURFACE(((1.,0.748955720789002,1.),(1.,0.76017297487987,
1.),(1.,0.771047258289371,1.),(1.,0.792164805631491,1.),(1.,0.802506387593797,
1.),(1.,0.821938683277595,1.),(1.,0.83105518977779,1.),(1.,0.843821930267307,
1.),(1.,0.847925078305022,1.),(1.,0.855808932317248,1.),(1.,0.859614300419415,
1.),(1.,0.87027758322137,1.),(1.,0.876401549840654,1.),(1.,0.88652670607176,
1.),(1.,0.890548210266293,1.),(1.,0.894400461302936,1.),(1.,0.895338782452428,
1.),(1.,0.896497135067126,1.),(1.,0.896712673869015,1.),(1.,0.896228932588355,
1.),(1.,0.894438559265128,1.),(1.,0.891217425172832,1.)))
REPRESENTATION_ITEM('')
SURFACE()
);
#3971=(
BOUNDED_SURFACE()
B_SPLINE_SURFACE(3,2,((#258360,#258361,#258362),(#258363,#258364,#258365),
(#258366,#258367,#258368),(#258369,#258370,#258371),(#258372,#258373,#258374),
(#258375,#258376,#258377),(#258378,#258379,#258380),(#258381,#258382,#258383),
(#258384,#258385,#258386),(#258387,#258388,#258389),(#258390,#258391,#258392),
(#258393,#258394,#258395),(#258396,#258397,#258398),(#258399,#258400,#258401),
(#258402,#258403,#258404),(#258405,#258406,#258407),(#258408,#258409,#258410),
(#258411,#258412,#258413),(#258414,#258415,#258416),(#258417,#258418,#258419)),
 .UNSPECIFIED.,.F.,.F.,.F.)
B_SPLINE_SURFACE_WITH_KNOTS((4,2,2,2,2,2,2,2,2,4),(3,3),(0.0112764198461948,
0.0121119087584979,0.0125296532146495,0.0129473976708011,0.0137828865831043,
0.0146183754954074,0.0154538644077106,0.0162893533200137,0.0171248422323169,
0.0179603311446201),(0.,1.),.UNSPECIFIED.)
GEOMETRIC_REPRESENTATION_ITEM()
RATIONAL_B_SPLINE_SURFACE(((1.,0.891218979093247,1.),(1.,0.89442943322708,
1.),(1.,0.896207982264393,1.),(1.,0.896714045563283,1.),(1.,0.896515267970747,
1.),(1.,0.895381325101006,1.),(1.,0.894455556169837,1.),(1.,0.890656783919796,
1.),(1.,0.886687750370708,1.),(1.,0.876609320012963,1.),(1.,0.870508986222868,
1.),(1.,0.856349909354336,1.),(1.,0.848419209156267,1.),(1.,0.831316008677429,
1.),(1.,0.822011223916974,1.),(1.,0.802558903412434,1.),(1.,0.792407582620859,
1.),(1.,0.771230982137498,1.),(1.,0.760139004794817,1.),(1.,0.748955720788999,
1.)))
REPRESENTATION_ITEM('')
SURFACE()
);
#3972=(
BOUNDED_SURFACE()
B_SPLINE_SURFACE(3,2,((#258588,#258589,#258590),(#258591,#258592,#258593),
(#258594,#258595,#258596),(#258597,#258598,#258599),(#258600,#258601,#258602),
(#258603,#258604,#258605),(#258606,#258607,#258608),(#258609,#258610,#258611),
(#258612,#258613,#258614),(#258615,#258616,#258617),(#258618,#258619,#258620),
(#258621,#258622,#258623),(#258624,#258625,#258626),(#258627,#258628,#258629),
(#258630,#258631,#258632),(#258633,#258634,#258635),(#258636,#258637,#258638),
(#258639,#258640,#258641),(#258642,#258643,#258644),(#258645,#258646,#258647),
(#258648,#258649,#258650),(#258651,#258652,#258653)),.UNSPECIFIED.,.F.,
 .F.,.F.)
B_SPLINE_SURFACE_WITH_KNOTS((4,2,2,2,2,2,2,2,2,2,4),(3,3),(0.00948259018043928,
0.0103154262700518,0.0111482623596644,0.011981098449277,0.0123975164940833,
0.0128139345388895,0.0136467706285021,0.0144796067181147,0.0148960247629209,
0.0153124428077272,0.0161452788973398),(0.,1.),.UNSPECIFIED.)
GEOMETRIC_REPRESENTATION_ITEM()
RATIONAL_B_SPLINE_SURFACE(((1.,0.748955720789,1.),(1.,0.760172974879684,
1.),(1.,0.771047258289592,1.),(1.,0.792164805631237,1.),(1.,0.8025063875938,
1.),(1.,0.821938683277527,1.),(1.,0.831055189777864,1.),(1.,0.843821930267213,
1.),(1.,0.847925078305238,1.),(1.,0.855808932316948,1.),(1.,0.859614300419269,
1.),(1.,0.870277583221523,1.),(1.,0.876401549840585,1.),(1.,0.886526706071749,
1.),(1.,0.890548210266254,1.),(1.,0.894400461302918,1.),(1.,0.895338782452494,
1.),(1.,0.896497135067036,1.),(1.,0.896712673869119,1.),(1.,0.896228932588154,
1.),(1.,0.894438559265315,1.),(1.,0.89121742517287,1.)))
REPRESENTATION_ITEM('')
SURFACE()
);
#3973=(
BOUNDED_SURFACE()
B_SPLINE_SURFACE(3,2,((#258828,#258829,#258830),(#258831,#258832,#258833),
(#258834,#258835,#258836),(#258837,#258838,#258839),(#258840,#258841,#258842),
(#258843,#258844,#258845),(#258846,#258847,#258848),(#258849,#258850,#258851),
(#258852,#258853,#258854),(#258855,#258856,#258857),(#258858,#258859,#258860),
(#258861,#258862,#258863),(#258864,#258865,#258866),(#258867,#258868,#258869),
(#258870,#258871,#258872),(#258873,#258874,#258875),(#258876,#258877,#258878),
(#258879,#258880,#258881)),.UNSPECIFIED.,.F.,.F.,.F.)
B_SPLINE_SURFACE_WITH_KNOTS((4,2,2,2,2,2,2,2,4),(3,3),(0.0113523220585582,
0.012178323194316,0.0125913237621948,0.0130043243300737,0.0138303254658314,
0.0146563266015892,0.0154823277373469,0.0163083288731046,0.0179603311446201),
(0.,1.),.UNSPECIFIED.)
GEOMETRIC_REPRESENTATION_ITEM()
RATIONAL_B_SPLINE_SURFACE(((1.,0.892059672490622,1.),(1.,0.89497186029643,
1.),(1.,0.896493669878046,1.),(1.,0.89665049960315,1.),(1.,0.896338830961171,
1.),(1.,0.895008636648382,1.),(1.,0.893996388994617,1.),(1.,0.889965092157251,
1.),(1.,0.885881976568346,1.),(1.,0.875677600351648,1.),(1.,0.869546831587427,
1.),(1.,0.855370301029908,1.),(1.,0.847491252571126,1.),(1.,0.83049125023834,
1.),(1.,0.82125667883682,1.),(1.,0.792351743707096,1.),(1.,0.771269968248487,
1.),(1.,0.748955720788999,1.)))
REPRESENTATION_ITEM('')
SURFACE()
);
#3974=(
BOUNDED_SURFACE()
B_SPLINE_SURFACE(3,2,((#259007,#259008,#259009),(#259010,#259011,#259012),
(#259013,#259014,#259015),(#259016,#259017,#259018),(#259019,#259020,#259021),
(#259022,#259023,#259024),(#259025,#259026,#259027),(#259028,#259029,#259030),
(#259031,#259032,#259033),(#259034,#259035,#259036),(#259037,#259038,#259039),
(#259040,#259041,#259042),(#259043,#259044,#259045),(#259046,#259047,#259048),
(#259049,#259050,#259051),(#259052,#259053,#259054),(#259055,#259056,#259057),
(#259058,#259059,#259060),(#259061,#259062,#259063),(#259064,#259065,#259066)),
 .UNSPECIFIED.,.F.,.F.,.F.)
B_SPLINE_SURFACE_WITH_KNOTS((4,2,2,2,2,2,2,2,2,4),(3,3),(0.0112764198461918,
0.0121119087584954,0.0125296532146471,0.0129473976707989,0.0137828865831024,
0.0146183754954059,0.0154538644077094,0.016289353320013,0.0171248422323165,
0.01796033114462),(0.,1.),.UNSPECIFIED.)
GEOMETRIC_REPRESENTATION_ITEM()
RATIONAL_B_SPLINE_SURFACE(((1.,0.891218979093214,1.),(1.,0.894429433227121,
1.),(1.,0.896207982264297,1.),(1.,0.896714045563326,1.),(1.,0.896515267970734,
1.),(1.,0.895381325101037,1.),(1.,0.894455556169857,1.),(1.,0.890656783919815,
1.),(1.,0.88668775037085,1.),(1.,0.876609320012884,1.),(1.,0.870508986223,
1.),(1.,0.856349909354275,1.),(1.,0.848419209156365,1.),(1.,0.831316008677397,
1.),(1.,0.822011223917237,1.),(1.,0.802558903412222,1.),(1.,0.792407582620879,
1.),(1.,0.771230982137509,1.),(1.,0.760139004794819,1.),(1.,0.748955720789001,
1.)))
REPRESENTATION_ITEM('')
SURFACE()
);
#3975=(
BOUNDED_SURFACE()
B_SPLINE_SURFACE(3,2,((#259238,#259239,#259240),(#259241,#259242,#259243),
(#259244,#259245,#259246),(#259247,#259248,#259249),(#259250,#259251,#259252),
(#259253,#259254,#259255),(#259256,#259257,#259258),(#259259,#259260,#259261),
(#259262,#259263,#259264),(#259265,#259266,#259267),(#259268,#259269,#259270),
(#259271,#259272,#259273),(#259274,#259275,#259276),(#259277,#259278,#259279),
(#259280,#259281,#259282),(#259283,#259284,#259285),(#259286,#259287,#259288),
(#259289,#259290,#259291),(#259292,#259293,#259294),(#259295,#259296,#259297),
(#259298,#259299,#259300),(#259301,#259302,#259303)),.UNSPECIFIED.,.F.,
 .F.,.F.)
B_SPLINE_SURFACE_WITH_KNOTS((4,2,2,2,2,2,2,2,2,2,4),(3,3),(0.00948259018043951,
0.0103154262700521,0.0111482623596647,0.0119810984492773,0.0123975164940836,
0.0128139345388899,0.0136467706285025,0.0144796067181151,0.0148960247629214,
0.0153124428077277,0.0161452788973402),(0.,1.),.UNSPECIFIED.)
GEOMETRIC_REPRESENTATION_ITEM()
RATIONAL_B_SPLINE_SURFACE(((1.,0.748955720789002,1.),(1.,0.760172974879873,
1.),(1.,0.771047258289347,1.),(1.,0.792164805631487,1.),(1.,0.802506387594021,
1.),(1.,0.821938683277315,1.),(1.,0.831055189777944,1.),(1.,0.843821930267178,
1.),(1.,0.847925078304869,1.),(1.,0.855808932317324,1.),(1.,0.859614300419331,
1.),(1.,0.870277583221421,1.),(1.,0.87640154984062,1.),(1.,0.886526706071721,
1.),(1.,0.890548210266257,1.),(1.,0.894400461302922,1.),(1.,0.895338782452309,
1.),(1.,0.896497135067225,1.),(1.,0.896712673869011,1.),(1.,0.896228932588374,
1.),(1.,0.894438559265147,1.),(1.,0.891217425172868,1.)))
REPRESENTATION_ITEM('')
SURFACE()
);
#3976=(
BOUNDED_SURFACE()
B_SPLINE_SURFACE(3,2,((#259475,#259476,#259477),(#259478,#259479,#259480),
(#259481,#259482,#259483),(#259484,#259485,#259486)),.UNSPECIFIED.,.F.,
 .F.,.F.)
B_SPLINE_SURFACE_WITH_KNOTS((4,4),(3,3),(0.,0.0230962378966021),(0.,1.),
 .UNSPECIFIED.)
GEOMETRIC_REPRESENTATION_ITEM()
RATIONAL_B_SPLINE_SURFACE(((1.,0.75328262365528,1.),(1.,0.753799666532188,
1.),(1.,0.754334066265409,1.),(1.,0.754887701397112,1.)))
REPRESENTATION_ITEM('')
SURFACE()
);
#3977=(
BOUNDED_SURFACE()
B_SPLINE_SURFACE(3,2,((#259540,#259541,#259542),(#259543,#259544,#259545),
(#259546,#259547,#259548),(#259549,#259550,#259551)),.UNSPECIFIED.,.F.,
 .F.,.F.)
B_SPLINE_SURFACE_WITH_KNOTS((4,4),(3,3),(0.,0.000930412332424302),(0.,1.),
 .UNSPECIFIED.)
GEOMETRIC_REPRESENTATION_ITEM()
RATIONAL_B_SPLINE_SURFACE(((1.,0.753587188732319,1.),(1.,0.753587087859367,
1.),(1.,0.75348573487314,1.),(1.,0.75328262365528,1.)))
REPRESENTATION_ITEM('')
SURFACE()
);
#3978=(
BOUNDED_SURFACE()
B_SPLINE_SURFACE(3,2,((#259560,#259561,#259562),(#259563,#259564,#259565),
(#259566,#259567,#259568),(#259569,#259570,#259571)),.UNSPECIFIED.,.F.,
 .F.,.F.)
B_SPLINE_SURFACE_WITH_KNOTS((4,4),(3,3),(0.,0.023096237896602),(0.,1.),
 .UNSPECIFIED.)
GEOMETRIC_REPRESENTATION_ITEM()
RATIONAL_B_SPLINE_SURFACE(((1.,0.75328262365528,1.),(1.,0.753799666532188,
1.),(1.,0.75433406626541,1.),(1.,0.754887701397112,1.)))
REPRESENTATION_ITEM('')
SURFACE()
);
#3979=(
BOUNDED_SURFACE()
B_SPLINE_SURFACE(3,2,((#259613,#259614,#259615),(#259616,#259617,#259618),
(#259619,#259620,#259621),(#259622,#259623,#259624)),.UNSPECIFIED.,.F.,
 .F.,.F.)
B_SPLINE_SURFACE_WITH_KNOTS((4,4),(3,3),(-3.03576608295941E-18,0.000930412332424306),
(0.,1.),.UNSPECIFIED.)
GEOMETRIC_REPRESENTATION_ITEM()
RATIONAL_B_SPLINE_SURFACE(((1.,0.753587188732319,1.),(1.,0.753587087859366,
1.),(1.,0.75348573487314,1.),(1.,0.75328262365528,1.)))
REPRESENTATION_ITEM('')
SURFACE()
);
#3980=(
BOUNDED_SURFACE()
B_SPLINE_SURFACE(3,2,((#259633,#259634,#259635),(#259636,#259637,#259638),
(#259639,#259640,#259641),(#259642,#259643,#259644),(#259645,#259646,#259647),
(#259648,#259649,#259650)),.UNSPECIFIED.,.F.,.F.,.F.)
B_SPLINE_SURFACE_WITH_KNOTS((4,2,4),(3,3),(-1.65496705948116E-5,0.0175045710699778,
0.0350091421399555),(-1.65496705948116E-5,1.),.UNSPECIFIED.)
GEOMETRIC_REPRESENTATION_ITEM()
RATIONAL_B_SPLINE_SURFACE(((1.00000066361291,0.979950872403389,1.),(1.00000060946638,
0.981586752043857,1.),(1.00000054507474,0.983532157510661,1.),(1.00000038175755,
0.988466309672037,1.),(1.00000028087796,0.991514092184472,1.),(1.00000016544838,
0.995001460146994,1.)))
REPRESENTATION_ITEM('')
SURFACE()
);
#3981=(
BOUNDED_SURFACE()
B_SPLINE_SURFACE(3,2,((#259653,#259654,#259655),(#259656,#259657,#259658),
(#259659,#259660,#259661),(#259662,#259663,#259664),(#259665,#259666,#259667),
(#259668,#259669,#259670)),.UNSPECIFIED.,.F.,.F.,.F.)
B_SPLINE_SURFACE_WITH_KNOTS((4,2,4),(3,3),(-1.65496862290218E-5,0.0175045710699895,
0.0350091421399791),(0.,1.00001654968623),.UNSPECIFIED.)
GEOMETRIC_REPRESENTATION_ITEM()
RATIONAL_B_SPLINE_SURFACE(((1.,0.979950872398696,1.00000066361354),(1.,
0.981586752040342,1.00000060946695),(1.,0.98353215750788,1.00000054507525),
(1.,0.988466309672187,1.00000038175791),(1.,0.991514092184107,1.00000028087822),
(1.,0.99500146014693,1.00000016544853)))
REPRESENTATION_ITEM('')
SURFACE()
);
#3982=(
BOUNDED_SURFACE()
B_SPLINE_SURFACE(3,2,((#259673,#259674,#259675),(#259676,#259677,#259678),
(#259679,#259680,#259681),(#259682,#259683,#259684),(#259685,#259686,#259687),
(#259688,#259689,#259690),(#259691,#259692,#259693),(#259694,#259695,#259696),
(#259697,#259698,#259699),(#259700,#259701,#259702)),.UNSPECIFIED.,.F.,
 .F.,.F.)
B_SPLINE_SURFACE_WITH_KNOTS((4,2,2,2,4),(3,3),(0.0086793904370147,0.0137994096303372,
0.0163087030209128,0.0188179964114884,0.0289567865427477),(-0.000220356291476092,
1.),.UNSPECIFIED.)
GEOMETRIC_REPRESENTATION_ITEM()
RATIONAL_B_SPLINE_SURFACE(((1.0001233642456,0.720080046788299,0.999999999999999),
(1.00012059154998,0.726371438799624,1.),(1.00011860533177,0.73087827224561,
1.),(1.00011665984081,0.735292693407743,1.),(1.00011618394181,0.736372533239929,
1.),(1.00011554908712,0.737813051874643,1.),(1.00011539013292,0.738173727316974,
1.),(1.00011539009736,0.738173807996126,1.),(1.00011790792365,0.732460727893791,
1.),(1.00012336347158,0.720081803084609,1.)))
REPRESENTATION_ITEM('')
SURFACE()
);
#3983=(
BOUNDED_SURFACE()
B_SPLINE_SURFACE(3,2,((#259703,#259704,#259705),(#259706,#259707,#259708),
(#259709,#259710,#259711),(#259712,#259713,#259714)),.UNSPECIFIED.,.F.,
 .F.,.F.)
B_SPLINE_SURFACE_WITH_KNOTS((4,4),(3,3),(-1.0256276502154E-5,0.000591581032812799),
(0.,1.00225319390743),.UNSPECIFIED.)
GEOMETRIC_REPRESENTATION_ITEM()
RATIONAL_B_SPLINE_SURFACE(((1.,1.,1.),(1.,0.999985346901776,1.00000006603254),
(1.,0.99550874156864,1.00002023935227),(1.,0.988241468901958,1.00005298850126)))
REPRESENTATION_ITEM('')
SURFACE()
);
#3984=(
BOUNDED_SURFACE()
B_SPLINE_SURFACE(3,2,((#259725,#259726,#259727),(#259728,#259729,#259730),
(#259731,#259732,#259733),(#259734,#259735,#259736)),.UNSPECIFIED.,.F.,
 .F.,.F.)
B_SPLINE_SURFACE_WITH_KNOTS((4,4),(3,3),(-2.90836419617607E-14,0.000545703078886337),
(-0.00848691895860184,1.),.UNSPECIFIED.)
GEOMETRIC_REPRESENTATION_ITEM()
RATIONAL_B_SPLINE_SURFACE(((1.00000837657878,0.999506500603085,1.),(1.00000181717849,
0.999892942391636,1.),(1.00000000707574,0.999999583138454,1.),(1.,1.,1.)))
REPRESENTATION_ITEM('')
SURFACE()
);
#3985=(
BOUNDED_SURFACE()
B_SPLINE_SURFACE(3,2,((#259738,#259739,#259740),(#259741,#259742,#259743),
(#259744,#259745,#259746),(#259747,#259748,#259749),(#259750,#259751,#259752),
(#259753,#259754,#259755),(#259756,#259757,#259758),(#259759,#259760,#259761),
(#259762,#259763,#259764),(#259765,#259766,#259767),(#259768,#259769,#259770),
(#259771,#259772,#259773),(#259774,#259775,#259776),(#259777,#259778,#259779),
(#259780,#259781,#259782),(#259783,#259784,#259785),(#259786,#259787,#259788),
(#259789,#259790,#259791),(#259792,#259793,#259794),(#259795,#259796,#259797),
(#259798,#259799,#259800),(#259801,#259802,#259803),(#259804,#259805,#259806),
(#259807,#259808,#259809)),.UNSPECIFIED.,.F.,.F.,.F.)
B_SPLINE_SURFACE_WITH_KNOTS((4,2,2,2,2,2,2,2,2,2,2,4),(3,3),(0.00710973580532299,
0.00820484501164228,0.00898706587329885,0.00976928673495541,0.0101603971657837,
0.0103559523811978,0.0104537299889049,0.0104781743908317,0.0105026187927584,
0.0105270631946852,0.0105392853956486,0.0108643959412746),(-0.000692463643722109,
1.00461072647643),.UNSPECIFIED.)
GEOMETRIC_REPRESENTATION_ITEM()
RATIONAL_B_SPLINE_SURFACE(((1.00000418087808,0.996967228287315,1.00002794712048),
(1.00000539179128,0.996088842637076,1.00003604148165),(1.00000726417762,
0.994730630263104,1.00004855746652),(1.00001073944744,0.992209700500032,
1.00007178794164),(1.00001228661455,0.991087399257731,1.00008212999538),
(1.00001544659885,0.988795174797729,1.00010325294139),(1.00001711982762,
0.987581429549803,1.00011443765554),(1.00001894473692,0.986257656599376,
1.00012663627965),(1.00001951290412,0.985845513177767,1.00013043419883),
(1.00001922291158,0.98605587117993,1.00012849574088),(1.00001901775458,
0.986204690244211,1.00012712436687),(1.00001719907502,0.987523944194307,
1.00011496738554),(1.00001645641015,0.98806266667551,1.00011000303493),
(1.0000138946614,0.989920936399478,1.00009287900029),(1.00001328788623,
0.990361085704145,1.0000888230057),(1.00001167839794,0.991528594169834,
1.00007806436548),(1.00001068816558,0.992246899899225,1.00007144514759),
(1.00000775165148,0.99437702106797,1.00005181599031),(1.00000547142344,
0.996031078173962,1.00003657378364),(1.000002398545,0.998260116824386,1.00001603309756),
(1.00000153695282,0.998885108118202,1.00001027377617),(0.999987792404643,
1.00885528092366,0.999918398209191),(1.00027966865476,0.797130849193336,
1.00186944786376),(0.997855728441201,2.55543548703647,0.985666595749524)))
REPRESENTATION_ITEM('')
SURFACE()
);
#3986=(
BOUNDED_SURFACE()
B_SPLINE_SURFACE(3,2,((#259811,#259812,#259813),(#259814,#259815,#259816),
(#259817,#259818,#259819),(#259820,#259821,#259822)),.UNSPECIFIED.,.F.,
 .F.,.F.)
B_SPLINE_SURFACE_WITH_KNOTS((4,4),(3,3),(-2.85745148634754E-5,0.000314319663498228),
(0.,1.00095479621378),.UNSPECIFIED.)
GEOMETRIC_REPRESENTATION_ITEM()
RATIONAL_B_SPLINE_SURFACE(((1.,0.995946994781572,1.00000773958807),(1.,
0.996651841079251,1.00000639361892),(1.,0.997316919425854,1.00000512359035),
(1.,0.997737992799635,1.00000431951182)))
REPRESENTATION_ITEM('')
SURFACE()
);
#3987=(
BOUNDED_SURFACE()
B_SPLINE_SURFACE(3,2,((#259824,#259825,#259826),(#259827,#259828,#259829),
(#259830,#259831,#259832),(#259833,#259834,#259835)),.UNSPECIFIED.,.F.,
 .F.,.F.)
B_SPLINE_SURFACE_WITH_KNOTS((4,4),(3,3),(0.,0.000609810285548055),(0.,1.),
 .UNSPECIFIED.)
GEOMETRIC_REPRESENTATION_ITEM()
RATIONAL_B_SPLINE_SURFACE(((1.,0.99763002205783,1.),(1.,0.999169954497569,
1.),(1.,1.00000047407105,1.),(1.,1.,1.)))
REPRESENTATION_ITEM('')
SURFACE()
);
#3988=(
BOUNDED_SURFACE()
B_SPLINE_SURFACE(3,2,((#259836,#259837,#259838),(#259839,#259840,#259841),
(#259842,#259843,#259844),(#259845,#259846,#259847),(#259848,#259849,#259850),
(#259851,#259852,#259853),(#259854,#259855,#259856),(#259857,#259858,#259859),
(#259860,#259861,#259862),(#259863,#259864,#259865),(#259866,#259867,#259868),
(#259869,#259870,#259871),(#259872,#259873,#259874),(#259875,#259876,#259877),
(#259878,#259879,#259880),(#259881,#259882,#259883),(#259884,#259885,#259886),
(#259887,#259888,#259889),(#259890,#259891,#259892),(#259893,#259894,#259895),
(#259896,#259897,#259898),(#259899,#259900,#259901),(#259902,#259903,#259904),
(#259905,#259906,#259907),(#259908,#259909,#259910),(#259911,#259912,#259913),
(#259914,#259915,#259916),(#259917,#259918,#259919),(#259920,#259921,#259922),
(#259923,#259924,#259925),(#259926,#259927,#259928),(#259929,#259930,#259931),
(#259932,#259933,#259934),(#259935,#259936,#259937),(#259938,#259939,#259940),
(#259941,#259942,#259943)),.UNSPECIFIED.,.F.,.F.,.F.)
B_SPLINE_SURFACE_WITH_KNOTS((4,2,2,2,2,2,2,2,2,2,2,2,2,2,2,2,2,4),(3,3),
(-0.000333469135128296,0.000833672837820777,0.00166734567564155,0.00250101851346233,
0.00270943672291753,0.00291785493237272,0.00302206403710032,0.00307416858946412,
0.00310022086564602,0.00312627314182791,0.00313929927991886,0.00315232541800981,
0.00316535155610076,0.00317186462514624,0.00317837769419171,0.00320442997037361,
0.00323048224655551,0.00364829276517634),(0.,1.00460570884614),
 .UNSPECIFIED.)
GEOMETRIC_REPRESENTATION_ITEM()
RATIONAL_B_SPLINE_SURFACE(((1.,0.997054706395359,1.00002713032962),(1.,
0.99605271523388,1.00003636008873),(1.,0.994673259186161,1.00004906683457),
(1.,0.992006802794343,1.00007362867816),(1.,0.990790384906993,1.00008483361141),
(1.,0.988393785580759,1.00010690968884),(1.,0.987091346369295,1.00011890700044),
(1.,0.986150203297001,1.00012757626238),(1.,0.986003642672709,1.00012892629351),
(1.,0.98594923782718,1.00012942743927),(1.,0.986000799357347,1.00012895248448),
(1.,0.986777873089688,1.00012179453375),(1.,0.987137483619352,1.00011848201096),
(1.,0.988298093339298,1.00010779115005),(1.,0.988782642230707,1.00010332776782),
(1.,0.989957253593815,1.00009250793192),(1.,0.990423861711881,1.00008820980965),
(1.,0.991688273857576,1.00007656278124),(1.,0.99247603863951,1.00006930635079),
(1.,0.994284431414231,1.00005264848959),(1.,0.995010326911407,1.00004596196297),
(1.,0.996626426244886,1.00003107539697),(1.,0.997501337999239,1.00002301621936),
(1.,0.998874113903667,1.00001037100711),(1.,0.999376314879074,1.00000574502416),
(1.,0.999608475942123,1.00000360649163),(1.,0.999592989064556,1.00000374914773),
(1.,0.999491456297205,1.00000468440846),(1.,0.99940936032604,1.00000544062874),
(1.,0.998997449457976,1.0000092349118),(1.,0.998651286170311,1.00001242356643),
(1.,0.998071024137407,1.00001776860239),(1.,0.997813344969381,1.00002014219284),
(1.,0.993788013597043,1.00005722120146),(1.,0.995307700675226,1.00004322272902),
(0.999999999999997,0.985483842090745,1.00013371439379)))
REPRESENTATION_ITEM('')
SURFACE()
);
#3989=(
BOUNDED_SURFACE()
B_SPLINE_SURFACE(3,2,((#259945,#259946,#259947),(#259948,#259949,#259950),
(#259951,#259952,#259953),(#259954,#259955,#259956)),.UNSPECIFIED.,.F.,
 .F.,.F.)
B_SPLINE_SURFACE_WITH_KNOTS((4,4),(3,3),(-2.85745148645305E-5,0.000314319663509816),
(0.,1.00095479655756),.UNSPECIFIED.)
GEOMETRIC_REPRESENTATION_ITEM()
RATIONAL_B_SPLINE_SURFACE(((1.,0.997737992798767,1.00000431951338),(1.,
0.997316919425135,1.00000512359219),(1.,0.99665184107804,1.00000639362123),
(1.,0.995946994780193,1.00000773959086)))
REPRESENTATION_ITEM('')
SURFACE()
);
#3990=(
BOUNDED_SURFACE()
B_SPLINE_SURFACE(3,2,((#259958,#259959,#259960),(#259961,#259962,#259963),
(#259964,#259965,#259966),(#259967,#259968,#259969)),.UNSPECIFIED.,.F.,
 .F.,.F.)
B_SPLINE_SURFACE_WITH_KNOTS((4,4),(3,3),(-3.03576608295941E-18,0.000609810285535259),
(0.,1.),.UNSPECIFIED.)
GEOMETRIC_REPRESENTATION_ITEM()
RATIONAL_B_SPLINE_SURFACE(((1.,0.997630022057913,1.),(1.,0.999169954497594,
1.),(1.,1.00000047407104,1.),(1.,1.,1.)))
REPRESENTATION_ITEM('')
SURFACE()
);
#3991=(
BOUNDED_SURFACE()
B_SPLINE_SURFACE(3,2,((#259970,#259971,#259972),(#259973,#259974,#259975),
(#259976,#259977,#259978),(#259979,#259980,#259981),(#259982,#259983,#259984),
(#259985,#259986,#259987),(#259988,#259989,#259990),(#259991,#259992,#259993),
(#259994,#259995,#259996),(#259997,#259998,#259999),(#260000,#260001,#260002),
(#260003,#260004,#260005),(#260006,#260007,#260008),(#260009,#260010,#260011),
(#260012,#260013,#260014),(#260015,#260016,#260017),(#260018,#260019,#260020),
(#260021,#260022,#260023),(#260024,#260025,#260026),(#260027,#260028,#260029),
(#260030,#260031,#260032),(#260033,#260034,#260035),(#260036,#260037,#260038),
(#260039,#260040,#260041),(#260042,#260043,#260044),(#260045,#260046,#260047),
(#260048,#260049,#260050),(#260051,#260052,#260053),(#260054,#260055,#260056),
(#260057,#260058,#260059),(#260060,#260061,#260062),(#260063,#260064,#260065),
(#260066,#260067,#260068),(#260069,#260070,#260071),(#260072,#260073,#260074),
(#260075,#260076,#260077),(#260078,#260079,#260080),(#260081,#260082,#260083)),
 .UNSPECIFIED.,.F.,.F.,.F.)
B_SPLINE_SURFACE_WITH_KNOTS((4,2,2,2,2,2,2,2,2,2,2,2,2,2,2,2,2,2,4),(3,
3),(-0.000333361155037782,0.000833402887594952,0.0016668057751899,0.00250020866278486,
0.00270855938468359,0.00291691010658233,0.0030210854675317,0.00307317314800638,
0.00309921698824373,0.00312526082848107,0.00313828274859974,0.00315130466871841,
0.00316432658883708,0.00317083754889642,0.00317734850895575,0.00319037042907442,
0.0032033923491931,0.00322943618943044,0.00364710253335728),(-0.00578770259235711,
1.),.UNSPECIFIED.)
GEOMETRIC_REPRESENTATION_ITEM()
RATIONAL_B_SPLINE_SURFACE(((1.00003412924228,0.997051572559778,1.),(1.00004574779706,
0.996047844863059,1.),(1.00006173418376,0.994666779885507,1.),(1.00009261872355,
0.991998662502961,1.),(1.00010672130462,0.990780339615383,1.),(1.00013449167914,
0.9883812551701,1.),(1.00014956154484,0.987079368501341,1.),(1.00016049009589,
0.986135250271367,1.),(1.00016219281536,0.985988152226901,1.),(1.00016284042277,
0.985932205381424,1.),(1.0001622503025,0.985983185909607,1.),(1.0001533122673,
0.986755343345934,1.),(1.00014917060097,0.987113142167373,1.),(1.00013582833498,
0.988265781386087,1.),(1.00013025774237,0.98874702524063,1.),(1.00011679689681,
0.989909908556455,1.),(1.00011145395186,0.990371485915094,1.),(1.0000970158952,
0.991618790560121,1.),(1.00008804413747,0.99239386128949,1.),(1.0000674722456,
0.99417106835355,1.),(1.0000592294594,0.994883163184569,1.),(1.00004065487868,
0.996487822410277,1.),(1.0000304112453,0.997372770558565,1.),(1.00001405173748,
0.998786069493821,1.),(1.00000795752204,0.999312549158501,1.),(1.00000465267014,
0.999598055526461,1.),(1.00000463105855,0.999599922553604,1.),(1.00000563530084,
0.99951316599758,1.),(1.00000656546673,0.999432808905664,1.),(1.00000942801062,
0.999185513555113,1.),(1.00001147197509,0.999008935332597,1.),(1.00001530309848,
0.998677964335571,1.),(1.00001710470033,0.998522323835872,1.),(1.00002219973076,
0.998082163829078,1.),(1.00002520463239,0.997822570182858,1.),(1.00007209350726,
0.993771837260874,1.),(1.00005489075981,0.99525798372191,1.),(1.00016523340031,
0.985725475896788,1.)))
REPRESENTATION_ITEM('')
SURFACE()
);
#3992=(
BOUNDED_SURFACE()
B_SPLINE_SURFACE(3,2,((#260085,#260086,#260087),(#260088,#260089,#260090),
(#260091,#260092,#260093),(#260094,#260095,#260096)),.UNSPECIFIED.,.F.,
 .F.,.F.)
B_SPLINE_SURFACE_WITH_KNOTS((4,4),(3,3),(-2.85745148634742E-5,0.000314319663498371),
(0.,1.00095479620998),.UNSPECIFIED.)
GEOMETRIC_REPRESENTATION_ITEM()
RATIONAL_B_SPLINE_SURFACE(((1.,0.995946994781608,1.00000773958804),(1.,
0.996651841079179,1.0000063936189),(1.,0.997316919426007,1.00000512359033),
(1.,0.997737992799513,1.0000043195118)))
REPRESENTATION_ITEM('')
SURFACE()
);
#3993=(
BOUNDED_SURFACE()
B_SPLINE_SURFACE(3,2,((#260098,#260099,#260100),(#260101,#260102,#260103),
(#260104,#260105,#260106),(#260107,#260108,#260109)),.UNSPECIFIED.,.F.,
 .F.,.F.)
B_SPLINE_SURFACE_WITH_KNOTS((4,4),(3,3),(2.16840434497101E-19,0.000609810285548116),
(0.,1.),.UNSPECIFIED.)
GEOMETRIC_REPRESENTATION_ITEM()
RATIONAL_B_SPLINE_SURFACE(((1.,0.99763002205783,1.),(1.,0.999169954497568,
1.),(1.,1.00000047407105,1.),(1.,1.,1.)))
REPRESENTATION_ITEM('')
SURFACE()
);
#3994=(
BOUNDED_SURFACE()
B_SPLINE_SURFACE(3,2,((#260110,#260111,#260112),(#260113,#260114,#260115),
(#260116,#260117,#260118),(#260119,#260120,#260121),(#260122,#260123,#260124),
(#260125,#260126,#260127),(#260128,#260129,#260130),(#260131,#260132,#260133),
(#260134,#260135,#260136),(#260137,#260138,#260139),(#260140,#260141,#260142),
(#260143,#260144,#260145),(#260146,#260147,#260148),(#260149,#260150,#260151),
(#260152,#260153,#260154),(#260155,#260156,#260157),(#260158,#260159,#260160),
(#260161,#260162,#260163),(#260164,#260165,#260166),(#260167,#260168,#260169),
(#260170,#260171,#260172),(#260173,#260174,#260175),(#260176,#260177,#260178),
(#260179,#260180,#260181),(#260182,#260183,#260184),(#260185,#260186,#260187),
(#260188,#260189,#260190),(#260191,#260192,#260193),(#260194,#260195,#260196),
(#260197,#260198,#260199),(#260200,#260201,#260202),(#260203,#260204,#260205),
(#260206,#260207,#260208),(#260209,#260210,#260211),(#260212,#260213,#260214),
(#260215,#260216,#260217)),.UNSPECIFIED.,.F.,.F.,.F.)
B_SPLINE_SURFACE_WITH_KNOTS((4,2,2,2,2,2,2,2,2,2,2,2,2,2,2,2,2,4),(3,3),
(0.,0.000833672837821486,0.00166734567564297,0.00250101851346446,0.00270943672291983,
0.0029178549323752,0.00302206403710289,0.00307416858946673,0.00310022086564865,
0.00312627314183057,0.00313929927992153,0.00315232541801249,0.00316535155610345,
0.00317186462514893,0.00317837769419441,0.00320442997037634,0.00323048224655826,
0.00364829276517993),(0.,1.00358549869618),.UNSPECIFIED.)
GEOMETRIC_REPRESENTATION_ITEM()
RATIONAL_B_SPLINE_SURFACE(((1.,0.99611206821392,1.0000278803487),(1.,0.995254912868937,
1.00003402700744),(1.,0.994234710580471,1.00004134287539),(1.,0.992014920149054,
1.00005726098679),(1.,0.990799737574257,1.00006597505786),(1.,0.988405572073208,
1.00008314361243),(1.,0.987104455530704,1.00009247391576),(1.,0.986164268221475,
1.00009921599651),(1.,0.986017856433839,1.00010026591505),(1.,0.985963506838659,
1.00010065565586),(1.,0.986015016006277,1.00010028628375),(1.,0.986791300594523,
1.00009471954899),(1.,0.987150545928039,1.00009214340164),(1.,0.9883099770105,
1.00008382912437),(1.,0.988794033826467,1.00008035795421),(1.,0.989967452333396,
1.00007194337316),(1.,0.990433586595655,1.00006860072558),(1.,0.991696714688982,
1.00005954283731),(1.,0.992483679469992,1.00005389951492),(1.,0.994290235762475,
1.00004094470446),(1.,0.995015394088985,1.00003574459599),(1.,0.99662985222034,
1.00002416732094),(1.,0.997503875472981,1.00001789970247),(1.,0.998875257278488,
1.00000806552712),(1.,0.999376948252015,1.00000446790246),(1.,0.999608873547708,
1.00000280476677),(1.,0.999593402397524,1.00000291571035),(1.,0.999491972739996,
1.00000364306216),(1.,0.999409960139993,1.0000042311743),(1.,0.998998467580922,
1.00000718198637),(1.,0.998652655833498,1.0000096618015),(1.,0.998072983075812,
1.00001381863334),(1.,0.997815565589447,1.00001566457346),(1.,0.993794322073923,
1.00004450090023),(1.,0.995312465856801,1.00003361429512),(1.,0.985498583743996,
1.00010398961816)))
REPRESENTATION_ITEM('')
SURFACE()
);
#3995=(
BOUNDED_SURFACE()
B_SPLINE_SURFACE(3,2,((#260219,#260220,#260221),(#260222,#260223,#260224),
(#260225,#260226,#260227),(#260228,#260229,#260230)),.UNSPECIFIED.,.F.,
 .F.,.F.)
B_SPLINE_SURFACE_WITH_KNOTS((4,4),(3,3),(-2.85745148645381E-5,0.000314319663509926),
(0.,1.00095479654686),.UNSPECIFIED.)
GEOMETRIC_REPRESENTATION_ITEM()
RATIONAL_B_SPLINE_SURFACE(((1.,0.997737992798791,1.00000431951333),(1.,
0.997316919425162,1.00000512359214),(1.,0.996651841078075,1.00000639362115),
(1.,0.995946994780235,1.00000773959078)))
REPRESENTATION_ITEM('')
SURFACE()
);
#3996=(
BOUNDED_SURFACE()
B_SPLINE_SURFACE(3,2,((#260232,#260233,#260234),(#260235,#260236,#260237),
(#260238,#260239,#260240),(#260241,#260242,#260243)),.UNSPECIFIED.,.F.,
 .F.,.F.)
B_SPLINE_SURFACE_WITH_KNOTS((4,4),(3,3),(-1.30104260698261E-17,0.00060981028553535),
(0.,1.),.UNSPECIFIED.)
GEOMETRIC_REPRESENTATION_ITEM()
RATIONAL_B_SPLINE_SURFACE(((1.,0.997630022057914,1.),(1.,0.999169954497593,
1.),(1.,1.00000047407104,1.),(1.,1.,1.)))
REPRESENTATION_ITEM('')
SURFACE()
);
#3997=(
BOUNDED_SURFACE()
B_SPLINE_SURFACE(3,2,((#260244,#260245,#260246),(#260247,#260248,#260249),
(#260250,#260251,#260252),(#260253,#260254,#260255),(#260256,#260257,#260258),
(#260259,#260260,#260261),(#260262,#260263,#260264),(#260265,#260266,#260267),
(#260268,#260269,#260270),(#260271,#260272,#260273),(#260274,#260275,#260276),
(#260277,#260278,#260279),(#260280,#260281,#260282),(#260283,#260284,#260285),
(#260286,#260287,#260288),(#260289,#260290,#260291),(#260292,#260293,#260294),
(#260295,#260296,#260297),(#260298,#260299,#260300),(#260301,#260302,#260303),
(#260304,#260305,#260306),(#260307,#260308,#260309),(#260310,#260311,#260312),
(#260313,#260314,#260315),(#260316,#260317,#260318),(#260319,#260320,#260321),
(#260322,#260323,#260324),(#260325,#260326,#260327),(#260328,#260329,#260330),
(#260331,#260332,#260333),(#260334,#260335,#260336),(#260337,#260338,#260339),
(#260340,#260341,#260342),(#260343,#260344,#260345),(#260346,#260347,#260348),
(#260349,#260350,#260351),(#260352,#260353,#260354),(#260355,#260356,#260357)),
 .UNSPECIFIED.,.F.,.F.,.F.)
B_SPLINE_SURFACE_WITH_KNOTS((4,2,2,2,2,2,2,2,2,2,2,2,2,2,2,2,2,2,4),(3,
3),(0.,0.000833402889145506,0.00166680577829101,0.00250020866743652,0.0027085593897229,
0.00291691011200927,0.00302108547315246,0.00307317315372405,0.00309921699400985,
0.00312526083429565,0.00313828275443855,0.00315130467458145,0.00316432659472434,
0.00317083755479579,0.00317734851486724,0.00319037043501014,0.00320339235515304,
0.00322943619543884,0.00364710254014991),(-0.000788950096851769,1.),
 .UNSPECIFIED.)
GEOMETRIC_REPRESENTATION_ITEM()
RATIONAL_B_SPLINE_SURFACE(((1.00000611767343,0.996122902159017,1.),(1.00000746664395,
0.99526798717725,1.),(1.00000907164837,0.994250809774906,1.),(1.00001256256436,
0.992038429042989,1.),(1.00001447540202,0.990826161202841,1.),(1.00001824210387,
0.988439000173286,1.),(1.00002028614152,0.987143583861509,1.),(1.00002176846193,
0.986204157895867,1.),(1.00002199941439,0.986057790929556,1.),(1.00002208725417,
0.986002122151637,1.),(1.00002200721177,0.986052849314101,1.),(1.0000207948797,
0.986821169180919,1.),(1.00002023311476,0.987177189764058,1.),(1.00001842340415,
0.988324100457808,1.),(1.00001766782331,0.988802952568642,1.),(1.00001584202883,
0.98996005647675,1.),(1.00001511732551,0.990419339847295,1.),(1.00001315898457,
0.991660445556412,1.),(1.00001194207836,0.992431664304351,1.),(1.00000915175965,
0.99420003895694,1.),(1.00000803372924,0.994908594810006,1.),(1.0000055143209,
0.996505279029039,1.),(1.00000412490098,0.997385828969795,1.),(1.00000190594012,
0.998792103501718,1.),(1.00000107933685,0.999315966336424,1.),(1.00000063107598,
0.999600053297392,1.),(1.00000062814488,0.999601910890056,1.),(1.00000076435795,
0.999515585363006,1.),(1.00000089052328,0.999435627624268,1.),(1.00000127879138,
0.999189561299934,1.),(1.00000155602942,0.999013860679829,1.),(1.00000207567308,
0.998684534617987,1.),(1.00000232003768,0.998529667660177,1.),(1.00000301111441,
0.998091695265869,1.),(1.00000341869149,0.99783339180862,1.),(1.00000977857705,
0.993802791147178,1.),(1.00000744524123,0.995281551233468,1.),(1.00002241183025,
0.985796420873754,0.999999999999997)))
REPRESENTATION_ITEM('')
SURFACE()
);
#3998=(
BOUNDED_SURFACE()
B_SPLINE_SURFACE(3,2,((#260359,#260360,#260361),(#260362,#260363,#260364),
(#260365,#260366,#260367),(#260368,#260369,#260370)),.UNSPECIFIED.,.F.,
 .F.,.F.)
B_SPLINE_SURFACE_WITH_KNOTS((4,4),(3,3),(-2.8574514863482E-5,0.000314319663498302),
(0.,1.00095479615814),.UNSPECIFIED.)
GEOMETRIC_REPRESENTATION_ITEM()
RATIONAL_B_SPLINE_SURFACE(((1.,0.995946994781818,1.00000773958762),(1.,
0.996651841079349,1.00000639361855),(1.,0.997316919426149,1.00000512359005),
(1.,0.997737992799628,1.00000431951157)))
REPRESENTATION_ITEM('')
SURFACE()
);
#3999=(
BOUNDED_SURFACE()
B_SPLINE_SURFACE(3,2,((#260372,#260373,#260374),(#260375,#260376,#260377),
(#260378,#260379,#260380),(#260381,#260382,#260383)),.UNSPECIFIED.,.F.,
 .F.,.F.)
B_SPLINE_SURFACE_WITH_KNOTS((4,4),(3,3),(2.16840434497101E-19,0.000609810285548094),
(0.,1.),.UNSPECIFIED.)
GEOMETRIC_REPRESENTATION_ITEM()
RATIONAL_B_SPLINE_SURFACE(((1.,0.997630022057829,1.),(1.,0.999169954497567,
1.),(1.,1.00000047407105,1.),(1.,1.,1.)))
REPRESENTATION_ITEM('')
SURFACE()
);
#4000=(
BOUNDED_SURFACE()
B_SPLINE_SURFACE(3,2,((#260384,#260385,#260386),(#260387,#260388,#260389),
(#260390,#260391,#260392),(#260393,#260394,#260395),(#260396,#260397,#260398),
(#260399,#260400,#260401),(#260402,#260403,#260404),(#260405,#260406,#260407),
(#260408,#260409,#260410),(#260411,#260412,#260413),(#260414,#260415,#260416),
(#260417,#260418,#260419),(#260420,#260421,#260422),(#260423,#260424,#260425),
(#260426,#260427,#260428),(#260429,#260430,#260431),(#260432,#260433,#260434),
(#260435,#260436,#260437),(#260438,#260439,#260440),(#260441,#260442,#260443),
(#260444,#260445,#260446),(#260447,#260448,#260449),(#260450,#260451,#260452),
(#260453,#260454,#260455),(#260456,#260457,#260458),(#260459,#260460,#260461),
(#260462,#260463,#260464),(#260465,#260466,#260467),(#260468,#260469,#260470),
(#260471,#260472,#260473),(#260474,#260475,#260476),(#260477,#260478,#260479),
(#260480,#260481,#260482),(#260483,#260484,#260485),(#260486,#260487,#260488),
(#260489,#260490,#260491)),.UNSPECIFIED.,.F.,.F.,.F.)
B_SPLINE_SURFACE_WITH_KNOTS((4,2,2,2,2,2,2,2,2,2,2,2,2,2,2,2,2,4),(3,3),
(-0.0003334691351286,0.000833672837821643,0.00166734567564329,0.00250101851346493,
0.00270943672292034,0.00291785493237575,0.00302206403710345,0.00307416858946731,
0.00310022086564923,0.00312627314183116,0.00313929927992212,0.00315232541801309,
0.00316535155610405,0.00317186462514953,0.00317837769419501,0.00320442997037694,
0.00323048224655887,0.00364829276517932),(0.,1.00460570885116),
 .UNSPECIFIED.)
GEOMETRIC_REPRESENTATION_ITEM()
RATIONAL_B_SPLINE_SURFACE(((1.,0.99705470639553,1.00002713032965),(1.,0.996052715233661,
1.00003636008877),(1.,0.99467325918624,1.00004906683463),(1.,0.99200680279422,
1.00007362867824),(1.,0.990790384906983,1.0000848336115),(1.,0.988393785580642,
1.00010690968896),(1.,0.987091346368492,1.00011890700057),(1.,0.986150203297094,
1.00012757626252),(1.,0.986003642672512,1.00012892629365),(1.,0.985949237827209,
1.00012942743941),(1.,0.986000799357252,1.00012895248462),(1.,0.986777873089627,
1.00012179453388),(1.,0.987137483619315,1.00011848201109),(1.,0.988298093339291,
1.00010779115017),(1.,0.98878264223078,1.00010332776793),(1.,0.989957253593888,
1.00009250793203),(1.,0.990423861712164,1.00008820980974),(1.,0.991688273857629,
1.00007656278132),(1.,0.992476038639695,1.00006930635087),(1.,0.994284431414586,
1.00005264848965),(1.,0.995010326911815,1.00004596196301),(1.,0.996626426245307,
1.000031075397),(1.,0.99750133799964,1.00002301621938),(1.,0.998874113904101,
1.00001037100711),(1.,0.999376314879296,1.00000574502416),(1.,0.999608475942149,
1.00000360649164),(1.,0.999592989064516,1.00000374914774),(1.,0.999491456297114,
1.00000468440847),(1.,0.99940936032594,1.00000544062875),(1.,0.998997449457861,
1.00000923491181),(1.,0.99865128617018,1.00001242356645),(1.,0.998071024137341,
1.00001776860241),(1.,0.997813344969334,1.00002014219286),(1.,0.993788013596569,
1.00005722120152),(1.,0.995307700678994,1.00004322272903),(1.,0.985483842068487,
1.00013371439414)))
REPRESENTATION_ITEM('')
SURFACE()
);
#4001=(
BOUNDED_SURFACE()
B_SPLINE_SURFACE(3,2,((#260493,#260494,#260495),(#260496,#260497,#260498),
(#260499,#260500,#260501),(#260502,#260503,#260504)),.UNSPECIFIED.,.F.,
 .F.,.F.)
B_SPLINE_SURFACE_WITH_KNOTS((4,4),(3,3),(-2.85745148645395E-5,0.000314319663509989),
(0.,1.00095479660429),.UNSPECIFIED.)
GEOMETRIC_REPRESENTATION_ITEM()
RATIONAL_B_SPLINE_SURFACE(((1.,0.997737992798662,1.00000431951359),(1.,
0.997316919425008,1.00000512359244),(1.,0.996651841077884,1.00000639362154),
(1.,0.995946994780003,1.00000773959124)))
REPRESENTATION_ITEM('')
SURFACE()
);
#4002=(
BOUNDED_SURFACE()
B_SPLINE_SURFACE(3,2,((#260506,#260507,#260508),(#260509,#260510,#260511),
(#260512,#260513,#260514),(#260515,#260516,#260517)),.UNSPECIFIED.,.F.,
 .F.,.F.)
B_SPLINE_SURFACE_WITH_KNOTS((4,4),(3,3),(-4.77048955893622E-18,0.000609810285535309),
(0.,1.),.UNSPECIFIED.)
GEOMETRIC_REPRESENTATION_ITEM()
RATIONAL_B_SPLINE_SURFACE(((1.,0.997630022057914,1.),(1.,0.999169954497594,
1.),(1.,1.00000047407104,1.),(1.,1.,1.)))
REPRESENTATION_ITEM('')
SURFACE()
);
#4003=(
BOUNDED_SURFACE()
B_SPLINE_SURFACE(3,2,((#260518,#260519,#260520),(#260521,#260522,#260523),
(#260524,#260525,#260526),(#260527,#260528,#260529)),.UNSPECIFIED.,.F.,
 .F.,.F.)
B_SPLINE_SURFACE_WITH_KNOTS((4,4),(3,3),(0.,0.000609810285548325),(0.,1.),
 .UNSPECIFIED.)
GEOMETRIC_REPRESENTATION_ITEM()
RATIONAL_B_SPLINE_SURFACE(((1.,0.997630022057829,1.),(1.,0.999169954497567,
1.),(1.,1.00000047407105,1.),(1.,1.,1.)))
REPRESENTATION_ITEM('')
SURFACE()
);
#4004=(
BOUNDED_SURFACE()
B_SPLINE_SURFACE(3,2,((#260531,#260532,#260533),(#260534,#260535,#260536),
(#260537,#260538,#260539),(#260540,#260541,#260542)),.UNSPECIFIED.,.F.,
 .F.,.F.)
B_SPLINE_SURFACE_WITH_KNOTS((4,4),(3,3),(-2.85745148634637E-5,0.000314319663498177),
(0.,1.00095479624155),.UNSPECIFIED.)
GEOMETRIC_REPRESENTATION_ITEM()
RATIONAL_B_SPLINE_SURFACE(((1.,0.995946994781479,1.0000077395883),(1.,0.996651841079075,
1.00000639361911),(1.,0.997316919425921,1.0000051235905),(1.,0.997737992799442,
1.00000431951195)))
REPRESENTATION_ITEM('')
SURFACE()
);
#4005=(
BOUNDED_SURFACE()
B_SPLINE_SURFACE(3,2,((#260544,#260545,#260546),(#260547,#260548,#260549),
(#260550,#260551,#260552),(#260553,#260554,#260555),(#260556,#260557,#260558),
(#260559,#260560,#260561),(#260562,#260563,#260564),(#260565,#260566,#260567),
(#260568,#260569,#260570),(#260571,#260572,#260573),(#260574,#260575,#260576),
(#260577,#260578,#260579),(#260580,#260581,#260582),(#260583,#260584,#260585),
(#260586,#260587,#260588),(#260589,#260590,#260591),(#260592,#260593,#260594),
(#260595,#260596,#260597),(#260598,#260599,#260600),(#260601,#260602,#260603),
(#260604,#260605,#260606),(#260607,#260608,#260609),(#260610,#260611,#260612),
(#260613,#260614,#260615),(#260616,#260617,#260618),(#260619,#260620,#260621),
(#260622,#260623,#260624),(#260625,#260626,#260627),(#260628,#260629,#260630),
(#260631,#260632,#260633),(#260634,#260635,#260636),(#260637,#260638,#260639),
(#260640,#260641,#260642),(#260643,#260644,#260645),(#260646,#260647,#260648),
(#260649,#260650,#260651),(#260652,#260653,#260654),(#260655,#260656,#260657)),
 .UNSPECIFIED.,.F.,.F.,.F.)
B_SPLINE_SURFACE_WITH_KNOTS((4,2,2,2,2,2,2,2,2,2,2,2,2,2,2,2,2,2,4),(3,
3),(-0.000333361155718326,0.000833402889296124,0.00166680577859225,0.00250020866788837,
0.0027085593902124,0.00291691011253643,0.00302108547369845,0.00307317315427946,
0.00309921699456996,0.00312526083486046,0.00313828275500572,0.00315130467515097,
0.00316432659529622,0.00317083755536884,0.00317734851544147,0.00319037043558672,
0.00320339235573198,0.00322943619602248,0.00364710254080976),(-0.00578770663227079,
1.),.UNSPECIFIED.)
GEOMETRIC_REPRESENTATION_ITEM()
RATIONAL_B_SPLINE_SURFACE(((1.00003412926621,0.997051572550087,1.),(1.00004574782918,
0.996047844846918,1.),(1.00006173422714,0.994666779861184,1.),(1.00009261878868,
0.991998662461224,1.),(1.00010672137968,0.990780339566208,1.),(1.00013449177376,
0.988381255106199,1.),(1.00014956165008,0.98707936842808,1.),(1.0001604902087,
0.986135250203682,1.),(1.00016219292933,0.985988152161554,1.),(1.00016284053703,
0.98593220532956,1.),(1.00016225041626,0.98598318586536,1.),(1.00015331237424,
0.986755343352947,1.),(1.00014917070478,0.987113142194872,1.),(1.00013582842843,
0.988265781504093,1.),(1.0001302578315,0.988747025396118,1.),(1.0001167969751,
0.989909908835822,1.),(1.00011145402582,0.990371486246688,1.),(1.00009701595708,
0.991618791065173,1.),(1.00008804419163,0.992393861919777,1.),(1.00006747228168,
0.994171069305731,1.),(1.0000592294881,0.994883164277001,1.),(1.00004065489268,
0.996487823652573,1.),(1.00003041125244,0.997372771775525,1.),(1.00001405173728,
0.998786070358076,1.),(1.00000795752053,0.999312549768481,1.),(1.00000465267198,
0.999598055648167,1.),(1.00000463106235,0.999599922504002,1.),(1.00000563530726,
0.999513165782186,1.),(1.00000656547408,0.999432808667257,1.),(1.00000942802033,
0.99918551328416,1.),(1.0000114719861,0.999008935072858,1.),(1.00001530311202,
0.998677964089285,1.),(1.00001710471499,0.998522323600551,1.),(1.00002219974871,
0.998082163617035,1.),(1.00002520465231,0.997822569982669,1.),(1.00007209355794,
0.993771837229935,1.),(1.0000548908016,0.995257983422156,1.),(1.00016523350623,
0.985725476710866,1.)))
REPRESENTATION_ITEM('')
SURFACE()
);
#4006=(
BOUNDED_SURFACE()
B_SPLINE_SURFACE(3,2,((#260658,#260659,#260660),(#260661,#260662,#260663),
(#260664,#260665,#260666),(#260667,#260668,#260669),(#260670,#260671,#260672),
(#260673,#260674,#260675),(#260676,#260677,#260678),(#260679,#260680,#260681),
(#260682,#260683,#260684),(#260685,#260686,#260687),(#260688,#260689,#260690),
(#260691,#260692,#260693),(#260694,#260695,#260696),(#260697,#260698,#260699),
(#260700,#260701,#260702),(#260703,#260704,#260705),(#260706,#260707,#260708),
(#260709,#260710,#260711),(#260712,#260713,#260714),(#260715,#260716,#260717),
(#260718,#260719,#260720),(#260721,#260722,#260723),(#260724,#260725,#260726),
(#260727,#260728,#260729),(#260730,#260731,#260732),(#260733,#260734,#260735),
(#260736,#260737,#260738),(#260739,#260740,#260741),(#260742,#260743,#260744),
(#260745,#260746,#260747),(#260748,#260749,#260750),(#260751,#260752,#260753),
(#260754,#260755,#260756),(#260757,#260758,#260759),(#260760,#260761,#260762),
(#260763,#260764,#260765)),.UNSPECIFIED.,.F.,.F.,.F.)
B_SPLINE_SURFACE_WITH_KNOTS((4,2,2,2,2,2,2,2,2,2,2,2,2,2,2,2,2,4),(3,3),
(-0.000333469135129058,0.000833672837822158,0.00166734567564438,0.00250101851346661,
0.00270943672292216,0.00291785493237772,0.0030220640371055,0.00307416858946939,
0.00310022086565133,0.00312627314183328,0.00313929927992425,0.00315232541801522,
0.00316535155610619,0.00317186462515168,0.00317837769419717,0.00320442997037911,
0.00323048224656105,0.00364829276518163),(0.,1.0046057089022),
 .UNSPECIFIED.)
GEOMETRIC_REPRESENTATION_ITEM()
RATIONAL_B_SPLINE_SURFACE(((1.,0.997054706395145,1.00002713032995),(1.,
0.996052715233707,1.00003636008918),(1.,0.994673259185837,1.00004906683517),
(1.,0.992006802793903,1.00007362867906),(1.,0.990790384906695,1.00008483361244),
(1.,0.988393785579858,1.00010690969015),(1.,0.987091346368048,1.0001189070019),
(1.,0.986150203296328,1.00012757626394),(1.,0.986003642671745,1.00012892629509),
(1.,0.985949237826535,1.00012942744085),(1.,0.986000799356981,1.00012895248605),
(1.,0.98677787308873,1.00012179453524),(1.,0.987137483618698,1.0001184820124),
(1.,0.988298093338714,1.00010779115137),(1.,0.988782642230273,1.00010332776908),
(1.,0.989957253593439,1.00009250793305),(1.,0.990423861711556,1.00008820981073),
(1.,0.99168827385752,1.00007656278217),(1.,0.992476038639505,1.00006930635164),
(1.,0.994284431414554,1.00005264849023),(1.,0.995010326911985,1.00004596196352),
(1.,0.996626426245523,1.00003107539735),(1.,0.997501337999955,1.00002301621963),
(1.,0.998874113904281,1.00001037100723),(1.,0.999376314879437,1.00000574502422),
(1.,0.99960847594215,1.00000360649168),(1.,0.999592989064471,1.00000374914778),
(1.,0.999491456297019,1.00000468440852),(1.,0.999409360325836,1.00000544062881),
(1.,0.998997449457727,1.00000923491191),(1.,0.998651286170026,1.00001242356659),
(1.,0.998071024137219,1.00001776860261),(1.,0.997813344969144,1.00002014219308),
(1.,0.993788013596835,1.00005722120215),(1.,0.995307700673881,1.00004322272956),
(1.,0.985483842096778,1.00013371439536)))
REPRESENTATION_ITEM('')
SURFACE()
);
#4007=(
BOUNDED_SURFACE()
B_SPLINE_SURFACE(3,2,((#260767,#260768,#260769),(#260770,#260771,#260772),
(#260773,#260774,#260775),(#260776,#260777,#260778)),.UNSPECIFIED.,.F.,
 .F.,.F.)
B_SPLINE_SURFACE_WITH_KNOTS((4,4),(3,3),(-2.85745148645424E-5,0.000314319663509999),
(0.,1.00095479657711),.UNSPECIFIED.)
GEOMETRIC_REPRESENTATION_ITEM()
RATIONAL_B_SPLINE_SURFACE(((1.,0.997737992798722,1.00000431951347),(1.,
0.997316919425082,1.0000051235923),(1.,0.996651841077974,1.00000639362136),
(1.,0.995946994780112,1.00000773959102)))
REPRESENTATION_ITEM('')
SURFACE()
);
#4008=(
BOUNDED_SURFACE()
B_SPLINE_SURFACE(3,2,((#260780,#260781,#260782),(#260783,#260784,#260785),
(#260786,#260787,#260788),(#260789,#260790,#260791)),.UNSPECIFIED.,.F.,
 .F.,.F.)
B_SPLINE_SURFACE_WITH_KNOTS((4,4),(3,3),(-1.23599047663348E-17,0.000609810285535295),
(0.,1.),.UNSPECIFIED.)
GEOMETRIC_REPRESENTATION_ITEM()
RATIONAL_B_SPLINE_SURFACE(((1.,0.997630022057914,1.),(1.,0.999169954497594,
1.),(1.,1.00000047407104,1.),(1.,1.,1.)))
REPRESENTATION_ITEM('')
SURFACE()
);
#4009=(
BOUNDED_SURFACE()
B_SPLINE_SURFACE(3,2,((#260792,#260793,#260794),(#260795,#260796,#260797),
(#260798,#260799,#260800),(#260801,#260802,#260803),(#260804,#260805,#260806),
(#260807,#260808,#260809),(#260810,#260811,#260812),(#260813,#260814,#260815),
(#260816,#260817,#260818),(#260819,#260820,#260821),(#260822,#260823,#260824),
(#260825,#260826,#260827),(#260828,#260829,#260830),(#260831,#260832,#260833)),
 .UNSPECIFIED.,.F.,.F.,.F.)
B_SPLINE_SURFACE_WITH_KNOTS((4,2,2,2,2,2,4),(3,3),(-1.73472347597681E-18,
0.00136118311773746,0.00204177467660619,0.00272236623547492,0.00340295779434365,
0.00408354935321238,0.00544473247094984),(0.,1.),.UNSPECIFIED.)
GEOMETRIC_REPRESENTATION_ITEM()
RATIONAL_B_SPLINE_SURFACE(((1.,0.748955720789002,1.),(1.,0.74826415820711,
1.),(1.,0.746711680960384,1.),(1.,0.74314634401593,1.),(1.,0.741776455602707,
1.),(1.,0.738679679513325,1.),(1.,0.736933927001107,1.),(1.,0.733153776741552,
1.),(1.,0.731132725915841,1.),(1.,0.726827414419606,1.),(1.,0.724518460380596,
1.),(1.,0.717397817977927,1.),(1.,0.71235845960716,1.),(1.,0.707106781186548,
1.)))
REPRESENTATION_ITEM('')
SURFACE()
);
#4010=(
BOUNDED_SURFACE()
B_SPLINE_SURFACE(3,2,((#260850,#260851,#260852),(#260853,#260854,#260855),
(#260856,#260857,#260858),(#260859,#260860,#260861),(#260862,#260863,#260864),
(#260865,#260866,#260867),(#260868,#260869,#260870),(#260871,#260872,#260873),
(#260874,#260875,#260876),(#260877,#260878,#260879),(#260880,#260881,#260882),
(#260883,#260884,#260885),(#260886,#260887,#260888),(#260889,#260890,#260891)),
 .UNSPECIFIED.,.F.,.F.,.F.)
B_SPLINE_SURFACE_WITH_KNOTS((4,2,2,2,2,2,4),(3,3),(0.,0.00136134654673614,
0.00204201982010421,0.00272269309347228,0.00340336636684036,0.00408403964020843,
0.00544538618694457),(0.,1.),.UNSPECIFIED.)
GEOMETRIC_REPRESENTATION_ITEM()
RATIONAL_B_SPLINE_SURFACE(((1.,0.707106781186547,1.),(1.,0.712303169346064,
1.),(1.,0.717355648681421,1.),(1.,0.724523494465793,1.),(1.,0.726790378288212,
1.),(1.,0.731092716345856,1.),(1.,0.733143854998034,1.),(1.,0.736930899570443,
1.),(1.,0.738649526515843,1.),(1.,0.741751075820653,1.),(1.,0.743145323860387,
1.),(1.,0.746698948407202,1.),(1.,0.748249049712917,1.),(1.,0.748955720789002,
1.)))
REPRESENTATION_ITEM('')
SURFACE()
);
#4011=(
BOUNDED_SURFACE()
B_SPLINE_SURFACE(3,2,((#260929,#260930,#260931),(#260932,#260933,#260934),
(#260935,#260936,#260937),(#260938,#260939,#260940),(#260941,#260942,#260943),
(#260944,#260945,#260946),(#260947,#260948,#260949),(#260950,#260951,#260952),
(#260953,#260954,#260955),(#260956,#260957,#260958),(#260959,#260960,#260961),
(#260962,#260963,#260964),(#260965,#260966,#260967),(#260968,#260969,#260970),
(#260971,#260972,#260973),(#260974,#260975,#260976),(#260977,#260978,#260979),
(#260980,#260981,#260982),(#260983,#260984,#260985),(#260986,#260987,#260988),
(#260989,#260990,#260991),(#260992,#260993,#260994)),.UNSPECIFIED.,.F.,
 .F.,.F.)
B_SPLINE_SURFACE_WITH_KNOTS((4,2,2,2,2,2,2,2,2,2,4),(3,3),(-5.08913310798276E-12,
0.000351116935758021,0.000526675406181597,0.000702233876605174,0.00105335081745233,
0.00140446775829948,0.00175558469914664,0.00193114316957021,0.00210670163999379,
0.00245781858084094,0.0028089355216881),(0.,1.00212154420491),
 .UNSPECIFIED.)
GEOMETRIC_REPRESENTATION_ITEM()
RATIONAL_B_SPLINE_SURFACE(((1.,0.981880755432236,1.00007688155662),(1.,
0.981882092332791,1.00007687588403),(1.,0.981880407724475,1.00007688303197),
(1.,0.981878412726316,1.00007689149693),(1.,0.98187708093562,1.00007689714783),
(1.,0.981874393254514,1.0000769085519),(1.,0.981872947013521,1.00007691468843),
(1.,0.981868716388952,1.00007693263935),(1.,0.981866966616579,1.00007694006378),
(1.,0.98186071974881,1.0000769665698),(1.,0.981861064282868,1.00007696510791),
(1.,0.981858769625711,1.00007697484434),(1.,0.981858540956784,1.0000769758146),
(1.,0.981862047984854,1.00007696093397),(1.,0.981862448285702,1.00007695923546),
(1.,0.981864314970464,1.00007695131495),(1.,0.981865383122516,1.00007694678269),
(1.,0.981869817883337,1.00007692796561),(1.,0.98187226500369,1.00007691758226),
(1.,0.98187820748076,1.0000768923678),(1.,0.981879815049627,1.00007688554675),
(1.,0.98188078670202,1.00007688142394)))
REPRESENTATION_ITEM('')
SURFACE()
);
#4012=(
BOUNDED_SURFACE()
B_SPLINE_SURFACE(3,2,((#261416,#261417,#261418),(#261419,#261420,#261421),
(#261422,#261423,#261424),(#261425,#261426,#261427),(#261428,#261429,#261430),
(#261431,#261432,#261433),(#261434,#261435,#261436),(#261437,#261438,#261439),
(#261440,#261441,#261442),(#261443,#261444,#261445),(#261446,#261447,#261448),
(#261449,#261450,#261451),(#261452,#261453,#261454),(#261455,#261456,#261457),
(#261458,#261459,#261460),(#261461,#261462,#261463),(#261464,#261465,#261466),
(#261467,#261468,#261469),(#261470,#261471,#261472),(#261473,#261474,#261475)),
 .UNSPECIFIED.,.F.,.F.,.F.)
B_SPLINE_SURFACE_WITH_KNOTS((4,2,2,2,2,2,2,2,2,4),(3,3),(0.0026254766208179,
0.00351116940646127,0.0038622863488768,0.00403784482008456,0.00421340329129233,
0.00456452023370786,0.00491563717612339,0.00509119564733115,0.00526675411853892,
0.00589876461495421),(-0.00125569467631438,1.00180257992218),
 .UNSPECIFIED.)
GEOMETRIC_REPRESENTATION_ITEM()
RATIONAL_B_SPLINE_SURFACE(((1.00004547719783,0.981858935225732,1.00006531926962),
(1.00004544657458,0.981871150982356,1.00006527528519),(1.00004547473781,
0.981859916538268,1.00006531573627),(1.00004549367077,0.981852364094264,
1.00006534292983),(1.00004550322764,0.981848551814997,1.00006535665644),
(1.00004551019068,0.981845774225094,1.00006536665751),(1.00004551240719,
0.981844890048581,1.00006536984111),(1.00004551592272,0.981843487685747,
1.0000653748905),(1.00004551706357,0.981843032597144,1.0000653765291),(1.00004551844175,
0.981842482833192,1.0000653785086),(1.00004551600531,0.981843454742648,
1.00006537500911),(1.00004551339811,0.981844494765837,1.00006537126438),
(1.00004550803579,0.981846633818991,1.00006536356243),(1.00004549615002,
0.981851375109875,1.0000653464908),(1.00004549312932,0.981852580080655,
1.00006534215214),(1.00004548600682,0.981855421277189,1.00006533192205),
(1.0000454836188,0.981856373870441,1.00006532849211),(1.00004546289328,
0.981864641377868,1.00006529872387),(1.00004547077922,0.981861495638696,
1.00006531005052),(1.00004544888931,0.981870227625078,1.00006527860986)))
REPRESENTATION_ITEM('')
SURFACE()
);
#4013=(
BOUNDED_SURFACE()
B_SPLINE_SURFACE(1,2,((#262489,#262490,#262491,#262492,#262493,#262494,
#262495,#262496,#262497,#262498,#262499,#262500,#262501,#262502,#262503,
#262504,#262505,#262506,#262507,#262508,#262509,#262510,#262511,#262512,
#262513,#262514,#262515,#262516,#262517,#262518,#262519,#262520,#262521,
#262522,#262523,#262524,#262525,#262526,#262527,#262528,#262529,#262530,
#262531,#262532,#262533,#262534,#262535,#262536,#262537,#262538,#262539,
#262540,#262541,#262542,#262543,#262544,#262545,#262546,#262547,#262548,
#262549,#262550,#262551,#262552,#262553,#262554,#262555,#262556,#262557,
#262558,#262559,#262560,#262561,#262562,#262563,#262564,#262565,#262566,
#262567,#262568,#262569,#262570,#262571,#262572,#262573,#262574,#262575,
#262576,#262577,#262578,#262579,#262580,#262581,#262582,#262583,#262584,
#262585,#262586,#262587,#262588,#262589,#262590,#262591,#262592,#262593,
#262594,#262595,#262596,#262597,#262598,#262599,#262600,#262601,#262602,
#262603,#262604,#262605,#262606,#262607,#262608,#262609,#262610,#262611,
#262612,#262613,#262614,#262615,#262616,#262617,#262618,#262619,#262620,
#262621,#262622,#262623,#262624,#262625,#262626,#262627,#262628,#262629,
#262630,#262631,#262632,#262633,#262634,#262635,#262636,#262637,#262638,
#262639,#262640,#262641,#262642,#262643,#262644,#262645,#262646,#262647,
#262648,#262649),(#262650,#262651,#262652,#262653,#262654,#262655,#262656,
#262657,#262658,#262659,#262660,#262661,#262662,#262663,#262664,#262665,
#262666,#262667,#262668,#262669,#262670,#262671,#262672,#262673,#262674,
#262675,#262676,#262677,#262678,#262679,#262680,#262681,#262682,#262683,
#262684,#262685,#262686,#262687,#262688,#262689,#262690,#262691,#262692,
#262693,#262694,#262695,#262696,#262697,#262698,#262699,#262700,#262701,
#262702,#262703,#262704,#262705,#262706,#262707,#262708,#262709,#262710,
#262711,#262712,#262713,#262714,#262715,#262716,#262717,#262718,#262719,
#262720,#262721,#262722,#262723,#262724,#262725,#262726,#262727,#262728,
#262729,#262730,#262731,#262732,#262733,#262734,#262735,#262736,#262737,
#262738,#262739,#262740,#262741,#262742,#262743,#262744,#262745,#262746,
#262747,#262748,#262749,#262750,#262751,#262752,#262753,#262754,#262755,
#262756,#262757,#262758,#262759,#262760,#262761,#262762,#262763,#262764,
#262765,#262766,#262767,#262768,#262769,#262770,#262771,#262772,#262773,
#262774,#262775,#262776,#262777,#262778,#262779,#262780,#262781,#262782,
#262783,#262784,#262785,#262786,#262787,#262788,#262789,#262790,#262791,
#262792,#262793,#262794,#262795,#262796,#262797,#262798,#262799,#262800,
#262801,#262802,#262803,#262804,#262805,#262806,#262807,#262808,#262809,
#262810)),.UNSPECIFIED.,.F.,.F.,.F.)
B_SPLINE_SURFACE_WITH_KNOTS((2,2),(3,2,2,2,2,2,2,2,2,2,2,2,2,2,2,2,2,2,
2,2,2,2,2,2,2,2,2,2,2,2,2,2,2,2,2,2,2,2,2,2,2,2,2,2,2,2,2,2,2,2,2,2,2,2,
2,2,2,2,2,2,2,2,2,2,2,2,2,2,2,2,2,2,2,2,2,2,2,2,2,2,3),(0.,1.),(0.,0.0125,
0.025,0.0375,0.05,0.0625,0.075,0.0875,0.1,0.1125,0.125,0.1375,0.15,0.1625,
0.175,0.1875,0.2,0.2125,0.225,0.2375,0.25,0.2625,0.275,0.2875,0.3,0.3125,
0.325,0.3375,0.35,0.3625,0.375,0.3875,0.4,0.4125,0.425,0.4375,0.45,0.4625,
0.475,0.4875,0.5,0.5125,0.525,0.5375,0.55,0.5625,0.575,0.5875,0.6,0.6125,
0.625,0.6375,0.65,0.6625,0.675,0.6875,0.7,0.7125,0.725,0.7375,0.75,0.7625,
0.775,0.7875,0.8,0.8125,0.825,0.8375,0.85,0.8625,0.875,0.8875,0.9,0.9125,
0.925,0.9375,0.95,0.9625,0.975,0.9875,1.),.UNSPECIFIED.)
GEOMETRIC_REPRESENTATION_ITEM()
RATIONAL_B_SPLINE_SURFACE(((1.,0.923879532511287,1.,0.923879532511287,1.,
0.923879532511287,1.,0.923879532511287,1.,0.923879532511287,1.,0.923879532511287,
1.,0.923879532511287,1.,0.923879532511287,1.,0.923879532511287,1.,0.923879532511287,
1.,0.923879532511287,1.,0.923879532511287,1.,0.923879532511287,1.,0.923879532511287,
1.,0.923879532511287,1.,0.923879532511287,1.,0.923879532511287,1.,0.923879532511287,
1.,0.923879532511287,1.,0.923879532511287,1.,0.923879532511287,1.,0.923879532511287,
1.,0.923879532511287,1.,0.923879532511287,1.,0.923879532511287,1.,0.923879532511287,
1.,0.923879532511287,1.,0.923879532511287,1.,0.923879532511287,1.,0.923879532511287,
1.,0.923879532511287,1.,0.923879532511287,1.,0.923879532511287,1.,0.923879532511287,
1.,0.923879532511287,1.,0.923879532511287,1.,0.923879532511287,1.,0.923879532511287,
1.,0.923879532511287,1.,0.923879532511287,1.,0.923879532511287,1.,0.923879532511287,
1.,0.923879532511287,1.,0.923879532511287,1.,0.923879532511287,1.,0.923879532511287,
1.,0.923879532511287,1.,0.923879532511287,1.,0.923879532511287,1.,0.923879532511287,
1.,0.923879532511287,1.,0.923879532511287,1.,0.923879532511287,1.,0.923879532511287,
1.,0.923879532511287,1.,0.923879532511287,1.,0.923879532511287,1.,0.923879532511287,
1.,0.923879532511287,1.,0.923879532511287,1.,0.923879532511287,1.,0.923879532511287,
1.,0.923879532511287,1.,0.923879532511287,1.,0.923879532511287,1.,0.923879532511287,
1.,0.923879532511287,1.,0.923879532511287,1.,0.923879532511287,1.,0.923879532511287,
1.,0.923879532511287,1.,0.923879532511287,1.,0.923879532511287,1.,0.923879532511287,
1.,0.923879532511287,1.,0.923879532511287,1.,0.923879532511287,1.,0.923879532511287,
1.,0.923879532511287,1.,0.923879532511287,1.),(1.,0.923879532511287,1.,
0.923879532511287,1.,0.923879532511287,1.,0.923879532511287,1.,0.923879532511287,
1.,0.923879532511287,1.,0.923879532511287,1.,0.923879532511287,1.,0.923879532511287,
1.,0.923879532511287,1.,0.923879532511287,1.,0.923879532511287,1.,0.923879532511287,
1.,0.923879532511287,1.,0.923879532511287,1.,0.923879532511287,1.,0.923879532511287,
1.,0.923879532511287,1.,0.923879532511287,1.,0.923879532511287,1.,0.923879532511287,
1.,0.923879532511287,1.,0.923879532511287,1.,0.923879532511287,1.,0.923879532511287,
1.,0.923879532511287,1.,0.923879532511287,1.,0.923879532511287,1.,0.923879532511287,
1.,0.923879532511287,1.,0.923879532511287,1.,0.923879532511287,1.,0.923879532511287,
1.,0.923879532511287,1.,0.923879532511287,1.,0.923879532511287,1.,0.923879532511287,
1.,0.923879532511287,1.,0.923879532511287,1.,0.923879532511287,1.,0.923879532511287,
1.,0.923879532511287,1.,0.923879532511287,1.,0.923879532511287,1.,0.923879532511287,
1.,0.923879532511287,1.,0.923879532511287,1.,0.923879532511287,1.,0.923879532511287,
1.,0.923879532511287,1.,0.923879532511287,1.,0.923879532511287,1.,0.923879532511287,
1.,0.923879532511287,1.,0.923879532511287,1.,0.923879532511287,1.,0.923879532511287,
1.,0.923879532511287,1.,0.923879532511287,1.,0.923879532511287,1.,0.923879532511287,
1.,0.923879532511287,1.,0.923879532511287,1.,0.923879532511287,1.,0.923879532511287,
1.,0.923879532511287,1.,0.923879532511287,1.,0.923879532511287,1.,0.923879532511287,
1.,0.923879532511287,1.,0.923879532511287,1.,0.923879532511287,1.,0.923879532511287,
1.,0.923879532511287,1.,0.923879532511287,1.,0.923879532511287,1.,0.923879532511287,
1.,0.923879532511287,1.,0.923879532511287,1.,0.923879532511287,1.)))
REPRESENTATION_ITEM('')
SURFACE()
);
#4014=(
BOUNDED_SURFACE()
B_SPLINE_SURFACE(1,2,((#262846,#262847,#262848,#262849,#262850,#262851,
#262852,#262853,#262854,#262855,#262856,#262857,#262858,#262859,#262860,
#262861,#262862,#262863,#262864,#262865,#262866,#262867,#262868,#262869,
#262870,#262871,#262872,#262873,#262874,#262875,#262876,#262877,#262878,
#262879,#262880,#262881,#262882,#262883,#262884,#262885,#262886,#262887,
#262888,#262889,#262890,#262891,#262892,#262893,#262894,#262895,#262896,
#262897,#262898,#262899,#262900,#262901,#262902,#262903,#262904,#262905,
#262906,#262907,#262908,#262909,#262910,#262911,#262912,#262913,#262914,
#262915,#262916,#262917,#262918,#262919,#262920,#262921,#262922,#262923,
#262924,#262925,#262926,#262927,#262928,#262929,#262930,#262931,#262932,
#262933,#262934,#262935,#262936,#262937,#262938,#262939,#262940,#262941,
#262942,#262943,#262944,#262945,#262946,#262947,#262948,#262949,#262950,
#262951,#262952,#262953,#262954,#262955,#262956,#262957,#262958,#262959,
#262960,#262961,#262962,#262963,#262964,#262965,#262966,#262967,#262968,
#262969,#262970,#262971,#262972,#262973,#262974,#262975,#262976,#262977,
#262978,#262979,#262980,#262981,#262982,#262983,#262984,#262985,#262986,
#262987,#262988,#262989,#262990,#262991,#262992,#262993,#262994,#262995,
#262996,#262997,#262998,#262999,#263000,#263001,#263002,#263003,#263004,
#263005,#263006),(#263007,#263008,#263009,#263010,#263011,#263012,#263013,
#263014,#263015,#263016,#263017,#263018,#263019,#263020,#263021,#263022,
#263023,#263024,#263025,#263026,#263027,#263028,#263029,#263030,#263031,
#263032,#263033,#263034,#263035,#263036,#263037,#263038,#263039,#263040,
#263041,#263042,#263043,#263044,#263045,#263046,#263047,#263048,#263049,
#263050,#263051,#263052,#263053,#263054,#263055,#263056,#263057,#263058,
#263059,#263060,#263061,#263062,#263063,#263064,#263065,#263066,#263067,
#263068,#263069,#263070,#263071,#263072,#263073,#263074,#263075,#263076,
#263077,#263078,#263079,#263080,#263081,#263082,#263083,#263084,#263085,
#263086,#263087,#263088,#263089,#263090,#263091,#263092,#263093,#263094,
#263095,#263096,#263097,#263098,#263099,#263100,#263101,#263102,#263103,
#263104,#263105,#263106,#263107,#263108,#263109,#263110,#263111,#263112,
#263113,#263114,#263115,#263116,#263117,#263118,#263119,#263120,#263121,
#263122,#263123,#263124,#263125,#263126,#263127,#263128,#263129,#263130,
#263131,#263132,#263133,#263134,#263135,#263136,#263137,#263138,#263139,
#263140,#263141,#263142,#263143,#263144,#263145,#263146,#263147,#263148,
#263149,#263150,#263151,#263152,#263153,#263154,#263155,#263156,#263157,
#263158,#263159,#263160,#263161,#263162,#263163,#263164,#263165,#263166,
#263167)),.UNSPECIFIED.,.F.,.F.,.F.)
B_SPLINE_SURFACE_WITH_KNOTS((2,2),(3,2,2,2,2,2,2,2,2,2,2,2,2,2,2,2,2,2,
2,2,2,2,2,2,2,2,2,2,2,2,2,2,2,2,2,2,2,2,2,2,2,2,2,2,2,2,2,2,2,2,2,2,2,2,
2,2,2,2,2,2,2,2,2,2,2,2,2,2,2,2,2,2,2,2,2,2,2,2,2,2,3),(0.,1.),(0.,0.0125,
0.025,0.0375,0.05,0.0625,0.075,0.0875,0.1,0.1125,0.125,0.1375,0.15,0.1625,
0.175,0.1875,0.2,0.2125,0.225,0.2375,0.25,0.2625,0.275,0.2875,0.3,0.3125,
0.325,0.3375,0.35,0.3625,0.375,0.3875,0.4,0.4125,0.425,0.4375,0.45,0.4625,
0.475,0.4875,0.5,0.5125,0.525,0.5375,0.55,0.5625,0.575,0.5875,0.6,0.6125,
0.625,0.6375,0.65,0.6625,0.675,0.6875,0.7,0.7125,0.725,0.7375,0.75,0.7625,
0.775,0.7875,0.8,0.8125,0.825,0.8375,0.85,0.8625,0.875,0.8875,0.9,0.9125,
0.925,0.9375,0.95,0.9625,0.975,0.9875,1.),.UNSPECIFIED.)
GEOMETRIC_REPRESENTATION_ITEM()
RATIONAL_B_SPLINE_SURFACE(((1.,0.923879532511287,1.,0.923879532511287,1.,
0.923879532511287,1.,0.923879532511287,1.,0.923879532511287,1.,0.923879532511287,
1.,0.923879532511287,1.,0.923879532511287,1.,0.923879532511287,1.,0.923879532511287,
1.,0.923879532511287,1.,0.923879532511287,1.,0.923879532511287,1.,0.923879532511287,
1.,0.923879532511287,1.,0.923879532511287,1.,0.923879532511287,1.,0.923879532511287,
1.,0.923879532511287,1.,0.923879532511287,1.,0.923879532511287,1.,0.923879532511287,
1.,0.923879532511287,1.,0.923879532511287,1.,0.923879532511287,1.,0.923879532511287,
1.,0.923879532511287,1.,0.923879532511287,1.,0.923879532511287,1.,0.923879532511287,
1.,0.923879532511287,1.,0.923879532511287,1.,0.923879532511287,1.,0.923879532511287,
1.,0.923879532511287,1.,0.923879532511287,1.,0.923879532511287,1.,0.923879532511287,
1.,0.923879532511287,1.,0.923879532511287,1.,0.923879532511287,1.,0.923879532511287,
1.,0.923879532511287,1.,0.923879532511287,1.,0.923879532511287,1.,0.923879532511287,
1.,0.923879532511287,1.,0.923879532511287,1.,0.923879532511287,1.,0.923879532511287,
1.,0.923879532511287,1.,0.923879532511287,1.,0.923879532511287,1.,0.923879532511287,
1.,0.923879532511287,1.,0.923879532511287,1.,0.923879532511287,1.,0.923879532511287,
1.,0.923879532511287,1.,0.923879532511287,1.,0.923879532511287,1.,0.923879532511287,
1.,0.923879532511287,1.,0.923879532511287,1.,0.923879532511287,1.,0.923879532511287,
1.,0.923879532511287,1.,0.923879532511287,1.,0.923879532511287,1.,0.923879532511287,
1.,0.923879532511287,1.,0.923879532511287,1.,0.923879532511287,1.,0.923879532511287,
1.,0.923879532511287,1.,0.923879532511287,1.,0.923879532511287,1.,0.923879532511287,
1.,0.923879532511287,1.,0.923879532511287,1.),(1.,0.923879532511287,1.,
0.923879532511287,1.,0.923879532511287,1.,0.923879532511287,1.,0.923879532511287,
1.,0.923879532511287,1.,0.923879532511287,1.,0.923879532511287,1.,0.923879532511287,
1.,0.923879532511287,1.,0.923879532511287,1.,0.923879532511287,1.,0.923879532511287,
1.,0.923879532511287,1.,0.923879532511287,1.,0.923879532511287,1.,0.923879532511287,
1.,0.923879532511287,1.,0.923879532511287,1.,0.923879532511287,1.,0.923879532511287,
1.,0.923879532511287,1.,0.923879532511287,1.,0.923879532511287,1.,0.923879532511287,
1.,0.923879532511287,1.,0.923879532511287,1.,0.923879532511287,1.,0.923879532511287,
1.,0.923879532511287,1.,0.923879532511287,1.,0.923879532511287,1.,0.923879532511287,
1.,0.923879532511287,1.,0.923879532511287,1.,0.923879532511287,1.,0.923879532511287,
1.,0.923879532511287,1.,0.923879532511287,1.,0.923879532511287,1.,0.923879532511287,
1.,0.923879532511287,1.,0.923879532511287,1.,0.923879532511287,1.,0.923879532511287,
1.,0.923879532511287,1.,0.923879532511287,1.,0.923879532511287,1.,0.923879532511287,
1.,0.923879532511287,1.,0.923879532511287,1.,0.923879532511287,1.,0.923879532511287,
1.,0.923879532511287,1.,0.923879532511287,1.,0.923879532511287,1.,0.923879532511287,
1.,0.923879532511287,1.,0.923879532511287,1.,0.923879532511287,1.,0.923879532511287,
1.,0.923879532511287,1.,0.923879532511287,1.,0.923879532511287,1.,0.923879532511287,
1.,0.923879532511287,1.,0.923879532511287,1.,0.923879532511287,1.,0.923879532511287,
1.,0.923879532511287,1.,0.923879532511287,1.,0.923879532511287,1.,0.923879532511287,
1.,0.923879532511287,1.,0.923879532511287,1.,0.923879532511287,1.,0.923879532511287,
1.,0.923879532511287,1.,0.923879532511287,1.,0.923879532511287,1.)))
REPRESENTATION_ITEM('')
SURFACE()
);
#4015=(
BOUNDED_SURFACE()
B_SPLINE_SURFACE(1,2,((#264016,#264017,#264018,#264019,#264020,#264021,
#264022,#264023,#264024,#264025,#264026,#264027,#264028,#264029,#264030,
#264031,#264032,#264033,#264034,#264035,#264036,#264037,#264038,#264039,
#264040,#264041,#264042,#264043,#264044,#264045,#264046,#264047,#264048,
#264049,#264050,#264051,#264052,#264053,#264054,#264055,#264056,#264057,
#264058,#264059,#264060,#264061,#264062,#264063,#264064,#264065,#264066,
#264067,#264068,#264069,#264070,#264071,#264072,#264073,#264074,#264075,
#264076,#264077,#264078,#264079,#264080,#264081,#264082,#264083,#264084,
#264085,#264086,#264087,#264088,#264089,#264090,#264091,#264092,#264093,
#264094,#264095,#264096,#264097,#264098,#264099,#264100,#264101,#264102,
#264103,#264104,#264105,#264106,#264107,#264108,#264109,#264110,#264111,
#264112,#264113,#264114,#264115,#264116,#264117,#264118,#264119,#264120,
#264121,#264122,#264123,#264124,#264125,#264126,#264127,#264128,#264129,
#264130,#264131,#264132,#264133,#264134,#264135,#264136,#264137,#264138,
#264139,#264140,#264141,#264142,#264143,#264144,#264145,#264146,#264147,
#264148,#264149,#264150,#264151,#264152,#264153,#264154,#264155,#264156,
#264157,#264158,#264159,#264160,#264161,#264162,#264163,#264164,#264165,
#264166,#264167,#264168,#264169,#264170,#264171,#264172,#264173,#264174,
#264175,#264176),(#264177,#264178,#264179,#264180,#264181,#264182,#264183,
#264184,#264185,#264186,#264187,#264188,#264189,#264190,#264191,#264192,
#264193,#264194,#264195,#264196,#264197,#264198,#264199,#264200,#264201,
#264202,#264203,#264204,#264205,#264206,#264207,#264208,#264209,#264210,
#264211,#264212,#264213,#264214,#264215,#264216,#264217,#264218,#264219,
#264220,#264221,#264222,#264223,#264224,#264225,#264226,#264227,#264228,
#264229,#264230,#264231,#264232,#264233,#264234,#264235,#264236,#264237,
#264238,#264239,#264240,#264241,#264242,#264243,#264244,#264245,#264246,
#264247,#264248,#264249,#264250,#264251,#264252,#264253,#264254,#264255,
#264256,#264257,#264258,#264259,#264260,#264261,#264262,#264263,#264264,
#264265,#264266,#264267,#264268,#264269,#264270,#264271,#264272,#264273,
#264274,#264275,#264276,#264277,#264278,#264279,#264280,#264281,#264282,
#264283,#264284,#264285,#264286,#264287,#264288,#264289,#264290,#264291,
#264292,#264293,#264294,#264295,#264296,#264297,#264298,#264299,#264300,
#264301,#264302,#264303,#264304,#264305,#264306,#264307,#264308,#264309,
#264310,#264311,#264312,#264313,#264314,#264315,#264316,#264317,#264318,
#264319,#264320,#264321,#264322,#264323,#264324,#264325,#264326,#264327,
#264328,#264329,#264330,#264331,#264332,#264333,#264334,#264335,#264336,
#264337)),.UNSPECIFIED.,.F.,.F.,.F.)
B_SPLINE_SURFACE_WITH_KNOTS((2,2),(3,2,2,2,2,2,2,2,2,2,2,2,2,2,2,2,2,2,
2,2,2,2,2,2,2,2,2,2,2,2,2,2,2,2,2,2,2,2,2,2,2,2,2,2,2,2,2,2,2,2,2,2,2,2,
2,2,2,2,2,2,2,2,2,2,2,2,2,2,2,2,2,2,2,2,2,2,2,2,2,2,3),(0.,1.),(0.,0.0125,
0.025,0.0375,0.05,0.0625,0.075,0.0875,0.1,0.1125,0.125,0.1375,0.15,0.1625,
0.175,0.1875,0.2,0.2125,0.225,0.2375,0.25,0.2625,0.275,0.2875,0.3,0.3125,
0.325,0.3375,0.35,0.3625,0.375,0.3875,0.4,0.4125,0.425,0.4375,0.45,0.4625,
0.475,0.4875,0.5,0.5125,0.525,0.5375,0.55,0.5625,0.575,0.5875,0.6,0.6125,
0.625,0.6375,0.65,0.6625,0.675,0.6875,0.7,0.7125,0.725,0.7375,0.75,0.7625,
0.775,0.7875,0.8,0.8125,0.825,0.8375,0.85,0.8625,0.875,0.8875,0.9,0.9125,
0.925,0.9375,0.95,0.9625,0.975,0.9875,1.),.UNSPECIFIED.)
GEOMETRIC_REPRESENTATION_ITEM()
RATIONAL_B_SPLINE_SURFACE(((1.,0.923879532511287,1.,0.923879532511287,1.,
0.923879532511287,1.,0.923879532511287,1.,0.923879532511287,1.,0.923879532511287,
1.,0.923879532511287,1.,0.923879532511287,1.,0.923879532511287,1.,0.923879532511287,
1.,0.923879532511287,1.,0.923879532511287,1.,0.923879532511287,1.,0.923879532511287,
1.,0.923879532511287,1.,0.923879532511287,1.,0.923879532511287,1.,0.923879532511287,
1.,0.923879532511287,1.,0.923879532511287,1.,0.923879532511287,1.,0.923879532511287,
1.,0.923879532511287,1.,0.923879532511287,1.,0.923879532511287,1.,0.923879532511287,
1.,0.923879532511287,1.,0.923879532511287,1.,0.923879532511287,1.,0.923879532511287,
1.,0.923879532511287,1.,0.923879532511287,1.,0.923879532511287,1.,0.923879532511287,
1.,0.923879532511287,1.,0.923879532511287,1.,0.923879532511287,1.,0.923879532511287,
1.,0.923879532511287,1.,0.923879532511287,1.,0.923879532511287,1.,0.923879532511287,
1.,0.923879532511287,1.,0.923879532511287,1.,0.923879532511287,1.,0.923879532511287,
1.,0.923879532511287,1.,0.923879532511287,1.,0.923879532511287,1.,0.923879532511287,
1.,0.923879532511287,1.,0.923879532511287,1.,0.923879532511287,1.,0.923879532511287,
1.,0.923879532511287,1.,0.923879532511287,1.,0.923879532511287,1.,0.923879532511287,
1.,0.923879532511287,1.,0.923879532511287,1.,0.923879532511287,1.,0.923879532511287,
1.,0.923879532511287,1.,0.923879532511287,1.,0.923879532511287,1.,0.923879532511287,
1.,0.923879532511287,1.,0.923879532511287,1.,0.923879532511287,1.,0.923879532511287,
1.,0.923879532511287,1.,0.923879532511287,1.,0.923879532511287,1.,0.923879532511287,
1.,0.923879532511287,1.,0.923879532511287,1.,0.923879532511287,1.,0.923879532511287,
1.,0.923879532511287,1.,0.923879532511287,1.),(1.,0.923879532511287,1.,
0.923879532511287,1.,0.923879532511287,1.,0.923879532511287,1.,0.923879532511287,
1.,0.923879532511287,1.,0.923879532511287,1.,0.923879532511287,1.,0.923879532511287,
1.,0.923879532511287,1.,0.923879532511287,1.,0.923879532511287,1.,0.923879532511287,
1.,0.923879532511287,1.,0.923879532511287,1.,0.923879532511287,1.,0.923879532511287,
1.,0.923879532511287,1.,0.923879532511287,1.,0.923879532511287,1.,0.923879532511287,
1.,0.923879532511287,1.,0.923879532511287,1.,0.923879532511287,1.,0.923879532511287,
1.,0.923879532511287,1.,0.923879532511287,1.,0.923879532511287,1.,0.923879532511287,
1.,0.923879532511287,1.,0.923879532511287,1.,0.923879532511287,1.,0.923879532511287,
1.,0.923879532511287,1.,0.923879532511287,1.,0.923879532511287,1.,0.923879532511287,
1.,0.923879532511287,1.,0.923879532511287,1.,0.923879532511287,1.,0.923879532511287,
1.,0.923879532511287,1.,0.923879532511287,1.,0.923879532511287,1.,0.923879532511287,
1.,0.923879532511287,1.,0.923879532511287,1.,0.923879532511287,1.,0.923879532511287,
1.,0.923879532511287,1.,0.923879532511287,1.,0.923879532511287,1.,0.923879532511287,
1.,0.923879532511287,1.,0.923879532511287,1.,0.923879532511287,1.,0.923879532511287,
1.,0.923879532511287,1.,0.923879532511287,1.,0.923879532511287,1.,0.923879532511287,
1.,0.923879532511287,1.,0.923879532511287,1.,0.923879532511287,1.,0.923879532511287,
1.,0.923879532511287,1.,0.923879532511287,1.,0.923879532511287,1.,0.923879532511287,
1.,0.923879532511287,1.,0.923879532511287,1.,0.923879532511287,1.,0.923879532511287,
1.,0.923879532511287,1.,0.923879532511287,1.,0.923879532511287,1.,0.923879532511287,
1.,0.923879532511287,1.,0.923879532511287,1.,0.923879532511287,1.)))
REPRESENTATION_ITEM('')
SURFACE()
);
#4016=(
BOUNDED_SURFACE()
B_SPLINE_SURFACE(1,2,((#264373,#264374,#264375,#264376,#264377,#264378,
#264379,#264380,#264381,#264382,#264383,#264384,#264385,#264386,#264387,
#264388,#264389,#264390,#264391,#264392,#264393,#264394,#264395,#264396,
#264397,#264398,#264399,#264400,#264401,#264402,#264403,#264404,#264405,
#264406,#264407,#264408,#264409,#264410,#264411,#264412,#264413,#264414,
#264415,#264416,#264417,#264418,#264419,#264420,#264421,#264422,#264423,
#264424,#264425,#264426,#264427,#264428,#264429,#264430,#264431,#264432,
#264433,#264434,#264435,#264436,#264437,#264438,#264439,#264440,#264441,
#264442,#264443,#264444,#264445,#264446,#264447,#264448,#264449,#264450,
#264451,#264452,#264453,#264454,#264455,#264456,#264457,#264458,#264459,
#264460,#264461,#264462,#264463,#264464,#264465,#264466,#264467,#264468,
#264469,#264470,#264471,#264472,#264473,#264474,#264475,#264476,#264477,
#264478,#264479,#264480,#264481,#264482,#264483,#264484,#264485,#264486,
#264487,#264488,#264489,#264490,#264491,#264492,#264493,#264494,#264495,
#264496,#264497,#264498,#264499,#264500,#264501,#264502,#264503,#264504,
#264505,#264506,#264507,#264508,#264509,#264510,#264511,#264512,#264513,
#264514,#264515,#264516,#264517,#264518,#264519,#264520,#264521,#264522,
#264523,#264524,#264525,#264526,#264527,#264528,#264529,#264530,#264531,
#264532,#264533),(#264534,#264535,#264536,#264537,#264538,#264539,#264540,
#264541,#264542,#264543,#264544,#264545,#264546,#264547,#264548,#264549,
#264550,#264551,#264552,#264553,#264554,#264555,#264556,#264557,#264558,
#264559,#264560,#264561,#264562,#264563,#264564,#264565,#264566,#264567,
#264568,#264569,#264570,#264571,#264572,#264573,#264574,#264575,#264576,
#264577,#264578,#264579,#264580,#264581,#264582,#264583,#264584,#264585,
#264586,#264587,#264588,#264589,#264590,#264591,#264592,#264593,#264594,
#264595,#264596,#264597,#264598,#264599,#264600,#264601,#264602,#264603,
#264604,#264605,#264606,#264607,#264608,#264609,#264610,#264611,#264612,
#264613,#264614,#264615,#264616,#264617,#264618,#264619,#264620,#264621,
#264622,#264623,#264624,#264625,#264626,#264627,#264628,#264629,#264630,
#264631,#264632,#264633,#264634,#264635,#264636,#264637,#264638,#264639,
#264640,#264641,#264642,#264643,#264644,#264645,#264646,#264647,#264648,
#264649,#264650,#264651,#264652,#264653,#264654,#264655,#264656,#264657,
#264658,#264659,#264660,#264661,#264662,#264663,#264664,#264665,#264666,
#264667,#264668,#264669,#264670,#264671,#264672,#264673,#264674,#264675,
#264676,#264677,#264678,#264679,#264680,#264681,#264682,#264683,#264684,
#264685,#264686,#264687,#264688,#264689,#264690,#264691,#264692,#264693,
#264694)),.UNSPECIFIED.,.F.,.F.,.F.)
B_SPLINE_SURFACE_WITH_KNOTS((2,2),(3,2,2,2,2,2,2,2,2,2,2,2,2,2,2,2,2,2,
2,2,2,2,2,2,2,2,2,2,2,2,2,2,2,2,2,2,2,2,2,2,2,2,2,2,2,2,2,2,2,2,2,2,2,2,
2,2,2,2,2,2,2,2,2,2,2,2,2,2,2,2,2,2,2,2,2,2,2,2,2,2,3),(0.,1.),(0.,0.0125,
0.025,0.0375,0.05,0.0625,0.075,0.0875,0.1,0.1125,0.125,0.1375,0.15,0.1625,
0.175,0.1875,0.2,0.2125,0.225,0.2375,0.25,0.2625,0.275,0.2875,0.3,0.3125,
0.325,0.3375,0.35,0.3625,0.375,0.3875,0.4,0.4125,0.425,0.4375,0.45,0.4625,
0.475,0.4875,0.5,0.5125,0.525,0.5375,0.55,0.5625,0.575,0.5875,0.6,0.6125,
0.625,0.6375,0.65,0.6625,0.675,0.6875,0.7,0.7125,0.725,0.7375,0.75,0.7625,
0.775,0.7875,0.8,0.8125,0.825,0.8375,0.85,0.8625,0.875,0.8875,0.9,0.9125,
0.925,0.9375,0.95,0.9625,0.975,0.9875,1.),.UNSPECIFIED.)
GEOMETRIC_REPRESENTATION_ITEM()
RATIONAL_B_SPLINE_SURFACE(((1.,0.923879532511287,1.,0.923879532511287,1.,
0.923879532511287,1.,0.923879532511287,1.,0.923879532511287,1.,0.923879532511287,
1.,0.923879532511287,1.,0.923879532511287,1.,0.923879532511287,1.,0.923879532511287,
1.,0.923879532511287,1.,0.923879532511287,1.,0.923879532511287,1.,0.923879532511287,
1.,0.923879532511287,1.,0.923879532511287,1.,0.923879532511287,1.,0.923879532511287,
1.,0.923879532511287,1.,0.923879532511287,1.,0.923879532511287,1.,0.923879532511287,
1.,0.923879532511287,1.,0.923879532511287,1.,0.923879532511287,1.,0.923879532511287,
1.,0.923879532511287,1.,0.923879532511287,1.,0.923879532511287,1.,0.923879532511287,
1.,0.923879532511287,1.,0.923879532511287,1.,0.923879532511287,1.,0.923879532511287,
1.,0.923879532511287,1.,0.923879532511287,1.,0.923879532511287,1.,0.923879532511287,
1.,0.923879532511287,1.,0.923879532511287,1.,0.923879532511287,1.,0.923879532511287,
1.,0.923879532511287,1.,0.923879532511287,1.,0.923879532511287,1.,0.923879532511287,
1.,0.923879532511287,1.,0.923879532511287,1.,0.923879532511287,1.,0.923879532511287,
1.,0.923879532511287,1.,0.923879532511287,1.,0.923879532511287,1.,0.923879532511287,
1.,0.923879532511287,1.,0.923879532511287,1.,0.923879532511287,1.,0.923879532511287,
1.,0.923879532511287,1.,0.923879532511287,1.,0.923879532511287,1.,0.923879532511287,
1.,0.923879532511287,1.,0.923879532511287,1.,0.923879532511287,1.,0.923879532511287,
1.,0.923879532511287,1.,0.923879532511287,1.,0.923879532511287,1.,0.923879532511287,
1.,0.923879532511287,1.,0.923879532511287,1.,0.923879532511287,1.,0.923879532511287,
1.,0.923879532511287,1.,0.923879532511287,1.,0.923879532511287,1.,0.923879532511287,
1.,0.923879532511287,1.,0.923879532511287,1.),(1.,0.923879532511287,1.,
0.923879532511287,1.,0.923879532511287,1.,0.923879532511287,1.,0.923879532511287,
1.,0.923879532511287,1.,0.923879532511287,1.,0.923879532511287,1.,0.923879532511287,
1.,0.923879532511287,1.,0.923879532511287,1.,0.923879532511287,1.,0.923879532511287,
1.,0.923879532511287,1.,0.923879532511287,1.,0.923879532511287,1.,0.923879532511287,
1.,0.923879532511287,1.,0.923879532511287,1.,0.923879532511287,1.,0.923879532511287,
1.,0.923879532511287,1.,0.923879532511287,1.,0.923879532511287,1.,0.923879532511287,
1.,0.923879532511287,1.,0.923879532511287,1.,0.923879532511287,1.,0.923879532511287,
1.,0.923879532511287,1.,0.923879532511287,1.,0.923879532511287,1.,0.923879532511287,
1.,0.923879532511287,1.,0.923879532511287,1.,0.923879532511287,1.,0.923879532511287,
1.,0.923879532511287,1.,0.923879532511287,1.,0.923879532511287,1.,0.923879532511287,
1.,0.923879532511287,1.,0.923879532511287,1.,0.923879532511287,1.,0.923879532511287,
1.,0.923879532511287,1.,0.923879532511287,1.,0.923879532511287,1.,0.923879532511287,
1.,0.923879532511287,1.,0.923879532511287,1.,0.923879532511287,1.,0.923879532511287,
1.,0.923879532511287,1.,0.923879532511287,1.,0.923879532511287,1.,0.923879532511287,
1.,0.923879532511287,1.,0.923879532511287,1.,0.923879532511287,1.,0.923879532511287,
1.,0.923879532511287,1.,0.923879532511287,1.,0.923879532511287,1.,0.923879532511287,
1.,0.923879532511287,1.,0.923879532511287,1.,0.923879532511287,1.,0.923879532511287,
1.,0.923879532511287,1.,0.923879532511287,1.,0.923879532511287,1.,0.923879532511287,
1.,0.923879532511287,1.,0.923879532511287,1.,0.923879532511287,1.,0.923879532511287,
1.,0.923879532511287,1.,0.923879532511287,1.,0.923879532511287,1.)))
REPRESENTATION_ITEM('')
SURFACE()
);
#4017=(
BOUNDED_SURFACE()
B_SPLINE_SURFACE(1,2,((#265160,#265161,#265162,#265163,#265164,#265165,
#265166,#265167,#265168,#265169,#265170,#265171,#265172,#265173,#265174,
#265175,#265176,#265177,#265178,#265179,#265180,#265181,#265182,#265183,
#265184,#265185,#265186,#265187,#265188,#265189,#265190,#265191,#265192,
#265193,#265194,#265195,#265196,#265197,#265198,#265199,#265200,#265201,
#265202,#265203,#265204,#265205,#265206,#265207,#265208,#265209,#265210,
#265211,#265212,#265213,#265214,#265215,#265216,#265217,#265218,#265219,
#265220,#265221,#265222,#265223,#265224,#265225,#265226,#265227,#265228,
#265229,#265230,#265231,#265232,#265233,#265234,#265235,#265236,#265237,
#265238,#265239,#265240),(#265241,#265242,#265243,#265244,#265245,#265246,
#265247,#265248,#265249,#265250,#265251,#265252,#265253,#265254,#265255,
#265256,#265257,#265258,#265259,#265260,#265261,#265262,#265263,#265264,
#265265,#265266,#265267,#265268,#265269,#265270,#265271,#265272,#265273,
#265274,#265275,#265276,#265277,#265278,#265279,#265280,#265281,#265282,
#265283,#265284,#265285,#265286,#265287,#265288,#265289,#265290,#265291,
#265292,#265293,#265294,#265295,#265296,#265297,#265298,#265299,#265300,
#265301,#265302,#265303,#265304,#265305,#265306,#265307,#265308,#265309,
#265310,#265311,#265312,#265313,#265314,#265315,#265316,#265317,#265318,
#265319,#265320,#265321)),.UNSPECIFIED.,.F.,.F.,.F.)
B_SPLINE_SURFACE_WITH_KNOTS((2,2),(3,2,2,2,2,2,2,2,2,2,2,2,2,2,2,2,2,2,
2,2,2,2,2,2,2,2,2,2,2,2,2,2,2,2,2,2,2,2,2,2,3),(0.,1.),(0.,0.025,0.05,0.075,
0.1,0.125,0.15,0.175,0.2,0.225,0.25,0.275,0.3,0.325,0.35,0.375,0.4,0.425,
0.45,0.475,0.5,0.525,0.55,0.575,0.6,0.625,0.65,0.675,0.7,0.725,0.75,0.775,
0.8,0.825,0.85,0.875,0.9,0.925,0.95,0.975,1.),.UNSPECIFIED.)
GEOMETRIC_REPRESENTATION_ITEM()
RATIONAL_B_SPLINE_SURFACE(((1.,0.996917333733128,1.,0.996917333733128,1.,
0.996917333733128,1.,0.996917333733128,1.,0.996917333733128,1.,0.996917333733128,
1.,0.996917333733128,1.,0.996917333733128,1.,0.996917333733128,1.,0.996917333733128,
1.,0.996917333733128,1.,0.996917333733128,1.,0.996917333733128,1.,0.996917333733128,
1.,0.996917333733128,1.,0.996917333733128,1.,0.996917333733128,1.,0.996917333733128,
1.,0.996917333733128,1.,0.996917333733128,1.,0.996917333733128,1.,0.996917333733128,
1.,0.996917333733128,1.,0.996917333733128,1.,0.996917333733128,1.,0.996917333733128,
1.,0.996917333733128,1.,0.996917333733128,1.,0.996917333733128,1.,0.996917333733128,
1.,0.996917333733128,1.,0.996917333733128,1.,0.996917333733128,1.,0.996917333733128,
1.,0.996917333733128,1.,0.996917333733128,1.,0.996917333733128,1.,0.996917333733128,
1.,0.996917333733128,1.,0.996917333733128,1.),(1.,0.996917333733128,1.,
0.996917333733128,1.,0.996917333733128,1.,0.996917333733128,1.,0.996917333733128,
1.,0.996917333733128,1.,0.996917333733128,1.,0.996917333733128,1.,0.996917333733128,
1.,0.996917333733128,1.,0.996917333733128,1.,0.996917333733128,1.,0.996917333733128,
1.,0.996917333733128,1.,0.996917333733128,1.,0.996917333733128,1.,0.996917333733128,
1.,0.996917333733128,1.,0.996917333733128,1.,0.996917333733128,1.,0.996917333733128,
1.,0.996917333733128,1.,0.996917333733128,1.,0.996917333733128,1.,0.996917333733128,
1.,0.996917333733128,1.,0.996917333733128,1.,0.996917333733128,1.,0.996917333733128,
1.,0.996917333733128,1.,0.996917333733128,1.,0.996917333733128,1.,0.996917333733128,
1.,0.996917333733128,1.,0.996917333733128,1.,0.996917333733128,1.,0.996917333733128,
1.,0.996917333733128,1.,0.996917333733128,1.,0.996917333733128,1.)))
REPRESENTATION_ITEM('')
SURFACE()
);
#4018=(
BOUNDED_SURFACE()
B_SPLINE_SURFACE(1,2,((#265347,#265348,#265349,#265350,#265351,#265352,
#265353,#265354,#265355,#265356,#265357,#265358,#265359,#265360,#265361,
#265362,#265363,#265364,#265365,#265366,#265367,#265368,#265369,#265370,
#265371,#265372,#265373,#265374,#265375,#265376,#265377,#265378,#265379,
#265380,#265381,#265382,#265383,#265384,#265385,#265386,#265387,#265388,
#265389,#265390,#265391,#265392,#265393,#265394,#265395,#265396,#265397,
#265398,#265399,#265400,#265401,#265402,#265403,#265404,#265405,#265406,
#265407,#265408,#265409,#265410,#265411,#265412,#265413,#265414,#265415,
#265416,#265417,#265418,#265419,#265420,#265421,#265422,#265423,#265424,
#265425,#265426,#265427),(#265428,#265429,#265430,#265431,#265432,#265433,
#265434,#265435,#265436,#265437,#265438,#265439,#265440,#265441,#265442,
#265443,#265444,#265445,#265446,#265447,#265448,#265449,#265450,#265451,
#265452,#265453,#265454,#265455,#265456,#265457,#265458,#265459,#265460,
#265461,#265462,#265463,#265464,#265465,#265466,#265467,#265468,#265469,
#265470,#265471,#265472,#265473,#265474,#265475,#265476,#265477,#265478,
#265479,#265480,#265481,#265482,#265483,#265484,#265485,#265486,#265487,
#265488,#265489,#265490,#265491,#265492,#265493,#265494,#265495,#265496,
#265497,#265498,#265499,#265500,#265501,#265502,#265503,#265504,#265505,
#265506,#265507,#265508)),.UNSPECIFIED.,.F.,.F.,.F.)
B_SPLINE_SURFACE_WITH_KNOTS((2,2),(3,2,2,2,2,2,2,2,2,2,2,2,2,2,2,2,2,2,
2,2,2,2,2,2,2,2,2,2,2,2,2,2,2,2,2,2,2,2,2,2,3),(0.,1.),(0.,0.025,0.05,0.075,
0.1,0.125,0.15,0.175,0.2,0.225,0.25,0.275,0.3,0.325,0.35,0.375,0.4,0.425,
0.45,0.475,0.5,0.525,0.55,0.575,0.6,0.625,0.65,0.675,0.7,0.725,0.75,0.775,
0.8,0.825,0.85,0.875,0.9,0.925,0.95,0.975,1.),.UNSPECIFIED.)
GEOMETRIC_REPRESENTATION_ITEM()
RATIONAL_B_SPLINE_SURFACE(((1.,0.996917333733128,1.,0.996917333733128,1.,
0.996917333733128,1.,0.996917333733128,1.,0.996917333733128,1.,0.996917333733128,
1.,0.996917333733128,1.,0.996917333733128,1.,0.996917333733128,1.,0.996917333733128,
1.,0.996917333733128,1.,0.996917333733128,1.,0.996917333733128,1.,0.996917333733128,
1.,0.996917333733128,1.,0.996917333733128,1.,0.996917333733128,1.,0.996917333733128,
1.,0.996917333733128,1.,0.996917333733128,1.,0.996917333733128,1.,0.996917333733128,
1.,0.996917333733128,1.,0.996917333733128,1.,0.996917333733128,1.,0.996917333733128,
1.,0.996917333733128,1.,0.996917333733128,1.,0.996917333733128,1.,0.996917333733128,
1.,0.996917333733128,1.,0.996917333733128,1.,0.996917333733128,1.,0.996917333733128,
1.,0.996917333733128,1.,0.996917333733128,1.,0.996917333733128,1.,0.996917333733128,
1.,0.996917333733128,1.,0.996917333733128,1.),(1.,0.996917333733128,1.,
0.996917333733128,1.,0.996917333733128,1.,0.996917333733128,1.,0.996917333733128,
1.,0.996917333733128,1.,0.996917333733128,1.,0.996917333733128,1.,0.996917333733128,
1.,0.996917333733128,1.,0.996917333733128,1.,0.996917333733128,1.,0.996917333733128,
1.,0.996917333733128,1.,0.996917333733128,1.,0.996917333733128,1.,0.996917333733128,
1.,0.996917333733128,1.,0.996917333733128,1.,0.996917333733128,1.,0.996917333733128,
1.,0.996917333733128,1.,0.996917333733128,1.,0.996917333733128,1.,0.996917333733128,
1.,0.996917333733128,1.,0.996917333733128,1.,0.996917333733128,1.,0.996917333733128,
1.,0.996917333733128,1.,0.996917333733128,1.,0.996917333733128,1.,0.996917333733128,
1.,0.996917333733128,1.,0.996917333733128,1.,0.996917333733128,1.,0.996917333733128,
1.,0.996917333733128,1.,0.996917333733128,1.,0.996917333733128,1.)))
REPRESENTATION_ITEM('')
SURFACE()
);
#4019=(
BOUNDED_SURFACE()
B_SPLINE_SURFACE(1,2,((#265518,#265519,#265520,#265521,#265522,#265523,
#265524,#265525,#265526,#265527,#265528,#265529,#265530,#265531,#265532,
#265533,#265534,#265535,#265536,#265537,#265538,#265539,#265540,#265541,
#265542,#265543,#265544,#265545,#265546,#265547,#265548,#265549,#265550,
#265551,#265552,#265553,#265554,#265555,#265556,#265557,#265558,#265559,
#265560,#265561,#265562,#265563,#265564,#265565,#265566,#265567,#265568,
#265569,#265570,#265571,#265572,#265573,#265574,#265575,#265576,#265577,
#265578,#265579,#265580,#265581,#265582,#265583,#265584,#265585,#265586,
#265587,#265588,#265589,#265590,#265591,#265592,#265593,#265594,#265595,
#265596,#265597,#265598),(#265599,#265600,#265601,#265602,#265603,#265604,
#265605,#265606,#265607,#265608,#265609,#265610,#265611,#265612,#265613,
#265614,#265615,#265616,#265617,#265618,#265619,#265620,#265621,#265622,
#265623,#265624,#265625,#265626,#265627,#265628,#265629,#265630,#265631,
#265632,#265633,#265634,#265635,#265636,#265637,#265638,#265639,#265640,
#265641,#265642,#265643,#265644,#265645,#265646,#265647,#265648,#265649,
#265650,#265651,#265652,#265653,#265654,#265655,#265656,#265657,#265658,
#265659,#265660,#265661,#265662,#265663,#265664,#265665,#265666,#265667,
#265668,#265669,#265670,#265671,#265672,#265673,#265674,#265675,#265676,
#265677,#265678,#265679)),.UNSPECIFIED.,.F.,.F.,.F.)
B_SPLINE_SURFACE_WITH_KNOTS((2,2),(3,2,2,2,2,2,2,2,2,2,2,2,2,2,2,2,2,2,
2,2,2,2,2,2,2,2,2,2,2,2,2,2,2,2,2,2,2,2,2,2,3),(0.,1.),(0.,0.025,0.05,0.075,
0.1,0.125,0.15,0.175,0.2,0.225,0.25,0.275,0.3,0.325,0.35,0.375,0.4,0.425,
0.45,0.475,0.5,0.525,0.55,0.575,0.6,0.625,0.65,0.675,0.7,0.725,0.75,0.775,
0.8,0.825,0.85,0.875,0.9,0.925,0.95,0.975,1.),.UNSPECIFIED.)
GEOMETRIC_REPRESENTATION_ITEM()
RATIONAL_B_SPLINE_SURFACE(((1.,0.996917333733128,1.,0.996917333733128,1.,
0.996917333733128,1.,0.996917333733128,1.,0.996917333733128,1.,0.996917333733128,
1.,0.996917333733128,1.,0.996917333733128,1.,0.996917333733128,1.,0.996917333733128,
1.,0.996917333733128,1.,0.996917333733128,1.,0.996917333733128,1.,0.996917333733128,
1.,0.996917333733128,1.,0.996917333733128,1.,0.996917333733128,1.,0.996917333733128,
1.,0.996917333733128,1.,0.996917333733128,1.,0.996917333733128,1.,0.996917333733128,
1.,0.996917333733128,1.,0.996917333733128,1.,0.996917333733128,1.,0.996917333733128,
1.,0.996917333733128,1.,0.996917333733128,1.,0.996917333733128,1.,0.996917333733128,
1.,0.996917333733128,1.,0.996917333733128,1.,0.996917333733128,1.,0.996917333733128,
1.,0.996917333733128,1.,0.996917333733128,1.,0.996917333733128,1.,0.996917333733128,
1.,0.996917333733128,1.,0.996917333733128,1.),(1.,0.996917333733128,1.,
0.996917333733128,1.,0.996917333733128,1.,0.996917333733128,1.,0.996917333733128,
1.,0.996917333733128,1.,0.996917333733128,1.,0.996917333733128,1.,0.996917333733128,
1.,0.996917333733128,1.,0.996917333733128,1.,0.996917333733128,1.,0.996917333733128,
1.,0.996917333733128,1.,0.996917333733128,1.,0.996917333733128,1.,0.996917333733128,
1.,0.996917333733128,1.,0.996917333733128,1.,0.996917333733128,1.,0.996917333733128,
1.,0.996917333733128,1.,0.996917333733128,1.,0.996917333733128,1.,0.996917333733128,
1.,0.996917333733128,1.,0.996917333733128,1.,0.996917333733128,1.,0.996917333733128,
1.,0.996917333733128,1.,0.996917333733128,1.,0.996917333733128,1.,0.996917333733128,
1.,0.996917333733128,1.,0.996917333733128,1.,0.996917333733128,1.,0.996917333733128,
1.,0.996917333733128,1.,0.996917333733128,1.,0.996917333733128,1.)))
REPRESENTATION_ITEM('')
SURFACE()
);
#4020=(
BOUNDED_SURFACE()
B_SPLINE_SURFACE(1,2,((#265698,#265699,#265700,#265701,#265702,#265703,
#265704,#265705,#265706,#265707,#265708,#265709,#265710,#265711,#265712,
#265713,#265714,#265715,#265716,#265717,#265718,#265719,#265720,#265721,
#265722,#265723,#265724,#265725,#265726,#265727,#265728,#265729,#265730,
#265731,#265732,#265733,#265734,#265735,#265736,#265737,#265738,#265739,
#265740,#265741,#265742,#265743,#265744,#265745,#265746,#265747,#265748,
#265749,#265750,#265751,#265752,#265753,#265754,#265755,#265756,#265757,
#265758,#265759,#265760,#265761,#265762,#265763,#265764,#265765,#265766,
#265767,#265768,#265769,#265770,#265771,#265772,#265773,#265774,#265775,
#265776,#265777,#265778),(#265779,#265780,#265781,#265782,#265783,#265784,
#265785,#265786,#265787,#265788,#265789,#265790,#265791,#265792,#265793,
#265794,#265795,#265796,#265797,#265798,#265799,#265800,#265801,#265802,
#265803,#265804,#265805,#265806,#265807,#265808,#265809,#265810,#265811,
#265812,#265813,#265814,#265815,#265816,#265817,#265818,#265819,#265820,
#265821,#265822,#265823,#265824,#265825,#265826,#265827,#265828,#265829,
#265830,#265831,#265832,#265833,#265834,#265835,#265836,#265837,#265838,
#265839,#265840,#265841,#265842,#265843,#265844,#265845,#265846,#265847,
#265848,#265849,#265850,#265851,#265852,#265853,#265854,#265855,#265856,
#265857,#265858,#265859)),.UNSPECIFIED.,.F.,.F.,.F.)
B_SPLINE_SURFACE_WITH_KNOTS((2,2),(3,2,2,2,2,2,2,2,2,2,2,2,2,2,2,2,2,2,
2,2,2,2,2,2,2,2,2,2,2,2,2,2,2,2,2,2,2,2,2,2,3),(0.,1.),(0.,0.025,0.05,0.075,
0.1,0.125,0.15,0.175,0.2,0.225,0.25,0.275,0.3,0.325,0.35,0.375,0.4,0.425,
0.45,0.475,0.5,0.525,0.55,0.575,0.6,0.625,0.65,0.675,0.7,0.725,0.75,0.775,
0.8,0.825,0.85,0.875,0.9,0.925,0.95,0.975,1.),.UNSPECIFIED.)
GEOMETRIC_REPRESENTATION_ITEM()
RATIONAL_B_SPLINE_SURFACE(((1.,0.996917333733128,1.,0.996917333733128,1.,
0.996917333733128,1.,0.996917333733128,1.,0.996917333733128,1.,0.996917333733128,
1.,0.996917333733128,1.,0.996917333733128,1.,0.996917333733128,1.,0.996917333733128,
1.,0.996917333733128,1.,0.996917333733128,1.,0.996917333733128,1.,0.996917333733128,
1.,0.996917333733128,1.,0.996917333733128,1.,0.996917333733128,1.,0.996917333733128,
1.,0.996917333733128,1.,0.996917333733128,1.,0.996917333733128,1.,0.996917333733128,
1.,0.996917333733128,1.,0.996917333733128,1.,0.996917333733128,1.,0.996917333733128,
1.,0.996917333733128,1.,0.996917333733128,1.,0.996917333733128,1.,0.996917333733128,
1.,0.996917333733128,1.,0.996917333733128,1.,0.996917333733128,1.,0.996917333733128,
1.,0.996917333733128,1.,0.996917333733128,1.,0.996917333733128,1.,0.996917333733128,
1.,0.996917333733128,1.,0.996917333733128,1.),(1.,0.996917333733128,1.,
0.996917333733128,1.,0.996917333733128,1.,0.996917333733128,1.,0.996917333733128,
1.,0.996917333733128,1.,0.996917333733128,1.,0.996917333733128,1.,0.996917333733128,
1.,0.996917333733128,1.,0.996917333733128,1.,0.996917333733128,1.,0.996917333733128,
1.,0.996917333733128,1.,0.996917333733128,1.,0.996917333733128,1.,0.996917333733128,
1.,0.996917333733128,1.,0.996917333733128,1.,0.996917333733128,1.,0.996917333733128,
1.,0.996917333733128,1.,0.996917333733128,1.,0.996917333733128,1.,0.996917333733128,
1.,0.996917333733128,1.,0.996917333733128,1.,0.996917333733128,1.,0.996917333733128,
1.,0.996917333733128,1.,0.996917333733128,1.,0.996917333733128,1.,0.996917333733128,
1.,0.996917333733128,1.,0.996917333733128,1.,0.996917333733128,1.,0.996917333733128,
1.,0.996917333733128,1.,0.996917333733128,1.,0.996917333733128,1.)))
REPRESENTATION_ITEM('')
SURFACE()
);
#4021=(
BOUNDED_SURFACE()
B_SPLINE_SURFACE(1,2,((#265864,#265865,#265866,#265867,#265868,#265869,
#265870,#265871,#265872,#265873,#265874,#265875,#265876,#265877,#265878,
#265879,#265880,#265881,#265882,#265883,#265884,#265885,#265886,#265887,
#265888,#265889,#265890,#265891,#265892,#265893,#265894,#265895,#265896,
#265897,#265898,#265899,#265900,#265901,#265902,#265903,#265904,#265905,
#265906,#265907,#265908,#265909,#265910,#265911,#265912,#265913,#265914,
#265915,#265916,#265917,#265918,#265919,#265920,#265921,#265922,#265923,
#265924,#265925,#265926,#265927,#265928,#265929,#265930,#265931,#265932,
#265933,#265934,#265935,#265936,#265937,#265938,#265939,#265940,#265941,
#265942,#265943,#265944),(#265945,#265946,#265947,#265948,#265949,#265950,
#265951,#265952,#265953,#265954,#265955,#265956,#265957,#265958,#265959,
#265960,#265961,#265962,#265963,#265964,#265965,#265966,#265967,#265968,
#265969,#265970,#265971,#265972,#265973,#265974,#265975,#265976,#265977,
#265978,#265979,#265980,#265981,#265982,#265983,#265984,#265985,#265986,
#265987,#265988,#265989,#265990,#265991,#265992,#265993,#265994,#265995,
#265996,#265997,#265998,#265999,#266000,#266001,#266002,#266003,#266004,
#266005,#266006,#266007,#266008,#266009,#266010,#266011,#266012,#266013,
#266014,#266015,#266016,#266017,#266018,#266019,#266020,#266021,#266022,
#266023,#266024,#266025)),.UNSPECIFIED.,.F.,.F.,.F.)
B_SPLINE_SURFACE_WITH_KNOTS((2,2),(3,2,2,2,2,2,2,2,2,2,2,2,2,2,2,2,2,2,
2,2,2,2,2,2,2,2,2,2,2,2,2,2,2,2,2,2,2,2,2,2,3),(0.,1.),(0.,0.025,0.05,0.075,
0.1,0.125,0.15,0.175,0.2,0.225,0.25,0.275,0.3,0.325,0.35,0.375,0.4,0.425,
0.45,0.475,0.5,0.525,0.55,0.575,0.6,0.625,0.65,0.675,0.7,0.725,0.75,0.775,
0.8,0.825,0.85,0.875,0.9,0.925,0.95,0.975,1.),.UNSPECIFIED.)
GEOMETRIC_REPRESENTATION_ITEM()
RATIONAL_B_SPLINE_SURFACE(((1.,0.996917333733128,1.,0.996917333733128,1.,
0.996917333733128,1.,0.996917333733128,1.,0.996917333733128,1.,0.996917333733128,
1.,0.996917333733128,1.,0.996917333733128,1.,0.996917333733128,1.,0.996917333733128,
1.,0.996917333733128,1.,0.996917333733128,1.,0.996917333733128,1.,0.996917333733128,
1.,0.996917333733128,1.,0.996917333733128,1.,0.996917333733128,1.,0.996917333733128,
1.,0.996917333733128,1.,0.996917333733128,1.,0.996917333733128,1.,0.996917333733128,
1.,0.996917333733128,1.,0.996917333733128,1.,0.996917333733128,1.,0.996917333733128,
1.,0.996917333733128,1.,0.996917333733128,1.,0.996917333733128,1.,0.996917333733128,
1.,0.996917333733128,1.,0.996917333733128,1.,0.996917333733128,1.,0.996917333733128,
1.,0.996917333733128,1.,0.996917333733128,1.,0.996917333733128,1.,0.996917333733128,
1.,0.996917333733128,1.,0.996917333733128,1.),(1.,0.996917333733128,1.,
0.996917333733128,1.,0.996917333733128,1.,0.996917333733128,1.,0.996917333733128,
1.,0.996917333733128,1.,0.996917333733128,1.,0.996917333733128,1.,0.996917333733128,
1.,0.996917333733128,1.,0.996917333733128,1.,0.996917333733128,1.,0.996917333733128,
1.,0.996917333733128,1.,0.996917333733128,1.,0.996917333733128,1.,0.996917333733128,
1.,0.996917333733128,1.,0.996917333733128,1.,0.996917333733128,1.,0.996917333733128,
1.,0.996917333733128,1.,0.996917333733128,1.,0.996917333733128,1.,0.996917333733128,
1.,0.996917333733128,1.,0.996917333733128,1.,0.996917333733128,1.,0.996917333733128,
1.,0.996917333733128,1.,0.996917333733128,1.,0.996917333733128,1.,0.996917333733128,
1.,0.996917333733128,1.,0.996917333733128,1.,0.996917333733128,1.,0.996917333733128,
1.,0.996917333733128,1.,0.996917333733128,1.,0.996917333733128,1.)))
REPRESENTATION_ITEM('')
SURFACE()
);
#4022=(
BOUNDED_SURFACE()
B_SPLINE_SURFACE(1,2,((#266051,#266052,#266053,#266054,#266055,#266056,
#266057,#266058,#266059,#266060,#266061,#266062,#266063,#266064,#266065,
#266066,#266067,#266068,#266069,#266070,#266071,#266072,#266073,#266074,
#266075,#266076,#266077,#266078,#266079,#266080,#266081,#266082,#266083,
#266084,#266085,#266086,#266087,#266088,#266089,#266090,#266091,#266092,
#266093,#266094,#266095,#266096,#266097,#266098,#266099,#266100,#266101,
#266102,#266103,#266104,#266105,#266106,#266107,#266108,#266109,#266110,
#266111,#266112,#266113,#266114,#266115,#266116,#266117,#266118,#266119,
#266120,#266121,#266122,#266123,#266124,#266125,#266126,#266127,#266128,
#266129,#266130,#266131),(#266132,#266133,#266134,#266135,#266136,#266137,
#266138,#266139,#266140,#266141,#266142,#266143,#266144,#266145,#266146,
#266147,#266148,#266149,#266150,#266151,#266152,#266153,#266154,#266155,
#266156,#266157,#266158,#266159,#266160,#266161,#266162,#266163,#266164,
#266165,#266166,#266167,#266168,#266169,#266170,#266171,#266172,#266173,
#266174,#266175,#266176,#266177,#266178,#266179,#266180,#266181,#266182,
#266183,#266184,#266185,#266186,#266187,#266188,#266189,#266190,#266191,
#266192,#266193,#266194,#266195,#266196,#266197,#266198,#266199,#266200,
#266201,#266202,#266203,#266204,#266205,#266206,#266207,#266208,#266209,
#266210,#266211,#266212)),.UNSPECIFIED.,.F.,.F.,.F.)
B_SPLINE_SURFACE_WITH_KNOTS((2,2),(3,2,2,2,2,2,2,2,2,2,2,2,2,2,2,2,2,2,
2,2,2,2,2,2,2,2,2,2,2,2,2,2,2,2,2,2,2,2,2,2,3),(0.,1.),(0.,0.025,0.05,0.075,
0.1,0.125,0.15,0.175,0.2,0.225,0.25,0.275,0.3,0.325,0.35,0.375,0.4,0.425,
0.45,0.475,0.5,0.525,0.55,0.575,0.6,0.625,0.65,0.675,0.7,0.725,0.75,0.775,
0.8,0.825,0.85,0.875,0.9,0.925,0.95,0.975,1.),.UNSPECIFIED.)
GEOMETRIC_REPRESENTATION_ITEM()
RATIONAL_B_SPLINE_SURFACE(((1.,0.996917333733128,1.,0.996917333733128,1.,
0.996917333733128,1.,0.996917333733128,1.,0.996917333733128,1.,0.996917333733128,
1.,0.996917333733128,1.,0.996917333733128,1.,0.996917333733128,1.,0.996917333733128,
1.,0.996917333733128,1.,0.996917333733128,1.,0.996917333733128,1.,0.996917333733128,
1.,0.996917333733128,1.,0.996917333733128,1.,0.996917333733128,1.,0.996917333733128,
1.,0.996917333733128,1.,0.996917333733128,1.,0.996917333733128,1.,0.996917333733128,
1.,0.996917333733128,1.,0.996917333733128,1.,0.996917333733128,1.,0.996917333733128,
1.,0.996917333733128,1.,0.996917333733128,1.,0.996917333733128,1.,0.996917333733128,
1.,0.996917333733128,1.,0.996917333733128,1.,0.996917333733128,1.,0.996917333733128,
1.,0.996917333733128,1.,0.996917333733128,1.,0.996917333733128,1.,0.996917333733128,
1.,0.996917333733128,1.,0.996917333733128,1.),(1.,0.996917333733128,1.,
0.996917333733128,1.,0.996917333733128,1.,0.996917333733128,1.,0.996917333733128,
1.,0.996917333733128,1.,0.996917333733128,1.,0.996917333733128,1.,0.996917333733128,
1.,0.996917333733128,1.,0.996917333733128,1.,0.996917333733128,1.,0.996917333733128,
1.,0.996917333733128,1.,0.996917333733128,1.,0.996917333733128,1.,0.996917333733128,
1.,0.996917333733128,1.,0.996917333733128,1.,0.996917333733128,1.,0.996917333733128,
1.,0.996917333733128,1.,0.996917333733128,1.,0.996917333733128,1.,0.996917333733128,
1.,0.996917333733128,1.,0.996917333733128,1.,0.996917333733128,1.,0.996917333733128,
1.,0.996917333733128,1.,0.996917333733128,1.,0.996917333733128,1.,0.996917333733128,
1.,0.996917333733128,1.,0.996917333733128,1.,0.996917333733128,1.,0.996917333733128,
1.,0.996917333733128,1.,0.996917333733128,1.,0.996917333733128,1.)))
REPRESENTATION_ITEM('')
SURFACE()
);
#4023=(
BOUNDED_SURFACE()
B_SPLINE_SURFACE(1,2,((#266224,#266225,#266226,#266227,#266228,#266229,
#266230,#266231,#266232,#266233,#266234,#266235,#266236,#266237,#266238,
#266239,#266240,#266241,#266242,#266243,#266244,#266245,#266246,#266247,
#266248,#266249,#266250,#266251,#266252,#266253,#266254,#266255,#266256,
#266257,#266258,#266259,#266260,#266261,#266262,#266263,#266264,#266265,
#266266,#266267,#266268,#266269,#266270,#266271,#266272,#266273,#266274,
#266275,#266276,#266277,#266278,#266279,#266280,#266281,#266282,#266283,
#266284,#266285,#266286,#266287,#266288,#266289,#266290,#266291,#266292,
#266293,#266294,#266295,#266296,#266297,#266298,#266299,#266300,#266301,
#266302,#266303,#266304),(#266305,#266306,#266307,#266308,#266309,#266310,
#266311,#266312,#266313,#266314,#266315,#266316,#266317,#266318,#266319,
#266320,#266321,#266322,#266323,#266324,#266325,#266326,#266327,#266328,
#266329,#266330,#266331,#266332,#266333,#266334,#266335,#266336,#266337,
#266338,#266339,#266340,#266341,#266342,#266343,#266344,#266345,#266346,
#266347,#266348,#266349,#266350,#266351,#266352,#266353,#266354,#266355,
#266356,#266357,#266358,#266359,#266360,#266361,#266362,#266363,#266364,
#266365,#266366,#266367,#266368,#266369,#266370,#266371,#266372,#266373,
#266374,#266375,#266376,#266377,#266378,#266379,#266380,#266381,#266382,
#266383,#266384,#266385)),.UNSPECIFIED.,.F.,.F.,.F.)
B_SPLINE_SURFACE_WITH_KNOTS((2,2),(3,2,2,2,2,2,2,2,2,2,2,2,2,2,2,2,2,2,
2,2,2,2,2,2,2,2,2,2,2,2,2,2,2,2,2,2,2,2,2,2,3),(0.,1.),(0.,0.025,0.05,0.075,
0.1,0.125,0.15,0.175,0.2,0.225,0.25,0.275,0.3,0.325,0.35,0.375,0.4,0.425,
0.45,0.475,0.5,0.525,0.55,0.575,0.6,0.625,0.65,0.675,0.7,0.725,0.75,0.775,
0.8,0.825,0.85,0.875,0.9,0.925,0.95,0.975,1.),.UNSPECIFIED.)
GEOMETRIC_REPRESENTATION_ITEM()
RATIONAL_B_SPLINE_SURFACE(((1.,0.996917333733128,1.,0.996917333733128,1.,
0.996917333733128,1.,0.996917333733128,1.,0.996917333733128,1.,0.996917333733128,
1.,0.996917333733128,1.,0.996917333733128,1.,0.996917333733128,1.,0.996917333733128,
1.,0.996917333733128,1.,0.996917333733128,1.,0.996917333733128,1.,0.996917333733128,
1.,0.996917333733128,1.,0.996917333733128,1.,0.996917333733128,1.,0.996917333733128,
1.,0.996917333733128,1.,0.996917333733128,1.,0.996917333733128,1.,0.996917333733128,
1.,0.996917333733128,1.,0.996917333733128,1.,0.996917333733128,1.,0.996917333733128,
1.,0.996917333733128,1.,0.996917333733128,1.,0.996917333733128,1.,0.996917333733128,
1.,0.996917333733128,1.,0.996917333733128,1.,0.996917333733128,1.,0.996917333733128,
1.,0.996917333733128,1.,0.996917333733128,1.,0.996917333733128,1.,0.996917333733128,
1.,0.996917333733128,1.,0.996917333733128,1.),(1.,0.996917333733128,1.,
0.996917333733128,1.,0.996917333733128,1.,0.996917333733128,1.,0.996917333733128,
1.,0.996917333733128,1.,0.996917333733128,1.,0.996917333733128,1.,0.996917333733128,
1.,0.996917333733128,1.,0.996917333733128,1.,0.996917333733128,1.,0.996917333733128,
1.,0.996917333733128,1.,0.996917333733128,1.,0.996917333733128,1.,0.996917333733128,
1.,0.996917333733128,1.,0.996917333733128,1.,0.996917333733128,1.,0.996917333733128,
1.,0.996917333733128,1.,0.996917333733128,1.,0.996917333733128,1.,0.996917333733128,
1.,0.996917333733128,1.,0.996917333733128,1.,0.996917333733128,1.,0.996917333733128,
1.,0.996917333733128,1.,0.996917333733128,1.,0.996917333733128,1.,0.996917333733128,
1.,0.996917333733128,1.,0.996917333733128,1.,0.996917333733128,1.,0.996917333733128,
1.,0.996917333733128,1.,0.996917333733128,1.,0.996917333733128,1.)))
REPRESENTATION_ITEM('')
SURFACE()
);
#4024=(
BOUNDED_SURFACE()
B_SPLINE_SURFACE(1,2,((#266402,#266403,#266404,#266405,#266406,#266407,
#266408,#266409,#266410,#266411,#266412,#266413,#266414,#266415,#266416,
#266417,#266418,#266419,#266420,#266421,#266422,#266423,#266424,#266425,
#266426,#266427,#266428,#266429,#266430,#266431,#266432,#266433,#266434,
#266435,#266436,#266437,#266438,#266439,#266440,#266441,#266442,#266443,
#266444,#266445,#266446,#266447,#266448,#266449,#266450,#266451,#266452,
#266453,#266454,#266455,#266456,#266457,#266458,#266459,#266460,#266461,
#266462,#266463,#266464,#266465,#266466,#266467,#266468,#266469,#266470,
#266471,#266472,#266473,#266474,#266475,#266476,#266477,#266478,#266479,
#266480,#266481,#266482),(#266483,#266484,#266485,#266486,#266487,#266488,
#266489,#266490,#266491,#266492,#266493,#266494,#266495,#266496,#266497,
#266498,#266499,#266500,#266501,#266502,#266503,#266504,#266505,#266506,
#266507,#266508,#266509,#266510,#266511,#266512,#266513,#266514,#266515,
#266516,#266517,#266518,#266519,#266520,#266521,#266522,#266523,#266524,
#266525,#266526,#266527,#266528,#266529,#266530,#266531,#266532,#266533,
#266534,#266535,#266536,#266537,#266538,#266539,#266540,#266541,#266542,
#266543,#266544,#266545,#266546,#266547,#266548,#266549,#266550,#266551,
#266552,#266553,#266554,#266555,#266556,#266557,#266558,#266559,#266560,
#266561,#266562,#266563)),.UNSPECIFIED.,.F.,.F.,.F.)
B_SPLINE_SURFACE_WITH_KNOTS((2,2),(3,2,2,2,2,2,2,2,2,2,2,2,2,2,2,2,2,2,
2,2,2,2,2,2,2,2,2,2,2,2,2,2,2,2,2,2,2,2,2,2,3),(0.,1.),(0.,0.025,0.05,0.075,
0.1,0.125,0.15,0.175,0.2,0.225,0.25,0.275,0.3,0.325,0.35,0.375,0.4,0.425,
0.45,0.475,0.5,0.525,0.55,0.575,0.6,0.625,0.65,0.675,0.7,0.725,0.75,0.775,
0.8,0.825,0.85,0.875,0.9,0.925,0.95,0.975,1.),.UNSPECIFIED.)
GEOMETRIC_REPRESENTATION_ITEM()
RATIONAL_B_SPLINE_SURFACE(((1.,0.996917333733128,1.,0.996917333733128,1.,
0.996917333733128,1.,0.996917333733128,1.,0.996917333733128,1.,0.996917333733128,
1.,0.996917333733128,1.,0.996917333733128,1.,0.996917333733128,1.,0.996917333733128,
1.,0.996917333733128,1.,0.996917333733128,1.,0.996917333733128,1.,0.996917333733128,
1.,0.996917333733128,1.,0.996917333733128,1.,0.996917333733128,1.,0.996917333733128,
1.,0.996917333733128,1.,0.996917333733128,1.,0.996917333733128,1.,0.996917333733128,
1.,0.996917333733128,1.,0.996917333733128,1.,0.996917333733128,1.,0.996917333733128,
1.,0.996917333733128,1.,0.996917333733128,1.,0.996917333733128,1.,0.996917333733128,
1.,0.996917333733128,1.,0.996917333733128,1.,0.996917333733128,1.,0.996917333733128,
1.,0.996917333733128,1.,0.996917333733128,1.,0.996917333733128,1.,0.996917333733128,
1.,0.996917333733128,1.,0.996917333733128,1.),(1.,0.996917333733128,1.,
0.996917333733128,1.,0.996917333733128,1.,0.996917333733128,1.,0.996917333733128,
1.,0.996917333733128,1.,0.996917333733128,1.,0.996917333733128,1.,0.996917333733128,
1.,0.996917333733128,1.,0.996917333733128,1.,0.996917333733128,1.,0.996917333733128,
1.,0.996917333733128,1.,0.996917333733128,1.,0.996917333733128,1.,0.996917333733128,
1.,0.996917333733128,1.,0.996917333733128,1.,0.996917333733128,1.,0.996917333733128,
1.,0.996917333733128,1.,0.996917333733128,1.,0.996917333733128,1.,0.996917333733128,
1.,0.996917333733128,1.,0.996917333733128,1.,0.996917333733128,1.,0.996917333733128,
1.,0.996917333733128,1.,0.996917333733128,1.,0.996917333733128,1.,0.996917333733128,
1.,0.996917333733128,1.,0.996917333733128,1.,0.996917333733128,1.,0.996917333733128,
1.,0.996917333733128,1.,0.996917333733128,1.,0.996917333733128,1.)))
REPRESENTATION_ITEM('')
SURFACE()
);
#4025=(
BOUNDED_SURFACE()
B_SPLINE_SURFACE(1,2,((#267127,#267128,#267129,#267130,#267131,#267132,
#267133,#267134,#267135,#267136,#267137,#267138,#267139,#267140,#267141,
#267142,#267143,#267144,#267145,#267146,#267147,#267148,#267149,#267150,
#267151,#267152,#267153,#267154,#267155,#267156,#267157,#267158,#267159,
#267160,#267161,#267162,#267163,#267164,#267165,#267166,#267167,#267168,
#267169,#267170,#267171,#267172,#267173,#267174,#267175,#267176,#267177,
#267178,#267179,#267180,#267181,#267182,#267183,#267184,#267185,#267186,
#267187,#267188,#267189,#267190,#267191,#267192,#267193,#267194,#267195,
#267196,#267197,#267198,#267199,#267200,#267201,#267202,#267203,#267204,
#267205,#267206,#267207),(#267208,#267209,#267210,#267211,#267212,#267213,
#267214,#267215,#267216,#267217,#267218,#267219,#267220,#267221,#267222,
#267223,#267224,#267225,#267226,#267227,#267228,#267229,#267230,#267231,
#267232,#267233,#267234,#267235,#267236,#267237,#267238,#267239,#267240,
#267241,#267242,#267243,#267244,#267245,#267246,#267247,#267248,#267249,
#267250,#267251,#267252,#267253,#267254,#267255,#267256,#267257,#267258,
#267259,#267260,#267261,#267262,#267263,#267264,#267265,#267266,#267267,
#267268,#267269,#267270,#267271,#267272,#267273,#267274,#267275,#267276,
#267277,#267278,#267279,#267280,#267281,#267282,#267283,#267284,#267285,
#267286,#267287,#267288)),.UNSPECIFIED.,.F.,.F.,.F.)
B_SPLINE_SURFACE_WITH_KNOTS((2,2),(3,2,2,2,2,2,2,2,2,2,2,2,2,2,2,2,2,2,
2,2,2,2,2,2,2,2,2,2,2,2,2,2,2,2,2,2,2,2,2,2,3),(0.,1.),(0.,0.025,0.05,0.075,
0.1,0.125,0.15,0.175,0.2,0.225,0.25,0.275,0.3,0.325,0.35,0.375,0.4,0.425,
0.45,0.475,0.5,0.525,0.55,0.575,0.6,0.625,0.65,0.675,0.7,0.725,0.75,0.775,
0.8,0.825,0.85,0.875,0.9,0.925,0.95,0.975,1.),.UNSPECIFIED.)
GEOMETRIC_REPRESENTATION_ITEM()
RATIONAL_B_SPLINE_SURFACE(((1.,0.996917333733128,1.,0.996917333733128,1.,
0.996917333733128,1.,0.996917333733128,1.,0.996917333733128,1.,0.996917333733128,
1.,0.996917333733128,1.,0.996917333733128,1.,0.996917333733128,1.,0.996917333733128,
1.,0.996917333733128,1.,0.996917333733128,1.,0.996917333733128,1.,0.996917333733128,
1.,0.996917333733128,1.,0.996917333733128,1.,0.996917333733128,1.,0.996917333733128,
1.,0.996917333733128,1.,0.996917333733128,1.,0.996917333733128,1.,0.996917333733128,
1.,0.996917333733128,1.,0.996917333733128,1.,0.996917333733128,1.,0.996917333733128,
1.,0.996917333733128,1.,0.996917333733128,1.,0.996917333733128,1.,0.996917333733128,
1.,0.996917333733128,1.,0.996917333733128,1.,0.996917333733128,1.,0.996917333733128,
1.,0.996917333733128,1.,0.996917333733128,1.,0.996917333733128,1.,0.996917333733128,
1.,0.996917333733128,1.,0.996917333733128,1.),(1.,0.996917333733128,1.,
0.996917333733128,1.,0.996917333733128,1.,0.996917333733128,1.,0.996917333733128,
1.,0.996917333733128,1.,0.996917333733128,1.,0.996917333733128,1.,0.996917333733128,
1.,0.996917333733128,1.,0.996917333733128,1.,0.996917333733128,1.,0.996917333733128,
1.,0.996917333733128,1.,0.996917333733128,1.,0.996917333733128,1.,0.996917333733128,
1.,0.996917333733128,1.,0.996917333733128,1.,0.996917333733128,1.,0.996917333733128,
1.,0.996917333733128,1.,0.996917333733128,1.,0.996917333733128,1.,0.996917333733128,
1.,0.996917333733128,1.,0.996917333733128,1.,0.996917333733128,1.,0.996917333733128,
1.,0.996917333733128,1.,0.996917333733128,1.,0.996917333733128,1.,0.996917333733128,
1.,0.996917333733128,1.,0.996917333733128,1.,0.996917333733128,1.,0.996917333733128,
1.,0.996917333733128,1.,0.996917333733128,1.,0.996917333733128,1.)))
REPRESENTATION_ITEM('')
SURFACE()
);
#4026=(
BOUNDED_SURFACE()
B_SPLINE_SURFACE(1,2,((#267451,#267452,#267453,#267454,#267455,#267456,
#267457,#267458,#267459,#267460,#267461,#267462,#267463,#267464,#267465,
#267466,#267467,#267468,#267469,#267470,#267471,#267472,#267473,#267474,
#267475,#267476,#267477,#267478,#267479,#267480,#267481,#267482,#267483,
#267484,#267485,#267486,#267487,#267488,#267489,#267490,#267491,#267492,
#267493,#267494,#267495,#267496,#267497,#267498,#267499,#267500,#267501,
#267502,#267503,#267504,#267505,#267506,#267507,#267508,#267509,#267510,
#267511,#267512,#267513,#267514,#267515,#267516,#267517,#267518,#267519,
#267520,#267521,#267522,#267523,#267524,#267525,#267526,#267527,#267528,
#267529,#267530,#267531),(#267532,#267533,#267534,#267535,#267536,#267537,
#267538,#267539,#267540,#267541,#267542,#267543,#267544,#267545,#267546,
#267547,#267548,#267549,#267550,#267551,#267552,#267553,#267554,#267555,
#267556,#267557,#267558,#267559,#267560,#267561,#267562,#267563,#267564,
#267565,#267566,#267567,#267568,#267569,#267570,#267571,#267572,#267573,
#267574,#267575,#267576,#267577,#267578,#267579,#267580,#267581,#267582,
#267583,#267584,#267585,#267586,#267587,#267588,#267589,#267590,#267591,
#267592,#267593,#267594,#267595,#267596,#267597,#267598,#267599,#267600,
#267601,#267602,#267603,#267604,#267605,#267606,#267607,#267608,#267609,
#267610,#267611,#267612)),.UNSPECIFIED.,.F.,.F.,.F.)
B_SPLINE_SURFACE_WITH_KNOTS((2,2),(3,2,2,2,2,2,2,2,2,2,2,2,2,2,2,2,2,2,
2,2,2,2,2,2,2,2,2,2,2,2,2,2,2,2,2,2,2,2,2,2,3),(0.,1.),(0.,0.025,0.05,0.075,
0.1,0.125,0.15,0.175,0.2,0.225,0.25,0.275,0.3,0.325,0.35,0.375,0.4,0.425,
0.45,0.475,0.5,0.525,0.55,0.575,0.6,0.625,0.65,0.675,0.7,0.725,0.75,0.775,
0.8,0.825,0.85,0.875,0.9,0.925,0.95,0.975,1.),.UNSPECIFIED.)
GEOMETRIC_REPRESENTATION_ITEM()
RATIONAL_B_SPLINE_SURFACE(((1.,0.996917333733128,1.,0.996917333733128,1.,
0.996917333733128,1.,0.996917333733128,1.,0.996917333733128,1.,0.996917333733128,
1.,0.996917333733128,1.,0.996917333733128,1.,0.996917333733128,1.,0.996917333733128,
1.,0.996917333733128,1.,0.996917333733128,1.,0.996917333733128,1.,0.996917333733128,
1.,0.996917333733128,1.,0.996917333733128,1.,0.996917333733128,1.,0.996917333733128,
1.,0.996917333733128,1.,0.996917333733128,1.,0.996917333733128,1.,0.996917333733128,
1.,0.996917333733128,1.,0.996917333733128,1.,0.996917333733128,1.,0.996917333733128,
1.,0.996917333733128,1.,0.996917333733128,1.,0.996917333733128,1.,0.996917333733128,
1.,0.996917333733128,1.,0.996917333733128,1.,0.996917333733128,1.,0.996917333733128,
1.,0.996917333733128,1.,0.996917333733128,1.,0.996917333733128,1.,0.996917333733128,
1.,0.996917333733128,1.,0.996917333733128,1.),(1.,0.996917333733128,1.,
0.996917333733128,1.,0.996917333733128,1.,0.996917333733128,1.,0.996917333733128,
1.,0.996917333733128,1.,0.996917333733128,1.,0.996917333733128,1.,0.996917333733128,
1.,0.996917333733128,1.,0.996917333733128,1.,0.996917333733128,1.,0.996917333733128,
1.,0.996917333733128,1.,0.996917333733128,1.,0.996917333733128,1.,0.996917333733128,
1.,0.996917333733128,1.,0.996917333733128,1.,0.996917333733128,1.,0.996917333733128,
1.,0.996917333733128,1.,0.996917333733128,1.,0.996917333733128,1.,0.996917333733128,
1.,0.996917333733128,1.,0.996917333733128,1.,0.996917333733128,1.,0.996917333733128,
1.,0.996917333733128,1.,0.996917333733128,1.,0.996917333733128,1.,0.996917333733128,
1.,0.996917333733128,1.,0.996917333733128,1.,0.996917333733128,1.,0.996917333733128,
1.,0.996917333733128,1.,0.996917333733128,1.,0.996917333733128,1.)))
REPRESENTATION_ITEM('')
SURFACE()
);
#4027=(
BOUNDED_SURFACE()
B_SPLINE_SURFACE(1,2,((#267694,#267695,#267696,#267697,#267698,#267699,
#267700,#267701,#267702,#267703,#267704,#267705,#267706,#267707,#267708,
#267709,#267710,#267711,#267712,#267713,#267714,#267715,#267716,#267717,
#267718,#267719,#267720,#267721,#267722,#267723,#267724,#267725,#267726,
#267727,#267728,#267729,#267730,#267731,#267732,#267733,#267734,#267735,
#267736,#267737,#267738,#267739,#267740,#267741,#267742,#267743,#267744,
#267745,#267746,#267747,#267748,#267749,#267750,#267751,#267752,#267753,
#267754,#267755,#267756,#267757,#267758,#267759,#267760,#267761,#267762,
#267763,#267764,#267765,#267766,#267767,#267768,#267769,#267770,#267771,
#267772,#267773,#267774),(#267775,#267776,#267777,#267778,#267779,#267780,
#267781,#267782,#267783,#267784,#267785,#267786,#267787,#267788,#267789,
#267790,#267791,#267792,#267793,#267794,#267795,#267796,#267797,#267798,
#267799,#267800,#267801,#267802,#267803,#267804,#267805,#267806,#267807,
#267808,#267809,#267810,#267811,#267812,#267813,#267814,#267815,#267816,
#267817,#267818,#267819,#267820,#267821,#267822,#267823,#267824,#267825,
#267826,#267827,#267828,#267829,#267830,#267831,#267832,#267833,#267834,
#267835,#267836,#267837,#267838,#267839,#267840,#267841,#267842,#267843,
#267844,#267845,#267846,#267847,#267848,#267849,#267850,#267851,#267852,
#267853,#267854,#267855)),.UNSPECIFIED.,.F.,.F.,.F.)
B_SPLINE_SURFACE_WITH_KNOTS((2,2),(3,2,2,2,2,2,2,2,2,2,2,2,2,2,2,2,2,2,
2,2,2,2,2,2,2,2,2,2,2,2,2,2,2,2,2,2,2,2,2,2,3),(0.,1.),(0.,0.025,0.05,0.075,
0.1,0.125,0.15,0.175,0.2,0.225,0.25,0.275,0.3,0.325,0.35,0.375,0.4,0.425,
0.45,0.475,0.5,0.525,0.55,0.575,0.6,0.625,0.65,0.675,0.7,0.725,0.75,0.775,
0.8,0.825,0.85,0.875,0.9,0.925,0.95,0.975,1.),.UNSPECIFIED.)
GEOMETRIC_REPRESENTATION_ITEM()
RATIONAL_B_SPLINE_SURFACE(((1.,0.996917333733128,1.,0.996917333733128,1.,
0.996917333733128,1.,0.996917333733128,1.,0.996917333733128,1.,0.996917333733128,
1.,0.996917333733128,1.,0.996917333733128,1.,0.996917333733128,1.,0.996917333733128,
1.,0.996917333733128,1.,0.996917333733128,1.,0.996917333733128,1.,0.996917333733128,
1.,0.996917333733128,1.,0.996917333733128,1.,0.996917333733128,1.,0.996917333733128,
1.,0.996917333733128,1.,0.996917333733128,1.,0.996917333733128,1.,0.996917333733128,
1.,0.996917333733128,1.,0.996917333733128,1.,0.996917333733128,1.,0.996917333733128,
1.,0.996917333733128,1.,0.996917333733128,1.,0.996917333733128,1.,0.996917333733128,
1.,0.996917333733128,1.,0.996917333733128,1.,0.996917333733128,1.,0.996917333733128,
1.,0.996917333733128,1.,0.996917333733128,1.,0.996917333733128,1.,0.996917333733128,
1.,0.996917333733128,1.,0.996917333733128,1.),(1.,0.996917333733128,1.,
0.996917333733128,1.,0.996917333733128,1.,0.996917333733128,1.,0.996917333733128,
1.,0.996917333733128,1.,0.996917333733128,1.,0.996917333733128,1.,0.996917333733128,
1.,0.996917333733128,1.,0.996917333733128,1.,0.996917333733128,1.,0.996917333733128,
1.,0.996917333733128,1.,0.996917333733128,1.,0.996917333733128,1.,0.996917333733128,
1.,0.996917333733128,1.,0.996917333733128,1.,0.996917333733128,1.,0.996917333733128,
1.,0.996917333733128,1.,0.996917333733128,1.,0.996917333733128,1.,0.996917333733128,
1.,0.996917333733128,1.,0.996917333733128,1.,0.996917333733128,1.,0.996917333733128,
1.,0.996917333733128,1.,0.996917333733128,1.,0.996917333733128,1.,0.996917333733128,
1.,0.996917333733128,1.,0.996917333733128,1.,0.996917333733128,1.,0.996917333733128,
1.,0.996917333733128,1.,0.996917333733128,1.,0.996917333733128,1.)))
REPRESENTATION_ITEM('')
SURFACE()
);
#4028=(
BOUNDED_SURFACE()
B_SPLINE_SURFACE(1,2,((#267937,#267938,#267939,#267940,#267941,#267942,
#267943,#267944,#267945,#267946,#267947,#267948,#267949,#267950,#267951,
#267952,#267953,#267954,#267955,#267956,#267957,#267958,#267959,#267960,
#267961,#267962,#267963,#267964,#267965,#267966,#267967,#267968,#267969,
#267970,#267971,#267972,#267973,#267974,#267975,#267976,#267977,#267978,
#267979,#267980,#267981,#267982,#267983,#267984,#267985,#267986,#267987,
#267988,#267989,#267990,#267991,#267992,#267993,#267994,#267995,#267996,
#267997,#267998,#267999,#268000,#268001,#268002,#268003,#268004,#268005,
#268006,#268007,#268008,#268009,#268010,#268011,#268012,#268013,#268014,
#268015,#268016,#268017),(#268018,#268019,#268020,#268021,#268022,#268023,
#268024,#268025,#268026,#268027,#268028,#268029,#268030,#268031,#268032,
#268033,#268034,#268035,#268036,#268037,#268038,#268039,#268040,#268041,
#268042,#268043,#268044,#268045,#268046,#268047,#268048,#268049,#268050,
#268051,#268052,#268053,#268054,#268055,#268056,#268057,#268058,#268059,
#268060,#268061,#268062,#268063,#268064,#268065,#268066,#268067,#268068,
#268069,#268070,#268071,#268072,#268073,#268074,#268075,#268076,#268077,
#268078,#268079,#268080,#268081,#268082,#268083,#268084,#268085,#268086,
#268087,#268088,#268089,#268090,#268091,#268092,#268093,#268094,#268095,
#268096,#268097,#268098)),.UNSPECIFIED.,.F.,.F.,.F.)
B_SPLINE_SURFACE_WITH_KNOTS((2,2),(3,2,2,2,2,2,2,2,2,2,2,2,2,2,2,2,2,2,
2,2,2,2,2,2,2,2,2,2,2,2,2,2,2,2,2,2,2,2,2,2,3),(0.,1.),(0.,0.025,0.05,0.075,
0.1,0.125,0.15,0.175,0.2,0.225,0.25,0.275,0.3,0.325,0.35,0.375,0.4,0.425,
0.45,0.475,0.5,0.525,0.55,0.575,0.6,0.625,0.65,0.675,0.7,0.725,0.75,0.775,
0.8,0.825,0.85,0.875,0.9,0.925,0.95,0.975,1.),.UNSPECIFIED.)
GEOMETRIC_REPRESENTATION_ITEM()
RATIONAL_B_SPLINE_SURFACE(((1.,0.996917333733128,1.,0.996917333733128,1.,
0.996917333733128,1.,0.996917333733128,1.,0.996917333733128,1.,0.996917333733128,
1.,0.996917333733128,1.,0.996917333733128,1.,0.996917333733128,1.,0.996917333733128,
1.,0.996917333733128,1.,0.996917333733128,1.,0.996917333733128,1.,0.996917333733128,
1.,0.996917333733128,1.,0.996917333733128,1.,0.996917333733128,1.,0.996917333733128,
1.,0.996917333733128,1.,0.996917333733128,1.,0.996917333733128,1.,0.996917333733128,
1.,0.996917333733128,1.,0.996917333733128,1.,0.996917333733128,1.,0.996917333733128,
1.,0.996917333733128,1.,0.996917333733128,1.,0.996917333733128,1.,0.996917333733128,
1.,0.996917333733128,1.,0.996917333733128,1.,0.996917333733128,1.,0.996917333733128,
1.,0.996917333733128,1.,0.996917333733128,1.,0.996917333733128,1.,0.996917333733128,
1.,0.996917333733128,1.,0.996917333733128,1.),(1.,0.996917333733128,1.,
0.996917333733128,1.,0.996917333733128,1.,0.996917333733128,1.,0.996917333733128,
1.,0.996917333733128,1.,0.996917333733128,1.,0.996917333733128,1.,0.996917333733128,
1.,0.996917333733128,1.,0.996917333733128,1.,0.996917333733128,1.,0.996917333733128,
1.,0.996917333733128,1.,0.996917333733128,1.,0.996917333733128,1.,0.996917333733128,
1.,0.996917333733128,1.,0.996917333733128,1.,0.996917333733128,1.,0.996917333733128,
1.,0.996917333733128,1.,0.996917333733128,1.,0.996917333733128,1.,0.996917333733128,
1.,0.996917333733128,1.,0.996917333733128,1.,0.996917333733128,1.,0.996917333733128,
1.,0.996917333733128,1.,0.996917333733128,1.,0.996917333733128,1.,0.996917333733128,
1.,0.996917333733128,1.,0.996917333733128,1.,0.996917333733128,1.,0.996917333733128,
1.,0.996917333733128,1.,0.996917333733128,1.,0.996917333733128,1.)))
REPRESENTATION_ITEM('')
SURFACE()
);
#4029=(
BOUNDED_SURFACE()
B_SPLINE_SURFACE(1,2,((#268129,#268130,#268131,#268132,#268133,#268134,
#268135,#268136,#268137,#268138,#268139,#268140,#268141,#268142,#268143,
#268144,#268145,#268146,#268147,#268148,#268149,#268150,#268151,#268152,
#268153,#268154,#268155,#268156,#268157,#268158,#268159,#268160,#268161,
#268162,#268163,#268164,#268165,#268166,#268167,#268168,#268169,#268170,
#268171,#268172,#268173,#268174,#268175,#268176,#268177,#268178,#268179,
#268180,#268181,#268182,#268183,#268184,#268185,#268186,#268187,#268188,
#268189,#268190,#268191,#268192,#268193,#268194,#268195,#268196,#268197,
#268198,#268199,#268200,#268201,#268202,#268203,#268204,#268205,#268206,
#268207,#268208,#268209),(#268210,#268211,#268212,#268213,#268214,#268215,
#268216,#268217,#268218,#268219,#268220,#268221,#268222,#268223,#268224,
#268225,#268226,#268227,#268228,#268229,#268230,#268231,#268232,#268233,
#268234,#268235,#268236,#268237,#268238,#268239,#268240,#268241,#268242,
#268243,#268244,#268245,#268246,#268247,#268248,#268249,#268250,#268251,
#268252,#268253,#268254,#268255,#268256,#268257,#268258,#268259,#268260,
#268261,#268262,#268263,#268264,#268265,#268266,#268267,#268268,#268269,
#268270,#268271,#268272,#268273,#268274,#268275,#268276,#268277,#268278,
#268279,#268280,#268281,#268282,#268283,#268284,#268285,#268286,#268287,
#268288,#268289,#268290)),.UNSPECIFIED.,.F.,.F.,.F.)
B_SPLINE_SURFACE_WITH_KNOTS((2,2),(3,2,2,2,2,2,2,2,2,2,2,2,2,2,2,2,2,2,
2,2,2,2,2,2,2,2,2,2,2,2,2,2,2,2,2,2,2,2,2,2,3),(0.,1.),(0.,0.025,0.05,0.075,
0.1,0.125,0.15,0.175,0.2,0.225,0.25,0.275,0.3,0.325,0.35,0.375,0.4,0.425,
0.45,0.475,0.5,0.525,0.55,0.575,0.6,0.625,0.65,0.675,0.7,0.725,0.75,0.775,
0.8,0.825,0.85,0.875,0.9,0.925,0.95,0.975,1.),.UNSPECIFIED.)
GEOMETRIC_REPRESENTATION_ITEM()
RATIONAL_B_SPLINE_SURFACE(((1.,0.996917333733128,1.,0.996917333733128,1.,
0.996917333733128,1.,0.996917333733128,1.,0.996917333733128,1.,0.996917333733128,
1.,0.996917333733128,1.,0.996917333733128,1.,0.996917333733128,1.,0.996917333733128,
1.,0.996917333733128,1.,0.996917333733128,1.,0.996917333733128,1.,0.996917333733128,
1.,0.996917333733128,1.,0.996917333733128,1.,0.996917333733128,1.,0.996917333733128,
1.,0.996917333733128,1.,0.996917333733128,1.,0.996917333733128,1.,0.996917333733128,
1.,0.996917333733128,1.,0.996917333733128,1.,0.996917333733128,1.,0.996917333733128,
1.,0.996917333733128,1.,0.996917333733128,1.,0.996917333733128,1.,0.996917333733128,
1.,0.996917333733128,1.,0.996917333733128,1.,0.996917333733128,1.,0.996917333733128,
1.,0.996917333733128,1.,0.996917333733128,1.,0.996917333733128,1.,0.996917333733128,
1.,0.996917333733128,1.,0.996917333733128,1.),(1.,0.996917333733128,1.,
0.996917333733128,1.,0.996917333733128,1.,0.996917333733128,1.,0.996917333733128,
1.,0.996917333733128,1.,0.996917333733128,1.,0.996917333733128,1.,0.996917333733128,
1.,0.996917333733128,1.,0.996917333733128,1.,0.996917333733128,1.,0.996917333733128,
1.,0.996917333733128,1.,0.996917333733128,1.,0.996917333733128,1.,0.996917333733128,
1.,0.996917333733128,1.,0.996917333733128,1.,0.996917333733128,1.,0.996917333733128,
1.,0.996917333733128,1.,0.996917333733128,1.,0.996917333733128,1.,0.996917333733128,
1.,0.996917333733128,1.,0.996917333733128,1.,0.996917333733128,1.,0.996917333733128,
1.,0.996917333733128,1.,0.996917333733128,1.,0.996917333733128,1.,0.996917333733128,
1.,0.996917333733128,1.,0.996917333733128,1.,0.996917333733128,1.,0.996917333733128,
1.,0.996917333733128,1.,0.996917333733128,1.,0.996917333733128,1.)))
REPRESENTATION_ITEM('')
SURFACE()
);
#4030=(
BOUNDED_SURFACE()
B_SPLINE_SURFACE(1,2,((#268292,#268293,#268294,#268295,#268296,#268297,
#268298,#268299,#268300,#268301,#268302,#268303,#268304,#268305,#268306,
#268307,#268308,#268309,#268310,#268311,#268312,#268313,#268314,#268315,
#268316,#268317,#268318,#268319,#268320,#268321,#268322,#268323,#268324,
#268325,#268326,#268327,#268328,#268329,#268330,#268331,#268332,#268333,
#268334,#268335,#268336,#268337,#268338,#268339,#268340,#268341,#268342,
#268343,#268344,#268345,#268346,#268347,#268348,#268349,#268350,#268351,
#268352,#268353,#268354,#268355,#268356,#268357,#268358,#268359,#268360,
#268361,#268362,#268363,#268364,#268365,#268366,#268367,#268368,#268369,
#268370,#268371,#268372),(#268373,#268374,#268375,#268376,#268377,#268378,
#268379,#268380,#268381,#268382,#268383,#268384,#268385,#268386,#268387,
#268388,#268389,#268390,#268391,#268392,#268393,#268394,#268395,#268396,
#268397,#268398,#268399,#268400,#268401,#268402,#268403,#268404,#268405,
#268406,#268407,#268408,#268409,#268410,#268411,#268412,#268413,#268414,
#268415,#268416,#268417,#268418,#268419,#268420,#268421,#268422,#268423,
#268424,#268425,#268426,#268427,#268428,#268429,#268430,#268431,#268432,
#268433,#268434,#268435,#268436,#268437,#268438,#268439,#268440,#268441,
#268442,#268443,#268444,#268445,#268446,#268447,#268448,#268449,#268450,
#268451,#268452,#268453)),.UNSPECIFIED.,.F.,.F.,.F.)
B_SPLINE_SURFACE_WITH_KNOTS((2,2),(3,2,2,2,2,2,2,2,2,2,2,2,2,2,2,2,2,2,
2,2,2,2,2,2,2,2,2,2,2,2,2,2,2,2,2,2,2,2,2,2,3),(0.,1.),(0.,0.025,0.05,0.075,
0.1,0.125,0.15,0.175,0.2,0.225,0.25,0.275,0.3,0.325,0.35,0.375,0.4,0.425,
0.45,0.475,0.5,0.525,0.55,0.575,0.6,0.625,0.65,0.675,0.7,0.725,0.75,0.775,
0.8,0.825,0.85,0.875,0.9,0.925,0.95,0.975,1.),.UNSPECIFIED.)
GEOMETRIC_REPRESENTATION_ITEM()
RATIONAL_B_SPLINE_SURFACE(((1.,0.996917333733128,1.,0.996917333733128,1.,
0.996917333733128,1.,0.996917333733128,1.,0.996917333733128,1.,0.996917333733128,
1.,0.996917333733128,1.,0.996917333733128,1.,0.996917333733128,1.,0.996917333733128,
1.,0.996917333733128,1.,0.996917333733128,1.,0.996917333733128,1.,0.996917333733128,
1.,0.996917333733128,1.,0.996917333733128,1.,0.996917333733128,1.,0.996917333733128,
1.,0.996917333733128,1.,0.996917333733128,1.,0.996917333733128,1.,0.996917333733128,
1.,0.996917333733128,1.,0.996917333733128,1.,0.996917333733128,1.,0.996917333733128,
1.,0.996917333733128,1.,0.996917333733128,1.,0.996917333733128,1.,0.996917333733128,
1.,0.996917333733128,1.,0.996917333733128,1.,0.996917333733128,1.,0.996917333733128,
1.,0.996917333733128,1.,0.996917333733128,1.,0.996917333733128,1.,0.996917333733128,
1.,0.996917333733128,1.,0.996917333733128,1.),(1.,0.996917333733128,1.,
0.996917333733128,1.,0.996917333733128,1.,0.996917333733128,1.,0.996917333733128,
1.,0.996917333733128,1.,0.996917333733128,1.,0.996917333733128,1.,0.996917333733128,
1.,0.996917333733128,1.,0.996917333733128,1.,0.996917333733128,1.,0.996917333733128,
1.,0.996917333733128,1.,0.996917333733128,1.,0.996917333733128,1.,0.996917333733128,
1.,0.996917333733128,1.,0.996917333733128,1.,0.996917333733128,1.,0.996917333733128,
1.,0.996917333733128,1.,0.996917333733128,1.,0.996917333733128,1.,0.996917333733128,
1.,0.996917333733128,1.,0.996917333733128,1.,0.996917333733128,1.,0.996917333733128,
1.,0.996917333733128,1.,0.996917333733128,1.,0.996917333733128,1.,0.996917333733128,
1.,0.996917333733128,1.,0.996917333733128,1.,0.996917333733128,1.,0.996917333733128,
1.,0.996917333733128,1.,0.996917333733128,1.,0.996917333733128,1.)))
REPRESENTATION_ITEM('')
SURFACE()
);
#4031=(
BOUNDED_SURFACE()
B_SPLINE_SURFACE(1,2,((#268454,#268455,#268456,#268457,#268458,#268459,
#268460,#268461,#268462,#268463,#268464,#268465,#268466,#268467,#268468,
#268469,#268470,#268471,#268472,#268473,#268474,#268475,#268476,#268477,
#268478,#268479,#268480,#268481,#268482,#268483,#268484,#268485,#268486,
#268487,#268488,#268489,#268490,#268491,#268492,#268493,#268494,#268495,
#268496,#268497,#268498,#268499,#268500,#268501,#268502,#268503,#268504,
#268505,#268506,#268507,#268508,#268509,#268510,#268511,#268512,#268513,
#268514,#268515,#268516,#268517,#268518,#268519,#268520,#268521,#268522,
#268523,#268524,#268525,#268526,#268527,#268528,#268529,#268530,#268531,
#268532,#268533,#268534),(#268535,#268536,#268537,#268538,#268539,#268540,
#268541,#268542,#268543,#268544,#268545,#268546,#268547,#268548,#268549,
#268550,#268551,#268552,#268553,#268554,#268555,#268556,#268557,#268558,
#268559,#268560,#268561,#268562,#268563,#268564,#268565,#268566,#268567,
#268568,#268569,#268570,#268571,#268572,#268573,#268574,#268575,#268576,
#268577,#268578,#268579,#268580,#268581,#268582,#268583,#268584,#268585,
#268586,#268587,#268588,#268589,#268590,#268591,#268592,#268593,#268594,
#268595,#268596,#268597,#268598,#268599,#268600,#268601,#268602,#268603,
#268604,#268605,#268606,#268607,#268608,#268609,#268610,#268611,#268612,
#268613,#268614,#268615)),.UNSPECIFIED.,.F.,.F.,.F.)
B_SPLINE_SURFACE_WITH_KNOTS((2,2),(3,2,2,2,2,2,2,2,2,2,2,2,2,2,2,2,2,2,
2,2,2,2,2,2,2,2,2,2,2,2,2,2,2,2,2,2,2,2,2,2,3),(0.,1.),(0.,0.025,0.05,0.075,
0.1,0.125,0.15,0.175,0.2,0.225,0.25,0.275,0.3,0.325,0.35,0.375,0.4,0.425,
0.45,0.475,0.5,0.525,0.55,0.575,0.6,0.625,0.65,0.675,0.7,0.725,0.75,0.775,
0.8,0.825,0.85,0.875,0.9,0.925,0.95,0.975,1.),.UNSPECIFIED.)
GEOMETRIC_REPRESENTATION_ITEM()
RATIONAL_B_SPLINE_SURFACE(((1.,0.996917333733128,1.,0.996917333733128,1.,
0.996917333733128,1.,0.996917333733128,1.,0.996917333733128,1.,0.996917333733128,
1.,0.996917333733128,1.,0.996917333733128,1.,0.996917333733128,1.,0.996917333733128,
1.,0.996917333733128,1.,0.996917333733128,1.,0.996917333733128,1.,0.996917333733128,
1.,0.996917333733128,1.,0.996917333733128,1.,0.996917333733128,1.,0.996917333733128,
1.,0.996917333733128,1.,0.996917333733128,1.,0.996917333733128,1.,0.996917333733128,
1.,0.996917333733128,1.,0.996917333733128,1.,0.996917333733128,1.,0.996917333733128,
1.,0.996917333733128,1.,0.996917333733128,1.,0.996917333733128,1.,0.996917333733128,
1.,0.996917333733128,1.,0.996917333733128,1.,0.996917333733128,1.,0.996917333733128,
1.,0.996917333733128,1.,0.996917333733128,1.,0.996917333733128,1.,0.996917333733128,
1.,0.996917333733128,1.,0.996917333733128,1.),(1.,0.996917333733128,1.,
0.996917333733128,1.,0.996917333733128,1.,0.996917333733128,1.,0.996917333733128,
1.,0.996917333733128,1.,0.996917333733128,1.,0.996917333733128,1.,0.996917333733128,
1.,0.996917333733128,1.,0.996917333733128,1.,0.996917333733128,1.,0.996917333733128,
1.,0.996917333733128,1.,0.996917333733128,1.,0.996917333733128,1.,0.996917333733128,
1.,0.996917333733128,1.,0.996917333733128,1.,0.996917333733128,1.,0.996917333733128,
1.,0.996917333733128,1.,0.996917333733128,1.,0.996917333733128,1.,0.996917333733128,
1.,0.996917333733128,1.,0.996917333733128,1.,0.996917333733128,1.,0.996917333733128,
1.,0.996917333733128,1.,0.996917333733128,1.,0.996917333733128,1.,0.996917333733128,
1.,0.996917333733128,1.,0.996917333733128,1.,0.996917333733128,1.,0.996917333733128,
1.,0.996917333733128,1.,0.996917333733128,1.,0.996917333733128,1.)))
REPRESENTATION_ITEM('')
SURFACE()
);
#4032=(
BOUNDED_SURFACE()
B_SPLINE_SURFACE(1,2,((#268617,#268618,#268619,#268620,#268621,#268622,
#268623,#268624,#268625,#268626,#268627,#268628,#268629,#268630,#268631,
#268632,#268633,#268634,#268635,#268636,#268637,#268638,#268639,#268640,
#268641,#268642,#268643,#268644,#268645,#268646,#268647,#268648,#268649,
#268650,#268651,#268652,#268653,#268654,#268655,#268656,#268657,#268658,
#268659,#268660,#268661,#268662,#268663,#268664,#268665,#268666,#268667,
#268668,#268669,#268670,#268671,#268672,#268673,#268674,#268675,#268676,
#268677,#268678,#268679,#268680,#268681,#268682,#268683,#268684,#268685,
#268686,#268687,#268688,#268689,#268690,#268691,#268692,#268693,#268694,
#268695,#268696,#268697),(#268698,#268699,#268700,#268701,#268702,#268703,
#268704,#268705,#268706,#268707,#268708,#268709,#268710,#268711,#268712,
#268713,#268714,#268715,#268716,#268717,#268718,#268719,#268720,#268721,
#268722,#268723,#268724,#268725,#268726,#268727,#268728,#268729,#268730,
#268731,#268732,#268733,#268734,#268735,#268736,#268737,#268738,#268739,
#268740,#268741,#268742,#268743,#268744,#268745,#268746,#268747,#268748,
#268749,#268750,#268751,#268752,#268753,#268754,#268755,#268756,#268757,
#268758,#268759,#268760,#268761,#268762,#268763,#268764,#268765,#268766,
#268767,#268768,#268769,#268770,#268771,#268772,#268773,#268774,#268775,
#268776,#268777,#268778)),.UNSPECIFIED.,.F.,.F.,.F.)
B_SPLINE_SURFACE_WITH_KNOTS((2,2),(3,2,2,2,2,2,2,2,2,2,2,2,2,2,2,2,2,2,
2,2,2,2,2,2,2,2,2,2,2,2,2,2,2,2,2,2,2,2,2,2,3),(0.,1.),(0.,0.025,0.05,0.075,
0.1,0.125,0.15,0.175,0.2,0.225,0.25,0.275,0.3,0.325,0.35,0.375,0.4,0.425,
0.45,0.475,0.5,0.525,0.55,0.575,0.6,0.625,0.65,0.675,0.7,0.725,0.75,0.775,
0.8,0.825,0.85,0.875,0.9,0.925,0.95,0.975,1.),.UNSPECIFIED.)
GEOMETRIC_REPRESENTATION_ITEM()
RATIONAL_B_SPLINE_SURFACE(((1.,0.996917333733128,1.,0.996917333733128,1.,
0.996917333733128,1.,0.996917333733128,1.,0.996917333733128,1.,0.996917333733128,
1.,0.996917333733128,1.,0.996917333733128,1.,0.996917333733128,1.,0.996917333733128,
1.,0.996917333733128,1.,0.996917333733128,1.,0.996917333733128,1.,0.996917333733128,
1.,0.996917333733128,1.,0.996917333733128,1.,0.996917333733128,1.,0.996917333733128,
1.,0.996917333733128,1.,0.996917333733128,1.,0.996917333733128,1.,0.996917333733128,
1.,0.996917333733128,1.,0.996917333733128,1.,0.996917333733128,1.,0.996917333733128,
1.,0.996917333733128,1.,0.996917333733128,1.,0.996917333733128,1.,0.996917333733128,
1.,0.996917333733128,1.,0.996917333733128,1.,0.996917333733128,1.,0.996917333733128,
1.,0.996917333733128,1.,0.996917333733128,1.,0.996917333733128,1.,0.996917333733128,
1.,0.996917333733128,1.,0.996917333733128,1.),(1.,0.996917333733128,1.,
0.996917333733128,1.,0.996917333733128,1.,0.996917333733128,1.,0.996917333733128,
1.,0.996917333733128,1.,0.996917333733128,1.,0.996917333733128,1.,0.996917333733128,
1.,0.996917333733128,1.,0.996917333733128,1.,0.996917333733128,1.,0.996917333733128,
1.,0.996917333733128,1.,0.996917333733128,1.,0.996917333733128,1.,0.996917333733128,
1.,0.996917333733128,1.,0.996917333733128,1.,0.996917333733128,1.,0.996917333733128,
1.,0.996917333733128,1.,0.996917333733128,1.,0.996917333733128,1.,0.996917333733128,
1.,0.996917333733128,1.,0.996917333733128,1.,0.996917333733128,1.,0.996917333733128,
1.,0.996917333733128,1.,0.996917333733128,1.,0.996917333733128,1.,0.996917333733128,
1.,0.996917333733128,1.,0.996917333733128,1.,0.996917333733128,1.,0.996917333733128,
1.,0.996917333733128,1.,0.996917333733128,1.,0.996917333733128,1.)))
REPRESENTATION_ITEM('')
SURFACE()
);
#4033=(
BOUNDED_SURFACE()
B_SPLINE_SURFACE(1,2,((#268779,#268780,#268781,#268782,#268783,#268784,
#268785,#268786,#268787,#268788,#268789,#268790,#268791,#268792,#268793,
#268794,#268795,#268796,#268797,#268798,#268799,#268800,#268801,#268802,
#268803,#268804,#268805,#268806,#268807,#268808,#268809,#268810,#268811,
#268812,#268813,#268814,#268815,#268816,#268817,#268818,#268819,#268820,
#268821,#268822,#268823,#268824,#268825,#268826,#268827,#268828,#268829,
#268830,#268831,#268832,#268833,#268834,#268835,#268836,#268837,#268838,
#268839,#268840,#268841,#268842,#268843,#268844,#268845,#268846,#268847,
#268848,#268849,#268850,#268851,#268852,#268853,#268854,#268855,#268856,
#268857,#268858,#268859),(#268860,#268861,#268862,#268863,#268864,#268865,
#268866,#268867,#268868,#268869,#268870,#268871,#268872,#268873,#268874,
#268875,#268876,#268877,#268878,#268879,#268880,#268881,#268882,#268883,
#268884,#268885,#268886,#268887,#268888,#268889,#268890,#268891,#268892,
#268893,#268894,#268895,#268896,#268897,#268898,#268899,#268900,#268901,
#268902,#268903,#268904,#268905,#268906,#268907,#268908,#268909,#268910,
#268911,#268912,#268913,#268914,#268915,#268916,#268917,#268918,#268919,
#268920,#268921,#268922,#268923,#268924,#268925,#268926,#268927,#268928,
#268929,#268930,#268931,#268932,#268933,#268934,#268935,#268936,#268937,
#268938,#268939,#268940)),.UNSPECIFIED.,.F.,.F.,.F.)
B_SPLINE_SURFACE_WITH_KNOTS((2,2),(3,2,2,2,2,2,2,2,2,2,2,2,2,2,2,2,2,2,
2,2,2,2,2,2,2,2,2,2,2,2,2,2,2,2,2,2,2,2,2,2,3),(0.,1.),(0.,0.025,0.05,0.075,
0.1,0.125,0.15,0.175,0.2,0.225,0.25,0.275,0.3,0.325,0.35,0.375,0.4,0.425,
0.45,0.475,0.5,0.525,0.55,0.575,0.6,0.625,0.65,0.675,0.7,0.725,0.75,0.775,
0.8,0.825,0.85,0.875,0.9,0.925,0.95,0.975,1.),.UNSPECIFIED.)
GEOMETRIC_REPRESENTATION_ITEM()
RATIONAL_B_SPLINE_SURFACE(((1.,0.996917333733128,1.,0.996917333733128,1.,
0.996917333733128,1.,0.996917333733128,1.,0.996917333733128,1.,0.996917333733128,
1.,0.996917333733128,1.,0.996917333733128,1.,0.996917333733128,1.,0.996917333733128,
1.,0.996917333733128,1.,0.996917333733128,1.,0.996917333733128,1.,0.996917333733128,
1.,0.996917333733128,1.,0.996917333733128,1.,0.996917333733128,1.,0.996917333733128,
1.,0.996917333733128,1.,0.996917333733128,1.,0.996917333733128,1.,0.996917333733128,
1.,0.996917333733128,1.,0.996917333733128,1.,0.996917333733128,1.,0.996917333733128,
1.,0.996917333733128,1.,0.996917333733128,1.,0.996917333733128,1.,0.996917333733128,
1.,0.996917333733128,1.,0.996917333733128,1.,0.996917333733128,1.,0.996917333733128,
1.,0.996917333733128,1.,0.996917333733128,1.,0.996917333733128,1.,0.996917333733128,
1.,0.996917333733128,1.,0.996917333733128,1.),(1.,0.996917333733128,1.,
0.996917333733128,1.,0.996917333733128,1.,0.996917333733128,1.,0.996917333733128,
1.,0.996917333733128,1.,0.996917333733128,1.,0.996917333733128,1.,0.996917333733128,
1.,0.996917333733128,1.,0.996917333733128,1.,0.996917333733128,1.,0.996917333733128,
1.,0.996917333733128,1.,0.996917333733128,1.,0.996917333733128,1.,0.996917333733128,
1.,0.996917333733128,1.,0.996917333733128,1.,0.996917333733128,1.,0.996917333733128,
1.,0.996917333733128,1.,0.996917333733128,1.,0.996917333733128,1.,0.996917333733128,
1.,0.996917333733128,1.,0.996917333733128,1.,0.996917333733128,1.,0.996917333733128,
1.,0.996917333733128,1.,0.996917333733128,1.,0.996917333733128,1.,0.996917333733128,
1.,0.996917333733128,1.,0.996917333733128,1.,0.996917333733128,1.,0.996917333733128,
1.,0.996917333733128,1.,0.996917333733128,1.,0.996917333733128,1.)))
REPRESENTATION_ITEM('')
SURFACE()
);
#4034=(
BOUNDED_SURFACE()
B_SPLINE_SURFACE(1,2,((#269103,#269104,#269105,#269106,#269107,#269108,
#269109,#269110,#269111,#269112,#269113,#269114,#269115,#269116,#269117,
#269118,#269119,#269120,#269121,#269122,#269123,#269124,#269125,#269126,
#269127,#269128,#269129,#269130,#269131,#269132,#269133,#269134,#269135,
#269136,#269137,#269138,#269139,#269140,#269141,#269142,#269143,#269144,
#269145,#269146,#269147,#269148,#269149,#269150,#269151,#269152,#269153,
#269154,#269155,#269156,#269157,#269158,#269159,#269160,#269161,#269162,
#269163,#269164,#269165,#269166,#269167,#269168,#269169,#269170,#269171,
#269172,#269173,#269174,#269175,#269176,#269177,#269178,#269179,#269180,
#269181,#269182,#269183),(#269184,#269185,#269186,#269187,#269188,#269189,
#269190,#269191,#269192,#269193,#269194,#269195,#269196,#269197,#269198,
#269199,#269200,#269201,#269202,#269203,#269204,#269205,#269206,#269207,
#269208,#269209,#269210,#269211,#269212,#269213,#269214,#269215,#269216,
#269217,#269218,#269219,#269220,#269221,#269222,#269223,#269224,#269225,
#269226,#269227,#269228,#269229,#269230,#269231,#269232,#269233,#269234,
#269235,#269236,#269237,#269238,#269239,#269240,#269241,#269242,#269243,
#269244,#269245,#269246,#269247,#269248,#269249,#269250,#269251,#269252,
#269253,#269254,#269255,#269256,#269257,#269258,#269259,#269260,#269261,
#269262,#269263,#269264)),.UNSPECIFIED.,.F.,.F.,.F.)
B_SPLINE_SURFACE_WITH_KNOTS((2,2),(3,2,2,2,2,2,2,2,2,2,2,2,2,2,2,2,2,2,
2,2,2,2,2,2,2,2,2,2,2,2,2,2,2,2,2,2,2,2,2,2,3),(0.,1.),(0.,0.025,0.05,0.075,
0.1,0.125,0.15,0.175,0.2,0.225,0.25,0.275,0.3,0.325,0.35,0.375,0.4,0.425,
0.45,0.475,0.5,0.525,0.55,0.575,0.6,0.625,0.65,0.675,0.7,0.725,0.75,0.775,
0.8,0.825,0.85,0.875,0.9,0.925,0.95,0.975,1.),.UNSPECIFIED.)
GEOMETRIC_REPRESENTATION_ITEM()
RATIONAL_B_SPLINE_SURFACE(((1.,0.996917333733128,1.,0.996917333733128,1.,
0.996917333733128,1.,0.996917333733128,1.,0.996917333733128,1.,0.996917333733128,
1.,0.996917333733128,1.,0.996917333733128,1.,0.996917333733128,1.,0.996917333733128,
1.,0.996917333733128,1.,0.996917333733128,1.,0.996917333733128,1.,0.996917333733128,
1.,0.996917333733128,1.,0.996917333733128,1.,0.996917333733128,1.,0.996917333733128,
1.,0.996917333733128,1.,0.996917333733128,1.,0.996917333733128,1.,0.996917333733128,
1.,0.996917333733128,1.,0.996917333733128,1.,0.996917333733128,1.,0.996917333733128,
1.,0.996917333733128,1.,0.996917333733128,1.,0.996917333733128,1.,0.996917333733128,
1.,0.996917333733128,1.,0.996917333733128,1.,0.996917333733128,1.,0.996917333733128,
1.,0.996917333733128,1.,0.996917333733128,1.,0.996917333733128,1.,0.996917333733128,
1.,0.996917333733128,1.,0.996917333733128,1.),(1.,0.996917333733128,1.,
0.996917333733128,1.,0.996917333733128,1.,0.996917333733128,1.,0.996917333733128,
1.,0.996917333733128,1.,0.996917333733128,1.,0.996917333733128,1.,0.996917333733128,
1.,0.996917333733128,1.,0.996917333733128,1.,0.996917333733128,1.,0.996917333733128,
1.,0.996917333733128,1.,0.996917333733128,1.,0.996917333733128,1.,0.996917333733128,
1.,0.996917333733128,1.,0.996917333733128,1.,0.996917333733128,1.,0.996917333733128,
1.,0.996917333733128,1.,0.996917333733128,1.,0.996917333733128,1.,0.996917333733128,
1.,0.996917333733128,1.,0.996917333733128,1.,0.996917333733128,1.,0.996917333733128,
1.,0.996917333733128,1.,0.996917333733128,1.,0.996917333733128,1.,0.996917333733128,
1.,0.996917333733128,1.,0.996917333733128,1.,0.996917333733128,1.,0.996917333733128,
1.,0.996917333733128,1.,0.996917333733128,1.,0.996917333733128,1.)))
REPRESENTATION_ITEM('')
SURFACE()
);
#4035=(
BOUNDED_SURFACE()
B_SPLINE_SURFACE(1,2,((#269346,#269347,#269348,#269349,#269350,#269351,
#269352,#269353,#269354,#269355,#269356,#269357,#269358,#269359,#269360,
#269361,#269362,#269363,#269364,#269365,#269366,#269367,#269368,#269369,
#269370,#269371,#269372,#269373,#269374,#269375,#269376,#269377,#269378,
#269379,#269380,#269381,#269382,#269383,#269384,#269385,#269386,#269387,
#269388,#269389,#269390,#269391,#269392,#269393,#269394,#269395,#269396,
#269397,#269398,#269399,#269400,#269401,#269402,#269403,#269404,#269405,
#269406,#269407,#269408,#269409,#269410,#269411,#269412,#269413,#269414,
#269415,#269416,#269417,#269418,#269419,#269420,#269421,#269422,#269423,
#269424,#269425,#269426),(#269427,#269428,#269429,#269430,#269431,#269432,
#269433,#269434,#269435,#269436,#269437,#269438,#269439,#269440,#269441,
#269442,#269443,#269444,#269445,#269446,#269447,#269448,#269449,#269450,
#269451,#269452,#269453,#269454,#269455,#269456,#269457,#269458,#269459,
#269460,#269461,#269462,#269463,#269464,#269465,#269466,#269467,#269468,
#269469,#269470,#269471,#269472,#269473,#269474,#269475,#269476,#269477,
#269478,#269479,#269480,#269481,#269482,#269483,#269484,#269485,#269486,
#269487,#269488,#269489,#269490,#269491,#269492,#269493,#269494,#269495,
#269496,#269497,#269498,#269499,#269500,#269501,#269502,#269503,#269504,
#269505,#269506,#269507)),.UNSPECIFIED.,.F.,.F.,.F.)
B_SPLINE_SURFACE_WITH_KNOTS((2,2),(3,2,2,2,2,2,2,2,2,2,2,2,2,2,2,2,2,2,
2,2,2,2,2,2,2,2,2,2,2,2,2,2,2,2,2,2,2,2,2,2,3),(0.,1.),(0.,0.025,0.05,0.075,
0.1,0.125,0.15,0.175,0.2,0.225,0.25,0.275,0.3,0.325,0.35,0.375,0.4,0.425,
0.45,0.475,0.5,0.525,0.55,0.575,0.6,0.625,0.65,0.675,0.7,0.725,0.75,0.775,
0.8,0.825,0.85,0.875,0.9,0.925,0.95,0.975,1.),.UNSPECIFIED.)
GEOMETRIC_REPRESENTATION_ITEM()
RATIONAL_B_SPLINE_SURFACE(((1.,0.996917333733128,1.,0.996917333733128,1.,
0.996917333733128,1.,0.996917333733128,1.,0.996917333733128,1.,0.996917333733128,
1.,0.996917333733128,1.,0.996917333733128,1.,0.996917333733128,1.,0.996917333733128,
1.,0.996917333733128,1.,0.996917333733128,1.,0.996917333733128,1.,0.996917333733128,
1.,0.996917333733128,1.,0.996917333733128,1.,0.996917333733128,1.,0.996917333733128,
1.,0.996917333733128,1.,0.996917333733128,1.,0.996917333733128,1.,0.996917333733128,
1.,0.996917333733128,1.,0.996917333733128,1.,0.996917333733128,1.,0.996917333733128,
1.,0.996917333733128,1.,0.996917333733128,1.,0.996917333733128,1.,0.996917333733128,
1.,0.996917333733128,1.,0.996917333733128,1.,0.996917333733128,1.,0.996917333733128,
1.,0.996917333733128,1.,0.996917333733128,1.,0.996917333733128,1.,0.996917333733128,
1.,0.996917333733128,1.,0.996917333733128,1.),(1.,0.996917333733128,1.,
0.996917333733128,1.,0.996917333733128,1.,0.996917333733128,1.,0.996917333733128,
1.,0.996917333733128,1.,0.996917333733128,1.,0.996917333733128,1.,0.996917333733128,
1.,0.996917333733128,1.,0.996917333733128,1.,0.996917333733128,1.,0.996917333733128,
1.,0.996917333733128,1.,0.996917333733128,1.,0.996917333733128,1.,0.996917333733128,
1.,0.996917333733128,1.,0.996917333733128,1.,0.996917333733128,1.,0.996917333733128,
1.,0.996917333733128,1.,0.996917333733128,1.,0.996917333733128,1.,0.996917333733128,
1.,0.996917333733128,1.,0.996917333733128,1.,0.996917333733128,1.,0.996917333733128,
1.,0.996917333733128,1.,0.996917333733128,1.,0.996917333733128,1.,0.996917333733128,
1.,0.996917333733128,1.,0.996917333733128,1.,0.996917333733128,1.,0.996917333733128,
1.,0.996917333733128,1.,0.996917333733128,1.,0.996917333733128,1.)))
REPRESENTATION_ITEM('')
SURFACE()
);
#4036=(
BOUNDED_SURFACE()
B_SPLINE_SURFACE(1,2,((#269589,#269590,#269591,#269592,#269593,#269594,
#269595,#269596,#269597,#269598,#269599,#269600,#269601,#269602,#269603,
#269604,#269605,#269606,#269607,#269608,#269609,#269610,#269611,#269612,
#269613,#269614,#269615,#269616,#269617,#269618,#269619,#269620,#269621,
#269622,#269623,#269624,#269625,#269626,#269627,#269628,#269629,#269630,
#269631,#269632,#269633,#269634,#269635,#269636,#269637,#269638,#269639,
#269640,#269641,#269642,#269643,#269644,#269645,#269646,#269647,#269648,
#269649,#269650,#269651,#269652,#269653,#269654,#269655,#269656,#269657,
#269658,#269659,#269660,#269661,#269662,#269663,#269664,#269665,#269666,
#269667,#269668,#269669),(#269670,#269671,#269672,#269673,#269674,#269675,
#269676,#269677,#269678,#269679,#269680,#269681,#269682,#269683,#269684,
#269685,#269686,#269687,#269688,#269689,#269690,#269691,#269692,#269693,
#269694,#269695,#269696,#269697,#269698,#269699,#269700,#269701,#269702,
#269703,#269704,#269705,#269706,#269707,#269708,#269709,#269710,#269711,
#269712,#269713,#269714,#269715,#269716,#269717,#269718,#269719,#269720,
#269721,#269722,#269723,#269724,#269725,#269726,#269727,#269728,#269729,
#269730,#269731,#269732,#269733,#269734,#269735,#269736,#269737,#269738,
#269739,#269740,#269741,#269742,#269743,#269744,#269745,#269746,#269747,
#269748,#269749,#269750)),.UNSPECIFIED.,.F.,.F.,.F.)
B_SPLINE_SURFACE_WITH_KNOTS((2,2),(3,2,2,2,2,2,2,2,2,2,2,2,2,2,2,2,2,2,
2,2,2,2,2,2,2,2,2,2,2,2,2,2,2,2,2,2,2,2,2,2,3),(0.,1.),(0.,0.025,0.05,0.075,
0.1,0.125,0.15,0.175,0.2,0.225,0.25,0.275,0.3,0.325,0.35,0.375,0.4,0.425,
0.45,0.475,0.5,0.525,0.55,0.575,0.6,0.625,0.65,0.675,0.7,0.725,0.75,0.775,
0.8,0.825,0.85,0.875,0.9,0.925,0.95,0.975,1.),.UNSPECIFIED.)
GEOMETRIC_REPRESENTATION_ITEM()
RATIONAL_B_SPLINE_SURFACE(((1.,0.996917333733128,1.,0.996917333733128,1.,
0.996917333733128,1.,0.996917333733128,1.,0.996917333733128,1.,0.996917333733128,
1.,0.996917333733128,1.,0.996917333733128,1.,0.996917333733128,1.,0.996917333733128,
1.,0.996917333733128,1.,0.996917333733128,1.,0.996917333733128,1.,0.996917333733128,
1.,0.996917333733128,1.,0.996917333733128,1.,0.996917333733128,1.,0.996917333733128,
1.,0.996917333733128,1.,0.996917333733128,1.,0.996917333733128,1.,0.996917333733128,
1.,0.996917333733128,1.,0.996917333733128,1.,0.996917333733128,1.,0.996917333733128,
1.,0.996917333733128,1.,0.996917333733128,1.,0.996917333733128,1.,0.996917333733128,
1.,0.996917333733128,1.,0.996917333733128,1.,0.996917333733128,1.,0.996917333733128,
1.,0.996917333733128,1.,0.996917333733128,1.,0.996917333733128,1.,0.996917333733128,
1.,0.996917333733128,1.,0.996917333733128,1.),(1.,0.996917333733128,1.,
0.996917333733128,1.,0.996917333733128,1.,0.996917333733128,1.,0.996917333733128,
1.,0.996917333733128,1.,0.996917333733128,1.,0.996917333733128,1.,0.996917333733128,
1.,0.996917333733128,1.,0.996917333733128,1.,0.996917333733128,1.,0.996917333733128,
1.,0.996917333733128,1.,0.996917333733128,1.,0.996917333733128,1.,0.996917333733128,
1.,0.996917333733128,1.,0.996917333733128,1.,0.996917333733128,1.,0.996917333733128,
1.,0.996917333733128,1.,0.996917333733128,1.,0.996917333733128,1.,0.996917333733128,
1.,0.996917333733128,1.,0.996917333733128,1.,0.996917333733128,1.,0.996917333733128,
1.,0.996917333733128,1.,0.996917333733128,1.,0.996917333733128,1.,0.996917333733128,
1.,0.996917333733128,1.,0.996917333733128,1.,0.996917333733128,1.,0.996917333733128,
1.,0.996917333733128,1.,0.996917333733128,1.,0.996917333733128,1.)))
REPRESENTATION_ITEM('')
SURFACE()
);
#4037=(
BOUNDED_SURFACE()
B_SPLINE_SURFACE(1,2,((#269751,#269752,#269753,#269754,#269755,#269756,
#269757,#269758,#269759,#269760,#269761,#269762,#269763,#269764,#269765,
#269766,#269767,#269768,#269769,#269770,#269771,#269772,#269773,#269774,
#269775,#269776,#269777,#269778,#269779,#269780,#269781,#269782,#269783,
#269784,#269785,#269786,#269787,#269788,#269789,#269790,#269791,#269792,
#269793,#269794,#269795,#269796,#269797,#269798,#269799,#269800,#269801,
#269802,#269803,#269804,#269805,#269806,#269807,#269808,#269809,#269810,
#269811,#269812,#269813,#269814,#269815,#269816,#269817,#269818,#269819,
#269820,#269821,#269822,#269823,#269824,#269825,#269826,#269827,#269828,
#269829,#269830,#269831),(#269832,#269833,#269834,#269835,#269836,#269837,
#269838,#269839,#269840,#269841,#269842,#269843,#269844,#269845,#269846,
#269847,#269848,#269849,#269850,#269851,#269852,#269853,#269854,#269855,
#269856,#269857,#269858,#269859,#269860,#269861,#269862,#269863,#269864,
#269865,#269866,#269867,#269868,#269869,#269870,#269871,#269872,#269873,
#269874,#269875,#269876,#269877,#269878,#269879,#269880,#269881,#269882,
#269883,#269884,#269885,#269886,#269887,#269888,#269889,#269890,#269891,
#269892,#269893,#269894,#269895,#269896,#269897,#269898,#269899,#269900,
#269901,#269902,#269903,#269904,#269905,#269906,#269907,#269908,#269909,
#269910,#269911,#269912)),.UNSPECIFIED.,.F.,.F.,.F.)
B_SPLINE_SURFACE_WITH_KNOTS((2,2),(3,2,2,2,2,2,2,2,2,2,2,2,2,2,2,2,2,2,
2,2,2,2,2,2,2,2,2,2,2,2,2,2,2,2,2,2,2,2,2,2,3),(0.,1.),(0.,0.025,0.05,0.075,
0.1,0.125,0.15,0.175,0.2,0.225,0.25,0.275,0.3,0.325,0.35,0.375,0.4,0.425,
0.45,0.475,0.5,0.525,0.55,0.575,0.6,0.625,0.65,0.675,0.7,0.725,0.75,0.775,
0.8,0.825,0.85,0.875,0.9,0.925,0.95,0.975,1.),.UNSPECIFIED.)
GEOMETRIC_REPRESENTATION_ITEM()
RATIONAL_B_SPLINE_SURFACE(((1.,0.996917333733128,1.,0.996917333733128,1.,
0.996917333733128,1.,0.996917333733128,1.,0.996917333733128,1.,0.996917333733128,
1.,0.996917333733128,1.,0.996917333733128,1.,0.996917333733128,1.,0.996917333733128,
1.,0.996917333733128,1.,0.996917333733128,1.,0.996917333733128,1.,0.996917333733128,
1.,0.996917333733128,1.,0.996917333733128,1.,0.996917333733128,1.,0.996917333733128,
1.,0.996917333733128,1.,0.996917333733128,1.,0.996917333733128,1.,0.996917333733128,
1.,0.996917333733128,1.,0.996917333733128,1.,0.996917333733128,1.,0.996917333733128,
1.,0.996917333733128,1.,0.996917333733128,1.,0.996917333733128,1.,0.996917333733128,
1.,0.996917333733128,1.,0.996917333733128,1.,0.996917333733128,1.,0.996917333733128,
1.,0.996917333733128,1.,0.996917333733128,1.,0.996917333733128,1.,0.996917333733128,
1.,0.996917333733128,1.,0.996917333733128,1.),(1.,0.996917333733128,1.,
0.996917333733128,1.,0.996917333733128,1.,0.996917333733128,1.,0.996917333733128,
1.,0.996917333733128,1.,0.996917333733128,1.,0.996917333733128,1.,0.996917333733128,
1.,0.996917333733128,1.,0.996917333733128,1.,0.996917333733128,1.,0.996917333733128,
1.,0.996917333733128,1.,0.996917333733128,1.,0.996917333733128,1.,0.996917333733128,
1.,0.996917333733128,1.,0.996917333733128,1.,0.996917333733128,1.,0.996917333733128,
1.,0.996917333733128,1.,0.996917333733128,1.,0.996917333733128,1.,0.996917333733128,
1.,0.996917333733128,1.,0.996917333733128,1.,0.996917333733128,1.,0.996917333733128,
1.,0.996917333733128,1.,0.996917333733128,1.,0.996917333733128,1.,0.996917333733128,
1.,0.996917333733128,1.,0.996917333733128,1.,0.996917333733128,1.,0.996917333733128,
1.,0.996917333733128,1.,0.996917333733128,1.,0.996917333733128,1.)))
REPRESENTATION_ITEM('')
SURFACE()
);
#4038=(
BOUNDED_SURFACE()
B_SPLINE_SURFACE(1,2,((#270075,#270076,#270077,#270078,#270079,#270080,
#270081,#270082,#270083,#270084,#270085,#270086,#270087,#270088,#270089,
#270090,#270091,#270092,#270093,#270094,#270095,#270096,#270097,#270098,
#270099,#270100,#270101,#270102,#270103,#270104,#270105,#270106,#270107,
#270108,#270109,#270110,#270111,#270112,#270113,#270114,#270115,#270116,
#270117,#270118,#270119,#270120,#270121,#270122,#270123,#270124,#270125,
#270126,#270127,#270128,#270129,#270130,#270131,#270132,#270133,#270134,
#270135,#270136,#270137,#270138,#270139,#270140,#270141,#270142,#270143,
#270144,#270145,#270146,#270147,#270148,#270149,#270150,#270151,#270152,
#270153,#270154,#270155),(#270156,#270157,#270158,#270159,#270160,#270161,
#270162,#270163,#270164,#270165,#270166,#270167,#270168,#270169,#270170,
#270171,#270172,#270173,#270174,#270175,#270176,#270177,#270178,#270179,
#270180,#270181,#270182,#270183,#270184,#270185,#270186,#270187,#270188,
#270189,#270190,#270191,#270192,#270193,#270194,#270195,#270196,#270197,
#270198,#270199,#270200,#270201,#270202,#270203,#270204,#270205,#270206,
#270207,#270208,#270209,#270210,#270211,#270212,#270213,#270214,#270215,
#270216,#270217,#270218,#270219,#270220,#270221,#270222,#270223,#270224,
#270225,#270226,#270227,#270228,#270229,#270230,#270231,#270232,#270233,
#270234,#270235,#270236)),.UNSPECIFIED.,.F.,.F.,.F.)
B_SPLINE_SURFACE_WITH_KNOTS((2,2),(3,2,2,2,2,2,2,2,2,2,2,2,2,2,2,2,2,2,
2,2,2,2,2,2,2,2,2,2,2,2,2,2,2,2,2,2,2,2,2,2,3),(0.,1.),(0.,0.025,0.05,0.075,
0.1,0.125,0.15,0.175,0.2,0.225,0.25,0.275,0.3,0.325,0.35,0.375,0.4,0.425,
0.45,0.475,0.5,0.525,0.55,0.575,0.6,0.625,0.65,0.675,0.7,0.725,0.75,0.775,
0.8,0.825,0.85,0.875,0.9,0.925,0.95,0.975,1.),.UNSPECIFIED.)
GEOMETRIC_REPRESENTATION_ITEM()
RATIONAL_B_SPLINE_SURFACE(((1.,0.996917333733128,1.,0.996917333733128,1.,
0.996917333733128,1.,0.996917333733128,1.,0.996917333733128,1.,0.996917333733128,
1.,0.996917333733128,1.,0.996917333733128,1.,0.996917333733128,1.,0.996917333733128,
1.,0.996917333733128,1.,0.996917333733128,1.,0.996917333733128,1.,0.996917333733128,
1.,0.996917333733128,1.,0.996917333733128,1.,0.996917333733128,1.,0.996917333733128,
1.,0.996917333733128,1.,0.996917333733128,1.,0.996917333733128,1.,0.996917333733128,
1.,0.996917333733128,1.,0.996917333733128,1.,0.996917333733128,1.,0.996917333733128,
1.,0.996917333733128,1.,0.996917333733128,1.,0.996917333733128,1.,0.996917333733128,
1.,0.996917333733128,1.,0.996917333733128,1.,0.996917333733128,1.,0.996917333733128,
1.,0.996917333733128,1.,0.996917333733128,1.,0.996917333733128,1.,0.996917333733128,
1.,0.996917333733128,1.,0.996917333733128,1.),(1.,0.996917333733128,1.,
0.996917333733128,1.,0.996917333733128,1.,0.996917333733128,1.,0.996917333733128,
1.,0.996917333733128,1.,0.996917333733128,1.,0.996917333733128,1.,0.996917333733128,
1.,0.996917333733128,1.,0.996917333733128,1.,0.996917333733128,1.,0.996917333733128,
1.,0.996917333733128,1.,0.996917333733128,1.,0.996917333733128,1.,0.996917333733128,
1.,0.996917333733128,1.,0.996917333733128,1.,0.996917333733128,1.,0.996917333733128,
1.,0.996917333733128,1.,0.996917333733128,1.,0.996917333733128,1.,0.996917333733128,
1.,0.996917333733128,1.,0.996917333733128,1.,0.996917333733128,1.,0.996917333733128,
1.,0.996917333733128,1.,0.996917333733128,1.,0.996917333733128,1.,0.996917333733128,
1.,0.996917333733128,1.,0.996917333733128,1.,0.996917333733128,1.,0.996917333733128,
1.,0.996917333733128,1.,0.996917333733128,1.,0.996917333733128,1.)))
REPRESENTATION_ITEM('')
SURFACE()
);
#4039=(
BOUNDED_SURFACE()
B_SPLINE_SURFACE(1,2,((#270318,#270319,#270320,#270321,#270322,#270323,
#270324,#270325,#270326,#270327,#270328,#270329,#270330,#270331,#270332,
#270333,#270334,#270335,#270336,#270337,#270338,#270339,#270340,#270341,
#270342,#270343,#270344,#270345,#270346,#270347,#270348,#270349,#270350,
#270351,#270352,#270353,#270354,#270355,#270356,#270357,#270358,#270359,
#270360,#270361,#270362,#270363,#270364,#270365,#270366,#270367,#270368,
#270369,#270370,#270371,#270372,#270373,#270374,#270375,#270376,#270377,
#270378,#270379,#270380,#270381,#270382,#270383,#270384,#270385,#270386,
#270387,#270388,#270389,#270390,#270391,#270392,#270393,#270394,#270395,
#270396,#270397,#270398),(#270399,#270400,#270401,#270402,#270403,#270404,
#270405,#270406,#270407,#270408,#270409,#270410,#270411,#270412,#270413,
#270414,#270415,#270416,#270417,#270418,#270419,#270420,#270421,#270422,
#270423,#270424,#270425,#270426,#270427,#270428,#270429,#270430,#270431,
#270432,#270433,#270434,#270435,#270436,#270437,#270438,#270439,#270440,
#270441,#270442,#270443,#270444,#270445,#270446,#270447,#270448,#270449,
#270450,#270451,#270452,#270453,#270454,#270455,#270456,#270457,#270458,
#270459,#270460,#270461,#270462,#270463,#270464,#270465,#270466,#270467,
#270468,#270469,#270470,#270471,#270472,#270473,#270474,#270475,#270476,
#270477,#270478,#270479)),.UNSPECIFIED.,.F.,.F.,.F.)
B_SPLINE_SURFACE_WITH_KNOTS((2,2),(3,2,2,2,2,2,2,2,2,2,2,2,2,2,2,2,2,2,
2,2,2,2,2,2,2,2,2,2,2,2,2,2,2,2,2,2,2,2,2,2,3),(0.,1.),(0.,0.025,0.05,0.075,
0.1,0.125,0.15,0.175,0.2,0.225,0.25,0.275,0.3,0.325,0.35,0.375,0.4,0.425,
0.45,0.475,0.5,0.525,0.55,0.575,0.6,0.625,0.65,0.675,0.7,0.725,0.75,0.775,
0.8,0.825,0.85,0.875,0.9,0.925,0.95,0.975,1.),.UNSPECIFIED.)
GEOMETRIC_REPRESENTATION_ITEM()
RATIONAL_B_SPLINE_SURFACE(((1.,0.996917333733128,1.,0.996917333733128,1.,
0.996917333733128,1.,0.996917333733128,1.,0.996917333733128,1.,0.996917333733128,
1.,0.996917333733128,1.,0.996917333733128,1.,0.996917333733128,1.,0.996917333733128,
1.,0.996917333733128,1.,0.996917333733128,1.,0.996917333733128,1.,0.996917333733128,
1.,0.996917333733128,1.,0.996917333733128,1.,0.996917333733128,1.,0.996917333733128,
1.,0.996917333733128,1.,0.996917333733128,1.,0.996917333733128,1.,0.996917333733128,
1.,0.996917333733128,1.,0.996917333733128,1.,0.996917333733128,1.,0.996917333733128,
1.,0.996917333733128,1.,0.996917333733128,1.,0.996917333733128,1.,0.996917333733128,
1.,0.996917333733128,1.,0.996917333733128,1.,0.996917333733128,1.,0.996917333733128,
1.,0.996917333733128,1.,0.996917333733128,1.,0.996917333733128,1.,0.996917333733128,
1.,0.996917333733128,1.,0.996917333733128,1.),(1.,0.996917333733128,1.,
0.996917333733128,1.,0.996917333733128,1.,0.996917333733128,1.,0.996917333733128,
1.,0.996917333733128,1.,0.996917333733128,1.,0.996917333733128,1.,0.996917333733128,
1.,0.996917333733128,1.,0.996917333733128,1.,0.996917333733128,1.,0.996917333733128,
1.,0.996917333733128,1.,0.996917333733128,1.,0.996917333733128,1.,0.996917333733128,
1.,0.996917333733128,1.,0.996917333733128,1.,0.996917333733128,1.,0.996917333733128,
1.,0.996917333733128,1.,0.996917333733128,1.,0.996917333733128,1.,0.996917333733128,
1.,0.996917333733128,1.,0.996917333733128,1.,0.996917333733128,1.,0.996917333733128,
1.,0.996917333733128,1.,0.996917333733128,1.,0.996917333733128,1.,0.996917333733128,
1.,0.996917333733128,1.,0.996917333733128,1.,0.996917333733128,1.,0.996917333733128,
1.,0.996917333733128,1.,0.996917333733128,1.,0.996917333733128,1.)))
REPRESENTATION_ITEM('')
SURFACE()
);
#4040=(
BOUNDED_SURFACE()
B_SPLINE_SURFACE(1,2,((#270561,#270562,#270563,#270564,#270565,#270566,
#270567,#270568,#270569,#270570,#270571,#270572,#270573,#270574,#270575,
#270576,#270577,#270578,#270579,#270580,#270581,#270582,#270583,#270584,
#270585,#270586,#270587,#270588,#270589,#270590,#270591,#270592,#270593,
#270594,#270595,#270596,#270597,#270598,#270599,#270600,#270601,#270602,
#270603,#270604,#270605,#270606,#270607,#270608,#270609,#270610,#270611,
#270612,#270613,#270614,#270615,#270616,#270617,#270618,#270619,#270620,
#270621,#270622,#270623,#270624,#270625,#270626,#270627,#270628,#270629,
#270630,#270631,#270632,#270633,#270634,#270635,#270636,#270637,#270638,
#270639,#270640,#270641),(#270642,#270643,#270644,#270645,#270646,#270647,
#270648,#270649,#270650,#270651,#270652,#270653,#270654,#270655,#270656,
#270657,#270658,#270659,#270660,#270661,#270662,#270663,#270664,#270665,
#270666,#270667,#270668,#270669,#270670,#270671,#270672,#270673,#270674,
#270675,#270676,#270677,#270678,#270679,#270680,#270681,#270682,#270683,
#270684,#270685,#270686,#270687,#270688,#270689,#270690,#270691,#270692,
#270693,#270694,#270695,#270696,#270697,#270698,#270699,#270700,#270701,
#270702,#270703,#270704,#270705,#270706,#270707,#270708,#270709,#270710,
#270711,#270712,#270713,#270714,#270715,#270716,#270717,#270718,#270719,
#270720,#270721,#270722)),.UNSPECIFIED.,.F.,.F.,.F.)
B_SPLINE_SURFACE_WITH_KNOTS((2,2),(3,2,2,2,2,2,2,2,2,2,2,2,2,2,2,2,2,2,
2,2,2,2,2,2,2,2,2,2,2,2,2,2,2,2,2,2,2,2,2,2,3),(0.,1.),(0.,0.025,0.05,0.075,
0.1,0.125,0.15,0.175,0.2,0.225,0.25,0.275,0.3,0.325,0.35,0.375,0.4,0.425,
0.45,0.475,0.5,0.525,0.55,0.575,0.6,0.625,0.65,0.675,0.7,0.725,0.75,0.775,
0.8,0.825,0.85,0.875,0.9,0.925,0.95,0.975,1.),.UNSPECIFIED.)
GEOMETRIC_REPRESENTATION_ITEM()
RATIONAL_B_SPLINE_SURFACE(((1.,0.996917333733128,1.,0.996917333733128,1.,
0.996917333733128,1.,0.996917333733128,1.,0.996917333733128,1.,0.996917333733128,
1.,0.996917333733128,1.,0.996917333733128,1.,0.996917333733128,1.,0.996917333733128,
1.,0.996917333733128,1.,0.996917333733128,1.,0.996917333733128,1.,0.996917333733128,
1.,0.996917333733128,1.,0.996917333733128,1.,0.996917333733128,1.,0.996917333733128,
1.,0.996917333733128,1.,0.996917333733128,1.,0.996917333733128,1.,0.996917333733128,
1.,0.996917333733128,1.,0.996917333733128,1.,0.996917333733128,1.,0.996917333733128,
1.,0.996917333733128,1.,0.996917333733128,1.,0.996917333733128,1.,0.996917333733128,
1.,0.996917333733128,1.,0.996917333733128,1.,0.996917333733128,1.,0.996917333733128,
1.,0.996917333733128,1.,0.996917333733128,1.,0.996917333733128,1.,0.996917333733128,
1.,0.996917333733128,1.,0.996917333733128,1.),(1.,0.996917333733128,1.,
0.996917333733128,1.,0.996917333733128,1.,0.996917333733128,1.,0.996917333733128,
1.,0.996917333733128,1.,0.996917333733128,1.,0.996917333733128,1.,0.996917333733128,
1.,0.996917333733128,1.,0.996917333733128,1.,0.996917333733128,1.,0.996917333733128,
1.,0.996917333733128,1.,0.996917333733128,1.,0.996917333733128,1.,0.996917333733128,
1.,0.996917333733128,1.,0.996917333733128,1.,0.996917333733128,1.,0.996917333733128,
1.,0.996917333733128,1.,0.996917333733128,1.,0.996917333733128,1.,0.996917333733128,
1.,0.996917333733128,1.,0.996917333733128,1.,0.996917333733128,1.,0.996917333733128,
1.,0.996917333733128,1.,0.996917333733128,1.,0.996917333733128,1.,0.996917333733128,
1.,0.996917333733128,1.,0.996917333733128,1.,0.996917333733128,1.,0.996917333733128,
1.,0.996917333733128,1.,0.996917333733128,1.,0.996917333733128,1.)))
REPRESENTATION_ITEM('')
SURFACE()
);
#4041=(
BOUNDED_SURFACE()
B_SPLINE_SURFACE(1,2,((#270723,#270724,#270725,#270726,#270727,#270728,
#270729,#270730,#270731,#270732,#270733,#270734,#270735,#270736,#270737,
#270738,#270739,#270740,#270741,#270742,#270743,#270744,#270745,#270746,
#270747,#270748,#270749,#270750,#270751,#270752,#270753,#270754,#270755,
#270756,#270757,#270758,#270759,#270760,#270761,#270762,#270763,#270764,
#270765,#270766,#270767,#270768,#270769,#270770,#270771,#270772,#270773,
#270774,#270775,#270776,#270777,#270778,#270779,#270780,#270781,#270782,
#270783,#270784,#270785,#270786,#270787,#270788,#270789,#270790,#270791,
#270792,#270793,#270794,#270795,#270796,#270797,#270798,#270799,#270800,
#270801,#270802,#270803),(#270804,#270805,#270806,#270807,#270808,#270809,
#270810,#270811,#270812,#270813,#270814,#270815,#270816,#270817,#270818,
#270819,#270820,#270821,#270822,#270823,#270824,#270825,#270826,#270827,
#270828,#270829,#270830,#270831,#270832,#270833,#270834,#270835,#270836,
#270837,#270838,#270839,#270840,#270841,#270842,#270843,#270844,#270845,
#270846,#270847,#270848,#270849,#270850,#270851,#270852,#270853,#270854,
#270855,#270856,#270857,#270858,#270859,#270860,#270861,#270862,#270863,
#270864,#270865,#270866,#270867,#270868,#270869,#270870,#270871,#270872,
#270873,#270874,#270875,#270876,#270877,#270878,#270879,#270880,#270881,
#270882,#270883,#270884)),.UNSPECIFIED.,.F.,.F.,.F.)
B_SPLINE_SURFACE_WITH_KNOTS((2,2),(3,2,2,2,2,2,2,2,2,2,2,2,2,2,2,2,2,2,
2,2,2,2,2,2,2,2,2,2,2,2,2,2,2,2,2,2,2,2,2,2,3),(0.,1.),(0.,0.025,0.05,0.075,
0.1,0.125,0.15,0.175,0.2,0.225,0.25,0.275,0.3,0.325,0.35,0.375,0.4,0.425,
0.45,0.475,0.5,0.525,0.55,0.575,0.6,0.625,0.65,0.675,0.7,0.725,0.75,0.775,
0.8,0.825,0.85,0.875,0.9,0.925,0.95,0.975,1.),.UNSPECIFIED.)
GEOMETRIC_REPRESENTATION_ITEM()
RATIONAL_B_SPLINE_SURFACE(((1.,0.996917333733128,1.,0.996917333733128,1.,
0.996917333733128,1.,0.996917333733128,1.,0.996917333733128,1.,0.996917333733128,
1.,0.996917333733128,1.,0.996917333733128,1.,0.996917333733128,1.,0.996917333733128,
1.,0.996917333733128,1.,0.996917333733128,1.,0.996917333733128,1.,0.996917333733128,
1.,0.996917333733128,1.,0.996917333733128,1.,0.996917333733128,1.,0.996917333733128,
1.,0.996917333733128,1.,0.996917333733128,1.,0.996917333733128,1.,0.996917333733128,
1.,0.996917333733128,1.,0.996917333733128,1.,0.996917333733128,1.,0.996917333733128,
1.,0.996917333733128,1.,0.996917333733128,1.,0.996917333733128,1.,0.996917333733128,
1.,0.996917333733128,1.,0.996917333733128,1.,0.996917333733128,1.,0.996917333733128,
1.,0.996917333733128,1.,0.996917333733128,1.,0.996917333733128,1.,0.996917333733128,
1.,0.996917333733128,1.,0.996917333733128,1.),(1.,0.996917333733128,1.,
0.996917333733128,1.,0.996917333733128,1.,0.996917333733128,1.,0.996917333733128,
1.,0.996917333733128,1.,0.996917333733128,1.,0.996917333733128,1.,0.996917333733128,
1.,0.996917333733128,1.,0.996917333733128,1.,0.996917333733128,1.,0.996917333733128,
1.,0.996917333733128,1.,0.996917333733128,1.,0.996917333733128,1.,0.996917333733128,
1.,0.996917333733128,1.,0.996917333733128,1.,0.996917333733128,1.,0.996917333733128,
1.,0.996917333733128,1.,0.996917333733128,1.,0.996917333733128,1.,0.996917333733128,
1.,0.996917333733128,1.,0.996917333733128,1.,0.996917333733128,1.,0.996917333733128,
1.,0.996917333733128,1.,0.996917333733128,1.,0.996917333733128,1.,0.996917333733128,
1.,0.996917333733128,1.,0.996917333733128,1.,0.996917333733128,1.,0.996917333733128,
1.,0.996917333733128,1.,0.996917333733128,1.,0.996917333733128,1.)))
REPRESENTATION_ITEM('')
SURFACE()
);
#4042=(
BOUNDED_SURFACE()
B_SPLINE_SURFACE(1,2,((#271047,#271048,#271049,#271050,#271051,#271052,
#271053,#271054,#271055,#271056,#271057,#271058,#271059,#271060,#271061,
#271062,#271063,#271064,#271065,#271066,#271067,#271068,#271069,#271070,
#271071,#271072,#271073,#271074,#271075,#271076,#271077,#271078,#271079,
#271080,#271081,#271082,#271083,#271084,#271085,#271086,#271087,#271088,
#271089,#271090,#271091,#271092,#271093,#271094,#271095,#271096,#271097,
#271098,#271099,#271100,#271101,#271102,#271103,#271104,#271105,#271106,
#271107,#271108,#271109,#271110,#271111,#271112,#271113,#271114,#271115,
#271116,#271117,#271118,#271119,#271120,#271121,#271122,#271123,#271124,
#271125,#271126,#271127),(#271128,#271129,#271130,#271131,#271132,#271133,
#271134,#271135,#271136,#271137,#271138,#271139,#271140,#271141,#271142,
#271143,#271144,#271145,#271146,#271147,#271148,#271149,#271150,#271151,
#271152,#271153,#271154,#271155,#271156,#271157,#271158,#271159,#271160,
#271161,#271162,#271163,#271164,#271165,#271166,#271167,#271168,#271169,
#271170,#271171,#271172,#271173,#271174,#271175,#271176,#271177,#271178,
#271179,#271180,#271181,#271182,#271183,#271184,#271185,#271186,#271187,
#271188,#271189,#271190,#271191,#271192,#271193,#271194,#271195,#271196,
#271197,#271198,#271199,#271200,#271201,#271202,#271203,#271204,#271205,
#271206,#271207,#271208)),.UNSPECIFIED.,.F.,.F.,.F.)
B_SPLINE_SURFACE_WITH_KNOTS((2,2),(3,2,2,2,2,2,2,2,2,2,2,2,2,2,2,2,2,2,
2,2,2,2,2,2,2,2,2,2,2,2,2,2,2,2,2,2,2,2,2,2,3),(0.,1.),(0.,0.025,0.05,0.075,
0.1,0.125,0.15,0.175,0.2,0.225,0.25,0.275,0.3,0.325,0.35,0.375,0.4,0.425,
0.45,0.475,0.5,0.525,0.55,0.575,0.6,0.625,0.65,0.675,0.7,0.725,0.75,0.775,
0.8,0.825,0.85,0.875,0.9,0.925,0.95,0.975,1.),.UNSPECIFIED.)
GEOMETRIC_REPRESENTATION_ITEM()
RATIONAL_B_SPLINE_SURFACE(((1.,0.996917333733128,1.,0.996917333733128,1.,
0.996917333733128,1.,0.996917333733128,1.,0.996917333733128,1.,0.996917333733128,
1.,0.996917333733128,1.,0.996917333733128,1.,0.996917333733128,1.,0.996917333733128,
1.,0.996917333733128,1.,0.996917333733128,1.,0.996917333733128,1.,0.996917333733128,
1.,0.996917333733128,1.,0.996917333733128,1.,0.996917333733128,1.,0.996917333733128,
1.,0.996917333733128,1.,0.996917333733128,1.,0.996917333733128,1.,0.996917333733128,
1.,0.996917333733128,1.,0.996917333733128,1.,0.996917333733128,1.,0.996917333733128,
1.,0.996917333733128,1.,0.996917333733128,1.,0.996917333733128,1.,0.996917333733128,
1.,0.996917333733128,1.,0.996917333733128,1.,0.996917333733128,1.,0.996917333733128,
1.,0.996917333733128,1.,0.996917333733128,1.,0.996917333733128,1.,0.996917333733128,
1.,0.996917333733128,1.,0.996917333733128,1.),(1.,0.996917333733128,1.,
0.996917333733128,1.,0.996917333733128,1.,0.996917333733128,1.,0.996917333733128,
1.,0.996917333733128,1.,0.996917333733128,1.,0.996917333733128,1.,0.996917333733128,
1.,0.996917333733128,1.,0.996917333733128,1.,0.996917333733128,1.,0.996917333733128,
1.,0.996917333733128,1.,0.996917333733128,1.,0.996917333733128,1.,0.996917333733128,
1.,0.996917333733128,1.,0.996917333733128,1.,0.996917333733128,1.,0.996917333733128,
1.,0.996917333733128,1.,0.996917333733128,1.,0.996917333733128,1.,0.996917333733128,
1.,0.996917333733128,1.,0.996917333733128,1.,0.996917333733128,1.,0.996917333733128,
1.,0.996917333733128,1.,0.996917333733128,1.,0.996917333733128,1.,0.996917333733128,
1.,0.996917333733128,1.,0.996917333733128,1.,0.996917333733128,1.,0.996917333733128,
1.,0.996917333733128,1.,0.996917333733128,1.,0.996917333733128,1.)))
REPRESENTATION_ITEM('')
SURFACE()
);
#4043=(
BOUNDED_SURFACE()
B_SPLINE_SURFACE(1,2,((#271290,#271291,#271292,#271293,#271294,#271295,
#271296,#271297,#271298,#271299,#271300,#271301,#271302,#271303,#271304,
#271305,#271306,#271307,#271308,#271309,#271310,#271311,#271312,#271313,
#271314,#271315,#271316,#271317,#271318,#271319,#271320,#271321,#271322,
#271323,#271324,#271325,#271326,#271327,#271328,#271329,#271330,#271331,
#271332,#271333,#271334,#271335,#271336,#271337,#271338,#271339,#271340,
#271341,#271342,#271343,#271344,#271345,#271346,#271347,#271348,#271349,
#271350,#271351,#271352,#271353,#271354,#271355,#271356,#271357,#271358,
#271359,#271360,#271361,#271362,#271363,#271364,#271365,#271366,#271367,
#271368,#271369,#271370),(#271371,#271372,#271373,#271374,#271375,#271376,
#271377,#271378,#271379,#271380,#271381,#271382,#271383,#271384,#271385,
#271386,#271387,#271388,#271389,#271390,#271391,#271392,#271393,#271394,
#271395,#271396,#271397,#271398,#271399,#271400,#271401,#271402,#271403,
#271404,#271405,#271406,#271407,#271408,#271409,#271410,#271411,#271412,
#271413,#271414,#271415,#271416,#271417,#271418,#271419,#271420,#271421,
#271422,#271423,#271424,#271425,#271426,#271427,#271428,#271429,#271430,
#271431,#271432,#271433,#271434,#271435,#271436,#271437,#271438,#271439,
#271440,#271441,#271442,#271443,#271444,#271445,#271446,#271447,#271448,
#271449,#271450,#271451)),.UNSPECIFIED.,.F.,.F.,.F.)
B_SPLINE_SURFACE_WITH_KNOTS((2,2),(3,2,2,2,2,2,2,2,2,2,2,2,2,2,2,2,2,2,
2,2,2,2,2,2,2,2,2,2,2,2,2,2,2,2,2,2,2,2,2,2,3),(0.,1.),(0.,0.025,0.05,0.075,
0.1,0.125,0.15,0.175,0.2,0.225,0.25,0.275,0.3,0.325,0.35,0.375,0.4,0.425,
0.45,0.475,0.5,0.525,0.55,0.575,0.6,0.625,0.65,0.675,0.7,0.725,0.75,0.775,
0.8,0.825,0.85,0.875,0.9,0.925,0.95,0.975,1.),.UNSPECIFIED.)
GEOMETRIC_REPRESENTATION_ITEM()
RATIONAL_B_SPLINE_SURFACE(((1.,0.996917333733128,1.,0.996917333733128,1.,
0.996917333733128,1.,0.996917333733128,1.,0.996917333733128,1.,0.996917333733128,
1.,0.996917333733128,1.,0.996917333733128,1.,0.996917333733128,1.,0.996917333733128,
1.,0.996917333733128,1.,0.996917333733128,1.,0.996917333733128,1.,0.996917333733128,
1.,0.996917333733128,1.,0.996917333733128,1.,0.996917333733128,1.,0.996917333733128,
1.,0.996917333733128,1.,0.996917333733128,1.,0.996917333733128,1.,0.996917333733128,
1.,0.996917333733128,1.,0.996917333733128,1.,0.996917333733128,1.,0.996917333733128,
1.,0.996917333733128,1.,0.996917333733128,1.,0.996917333733128,1.,0.996917333733128,
1.,0.996917333733128,1.,0.996917333733128,1.,0.996917333733128,1.,0.996917333733128,
1.,0.996917333733128,1.,0.996917333733128,1.,0.996917333733128,1.,0.996917333733128,
1.,0.996917333733128,1.,0.996917333733128,1.),(1.,0.996917333733128,1.,
0.996917333733128,1.,0.996917333733128,1.,0.996917333733128,1.,0.996917333733128,
1.,0.996917333733128,1.,0.996917333733128,1.,0.996917333733128,1.,0.996917333733128,
1.,0.996917333733128,1.,0.996917333733128,1.,0.996917333733128,1.,0.996917333733128,
1.,0.996917333733128,1.,0.996917333733128,1.,0.996917333733128,1.,0.996917333733128,
1.,0.996917333733128,1.,0.996917333733128,1.,0.996917333733128,1.,0.996917333733128,
1.,0.996917333733128,1.,0.996917333733128,1.,0.996917333733128,1.,0.996917333733128,
1.,0.996917333733128,1.,0.996917333733128,1.,0.996917333733128,1.,0.996917333733128,
1.,0.996917333733128,1.,0.996917333733128,1.,0.996917333733128,1.,0.996917333733128,
1.,0.996917333733128,1.,0.996917333733128,1.,0.996917333733128,1.,0.996917333733128,
1.,0.996917333733128,1.,0.996917333733128,1.,0.996917333733128,1.)))
REPRESENTATION_ITEM('')
SURFACE()
);
#4044=(
BOUNDED_SURFACE()
B_SPLINE_SURFACE(1,2,((#271533,#271534,#271535,#271536,#271537,#271538,
#271539,#271540,#271541,#271542,#271543,#271544,#271545,#271546,#271547,
#271548,#271549,#271550,#271551,#271552,#271553,#271554,#271555,#271556,
#271557,#271558,#271559,#271560,#271561,#271562,#271563,#271564,#271565,
#271566,#271567,#271568,#271569,#271570,#271571,#271572,#271573,#271574,
#271575,#271576,#271577,#271578,#271579,#271580,#271581,#271582,#271583,
#271584,#271585,#271586,#271587,#271588,#271589,#271590,#271591,#271592,
#271593,#271594,#271595,#271596,#271597,#271598,#271599,#271600,#271601,
#271602,#271603,#271604,#271605,#271606,#271607,#271608,#271609,#271610,
#271611,#271612,#271613),(#271614,#271615,#271616,#271617,#271618,#271619,
#271620,#271621,#271622,#271623,#271624,#271625,#271626,#271627,#271628,
#271629,#271630,#271631,#271632,#271633,#271634,#271635,#271636,#271637,
#271638,#271639,#271640,#271641,#271642,#271643,#271644,#271645,#271646,
#271647,#271648,#271649,#271650,#271651,#271652,#271653,#271654,#271655,
#271656,#271657,#271658,#271659,#271660,#271661,#271662,#271663,#271664,
#271665,#271666,#271667,#271668,#271669,#271670,#271671,#271672,#271673,
#271674,#271675,#271676,#271677,#271678,#271679,#271680,#271681,#271682,
#271683,#271684,#271685,#271686,#271687,#271688,#271689,#271690,#271691,
#271692,#271693,#271694)),.UNSPECIFIED.,.F.,.F.,.F.)
B_SPLINE_SURFACE_WITH_KNOTS((2,2),(3,2,2,2,2,2,2,2,2,2,2,2,2,2,2,2,2,2,
2,2,2,2,2,2,2,2,2,2,2,2,2,2,2,2,2,2,2,2,2,2,3),(0.,1.),(0.,0.025,0.05,0.075,
0.1,0.125,0.15,0.175,0.2,0.225,0.25,0.275,0.3,0.325,0.35,0.375,0.4,0.425,
0.45,0.475,0.5,0.525,0.55,0.575,0.6,0.625,0.65,0.675,0.7,0.725,0.75,0.775,
0.8,0.825,0.85,0.875,0.9,0.925,0.95,0.975,1.),.UNSPECIFIED.)
GEOMETRIC_REPRESENTATION_ITEM()
RATIONAL_B_SPLINE_SURFACE(((1.,0.996917333733128,1.,0.996917333733128,1.,
0.996917333733128,1.,0.996917333733128,1.,0.996917333733128,1.,0.996917333733128,
1.,0.996917333733128,1.,0.996917333733128,1.,0.996917333733128,1.,0.996917333733128,
1.,0.996917333733128,1.,0.996917333733128,1.,0.996917333733128,1.,0.996917333733128,
1.,0.996917333733128,1.,0.996917333733128,1.,0.996917333733128,1.,0.996917333733128,
1.,0.996917333733128,1.,0.996917333733128,1.,0.996917333733128,1.,0.996917333733128,
1.,0.996917333733128,1.,0.996917333733128,1.,0.996917333733128,1.,0.996917333733128,
1.,0.996917333733128,1.,0.996917333733128,1.,0.996917333733128,1.,0.996917333733128,
1.,0.996917333733128,1.,0.996917333733128,1.,0.996917333733128,1.,0.996917333733128,
1.,0.996917333733128,1.,0.996917333733128,1.,0.996917333733128,1.,0.996917333733128,
1.,0.996917333733128,1.,0.996917333733128,1.),(1.,0.996917333733128,1.,
0.996917333733128,1.,0.996917333733128,1.,0.996917333733128,1.,0.996917333733128,
1.,0.996917333733128,1.,0.996917333733128,1.,0.996917333733128,1.,0.996917333733128,
1.,0.996917333733128,1.,0.996917333733128,1.,0.996917333733128,1.,0.996917333733128,
1.,0.996917333733128,1.,0.996917333733128,1.,0.996917333733128,1.,0.996917333733128,
1.,0.996917333733128,1.,0.996917333733128,1.,0.996917333733128,1.,0.996917333733128,
1.,0.996917333733128,1.,0.996917333733128,1.,0.996917333733128,1.,0.996917333733128,
1.,0.996917333733128,1.,0.996917333733128,1.,0.996917333733128,1.,0.996917333733128,
1.,0.996917333733128,1.,0.996917333733128,1.,0.996917333733128,1.,0.996917333733128,
1.,0.996917333733128,1.,0.996917333733128,1.,0.996917333733128,1.,0.996917333733128,
1.,0.996917333733128,1.,0.996917333733128,1.,0.996917333733128,1.)))
REPRESENTATION_ITEM('')
SURFACE()
);
#4045=(
BOUNDED_SURFACE()
B_SPLINE_SURFACE(1,2,((#271725,#271726,#271727,#271728,#271729,#271730,
#271731,#271732,#271733,#271734,#271735,#271736,#271737,#271738,#271739,
#271740,#271741,#271742,#271743,#271744,#271745,#271746,#271747,#271748,
#271749,#271750,#271751,#271752,#271753,#271754,#271755,#271756,#271757,
#271758,#271759,#271760,#271761,#271762,#271763,#271764,#271765,#271766,
#271767,#271768,#271769,#271770,#271771,#271772,#271773,#271774,#271775,
#271776,#271777,#271778,#271779,#271780,#271781,#271782,#271783,#271784,
#271785,#271786,#271787,#271788,#271789,#271790,#271791,#271792,#271793,
#271794,#271795,#271796,#271797,#271798,#271799,#271800,#271801,#271802,
#271803,#271804,#271805),(#271806,#271807,#271808,#271809,#271810,#271811,
#271812,#271813,#271814,#271815,#271816,#271817,#271818,#271819,#271820,
#271821,#271822,#271823,#271824,#271825,#271826,#271827,#271828,#271829,
#271830,#271831,#271832,#271833,#271834,#271835,#271836,#271837,#271838,
#271839,#271840,#271841,#271842,#271843,#271844,#271845,#271846,#271847,
#271848,#271849,#271850,#271851,#271852,#271853,#271854,#271855,#271856,
#271857,#271858,#271859,#271860,#271861,#271862,#271863,#271864,#271865,
#271866,#271867,#271868,#271869,#271870,#271871,#271872,#271873,#271874,
#271875,#271876,#271877,#271878,#271879,#271880,#271881,#271882,#271883,
#271884,#271885,#271886)),.UNSPECIFIED.,.F.,.F.,.F.)
B_SPLINE_SURFACE_WITH_KNOTS((2,2),(3,2,2,2,2,2,2,2,2,2,2,2,2,2,2,2,2,2,
2,2,2,2,2,2,2,2,2,2,2,2,2,2,2,2,2,2,2,2,2,2,3),(0.,1.),(0.,0.025,0.05,0.075,
0.1,0.125,0.15,0.175,0.2,0.225,0.25,0.275,0.3,0.325,0.35,0.375,0.4,0.425,
0.45,0.475,0.5,0.525,0.55,0.575,0.6,0.625,0.65,0.675,0.7,0.725,0.75,0.775,
0.8,0.825,0.85,0.875,0.9,0.925,0.95,0.975,1.),.UNSPECIFIED.)
GEOMETRIC_REPRESENTATION_ITEM()
RATIONAL_B_SPLINE_SURFACE(((1.,0.996917333733128,1.,0.996917333733128,1.,
0.996917333733128,1.,0.996917333733128,1.,0.996917333733128,1.,0.996917333733128,
1.,0.996917333733128,1.,0.996917333733128,1.,0.996917333733128,1.,0.996917333733128,
1.,0.996917333733128,1.,0.996917333733128,1.,0.996917333733128,1.,0.996917333733128,
1.,0.996917333733128,1.,0.996917333733128,1.,0.996917333733128,1.,0.996917333733128,
1.,0.996917333733128,1.,0.996917333733128,1.,0.996917333733128,1.,0.996917333733128,
1.,0.996917333733128,1.,0.996917333733128,1.,0.996917333733128,1.,0.996917333733128,
1.,0.996917333733128,1.,0.996917333733128,1.,0.996917333733128,1.,0.996917333733128,
1.,0.996917333733128,1.,0.996917333733128,1.,0.996917333733128,1.,0.996917333733128,
1.,0.996917333733128,1.,0.996917333733128,1.,0.996917333733128,1.,0.996917333733128,
1.,0.996917333733128,1.,0.996917333733128,1.),(1.,0.996917333733128,1.,
0.996917333733128,1.,0.996917333733128,1.,0.996917333733128,1.,0.996917333733128,
1.,0.996917333733128,1.,0.996917333733128,1.,0.996917333733128,1.,0.996917333733128,
1.,0.996917333733128,1.,0.996917333733128,1.,0.996917333733128,1.,0.996917333733128,
1.,0.996917333733128,1.,0.996917333733128,1.,0.996917333733128,1.,0.996917333733128,
1.,0.996917333733128,1.,0.996917333733128,1.,0.996917333733128,1.,0.996917333733128,
1.,0.996917333733128,1.,0.996917333733128,1.,0.996917333733128,1.,0.996917333733128,
1.,0.996917333733128,1.,0.996917333733128,1.,0.996917333733128,1.,0.996917333733128,
1.,0.996917333733128,1.,0.996917333733128,1.,0.996917333733128,1.,0.996917333733128,
1.,0.996917333733128,1.,0.996917333733128,1.,0.996917333733128,1.,0.996917333733128,
1.,0.996917333733128,1.,0.996917333733128,1.,0.996917333733128,1.)))
REPRESENTATION_ITEM('')
SURFACE()
);
#4046=(
BOUNDED_SURFACE()
B_SPLINE_SURFACE(1,2,((#271888,#271889,#271890,#271891,#271892,#271893,
#271894,#271895,#271896,#271897,#271898,#271899,#271900,#271901,#271902,
#271903,#271904,#271905,#271906,#271907,#271908,#271909,#271910,#271911,
#271912,#271913,#271914,#271915,#271916,#271917,#271918,#271919,#271920,
#271921,#271922,#271923,#271924,#271925,#271926,#271927,#271928,#271929,
#271930,#271931,#271932,#271933,#271934,#271935,#271936,#271937,#271938,
#271939,#271940,#271941,#271942,#271943,#271944,#271945,#271946,#271947,
#271948,#271949,#271950,#271951,#271952,#271953,#271954,#271955,#271956,
#271957,#271958,#271959,#271960,#271961,#271962,#271963,#271964,#271965,
#271966,#271967,#271968),(#271969,#271970,#271971,#271972,#271973,#271974,
#271975,#271976,#271977,#271978,#271979,#271980,#271981,#271982,#271983,
#271984,#271985,#271986,#271987,#271988,#271989,#271990,#271991,#271992,
#271993,#271994,#271995,#271996,#271997,#271998,#271999,#272000,#272001,
#272002,#272003,#272004,#272005,#272006,#272007,#272008,#272009,#272010,
#272011,#272012,#272013,#272014,#272015,#272016,#272017,#272018,#272019,
#272020,#272021,#272022,#272023,#272024,#272025,#272026,#272027,#272028,
#272029,#272030,#272031,#272032,#272033,#272034,#272035,#272036,#272037,
#272038,#272039,#272040,#272041,#272042,#272043,#272044,#272045,#272046,
#272047,#272048,#272049)),.UNSPECIFIED.,.F.,.F.,.F.)
B_SPLINE_SURFACE_WITH_KNOTS((2,2),(3,2,2,2,2,2,2,2,2,2,2,2,2,2,2,2,2,2,
2,2,2,2,2,2,2,2,2,2,2,2,2,2,2,2,2,2,2,2,2,2,3),(0.,1.),(0.,0.025,0.05,0.075,
0.1,0.125,0.15,0.175,0.2,0.225,0.25,0.275,0.3,0.325,0.35,0.375,0.4,0.425,
0.45,0.475,0.5,0.525,0.55,0.575,0.6,0.625,0.65,0.675,0.7,0.725,0.75,0.775,
0.8,0.825,0.85,0.875,0.9,0.925,0.95,0.975,1.),.UNSPECIFIED.)
GEOMETRIC_REPRESENTATION_ITEM()
RATIONAL_B_SPLINE_SURFACE(((1.,0.996917333733128,1.,0.996917333733128,1.,
0.996917333733128,1.,0.996917333733128,1.,0.996917333733128,1.,0.996917333733128,
1.,0.996917333733128,1.,0.996917333733128,1.,0.996917333733128,1.,0.996917333733128,
1.,0.996917333733128,1.,0.996917333733128,1.,0.996917333733128,1.,0.996917333733128,
1.,0.996917333733128,1.,0.996917333733128,1.,0.996917333733128,1.,0.996917333733128,
1.,0.996917333733128,1.,0.996917333733128,1.,0.996917333733128,1.,0.996917333733128,
1.,0.996917333733128,1.,0.996917333733128,1.,0.996917333733128,1.,0.996917333733128,
1.,0.996917333733128,1.,0.996917333733128,1.,0.996917333733128,1.,0.996917333733128,
1.,0.996917333733128,1.,0.996917333733128,1.,0.996917333733128,1.,0.996917333733128,
1.,0.996917333733128,1.,0.996917333733128,1.,0.996917333733128,1.,0.996917333733128,
1.,0.996917333733128,1.,0.996917333733128,1.),(1.,0.996917333733128,1.,
0.996917333733128,1.,0.996917333733128,1.,0.996917333733128,1.,0.996917333733128,
1.,0.996917333733128,1.,0.996917333733128,1.,0.996917333733128,1.,0.996917333733128,
1.,0.996917333733128,1.,0.996917333733128,1.,0.996917333733128,1.,0.996917333733128,
1.,0.996917333733128,1.,0.996917333733128,1.,0.996917333733128,1.,0.996917333733128,
1.,0.996917333733128,1.,0.996917333733128,1.,0.996917333733128,1.,0.996917333733128,
1.,0.996917333733128,1.,0.996917333733128,1.,0.996917333733128,1.,0.996917333733128,
1.,0.996917333733128,1.,0.996917333733128,1.,0.996917333733128,1.,0.996917333733128,
1.,0.996917333733128,1.,0.996917333733128,1.,0.996917333733128,1.,0.996917333733128,
1.,0.996917333733128,1.,0.996917333733128,1.,0.996917333733128,1.,0.996917333733128,
1.,0.996917333733128,1.,0.996917333733128,1.,0.996917333733128,1.)))
REPRESENTATION_ITEM('')
SURFACE()
);
#4047=(
BOUNDED_SURFACE()
B_SPLINE_SURFACE(1,2,((#272050,#272051,#272052,#272053,#272054,#272055,
#272056,#272057,#272058,#272059,#272060,#272061,#272062,#272063,#272064,
#272065,#272066,#272067,#272068,#272069,#272070,#272071,#272072,#272073,
#272074,#272075,#272076,#272077,#272078,#272079,#272080,#272081,#272082,
#272083,#272084,#272085,#272086,#272087,#272088,#272089,#272090,#272091,
#272092,#272093,#272094,#272095,#272096,#272097,#272098,#272099,#272100,
#272101,#272102,#272103,#272104,#272105,#272106,#272107,#272108,#272109,
#272110,#272111,#272112,#272113,#272114,#272115,#272116,#272117,#272118,
#272119,#272120,#272121,#272122,#272123,#272124,#272125,#272126,#272127,
#272128,#272129,#272130),(#272131,#272132,#272133,#272134,#272135,#272136,
#272137,#272138,#272139,#272140,#272141,#272142,#272143,#272144,#272145,
#272146,#272147,#272148,#272149,#272150,#272151,#272152,#272153,#272154,
#272155,#272156,#272157,#272158,#272159,#272160,#272161,#272162,#272163,
#272164,#272165,#272166,#272167,#272168,#272169,#272170,#272171,#272172,
#272173,#272174,#272175,#272176,#272177,#272178,#272179,#272180,#272181,
#272182,#272183,#272184,#272185,#272186,#272187,#272188,#272189,#272190,
#272191,#272192,#272193,#272194,#272195,#272196,#272197,#272198,#272199,
#272200,#272201,#272202,#272203,#272204,#272205,#272206,#272207,#272208,
#272209,#272210,#272211)),.UNSPECIFIED.,.F.,.F.,.F.)
B_SPLINE_SURFACE_WITH_KNOTS((2,2),(3,2,2,2,2,2,2,2,2,2,2,2,2,2,2,2,2,2,
2,2,2,2,2,2,2,2,2,2,2,2,2,2,2,2,2,2,2,2,2,2,3),(0.,1.),(0.,0.025,0.05,0.075,
0.1,0.125,0.15,0.175,0.2,0.225,0.25,0.275,0.3,0.325,0.35,0.375,0.4,0.425,
0.45,0.475,0.5,0.525,0.55,0.575,0.6,0.625,0.65,0.675,0.7,0.725,0.75,0.775,
0.8,0.825,0.85,0.875,0.9,0.925,0.95,0.975,1.),.UNSPECIFIED.)
GEOMETRIC_REPRESENTATION_ITEM()
RATIONAL_B_SPLINE_SURFACE(((1.,0.996917333733128,1.,0.996917333733128,1.,
0.996917333733128,1.,0.996917333733128,1.,0.996917333733128,1.,0.996917333733128,
1.,0.996917333733128,1.,0.996917333733128,1.,0.996917333733128,1.,0.996917333733128,
1.,0.996917333733128,1.,0.996917333733128,1.,0.996917333733128,1.,0.996917333733128,
1.,0.996917333733128,1.,0.996917333733128,1.,0.996917333733128,1.,0.996917333733128,
1.,0.996917333733128,1.,0.996917333733128,1.,0.996917333733128,1.,0.996917333733128,
1.,0.996917333733128,1.,0.996917333733128,1.,0.996917333733128,1.,0.996917333733128,
1.,0.996917333733128,1.,0.996917333733128,1.,0.996917333733128,1.,0.996917333733128,
1.,0.996917333733128,1.,0.996917333733128,1.,0.996917333733128,1.,0.996917333733128,
1.,0.996917333733128,1.,0.996917333733128,1.,0.996917333733128,1.,0.996917333733128,
1.,0.996917333733128,1.,0.996917333733128,1.),(1.,0.996917333733128,1.,
0.996917333733128,1.,0.996917333733128,1.,0.996917333733128,1.,0.996917333733128,
1.,0.996917333733128,1.,0.996917333733128,1.,0.996917333733128,1.,0.996917333733128,
1.,0.996917333733128,1.,0.996917333733128,1.,0.996917333733128,1.,0.996917333733128,
1.,0.996917333733128,1.,0.996917333733128,1.,0.996917333733128,1.,0.996917333733128,
1.,0.996917333733128,1.,0.996917333733128,1.,0.996917333733128,1.,0.996917333733128,
1.,0.996917333733128,1.,0.996917333733128,1.,0.996917333733128,1.,0.996917333733128,
1.,0.996917333733128,1.,0.996917333733128,1.,0.996917333733128,1.,0.996917333733128,
1.,0.996917333733128,1.,0.996917333733128,1.,0.996917333733128,1.,0.996917333733128,
1.,0.996917333733128,1.,0.996917333733128,1.,0.996917333733128,1.,0.996917333733128,
1.,0.996917333733128,1.,0.996917333733128,1.,0.996917333733128,1.)))
REPRESENTATION_ITEM('')
SURFACE()
);
#4048=(
BOUNDED_SURFACE()
B_SPLINE_SURFACE(1,2,((#272213,#272214,#272215,#272216,#272217,#272218,
#272219,#272220,#272221,#272222,#272223,#272224,#272225,#272226,#272227,
#272228,#272229,#272230,#272231,#272232,#272233,#272234,#272235,#272236,
#272237,#272238,#272239,#272240,#272241,#272242,#272243,#272244,#272245,
#272246,#272247,#272248,#272249,#272250,#272251,#272252,#272253,#272254,
#272255,#272256,#272257,#272258,#272259,#272260,#272261,#272262,#272263,
#272264,#272265,#272266,#272267,#272268,#272269,#272270,#272271,#272272,
#272273,#272274,#272275,#272276,#272277,#272278,#272279,#272280,#272281,
#272282,#272283,#272284,#272285,#272286,#272287,#272288,#272289,#272290,
#272291,#272292,#272293),(#272294,#272295,#272296,#272297,#272298,#272299,
#272300,#272301,#272302,#272303,#272304,#272305,#272306,#272307,#272308,
#272309,#272310,#272311,#272312,#272313,#272314,#272315,#272316,#272317,
#272318,#272319,#272320,#272321,#272322,#272323,#272324,#272325,#272326,
#272327,#272328,#272329,#272330,#272331,#272332,#272333,#272334,#272335,
#272336,#272337,#272338,#272339,#272340,#272341,#272342,#272343,#272344,
#272345,#272346,#272347,#272348,#272349,#272350,#272351,#272352,#272353,
#272354,#272355,#272356,#272357,#272358,#272359,#272360,#272361,#272362,
#272363,#272364,#272365,#272366,#272367,#272368,#272369,#272370,#272371,
#272372,#272373,#272374)),.UNSPECIFIED.,.F.,.F.,.F.)
B_SPLINE_SURFACE_WITH_KNOTS((2,2),(3,2,2,2,2,2,2,2,2,2,2,2,2,2,2,2,2,2,
2,2,2,2,2,2,2,2,2,2,2,2,2,2,2,2,2,2,2,2,2,2,3),(0.,1.),(0.,0.025,0.05,0.075,
0.1,0.125,0.15,0.175,0.2,0.225,0.25,0.275,0.3,0.325,0.35,0.375,0.4,0.425,
0.45,0.475,0.5,0.525,0.55,0.575,0.6,0.625,0.65,0.675,0.7,0.725,0.75,0.775,
0.8,0.825,0.85,0.875,0.9,0.925,0.95,0.975,1.),.UNSPECIFIED.)
GEOMETRIC_REPRESENTATION_ITEM()
RATIONAL_B_SPLINE_SURFACE(((1.,0.996917333733128,1.,0.996917333733128,1.,
0.996917333733128,1.,0.996917333733128,1.,0.996917333733128,1.,0.996917333733128,
1.,0.996917333733128,1.,0.996917333733128,1.,0.996917333733128,1.,0.996917333733128,
1.,0.996917333733128,1.,0.996917333733128,1.,0.996917333733128,1.,0.996917333733128,
1.,0.996917333733128,1.,0.996917333733128,1.,0.996917333733128,1.,0.996917333733128,
1.,0.996917333733128,1.,0.996917333733128,1.,0.996917333733128,1.,0.996917333733128,
1.,0.996917333733128,1.,0.996917333733128,1.,0.996917333733128,1.,0.996917333733128,
1.,0.996917333733128,1.,0.996917333733128,1.,0.996917333733128,1.,0.996917333733128,
1.,0.996917333733128,1.,0.996917333733128,1.,0.996917333733128,1.,0.996917333733128,
1.,0.996917333733128,1.,0.996917333733128,1.,0.996917333733128,1.,0.996917333733128,
1.,0.996917333733128,1.,0.996917333733128,1.),(1.,0.996917333733128,1.,
0.996917333733128,1.,0.996917333733128,1.,0.996917333733128,1.,0.996917333733128,
1.,0.996917333733128,1.,0.996917333733128,1.,0.996917333733128,1.,0.996917333733128,
1.,0.996917333733128,1.,0.996917333733128,1.,0.996917333733128,1.,0.996917333733128,
1.,0.996917333733128,1.,0.996917333733128,1.,0.996917333733128,1.,0.996917333733128,
1.,0.996917333733128,1.,0.996917333733128,1.,0.996917333733128,1.,0.996917333733128,
1.,0.996917333733128,1.,0.996917333733128,1.,0.996917333733128,1.,0.996917333733128,
1.,0.996917333733128,1.,0.996917333733128,1.,0.996917333733128,1.,0.996917333733128,
1.,0.996917333733128,1.,0.996917333733128,1.,0.996917333733128,1.,0.996917333733128,
1.,0.996917333733128,1.,0.996917333733128,1.,0.996917333733128,1.,0.996917333733128,
1.,0.996917333733128,1.,0.996917333733128,1.,0.996917333733128,1.)))
REPRESENTATION_ITEM('')
SURFACE()
);
#4049=(
BOUNDED_SURFACE()
B_SPLINE_SURFACE(1,2,((#272391,#272392,#272393,#272394,#272395,#272396,
#272397,#272398,#272399,#272400,#272401,#272402,#272403,#272404,#272405,
#272406,#272407,#272408,#272409,#272410,#272411,#272412,#272413,#272414,
#272415,#272416,#272417,#272418,#272419,#272420,#272421,#272422,#272423,
#272424,#272425,#272426,#272427,#272428,#272429,#272430,#272431,#272432,
#272433,#272434,#272435,#272436,#272437,#272438,#272439,#272440,#272441,
#272442,#272443,#272444,#272445,#272446,#272447,#272448,#272449,#272450,
#272451,#272452,#272453,#272454,#272455,#272456,#272457,#272458,#272459,
#272460,#272461,#272462,#272463,#272464,#272465,#272466,#272467,#272468,
#272469,#272470,#272471),(#272472,#272473,#272474,#272475,#272476,#272477,
#272478,#272479,#272480,#272481,#272482,#272483,#272484,#272485,#272486,
#272487,#272488,#272489,#272490,#272491,#272492,#272493,#272494,#272495,
#272496,#272497,#272498,#272499,#272500,#272501,#272502,#272503,#272504,
#272505,#272506,#272507,#272508,#272509,#272510,#272511,#272512,#272513,
#272514,#272515,#272516,#272517,#272518,#272519,#272520,#272521,#272522,
#272523,#272524,#272525,#272526,#272527,#272528,#272529,#272530,#272531,
#272532,#272533,#272534,#272535,#272536,#272537,#272538,#272539,#272540,
#272541,#272542,#272543,#272544,#272545,#272546,#272547,#272548,#272549,
#272550,#272551,#272552)),.UNSPECIFIED.,.F.,.F.,.F.)
B_SPLINE_SURFACE_WITH_KNOTS((2,2),(3,2,2,2,2,2,2,2,2,2,2,2,2,2,2,2,2,2,
2,2,2,2,2,2,2,2,2,2,2,2,2,2,2,2,2,2,2,2,2,2,3),(0.,1.),(0.,0.025,0.05,0.075,
0.1,0.125,0.15,0.175,0.2,0.225,0.25,0.275,0.3,0.325,0.35,0.375,0.4,0.425,
0.45,0.475,0.5,0.525,0.55,0.575,0.6,0.625,0.65,0.675,0.7,0.725,0.75,0.775,
0.8,0.825,0.85,0.875,0.9,0.925,0.95,0.975,1.),.UNSPECIFIED.)
GEOMETRIC_REPRESENTATION_ITEM()
RATIONAL_B_SPLINE_SURFACE(((1.,0.996917333733128,1.,0.996917333733128,1.,
0.996917333733128,1.,0.996917333733128,1.,0.996917333733128,1.,0.996917333733128,
1.,0.996917333733128,1.,0.996917333733128,1.,0.996917333733128,1.,0.996917333733128,
1.,0.996917333733128,1.,0.996917333733128,1.,0.996917333733128,1.,0.996917333733128,
1.,0.996917333733128,1.,0.996917333733128,1.,0.996917333733128,1.,0.996917333733128,
1.,0.996917333733128,1.,0.996917333733128,1.,0.996917333733128,1.,0.996917333733128,
1.,0.996917333733128,1.,0.996917333733128,1.,0.996917333733128,1.,0.996917333733128,
1.,0.996917333733128,1.,0.996917333733128,1.,0.996917333733128,1.,0.996917333733128,
1.,0.996917333733128,1.,0.996917333733128,1.,0.996917333733128,1.,0.996917333733128,
1.,0.996917333733128,1.,0.996917333733128,1.,0.996917333733128,1.,0.996917333733128,
1.,0.996917333733128,1.,0.996917333733128,1.),(1.,0.996917333733128,1.,
0.996917333733128,1.,0.996917333733128,1.,0.996917333733128,1.,0.996917333733128,
1.,0.996917333733128,1.,0.996917333733128,1.,0.996917333733128,1.,0.996917333733128,
1.,0.996917333733128,1.,0.996917333733128,1.,0.996917333733128,1.,0.996917333733128,
1.,0.996917333733128,1.,0.996917333733128,1.,0.996917333733128,1.,0.996917333733128,
1.,0.996917333733128,1.,0.996917333733128,1.,0.996917333733128,1.,0.996917333733128,
1.,0.996917333733128,1.,0.996917333733128,1.,0.996917333733128,1.,0.996917333733128,
1.,0.996917333733128,1.,0.996917333733128,1.,0.996917333733128,1.,0.996917333733128,
1.,0.996917333733128,1.,0.996917333733128,1.,0.996917333733128,1.,0.996917333733128,
1.,0.996917333733128,1.,0.996917333733128,1.,0.996917333733128,1.,0.996917333733128,
1.,0.996917333733128,1.,0.996917333733128,1.,0.996917333733128,1.)))
REPRESENTATION_ITEM('')
SURFACE()
);
#4050=(
BOUNDED_SURFACE()
B_SPLINE_SURFACE(1,2,((#272554,#272555,#272556,#272557,#272558,#272559,
#272560,#272561,#272562,#272563,#272564,#272565,#272566,#272567,#272568,
#272569,#272570,#272571,#272572,#272573,#272574,#272575,#272576,#272577,
#272578,#272579,#272580,#272581,#272582,#272583,#272584,#272585,#272586,
#272587,#272588,#272589,#272590,#272591,#272592,#272593,#272594,#272595,
#272596,#272597,#272598,#272599,#272600,#272601,#272602,#272603,#272604,
#272605,#272606,#272607,#272608,#272609,#272610,#272611,#272612,#272613,
#272614,#272615,#272616,#272617,#272618,#272619,#272620,#272621,#272622,
#272623,#272624,#272625,#272626,#272627,#272628,#272629,#272630,#272631,
#272632,#272633,#272634),(#272635,#272636,#272637,#272638,#272639,#272640,
#272641,#272642,#272643,#272644,#272645,#272646,#272647,#272648,#272649,
#272650,#272651,#272652,#272653,#272654,#272655,#272656,#272657,#272658,
#272659,#272660,#272661,#272662,#272663,#272664,#272665,#272666,#272667,
#272668,#272669,#272670,#272671,#272672,#272673,#272674,#272675,#272676,
#272677,#272678,#272679,#272680,#272681,#272682,#272683,#272684,#272685,
#272686,#272687,#272688,#272689,#272690,#272691,#272692,#272693,#272694,
#272695,#272696,#272697,#272698,#272699,#272700,#272701,#272702,#272703,
#272704,#272705,#272706,#272707,#272708,#272709,#272710,#272711,#272712,
#272713,#272714,#272715)),.UNSPECIFIED.,.F.,.F.,.F.)
B_SPLINE_SURFACE_WITH_KNOTS((2,2),(3,2,2,2,2,2,2,2,2,2,2,2,2,2,2,2,2,2,
2,2,2,2,2,2,2,2,2,2,2,2,2,2,2,2,2,2,2,2,2,2,3),(0.,1.),(0.,0.025,0.05,0.075,
0.1,0.125,0.15,0.175,0.2,0.225,0.25,0.275,0.3,0.325,0.35,0.375,0.4,0.425,
0.45,0.475,0.5,0.525,0.55,0.575,0.6,0.625,0.65,0.675,0.7,0.725,0.75,0.775,
0.8,0.825,0.85,0.875,0.9,0.925,0.95,0.975,1.),.UNSPECIFIED.)
GEOMETRIC_REPRESENTATION_ITEM()
RATIONAL_B_SPLINE_SURFACE(((1.,0.996917333733128,1.,0.996917333733128,1.,
0.996917333733128,1.,0.996917333733128,1.,0.996917333733128,1.,0.996917333733128,
1.,0.996917333733128,1.,0.996917333733128,1.,0.996917333733128,1.,0.996917333733128,
1.,0.996917333733128,1.,0.996917333733128,1.,0.996917333733128,1.,0.996917333733128,
1.,0.996917333733128,1.,0.996917333733128,1.,0.996917333733128,1.,0.996917333733128,
1.,0.996917333733128,1.,0.996917333733128,1.,0.996917333733128,1.,0.996917333733128,
1.,0.996917333733128,1.,0.996917333733128,1.,0.996917333733128,1.,0.996917333733128,
1.,0.996917333733128,1.,0.996917333733128,1.,0.996917333733128,1.,0.996917333733128,
1.,0.996917333733128,1.,0.996917333733128,1.,0.996917333733128,1.,0.996917333733128,
1.,0.996917333733128,1.,0.996917333733128,1.,0.996917333733128,1.,0.996917333733128,
1.,0.996917333733128,1.,0.996917333733128,1.),(1.,0.996917333733128,1.,
0.996917333733128,1.,0.996917333733128,1.,0.996917333733128,1.,0.996917333733128,
1.,0.996917333733128,1.,0.996917333733128,1.,0.996917333733128,1.,0.996917333733128,
1.,0.996917333733128,1.,0.996917333733128,1.,0.996917333733128,1.,0.996917333733128,
1.,0.996917333733128,1.,0.996917333733128,1.,0.996917333733128,1.,0.996917333733128,
1.,0.996917333733128,1.,0.996917333733128,1.,0.996917333733128,1.,0.996917333733128,
1.,0.996917333733128,1.,0.996917333733128,1.,0.996917333733128,1.,0.996917333733128,
1.,0.996917333733128,1.,0.996917333733128,1.,0.996917333733128,1.,0.996917333733128,
1.,0.996917333733128,1.,0.996917333733128,1.,0.996917333733128,1.,0.996917333733128,
1.,0.996917333733128,1.,0.996917333733128,1.,0.996917333733128,1.,0.996917333733128,
1.,0.996917333733128,1.,0.996917333733128,1.,0.996917333733128,1.)))
REPRESENTATION_ITEM('')
SURFACE()
);
#4051=(
BOUNDED_SURFACE()
B_SPLINE_SURFACE(1,2,((#272732,#272733,#272734,#272735,#272736,#272737,
#272738,#272739,#272740,#272741,#272742,#272743,#272744,#272745,#272746,
#272747,#272748,#272749,#272750,#272751,#272752,#272753,#272754,#272755,
#272756,#272757,#272758,#272759,#272760,#272761,#272762,#272763,#272764,
#272765,#272766,#272767,#272768,#272769,#272770,#272771,#272772,#272773,
#272774,#272775,#272776,#272777,#272778,#272779,#272780,#272781,#272782,
#272783,#272784,#272785,#272786,#272787,#272788,#272789,#272790,#272791,
#272792,#272793,#272794,#272795,#272796,#272797,#272798,#272799,#272800,
#272801,#272802,#272803,#272804,#272805,#272806,#272807,#272808,#272809,
#272810,#272811,#272812),(#272813,#272814,#272815,#272816,#272817,#272818,
#272819,#272820,#272821,#272822,#272823,#272824,#272825,#272826,#272827,
#272828,#272829,#272830,#272831,#272832,#272833,#272834,#272835,#272836,
#272837,#272838,#272839,#272840,#272841,#272842,#272843,#272844,#272845,
#272846,#272847,#272848,#272849,#272850,#272851,#272852,#272853,#272854,
#272855,#272856,#272857,#272858,#272859,#272860,#272861,#272862,#272863,
#272864,#272865,#272866,#272867,#272868,#272869,#272870,#272871,#272872,
#272873,#272874,#272875,#272876,#272877,#272878,#272879,#272880,#272881,
#272882,#272883,#272884,#272885,#272886,#272887,#272888,#272889,#272890,
#272891,#272892,#272893)),.UNSPECIFIED.,.F.,.F.,.F.)
B_SPLINE_SURFACE_WITH_KNOTS((2,2),(3,2,2,2,2,2,2,2,2,2,2,2,2,2,2,2,2,2,
2,2,2,2,2,2,2,2,2,2,2,2,2,2,2,2,2,2,2,2,2,2,3),(0.,1.),(0.,0.025,0.05,0.075,
0.1,0.125,0.15,0.175,0.2,0.225,0.25,0.275,0.3,0.325,0.35,0.375,0.4,0.425,
0.45,0.475,0.5,0.525,0.55,0.575,0.6,0.625,0.65,0.675,0.7,0.725,0.75,0.775,
0.8,0.825,0.85,0.875,0.9,0.925,0.95,0.975,1.),.UNSPECIFIED.)
GEOMETRIC_REPRESENTATION_ITEM()
RATIONAL_B_SPLINE_SURFACE(((1.,0.996917333733128,1.,0.996917333733128,1.,
0.996917333733128,1.,0.996917333733128,1.,0.996917333733128,1.,0.996917333733128,
1.,0.996917333733128,1.,0.996917333733128,1.,0.996917333733128,1.,0.996917333733128,
1.,0.996917333733128,1.,0.996917333733128,1.,0.996917333733128,1.,0.996917333733128,
1.,0.996917333733128,1.,0.996917333733128,1.,0.996917333733128,1.,0.996917333733128,
1.,0.996917333733128,1.,0.996917333733128,1.,0.996917333733128,1.,0.996917333733128,
1.,0.996917333733128,1.,0.996917333733128,1.,0.996917333733128,1.,0.996917333733128,
1.,0.996917333733128,1.,0.996917333733128,1.,0.996917333733128,1.,0.996917333733128,
1.,0.996917333733128,1.,0.996917333733128,1.,0.996917333733128,1.,0.996917333733128,
1.,0.996917333733128,1.,0.996917333733128,1.,0.996917333733128,1.,0.996917333733128,
1.,0.996917333733128,1.,0.996917333733128,1.),(1.,0.996917333733128,1.,
0.996917333733128,1.,0.996917333733128,1.,0.996917333733128,1.,0.996917333733128,
1.,0.996917333733128,1.,0.996917333733128,1.,0.996917333733128,1.,0.996917333733128,
1.,0.996917333733128,1.,0.996917333733128,1.,0.996917333733128,1.,0.996917333733128,
1.,0.996917333733128,1.,0.996917333733128,1.,0.996917333733128,1.,0.996917333733128,
1.,0.996917333733128,1.,0.996917333733128,1.,0.996917333733128,1.,0.996917333733128,
1.,0.996917333733128,1.,0.996917333733128,1.,0.996917333733128,1.,0.996917333733128,
1.,0.996917333733128,1.,0.996917333733128,1.,0.996917333733128,1.,0.996917333733128,
1.,0.996917333733128,1.,0.996917333733128,1.,0.996917333733128,1.,0.996917333733128,
1.,0.996917333733128,1.,0.996917333733128,1.,0.996917333733128,1.,0.996917333733128,
1.,0.996917333733128,1.,0.996917333733128,1.,0.996917333733128,1.)))
REPRESENTATION_ITEM('')
SURFACE()
);
#4052=(
BOUNDED_SURFACE()
B_SPLINE_SURFACE(1,2,((#272895,#272896,#272897,#272898,#272899,#272900,
#272901,#272902,#272903,#272904,#272905,#272906,#272907,#272908,#272909,
#272910,#272911,#272912,#272913,#272914,#272915,#272916,#272917,#272918,
#272919,#272920,#272921,#272922,#272923,#272924,#272925,#272926,#272927,
#272928,#272929,#272930,#272931,#272932,#272933,#272934,#272935,#272936,
#272937,#272938,#272939,#272940,#272941,#272942,#272943,#272944,#272945,
#272946,#272947,#272948,#272949,#272950,#272951,#272952,#272953,#272954,
#272955,#272956,#272957,#272958,#272959,#272960,#272961,#272962,#272963,
#272964,#272965,#272966,#272967,#272968,#272969,#272970,#272971,#272972,
#272973,#272974,#272975),(#272976,#272977,#272978,#272979,#272980,#272981,
#272982,#272983,#272984,#272985,#272986,#272987,#272988,#272989,#272990,
#272991,#272992,#272993,#272994,#272995,#272996,#272997,#272998,#272999,
#273000,#273001,#273002,#273003,#273004,#273005,#273006,#273007,#273008,
#273009,#273010,#273011,#273012,#273013,#273014,#273015,#273016,#273017,
#273018,#273019,#273020,#273021,#273022,#273023,#273024,#273025,#273026,
#273027,#273028,#273029,#273030,#273031,#273032,#273033,#273034,#273035,
#273036,#273037,#273038,#273039,#273040,#273041,#273042,#273043,#273044,
#273045,#273046,#273047,#273048,#273049,#273050,#273051,#273052,#273053,
#273054,#273055,#273056)),.UNSPECIFIED.,.F.,.F.,.F.)
B_SPLINE_SURFACE_WITH_KNOTS((2,2),(3,2,2,2,2,2,2,2,2,2,2,2,2,2,2,2,2,2,
2,2,2,2,2,2,2,2,2,2,2,2,2,2,2,2,2,2,2,2,2,2,3),(0.,1.),(0.,0.025,0.05,0.075,
0.1,0.125,0.15,0.175,0.2,0.225,0.25,0.275,0.3,0.325,0.35,0.375,0.4,0.425,
0.45,0.475,0.5,0.525,0.55,0.575,0.6,0.625,0.65,0.675,0.7,0.725,0.75,0.775,
0.8,0.825,0.85,0.875,0.9,0.925,0.95,0.975,1.),.UNSPECIFIED.)
GEOMETRIC_REPRESENTATION_ITEM()
RATIONAL_B_SPLINE_SURFACE(((1.,0.996917333733128,1.,0.996917333733128,1.,
0.996917333733128,1.,0.996917333733128,1.,0.996917333733128,1.,0.996917333733128,
1.,0.996917333733128,1.,0.996917333733128,1.,0.996917333733128,1.,0.996917333733128,
1.,0.996917333733128,1.,0.996917333733128,1.,0.996917333733128,1.,0.996917333733128,
1.,0.996917333733128,1.,0.996917333733128,1.,0.996917333733128,1.,0.996917333733128,
1.,0.996917333733128,1.,0.996917333733128,1.,0.996917333733128,1.,0.996917333733128,
1.,0.996917333733128,1.,0.996917333733128,1.,0.996917333733128,1.,0.996917333733128,
1.,0.996917333733128,1.,0.996917333733128,1.,0.996917333733128,1.,0.996917333733128,
1.,0.996917333733128,1.,0.996917333733128,1.,0.996917333733128,1.,0.996917333733128,
1.,0.996917333733128,1.,0.996917333733128,1.,0.996917333733128,1.,0.996917333733128,
1.,0.996917333733128,1.,0.996917333733128,1.),(1.,0.996917333733128,1.,
0.996917333733128,1.,0.996917333733128,1.,0.996917333733128,1.,0.996917333733128,
1.,0.996917333733128,1.,0.996917333733128,1.,0.996917333733128,1.,0.996917333733128,
1.,0.996917333733128,1.,0.996917333733128,1.,0.996917333733128,1.,0.996917333733128,
1.,0.996917333733128,1.,0.996917333733128,1.,0.996917333733128,1.,0.996917333733128,
1.,0.996917333733128,1.,0.996917333733128,1.,0.996917333733128,1.,0.996917333733128,
1.,0.996917333733128,1.,0.996917333733128,1.,0.996917333733128,1.,0.996917333733128,
1.,0.996917333733128,1.,0.996917333733128,1.,0.996917333733128,1.,0.996917333733128,
1.,0.996917333733128,1.,0.996917333733128,1.,0.996917333733128,1.,0.996917333733128,
1.,0.996917333733128,1.,0.996917333733128,1.,0.996917333733128,1.,0.996917333733128,
1.,0.996917333733128,1.,0.996917333733128,1.,0.996917333733128,1.)))
REPRESENTATION_ITEM('')
SURFACE()
);
#4053=(
BOUNDED_SURFACE()
B_SPLINE_SURFACE(1,2,((#273073,#273074,#273075,#273076,#273077,#273078,
#273079,#273080,#273081,#273082,#273083,#273084,#273085,#273086,#273087,
#273088,#273089,#273090,#273091,#273092,#273093,#273094,#273095,#273096,
#273097,#273098,#273099,#273100,#273101,#273102,#273103,#273104,#273105,
#273106,#273107,#273108,#273109,#273110,#273111,#273112,#273113,#273114,
#273115,#273116,#273117,#273118,#273119,#273120,#273121,#273122,#273123,
#273124,#273125,#273126,#273127,#273128,#273129,#273130,#273131,#273132,
#273133,#273134,#273135,#273136,#273137,#273138,#273139,#273140,#273141,
#273142,#273143,#273144,#273145,#273146,#273147,#273148,#273149,#273150,
#273151,#273152,#273153),(#273154,#273155,#273156,#273157,#273158,#273159,
#273160,#273161,#273162,#273163,#273164,#273165,#273166,#273167,#273168,
#273169,#273170,#273171,#273172,#273173,#273174,#273175,#273176,#273177,
#273178,#273179,#273180,#273181,#273182,#273183,#273184,#273185,#273186,
#273187,#273188,#273189,#273190,#273191,#273192,#273193,#273194,#273195,
#273196,#273197,#273198,#273199,#273200,#273201,#273202,#273203,#273204,
#273205,#273206,#273207,#273208,#273209,#273210,#273211,#273212,#273213,
#273214,#273215,#273216,#273217,#273218,#273219,#273220,#273221,#273222,
#273223,#273224,#273225,#273226,#273227,#273228,#273229,#273230,#273231,
#273232,#273233,#273234)),.UNSPECIFIED.,.F.,.F.,.F.)
B_SPLINE_SURFACE_WITH_KNOTS((2,2),(3,2,2,2,2,2,2,2,2,2,2,2,2,2,2,2,2,2,
2,2,2,2,2,2,2,2,2,2,2,2,2,2,2,2,2,2,2,2,2,2,3),(0.,1.),(0.,0.025,0.05,0.075,
0.1,0.125,0.15,0.175,0.2,0.225,0.25,0.275,0.3,0.325,0.35,0.375,0.4,0.425,
0.45,0.475,0.5,0.525,0.55,0.575,0.6,0.625,0.65,0.675,0.7,0.725,0.75,0.775,
0.8,0.825,0.85,0.875,0.9,0.925,0.95,0.975,1.),.UNSPECIFIED.)
GEOMETRIC_REPRESENTATION_ITEM()
RATIONAL_B_SPLINE_SURFACE(((1.,0.996917333733128,1.,0.996917333733128,1.,
0.996917333733128,1.,0.996917333733128,1.,0.996917333733128,1.,0.996917333733128,
1.,0.996917333733128,1.,0.996917333733128,1.,0.996917333733128,1.,0.996917333733128,
1.,0.996917333733128,1.,0.996917333733128,1.,0.996917333733128,1.,0.996917333733128,
1.,0.996917333733128,1.,0.996917333733128,1.,0.996917333733128,1.,0.996917333733128,
1.,0.996917333733128,1.,0.996917333733128,1.,0.996917333733128,1.,0.996917333733128,
1.,0.996917333733128,1.,0.996917333733128,1.,0.996917333733128,1.,0.996917333733128,
1.,0.996917333733128,1.,0.996917333733128,1.,0.996917333733128,1.,0.996917333733128,
1.,0.996917333733128,1.,0.996917333733128,1.,0.996917333733128,1.,0.996917333733128,
1.,0.996917333733128,1.,0.996917333733128,1.,0.996917333733128,1.,0.996917333733128,
1.,0.996917333733128,1.,0.996917333733128,1.),(1.,0.996917333733128,1.,
0.996917333733128,1.,0.996917333733128,1.,0.996917333733128,1.,0.996917333733128,
1.,0.996917333733128,1.,0.996917333733128,1.,0.996917333733128,1.,0.996917333733128,
1.,0.996917333733128,1.,0.996917333733128,1.,0.996917333733128,1.,0.996917333733128,
1.,0.996917333733128,1.,0.996917333733128,1.,0.996917333733128,1.,0.996917333733128,
1.,0.996917333733128,1.,0.996917333733128,1.,0.996917333733128,1.,0.996917333733128,
1.,0.996917333733128,1.,0.996917333733128,1.,0.996917333733128,1.,0.996917333733128,
1.,0.996917333733128,1.,0.996917333733128,1.,0.996917333733128,1.,0.996917333733128,
1.,0.996917333733128,1.,0.996917333733128,1.,0.996917333733128,1.,0.996917333733128,
1.,0.996917333733128,1.,0.996917333733128,1.,0.996917333733128,1.,0.996917333733128,
1.,0.996917333733128,1.,0.996917333733128,1.,0.996917333733128,1.)))
REPRESENTATION_ITEM('')
SURFACE()
);
#4054=(
BOUNDED_SURFACE()
B_SPLINE_SURFACE(1,2,((#273236,#273237,#273238,#273239,#273240,#273241,
#273242,#273243,#273244,#273245,#273246,#273247,#273248,#273249,#273250,
#273251,#273252,#273253,#273254,#273255,#273256,#273257,#273258,#273259,
#273260,#273261,#273262,#273263,#273264,#273265,#273266,#273267,#273268,
#273269,#273270,#273271,#273272,#273273,#273274,#273275,#273276,#273277,
#273278,#273279,#273280,#273281,#273282,#273283,#273284,#273285,#273286,
#273287,#273288,#273289,#273290,#273291,#273292,#273293,#273294,#273295,
#273296,#273297,#273298,#273299,#273300,#273301,#273302,#273303,#273304,
#273305,#273306,#273307,#273308,#273309,#273310,#273311,#273312,#273313,
#273314,#273315,#273316),(#273317,#273318,#273319,#273320,#273321,#273322,
#273323,#273324,#273325,#273326,#273327,#273328,#273329,#273330,#273331,
#273332,#273333,#273334,#273335,#273336,#273337,#273338,#273339,#273340,
#273341,#273342,#273343,#273344,#273345,#273346,#273347,#273348,#273349,
#273350,#273351,#273352,#273353,#273354,#273355,#273356,#273357,#273358,
#273359,#273360,#273361,#273362,#273363,#273364,#273365,#273366,#273367,
#273368,#273369,#273370,#273371,#273372,#273373,#273374,#273375,#273376,
#273377,#273378,#273379,#273380,#273381,#273382,#273383,#273384,#273385,
#273386,#273387,#273388,#273389,#273390,#273391,#273392,#273393,#273394,
#273395,#273396,#273397)),.UNSPECIFIED.,.F.,.F.,.F.)
B_SPLINE_SURFACE_WITH_KNOTS((2,2),(3,2,2,2,2,2,2,2,2,2,2,2,2,2,2,2,2,2,
2,2,2,2,2,2,2,2,2,2,2,2,2,2,2,2,2,2,2,2,2,2,3),(0.,1.),(0.,0.025,0.05,0.075,
0.1,0.125,0.15,0.175,0.2,0.225,0.25,0.275,0.3,0.325,0.35,0.375,0.4,0.425,
0.45,0.475,0.5,0.525,0.55,0.575,0.6,0.625,0.65,0.675,0.7,0.725,0.75,0.775,
0.8,0.825,0.85,0.875,0.9,0.925,0.95,0.975,1.),.UNSPECIFIED.)
GEOMETRIC_REPRESENTATION_ITEM()
RATIONAL_B_SPLINE_SURFACE(((1.,0.996917333733128,1.,0.996917333733128,1.,
0.996917333733128,1.,0.996917333733128,1.,0.996917333733128,1.,0.996917333733128,
1.,0.996917333733128,1.,0.996917333733128,1.,0.996917333733128,1.,0.996917333733128,
1.,0.996917333733128,1.,0.996917333733128,1.,0.996917333733128,1.,0.996917333733128,
1.,0.996917333733128,1.,0.996917333733128,1.,0.996917333733128,1.,0.996917333733128,
1.,0.996917333733128,1.,0.996917333733128,1.,0.996917333733128,1.,0.996917333733128,
1.,0.996917333733128,1.,0.996917333733128,1.,0.996917333733128,1.,0.996917333733128,
1.,0.996917333733128,1.,0.996917333733128,1.,0.996917333733128,1.,0.996917333733128,
1.,0.996917333733128,1.,0.996917333733128,1.,0.996917333733128,1.,0.996917333733128,
1.,0.996917333733128,1.,0.996917333733128,1.,0.996917333733128,1.,0.996917333733128,
1.,0.996917333733128,1.,0.996917333733128,1.),(1.,0.996917333733128,1.,
0.996917333733128,1.,0.996917333733128,1.,0.996917333733128,1.,0.996917333733128,
1.,0.996917333733128,1.,0.996917333733128,1.,0.996917333733128,1.,0.996917333733128,
1.,0.996917333733128,1.,0.996917333733128,1.,0.996917333733128,1.,0.996917333733128,
1.,0.996917333733128,1.,0.996917333733128,1.,0.996917333733128,1.,0.996917333733128,
1.,0.996917333733128,1.,0.996917333733128,1.,0.996917333733128,1.,0.996917333733128,
1.,0.996917333733128,1.,0.996917333733128,1.,0.996917333733128,1.,0.996917333733128,
1.,0.996917333733128,1.,0.996917333733128,1.,0.996917333733128,1.,0.996917333733128,
1.,0.996917333733128,1.,0.996917333733128,1.,0.996917333733128,1.,0.996917333733128,
1.,0.996917333733128,1.,0.996917333733128,1.,0.996917333733128,1.,0.996917333733128,
1.,0.996917333733128,1.,0.996917333733128,1.,0.996917333733128,1.)))
REPRESENTATION_ITEM('')
SURFACE()
);
#4055=(
BOUNDED_SURFACE()
B_SPLINE_SURFACE(1,2,((#273414,#273415,#273416,#273417,#273418,#273419,
#273420,#273421,#273422,#273423,#273424,#273425,#273426,#273427,#273428,
#273429,#273430,#273431,#273432,#273433,#273434,#273435,#273436,#273437,
#273438,#273439,#273440,#273441,#273442,#273443,#273444,#273445,#273446,
#273447,#273448,#273449,#273450,#273451,#273452,#273453,#273454,#273455,
#273456,#273457,#273458,#273459,#273460,#273461,#273462,#273463,#273464,
#273465,#273466,#273467,#273468,#273469,#273470,#273471,#273472,#273473,
#273474,#273475,#273476,#273477,#273478,#273479,#273480,#273481,#273482,
#273483,#273484,#273485,#273486,#273487,#273488,#273489,#273490,#273491,
#273492,#273493,#273494),(#273495,#273496,#273497,#273498,#273499,#273500,
#273501,#273502,#273503,#273504,#273505,#273506,#273507,#273508,#273509,
#273510,#273511,#273512,#273513,#273514,#273515,#273516,#273517,#273518,
#273519,#273520,#273521,#273522,#273523,#273524,#273525,#273526,#273527,
#273528,#273529,#273530,#273531,#273532,#273533,#273534,#273535,#273536,
#273537,#273538,#273539,#273540,#273541,#273542,#273543,#273544,#273545,
#273546,#273547,#273548,#273549,#273550,#273551,#273552,#273553,#273554,
#273555,#273556,#273557,#273558,#273559,#273560,#273561,#273562,#273563,
#273564,#273565,#273566,#273567,#273568,#273569,#273570,#273571,#273572,
#273573,#273574,#273575)),.UNSPECIFIED.,.F.,.F.,.F.)
B_SPLINE_SURFACE_WITH_KNOTS((2,2),(3,2,2,2,2,2,2,2,2,2,2,2,2,2,2,2,2,2,
2,2,2,2,2,2,2,2,2,2,2,2,2,2,2,2,2,2,2,2,2,2,3),(0.,1.),(0.,0.025,0.05,0.075,
0.1,0.125,0.15,0.175,0.2,0.225,0.25,0.275,0.3,0.325,0.35,0.375,0.4,0.425,
0.45,0.475,0.5,0.525,0.55,0.575,0.6,0.625,0.65,0.675,0.7,0.725,0.75,0.775,
0.8,0.825,0.85,0.875,0.9,0.925,0.95,0.975,1.),.UNSPECIFIED.)
GEOMETRIC_REPRESENTATION_ITEM()
RATIONAL_B_SPLINE_SURFACE(((1.,0.996917333733128,1.,0.996917333733128,1.,
0.996917333733128,1.,0.996917333733128,1.,0.996917333733128,1.,0.996917333733128,
1.,0.996917333733128,1.,0.996917333733128,1.,0.996917333733128,1.,0.996917333733128,
1.,0.996917333733128,1.,0.996917333733128,1.,0.996917333733128,1.,0.996917333733128,
1.,0.996917333733128,1.,0.996917333733128,1.,0.996917333733128,1.,0.996917333733128,
1.,0.996917333733128,1.,0.996917333733128,1.,0.996917333733128,1.,0.996917333733128,
1.,0.996917333733128,1.,0.996917333733128,1.,0.996917333733128,1.,0.996917333733128,
1.,0.996917333733128,1.,0.996917333733128,1.,0.996917333733128,1.,0.996917333733128,
1.,0.996917333733128,1.,0.996917333733128,1.,0.996917333733128,1.,0.996917333733128,
1.,0.996917333733128,1.,0.996917333733128,1.,0.996917333733128,1.,0.996917333733128,
1.,0.996917333733128,1.,0.996917333733128,1.),(1.,0.996917333733128,1.,
0.996917333733128,1.,0.996917333733128,1.,0.996917333733128,1.,0.996917333733128,
1.,0.996917333733128,1.,0.996917333733128,1.,0.996917333733128,1.,0.996917333733128,
1.,0.996917333733128,1.,0.996917333733128,1.,0.996917333733128,1.,0.996917333733128,
1.,0.996917333733128,1.,0.996917333733128,1.,0.996917333733128,1.,0.996917333733128,
1.,0.996917333733128,1.,0.996917333733128,1.,0.996917333733128,1.,0.996917333733128,
1.,0.996917333733128,1.,0.996917333733128,1.,0.996917333733128,1.,0.996917333733128,
1.,0.996917333733128,1.,0.996917333733128,1.,0.996917333733128,1.,0.996917333733128,
1.,0.996917333733128,1.,0.996917333733128,1.,0.996917333733128,1.,0.996917333733128,
1.,0.996917333733128,1.,0.996917333733128,1.,0.996917333733128,1.,0.996917333733128,
1.,0.996917333733128,1.,0.996917333733128,1.,0.996917333733128,1.)))
REPRESENTATION_ITEM('')
SURFACE()
);
#4056=(
BOUNDED_SURFACE()
B_SPLINE_SURFACE(1,2,((#273577,#273578,#273579,#273580,#273581,#273582,
#273583,#273584,#273585,#273586,#273587,#273588,#273589,#273590,#273591,
#273592,#273593,#273594,#273595,#273596,#273597,#273598,#273599,#273600,
#273601,#273602,#273603,#273604,#273605,#273606,#273607,#273608,#273609,
#273610,#273611,#273612,#273613,#273614,#273615,#273616,#273617,#273618,
#273619,#273620,#273621,#273622,#273623,#273624,#273625,#273626,#273627,
#273628,#273629,#273630,#273631,#273632,#273633,#273634,#273635,#273636,
#273637,#273638,#273639,#273640,#273641,#273642,#273643,#273644,#273645,
#273646,#273647,#273648,#273649,#273650,#273651,#273652,#273653,#273654,
#273655,#273656,#273657),(#273658,#273659,#273660,#273661,#273662,#273663,
#273664,#273665,#273666,#273667,#273668,#273669,#273670,#273671,#273672,
#273673,#273674,#273675,#273676,#273677,#273678,#273679,#273680,#273681,
#273682,#273683,#273684,#273685,#273686,#273687,#273688,#273689,#273690,
#273691,#273692,#273693,#273694,#273695,#273696,#273697,#273698,#273699,
#273700,#273701,#273702,#273703,#273704,#273705,#273706,#273707,#273708,
#273709,#273710,#273711,#273712,#273713,#273714,#273715,#273716,#273717,
#273718,#273719,#273720,#273721,#273722,#273723,#273724,#273725,#273726,
#273727,#273728,#273729,#273730,#273731,#273732,#273733,#273734,#273735,
#273736,#273737,#273738)),.UNSPECIFIED.,.F.,.F.,.F.)
B_SPLINE_SURFACE_WITH_KNOTS((2,2),(3,2,2,2,2,2,2,2,2,2,2,2,2,2,2,2,2,2,
2,2,2,2,2,2,2,2,2,2,2,2,2,2,2,2,2,2,2,2,2,2,3),(0.,1.),(0.,0.025,0.05,0.075,
0.1,0.125,0.15,0.175,0.2,0.225,0.25,0.275,0.3,0.325,0.35,0.375,0.4,0.425,
0.45,0.475,0.5,0.525,0.55,0.575,0.6,0.625,0.65,0.675,0.7,0.725,0.75,0.775,
0.8,0.825,0.85,0.875,0.9,0.925,0.95,0.975,1.),.UNSPECIFIED.)
GEOMETRIC_REPRESENTATION_ITEM()
RATIONAL_B_SPLINE_SURFACE(((1.,0.996917333733128,1.,0.996917333733128,1.,
0.996917333733128,1.,0.996917333733128,1.,0.996917333733128,1.,0.996917333733128,
1.,0.996917333733128,1.,0.996917333733128,1.,0.996917333733128,1.,0.996917333733128,
1.,0.996917333733128,1.,0.996917333733128,1.,0.996917333733128,1.,0.996917333733128,
1.,0.996917333733128,1.,0.996917333733128,1.,0.996917333733128,1.,0.996917333733128,
1.,0.996917333733128,1.,0.996917333733128,1.,0.996917333733128,1.,0.996917333733128,
1.,0.996917333733128,1.,0.996917333733128,1.,0.996917333733128,1.,0.996917333733128,
1.,0.996917333733128,1.,0.996917333733128,1.,0.996917333733128,1.,0.996917333733128,
1.,0.996917333733128,1.,0.996917333733128,1.,0.996917333733128,1.,0.996917333733128,
1.,0.996917333733128,1.,0.996917333733128,1.,0.996917333733128,1.,0.996917333733128,
1.,0.996917333733128,1.,0.996917333733128,1.),(1.,0.996917333733128,1.,
0.996917333733128,1.,0.996917333733128,1.,0.996917333733128,1.,0.996917333733128,
1.,0.996917333733128,1.,0.996917333733128,1.,0.996917333733128,1.,0.996917333733128,
1.,0.996917333733128,1.,0.996917333733128,1.,0.996917333733128,1.,0.996917333733128,
1.,0.996917333733128,1.,0.996917333733128,1.,0.996917333733128,1.,0.996917333733128,
1.,0.996917333733128,1.,0.996917333733128,1.,0.996917333733128,1.,0.996917333733128,
1.,0.996917333733128,1.,0.996917333733128,1.,0.996917333733128,1.,0.996917333733128,
1.,0.996917333733128,1.,0.996917333733128,1.,0.996917333733128,1.,0.996917333733128,
1.,0.996917333733128,1.,0.996917333733128,1.,0.996917333733128,1.,0.996917333733128,
1.,0.996917333733128,1.,0.996917333733128,1.,0.996917333733128,1.,0.996917333733128,
1.,0.996917333733128,1.,0.996917333733128,1.,0.996917333733128,1.)))
REPRESENTATION_ITEM('')
SURFACE()
);
#4057=(
BOUNDED_SURFACE()
B_SPLINE_SURFACE(2,2,((#273891,#273892,#273893),(#273894,#273895,#273896),
(#273897,#273898,#273899)),.UNSPECIFIED.,.F.,.F.,.F.)
B_SPLINE_SURFACE_WITH_KNOTS((3,3),(3,3),(0.,1.57079632679491),(-3.14159265358979,
-1.5707963267949),.UNSPECIFIED.)
GEOMETRIC_REPRESENTATION_ITEM()
RATIONAL_B_SPLINE_SURFACE(((1.,0.707106781186548,1.),(0.707106781186546,
0.499999999999999,0.707106781186546),(1.,0.707106781186548,1.)))
REPRESENTATION_ITEM('')
SURFACE()
);
#4058=(
BOUNDED_SURFACE()
B_SPLINE_SURFACE(2,2,((#273906,#273907,#273908),(#273909,#273910,#273911),
(#273912,#273913,#273914)),.UNSPECIFIED.,.F.,.F.,.F.)
B_SPLINE_SURFACE_WITH_KNOTS((3,3),(3,3),(0.,1.57079632679491),(-1.5707963267949,
0.),.UNSPECIFIED.)
GEOMETRIC_REPRESENTATION_ITEM()
RATIONAL_B_SPLINE_SURFACE(((1.,0.707106781186547,1.),(0.707106781186542,
0.499999999999996,0.707106781186542),(1.,0.707106781186547,1.)))
REPRESENTATION_ITEM('')
SURFACE()
);
#4059=(
BOUNDED_SURFACE()
B_SPLINE_SURFACE(2,2,((#273916,#273917,#273918),(#273919,#273920,#273921),
(#273922,#273923,#273924)),.UNSPECIFIED.,.F.,.F.,.F.)
B_SPLINE_SURFACE_WITH_KNOTS((3,3),(3,3),(0.,1.57079632679491),(1.5707963267949,
3.14159265358979),.UNSPECIFIED.)
GEOMETRIC_REPRESENTATION_ITEM()
RATIONAL_B_SPLINE_SURFACE(((1.,0.707106781186548,1.),(0.707106781186542,
0.499999999999996,0.707106781186542),(1.,0.707106781186548,1.)))
REPRESENTATION_ITEM('')
SURFACE()
);
#4060=(
BOUNDED_SURFACE()
B_SPLINE_SURFACE(2,2,((#273930,#273931,#273932),(#273933,#273934,#273935),
(#273936,#273937,#273938)),.UNSPECIFIED.,.F.,.F.,.F.)
B_SPLINE_SURFACE_WITH_KNOTS((3,3),(3,3),(0.,1.57079632679491),(0.,1.5707963267949),
 .UNSPECIFIED.)
GEOMETRIC_REPRESENTATION_ITEM()
RATIONAL_B_SPLINE_SURFACE(((1.,0.707106781186548,1.),(0.707106781186542,
0.499999999999996,0.707106781186542),(1.,0.707106781186548,1.)))
REPRESENTATION_ITEM('')
SURFACE()
);
#4061=(
BOUNDED_SURFACE()
B_SPLINE_SURFACE(3,2,((#274053,#274054,#274055),(#274056,#274057,#274058),
(#274059,#274060,#274061),(#274062,#274063,#274064)),.UNSPECIFIED.,.F.,
 .F.,.F.)
B_SPLINE_SURFACE_WITH_KNOTS((4,4),(3,3),(0.00902295194197484,0.0107038053334674),
(0.,1.),.UNSPECIFIED.)
GEOMETRIC_REPRESENTATION_ITEM()
RATIONAL_B_SPLINE_SURFACE(((1.,0.717027218350901,1.),(1.,0.717027379451177,
1.),(1.,0.713716651700049,1.),(1.,0.707106781186548,1.)))
REPRESENTATION_ITEM('')
SURFACE()
);
#4062=(
BOUNDED_SURFACE()
B_SPLINE_SURFACE(3,2,((#274072,#274073,#274074),(#274075,#274076,#274077),
(#274078,#274079,#274080),(#274081,#274082,#274083)),.UNSPECIFIED.,.F.,
 .F.,.F.)
B_SPLINE_SURFACE_WITH_KNOTS((4,4),(3,3),(0.00902295194197483,0.0107038053334674),
(0.,1.),.UNSPECIFIED.)
GEOMETRIC_REPRESENTATION_ITEM()
RATIONAL_B_SPLINE_SURFACE(((1.,0.717027218350901,1.),(1.,0.717027379451176,
1.),(1.,0.713716651700055,1.),(1.,0.707106781186548,1.)))
REPRESENTATION_ITEM('')
SURFACE()
);
#4063=(
BOUNDED_SURFACE()
B_SPLINE_SURFACE(3,2,((#274085,#274086,#274087),(#274088,#274089,#274090),
(#274091,#274092,#274093),(#274094,#274095,#274096)),.UNSPECIFIED.,.F.,
 .F.,.F.)
B_SPLINE_SURFACE_WITH_KNOTS((4,4),(3,3),(0.00902295194197484,0.0107038053334674),
(0.,1.),.UNSPECIFIED.)
GEOMETRIC_REPRESENTATION_ITEM()
RATIONAL_B_SPLINE_SURFACE(((1.,0.717027218350901,1.),(1.,0.717027379451177,
1.),(1.,0.713716651700049,1.),(1.,0.707106781186548,1.)))
REPRESENTATION_ITEM('')
SURFACE()
);
#4064=(
BOUNDED_SURFACE()
B_SPLINE_SURFACE(3,2,((#274104,#274105,#274106),(#274107,#274108,#274109),
(#274110,#274111,#274112),(#274113,#274114,#274115)),.UNSPECIFIED.,.F.,
 .F.,.F.)
B_SPLINE_SURFACE_WITH_KNOTS((4,4),(3,3),(0.00902295194197484,0.0107038053334674),
(0.,1.),.UNSPECIFIED.)
GEOMETRIC_REPRESENTATION_ITEM()
RATIONAL_B_SPLINE_SURFACE(((1.,0.717027218350901,1.),(1.,0.717027379451177,
1.),(1.,0.713716651700049,1.),(1.,0.707106781186548,1.)))
REPRESENTATION_ITEM('')
SURFACE()
);
#4065=(
BOUNDED_CURVE()
B_SPLINE_CURVE(2,(#143197,#143198,#143199,#143200,#143201,#143202,#143203,
#143204,#143205,#143206,#143207,#143208,#143209,#143210,#143211,#143212,
#143213,#143214,#143215,#143216,#143217,#143218,#143219,#143220,#143221,
#143222,#143223,#143224,#143225,#143226,#143227,#143228,#143229,#143230,
#143231),.UNSPECIFIED.,.F.,.F.)
B_SPLINE_CURVE_WITH_KNOTS((3,2,2,2,2,2,2,2,2,2,2,2,2,2,2,2,2,3),(0.,0.000980392156862745,
0.00196078431372549,0.00294117647058824,0.00392156862745098,0.00490196078431373,
0.00588235294117647,0.00686274509803922,0.00784313725490196,0.00882352941176471,
0.00980392156862745,0.0107843137254902,0.0117647058823529,0.0127450980392157,
0.0137254901960784,0.0147058823529412,0.0156862745098039,0.0166666666666667),
 .UNSPECIFIED.)
CURVE()
GEOMETRIC_REPRESENTATION_ITEM()
RATIONAL_B_SPLINE_CURVE((1.,0.995734176295034,1.,0.995734176295034,1.,0.995734176295034,
1.,0.995734176295034,1.,0.995734176295034,1.,0.995734176295034,1.,0.995734176295034,
1.,0.995734176295034,1.,0.995734176295034,1.,0.995734176295034,1.,0.995734176295034,
1.,0.995734176295034,1.,0.995734176295034,1.,0.995734176295034,1.,0.995734176295034,
1.,0.995734176295034,1.,0.995734176295034,1.))
REPRESENTATION_ITEM('')
);
#4066=(
BOUNDED_CURVE()
B_SPLINE_CURVE(2,(#143234,#143235,#143236,#143237,#143238,#143239,#143240,
#143241,#143242,#143243,#143244,#143245,#143246,#143247,#143248,#143249,
#143250,#143251,#143252,#143253,#143254,#143255,#143256,#143257,#143258,
#143259,#143260,#143261,#143262,#143263,#143264,#143265,#143266,#143267,
#143268),.UNSPECIFIED.,.F.,.F.)
B_SPLINE_CURVE_WITH_KNOTS((3,2,2,2,2,2,2,2,2,2,2,2,2,2,2,2,2,3),(0.,0.000994375769093022,
0.00198875153818604,0.00298312730727906,0.00397750307637209,0.00497187884546511,
0.00596625461455813,0.00696063038365115,0.00795500615274417,0.00894938192183719,
0.00994375769093021,0.0109381334600232,0.0119325092291163,0.0129268849982093,
0.0139212607673023,0.0149156365363953,0.0159100123054883,0.0169043880745814),
 .UNSPECIFIED.)
CURVE()
GEOMETRIC_REPRESENTATION_ITEM()
RATIONAL_B_SPLINE_CURVE((1.,0.995734176295034,1.,0.995734176295034,1.,0.995734176295034,
1.,0.995734176295034,1.,0.995734176295034,1.,0.995734176295034,1.,0.995734176295034,
1.,0.995734176295034,1.,0.995734176295034,1.,0.995734176295034,1.,0.995734176295034,
1.,0.995734176295034,1.,0.995734176295034,1.,0.995734176295034,1.,0.995734176295034,
1.,0.995734176295034,1.,0.995734176295034,1.))
REPRESENTATION_ITEM('')
);
#4067=(
BOUNDED_CURVE()
B_SPLINE_CURVE(2,(#143273,#143274,#143275,#143276,#143277,#143278,#143279,
#143280,#143281,#143282,#143283,#143284,#143285,#143286,#143287,#143288,
#143289,#143290,#143291,#143292,#143293,#143294,#143295,#143296,#143297,
#143298,#143299,#143300,#143301,#143302,#143303,#143304,#143305,#143306,
#143307,#143308,#143309,#143310,#143311,#143312,#143313,#143314,#143315,
#143316,#143317,#143318,#143319,#143320,#143321,#143322,#143323,#143324,
#143325,#143326,#143327,#143328,#143329,#143330,#143331,#143332,#143333,
#143334,#143335,#143336,#143337,#143338,#143339,#143340,#143341),
 .UNSPECIFIED.,.F.,.F.)
B_SPLINE_CURVE_WITH_KNOTS((3,2,2,2,2,2,2,2,2,2,2,2,2,2,2,2,2,2,2,2,2,2,
2,2,2,2,2,2,2,2,2,2,2,2,3),(0.0166666666666667,0.0176470588235294,0.0186274509803922,
0.0196078431372549,0.0205882352941176,0.0215686274509804,0.0225490196078431,
0.0235294117647059,0.0245098039215686,0.0254901960784314,0.0264705882352941,
0.0274509803921569,0.0284313725490196,0.0294117647058824,0.0303921568627451,
0.0313725490196078,0.0323529411764706,0.0333333333333333,0.0343137254901961,
0.0352941176470588,0.0362745098039216,0.0372549019607843,0.0382352941176471,
0.0392156862745098,0.0401960784313726,0.0411764705882353,0.042156862745098,
0.0431372549019608,0.0441176470588235,0.0450980392156863,0.046078431372549,
0.0470588235294118,0.0480392156862745,0.0490196078431373,0.05),
 .UNSPECIFIED.)
CURVE()
GEOMETRIC_REPRESENTATION_ITEM()
RATIONAL_B_SPLINE_CURVE((1.,0.995734176295034,1.,0.995734176295034,1.,0.995734176295034,
1.,0.995734176295034,1.,0.995734176295034,1.,0.995734176295034,1.,0.995734176295034,
1.,0.995734176295034,1.,0.995734176295034,1.,0.995734176295034,1.,0.995734176295034,
1.,0.995734176295034,1.,0.995734176295034,1.,0.995734176295034,1.,0.995734176295034,
1.,0.995734176295034,1.,0.995734176295034,1.,0.995734176295034,1.,0.995734176295034,
1.,0.995734176295034,1.,0.995734176295034,1.,0.995734176295034,1.,0.995734176295034,
1.,0.995734176295034,1.,0.995734176295034,1.,0.995734176295034,1.,0.995734176295034,
1.,0.995734176295034,1.,0.995734176295034,1.,0.995734176295034,1.,0.995734176295034,
1.,0.995734176295034,1.,0.995734176295034,1.,0.995734176295034,1.))
REPRESENTATION_ITEM('')
);
#4068=(
BOUNDED_CURVE()
B_SPLINE_CURVE(2,(#143342,#143343,#143344,#143345,#143346,#143347,#143348,
#143349,#143350,#143351,#143352,#143353,#143354,#143355,#143356,#143357,
#143358,#143359,#143360,#143361,#143362,#143363,#143364,#143365,#143366,
#143367,#143368,#143369,#143370,#143371,#143372,#143373,#143374,#143375,
#143376,#143377,#143378,#143379,#143380,#143381,#143382,#143383,#143384,
#143385,#143386,#143387,#143388,#143389,#143390,#143391,#143392,#143393,
#143394,#143395,#143396,#143397,#143398,#143399,#143400,#143401,#143402,
#143403,#143404,#143405,#143406,#143407,#143408,#143409,#143410),
 .UNSPECIFIED.,.F.,.F.)
B_SPLINE_CURVE_WITH_KNOTS((3,2,2,2,2,2,2,2,2,2,2,2,2,2,2,2,2,2,2,2,2,2,
2,2,2,2,2,2,2,2,2,2,2,2,3),(0.0169043880745814,0.0178987638436744,0.0188931396127674,
0.0198875153818604,0.0208818911509534,0.0218762669200465,0.0228706426891395,
0.0238650184582325,0.0248593942273255,0.0258537699964186,0.0268481457655116,
0.0278425215346046,0.0288368973036976,0.0298312730727906,0.0308256488418837,
0.0318200246109767,0.0328144003800697,0.0338087761491627,0.0348031519182558,
0.0357975276873488,0.0367919034564418,0.0377862792255348,0.0387806549946278,
0.0397750307637209,0.0407694065328139,0.0417637823019069,0.0427581580709999,
0.0437525338400929,0.044746909609186,0.045741285378279,0.046735661147372,
0.047730036916465,0.048724412685558,0.0497187884546511,0.0507131642237441),
 .UNSPECIFIED.)
CURVE()
GEOMETRIC_REPRESENTATION_ITEM()
RATIONAL_B_SPLINE_CURVE((1.,0.995734176295034,1.,0.995734176295034,1.,0.995734176295034,
1.,0.995734176295034,1.,0.995734176295034,1.,0.995734176295034,1.,0.995734176295034,
1.,0.995734176295034,1.,0.995734176295034,1.,0.995734176295034,1.,0.995734176295034,
1.,0.995734176295034,1.,0.995734176295034,1.,0.995734176295034,1.,0.995734176295034,
1.,0.995734176295034,1.,0.995734176295034,1.,0.995734176295034,1.,0.995734176295034,
1.,0.995734176295034,1.,0.995734176295034,1.,0.995734176295034,1.,0.995734176295034,
1.,0.995734176295034,1.,0.995734176295034,1.,0.995734176295034,1.,0.995734176295034,
1.,0.995734176295034,1.,0.995734176295034,1.,0.995734176295034,1.,0.995734176295034,
1.,0.995734176295034,1.,0.995734176295034,1.,0.995734176295034,1.))
REPRESENTATION_ITEM('')
);
#4069=(
BOUNDED_CURVE()
B_SPLINE_CURVE(2,(#143415,#143416,#143417,#143418,#143419,#143420,#143421,
#143422,#143423,#143424,#143425,#143426,#143427,#143428,#143429,#143430,
#143431,#143432,#143433,#143434,#143435,#143436,#143437,#143438,#143439,
#143440,#143441,#143442,#143443,#143444,#143445,#143446,#143447,#143448,
#143449,#143450,#143451,#143452,#143453,#143454,#143455,#143456,#143457,
#143458,#143459,#143460,#143461,#143462,#143463,#143464,#143465,#143466,
#143467,#143468,#143469,#143470,#143471,#143472,#143473,#143474,#143475,
#143476,#143477,#143478,#143479,#143480,#143481,#143482,#143483),
 .UNSPECIFIED.,.F.,.F.)
B_SPLINE_CURVE_WITH_KNOTS((3,2,2,2,2,2,2,2,2,2,2,2,2,2,2,2,2,2,2,2,2,2,
2,2,2,2,2,2,2,2,2,2,2,2,3),(0.05,0.0509803921568627,0.0519607843137255,
0.0529411764705882,0.053921568627451,0.0549019607843137,0.0558823529411765,
0.0568627450980392,0.057843137254902,0.0588235294117647,0.0598039215686275,
0.0607843137254902,0.061764705882353,0.0627450980392157,0.0637254901960784,
0.0647058823529412,0.0656862745098039,0.0666666666666667,0.0676470588235294,
0.0686274509803922,0.0696078431372549,0.0705882352941176,0.0715686274509804,
0.0725490196078431,0.0735294117647059,0.0745098039215686,0.0754901960784314,
0.0764705882352941,0.0774509803921569,0.0784313725490196,0.0794117647058823,
0.0803921568627451,0.0813725490196078,0.0823529411764706,0.0833333333333333),
 .UNSPECIFIED.)
CURVE()
GEOMETRIC_REPRESENTATION_ITEM()
RATIONAL_B_SPLINE_CURVE((1.,0.995734176295034,1.,0.995734176295034,1.,0.995734176295034,
1.,0.995734176295034,1.,0.995734176295034,1.,0.995734176295034,1.,0.995734176295034,
1.,0.995734176295034,1.,0.995734176295034,1.,0.995734176295034,1.,0.995734176295034,
1.,0.995734176295034,1.,0.995734176295034,1.,0.995734176295034,1.,0.995734176295034,
1.,0.995734176295034,1.,0.995734176295034,1.,0.995734176295034,1.,0.995734176295034,
1.,0.995734176295034,1.,0.995734176295034,1.,0.995734176295034,1.,0.995734176295034,
1.,0.995734176295034,1.,0.995734176295034,1.,0.995734176295034,1.,0.995734176295034,
1.,0.995734176295034,1.,0.995734176295034,1.,0.995734176295034,1.,0.995734176295034,
1.,0.995734176295034,1.,0.995734176295034,1.,0.995734176295034,1.))
REPRESENTATION_ITEM('')
);
#4070=(
BOUNDED_CURVE()
B_SPLINE_CURVE(2,(#143484,#143485,#143486,#143487,#143488,#143489,#143490,
#143491,#143492,#143493,#143494,#143495,#143496,#143497,#143498,#143499,
#143500,#143501,#143502,#143503,#143504,#143505,#143506,#143507,#143508,
#143509,#143510,#143511,#143512,#143513,#143514,#143515,#143516,#143517,
#143518,#143519,#143520,#143521,#143522,#143523,#143524,#143525,#143526,
#143527,#143528,#143529,#143530,#143531,#143532,#143533,#143534,#143535,
#143536,#143537,#143538,#143539,#143540,#143541,#143542,#143543,#143544,
#143545,#143546,#143547,#143548,#143549,#143550,#143551,#143552),
 .UNSPECIFIED.,.F.,.F.)
B_SPLINE_CURVE_WITH_KNOTS((3,2,2,2,2,2,2,2,2,2,2,2,2,2,2,2,2,2,2,2,2,2,
2,2,2,2,2,2,2,2,2,2,2,2,3),(0.0507131642237441,0.0517075399928371,0.0527019157619301,
0.0536962915310232,0.0546906673001162,0.0556850430692092,0.0566794188383022,
0.0576737946073952,0.0586681703764883,0.0596625461455813,0.0606569219146743,
0.0616512976837673,0.0626456734528604,0.0636400492219534,0.0646344249910464,
0.0656288007601394,0.0666231765292324,0.0676175522983255,0.0686119280674185,
0.0696063038365115,0.0706006796056045,0.0715950553746975,0.0725894311437906,
0.0735838069128836,0.0745781826819766,0.0755725584510696,0.0765669342201626,
0.0775613099892557,0.0785556857583487,0.0795500615274417,0.0805444372965347,
0.0815388130656278,0.0825331888347208,0.0835275646038138,0.0845219403729068),
 .UNSPECIFIED.)
CURVE()
GEOMETRIC_REPRESENTATION_ITEM()
RATIONAL_B_SPLINE_CURVE((1.,0.995734176295034,1.,0.995734176295034,1.,0.995734176295034,
1.,0.995734176295034,1.,0.995734176295034,1.,0.995734176295034,1.,0.995734176295034,
1.,0.995734176295034,1.,0.995734176295034,1.,0.995734176295034,1.,0.995734176295034,
1.,0.995734176295034,1.,0.995734176295034,1.,0.995734176295034,1.,0.995734176295034,
1.,0.995734176295034,1.,0.995734176295034,1.,0.995734176295034,1.,0.995734176295034,
1.,0.995734176295034,1.,0.995734176295034,1.,0.995734176295034,1.,0.995734176295034,
1.,0.995734176295034,1.,0.995734176295034,1.,0.995734176295034,1.,0.995734176295034,
1.,0.995734176295034,1.,0.995734176295034,1.,0.995734176295034,1.,0.995734176295034,
1.,0.995734176295034,1.,0.995734176295034,1.,0.995734176295034,1.))
REPRESENTATION_ITEM('')
);
#4071=(
BOUNDED_CURVE()
B_SPLINE_CURVE(2,(#143557,#143558,#143559,#143560,#143561,#143562,#143563,
#143564,#143565,#143566,#143567,#143568,#143569,#143570,#143571,#143572,
#143573,#143574,#143575,#143576,#143577,#143578,#143579,#143580,#143581,
#143582,#143583,#143584,#143585,#143586,#143587,#143588,#143589,#143590,
#143591,#143592,#143593,#143594,#143595,#143596,#143597,#143598,#143599,
#143600,#143601,#143602,#143603,#143604,#143605,#143606,#143607,#143608,
#143609,#143610,#143611,#143612,#143613,#143614,#143615,#143616,#143617,
#143618,#143619,#143620,#143621,#143622,#143623,#143624,#143625),
 .UNSPECIFIED.,.F.,.F.)
B_SPLINE_CURVE_WITH_KNOTS((3,2,2,2,2,2,2,2,2,2,2,2,2,2,2,2,2,2,2,2,2,2,
2,2,2,2,2,2,2,2,2,2,2,2,3),(0.0833333333333333,0.0843137254901961,0.0852941176470588,
0.0862745098039216,0.0872549019607843,0.0882352941176471,0.0892156862745098,
0.0901960784313725,0.0911764705882353,0.092156862745098,0.0931372549019608,
0.0941176470588235,0.0950980392156863,0.096078431372549,0.0970588235294118,
0.0980392156862745,0.0990196078431373,0.1,0.100980392156863,0.101960784313725,
0.102941176470588,0.103921568627451,0.104901960784314,0.105882352941176,
0.106862745098039,0.107843137254902,0.108823529411765,0.109803921568627,
0.11078431372549,0.111764705882353,0.112745098039216,0.113725490196078,
0.114705882352941,0.115686274509804,0.116666666666667),.UNSPECIFIED.)
CURVE()
GEOMETRIC_REPRESENTATION_ITEM()
RATIONAL_B_SPLINE_CURVE((1.,0.995734176295034,1.,0.995734176295034,1.,0.995734176295034,
1.,0.995734176295034,1.,0.995734176295034,1.,0.995734176295034,1.,0.995734176295034,
1.,0.995734176295034,1.,0.995734176295034,1.,0.995734176295034,1.,0.995734176295034,
1.,0.995734176295034,1.,0.995734176295034,1.,0.995734176295034,1.,0.995734176295034,
1.,0.995734176295034,1.,0.995734176295034,1.,0.995734176295034,1.,0.995734176295034,
1.,0.995734176295034,1.,0.995734176295034,1.,0.995734176295034,1.,0.995734176295034,
1.,0.995734176295034,1.,0.995734176295034,1.,0.995734176295034,1.,0.995734176295034,
1.,0.995734176295034,1.,0.995734176295034,1.,0.995734176295034,1.,0.995734176295034,
1.,0.995734176295034,1.,0.995734176295034,1.,0.995734176295034,1.))
REPRESENTATION_ITEM('')
);
#4072=(
BOUNDED_CURVE()
B_SPLINE_CURVE(2,(#143626,#143627,#143628,#143629,#143630,#143631,#143632,
#143633,#143634,#143635,#143636,#143637,#143638,#143639,#143640,#143641,
#143642,#143643,#143644,#143645,#143646,#143647,#143648,#143649,#143650,
#143651,#143652,#143653,#143654,#143655,#143656,#143657,#143658,#143659,
#143660,#143661,#143662,#143663,#143664,#143665,#143666,#143667,#143668,
#143669,#143670,#143671,#143672,#143673,#143674,#143675,#143676,#143677,
#143678,#143679,#143680,#143681,#143682,#143683,#143684,#143685,#143686,
#143687,#143688,#143689,#143690,#143691,#143692,#143693,#143694),
 .UNSPECIFIED.,.F.,.F.)
B_SPLINE_CURVE_WITH_KNOTS((3,2,2,2,2,2,2,2,2,2,2,2,2,2,2,2,2,2,2,2,2,2,
2,2,2,2,2,2,2,2,2,2,2,2,3),(0.0845219403729068,0.0855163161419998,0.0865106919110929,
0.0875050676801859,0.0884994434492789,0.0894938192183719,0.090488194987465,
0.091482570756558,0.092476946525651,0.093471322294744,0.094465698063837,
0.0954600738329301,0.0964544496020231,0.0974488253711161,0.0984432011402091,
0.0994375769093021,0.100431952678395,0.101426328447488,0.102420704216581,
0.103415079985674,0.104409455754767,0.10540383152386,0.106398207292953,
0.107392583062046,0.108386958831139,0.109381334600232,0.110375710369325,
0.111370086138418,0.112364461907511,0.113358837676604,0.114353213445697,
0.11534758921479,0.116341964983883,0.117336340752977,0.11833071652207),
 .UNSPECIFIED.)
CURVE()
GEOMETRIC_REPRESENTATION_ITEM()
RATIONAL_B_SPLINE_CURVE((1.,0.995734176295034,1.,0.995734176295034,1.,0.995734176295034,
1.,0.995734176295034,1.,0.995734176295034,1.,0.995734176295034,1.,0.995734176295034,
1.,0.995734176295034,1.,0.995734176295034,1.,0.995734176295034,1.,0.995734176295034,
1.,0.995734176295034,1.,0.995734176295034,1.,0.995734176295034,1.,0.995734176295034,
1.,0.995734176295034,1.,0.995734176295034,1.,0.995734176295034,1.,0.995734176295034,
1.,0.995734176295034,1.,0.995734176295034,1.,0.995734176295034,1.,0.995734176295034,
1.,0.995734176295034,1.,0.995734176295034,1.,0.995734176295034,1.,0.995734176295034,
1.,0.995734176295034,1.,0.995734176295034,1.,0.995734176295034,1.,0.995734176295034,
1.,0.995734176295034,1.,0.995734176295034,1.,0.995734176295034,1.))
REPRESENTATION_ITEM('')
);
#4073=(
BOUNDED_CURVE()
B_SPLINE_CURVE(2,(#143699,#143700,#143701,#143702,#143703,#143704,#143705,
#143706,#143707,#143708,#143709,#143710,#143711,#143712,#143713,#143714,
#143715,#143716,#143717,#143718,#143719,#143720,#143721,#143722,#143723,
#143724,#143725,#143726,#143727,#143728,#143729,#143730,#143731,#143732,
#143733,#143734,#143735,#143736,#143737,#143738,#143739,#143740,#143741,
#143742,#143743,#143744,#143745,#143746,#143747,#143748,#143749,#143750,
#143751,#143752,#143753,#143754,#143755,#143756,#143757,#143758,#143759,
#143760,#143761,#143762,#143763,#143764,#143765,#143766,#143767),
 .UNSPECIFIED.,.F.,.F.)
B_SPLINE_CURVE_WITH_KNOTS((3,2,2,2,2,2,2,2,2,2,2,2,2,2,2,2,2,2,2,2,2,2,
2,2,2,2,2,2,2,2,2,2,2,2,3),(0.116666666666667,0.117647058823529,0.118627450980392,
0.119607843137255,0.120588235294118,0.12156862745098,0.122549019607843,
0.123529411764706,0.124509803921569,0.125490196078431,0.126470588235294,
0.127450980392157,0.12843137254902,0.129411764705882,0.130392156862745,
0.131372549019608,0.132352941176471,0.133333333333333,0.134313725490196,
0.135294117647059,0.136274509803922,0.137254901960784,0.138235294117647,
0.13921568627451,0.140196078431373,0.141176470588235,0.142156862745098,
0.143137254901961,0.144117647058824,0.145098039215686,0.146078431372549,
0.147058823529412,0.148039215686275,0.149019607843137,0.15),
 .UNSPECIFIED.)
CURVE()
GEOMETRIC_REPRESENTATION_ITEM()
RATIONAL_B_SPLINE_CURVE((1.,0.995734176295034,1.,0.995734176295034,1.,0.995734176295034,
1.,0.995734176295034,1.,0.995734176295034,1.,0.995734176295034,1.,0.995734176295034,
1.,0.995734176295034,1.,0.995734176295034,1.,0.995734176295034,1.,0.995734176295034,
1.,0.995734176295034,1.,0.995734176295034,1.,0.995734176295034,1.,0.995734176295034,
1.,0.995734176295034,1.,0.995734176295034,1.,0.995734176295034,1.,0.995734176295034,
1.,0.995734176295034,1.,0.995734176295034,1.,0.995734176295034,1.,0.995734176295034,
1.,0.995734176295034,1.,0.995734176295034,1.,0.995734176295034,1.,0.995734176295034,
1.,0.995734176295034,1.,0.995734176295034,1.,0.995734176295034,1.,0.995734176295034,
1.,0.995734176295034,1.,0.995734176295034,1.,0.995734176295034,1.))
REPRESENTATION_ITEM('')
);
#4074=(
BOUNDED_CURVE()
B_SPLINE_CURVE(2,(#143768,#143769,#143770,#143771,#143772,#143773,#143774,
#143775,#143776,#143777,#143778,#143779,#143780,#143781,#143782,#143783,
#143784,#143785,#143786,#143787,#143788,#143789,#143790,#143791,#143792,
#143793,#143794,#143795,#143796,#143797,#143798,#143799,#143800,#143801,
#143802,#143803,#143804,#143805,#143806,#143807,#143808,#143809,#143810,
#143811,#143812,#143813,#143814,#143815,#143816,#143817,#143818,#143819,
#143820,#143821,#143822,#143823,#143824,#143825,#143826,#143827,#143828,
#143829,#143830,#143831,#143832,#143833,#143834,#143835,#143836),
 .UNSPECIFIED.,.F.,.F.)
B_SPLINE_CURVE_WITH_KNOTS((3,2,2,2,2,2,2,2,2,2,2,2,2,2,2,2,2,2,2,2,2,2,
2,2,2,2,2,2,2,2,2,2,2,2,3),(0.11833071652207,0.119325092291163,0.120319468060256,
0.121313843829349,0.122308219598442,0.123302595367535,0.124296971136628,
0.125291346905721,0.126285722674814,0.127280098443907,0.128274474213,0.129268849982093,
0.130263225751186,0.131257601520279,0.132251977289372,0.133246353058465,
0.134240728827558,0.135235104596651,0.136229480365744,0.137223856134837,
0.13821823190393,0.139212607673023,0.140206983442116,0.141201359211209,
0.142195734980302,0.143190110749395,0.144184486518488,0.145178862287581,
0.146173238056674,0.147167613825767,0.14816198959486,0.149156365363953,
0.150150741133046,0.151145116902139,0.152139492671232),.UNSPECIFIED.)
CURVE()
GEOMETRIC_REPRESENTATION_ITEM()
RATIONAL_B_SPLINE_CURVE((1.,0.995734176295034,1.,0.995734176295034,1.,0.995734176295034,
1.,0.995734176295034,1.,0.995734176295034,1.,0.995734176295034,1.,0.995734176295034,
1.,0.995734176295034,1.,0.995734176295034,1.,0.995734176295034,1.,0.995734176295034,
1.,0.995734176295034,1.,0.995734176295034,1.,0.995734176295034,1.,0.995734176295034,
1.,0.995734176295034,1.,0.995734176295034,1.,0.995734176295034,1.,0.995734176295034,
1.,0.995734176295034,1.,0.995734176295034,1.,0.995734176295034,1.,0.995734176295034,
1.,0.995734176295034,1.,0.995734176295034,1.,0.995734176295034,1.,0.995734176295034,
1.,0.995734176295034,1.,0.995734176295034,1.,0.995734176295034,1.,0.995734176295034,
1.,0.995734176295034,1.,0.995734176295034,1.,0.995734176295034,1.))
REPRESENTATION_ITEM('')
);
#4075=(
BOUNDED_CURVE()
B_SPLINE_CURVE(2,(#143841,#143842,#143843,#143844,#143845,#143846,#143847,
#143848,#143849,#143850,#143851,#143852,#143853,#143854,#143855,#143856,
#143857,#143858,#143859,#143860,#143861,#143862,#143863,#143864,#143865,
#143866,#143867,#143868,#143869,#143870,#143871,#143872,#143873,#143874,
#143875,#143876,#143877,#143878,#143879,#143880,#143881,#143882,#143883,
#143884,#143885,#143886,#143887,#143888,#143889,#143890,#143891,#143892,
#143893,#143894,#143895,#143896,#143897,#143898,#143899,#143900,#143901,
#143902,#143903,#143904,#143905,#143906,#143907,#143908,#143909),
 .UNSPECIFIED.,.F.,.F.)
B_SPLINE_CURVE_WITH_KNOTS((3,2,2,2,2,2,2,2,2,2,2,2,2,2,2,2,2,2,2,2,2,2,
2,2,2,2,2,2,2,2,2,2,2,2,3),(0.15,0.150980392156863,0.151960784313725,0.152941176470588,
0.153921568627451,0.154901960784314,0.155882352941176,0.156862745098039,
0.157843137254902,0.158823529411765,0.159803921568627,0.16078431372549,
0.161764705882353,0.162745098039216,0.163725490196078,0.164705882352941,
0.165686274509804,0.166666666666667,0.167647058823529,0.168627450980392,
0.169607843137255,0.170588235294118,0.17156862745098,0.172549019607843,
0.173529411764706,0.174509803921569,0.175490196078431,0.176470588235294,
0.177450980392157,0.17843137254902,0.179411764705882,0.180392156862745,
0.181372549019608,0.182352941176471,0.183333333333333),.UNSPECIFIED.)
CURVE()
GEOMETRIC_REPRESENTATION_ITEM()
RATIONAL_B_SPLINE_CURVE((1.,0.995734176295034,1.,0.995734176295034,1.,0.995734176295034,
1.,0.995734176295034,1.,0.995734176295034,1.,0.995734176295034,1.,0.995734176295034,
1.,0.995734176295034,1.,0.995734176295034,1.,0.995734176295034,1.,0.995734176295034,
1.,0.995734176295034,1.,0.995734176295034,1.,0.995734176295034,1.,0.995734176295034,
1.,0.995734176295034,1.,0.995734176295034,1.,0.995734176295034,1.,0.995734176295034,
1.,0.995734176295034,1.,0.995734176295034,1.,0.995734176295034,1.,0.995734176295034,
1.,0.995734176295034,1.,0.995734176295034,1.,0.995734176295034,1.,0.995734176295034,
1.,0.995734176295034,1.,0.995734176295034,1.,0.995734176295034,1.,0.995734176295034,
1.,0.995734176295034,1.,0.995734176295034,1.,0.995734176295034,1.))
REPRESENTATION_ITEM('')
);
#4076=(
BOUNDED_CURVE()
B_SPLINE_CURVE(2,(#143910,#143911,#143912,#143913,#143914,#143915,#143916,
#143917,#143918,#143919,#143920,#143921,#143922,#143923,#143924,#143925,
#143926,#143927,#143928,#143929,#143930,#143931,#143932,#143933,#143934,
#143935,#143936,#143937,#143938,#143939,#143940,#143941,#143942,#143943,
#143944,#143945,#143946,#143947,#143948,#143949,#143950,#143951,#143952,
#143953,#143954,#143955,#143956,#143957,#143958,#143959,#143960,#143961,
#143962,#143963,#143964,#143965,#143966,#143967,#143968,#143969,#143970,
#143971,#143972,#143973,#143974,#143975,#143976,#143977,#143978),
 .UNSPECIFIED.,.F.,.F.)
B_SPLINE_CURVE_WITH_KNOTS((3,2,2,2,2,2,2,2,2,2,2,2,2,2,2,2,2,2,2,2,2,2,
2,2,2,2,2,2,2,2,2,2,2,2,3),(0.152139492671232,0.153133868440325,0.154128244209418,
0.155122619978511,0.156116995747604,0.157111371516697,0.15810574728579,
0.159100123054883,0.160094498823976,0.161088874593069,0.162083250362162,
0.163077626131256,0.164072001900349,0.165066377669442,0.166060753438535,
0.167055129207628,0.168049504976721,0.169043880745814,0.170038256514907,
0.171032632284,0.172027008053093,0.173021383822186,0.174015759591279,0.175010135360372,
0.176004511129465,0.176998886898558,0.177993262667651,0.178987638436744,
0.179982014205837,0.18097638997493,0.181970765744023,0.182965141513116,
0.183959517282209,0.184953893051302,0.185948268820395),.UNSPECIFIED.)
CURVE()
GEOMETRIC_REPRESENTATION_ITEM()
RATIONAL_B_SPLINE_CURVE((1.,0.995734176295034,1.,0.995734176295034,1.,0.995734176295034,
1.,0.995734176295034,1.,0.995734176295034,1.,0.995734176295034,1.,0.995734176295034,
1.,0.995734176295034,1.,0.995734176295034,1.,0.995734176295034,1.,0.995734176295034,
1.,0.995734176295034,1.,0.995734176295034,1.,0.995734176295034,1.,0.995734176295034,
1.,0.995734176295034,1.,0.995734176295034,1.,0.995734176295034,1.,0.995734176295034,
1.,0.995734176295034,1.,0.995734176295034,1.,0.995734176295034,1.,0.995734176295034,
1.,0.995734176295034,1.,0.995734176295034,1.,0.995734176295034,1.,0.995734176295034,
1.,0.995734176295034,1.,0.995734176295034,1.,0.995734176295034,1.,0.995734176295034,
1.,0.995734176295034,1.,0.995734176295034,1.,0.995734176295034,1.))
REPRESENTATION_ITEM('')
);
#4077=(
BOUNDED_CURVE()
B_SPLINE_CURVE(2,(#143983,#143984,#143985,#143986,#143987,#143988,#143989,
#143990,#143991,#143992,#143993,#143994,#143995,#143996,#143997,#143998,
#143999,#144000,#144001,#144002,#144003,#144004,#144005,#144006,#144007,
#144008,#144009,#144010,#144011,#144012,#144013,#144014,#144015,#144016,
#144017,#144018,#144019,#144020,#144021,#144022,#144023,#144024,#144025,
#144026,#144027,#144028,#144029,#144030,#144031,#144032,#144033,#144034,
#144035,#144036,#144037,#144038,#144039,#144040,#144041,#144042,#144043,
#144044,#144045,#144046,#144047,#144048,#144049,#144050,#144051),
 .UNSPECIFIED.,.F.,.F.)
B_SPLINE_CURVE_WITH_KNOTS((3,2,2,2,2,2,2,2,2,2,2,2,2,2,2,2,2,2,2,2,2,2,
2,2,2,2,2,2,2,2,2,2,2,2,3),(0.183333333333333,0.184313725490196,0.185294117647059,
0.186274509803922,0.187254901960784,0.188235294117647,0.18921568627451,
0.190196078431373,0.191176470588235,0.192156862745098,0.193137254901961,
0.194117647058824,0.195098039215686,0.196078431372549,0.197058823529412,
0.198039215686275,0.199019607843137,0.2,0.200980392156863,0.201960784313725,
0.202941176470588,0.203921568627451,0.204901960784314,0.205882352941176,
0.206862745098039,0.207843137254902,0.208823529411765,0.209803921568627,
0.21078431372549,0.211764705882353,0.212745098039216,0.213725490196078,
0.214705882352941,0.215686274509804,0.216666666666667),.UNSPECIFIED.)
CURVE()
GEOMETRIC_REPRESENTATION_ITEM()
RATIONAL_B_SPLINE_CURVE((1.,0.995734176295034,1.,0.995734176295034,1.,0.995734176295034,
1.,0.995734176295034,1.,0.995734176295034,1.,0.995734176295034,1.,0.995734176295034,
1.,0.995734176295034,1.,0.995734176295034,1.,0.995734176295034,1.,0.995734176295034,
1.,0.995734176295034,1.,0.995734176295034,1.,0.995734176295034,1.,0.995734176295034,
1.,0.995734176295034,1.,0.995734176295034,1.,0.995734176295034,1.,0.995734176295034,
1.,0.995734176295034,1.,0.995734176295034,1.,0.995734176295034,1.,0.995734176295034,
1.,0.995734176295034,1.,0.995734176295034,1.,0.995734176295034,1.,0.995734176295034,
1.,0.995734176295034,1.,0.995734176295034,1.,0.995734176295034,1.,0.995734176295034,
1.,0.995734176295034,1.,0.995734176295034,1.,0.995734176295034,1.))
REPRESENTATION_ITEM('')
);
#4078=(
BOUNDED_CURVE()
B_SPLINE_CURVE(2,(#144052,#144053,#144054,#144055,#144056,#144057,#144058,
#144059,#144060,#144061,#144062,#144063,#144064,#144065,#144066,#144067,
#144068,#144069,#144070,#144071,#144072,#144073,#144074,#144075,#144076,
#144077,#144078,#144079,#144080,#144081,#144082,#144083,#144084,#144085,
#144086,#144087,#144088,#144089,#144090,#144091,#144092,#144093,#144094,
#144095,#144096,#144097,#144098,#144099,#144100,#144101,#144102,#144103,
#144104,#144105,#144106,#144107,#144108,#144109,#144110,#144111,#144112,
#144113,#144114,#144115,#144116,#144117,#144118,#144119,#144120),
 .UNSPECIFIED.,.F.,.F.)
B_SPLINE_CURVE_WITH_KNOTS((3,2,2,2,2,2,2,2,2,2,2,2,2,2,2,2,2,2,2,2,2,2,
2,2,2,2,2,2,2,2,2,2,2,2,3),(0.185948268820395,0.186942644589488,0.187937020358581,
0.188931396127674,0.189925771896767,0.19092014766586,0.191914523434953,
0.192908899204046,0.193903274973139,0.194897650742232,0.195892026511325,
0.196886402280418,0.197880778049511,0.198875153818604,0.199869529587697,
0.20086390535679,0.201858281125883,0.202852656894976,0.203847032664069,
0.204841408433162,0.205835784202255,0.206830159971348,0.207824535740441,
0.208818911509534,0.209813287278627,0.210807663047721,0.211802038816814,
0.212796414585907,0.213790790355,0.214785166124093,0.215779541893186,0.216773917662279,
0.217768293431372,0.218762669200465,0.219757044969558),.UNSPECIFIED.)
CURVE()
GEOMETRIC_REPRESENTATION_ITEM()
RATIONAL_B_SPLINE_CURVE((1.,0.995734176295034,1.,0.995734176295034,1.,0.995734176295034,
1.,0.995734176295034,1.,0.995734176295034,1.,0.995734176295034,1.,0.995734176295034,
1.,0.995734176295034,1.,0.995734176295034,1.,0.995734176295034,1.,0.995734176295034,
1.,0.995734176295034,1.,0.995734176295034,1.,0.995734176295034,1.,0.995734176295034,
1.,0.995734176295034,1.,0.995734176295034,1.,0.995734176295034,1.,0.995734176295034,
1.,0.995734176295034,1.,0.995734176295034,1.,0.995734176295034,1.,0.995734176295034,
1.,0.995734176295034,1.,0.995734176295034,1.,0.995734176295034,1.,0.995734176295034,
1.,0.995734176295034,1.,0.995734176295034,1.,0.995734176295034,1.,0.995734176295034,
1.,0.995734176295034,1.,0.995734176295034,1.,0.995734176295034,1.))
REPRESENTATION_ITEM('')
);
#4079=(
BOUNDED_CURVE()
B_SPLINE_CURVE(2,(#144125,#144126,#144127,#144128,#144129,#144130,#144131,
#144132,#144133,#144134,#144135,#144136,#144137,#144138,#144139,#144140,
#144141,#144142,#144143,#144144,#144145,#144146,#144147,#144148,#144149,
#144150,#144151,#144152,#144153,#144154,#144155,#144156,#144157,#144158,
#144159,#144160,#144161,#144162,#144163,#144164,#144165,#144166,#144167,
#144168,#144169,#144170,#144171,#144172,#144173,#144174,#144175,#144176,
#144177,#144178,#144179,#144180,#144181,#144182,#144183,#144184,#144185,
#144186,#144187,#144188,#144189,#144190,#144191,#144192,#144193),
 .UNSPECIFIED.,.F.,.F.)
B_SPLINE_CURVE_WITH_KNOTS((3,2,2,2,2,2,2,2,2,2,2,2,2,2,2,2,2,2,2,2,2,2,
2,2,2,2,2,2,2,2,2,2,2,2,3),(0.216666666666667,0.217647058823529,0.218627450980392,
0.219607843137255,0.220588235294118,0.22156862745098,0.222549019607843,
0.223529411764706,0.224509803921569,0.225490196078431,0.226470588235294,
0.227450980392157,0.22843137254902,0.229411764705882,0.230392156862745,
0.231372549019608,0.232352941176471,0.233333333333333,0.234313725490196,
0.235294117647059,0.236274509803922,0.237254901960784,0.238235294117647,
0.23921568627451,0.240196078431373,0.241176470588235,0.242156862745098,
0.243137254901961,0.244117647058824,0.245098039215686,0.246078431372549,
0.247058823529412,0.248039215686275,0.249019607843137,0.25),
 .UNSPECIFIED.)
CURVE()
GEOMETRIC_REPRESENTATION_ITEM()
RATIONAL_B_SPLINE_CURVE((1.,0.995734176295034,1.,0.995734176295034,1.,0.995734176295034,
1.,0.995734176295034,1.,0.995734176295034,1.,0.995734176295034,1.,0.995734176295034,
1.,0.995734176295034,1.,0.995734176295034,1.,0.995734176295034,1.,0.995734176295034,
1.,0.995734176295034,1.,0.995734176295034,1.,0.995734176295034,1.,0.995734176295034,
1.,0.995734176295034,1.,0.995734176295034,1.,0.995734176295034,1.,0.995734176295034,
1.,0.995734176295034,1.,0.995734176295034,1.,0.995734176295034,1.,0.995734176295034,
1.,0.995734176295034,1.,0.995734176295034,1.,0.995734176295034,1.,0.995734176295034,
1.,0.995734176295034,1.,0.995734176295034,1.,0.995734176295034,1.,0.995734176295034,
1.,0.995734176295034,1.,0.995734176295034,1.,0.995734176295034,1.))
REPRESENTATION_ITEM('')
);
#4080=(
BOUNDED_CURVE()
B_SPLINE_CURVE(2,(#144194,#144195,#144196,#144197,#144198,#144199,#144200,
#144201,#144202,#144203,#144204,#144205,#144206,#144207,#144208,#144209,
#144210,#144211,#144212,#144213,#144214,#144215,#144216,#144217,#144218,
#144219,#144220,#144221,#144222,#144223,#144224,#144225,#144226,#144227,
#144228,#144229,#144230,#144231,#144232,#144233,#144234,#144235,#144236,
#144237,#144238,#144239,#144240,#144241,#144242,#144243,#144244,#144245,
#144246,#144247,#144248,#144249,#144250,#144251,#144252,#144253,#144254,
#144255,#144256,#144257,#144258,#144259,#144260,#144261,#144262),
 .UNSPECIFIED.,.F.,.F.)
B_SPLINE_CURVE_WITH_KNOTS((3,2,2,2,2,2,2,2,2,2,2,2,2,2,2,2,2,2,2,2,2,2,
2,2,2,2,2,2,2,2,2,2,2,2,3),(0.219757044969558,0.220751420738651,0.221745796507744,
0.222740172276837,0.22373454804593,0.224728923815023,0.225723299584116,
0.226717675353209,0.227712051122302,0.228706426891395,0.229700802660488,
0.230695178429581,0.231689554198674,0.232683929967767,0.23367830573686,
0.234672681505953,0.235667057275046,0.236661433044139,0.237655808813232,
0.238650184582325,0.239644560351418,0.240638936120511,0.241633311889604,
0.242627687658697,0.24362206342779,0.244616439196883,0.245610814965976,
0.246605190735069,0.247599566504162,0.248593942273255,0.249588318042348,
0.250582693811441,0.251577069580534,0.252571445349627,0.25356582111872),
 .UNSPECIFIED.)
CURVE()
GEOMETRIC_REPRESENTATION_ITEM()
RATIONAL_B_SPLINE_CURVE((1.,0.995734176295034,1.,0.995734176295034,1.,0.995734176295034,
1.,0.995734176295034,1.,0.995734176295034,1.,0.995734176295034,1.,0.995734176295034,
1.,0.995734176295034,1.,0.995734176295034,1.,0.995734176295034,1.,0.995734176295034,
1.,0.995734176295034,1.,0.995734176295034,1.,0.995734176295034,1.,0.995734176295034,
1.,0.995734176295034,1.,0.995734176295034,1.,0.995734176295034,1.,0.995734176295034,
1.,0.995734176295034,1.,0.995734176295034,1.,0.995734176295034,1.,0.995734176295034,
1.,0.995734176295034,1.,0.995734176295034,1.,0.995734176295034,1.,0.995734176295034,
1.,0.995734176295034,1.,0.995734176295034,1.,0.995734176295034,1.,0.995734176295034,
1.,0.995734176295034,1.,0.995734176295034,1.,0.995734176295034,1.))
REPRESENTATION_ITEM('')
);
#4081=(
BOUNDED_CURVE()
B_SPLINE_CURVE(2,(#149844,#149845,#149846,#149847,#149848,#149849,#149850,
#149851,#149852,#149853,#149854,#149855,#149856,#149857,#149858,#149859,
#149860,#149861,#149862,#149863,#149864,#149865,#149866,#149867,#149868,
#149869,#149870,#149871,#149872,#149873,#149874,#149875,#149876,#149877,
#149878,#149879,#149880,#149881,#149882,#149883,#149884,#149885,#149886,
#149887,#149888,#149889,#149890,#149891,#149892,#149893,#149894,#149895,
#149896,#149897,#149898,#149899,#149900,#149901,#149902,#149903,#149904,
#149905,#149906,#149907,#149908,#149909,#149910,#149911,#149912,#149913,
#149914,#149915,#149916,#149917,#149918,#149919,#149920,#149921,#149922,
#149923,#149924,#149925,#149926,#149927,#149928,#149929,#149930,#149931,
#149932,#149933,#149934,#149935,#149936,#149937,#149938,#149939,#149940,
#149941,#149942,#149943,#149944,#149945,#149946,#149947,#149948,#149949,
#149950,#149951,#149952,#149953,#149954,#149955,#149956,#149957,#149958,
#149959,#149960,#149961,#149962,#149963,#149964,#149965,#149966,#149967,
#149968,#149969,#149970,#149971,#149972,#149973,#149974,#149975,#149976,
#149977,#149978,#149979,#149980,#149981,#149982,#149983,#149984,#149985,
#149986,#149987,#149988,#149989,#149990,#149991,#149992,#149993,#149994,
#149995,#149996,#149997,#149998,#149999,#150000,#150001,#150002,#150003,
#150004,#150005,#150006,#150007,#150008,#150009,#150010,#150011,#150012,
#150013,#150014,#150015,#150016,#150017,#150018,#150019,#150020,#150021,
#150022,#150023,#150024,#150025,#150026,#150027,#150028,#150029,#150030,
#150031,#150032,#150033,#150034,#150035,#150036,#150037,#150038,#150039,
#150040,#150041,#150042,#150043,#150044,#150045,#150046,#150047,#150048,
#150049,#150050,#150051,#150052,#150053,#150054,#150055,#150056,#150057,
#150058,#150059,#150060,#150061,#150062,#150063,#150064,#150065,#150066,
#150067,#150068,#150069,#150070,#150071,#150072,#150073,#150074,#150075,
#150076,#150077,#150078,#150079,#150080,#150081,#150082,#150083,#150084,
#150085,#150086,#150087,#150088,#150089,#150090,#150091,#150092,#150093,
#150094,#150095,#150096,#150097,#150098,#150099,#150100,#150101,#150102,
#150103,#150104,#150105,#150106,#150107,#150108,#150109,#150110,#150111,
#150112,#150113,#150114,#150115,#150116,#150117,#150118,#150119,#150120,
#150121,#150122,#150123,#150124,#150125,#150126,#150127,#150128,#150129,
#150130,#150131,#150132,#150133,#150134,#150135,#150136,#150137,#150138,
#150139,#150140,#150141,#150142,#150143,#150144,#150145,#150146,#150147,
#150148,#150149,#150150,#150151,#150152,#150153,#150154,#150155,#150156,
#150157,#150158,#150159,#150160,#150161,#150162,#150163,#150164,#150165,
#150166,#150167,#150168,#150169,#150170,#150171,#150172,#150173,#150174,
#150175,#150176,#150177,#150178,#150179,#150180,#150181,#150182,#150183,
#150184,#150185,#150186,#150187,#150188,#150189,#150190,#150191,#150192,
#150193,#150194,#150195,#150196,#150197,#150198,#150199,#150200,#150201,
#150202,#150203,#150204,#150205,#150206,#150207,#150208,#150209,#150210,
#150211,#150212,#150213,#150214,#150215,#150216,#150217,#150218,#150219,
#150220,#150221,#150222,#150223,#150224,#150225,#150226,#150227,#150228,
#150229,#150230,#150231,#150232,#150233,#150234,#150235,#150236,#150237,
#150238,#150239,#150240,#150241,#150242,#150243,#150244,#150245,#150246,
#150247,#150248,#150249,#150250,#150251,#150252,#150253,#150254,#150255,
#150256,#150257,#150258,#150259,#150260,#150261,#150262,#150263,#150264,
#150265,#150266,#150267,#150268,#150269,#150270,#150271,#150272,#150273,
#150274,#150275,#150276,#150277,#150278,#150279,#150280,#150281,#150282,
#150283,#150284,#150285,#150286,#150287,#150288,#150289,#150290,#150291,
#150292,#150293,#150294,#150295,#150296,#150297,#150298,#150299,#150300,
#150301,#150302,#150303,#150304,#150305,#150306,#150307,#150308,#150309,
#150310,#150311,#150312,#150313,#150314,#150315,#150316,#150317,#150318,
#150319,#150320,#150321,#150322,#150323,#150324,#150325,#150326,#150327,
#150328,#150329,#150330,#150331,#150332,#150333,#150334,#150335,#150336,
#150337,#150338,#150339,#150340,#150341,#150342,#150343,#150344,#150345,
#150346,#150347,#150348,#150349,#150350,#150351,#150352,#150353,#150354,
#150355,#150356,#150357,#150358,#150359,#150360,#150361,#150362,#150363,
#150364,#150365,#150366,#150367,#150368,#150369,#150370,#150371,#150372,
#150373,#150374,#150375,#150376,#150377,#150378,#150379,#150380,#150381,
#150382,#150383,#150384,#150385,#150386),.UNSPECIFIED.,.F.,.F.)
B_SPLINE_CURVE_WITH_KNOTS((3,2,2,2,2,2,2,2,2,2,2,2,2,2,2,2,2,2,2,2,2,2,
2,2,2,2,2,2,2,2,2,2,2,2,2,2,2,2,2,2,2,2,2,2,2,2,2,2,2,2,2,2,2,2,2,2,2,2,
2,2,2,2,2,2,2,2,2,2,2,2,2,2,2,2,2,2,2,2,2,2,2,2,2,2,2,2,2,2,2,2,2,2,2,2,
2,2,2,2,2,2,2,2,2,2,2,2,2,2,2,2,2,2,2,2,2,2,2,2,2,2,2,2,2,2,2,2,2,2,2,2,
2,2,2,2,2,2,2,2,2,2,2,2,2,2,2,2,2,2,2,2,2,2,2,2,2,2,2,2,2,2,2,2,2,2,2,2,
2,2,2,2,2,2,2,2,2,2,2,2,2,2,2,2,2,2,2,2,2,2,2,2,2,2,2,2,2,2,2,2,2,2,2,2,
2,2,2,2,2,2,2,2,2,2,2,2,2,2,2,2,2,2,2,2,2,2,2,2,2,2,2,2,2,2,2,2,2,2,2,2,
2,2,2,2,2,2,2,2,2,2,2,2,2,2,2,2,2,2,2,2,2,2,2,2,2,2,2,2,2,2,2,2,2,3),(0.,
0.0009943756807032,0.0019887513614064,0.0029831270421096,0.0039775027228128,
0.004971878403516,0.0059662540842192,0.0069606297649224,0.0079550054456256,
0.0089493811263288,0.009943756807032,0.0109381324877352,0.0119325081684384,
0.0129268838491416,0.0139212595298448,0.014915635210548,0.0159100108912512,
0.0169043865719544,0.0178987622526576,0.0188931379333608,0.019887513614064,
0.0208818892947672,0.0218762649754704,0.0228706406561736,0.0238650163368768,
0.02485939201758,0.0258537676982832,0.0268481433789864,0.0278425190596896,
0.0288368947403928,0.029831270421096,0.0308256461017992,0.0318200217825024,
0.0328143974632056,0.0338087731439088,0.034803148824612,0.0357975245053152,
0.0367919001860184,0.0377862758667216,0.0387806515474248,0.039775027228128,
0.0407694029088312,0.0417637785895344,0.0427581542702376,0.0437525299509408,
0.044746905631644,0.0457412813123472,0.0467356569930504,0.0477300326737536,
0.0487244083544568,0.04971878403516,0.0507131597158632,0.0517075353965664,
0.0527019110772696,0.0536962867579728,0.054690662438676,0.0556850381193792,
0.0566794138000824,0.0576737894807856,0.0586681651614888,0.059662540842192,
0.0606569165228952,0.0616512922035984,0.0626456678843016,0.0636400435650048,
0.064634419245708,0.0656287949264112,0.0666231706071144,0.0676175462878176,
0.0686119219685208,0.069606297649224,0.0706006733299272,0.0715950490106304,
0.0725894246913336,0.0735838003720368,0.07457817605274,0.0755725517334432,
0.0765669274141464,0.0775613030948496,0.0785556787755528,0.079550054456256,
0.0805444301369592,0.0815388058176624,0.0825331814983656,0.0835275571790688,
0.084521932859772,0.0855163085404752,0.0865106842211784,0.0875050599018816,
0.0884994355825848,0.089493811263288,0.0904881869439912,0.0914825626246944,
0.0924769383053976,0.0934713139861008,0.094465689666804,0.0954600653475072,
0.0964544410282104,0.0974488167089136,0.0984431923896168,0.09943756807032,
0.100431943751023,0.101426319431726,0.10242069511243,0.103415070793133,
0.104409446473836,0.105403822154539,0.106398197835242,0.107392573515946,
0.108386949196649,0.109381324877352,0.110375700558055,0.111370076238758,
0.112364451919462,0.113358827600165,0.114353203280868,0.115347578961571,
0.116341954642274,0.117336330322978,0.118330706003681,0.119325081684384,
0.120319457365087,0.12131383304579,0.122308208726494,0.123302584407197,
0.1242969600879,0.125291335768603,0.126285711449306,0.12728008713001,0.128274462810713,
0.129268838491416,0.130263214172119,0.131257589852822,0.132251965533526,
0.133246341214229,0.134240716894932,0.135235092575635,0.136229468256338,
0.137223843937042,0.138218219617745,0.139212595298448,0.140206970979151,
0.141201346659854,0.142195722340558,0.143190098021261,0.144184473701964,
0.145178849382667,0.14617322506337,0.147167600744074,0.148161976424777,
0.14915635210548,0.150150727786183,0.151145103466886,0.15213947914759,0.153133854828293,
0.154128230508996,0.155122606189699,0.156116981870402,0.157111357551106,
0.158105733231809,0.159100108912512,0.160094484593215,0.161088860273918,
0.162083235954622,0.163077611635325,0.164071987316028,0.165066362996731,
0.166060738677434,0.167055114358138,0.168049490038841,0.169043865719544,
0.170038241400247,0.17103261708095,0.172026992761654,0.173021368442357,
0.17401574412306,0.175010119803763,0.176004495484466,0.17699887116517,0.177993246845873,
0.178987622526576,0.179981998207279,0.180976373887982,0.181970749568686,
0.182965125249389,0.183959500930092,0.184953876610795,0.185948252291498,
0.186942627972202,0.187937003652905,0.188931379333608,0.189925755014311,
0.190920130695014,0.191914506375718,0.192908882056421,0.193903257737124,
0.194897633417827,0.19589200909853,0.196886384779234,0.197880760459937,
0.19887513614064,0.199869511821343,0.200863887502046,0.20185826318275,0.202852638863453,
0.203847014544156,0.204841390224859,0.205835765905562,0.206830141586266,
0.207824517266969,0.208818892947672,0.209813268628375,0.210807644309078,
0.211802019989782,0.212796395670485,0.213790771351188,0.214785147031891,
0.215779522712594,0.216773898393298,0.217768274074001,0.218762649754704,
0.219757025435407,0.22075140111611,0.221745776796814,0.222740152477517,
0.22373452815822,0.224728903838923,0.225723279519626,0.22671765520033,0.227712030881033,
0.228706406561736,0.229700782242439,0.230695157923142,0.231689533603846,
0.232683909284549,0.233678284965252,0.234672660645955,0.235667036326658,
0.236661412007362,0.237655787688065,0.238650163368768,0.239644539049471,
0.240638914730174,0.241633290410878,0.242627666091581,0.243622041772284,
0.244616417452987,0.24561079313369,0.246605168814394,0.247599544495097,
0.2485939201758,0.249588295856503,0.250582671537206,0.25157704721791,0.252571422898613,
0.253565798579316,0.254560174260019,0.255554549940722,0.256548925621426,
0.257543301302129,0.258537676982832,0.259532052663535,0.260526428344238,
0.261520804024942,0.262515179705645,0.263509555386348,0.264503931067051,
0.265498306747754,0.266492682428458,0.267487058109161,0.268481433789864,
0.268969065897308),.UNSPECIFIED.)
CURVE()
GEOMETRIC_REPRESENTATION_ITEM()
RATIONAL_B_SPLINE_CURVE((1.,0.995734176295034,1.,0.995734176295034,1.,0.995734176295034,
1.,0.995734176295034,1.,0.995734176295034,1.,0.995734176295034,1.,0.995734176295034,
1.,0.995734176295034,1.,0.995734176295034,1.,0.995734176295034,1.,0.995734176295034,
1.,0.995734176295034,1.,0.995734176295034,1.,0.995734176295034,1.,0.995734176295034,
1.,0.995734176295034,1.,0.995734176295034,1.,0.995734176295034,1.,0.995734176295034,
1.,0.995734176295034,1.,0.995734176295034,1.,0.995734176295034,1.,0.995734176295034,
1.,0.995734176295034,1.,0.995734176295034,1.,0.995734176295034,1.,0.995734176295034,
1.,0.995734176295034,1.,0.995734176295034,1.,0.995734176295034,1.,0.995734176295034,
1.,0.995734176295034,1.,0.995734176295034,1.,0.995734176295034,1.,0.995734176295034,
1.,0.995734176295034,1.,0.995734176295034,1.,0.995734176295034,1.,0.995734176295034,
1.,0.995734176295034,1.,0.995734176295034,1.,0.995734176295034,1.,0.995734176295034,
1.,0.995734176295034,1.,0.995734176295034,1.,0.995734176295034,1.,0.995734176295034,
1.,0.995734176295034,1.,0.995734176295034,1.,0.995734176295034,1.,0.995734176295034,
1.,0.995734176295034,1.,0.995734176295034,1.,0.995734176295034,1.,0.995734176295034,
1.,0.995734176295034,1.,0.995734176295034,1.,0.995734176295034,1.,0.995734176295034,
1.,0.995734176295034,1.,0.995734176295034,1.,0.995734176295034,1.,0.995734176295034,
1.,0.995734176295034,1.,0.995734176295034,1.,0.995734176295034,1.,0.995734176295034,
1.,0.995734176295034,1.,0.995734176295034,1.,0.995734176295034,1.,0.995734176295034,
1.,0.995734176295034,1.,0.995734176295034,1.,0.995734176295034,1.,0.995734176295034,
1.,0.995734176295034,1.,0.995734176295034,1.,0.995734176295034,1.,0.995734176295034,
1.,0.995734176295034,1.,0.995734176295034,1.,0.995734176295034,1.,0.995734176295034,
1.,0.995734176295034,1.,0.995734176295034,1.,0.995734176295034,1.,0.995734176295034,
1.,0.995734176295034,1.,0.995734176295034,1.,0.995734176295034,1.,0.995734176295034,
1.,0.995734176295034,1.,0.995734176295034,1.,0.995734176295034,1.,0.995734176295034,
1.,0.995734176295034,1.,0.995734176295034,1.,0.995734176295034,1.,0.995734176295034,
1.,0.995734176295034,1.,0.995734176295034,1.,0.995734176295034,1.,0.995734176295034,
1.,0.995734176295034,1.,0.995734176295034,1.,0.995734176295034,1.,0.995734176295034,
1.,0.995734176295034,1.,0.995734176295034,1.,0.995734176295034,1.,0.995734176295034,
1.,0.995734176295034,1.,0.995734176295034,1.,0.995734176295034,1.,0.995734176295034,
1.,0.995734176295034,1.,0.995734176295034,1.,0.995734176295034,1.,0.995734176295034,
1.,0.995734176295034,1.,0.995734176295034,1.,0.995734176295034,1.,0.995734176295034,
1.,0.995734176295034,1.,0.995734176295034,1.,0.995734176295034,1.,0.995734176295034,
1.,0.995734176295034,1.,0.995734176295034,1.,0.995734176295034,1.,0.995734176295034,
1.,0.995734176295034,1.,0.995734176295034,1.,0.995734176295034,1.,0.995734176295034,
1.,0.995734176295034,1.,0.995734176295034,1.,0.995734176295034,1.,0.995734176295034,
1.,0.995734176295034,1.,0.995734176295034,1.,0.995734176295034,1.,0.995734176295034,
1.,0.995734176295034,1.,0.995734176295034,1.,0.995734176295034,1.,0.995734176295034,
1.,0.995734176295034,1.,0.995734176295034,1.,0.995734176295034,1.,0.995734176295034,
1.,0.995734176295034,1.,0.995734176295034,1.,0.995734176295034,1.,0.995734176295034,
1.,0.995734176295034,1.,0.995734176295034,1.,0.995734176295034,1.,0.995734176295034,
1.,0.995734176295034,1.,0.995734176295034,1.,0.995734176295034,1.,0.995734176295034,
1.,0.995734176295034,1.,0.995734176295034,1.,0.995734176295034,1.,0.995734176295034,
1.,0.995734176295034,1.,0.995734176295034,1.,0.995734176295034,1.,0.995734176295034,
1.,0.995734176295034,1.,0.995734176295034,1.,0.995734176295034,1.,0.995734176295034,
1.,0.995734176295034,1.,0.995734176295034,1.,0.995734176295034,1.,0.995734176295034,
1.,0.995734176295034,1.,0.995734176295034,1.,0.995734176295034,1.,0.995734176295034,
1.,0.995734176295034,1.,0.995734176295034,1.,0.995734176295034,1.,0.995734176295034,
1.,0.995734176295034,1.,0.995734176295034,1.,0.995734176295034,1.,0.995734176295034,
1.,0.995734176295034,1.,0.995734176295034,1.,0.995734176295034,1.,0.995734176295034,
1.,0.995734176295034,1.,0.995734176295034,1.,0.995734176295034,1.,0.995734176295034,
1.,0.995734176295034,1.,0.995734176295034,1.,0.995734176295034,1.,0.995734176295034,
1.,0.995734176295034,1.,0.995734176295034,1.,0.995734176295034,1.,0.995734176295034,
1.,0.995734176295034,1.,0.995734176295034,1.,0.995734176295034,1.,0.995734176295034,
1.,0.995734176295034,1.,0.995734176295034,1.,0.995734176295034,1.,0.995734176295034,
1.,0.995734176295034,1.,0.995734176295034,1.,0.995734176295034,1.,0.995734176295034,
1.,0.995734176295034,1.,0.995734176295034,1.,0.995734176295034,1.,0.995734176295034,
1.,0.995734176295034,1.,0.995734176295034,1.,0.995734176295034,1.,0.995734176295034,
1.,0.995734176295034,1.,0.995734176295034,1.,0.995734176295034,1.,0.995734176295034,
1.,0.995734176295034,1.,0.995734176295034,1.,0.995734176295034,1.,0.995734176295034,
1.,0.995734176295034,1.,0.995734176295034,1.,0.995734176295034,1.,0.995734176295034,
1.,0.995734176295034,1.,0.995734176295034,1.,0.995734176295034,1.,0.995734176295034,
1.,0.995734176295034,1.,0.995734176295034,1.,0.995734176295034,1.,0.995734176295034,
1.,0.995734176295034,1.,0.995734176295034,1.,0.995734176295034,1.,0.995734176295034,
1.,0.995734176295034,1.,0.995734176295034,1.,0.995734176295034,1.,0.995734176295034,
1.,0.995734176295034,1.,0.995734176295034,1.,0.995734176295034,1.,0.995734176295034,
1.,0.995734176295034,1.,0.995734176295034,1.,0.995734176295034,1.,0.995734176295034,
1.,0.995734176295034,1.,0.995734176295034,1.,0.995734176295034,1.,0.995734176295034,
1.,0.995734176295034,1.,0.995734176295034,1.,0.995734176295034,1.,0.997908081780755,
0.997867876027224))
REPRESENTATION_ITEM('')
);
#4082=(
BOUNDED_CURVE()
B_SPLINE_CURVE(2,(#154422,#154423,#154424,#154425,#154426,#154427,#154428,
#154429,#154430,#154431,#154432,#154433,#154434,#154435,#154436,#154437,
#154438,#154439,#154440,#154441,#154442,#154443,#154444,#154445,#154446,
#154447,#154448,#154449,#154450,#154451,#154452,#154453,#154454,#154455,
#154456,#154457,#154458),.UNSPECIFIED.,.F.,.F.)
B_SPLINE_CURVE_WITH_KNOTS((3,2,2,2,2,2,2,2,2,2,2,2,2,2,2,2,2,2,3),(0.25,
0.250980392156863,0.251960784313725,0.252941176470588,0.253921568627451,
0.254901960784314,0.255882352941176,0.256862745098039,0.257843137254902,
0.258823529411765,0.259803921568627,0.26078431372549,0.261764705882353,
0.262745098039216,0.263725490196078,0.264705882352941,0.265686274509804,
0.266666666666667,0.26668268661721),.UNSPECIFIED.)
CURVE()
GEOMETRIC_REPRESENTATION_ITEM()
RATIONAL_B_SPLINE_CURVE((1.,0.995734176295034,1.,0.995734176295034,1.,0.995734176295034,
1.,0.995734176295034,1.,0.995734176295034,1.,0.995734176295034,1.,0.995734176295034,
1.,0.995734176295034,1.,0.995734176295034,1.,0.995734176295034,1.,0.995734176295034,
1.,0.995734176295034,1.,0.995734176295034,1.,0.995734176295034,1.,0.995734176295034,
1.,0.995734176295034,1.,0.995734176295034,1.,0.999930294949526,0.999862867908832))
REPRESENTATION_ITEM('')
);
#4083=(
BOUNDED_CURVE()
B_SPLINE_CURVE(2,(#158491,#158492,#158493,#158494,#158495,#158496,#158497,
#158498,#158499,#158500,#158501,#158502,#158503,#158504,#158505,#158506,
#158507,#158508,#158509,#158510,#158511,#158512,#158513,#158514,#158515,
#158516,#158517,#158518,#158519,#158520,#158521,#158522,#158523,#158524,
#158525,#158526,#158527),.UNSPECIFIED.,.F.,.F.)
B_SPLINE_CURVE_WITH_KNOTS((3,2,2,2,2,2,2,2,2,2,2,2,2,2,2,2,2,2,3),(0.25356582111872,
0.254560196887814,0.255554572656907,0.256548948426,0.257543324195093,0.258537699964186,
0.259532075733279,0.260526451502372,0.261520827271465,0.262515203040558,
0.263509578809651,0.264503954578744,0.265498330347837,0.26649270611693,
0.267487081886023,0.268481457655116,0.269475833424209,0.270470209193302,
0.27052030629005),.UNSPECIFIED.)
CURVE()
GEOMETRIC_REPRESENTATION_ITEM()
RATIONAL_B_SPLINE_CURVE((1.,0.995734176295034,1.,0.995734176295034,1.,0.995734176295034,
1.,0.995734176295034,1.,0.995734176295034,1.,0.995734176295034,1.,0.995734176295034,
1.,0.995734176295034,1.,0.995734176295034,1.,0.995734176295034,1.,0.995734176295034,
1.,0.995734176295034,1.,0.995734176295034,1.,0.995734176295034,1.,0.995734176295034,
1.,0.995734176295034,1.,0.995734176295034,1.,0.999785085890563,0.999591826719365))
REPRESENTATION_ITEM('')
);
#4084=(
BOUNDED_CURVE()
B_SPLINE_CURVE(2,(#162564,#162565,#162566,#162567,#162568,#162569,#162570,
#162571,#162572,#162573,#162574,#162575,#162576,#162577,#162578,#162579,
#162580,#162581,#162582,#162583,#162584,#162585,#162586,#162587,#162588,
#162589,#162590,#162591,#162592,#162593,#162594,#162595,#162596,#162597,
#162598,#162599,#162600,#162601,#162602,#162603,#162604,#162605,#162606,
#162607,#162608,#162609,#162610,#162611,#162612,#162613,#162614,#162615,
#162616,#162617,#162618,#162619,#162620,#162621,#162622,#162623,#162624,
#162625,#162626,#162627,#162628,#162629,#162630,#162631,#162632,#162633,
#162634,#162635,#162636,#162637,#162638,#162639,#162640,#162641,#162642,
#162643,#162644,#162645,#162646,#162647,#162648,#162649,#162650,#162651,
#162652,#162653,#162654,#162655,#162656,#162657,#162658,#162659,#162660,
#162661,#162662,#162663,#162664,#162665,#162666,#162667,#162668,#162669,
#162670,#162671,#162672,#162673,#162674,#162675,#162676,#162677,#162678,
#162679,#162680,#162681,#162682,#162683,#162684,#162685,#162686,#162687,
#162688,#162689,#162690,#162691,#162692,#162693,#162694,#162695,#162696,
#162697,#162698,#162699,#162700,#162701,#162702,#162703,#162704,#162705,
#162706,#162707,#162708,#162709,#162710,#162711,#162712,#162713,#162714,
#162715,#162716,#162717,#162718,#162719,#162720,#162721,#162722,#162723,
#162724,#162725,#162726,#162727,#162728,#162729,#162730,#162731,#162732,
#162733,#162734,#162735,#162736,#162737,#162738,#162739,#162740,#162741,
#162742,#162743,#162744,#162745,#162746,#162747,#162748,#162749,#162750,
#162751,#162752,#162753,#162754,#162755,#162756,#162757,#162758,#162759,
#162760,#162761,#162762,#162763,#162764,#162765,#162766,#162767,#162768,
#162769,#162770,#162771,#162772,#162773,#162774,#162775,#162776,#162777,
#162778,#162779,#162780,#162781,#162782,#162783,#162784,#162785,#162786,
#162787,#162788,#162789,#162790,#162791,#162792,#162793,#162794,#162795,
#162796,#162797,#162798,#162799,#162800,#162801,#162802,#162803,#162804,
#162805,#162806,#162807,#162808,#162809,#162810,#162811,#162812,#162813,
#162814,#162815,#162816,#162817,#162818,#162819,#162820,#162821,#162822,
#162823,#162824,#162825,#162826,#162827,#162828,#162829,#162830,#162831,
#162832,#162833,#162834,#162835,#162836,#162837,#162838,#162839,#162840,
#162841,#162842,#162843,#162844,#162845,#162846,#162847,#162848,#162849,
#162850,#162851,#162852,#162853,#162854,#162855,#162856,#162857,#162858,
#162859,#162860,#162861,#162862,#162863,#162864,#162865,#162866,#162867,
#162868,#162869,#162870,#162871,#162872,#162873,#162874,#162875,#162876,
#162877,#162878,#162879,#162880,#162881,#162882,#162883,#162884,#162885,
#162886,#162887,#162888,#162889,#162890,#162891,#162892,#162893,#162894,
#162895,#162896,#162897,#162898,#162899,#162900,#162901,#162902,#162903,
#162904,#162905,#162906,#162907,#162908,#162909,#162910,#162911,#162912,
#162913,#162914,#162915,#162916,#162917,#162918,#162919,#162920,#162921,
#162922,#162923,#162924,#162925,#162926,#162927,#162928,#162929,#162930,
#162931,#162932,#162933,#162934,#162935,#162936,#162937,#162938,#162939,
#162940,#162941,#162942,#162943,#162944,#162945,#162946,#162947,#162948,
#162949,#162950,#162951,#162952,#162953,#162954,#162955,#162956,#162957,
#162958,#162959,#162960,#162961,#162962,#162963,#162964,#162965,#162966,
#162967,#162968,#162969,#162970,#162971,#162972,#162973,#162974,#162975,
#162976,#162977,#162978,#162979,#162980,#162981,#162982,#162983,#162984,
#162985,#162986,#162987,#162988,#162989,#162990,#162991,#162992,#162993,
#162994,#162995,#162996,#162997,#162998,#162999,#163000,#163001,#163002,
#163003,#163004,#163005,#163006,#163007,#163008,#163009,#163010,#163011,
#163012,#163013,#163014,#163015,#163016,#163017,#163018,#163019,#163020,
#163021,#163022,#163023,#163024,#163025,#163026,#163027,#163028,#163029,
#163030,#163031,#163032,#163033,#163034,#163035,#163036,#163037,#163038,
#163039,#163040,#163041,#163042,#163043,#163044,#163045,#163046,#163047,
#163048,#163049,#163050,#163051,#163052,#163053,#163054,#163055,#163056,
#163057,#163058,#163059,#163060,#163061,#163062,#163063,#163064,#163065,
#163066,#163067,#163068,#163069,#163070,#163071,#163072,#163073,#163074,
#163075,#163076,#163077,#163078,#163079,#163080,#163081,#163082,#163083,
#163084,#163085,#163086,#163087,#163088,#163089,#163090,#163091,#163092,
#163093,#163094,#163095,#163096,#163097,#163098,#163099,#163100,#163101,
#163102,#163103,#163104,#163105,#163106),.UNSPECIFIED.,.F.,.F.)
B_SPLINE_CURVE_WITH_KNOTS((3,2,2,2,2,2,2,2,2,2,2,2,2,2,2,2,2,2,2,2,2,2,
2,2,2,2,2,2,2,2,2,2,2,2,2,2,2,2,2,2,2,2,2,2,2,2,2,2,2,2,2,2,2,2,2,2,2,2,
2,2,2,2,2,2,2,2,2,2,2,2,2,2,2,2,2,2,2,2,2,2,2,2,2,2,2,2,2,2,2,2,2,2,2,2,
2,2,2,2,2,2,2,2,2,2,2,2,2,2,2,2,2,2,2,2,2,2,2,2,2,2,2,2,2,2,2,2,2,2,2,2,
2,2,2,2,2,2,2,2,2,2,2,2,2,2,2,2,2,2,2,2,2,2,2,2,2,2,2,2,2,2,2,2,2,2,2,2,
2,2,2,2,2,2,2,2,2,2,2,2,2,2,2,2,2,2,2,2,2,2,2,2,2,2,2,2,2,2,2,2,2,2,2,2,
2,2,2,2,2,2,2,2,2,2,2,2,2,2,2,2,2,2,2,2,2,2,2,2,2,2,2,2,2,2,2,2,2,2,2,2,
2,2,2,2,2,2,2,2,2,2,2,2,2,2,2,2,2,2,2,2,2,2,2,2,2,2,2,2,2,2,2,2,2,3),(0.,
0.000980392156862745,0.00196078431372549,0.00294117647058824,0.00392156862745098,
0.00490196078431373,0.00588235294117647,0.00686274509803922,0.00784313725490196,
0.00882352941176471,0.00980392156862745,0.0107843137254902,0.0117647058823529,
0.0127450980392157,0.0137254901960784,0.0147058823529412,0.0156862745098039,
0.0166666666666667,0.0176470588235294,0.0186274509803922,0.0196078431372549,
0.0205882352941176,0.0215686274509804,0.0225490196078431,0.0235294117647059,
0.0245098039215686,0.0254901960784314,0.0264705882352941,0.0274509803921569,
0.0284313725490196,0.0294117647058824,0.0303921568627451,0.0313725490196078,
0.0323529411764706,0.0333333333333333,0.0343137254901961,0.0352941176470588,
0.0362745098039216,0.0372549019607843,0.0382352941176471,0.0392156862745098,
0.0401960784313726,0.0411764705882353,0.042156862745098,0.0431372549019608,
0.0441176470588235,0.0450980392156863,0.046078431372549,0.0470588235294118,
0.0480392156862745,0.0490196078431373,0.05,0.0509803921568627,0.0519607843137255,
0.0529411764705882,0.053921568627451,0.0549019607843137,0.0558823529411765,
0.0568627450980392,0.057843137254902,0.0588235294117647,0.0598039215686275,
0.0607843137254902,0.0617647058823529,0.0627450980392157,0.0637254901960784,
0.0647058823529412,0.0656862745098039,0.0666666666666667,0.0676470588235294,
0.0686274509803922,0.0696078431372549,0.0705882352941176,0.0715686274509804,
0.0725490196078431,0.0735294117647059,0.0745098039215686,0.0754901960784314,
0.0764705882352941,0.0774509803921569,0.0784313725490196,0.0794117647058823,
0.0803921568627451,0.0813725490196078,0.0823529411764706,0.0833333333333333,
0.0843137254901961,0.0852941176470588,0.0862745098039216,0.0872549019607843,
0.0882352941176471,0.0892156862745098,0.0901960784313725,0.0911764705882353,
0.092156862745098,0.0931372549019608,0.0941176470588235,0.0950980392156863,
0.096078431372549,0.0970588235294118,0.0980392156862745,0.0990196078431373,
0.1,0.100980392156863,0.101960784313725,0.102941176470588,0.103921568627451,
0.104901960784314,0.105882352941176,0.106862745098039,0.107843137254902,
0.108823529411765,0.109803921568627,0.11078431372549,0.111764705882353,
0.112745098039216,0.113725490196078,0.114705882352941,0.115686274509804,
0.116666666666667,0.117647058823529,0.118627450980392,0.119607843137255,
0.120588235294118,0.12156862745098,0.122549019607843,0.123529411764706,
0.124509803921569,0.125490196078431,0.126470588235294,0.127450980392157,
0.12843137254902,0.129411764705882,0.130392156862745,0.131372549019608,
0.132352941176471,0.133333333333333,0.134313725490196,0.135294117647059,
0.136274509803922,0.137254901960784,0.138235294117647,0.13921568627451,
0.140196078431373,0.141176470588235,0.142156862745098,0.143137254901961,
0.144117647058824,0.145098039215686,0.146078431372549,0.147058823529412,
0.148039215686275,0.149019607843137,0.15,0.150980392156863,0.151960784313725,
0.152941176470588,0.153921568627451,0.154901960784314,0.155882352941176,
0.156862745098039,0.157843137254902,0.158823529411765,0.159803921568627,
0.16078431372549,0.161764705882353,0.162745098039216,0.163725490196078,
0.164705882352941,0.165686274509804,0.166666666666667,0.167647058823529,
0.168627450980392,0.169607843137255,0.170588235294118,0.17156862745098,
0.172549019607843,0.173529411764706,0.174509803921569,0.175490196078431,
0.176470588235294,0.177450980392157,0.17843137254902,0.179411764705882,
0.180392156862745,0.181372549019608,0.182352941176471,0.183333333333333,
0.184313725490196,0.185294117647059,0.186274509803922,0.187254901960784,
0.188235294117647,0.18921568627451,0.190196078431373,0.191176470588235,
0.192156862745098,0.193137254901961,0.194117647058824,0.195098039215686,
0.196078431372549,0.197058823529412,0.198039215686275,0.199019607843137,
0.2,0.200980392156863,0.201960784313725,0.202941176470588,0.203921568627451,
0.204901960784314,0.205882352941176,0.206862745098039,0.207843137254902,
0.208823529411765,0.209803921568627,0.21078431372549,0.211764705882353,
0.212745098039216,0.213725490196078,0.214705882352941,0.215686274509804,
0.216666666666667,0.217647058823529,0.218627450980392,0.219607843137255,
0.220588235294118,0.22156862745098,0.222549019607843,0.223529411764706,
0.224509803921569,0.225490196078431,0.226470588235294,0.227450980392157,
0.22843137254902,0.229411764705882,0.230392156862745,0.231372549019608,
0.232352941176471,0.233333333333333,0.234313725490196,0.235294117647059,
0.236274509803922,0.237254901960784,0.238235294117647,0.23921568627451,
0.240196078431373,0.241176470588235,0.242156862745098,0.243137254901961,
0.244117647058824,0.245098039215686,0.246078431372549,0.247058823529412,
0.248039215686275,0.249019607843137,0.25,0.250980392156863,0.251960784313725,
0.252941176470588,0.253921568627451,0.254901960784314,0.255882352941176,
0.256862745098039,0.257843137254902,0.258823529411765,0.259803921568627,
0.26078431372549,0.261764705882353,0.262745098039216,0.263725490196078,
0.264705882352941,0.265153469650551),.UNSPECIFIED.)
CURVE()
GEOMETRIC_REPRESENTATION_ITEM()
RATIONAL_B_SPLINE_CURVE((1.,0.995734176295034,1.,0.995734176295034,1.,0.995734176295034,
1.,0.995734176295034,1.,0.995734176295034,1.,0.995734176295034,1.,0.995734176295034,
1.,0.995734176295034,1.,0.995734176295034,1.,0.995734176295034,1.,0.995734176295034,
1.,0.995734176295034,1.,0.995734176295034,1.,0.995734176295034,1.,0.995734176295034,
1.,0.995734176295034,1.,0.995734176295034,1.,0.995734176295034,1.,0.995734176295034,
1.,0.995734176295034,1.,0.995734176295034,1.,0.995734176295034,1.,0.995734176295034,
1.,0.995734176295034,1.,0.995734176295034,1.,0.995734176295034,1.,0.995734176295034,
1.,0.995734176295034,1.,0.995734176295034,1.,0.995734176295034,1.,0.995734176295034,
1.,0.995734176295034,1.,0.995734176295034,1.,0.995734176295034,1.,0.995734176295034,
1.,0.995734176295034,1.,0.995734176295034,1.,0.995734176295034,1.,0.995734176295034,
1.,0.995734176295034,1.,0.995734176295034,1.,0.995734176295034,1.,0.995734176295034,
1.,0.995734176295034,1.,0.995734176295034,1.,0.995734176295034,1.,0.995734176295034,
1.,0.995734176295034,1.,0.995734176295034,1.,0.995734176295034,1.,0.995734176295034,
1.,0.995734176295034,1.,0.995734176295034,1.,0.995734176295034,1.,0.995734176295034,
1.,0.995734176295034,1.,0.995734176295034,1.,0.995734176295034,1.,0.995734176295034,
1.,0.995734176295034,1.,0.995734176295034,1.,0.995734176295034,1.,0.995734176295034,
1.,0.995734176295034,1.,0.995734176295034,1.,0.995734176295034,1.,0.995734176295034,
1.,0.995734176295034,1.,0.995734176295034,1.,0.995734176295034,1.,0.995734176295034,
1.,0.995734176295034,1.,0.995734176295034,1.,0.995734176295034,1.,0.995734176295034,
1.,0.995734176295034,1.,0.995734176295034,1.,0.995734176295034,1.,0.995734176295034,
1.,0.995734176295034,1.,0.995734176295034,1.,0.995734176295034,1.,0.995734176295034,
1.,0.995734176295034,1.,0.995734176295034,1.,0.995734176295034,1.,0.995734176295034,
1.,0.995734176295034,1.,0.995734176295034,1.,0.995734176295034,1.,0.995734176295034,
1.,0.995734176295034,1.,0.995734176295034,1.,0.995734176295034,1.,0.995734176295034,
1.,0.995734176295034,1.,0.995734176295034,1.,0.995734176295034,1.,0.995734176295034,
1.,0.995734176295034,1.,0.995734176295034,1.,0.995734176295034,1.,0.995734176295034,
1.,0.995734176295034,1.,0.995734176295034,1.,0.995734176295034,1.,0.995734176295034,
1.,0.995734176295034,1.,0.995734176295034,1.,0.995734176295034,1.,0.995734176295034,
1.,0.995734176295034,1.,0.995734176295034,1.,0.995734176295034,1.,0.995734176295034,
1.,0.995734176295034,1.,0.995734176295034,1.,0.995734176295034,1.,0.995734176295034,
1.,0.995734176295034,1.,0.995734176295034,1.,0.995734176295034,1.,0.995734176295034,
1.,0.995734176295034,1.,0.995734176295034,1.,0.995734176295034,1.,0.995734176295034,
1.,0.995734176295034,1.,0.995734176295034,1.,0.995734176295034,1.,0.995734176295034,
1.,0.995734176295034,1.,0.995734176295034,1.,0.995734176295034,1.,0.995734176295034,
1.,0.995734176295034,1.,0.995734176295034,1.,0.995734176295034,1.,0.995734176295034,
1.,0.995734176295034,1.,0.995734176295034,1.,0.995734176295034,1.,0.995734176295034,
1.,0.995734176295034,1.,0.995734176295034,1.,0.995734176295034,1.,0.995734176295034,
1.,0.995734176295034,1.,0.995734176295034,1.,0.995734176295034,1.,0.995734176295034,
1.,0.995734176295034,1.,0.995734176295034,1.,0.995734176295034,1.,0.995734176295034,
1.,0.995734176295034,1.,0.995734176295034,1.,0.995734176295034,1.,0.995734176295034,
1.,0.995734176295034,1.,0.995734176295034,1.,0.995734176295034,1.,0.995734176295034,
1.,0.995734176295034,1.,0.995734176295034,1.,0.995734176295034,1.,0.995734176295034,
1.,0.995734176295034,1.,0.995734176295034,1.,0.995734176295034,1.,0.995734176295034,
1.,0.995734176295034,1.,0.995734176295034,1.,0.995734176295034,1.,0.995734176295034,
1.,0.995734176295034,1.,0.995734176295034,1.,0.995734176295034,1.,0.995734176295034,
1.,0.995734176295034,1.,0.995734176295034,1.,0.995734176295034,1.,0.995734176295034,
1.,0.995734176295034,1.,0.995734176295034,1.,0.995734176295034,1.,0.995734176295034,
1.,0.995734176295034,1.,0.995734176295034,1.,0.995734176295034,1.,0.995734176295034,
1.,0.995734176295034,1.,0.995734176295034,1.,0.995734176295034,1.,0.995734176295034,
1.,0.995734176295034,1.,0.995734176295034,1.,0.995734176295034,1.,0.995734176295034,
1.,0.995734176295034,1.,0.995734176295034,1.,0.995734176295034,1.,0.995734176295034,
1.,0.995734176295034,1.,0.995734176295034,1.,0.995734176295034,1.,0.995734176295034,
1.,0.995734176295034,1.,0.995734176295034,1.,0.995734176295034,1.,0.995734176295034,
1.,0.995734176295034,1.,0.995734176295034,1.,0.995734176295034,1.,0.995734176295034,
1.,0.995734176295034,1.,0.995734176295034,1.,0.995734176295034,1.,0.995734176295034,
1.,0.995734176295034,1.,0.995734176295034,1.,0.995734176295034,1.,0.995734176295034,
1.,0.995734176295034,1.,0.995734176295034,1.,0.995734176295034,1.,0.995734176295034,
1.,0.995734176295034,1.,0.995734176295034,1.,0.995734176295034,1.,0.995734176295034,
1.,0.995734176295034,1.,0.995734176295034,1.,0.995734176295034,1.,0.995734176295034,
1.,0.995734176295034,1.,0.995734176295034,1.,0.995734176295034,1.,0.995734176295034,
1.,0.995734176295034,1.,0.995734176295034,1.,0.995734176295034,1.,0.995734176295034,
1.,0.995734176295034,1.,0.995734176295034,1.,0.995734176295034,1.,0.995734176295034,
1.,0.995734176295034,1.,0.995734176295034,1.,0.995734176295034,1.,0.995734176295034,
1.,0.995734176295034,1.,0.995734176295034,1.,0.995734176295034,1.,0.995734176295034,
1.,0.995734176295034,1.,0.995734176295034,1.,0.995734176295034,1.,0.995734176295034,
1.,0.995734176295034,1.,0.995734176295034,1.,0.995734176295034,1.,0.995734176295034,
1.,0.995734176295034,1.,0.995734176295034,1.,0.995734176295034,1.,0.995734176295034,
1.,0.995734176295034,1.,0.995734176295034,1.,0.995734176295034,1.,0.998052484925732,
0.997883203190121))
REPRESENTATION_ITEM('')
);
#4085=(
BOUNDED_CURVE()
B_SPLINE_CURVE(2,(#167184,#167185,#167186),.UNSPECIFIED.,.F.,.F.)
B_SPLINE_CURVE_WITH_KNOTS((3,3),(-1.90587960023829,-1.38751706971772),
 .UNSPECIFIED.)
CURVE()
GEOMETRIC_REPRESENTATION_ITEM()
RATIONAL_B_SPLINE_CURVE((1.66210638417239,1.76950594708369,1.76950594708369))
REPRESENTATION_ITEM('')
);
#4086=(
BOUNDED_CURVE()
B_SPLINE_CURVE(2,(#167187,#167188,#167189),.UNSPECIFIED.,.F.,.F.)
B_SPLINE_CURVE_WITH_KNOTS((3,3),(-1.38751706971772,-0.869154539197601),
 .UNSPECIFIED.)
CURVE()
GEOMETRIC_REPRESENTATION_ITEM()
RATIONAL_B_SPLINE_CURVE((1.7695059470837,1.7695059470837,1.66210638417259))
REPRESENTATION_ITEM('')
);
#4087=(
BOUNDED_CURVE()
B_SPLINE_CURVE(2,(#167201,#167202,#167203),.UNSPECIFIED.,.F.,.F.)
B_SPLINE_CURVE_WITH_KNOTS((3,3),(-1.90587960023829,-1.38751706971772),
 .UNSPECIFIED.)
CURVE()
GEOMETRIC_REPRESENTATION_ITEM()
RATIONAL_B_SPLINE_CURVE((1.66210638417239,1.76950594708369,1.76950594708369))
REPRESENTATION_ITEM('')
);
#4088=(
BOUNDED_CURVE()
B_SPLINE_CURVE(2,(#167216,#167217,#167218),.UNSPECIFIED.,.F.,.F.)
B_SPLINE_CURVE_WITH_KNOTS((3,3),(-1.38751706971771,-0.869154539197602),
 .UNSPECIFIED.)
CURVE()
GEOMETRIC_REPRESENTATION_ITEM()
RATIONAL_B_SPLINE_CURVE((1.76950594708369,1.76950594708369,1.66210638417258))
REPRESENTATION_ITEM('')
);
#4089=(
BOUNDED_CURVE()
B_SPLINE_CURVE(2,(#167259,#167260,#167261),.UNSPECIFIED.,.F.,.F.)
B_SPLINE_CURVE_WITH_KNOTS((3,3),(-1.9058796002383,-1.38751706971772),
 .UNSPECIFIED.)
CURVE()
GEOMETRIC_REPRESENTATION_ITEM()
RATIONAL_B_SPLINE_CURVE((1.66210638417238,1.76950594708369,1.76950594708369))
REPRESENTATION_ITEM('')
);
#4090=(
BOUNDED_CURVE()
B_SPLINE_CURVE(2,(#167262,#167263,#167264),.UNSPECIFIED.,.F.,.F.)
B_SPLINE_CURVE_WITH_KNOTS((3,3),(-1.38751706971773,-0.869154539197622),
 .UNSPECIFIED.)
CURVE()
GEOMETRIC_REPRESENTATION_ITEM()
RATIONAL_B_SPLINE_CURVE((1.76950594708368,1.76950594708368,1.66210638417257))
REPRESENTATION_ITEM('')
);
#4091=(
BOUNDED_CURVE()
B_SPLINE_CURVE(2,(#167267,#167268,#167269),.UNSPECIFIED.,.F.,.F.)
B_SPLINE_CURVE_WITH_KNOTS((3,3),(-1.90587960023789,-1.38751706971772),
 .UNSPECIFIED.)
CURVE()
GEOMETRIC_REPRESENTATION_ITEM()
RATIONAL_B_SPLINE_CURVE((1.66210638417255,1.76950594708369,1.76950594708369))
REPRESENTATION_ITEM('')
);
#4092=(
BOUNDED_CURVE()
B_SPLINE_CURVE(2,(#167281,#167282,#167283),.UNSPECIFIED.,.F.,.F.)
B_SPLINE_CURVE_WITH_KNOTS((3,3),(-1.38751706971772,-0.869154539197605),
 .UNSPECIFIED.)
CURVE()
GEOMETRIC_REPRESENTATION_ITEM()
RATIONAL_B_SPLINE_CURVE((1.76950594708369,1.76950594708369,1.66210638417258))
REPRESENTATION_ITEM('')
);
#4093=(
BOUNDED_CURVE()
B_SPLINE_CURVE(2,(#167286,#167287,#167288),.UNSPECIFIED.,.F.,.F.)
B_SPLINE_CURVE_WITH_KNOTS((3,3),(-1.90587960023829,-1.38751706971771),
 .UNSPECIFIED.)
CURVE()
GEOMETRIC_REPRESENTATION_ITEM()
RATIONAL_B_SPLINE_CURVE((1.66210638417239,1.76950594708369,1.76950594708369))
REPRESENTATION_ITEM('')
);
#4094=(
BOUNDED_CURVE()
B_SPLINE_CURVE(2,(#167300,#167301,#167302),.UNSPECIFIED.,.F.,.F.)
B_SPLINE_CURVE_WITH_KNOTS((3,3),(-1.38751706971772,-0.869154539197604),
 .UNSPECIFIED.)
CURVE()
GEOMETRIC_REPRESENTATION_ITEM()
RATIONAL_B_SPLINE_CURVE((1.76950594708369,1.76950594708369,1.66210638417258))
REPRESENTATION_ITEM('')
);
#4095=(
BOUNDED_CURVE()
B_SPLINE_CURVE(2,(#167305,#167306,#167307),.UNSPECIFIED.,.F.,.F.)
B_SPLINE_CURVE_WITH_KNOTS((3,3),(-1.90587960023783,-1.38751706971773),
 .UNSPECIFIED.)
CURVE()
GEOMETRIC_REPRESENTATION_ITEM()
RATIONAL_B_SPLINE_CURVE((1.66210638417257,1.76950594708368,1.76950594708368))
REPRESENTATION_ITEM('')
);
#4096=(
BOUNDED_CURVE()
B_SPLINE_CURVE(2,(#167319,#167320,#167321),.UNSPECIFIED.,.F.,.F.)
B_SPLINE_CURVE_WITH_KNOTS((3,3),(-1.38751706971772,-0.869154539197607),
 .UNSPECIFIED.)
CURVE()
GEOMETRIC_REPRESENTATION_ITEM()
RATIONAL_B_SPLINE_CURVE((1.76950594708369,1.76950594708369,1.66210638417258))
REPRESENTATION_ITEM('')
);
#4097=(
BOUNDED_CURVE()
B_SPLINE_CURVE(2,(#167324,#167325,#167326),.UNSPECIFIED.,.F.,.F.)
B_SPLINE_CURVE_WITH_KNOTS((3,3),(-1.90587960023828,-1.38751706971773),
 .UNSPECIFIED.)
CURVE()
GEOMETRIC_REPRESENTATION_ITEM()
RATIONAL_B_SPLINE_CURVE((1.66210638417238,1.76950594708368,1.76950594708368))
REPRESENTATION_ITEM('')
);
#4098=(
BOUNDED_CURVE()
B_SPLINE_CURVE(2,(#167338,#167339,#167340),.UNSPECIFIED.,.F.,.F.)
B_SPLINE_CURVE_WITH_KNOTS((3,3),(-1.38751706971773,-0.869154539197555),
 .UNSPECIFIED.)
CURVE()
GEOMETRIC_REPRESENTATION_ITEM()
RATIONAL_B_SPLINE_CURVE((1.76950594708368,1.76950594708368,1.66210638417254))
REPRESENTATION_ITEM('')
);
#4099=(
BOUNDED_CURVE()
B_SPLINE_CURVE(2,(#167354,#167355,#167356),.UNSPECIFIED.,.F.,.F.)
B_SPLINE_CURVE_WITH_KNOTS((3,3),(-1.90587960023789,-1.38751706971771),
 .UNSPECIFIED.)
CURVE()
GEOMETRIC_REPRESENTATION_ITEM()
RATIONAL_B_SPLINE_CURVE((1.66210638417255,1.7695059470837,1.7695059470837))
REPRESENTATION_ITEM('')
);
#4100=(
BOUNDED_CURVE()
B_SPLINE_CURVE(2,(#167368,#167369,#167370),.UNSPECIFIED.,.F.,.F.)
B_SPLINE_CURVE_WITH_KNOTS((3,3),(-1.38751706971771,-0.869154539197607),
 .UNSPECIFIED.)
CURVE()
GEOMETRIC_REPRESENTATION_ITEM()
RATIONAL_B_SPLINE_CURVE((1.7695059470837,1.7695059470837,1.66210638417258))
REPRESENTATION_ITEM('')
);
#4101=(
BOUNDED_CURVE()
B_SPLINE_CURVE(2,(#167373,#167374,#167375),.UNSPECIFIED.,.F.,.F.)
B_SPLINE_CURVE_WITH_KNOTS((3,3),(-1.90587960023829,-1.38751706971771),
 .UNSPECIFIED.)
CURVE()
GEOMETRIC_REPRESENTATION_ITEM()
RATIONAL_B_SPLINE_CURVE((1.66210638417239,1.76950594708369,1.76950594708369))
REPRESENTATION_ITEM('')
);
#4102=(
BOUNDED_CURVE()
B_SPLINE_CURVE(2,(#167387,#167388,#167389),.UNSPECIFIED.,.F.,.F.)
B_SPLINE_CURVE_WITH_KNOTS((3,3),(-1.38751706971771,-0.869154539197605),
 .UNSPECIFIED.)
CURVE()
GEOMETRIC_REPRESENTATION_ITEM()
RATIONAL_B_SPLINE_CURVE((1.7695059470837,1.76950594708369,1.66210638417258))
REPRESENTATION_ITEM('')
);
#4103=(
BOUNDED_CURVE()
B_SPLINE_CURVE(2,(#167392,#167393,#167394),.UNSPECIFIED.,.F.,.F.)
B_SPLINE_CURVE_WITH_KNOTS((3,3),(-1.90587960023829,-1.38751706971772),
 .UNSPECIFIED.)
CURVE()
GEOMETRIC_REPRESENTATION_ITEM()
RATIONAL_B_SPLINE_CURVE((1.66210638417239,1.7695059470837,1.7695059470837))
REPRESENTATION_ITEM('')
);
#4104=(
BOUNDED_CURVE()
B_SPLINE_CURVE(2,(#167406,#167407,#167408),.UNSPECIFIED.,.F.,.F.)
B_SPLINE_CURVE_WITH_KNOTS((3,3),(-1.38751706971771,-0.869154539197604),
 .UNSPECIFIED.)
CURVE()
GEOMETRIC_REPRESENTATION_ITEM()
RATIONAL_B_SPLINE_CURVE((1.76950594708369,1.76950594708369,1.66210638417258))
REPRESENTATION_ITEM('')
);
#4105=(
BOUNDED_CURVE()
B_SPLINE_CURVE(2,(#167411,#167412,#167413),.UNSPECIFIED.,.F.,.F.)
B_SPLINE_CURVE_WITH_KNOTS((3,3),(-1.90587960023783,-1.38751706971772),
 .UNSPECIFIED.)
CURVE()
GEOMETRIC_REPRESENTATION_ITEM()
RATIONAL_B_SPLINE_CURVE((1.66210638417258,1.7695059470837,1.7695059470837))
REPRESENTATION_ITEM('')
);
#4106=(
BOUNDED_CURVE()
B_SPLINE_CURVE(2,(#167425,#167426,#167427),.UNSPECIFIED.,.F.,.F.)
B_SPLINE_CURVE_WITH_KNOTS((3,3),(-1.38751706971772,-0.869154539197609),
 .UNSPECIFIED.)
CURVE()
GEOMETRIC_REPRESENTATION_ITEM()
RATIONAL_B_SPLINE_CURVE((1.7695059470837,1.7695059470837,1.66210638417258))
REPRESENTATION_ITEM('')
);
#4107=(
BOUNDED_CURVE()
B_SPLINE_CURVE(2,(#167430,#167431,#167432),.UNSPECIFIED.,.F.,.F.)
B_SPLINE_CURVE_WITH_KNOTS((3,3),(-1.90587960023829,-1.38751706971772),
 .UNSPECIFIED.)
CURVE()
GEOMETRIC_REPRESENTATION_ITEM()
RATIONAL_B_SPLINE_CURVE((1.66210638417239,1.7695059470837,1.7695059470837))
REPRESENTATION_ITEM('')
);
#4108=(
BOUNDED_CURVE()
B_SPLINE_CURVE(2,(#167444,#167445,#167446),.UNSPECIFIED.,.F.,.F.)
B_SPLINE_CURVE_WITH_KNOTS((3,3),(-1.38751706971772,-0.869154539197543),
 .UNSPECIFIED.)
CURVE()
GEOMETRIC_REPRESENTATION_ITEM()
RATIONAL_B_SPLINE_CURVE((1.7695059470837,1.7695059470837,1.66210638417255))
REPRESENTATION_ITEM('')
);
#4109=(
BOUNDED_CURVE()
B_SPLINE_CURVE(2,(#261646,#261647,#261648,#261649,#261650,#261651,#261652,
#261653,#261654,#261655,#261656,#261657,#261658,#261659,#261660),
 .UNSPECIFIED.,.F.,.F.)
B_SPLINE_CURVE_WITH_KNOTS((3,2,2,2,2,2,2,3),(0.75,0.7625,0.775,0.7875,0.8,
0.8125,0.825,0.832478990784214),.UNSPECIFIED.)
CURVE()
GEOMETRIC_REPRESENTATION_ITEM()
RATIONAL_B_SPLINE_CURVE((1.,0.923879532511287,1.,0.923879532511287,1.,0.923879532511287,
1.,0.923879532511287,1.,0.923879532511287,1.,0.923879532511287,1.,0.954455658012946,
0.963411430264977))
REPRESENTATION_ITEM('')
);
#4110=(
BOUNDED_CURVE()
B_SPLINE_CURVE(2,(#261663,#261664,#261665,#261666,#261667,#261668,#261669,
#261670,#261671,#261672,#261673,#261674,#261675,#261676,#261677),
 .UNSPECIFIED.,.F.,.F.)
B_SPLINE_CURVE_WITH_KNOTS((3,2,2,2,2,2,2,3),(0.75,0.7625,0.775,0.7875,0.8,
0.8125,0.825,0.832004152079254),.UNSPECIFIED.)
CURVE()
GEOMETRIC_REPRESENTATION_ITEM()
RATIONAL_B_SPLINE_CURVE((1.,0.923879532511287,1.,0.923879532511287,1.,0.923879532511287,
1.,0.923879532511287,1.,0.923879532511287,1.,0.923879532511287,1.,0.957347253549212,
0.962493918736692))
REPRESENTATION_ITEM('')
);
#4111=(
BOUNDED_CURVE()
B_SPLINE_CURVE(2,(#261682,#261683,#261684,#261685,#261686,#261687,#261688,
#261689,#261690,#261691,#261692,#261693,#261694,#261695,#261696,#261697,
#261698),.UNSPECIFIED.,.F.,.F.)
B_SPLINE_CURVE_WITH_KNOTS((3,2,2,2,2,2,2,2,3),(0.65,0.6625,0.675,0.6875,
0.7,0.7125,0.725,0.7375,0.75),.UNSPECIFIED.)
CURVE()
GEOMETRIC_REPRESENTATION_ITEM()
RATIONAL_B_SPLINE_CURVE((1.,0.923879532511287,1.,0.923879532511287,1.,0.923879532511287,
1.,0.923879532511287,1.,0.923879532511287,1.,0.923879532511287,1.,0.923879532511287,
1.,0.923879532511287,1.))
REPRESENTATION_ITEM('')
);
#4112=(
BOUNDED_CURVE()
B_SPLINE_CURVE(2,(#261699,#261700,#261701,#261702,#261703,#261704,#261705,
#261706,#261707,#261708,#261709,#261710,#261711,#261712,#261713,#261714,
#261715),.UNSPECIFIED.,.F.,.F.)
B_SPLINE_CURVE_WITH_KNOTS((3,2,2,2,2,2,2,2,3),(0.65,0.6625,0.675,0.6875,
0.7,0.7125,0.725,0.7375,0.75),.UNSPECIFIED.)
CURVE()
GEOMETRIC_REPRESENTATION_ITEM()
RATIONAL_B_SPLINE_CURVE((1.,0.923879532511287,1.,0.923879532511287,1.,0.923879532511287,
1.,0.923879532511287,1.,0.923879532511287,1.,0.923879532511287,1.,0.923879532511287,
1.,0.923879532511287,1.))
REPRESENTATION_ITEM('')
);
#4113=(
BOUNDED_CURVE()
B_SPLINE_CURVE(2,(#261720,#261721,#261722,#261723,#261724,#261725,#261726,
#261727,#261728,#261729,#261730,#261731,#261732,#261733,#261734,#261735,
#261736),.UNSPECIFIED.,.F.,.F.)
B_SPLINE_CURVE_WITH_KNOTS((3,2,2,2,2,2,2,2,3),(0.55,0.5625,0.575,0.5875,
0.6,0.6125,0.625,0.6375,0.65),.UNSPECIFIED.)
CURVE()
GEOMETRIC_REPRESENTATION_ITEM()
RATIONAL_B_SPLINE_CURVE((1.,0.923879532511287,1.,0.923879532511287,1.,0.923879532511287,
1.,0.923879532511287,1.,0.923879532511287,1.,0.923879532511287,1.,0.923879532511287,
1.,0.923879532511287,1.))
REPRESENTATION_ITEM('')
);
#4114=(
BOUNDED_CURVE()
B_SPLINE_CURVE(2,(#261737,#261738,#261739,#261740,#261741,#261742,#261743,
#261744,#261745,#261746,#261747,#261748,#261749,#261750,#261751,#261752,
#261753),.UNSPECIFIED.,.F.,.F.)
B_SPLINE_CURVE_WITH_KNOTS((3,2,2,2,2,2,2,2,3),(0.55,0.5625,0.575,0.5875,
0.6,0.6125,0.625,0.6375,0.65),.UNSPECIFIED.)
CURVE()
GEOMETRIC_REPRESENTATION_ITEM()
RATIONAL_B_SPLINE_CURVE((1.,0.923879532511287,1.,0.923879532511287,1.,0.923879532511287,
1.,0.923879532511287,1.,0.923879532511287,1.,0.923879532511287,1.,0.923879532511287,
1.,0.923879532511287,1.))
REPRESENTATION_ITEM('')
);
#4115=(
BOUNDED_CURVE()
B_SPLINE_CURVE(2,(#261758,#261759,#261760,#261761,#261762,#261763,#261764,
#261765,#261766,#261767,#261768,#261769,#261770,#261771,#261772,#261773,
#261774),.UNSPECIFIED.,.F.,.F.)
B_SPLINE_CURVE_WITH_KNOTS((3,2,2,2,2,2,2,2,3),(0.45,0.4625,0.475,0.4875,
0.5,0.5125,0.525,0.5375,0.55),.UNSPECIFIED.)
CURVE()
GEOMETRIC_REPRESENTATION_ITEM()
RATIONAL_B_SPLINE_CURVE((1.,0.923879532511287,1.,0.923879532511287,1.,0.923879532511287,
1.,0.923879532511287,1.,0.923879532511287,1.,0.923879532511287,1.,0.923879532511287,
1.,0.923879532511287,1.))
REPRESENTATION_ITEM('')
);
#4116=(
BOUNDED_CURVE()
B_SPLINE_CURVE(2,(#261775,#261776,#261777,#261778,#261779,#261780,#261781,
#261782,#261783,#261784,#261785,#261786,#261787,#261788,#261789,#261790,
#261791),.UNSPECIFIED.,.F.,.F.)
B_SPLINE_CURVE_WITH_KNOTS((3,2,2,2,2,2,2,2,3),(0.45,0.4625,0.475,0.4875,
0.5,0.5125,0.525,0.5375,0.55),.UNSPECIFIED.)
CURVE()
GEOMETRIC_REPRESENTATION_ITEM()
RATIONAL_B_SPLINE_CURVE((1.,0.923879532511287,1.,0.923879532511287,1.,0.923879532511287,
1.,0.923879532511287,1.,0.923879532511287,1.,0.923879532511287,1.,0.923879532511287,
1.,0.923879532511287,1.))
REPRESENTATION_ITEM('')
);
#4117=(
BOUNDED_CURVE()
B_SPLINE_CURVE(2,(#261796,#261797,#261798,#261799,#261800,#261801,#261802,
#261803,#261804,#261805,#261806,#261807,#261808,#261809,#261810,#261811,
#261812),.UNSPECIFIED.,.F.,.F.)
B_SPLINE_CURVE_WITH_KNOTS((3,2,2,2,2,2,2,2,3),(0.35,0.3625,0.375,0.3875,
0.4,0.4125,0.425,0.4375,0.45),.UNSPECIFIED.)
CURVE()
GEOMETRIC_REPRESENTATION_ITEM()
RATIONAL_B_SPLINE_CURVE((1.,0.923879532511287,1.,0.923879532511287,1.,0.923879532511287,
1.,0.923879532511287,1.,0.923879532511287,1.,0.923879532511287,1.,0.923879532511287,
1.,0.923879532511287,1.))
REPRESENTATION_ITEM('')
);
#4118=(
BOUNDED_CURVE()
B_SPLINE_CURVE(2,(#261813,#261814,#261815,#261816,#261817,#261818,#261819,
#261820,#261821,#261822,#261823,#261824,#261825,#261826,#261827,#261828,
#261829),.UNSPECIFIED.,.F.,.F.)
B_SPLINE_CURVE_WITH_KNOTS((3,2,2,2,2,2,2,2,3),(0.35,0.3625,0.375,0.3875,
0.4,0.4125,0.425,0.4375,0.45),.UNSPECIFIED.)
CURVE()
GEOMETRIC_REPRESENTATION_ITEM()
RATIONAL_B_SPLINE_CURVE((1.,0.923879532511287,1.,0.923879532511287,1.,0.923879532511287,
1.,0.923879532511287,1.,0.923879532511287,1.,0.923879532511287,1.,0.923879532511287,
1.,0.923879532511287,1.))
REPRESENTATION_ITEM('')
);
#4119=(
BOUNDED_CURVE()
B_SPLINE_CURVE(2,(#261834,#261835,#261836,#261837,#261838,#261839,#261840,
#261841,#261842,#261843,#261844,#261845,#261846,#261847,#261848,#261849,
#261850),.UNSPECIFIED.,.F.,.F.)
B_SPLINE_CURVE_WITH_KNOTS((3,2,2,2,2,2,2,2,3),(0.25,0.2625,0.275,0.2875,
0.3,0.3125,0.325,0.3375,0.35),.UNSPECIFIED.)
CURVE()
GEOMETRIC_REPRESENTATION_ITEM()
RATIONAL_B_SPLINE_CURVE((1.,0.923879532511287,1.,0.923879532511287,1.,0.923879532511287,
1.,0.923879532511287,1.,0.923879532511287,1.,0.923879532511287,1.,0.923879532511287,
1.,0.923879532511287,1.))
REPRESENTATION_ITEM('')
);
#4120=(
BOUNDED_CURVE()
B_SPLINE_CURVE(2,(#261851,#261852,#261853,#261854,#261855,#261856,#261857,
#261858,#261859,#261860,#261861,#261862,#261863,#261864,#261865,#261866,
#261867),.UNSPECIFIED.,.F.,.F.)
B_SPLINE_CURVE_WITH_KNOTS((3,2,2,2,2,2,2,2,3),(0.25,0.2625,0.275,0.2875,
0.3,0.3125,0.325,0.3375,0.35),.UNSPECIFIED.)
CURVE()
GEOMETRIC_REPRESENTATION_ITEM()
RATIONAL_B_SPLINE_CURVE((1.,0.923879532511287,1.,0.923879532511287,1.,0.923879532511287,
1.,0.923879532511287,1.,0.923879532511287,1.,0.923879532511287,1.,0.923879532511287,
1.,0.923879532511287,1.))
REPRESENTATION_ITEM('')
);
#4121=(
BOUNDED_CURVE()
B_SPLINE_CURVE(2,(#262441,#262442,#262443),.UNSPECIFIED.,.F.,.F.)
B_SPLINE_CURVE_WITH_KNOTS((3,3),(-0.50202782853392,-0.138654436681084),
 .UNSPECIFIED.)
CURVE()
GEOMETRIC_REPRESENTATION_ITEM()
RATIONAL_B_SPLINE_CURVE((1.19489831606823,1.37974972887269,1.19489831606823))
REPRESENTATION_ITEM('')
);
#4122=(
BOUNDED_CURVE()
B_SPLINE_CURVE(2,(#262445,#262446,#262447),.UNSPECIFIED.,.F.,.F.)
B_SPLINE_CURVE_WITH_KNOTS((3,3),(-0.502027828533919,-0.138654436681081),
 .UNSPECIFIED.)
CURVE()
GEOMETRIC_REPRESENTATION_ITEM()
RATIONAL_B_SPLINE_CURVE((1.19489831606823,1.3797497288727,1.19489831606823))
REPRESENTATION_ITEM('')
);
#4123=(
BOUNDED_CURVE()
B_SPLINE_CURVE(2,(#262449,#262450,#262451),.UNSPECIFIED.,.F.,.F.)
B_SPLINE_CURVE_WITH_KNOTS((3,3),(-0.502027828533919,-0.138654436681082),
 .UNSPECIFIED.)
CURVE()
GEOMETRIC_REPRESENTATION_ITEM()
RATIONAL_B_SPLINE_CURVE((1.19489831606824,1.37974972887271,1.19489831606824))
REPRESENTATION_ITEM('')
);
#4124=(
BOUNDED_CURVE()
B_SPLINE_CURVE(2,(#262453,#262454,#262455),.UNSPECIFIED.,.F.,.F.)
B_SPLINE_CURVE_WITH_KNOTS((3,3),(-0.502027828533919,-0.138654436681086),
 .UNSPECIFIED.)
CURVE()
GEOMETRIC_REPRESENTATION_ITEM()
RATIONAL_B_SPLINE_CURVE((1.19489831606823,1.37974972887268,1.19489831606823))
REPRESENTATION_ITEM('')
);
#4125=(
BOUNDED_CURVE()
B_SPLINE_CURVE(2,(#262457,#262458,#262459),.UNSPECIFIED.,.F.,.F.)
B_SPLINE_CURVE_WITH_KNOTS((3,3),(-0.502027828533918,-0.138654436681083),
 .UNSPECIFIED.)
CURVE()
GEOMETRIC_REPRESENTATION_ITEM()
RATIONAL_B_SPLINE_CURVE((1.19489831606823,1.3797497288727,1.19489831606823))
REPRESENTATION_ITEM('')
);
#4126=(
BOUNDED_CURVE()
B_SPLINE_CURVE(2,(#262461,#262462,#262463),.UNSPECIFIED.,.F.,.F.)
B_SPLINE_CURVE_WITH_KNOTS((3,3),(-0.502027828533914,-0.138654436681084),
 .UNSPECIFIED.)
CURVE()
GEOMETRIC_REPRESENTATION_ITEM()
RATIONAL_B_SPLINE_CURVE((1.19489831606823,1.37974972887268,1.19489831606822))
REPRESENTATION_ITEM('')
);
#4127=(
BOUNDED_CURVE()
B_SPLINE_CURVE(2,(#262811,#262812,#262813,#262814,#262815,#262816,#262817,
#262818,#262819,#262820,#262821,#262822,#262823,#262824,#262825,#262826,
#262827),.UNSPECIFIED.,.F.,.F.)
B_SPLINE_CURVE_WITH_KNOTS((3,2,2,2,2,2,2,2,3),(0.152008120250914,0.1625,
0.175,0.1875,0.2,0.2125,0.225,0.2375,0.25),.UNSPECIFIED.)
CURVE()
GEOMETRIC_REPRESENTATION_ITEM()
RATIONAL_B_SPLINE_CURVE((0.979471631423889,0.936108256693134,1.,0.923879532511287,
1.,0.923879532511287,1.,0.923879532511287,1.,0.923879532511287,1.,0.923879532511287,
1.,0.923879532511287,1.,0.923879532511287,1.))
REPRESENTATION_ITEM('')
);
#4128=(
BOUNDED_CURVE()
B_SPLINE_CURVE(2,(#262829,#262830,#262831,#262832,#262833,#262834,#262835,
#262836,#262837,#262838,#262839,#262840,#262841,#262842,#262843,#262844,
#262845),.UNSPECIFIED.,.F.,.F.)
B_SPLINE_CURVE_WITH_KNOTS((3,2,2,2,2,2,2,2,3),(0.152504986222125,0.1625,
0.175,0.1875,0.2,0.2125,0.225,0.2375,0.25),.UNSPECIFIED.)
CURVE()
GEOMETRIC_REPRESENTATION_ITEM()
RATIONAL_B_SPLINE_CURVE((0.975605037486425,0.939133990293761,1.,0.923879532511287,
1.,0.923879532511287,1.,0.923879532511287,1.,0.923879532511287,1.,0.923879532511287,
1.,0.923879532511287,1.,0.923879532511287,1.))
REPRESENTATION_ITEM('')
);
#4129=(
BOUNDED_CURVE()
B_SPLINE_CURVE(2,(#263173,#263174,#263175,#263176,#263177,#263178,#263179,
#263180,#263181,#263182,#263183,#263184,#263185,#263186,#263187),
 .UNSPECIFIED.,.F.,.F.)
B_SPLINE_CURVE_WITH_KNOTS((3,2,2,2,2,2,2,3),(0.75,0.7625,0.775,0.7875,0.8,
0.8125,0.825,0.832478990784214),.UNSPECIFIED.)
CURVE()
GEOMETRIC_REPRESENTATION_ITEM()
RATIONAL_B_SPLINE_CURVE((1.,0.923879532511287,1.,0.923879532511287,1.,0.923879532511287,
1.,0.923879532511287,1.,0.923879532511287,1.,0.923879532511287,1.,0.954455658012946,
0.963411430264977))
REPRESENTATION_ITEM('')
);
#4130=(
BOUNDED_CURVE()
B_SPLINE_CURVE(2,(#263190,#263191,#263192,#263193,#263194,#263195,#263196,
#263197,#263198,#263199,#263200,#263201,#263202,#263203,#263204),
 .UNSPECIFIED.,.F.,.F.)
B_SPLINE_CURVE_WITH_KNOTS((3,2,2,2,2,2,2,3),(0.75,0.7625,0.775,0.7875,0.8,
0.8125,0.825,0.832004152079254),.UNSPECIFIED.)
CURVE()
GEOMETRIC_REPRESENTATION_ITEM()
RATIONAL_B_SPLINE_CURVE((1.,0.923879532511287,1.,0.923879532511287,1.,0.923879532511287,
1.,0.923879532511287,1.,0.923879532511287,1.,0.923879532511287,1.,0.957347253549212,
0.962493918736692))
REPRESENTATION_ITEM('')
);
#4131=(
BOUNDED_CURVE()
B_SPLINE_CURVE(2,(#263209,#263210,#263211,#263212,#263213,#263214,#263215,
#263216,#263217,#263218,#263219,#263220,#263221,#263222,#263223,#263224,
#263225),.UNSPECIFIED.,.F.,.F.)
B_SPLINE_CURVE_WITH_KNOTS((3,2,2,2,2,2,2,2,3),(0.65,0.6625,0.675,0.6875,
0.7,0.7125,0.725,0.7375,0.75),.UNSPECIFIED.)
CURVE()
GEOMETRIC_REPRESENTATION_ITEM()
RATIONAL_B_SPLINE_CURVE((1.,0.923879532511287,1.,0.923879532511287,1.,0.923879532511287,
1.,0.923879532511287,1.,0.923879532511287,1.,0.923879532511287,1.,0.923879532511287,
1.,0.923879532511287,1.))
REPRESENTATION_ITEM('')
);
#4132=(
BOUNDED_CURVE()
B_SPLINE_CURVE(2,(#263226,#263227,#263228,#263229,#263230,#263231,#263232,
#263233,#263234,#263235,#263236,#263237,#263238,#263239,#263240,#263241,
#263242),.UNSPECIFIED.,.F.,.F.)
B_SPLINE_CURVE_WITH_KNOTS((3,2,2,2,2,2,2,2,3),(0.65,0.6625,0.675,0.6875,
0.7,0.7125,0.725,0.7375,0.75),.UNSPECIFIED.)
CURVE()
GEOMETRIC_REPRESENTATION_ITEM()
RATIONAL_B_SPLINE_CURVE((1.,0.923879532511287,1.,0.923879532511287,1.,0.923879532511287,
1.,0.923879532511287,1.,0.923879532511287,1.,0.923879532511287,1.,0.923879532511287,
1.,0.923879532511287,1.))
REPRESENTATION_ITEM('')
);
#4133=(
BOUNDED_CURVE()
B_SPLINE_CURVE(2,(#263247,#263248,#263249,#263250,#263251,#263252,#263253,
#263254,#263255,#263256,#263257,#263258,#263259,#263260,#263261,#263262,
#263263),.UNSPECIFIED.,.F.,.F.)
B_SPLINE_CURVE_WITH_KNOTS((3,2,2,2,2,2,2,2,3),(0.55,0.5625,0.575,0.5875,
0.6,0.6125,0.625,0.6375,0.65),.UNSPECIFIED.)
CURVE()
GEOMETRIC_REPRESENTATION_ITEM()
RATIONAL_B_SPLINE_CURVE((1.,0.923879532511287,1.,0.923879532511287,1.,0.923879532511287,
1.,0.923879532511287,1.,0.923879532511287,1.,0.923879532511287,1.,0.923879532511287,
1.,0.923879532511287,1.))
REPRESENTATION_ITEM('')
);
#4134=(
BOUNDED_CURVE()
B_SPLINE_CURVE(2,(#263264,#263265,#263266,#263267,#263268,#263269,#263270,
#263271,#263272,#263273,#263274,#263275,#263276,#263277,#263278,#263279,
#263280),.UNSPECIFIED.,.F.,.F.)
B_SPLINE_CURVE_WITH_KNOTS((3,2,2,2,2,2,2,2,3),(0.55,0.5625,0.575,0.5875,
0.6,0.6125,0.625,0.6375,0.65),.UNSPECIFIED.)
CURVE()
GEOMETRIC_REPRESENTATION_ITEM()
RATIONAL_B_SPLINE_CURVE((1.,0.923879532511287,1.,0.923879532511287,1.,0.923879532511287,
1.,0.923879532511287,1.,0.923879532511287,1.,0.923879532511287,1.,0.923879532511287,
1.,0.923879532511287,1.))
REPRESENTATION_ITEM('')
);
#4135=(
BOUNDED_CURVE()
B_SPLINE_CURVE(2,(#263285,#263286,#263287,#263288,#263289,#263290,#263291,
#263292,#263293,#263294,#263295,#263296,#263297,#263298,#263299,#263300,
#263301),.UNSPECIFIED.,.F.,.F.)
B_SPLINE_CURVE_WITH_KNOTS((3,2,2,2,2,2,2,2,3),(0.45,0.4625,0.475,0.4875,
0.5,0.5125,0.525,0.5375,0.55),.UNSPECIFIED.)
CURVE()
GEOMETRIC_REPRESENTATION_ITEM()
RATIONAL_B_SPLINE_CURVE((1.,0.923879532511287,1.,0.923879532511287,1.,0.923879532511287,
1.,0.923879532511287,1.,0.923879532511287,1.,0.923879532511287,1.,0.923879532511287,
1.,0.923879532511287,1.))
REPRESENTATION_ITEM('')
);
#4136=(
BOUNDED_CURVE()
B_SPLINE_CURVE(2,(#263302,#263303,#263304,#263305,#263306,#263307,#263308,
#263309,#263310,#263311,#263312,#263313,#263314,#263315,#263316,#263317,
#263318),.UNSPECIFIED.,.F.,.F.)
B_SPLINE_CURVE_WITH_KNOTS((3,2,2,2,2,2,2,2,3),(0.45,0.4625,0.475,0.4875,
0.5,0.5125,0.525,0.5375,0.55),.UNSPECIFIED.)
CURVE()
GEOMETRIC_REPRESENTATION_ITEM()
RATIONAL_B_SPLINE_CURVE((1.,0.923879532511287,1.,0.923879532511287,1.,0.923879532511287,
1.,0.923879532511287,1.,0.923879532511287,1.,0.923879532511287,1.,0.923879532511287,
1.,0.923879532511287,1.))
REPRESENTATION_ITEM('')
);
#4137=(
BOUNDED_CURVE()
B_SPLINE_CURVE(2,(#263323,#263324,#263325,#263326,#263327,#263328,#263329,
#263330,#263331,#263332,#263333,#263334,#263335,#263336,#263337,#263338,
#263339),.UNSPECIFIED.,.F.,.F.)
B_SPLINE_CURVE_WITH_KNOTS((3,2,2,2,2,2,2,2,3),(0.35,0.3625,0.375,0.3875,
0.4,0.4125,0.425,0.4375,0.45),.UNSPECIFIED.)
CURVE()
GEOMETRIC_REPRESENTATION_ITEM()
RATIONAL_B_SPLINE_CURVE((1.,0.923879532511287,1.,0.923879532511287,1.,0.923879532511287,
1.,0.923879532511287,1.,0.923879532511287,1.,0.923879532511287,1.,0.923879532511287,
1.,0.923879532511287,1.))
REPRESENTATION_ITEM('')
);
#4138=(
BOUNDED_CURVE()
B_SPLINE_CURVE(2,(#263340,#263341,#263342,#263343,#263344,#263345,#263346,
#263347,#263348,#263349,#263350,#263351,#263352,#263353,#263354,#263355,
#263356),.UNSPECIFIED.,.F.,.F.)
B_SPLINE_CURVE_WITH_KNOTS((3,2,2,2,2,2,2,2,3),(0.35,0.3625,0.375,0.3875,
0.4,0.4125,0.425,0.4375,0.45),.UNSPECIFIED.)
CURVE()
GEOMETRIC_REPRESENTATION_ITEM()
RATIONAL_B_SPLINE_CURVE((1.,0.923879532511287,1.,0.923879532511287,1.,0.923879532511287,
1.,0.923879532511287,1.,0.923879532511287,1.,0.923879532511287,1.,0.923879532511287,
1.,0.923879532511287,1.))
REPRESENTATION_ITEM('')
);
#4139=(
BOUNDED_CURVE()
B_SPLINE_CURVE(2,(#263361,#263362,#263363,#263364,#263365,#263366,#263367,
#263368,#263369,#263370,#263371,#263372,#263373,#263374,#263375,#263376,
#263377),.UNSPECIFIED.,.F.,.F.)
B_SPLINE_CURVE_WITH_KNOTS((3,2,2,2,2,2,2,2,3),(0.25,0.2625,0.275,0.2875,
0.3,0.3125,0.325,0.3375,0.35),.UNSPECIFIED.)
CURVE()
GEOMETRIC_REPRESENTATION_ITEM()
RATIONAL_B_SPLINE_CURVE((1.,0.923879532511287,1.,0.923879532511287,1.,0.923879532511287,
1.,0.923879532511287,1.,0.923879532511287,1.,0.923879532511287,1.,0.923879532511287,
1.,0.923879532511287,1.))
REPRESENTATION_ITEM('')
);
#4140=(
BOUNDED_CURVE()
B_SPLINE_CURVE(2,(#263378,#263379,#263380,#263381,#263382,#263383,#263384,
#263385,#263386,#263387,#263388,#263389,#263390,#263391,#263392,#263393,
#263394),.UNSPECIFIED.,.F.,.F.)
B_SPLINE_CURVE_WITH_KNOTS((3,2,2,2,2,2,2,2,3),(0.25,0.2625,0.275,0.2875,
0.3,0.3125,0.325,0.3375,0.35),.UNSPECIFIED.)
CURVE()
GEOMETRIC_REPRESENTATION_ITEM()
RATIONAL_B_SPLINE_CURVE((1.,0.923879532511287,1.,0.923879532511287,1.,0.923879532511287,
1.,0.923879532511287,1.,0.923879532511287,1.,0.923879532511287,1.,0.923879532511287,
1.,0.923879532511287,1.))
REPRESENTATION_ITEM('')
);
#4141=(
BOUNDED_CURVE()
B_SPLINE_CURVE(2,(#263968,#263969,#263970),.UNSPECIFIED.,.F.,.F.)
B_SPLINE_CURVE_WITH_KNOTS((3,3),(-0.502027828533916,-0.138654436681082),
 .UNSPECIFIED.)
CURVE()
GEOMETRIC_REPRESENTATION_ITEM()
RATIONAL_B_SPLINE_CURVE((1.19489831606823,1.3797497288727,1.19489831606823))
REPRESENTATION_ITEM('')
);
#4142=(
BOUNDED_CURVE()
B_SPLINE_CURVE(2,(#263972,#263973,#263974),.UNSPECIFIED.,.F.,.F.)
B_SPLINE_CURVE_WITH_KNOTS((3,3),(-0.50202782853392,-0.138654436681083),
 .UNSPECIFIED.)
CURVE()
GEOMETRIC_REPRESENTATION_ITEM()
RATIONAL_B_SPLINE_CURVE((1.19489831606823,1.3797497288727,1.19489831606823))
REPRESENTATION_ITEM('')
);
#4143=(
BOUNDED_CURVE()
B_SPLINE_CURVE(2,(#263976,#263977,#263978),.UNSPECIFIED.,.F.,.F.)
B_SPLINE_CURVE_WITH_KNOTS((3,3),(-0.502027828533917,-0.138654436681082),
 .UNSPECIFIED.)
CURVE()
GEOMETRIC_REPRESENTATION_ITEM()
RATIONAL_B_SPLINE_CURVE((1.19489831606823,1.3797497288727,1.19489831606823))
REPRESENTATION_ITEM('')
);
#4144=(
BOUNDED_CURVE()
B_SPLINE_CURVE(2,(#263980,#263981,#263982),.UNSPECIFIED.,.F.,.F.)
B_SPLINE_CURVE_WITH_KNOTS((3,3),(-0.502027828533925,-0.138654436681083),
 .UNSPECIFIED.)
CURVE()
GEOMETRIC_REPRESENTATION_ITEM()
RATIONAL_B_SPLINE_CURVE((1.19489831606823,1.37974972887271,1.19489831606823))
REPRESENTATION_ITEM('')
);
#4145=(
BOUNDED_CURVE()
B_SPLINE_CURVE(2,(#263984,#263985,#263986),.UNSPECIFIED.,.F.,.F.)
B_SPLINE_CURVE_WITH_KNOTS((3,3),(-0.502027828533916,-0.138654436681082),
 .UNSPECIFIED.)
CURVE()
GEOMETRIC_REPRESENTATION_ITEM()
RATIONAL_B_SPLINE_CURVE((1.19489831606823,1.3797497288727,1.19489831606823))
REPRESENTATION_ITEM('')
);
#4146=(
BOUNDED_CURVE()
B_SPLINE_CURVE(2,(#263988,#263989,#263990),.UNSPECIFIED.,.F.,.F.)
B_SPLINE_CURVE_WITH_KNOTS((3,3),(-0.502027828533915,-0.138654436681083),
 .UNSPECIFIED.)
CURVE()
GEOMETRIC_REPRESENTATION_ITEM()
RATIONAL_B_SPLINE_CURVE((1.19489831606823,1.3797497288727,1.19489831606823))
REPRESENTATION_ITEM('')
);
#4147=(
BOUNDED_CURVE()
B_SPLINE_CURVE(2,(#264338,#264339,#264340,#264341,#264342,#264343,#264344,
#264345,#264346,#264347,#264348,#264349,#264350,#264351,#264352,#264353,
#264354),.UNSPECIFIED.,.F.,.F.)
B_SPLINE_CURVE_WITH_KNOTS((3,2,2,2,2,2,2,2,3),(0.152008120250914,0.1625,
0.175,0.1875,0.2,0.2125,0.225,0.2375,0.25),.UNSPECIFIED.)
CURVE()
GEOMETRIC_REPRESENTATION_ITEM()
RATIONAL_B_SPLINE_CURVE((0.979471631423889,0.936108256693134,1.,0.923879532511287,
1.,0.923879532511287,1.,0.923879532511287,1.,0.923879532511287,1.,0.923879532511287,
1.,0.923879532511287,1.,0.923879532511287,1.))
REPRESENTATION_ITEM('')
);
#4148=(
BOUNDED_CURVE()
B_SPLINE_CURVE(2,(#264356,#264357,#264358,#264359,#264360,#264361,#264362,
#264363,#264364,#264365,#264366,#264367,#264368,#264369,#264370,#264371,
#264372),.UNSPECIFIED.,.F.,.F.)
B_SPLINE_CURVE_WITH_KNOTS((3,2,2,2,2,2,2,2,3),(0.152504986222125,0.1625,
0.175,0.1875,0.2,0.2125,0.225,0.2375,0.25),.UNSPECIFIED.)
CURVE()
GEOMETRIC_REPRESENTATION_ITEM()
RATIONAL_B_SPLINE_CURVE((0.975605037486425,0.939133990293761,1.,0.923879532511287,
1.,0.923879532511287,1.,0.923879532511287,1.,0.923879532511287,1.,0.923879532511287,
1.,0.923879532511287,1.,0.923879532511287,1.))
REPRESENTATION_ITEM('')
);
#4149=(
BOUNDED_CURVE()
B_SPLINE_CURVE(2,(#265333,#265334,#265335,#265336,#265337),
 .UNSPECIFIED.,.F.,.F.)
B_SPLINE_CURVE_WITH_KNOTS((3,2,3),(0.,0.025,0.0310216655371715),
 .UNSPECIFIED.)
CURVE()
GEOMETRIC_REPRESENTATION_ITEM()
RATIONAL_B_SPLINE_CURVE((1.,0.996917333733128,1.,0.999257488591127,0.998872669611195))
REPRESENTATION_ITEM('')
);
#4150=(
BOUNDED_CURVE()
B_SPLINE_CURVE(2,(#265340,#265341,#265342,#265343,#265344,#265345,#265346),
 .UNSPECIFIED.,.F.,.F.)
B_SPLINE_CURVE_WITH_KNOTS((3,2,2,3),(0.,0.025,0.05,0.0627352828483757),
 .UNSPECIFIED.)
CURVE()
GEOMETRIC_REPRESENTATION_ITEM()
RATIONAL_B_SPLINE_CURVE((1.,0.996917333733128,1.,0.996917333733128,1.,0.99842965492657,
0.998459212947514))
REPRESENTATION_ITEM('')
);
#4151=(
BOUNDED_CURVE()
B_SPLINE_CURVE(2,(#265512,#265513,#265514,#265515,#265516),
 .UNSPECIFIED.,.F.,.F.)
B_SPLINE_CURVE_WITH_KNOTS((3,2,3),(0.,0.025,0.0310216655371717),
 .UNSPECIFIED.)
CURVE()
GEOMETRIC_REPRESENTATION_ITEM()
RATIONAL_B_SPLINE_CURVE((1.,0.996917333733128,1.,0.999257488591127,0.998872669611196))
REPRESENTATION_ITEM('')
);
#4152=(
BOUNDED_CURVE()
B_SPLINE_CURVE(2,(#265690,#265691,#265692,#265693,#265694,#265695,#265696),
 .UNSPECIFIED.,.F.,.F.)
B_SPLINE_CURVE_WITH_KNOTS((3,2,2,3),(0.,0.025,0.05,0.0627352828483766),
 .UNSPECIFIED.)
CURVE()
GEOMETRIC_REPRESENTATION_ITEM()
RATIONAL_B_SPLINE_CURVE((1.,0.996917333733128,1.,0.996917333733128,1.,0.998429654926569,
0.998459212947514))
REPRESENTATION_ITEM('')
);
#4153=(
BOUNDED_CURVE()
B_SPLINE_CURVE(2,(#266037,#266038,#266039,#266040,#266041,#266042,#266043),
 .UNSPECIFIED.,.F.,.F.)
B_SPLINE_CURVE_WITH_KNOTS((3,2,2,3),(0.,0.025,0.05,0.0627352828483767),
 .UNSPECIFIED.)
CURVE()
GEOMETRIC_REPRESENTATION_ITEM()
RATIONAL_B_SPLINE_CURVE((1.,0.996917333733128,1.,0.996917333733128,1.,0.998429654926569,
0.998459212947514))
REPRESENTATION_ITEM('')
);
#4154=(
BOUNDED_CURVE()
B_SPLINE_CURVE(2,(#266046,#266047,#266048,#266049,#266050),
 .UNSPECIFIED.,.F.,.F.)
B_SPLINE_CURVE_WITH_KNOTS((3,2,3),(0.,0.025,0.0310216655371729),
 .UNSPECIFIED.)
CURVE()
GEOMETRIC_REPRESENTATION_ITEM()
RATIONAL_B_SPLINE_CURVE((1.,0.996917333733128,1.,0.999257488591127,0.998872669611195))
REPRESENTATION_ITEM('')
);
#4155=(
BOUNDED_CURVE()
B_SPLINE_CURVE(2,(#266216,#266217,#266218,#266219,#266220,#266221,#266222),
 .UNSPECIFIED.,.F.,.F.)
B_SPLINE_CURVE_WITH_KNOTS((3,2,2,3),(0.,0.025,0.05,0.0627352828483775),
 .UNSPECIFIED.)
CURVE()
GEOMETRIC_REPRESENTATION_ITEM()
RATIONAL_B_SPLINE_CURVE((1.,0.996917333733128,1.,0.996917333733128,1.,0.998429654926569,
0.998459212947514))
REPRESENTATION_ITEM('')
);
#4156=(
BOUNDED_CURVE()
B_SPLINE_CURVE(2,(#266396,#266397,#266398,#266399,#266400),
 .UNSPECIFIED.,.F.,.F.)
B_SPLINE_CURVE_WITH_KNOTS((3,2,3),(0.,0.025,0.0310216655371733),
 .UNSPECIFIED.)
CURVE()
GEOMETRIC_REPRESENTATION_ITEM()
RATIONAL_B_SPLINE_CURVE((1.,0.996917333733128,1.,0.999257488591127,0.998872669611195))
REPRESENTATION_ITEM('')
);
#4157=(
BOUNDED_CURVE()
B_SPLINE_CURVE(2,(#267289,#267290,#267291,#267292,#267293,#267294,#267295,
#267296,#267297,#267298,#267299,#267300,#267301,#267302,#267303,#267304,
#267305,#267306,#267307,#267308,#267309,#267310,#267311,#267312,#267313,
#267314,#267315,#267316,#267317,#267318,#267319,#267320,#267321,#267322,
#267323,#267324,#267325,#267326,#267327,#267328,#267329,#267330,#267331,
#267332,#267333,#267334,#267335,#267336,#267337,#267338,#267339,#267340,
#267341,#267342,#267343,#267344,#267345,#267346,#267347,#267348,#267349,
#267350,#267351,#267352,#267353,#267354,#267355,#267356,#267357,#267358,
#267359,#267360,#267361,#267362,#267363,#267364,#267365,#267366,#267367,
#267368,#267369),.UNSPECIFIED.,.F.,.F.)
B_SPLINE_CURVE_WITH_KNOTS((3,2,2,2,2,2,2,2,2,2,2,2,2,2,2,2,2,2,2,2,2,2,
2,2,2,2,2,2,2,2,2,2,2,2,2,2,2,2,2,2,3),(0.0125710582477619,0.025,0.05,0.075,
0.1,0.125,0.15,0.175,0.2,0.225,0.25,0.275,0.3,0.325,0.35,0.375,0.4,0.425,
0.45,0.475,0.5,0.525,0.55,0.575,0.6,0.625,0.65,0.675,0.7,0.725,0.75,0.775,
0.8,0.825,0.85,0.875,0.9,0.925,0.95,0.975,0.996408889531233),
 .UNSPECIFIED.)
CURVE()
GEOMETRIC_REPRESENTATION_ITEM()
RATIONAL_B_SPLINE_CURVE((0.998458716675295,0.998467428821098,1.,0.996917333733128,
1.,0.996917333733128,1.,0.996917333733128,1.,0.996917333733128,1.,0.996917333733128,
1.,0.996917333733128,1.,0.996917333733128,1.,0.996917333733128,1.,0.996917333733128,
1.,0.996917333733128,1.,0.996917333733128,1.,0.996917333733128,1.,0.996917333733128,
1.,0.996917333733128,1.,0.996917333733128,1.,0.996917333733128,1.,0.996917333733128,
1.,0.996917333733128,1.,0.996917333733128,1.,0.996917333733128,1.,0.996917333733128,
1.,0.996917333733128,1.,0.996917333733128,1.,0.996917333733128,1.,0.996917333733128,
1.,0.996917333733128,1.,0.996917333733128,1.,0.996917333733128,1.,0.996917333733128,
1.,0.996917333733128,1.,0.996917333733128,1.,0.996917333733128,1.,0.996917333733128,
1.,0.996917333733128,1.,0.996917333733128,1.,0.996917333733128,1.,0.996917333733128,
1.,0.996917333733128,1.,0.997360141537235,0.999241598131064))
REPRESENTATION_ITEM('')
);
#4158=(
BOUNDED_CURVE()
B_SPLINE_CURVE(2,(#267370,#267371,#267372,#267373,#267374,#267375,#267376,
#267377,#267378,#267379,#267380,#267381,#267382,#267383,#267384,#267385,
#267386,#267387,#267388,#267389,#267390,#267391,#267392,#267393,#267394,
#267395,#267396,#267397,#267398,#267399,#267400,#267401,#267402,#267403,
#267404,#267405,#267406,#267407,#267408,#267409,#267410,#267411,#267412,
#267413,#267414,#267415,#267416,#267417,#267418,#267419,#267420,#267421,
#267422,#267423,#267424,#267425,#267426,#267427,#267428,#267429,#267430,
#267431,#267432,#267433,#267434,#267435,#267436,#267437,#267438,#267439,
#267440,#267441,#267442,#267443,#267444,#267445,#267446,#267447,#267448,
#267449,#267450),.UNSPECIFIED.,.F.,.F.)
B_SPLINE_CURVE_WITH_KNOTS((3,2,2,2,2,2,2,2,2,2,2,2,2,2,2,2,2,2,2,2,2,2,
2,2,2,2,2,2,2,2,2,2,2,2,2,2,2,2,2,2,3),(0.00359111046876693,0.025,0.05,
0.075,0.1,0.125,0.15,0.175,0.2,0.225,0.25,0.275,0.3,0.325,0.35,0.375,0.4,
0.425,0.45,0.475,0.5,0.525,0.55,0.575,0.6,0.625,0.65,0.675,0.7,0.725,0.75,
0.775,0.8,0.825,0.85,0.875,0.9,0.925,0.95,0.975,0.987428941752238),
 .UNSPECIFIED.)
CURVE()
GEOMETRIC_REPRESENTATION_ITEM()
RATIONAL_B_SPLINE_CURVE((0.999241598131064,0.997360141537235,1.,0.996917333733128,
1.,0.996917333733128,1.,0.996917333733128,1.,0.996917333733128,1.,0.996917333733128,
1.,0.996917333733128,1.,0.996917333733128,1.,0.996917333733128,1.,0.996917333733128,
1.,0.996917333733128,1.,0.996917333733128,1.,0.996917333733128,1.,0.996917333733128,
1.,0.996917333733128,1.,0.996917333733128,1.,0.996917333733128,1.,0.996917333733128,
1.,0.996917333733128,1.,0.996917333733128,1.,0.996917333733128,1.,0.996917333733128,
1.,0.996917333733128,1.,0.996917333733128,1.,0.996917333733128,1.,0.996917333733128,
1.,0.996917333733128,1.,0.996917333733128,1.,0.996917333733128,1.,0.996917333733128,
1.,0.996917333733128,1.,0.996917333733128,1.,0.996917333733128,1.,0.996917333733128,
1.,0.996917333733128,1.,0.996917333733128,1.,0.996917333733128,1.,0.996917333733128,
1.,0.996917333733128,1.,0.998467428821098,0.998458716675295))
REPRESENTATION_ITEM('')
);
#4159=(
BOUNDED_CURVE()
B_SPLINE_CURVE(2,(#267613,#267614,#267615,#267616,#267617,#267618,#267619,
#267620,#267621,#267622,#267623,#267624,#267625,#267626,#267627,#267628,
#267629,#267630,#267631,#267632,#267633,#267634,#267635,#267636,#267637,
#267638,#267639,#267640,#267641,#267642,#267643,#267644,#267645,#267646,
#267647,#267648,#267649,#267650,#267651,#267652,#267653,#267654,#267655,
#267656,#267657,#267658,#267659,#267660,#267661,#267662,#267663,#267664,
#267665,#267666,#267667,#267668,#267669,#267670,#267671,#267672,#267673,
#267674,#267675,#267676,#267677,#267678,#267679,#267680,#267681,#267682,
#267683,#267684,#267685,#267686,#267687,#267688,#267689,#267690,#267691,
#267692,#267693),.UNSPECIFIED.,.F.,.F.)
B_SPLINE_CURVE_WITH_KNOTS((3,2,2,2,2,2,2,2,2,2,2,2,2,2,2,2,2,2,2,2,2,2,
2,2,2,2,2,2,2,2,2,2,2,2,2,2,2,2,2,2,3),(0.00288613200956877,0.025,0.05,
0.075,0.1,0.125,0.15,0.175,0.2,0.225,0.25,0.275,0.3,0.325,0.35,0.375,0.4,
0.425,0.45,0.475,0.5,0.525,0.55,0.575,0.6,0.625,0.65,0.675,0.7,0.725,0.75,
0.775,0.8,0.825,0.85,0.875,0.9,0.925,0.95,0.975,0.98954155634899),
 .UNSPECIFIED.)
CURVE()
GEOMETRIC_REPRESENTATION_ITEM()
RATIONAL_B_SPLINE_CURVE((0.999370410621552,0.997273213004633,1.,0.996917333733128,
1.,0.996917333733128,1.,0.996917333733128,1.,0.996917333733128,1.,0.996917333733128,
1.,0.996917333733128,1.,0.996917333733128,1.,0.996917333733128,1.,0.996917333733128,
1.,0.996917333733128,1.,0.996917333733128,1.,0.996917333733128,1.,0.996917333733128,
1.,0.996917333733128,1.,0.996917333733128,1.,0.996917333733128,1.,0.996917333733128,
1.,0.996917333733128,1.,0.996917333733128,1.,0.996917333733128,1.,0.996917333733128,
1.,0.996917333733128,1.,0.996917333733128,1.,0.996917333733128,1.,0.996917333733128,
1.,0.996917333733128,1.,0.996917333733128,1.,0.996917333733128,1.,0.996917333733128,
1.,0.996917333733128,1.,0.996917333733128,1.,0.996917333733128,1.,0.996917333733128,
1.,0.996917333733128,1.,0.996917333733128,1.,0.996917333733128,1.,0.996917333733128,
1.,0.996917333733128,1.,0.998206929391006,0.998499781765884))
REPRESENTATION_ITEM('')
);
#4160=(
BOUNDED_CURVE()
B_SPLINE_CURVE(2,(#267856,#267857,#267858,#267859,#267860,#267861,#267862,
#267863,#267864,#267865,#267866,#267867,#267868,#267869,#267870,#267871,
#267872,#267873,#267874,#267875,#267876,#267877,#267878,#267879,#267880,
#267881,#267882,#267883,#267884,#267885,#267886,#267887,#267888,#267889,
#267890,#267891,#267892,#267893,#267894,#267895,#267896,#267897,#267898,
#267899,#267900,#267901,#267902,#267903,#267904,#267905,#267906,#267907,
#267908,#267909,#267910,#267911,#267912,#267913,#267914,#267915,#267916,
#267917,#267918,#267919,#267920,#267921,#267922,#267923,#267924,#267925,
#267926,#267927,#267928,#267929,#267930,#267931,#267932,#267933,#267934,
#267935,#267936),.UNSPECIFIED.,.F.,.F.)
B_SPLINE_CURVE_WITH_KNOTS((3,2,2,2,2,2,2,2,2,2,2,2,2,2,2,2,2,2,2,2,2,2,
2,2,2,2,2,2,2,2,2,2,2,2,2,2,2,2,2,2,3),(0.0104584436510098,0.025,0.05,0.075,
0.1,0.125,0.15,0.175,0.2,0.225,0.25,0.275,0.3,0.325,0.35,0.375,0.4,0.425,
0.45,0.475,0.5,0.525,0.55,0.575,0.6,0.625,0.65,0.675,0.7,0.725,0.75,0.775,
0.8,0.825,0.85,0.875,0.9,0.925,0.95,0.975,0.997113867990431),
 .UNSPECIFIED.)
CURVE()
GEOMETRIC_REPRESENTATION_ITEM()
RATIONAL_B_SPLINE_CURVE((0.998499781765884,0.998206929391006,1.,0.996917333733128,
1.,0.996917333733128,1.,0.996917333733128,1.,0.996917333733128,1.,0.996917333733128,
1.,0.996917333733128,1.,0.996917333733128,1.,0.996917333733128,1.,0.996917333733128,
1.,0.996917333733128,1.,0.996917333733128,1.,0.996917333733128,1.,0.996917333733128,
1.,0.996917333733128,1.,0.996917333733128,1.,0.996917333733128,1.,0.996917333733128,
1.,0.996917333733128,1.,0.996917333733128,1.,0.996917333733128,1.,0.996917333733128,
1.,0.996917333733128,1.,0.996917333733128,1.,0.996917333733128,1.,0.996917333733128,
1.,0.996917333733128,1.,0.996917333733128,1.,0.996917333733128,1.,0.996917333733128,
1.,0.996917333733128,1.,0.996917333733128,1.,0.996917333733128,1.,0.996917333733128,
1.,0.996917333733128,1.,0.996917333733128,1.,0.996917333733128,1.,0.996917333733128,
1.,0.996917333733128,1.,0.997273213004633,0.999370410621552))
REPRESENTATION_ITEM('')
);
#4161=(
BOUNDED_CURVE()
B_SPLINE_CURVE(2,(#268941,#268942,#268943,#268944,#268945,#268946,#268947,
#268948,#268949,#268950,#268951,#268952,#268953,#268954,#268955,#268956,
#268957,#268958,#268959,#268960,#268961,#268962,#268963,#268964,#268965,
#268966,#268967,#268968,#268969,#268970,#268971,#268972,#268973,#268974,
#268975,#268976,#268977,#268978,#268979,#268980,#268981,#268982,#268983,
#268984,#268985,#268986,#268987,#268988,#268989,#268990,#268991,#268992,
#268993,#268994,#268995,#268996,#268997,#268998,#268999,#269000,#269001,
#269002,#269003,#269004,#269005,#269006,#269007,#269008,#269009,#269010,
#269011,#269012,#269013,#269014,#269015,#269016,#269017,#269018,#269019,
#269020,#269021),.UNSPECIFIED.,.F.,.F.)
B_SPLINE_CURVE_WITH_KNOTS((3,2,2,2,2,2,2,2,2,2,2,2,2,2,2,2,2,2,2,2,2,2,
2,2,2,2,2,2,2,2,2,2,2,2,2,2,2,2,2,2,3),(0.00359111046876831,0.025,0.05,
0.075,0.1,0.125,0.15,0.175,0.2,0.225,0.25,0.275,0.3,0.325,0.35,0.375,0.4,
0.425,0.45,0.475,0.5,0.525,0.55,0.575,0.6,0.625,0.65,0.675,0.7,0.725,0.75,
0.775,0.8,0.825,0.85,0.875,0.9,0.925,0.95,0.975,0.987428941752238),
 .UNSPECIFIED.)
CURVE()
GEOMETRIC_REPRESENTATION_ITEM()
RATIONAL_B_SPLINE_CURVE((0.999241598131064,0.997360141537235,1.,0.996917333733128,
1.,0.996917333733128,1.,0.996917333733128,1.,0.996917333733128,1.,0.996917333733128,
1.,0.996917333733128,1.,0.996917333733128,1.,0.996917333733128,1.,0.996917333733128,
1.,0.996917333733128,1.,0.996917333733128,1.,0.996917333733128,1.,0.996917333733128,
1.,0.996917333733128,1.,0.996917333733128,1.,0.996917333733128,1.,0.996917333733128,
1.,0.996917333733128,1.,0.996917333733128,1.,0.996917333733128,1.,0.996917333733128,
1.,0.996917333733128,1.,0.996917333733128,1.,0.996917333733128,1.,0.996917333733128,
1.,0.996917333733128,1.,0.996917333733128,1.,0.996917333733128,1.,0.996917333733128,
1.,0.996917333733128,1.,0.996917333733128,1.,0.996917333733128,1.,0.996917333733128,
1.,0.996917333733128,1.,0.996917333733128,1.,0.996917333733128,1.,0.996917333733128,
1.,0.996917333733128,1.,0.998467428821098,0.998458716675295))
REPRESENTATION_ITEM('')
);
#4162=(
BOUNDED_CURVE()
B_SPLINE_CURVE(2,(#269022,#269023,#269024,#269025,#269026,#269027,#269028,
#269029,#269030,#269031,#269032,#269033,#269034,#269035,#269036,#269037,
#269038,#269039,#269040,#269041,#269042,#269043,#269044,#269045,#269046,
#269047,#269048,#269049,#269050,#269051,#269052,#269053,#269054,#269055,
#269056,#269057,#269058,#269059,#269060,#269061,#269062,#269063,#269064,
#269065,#269066,#269067,#269068,#269069,#269070,#269071,#269072,#269073,
#269074,#269075,#269076,#269077,#269078,#269079,#269080,#269081,#269082,
#269083,#269084,#269085,#269086,#269087,#269088,#269089,#269090,#269091,
#269092,#269093,#269094,#269095,#269096,#269097,#269098,#269099,#269100,
#269101,#269102),.UNSPECIFIED.,.F.,.F.)
B_SPLINE_CURVE_WITH_KNOTS((3,2,2,2,2,2,2,2,2,2,2,2,2,2,2,2,2,2,2,2,2,2,
2,2,2,2,2,2,2,2,2,2,2,2,2,2,2,2,2,2,3),(0.0125710582477632,0.025,0.05,0.075,
0.1,0.125,0.15,0.175,0.2,0.225,0.25,0.275,0.3,0.325,0.35,0.375,0.4,0.425,
0.45,0.475,0.5,0.525,0.55,0.575,0.6,0.625,0.65,0.675,0.7,0.725,0.75,0.775,
0.8,0.825,0.85,0.875,0.9,0.925,0.95,0.975,0.996408889531233),
 .UNSPECIFIED.)
CURVE()
GEOMETRIC_REPRESENTATION_ITEM()
RATIONAL_B_SPLINE_CURVE((0.998458716675295,0.998467428821098,1.,0.996917333733128,
1.,0.996917333733128,1.,0.996917333733128,1.,0.996917333733128,1.,0.996917333733128,
1.,0.996917333733128,1.,0.996917333733128,1.,0.996917333733128,1.,0.996917333733128,
1.,0.996917333733128,1.,0.996917333733128,1.,0.996917333733128,1.,0.996917333733128,
1.,0.996917333733128,1.,0.996917333733128,1.,0.996917333733128,1.,0.996917333733128,
1.,0.996917333733128,1.,0.996917333733128,1.,0.996917333733128,1.,0.996917333733128,
1.,0.996917333733128,1.,0.996917333733128,1.,0.996917333733128,1.,0.996917333733128,
1.,0.996917333733128,1.,0.996917333733128,1.,0.996917333733128,1.,0.996917333733128,
1.,0.996917333733128,1.,0.996917333733128,1.,0.996917333733128,1.,0.996917333733128,
1.,0.996917333733128,1.,0.996917333733128,1.,0.996917333733128,1.,0.996917333733128,
1.,0.996917333733128,1.,0.997360141537235,0.999241598131064))
REPRESENTATION_ITEM('')
);
#4163=(
BOUNDED_CURVE()
B_SPLINE_CURVE(2,(#269265,#269266,#269267,#269268,#269269,#269270,#269271,
#269272,#269273,#269274,#269275,#269276,#269277,#269278,#269279,#269280,
#269281,#269282,#269283,#269284,#269285,#269286,#269287,#269288,#269289,
#269290,#269291,#269292,#269293,#269294,#269295,#269296,#269297,#269298,
#269299,#269300,#269301,#269302,#269303,#269304,#269305,#269306,#269307,
#269308,#269309,#269310,#269311,#269312,#269313,#269314,#269315,#269316,
#269317,#269318,#269319,#269320,#269321,#269322,#269323,#269324,#269325,
#269326,#269327,#269328,#269329,#269330,#269331,#269332,#269333,#269334,
#269335,#269336,#269337,#269338,#269339,#269340,#269341,#269342,#269343,
#269344,#269345),.UNSPECIFIED.,.F.,.F.)
B_SPLINE_CURVE_WITH_KNOTS((3,2,2,2,2,2,2,2,2,2,2,2,2,2,2,2,2,2,2,2,2,2,
2,2,2,2,2,2,2,2,2,2,2,2,2,2,2,2,2,2,3),(0.00288613200956991,0.025,0.05,
0.075,0.1,0.125,0.15,0.175,0.2,0.225,0.25,0.275,0.3,0.325,0.35,0.375,0.4,
0.425,0.45,0.475,0.5,0.525,0.55,0.575,0.6,0.625,0.65,0.675,0.7,0.725,0.75,
0.775,0.8,0.825,0.85,0.875,0.9,0.925,0.95,0.975,0.98954155634899),
 .UNSPECIFIED.)
CURVE()
GEOMETRIC_REPRESENTATION_ITEM()
RATIONAL_B_SPLINE_CURVE((0.999370410621551,0.997273213004634,1.,0.996917333733128,
1.,0.996917333733128,1.,0.996917333733128,1.,0.996917333733128,1.,0.996917333733128,
1.,0.996917333733128,1.,0.996917333733128,1.,0.996917333733128,1.,0.996917333733128,
1.,0.996917333733128,1.,0.996917333733128,1.,0.996917333733128,1.,0.996917333733128,
1.,0.996917333733128,1.,0.996917333733128,1.,0.996917333733128,1.,0.996917333733128,
1.,0.996917333733128,1.,0.996917333733128,1.,0.996917333733128,1.,0.996917333733128,
1.,0.996917333733128,1.,0.996917333733128,1.,0.996917333733128,1.,0.996917333733128,
1.,0.996917333733128,1.,0.996917333733128,1.,0.996917333733128,1.,0.996917333733128,
1.,0.996917333733128,1.,0.996917333733128,1.,0.996917333733128,1.,0.996917333733128,
1.,0.996917333733128,1.,0.996917333733128,1.,0.996917333733128,1.,0.996917333733128,
1.,0.996917333733128,1.,0.998206929391006,0.998499781765884))
REPRESENTATION_ITEM('')
);
#4164=(
BOUNDED_CURVE()
B_SPLINE_CURVE(2,(#269508,#269509,#269510,#269511,#269512,#269513,#269514,
#269515,#269516,#269517,#269518,#269519,#269520,#269521,#269522,#269523,
#269524,#269525,#269526,#269527,#269528,#269529,#269530,#269531,#269532,
#269533,#269534,#269535,#269536,#269537,#269538,#269539,#269540,#269541,
#269542,#269543,#269544,#269545,#269546,#269547,#269548,#269549,#269550,
#269551,#269552,#269553,#269554,#269555,#269556,#269557,#269558,#269559,
#269560,#269561,#269562,#269563,#269564,#269565,#269566,#269567,#269568,
#269569,#269570,#269571,#269572,#269573,#269574,#269575,#269576,#269577,
#269578,#269579,#269580,#269581,#269582,#269583,#269584,#269585,#269586,
#269587,#269588),.UNSPECIFIED.,.F.,.F.)
B_SPLINE_CURVE_WITH_KNOTS((3,2,2,2,2,2,2,2,2,2,2,2,2,2,2,2,2,2,2,2,2,2,
2,2,2,2,2,2,2,2,2,2,2,2,2,2,2,2,2,2,3),(0.0104584436510109,0.025,0.05,0.075,
0.1,0.125,0.15,0.175,0.2,0.225,0.25,0.275,0.3,0.325,0.35,0.375,0.4,0.425,
0.45,0.475,0.5,0.525,0.55,0.575,0.6,0.625,0.65,0.675,0.7,0.725,0.75,0.775,
0.8,0.825,0.85,0.875,0.9,0.925,0.95,0.975,0.997113867990431),
 .UNSPECIFIED.)
CURVE()
GEOMETRIC_REPRESENTATION_ITEM()
RATIONAL_B_SPLINE_CURVE((0.998499781765884,0.998206929391006,1.,0.996917333733128,
1.,0.996917333733128,1.,0.996917333733128,1.,0.996917333733128,1.,0.996917333733128,
1.,0.996917333733128,1.,0.996917333733128,1.,0.996917333733128,1.,0.996917333733128,
1.,0.996917333733128,1.,0.996917333733128,1.,0.996917333733128,1.,0.996917333733128,
1.,0.996917333733128,1.,0.996917333733128,1.,0.996917333733128,1.,0.996917333733128,
1.,0.996917333733128,1.,0.996917333733128,1.,0.996917333733128,1.,0.996917333733128,
1.,0.996917333733128,1.,0.996917333733128,1.,0.996917333733128,1.,0.996917333733128,
1.,0.996917333733128,1.,0.996917333733128,1.,0.996917333733128,1.,0.996917333733128,
1.,0.996917333733128,1.,0.996917333733128,1.,0.996917333733128,1.,0.996917333733128,
1.,0.996917333733128,1.,0.996917333733128,1.,0.996917333733128,1.,0.996917333733128,
1.,0.996917333733128,1.,0.997273213004633,0.999370410621552))
REPRESENTATION_ITEM('')
);
#4165=(
BOUNDED_CURVE()
B_SPLINE_CURVE(2,(#269913,#269914,#269915,#269916,#269917,#269918,#269919,
#269920,#269921,#269922,#269923,#269924,#269925,#269926,#269927,#269928,
#269929,#269930,#269931,#269932,#269933,#269934,#269935,#269936,#269937,
#269938,#269939,#269940,#269941,#269942,#269943,#269944,#269945,#269946,
#269947,#269948,#269949,#269950,#269951,#269952,#269953,#269954,#269955,
#269956,#269957,#269958,#269959,#269960,#269961,#269962,#269963,#269964,
#269965,#269966,#269967,#269968,#269969,#269970,#269971,#269972,#269973,
#269974,#269975,#269976,#269977,#269978,#269979,#269980,#269981,#269982,
#269983,#269984,#269985,#269986,#269987,#269988,#269989,#269990,#269991,
#269992,#269993),.UNSPECIFIED.,.F.,.F.)
B_SPLINE_CURVE_WITH_KNOTS((3,2,2,2,2,2,2,2,2,2,2,2,2,2,2,2,2,2,2,2,2,2,
2,2,2,2,2,2,2,2,2,2,2,2,2,2,2,2,2,2,3),(0.0104584436510113,0.025,0.05,0.075,
0.1,0.125,0.15,0.175,0.2,0.225,0.25,0.275,0.3,0.325,0.35,0.375,0.4,0.425,
0.45,0.475,0.5,0.525,0.55,0.575,0.6,0.625,0.65,0.675,0.7,0.725,0.75,0.775,
0.8,0.825,0.85,0.875,0.9,0.925,0.95,0.975,0.997113867990431),
 .UNSPECIFIED.)
CURVE()
GEOMETRIC_REPRESENTATION_ITEM()
RATIONAL_B_SPLINE_CURVE((0.998499781765884,0.998206929391006,1.,0.996917333733128,
1.,0.996917333733128,1.,0.996917333733128,1.,0.996917333733128,1.,0.996917333733128,
1.,0.996917333733128,1.,0.996917333733128,1.,0.996917333733128,1.,0.996917333733128,
1.,0.996917333733128,1.,0.996917333733128,1.,0.996917333733128,1.,0.996917333733128,
1.,0.996917333733128,1.,0.996917333733128,1.,0.996917333733128,1.,0.996917333733128,
1.,0.996917333733128,1.,0.996917333733128,1.,0.996917333733128,1.,0.996917333733128,
1.,0.996917333733128,1.,0.996917333733128,1.,0.996917333733128,1.,0.996917333733128,
1.,0.996917333733128,1.,0.996917333733128,1.,0.996917333733128,1.,0.996917333733128,
1.,0.996917333733128,1.,0.996917333733128,1.,0.996917333733128,1.,0.996917333733128,
1.,0.996917333733128,1.,0.996917333733128,1.,0.996917333733128,1.,0.996917333733128,
1.,0.996917333733128,1.,0.997273213004634,0.999370410621552))
REPRESENTATION_ITEM('')
);
#4166=(
BOUNDED_CURVE()
B_SPLINE_CURVE(2,(#269994,#269995,#269996,#269997,#269998,#269999,#270000,
#270001,#270002,#270003,#270004,#270005,#270006,#270007,#270008,#270009,
#270010,#270011,#270012,#270013,#270014,#270015,#270016,#270017,#270018,
#270019,#270020,#270021,#270022,#270023,#270024,#270025,#270026,#270027,
#270028,#270029,#270030,#270031,#270032,#270033,#270034,#270035,#270036,
#270037,#270038,#270039,#270040,#270041,#270042,#270043,#270044,#270045,
#270046,#270047,#270048,#270049,#270050,#270051,#270052,#270053,#270054,
#270055,#270056,#270057,#270058,#270059,#270060,#270061,#270062,#270063,
#270064,#270065,#270066,#270067,#270068,#270069,#270070,#270071,#270072,
#270073,#270074),.UNSPECIFIED.,.F.,.F.)
B_SPLINE_CURVE_WITH_KNOTS((3,2,2,2,2,2,2,2,2,2,2,2,2,2,2,2,2,2,2,2,2,2,
2,2,2,2,2,2,2,2,2,2,2,2,2,2,2,2,2,2,3),(0.00288613200957066,0.025,0.05,
0.075,0.1,0.125,0.15,0.175,0.2,0.225,0.25,0.275,0.3,0.325,0.35,0.375,0.4,
0.425,0.45,0.475,0.5,0.525,0.55,0.575,0.6,0.625,0.65,0.675,0.7,0.725,0.75,
0.775,0.8,0.825,0.85,0.875,0.9,0.925,0.95,0.975,0.98954155634899),
 .UNSPECIFIED.)
CURVE()
GEOMETRIC_REPRESENTATION_ITEM()
RATIONAL_B_SPLINE_CURVE((0.999370410621551,0.997273213004634,1.,0.996917333733128,
1.,0.996917333733128,1.,0.996917333733128,1.,0.996917333733128,1.,0.996917333733128,
1.,0.996917333733128,1.,0.996917333733128,1.,0.996917333733128,1.,0.996917333733128,
1.,0.996917333733128,1.,0.996917333733128,1.,0.996917333733128,1.,0.996917333733128,
1.,0.996917333733128,1.,0.996917333733128,1.,0.996917333733128,1.,0.996917333733128,
1.,0.996917333733128,1.,0.996917333733128,1.,0.996917333733128,1.,0.996917333733128,
1.,0.996917333733128,1.,0.996917333733128,1.,0.996917333733128,1.,0.996917333733128,
1.,0.996917333733128,1.,0.996917333733128,1.,0.996917333733128,1.,0.996917333733128,
1.,0.996917333733128,1.,0.996917333733128,1.,0.996917333733128,1.,0.996917333733128,
1.,0.996917333733128,1.,0.996917333733128,1.,0.996917333733128,1.,0.996917333733128,
1.,0.996917333733128,1.,0.998206929391006,0.998499781765884))
REPRESENTATION_ITEM('')
);
#4167=(
BOUNDED_CURVE()
B_SPLINE_CURVE(2,(#270237,#270238,#270239,#270240,#270241,#270242,#270243,
#270244,#270245,#270246,#270247,#270248,#270249,#270250,#270251,#270252,
#270253,#270254,#270255,#270256,#270257,#270258,#270259,#270260,#270261,
#270262,#270263,#270264,#270265,#270266,#270267,#270268,#270269,#270270,
#270271,#270272,#270273,#270274,#270275,#270276,#270277,#270278,#270279,
#270280,#270281,#270282,#270283,#270284,#270285,#270286,#270287,#270288,
#270289,#270290,#270291,#270292,#270293,#270294,#270295,#270296,#270297,
#270298,#270299,#270300,#270301,#270302,#270303,#270304,#270305,#270306,
#270307,#270308,#270309,#270310,#270311,#270312,#270313,#270314,#270315,
#270316,#270317),.UNSPECIFIED.,.F.,.F.)
B_SPLINE_CURVE_WITH_KNOTS((3,2,2,2,2,2,2,2,2,2,2,2,2,2,2,2,2,2,2,2,2,2,
2,2,2,2,2,2,2,2,2,2,2,2,2,2,2,2,2,2,3),(0.0125710582477639,0.025,0.05,0.075,
0.1,0.125,0.15,0.175,0.2,0.225,0.25,0.275,0.3,0.325,0.35,0.375,0.4,0.425,
0.45,0.475,0.5,0.525,0.55,0.575,0.6,0.625,0.65,0.675,0.7,0.725,0.75,0.775,
0.8,0.825,0.85,0.875,0.9,0.925,0.95,0.975,0.996408889531232),
 .UNSPECIFIED.)
CURVE()
GEOMETRIC_REPRESENTATION_ITEM()
RATIONAL_B_SPLINE_CURVE((0.998458716675295,0.998467428821099,1.,0.996917333733128,
1.,0.996917333733128,1.,0.996917333733128,1.,0.996917333733128,1.,0.996917333733128,
1.,0.996917333733128,1.,0.996917333733128,1.,0.996917333733128,1.,0.996917333733128,
1.,0.996917333733128,1.,0.996917333733128,1.,0.996917333733128,1.,0.996917333733128,
1.,0.996917333733128,1.,0.996917333733128,1.,0.996917333733128,1.,0.996917333733128,
1.,0.996917333733128,1.,0.996917333733128,1.,0.996917333733128,1.,0.996917333733128,
1.,0.996917333733128,1.,0.996917333733128,1.,0.996917333733128,1.,0.996917333733128,
1.,0.996917333733128,1.,0.996917333733128,1.,0.996917333733128,1.,0.996917333733128,
1.,0.996917333733128,1.,0.996917333733128,1.,0.996917333733128,1.,0.996917333733128,
1.,0.996917333733128,1.,0.996917333733128,1.,0.996917333733128,1.,0.996917333733128,
1.,0.996917333733128,1.,0.997360141537235,0.999241598131064))
REPRESENTATION_ITEM('')
);
#4168=(
BOUNDED_CURVE()
B_SPLINE_CURVE(2,(#270480,#270481,#270482,#270483,#270484,#270485,#270486,
#270487,#270488,#270489,#270490,#270491,#270492,#270493,#270494,#270495,
#270496,#270497,#270498,#270499,#270500,#270501,#270502,#270503,#270504,
#270505,#270506,#270507,#270508,#270509,#270510,#270511,#270512,#270513,
#270514,#270515,#270516,#270517,#270518,#270519,#270520,#270521,#270522,
#270523,#270524,#270525,#270526,#270527,#270528,#270529,#270530,#270531,
#270532,#270533,#270534,#270535,#270536,#270537,#270538,#270539,#270540,
#270541,#270542,#270543,#270544,#270545,#270546,#270547,#270548,#270549,
#270550,#270551,#270552,#270553,#270554,#270555,#270556,#270557,#270558,
#270559,#270560),.UNSPECIFIED.,.F.,.F.)
B_SPLINE_CURVE_WITH_KNOTS((3,2,2,2,2,2,2,2,2,2,2,2,2,2,2,2,2,2,2,2,2,2,
2,2,2,2,2,2,2,2,2,2,2,2,2,2,2,2,2,2,3),(0.00359111046876932,0.025,0.05,
0.075,0.1,0.125,0.15,0.175,0.2,0.225,0.25,0.275,0.3,0.325,0.35,0.375,0.4,
0.425,0.45,0.475,0.5,0.525,0.55,0.575,0.6,0.625,0.65,0.675,0.7,0.725,0.75,
0.775,0.8,0.825,0.85,0.875,0.9,0.925,0.95,0.975,0.987428941752237),
 .UNSPECIFIED.)
CURVE()
GEOMETRIC_REPRESENTATION_ITEM()
RATIONAL_B_SPLINE_CURVE((0.999241598131064,0.997360141537235,1.,0.996917333733128,
1.,0.996917333733128,1.,0.996917333733128,1.,0.996917333733128,1.,0.996917333733128,
1.,0.996917333733128,1.,0.996917333733128,1.,0.996917333733128,1.,0.996917333733128,
1.,0.996917333733128,1.,0.996917333733128,1.,0.996917333733128,1.,0.996917333733128,
1.,0.996917333733128,1.,0.996917333733128,1.,0.996917333733128,1.,0.996917333733128,
1.,0.996917333733128,1.,0.996917333733128,1.,0.996917333733128,1.,0.996917333733128,
1.,0.996917333733128,1.,0.996917333733128,1.,0.996917333733128,1.,0.996917333733128,
1.,0.996917333733128,1.,0.996917333733128,1.,0.996917333733128,1.,0.996917333733128,
1.,0.996917333733128,1.,0.996917333733128,1.,0.996917333733128,1.,0.996917333733128,
1.,0.996917333733128,1.,0.996917333733128,1.,0.996917333733128,1.,0.996917333733128,
1.,0.996917333733128,1.,0.998467428821098,0.998458716675295))
REPRESENTATION_ITEM('')
);
#4169=(
BOUNDED_CURVE()
B_SPLINE_CURVE(2,(#270885,#270886,#270887,#270888,#270889,#270890,#270891,
#270892,#270893,#270894,#270895,#270896,#270897,#270898,#270899,#270900,
#270901,#270902,#270903,#270904,#270905,#270906,#270907,#270908,#270909,
#270910,#270911,#270912,#270913,#270914,#270915,#270916,#270917,#270918,
#270919,#270920,#270921,#270922,#270923,#270924,#270925,#270926,#270927,
#270928,#270929,#270930,#270931,#270932,#270933,#270934,#270935,#270936,
#270937,#270938,#270939,#270940,#270941,#270942,#270943,#270944,#270945,
#270946,#270947,#270948,#270949,#270950,#270951,#270952,#270953,#270954,
#270955,#270956,#270957,#270958,#270959,#270960,#270961,#270962,#270963,
#270964,#270965),.UNSPECIFIED.,.F.,.F.)
B_SPLINE_CURVE_WITH_KNOTS((3,2,2,2,2,2,2,2,2,2,2,2,2,2,2,2,2,2,2,2,2,2,
2,2,2,2,2,2,2,2,2,2,2,2,2,2,2,2,2,2,3),(0.0125710582477628,0.025,0.05,0.075,
0.1,0.125,0.15,0.175,0.2,0.225,0.25,0.275,0.3,0.325,0.35,0.375,0.4,0.425,
0.45,0.475,0.5,0.525,0.55,0.575,0.6,0.625,0.65,0.675,0.7,0.725,0.75,0.775,
0.8,0.825,0.85,0.875,0.9,0.925,0.95,0.975,0.996408889531232),
 .UNSPECIFIED.)
CURVE()
GEOMETRIC_REPRESENTATION_ITEM()
RATIONAL_B_SPLINE_CURVE((0.998458716675295,0.998467428821098,1.,0.996917333733128,
1.,0.996917333733128,1.,0.996917333733128,1.,0.996917333733128,1.,0.996917333733128,
1.,0.996917333733128,1.,0.996917333733128,1.,0.996917333733128,1.,0.996917333733128,
1.,0.996917333733128,1.,0.996917333733128,1.,0.996917333733128,1.,0.996917333733128,
1.,0.996917333733128,1.,0.996917333733128,1.,0.996917333733128,1.,0.996917333733128,
1.,0.996917333733128,1.,0.996917333733128,1.,0.996917333733128,1.,0.996917333733128,
1.,0.996917333733128,1.,0.996917333733128,1.,0.996917333733128,1.,0.996917333733128,
1.,0.996917333733128,1.,0.996917333733128,1.,0.996917333733128,1.,0.996917333733128,
1.,0.996917333733128,1.,0.996917333733128,1.,0.996917333733128,1.,0.996917333733128,
1.,0.996917333733128,1.,0.996917333733128,1.,0.996917333733128,1.,0.996917333733128,
1.,0.996917333733128,1.,0.997360141537235,0.999241598131064))
REPRESENTATION_ITEM('')
);
#4170=(
BOUNDED_CURVE()
B_SPLINE_CURVE(2,(#270966,#270967,#270968,#270969,#270970,#270971,#270972,
#270973,#270974,#270975,#270976,#270977,#270978,#270979,#270980,#270981,
#270982,#270983,#270984,#270985,#270986,#270987,#270988,#270989,#270990,
#270991,#270992,#270993,#270994,#270995,#270996,#270997,#270998,#270999,
#271000,#271001,#271002,#271003,#271004,#271005,#271006,#271007,#271008,
#271009,#271010,#271011,#271012,#271013,#271014,#271015,#271016,#271017,
#271018,#271019,#271020,#271021,#271022,#271023,#271024,#271025,#271026,
#271027,#271028,#271029,#271030,#271031,#271032,#271033,#271034,#271035,
#271036,#271037,#271038,#271039,#271040,#271041,#271042,#271043,#271044,
#271045,#271046),.UNSPECIFIED.,.F.,.F.)
B_SPLINE_CURVE_WITH_KNOTS((3,2,2,2,2,2,2,2,2,2,2,2,2,2,2,2,2,2,2,2,2,2,
2,2,2,2,2,2,2,2,2,2,2,2,2,2,2,2,2,2,3),(0.00359111046876783,0.025,0.05,
0.075,0.1,0.125,0.15,0.175,0.2,0.225,0.25,0.275,0.3,0.325,0.35,0.375,0.4,
0.425,0.45,0.475,0.5,0.525,0.55,0.575,0.6,0.625,0.65,0.675,0.7,0.725,0.75,
0.775,0.8,0.825,0.85,0.875,0.9,0.925,0.95,0.975,0.987428941752237),
 .UNSPECIFIED.)
CURVE()
GEOMETRIC_REPRESENTATION_ITEM()
RATIONAL_B_SPLINE_CURVE((0.999241598131064,0.997360141537235,1.,0.996917333733128,
1.,0.996917333733128,1.,0.996917333733128,1.,0.996917333733128,1.,0.996917333733128,
1.,0.996917333733128,1.,0.996917333733128,1.,0.996917333733128,1.,0.996917333733128,
1.,0.996917333733128,1.,0.996917333733128,1.,0.996917333733128,1.,0.996917333733128,
1.,0.996917333733128,1.,0.996917333733128,1.,0.996917333733128,1.,0.996917333733128,
1.,0.996917333733128,1.,0.996917333733128,1.,0.996917333733128,1.,0.996917333733128,
1.,0.996917333733128,1.,0.996917333733128,1.,0.996917333733128,1.,0.996917333733128,
1.,0.996917333733128,1.,0.996917333733128,1.,0.996917333733128,1.,0.996917333733128,
1.,0.996917333733128,1.,0.996917333733128,1.,0.996917333733128,1.,0.996917333733128,
1.,0.996917333733128,1.,0.996917333733128,1.,0.996917333733128,1.,0.996917333733128,
1.,0.996917333733128,1.,0.998467428821098,0.998458716675295))
REPRESENTATION_ITEM('')
);
#4171=(
BOUNDED_CURVE()
B_SPLINE_CURVE(2,(#271209,#271210,#271211,#271212,#271213,#271214,#271215,
#271216,#271217,#271218,#271219,#271220,#271221,#271222,#271223,#271224,
#271225,#271226,#271227,#271228,#271229,#271230,#271231,#271232,#271233,
#271234,#271235,#271236,#271237,#271238,#271239,#271240,#271241,#271242,
#271243,#271244,#271245,#271246,#271247,#271248,#271249,#271250,#271251,
#271252,#271253,#271254,#271255,#271256,#271257,#271258,#271259,#271260,
#271261,#271262,#271263,#271264,#271265,#271266,#271267,#271268,#271269,
#271270,#271271,#271272,#271273,#271274,#271275,#271276,#271277,#271278,
#271279,#271280,#271281,#271282,#271283,#271284,#271285,#271286,#271287,
#271288,#271289),.UNSPECIFIED.,.F.,.F.)
B_SPLINE_CURVE_WITH_KNOTS((3,2,2,2,2,2,2,2,2,2,2,2,2,2,2,2,2,2,2,2,2,2,
2,2,2,2,2,2,2,2,2,2,2,2,2,2,2,2,2,2,3),(0.0104584436510103,0.025,0.05,0.075,
0.1,0.125,0.15,0.175,0.2,0.225,0.25,0.275,0.3,0.325,0.35,0.375,0.4,0.425,
0.45,0.475,0.5,0.525,0.55,0.575,0.6,0.625,0.65,0.675,0.7,0.725,0.75,0.775,
0.8,0.825,0.85,0.875,0.9,0.925,0.95,0.975,0.997113867990431),
 .UNSPECIFIED.)
CURVE()
GEOMETRIC_REPRESENTATION_ITEM()
RATIONAL_B_SPLINE_CURVE((0.998499781765884,0.998206929391006,1.,0.996917333733128,
1.,0.996917333733128,1.,0.996917333733128,1.,0.996917333733128,1.,0.996917333733128,
1.,0.996917333733128,1.,0.996917333733128,1.,0.996917333733128,1.,0.996917333733128,
1.,0.996917333733128,1.,0.996917333733128,1.,0.996917333733128,1.,0.996917333733128,
1.,0.996917333733128,1.,0.996917333733128,1.,0.996917333733128,1.,0.996917333733128,
1.,0.996917333733128,1.,0.996917333733128,1.,0.996917333733128,1.,0.996917333733128,
1.,0.996917333733128,1.,0.996917333733128,1.,0.996917333733128,1.,0.996917333733128,
1.,0.996917333733128,1.,0.996917333733128,1.,0.996917333733128,1.,0.996917333733128,
1.,0.996917333733128,1.,0.996917333733128,1.,0.996917333733128,1.,0.996917333733128,
1.,0.996917333733128,1.,0.996917333733128,1.,0.996917333733128,1.,0.996917333733128,
1.,0.996917333733128,1.,0.997273213004634,0.999370410621552))
REPRESENTATION_ITEM('')
);
#4172=(
BOUNDED_CURVE()
B_SPLINE_CURVE(2,(#271452,#271453,#271454,#271455,#271456,#271457,#271458,
#271459,#271460,#271461,#271462,#271463,#271464,#271465,#271466,#271467,
#271468,#271469,#271470,#271471,#271472,#271473,#271474,#271475,#271476,
#271477,#271478,#271479,#271480,#271481,#271482,#271483,#271484,#271485,
#271486,#271487,#271488,#271489,#271490,#271491,#271492,#271493,#271494,
#271495,#271496,#271497,#271498,#271499,#271500,#271501,#271502,#271503,
#271504,#271505,#271506,#271507,#271508,#271509,#271510,#271511,#271512,
#271513,#271514,#271515,#271516,#271517,#271518,#271519,#271520,#271521,
#271522,#271523,#271524,#271525,#271526,#271527,#271528,#271529,#271530,
#271531,#271532),.UNSPECIFIED.,.F.,.F.)
B_SPLINE_CURVE_WITH_KNOTS((3,2,2,2,2,2,2,2,2,2,2,2,2,2,2,2,2,2,2,2,2,2,
2,2,2,2,2,2,2,2,2,2,2,2,2,2,2,2,2,2,3),(0.00288613200956948,0.025,0.05,
0.075,0.1,0.125,0.15,0.175,0.2,0.225,0.25,0.275,0.3,0.325,0.35,0.375,0.4,
0.425,0.45,0.475,0.5,0.525,0.55,0.575,0.6,0.625,0.65,0.675,0.7,0.725,0.75,
0.775,0.8,0.825,0.85,0.875,0.9,0.925,0.95,0.975,0.98954155634899),
 .UNSPECIFIED.)
CURVE()
GEOMETRIC_REPRESENTATION_ITEM()
RATIONAL_B_SPLINE_CURVE((0.999370410621552,0.997273213004634,1.,0.996917333733128,
1.,0.996917333733128,1.,0.996917333733128,1.,0.996917333733128,1.,0.996917333733128,
1.,0.996917333733128,1.,0.996917333733128,1.,0.996917333733128,1.,0.996917333733128,
1.,0.996917333733128,1.,0.996917333733128,1.,0.996917333733128,1.,0.996917333733128,
1.,0.996917333733128,1.,0.996917333733128,1.,0.996917333733128,1.,0.996917333733128,
1.,0.996917333733128,1.,0.996917333733128,1.,0.996917333733128,1.,0.996917333733128,
1.,0.996917333733128,1.,0.996917333733128,1.,0.996917333733128,1.,0.996917333733128,
1.,0.996917333733128,1.,0.996917333733128,1.,0.996917333733128,1.,0.996917333733128,
1.,0.996917333733128,1.,0.996917333733128,1.,0.996917333733128,1.,0.996917333733128,
1.,0.996917333733128,1.,0.996917333733128,1.,0.996917333733128,1.,0.996917333733128,
1.,0.996917333733128,1.,0.998206929391006,0.998499781765884))
REPRESENTATION_ITEM('')
);
#4173=B_SPLINE_CURVE_WITH_KNOTS('',3,(#142867,#142868,#142869,#142870,#142871,
#142872,#142873,#142874,#142875,#142876,#142877,#142878,#142879,#142880,
#142881,#142882,#142883,#142884),.UNSPECIFIED.,.F.,.F.,(4,2,2,2,2,2,2,2,
4),(-1.58055055147889,-1.3828040290386,-1.18505750659832,-0.987666391168882,
-0.790275275739446,-0.59288416031001,-0.395493044880575,-0.197746522440287,
0.),.UNSPECIFIED.);
#4174=B_SPLINE_CURVE_WITH_KNOTS('',3,(#142888,#142889,#142890,#142891,#142892,
#142893,#142894,#142895,#142896,#142897,#142898,#142899,#142900,#142901,
#142902,#142903,#142904,#142905),.UNSPECIFIED.,.F.,.F.,(4,2,2,2,2,2,2,2,
4),(0.,0.200360130478694,0.400720260957388,0.600044505959735,0.799368750962083,
0.99869299596443,1.19801724096678,1.39837737144547,1.59873750192417),
 .UNSPECIFIED.);
#4175=B_SPLINE_CURVE_WITH_KNOTS('',3,(#142906,#142907,#142908,#142909,#142910,
#142911,#142912,#142913,#142914,#142915,#142916,#142917,#142918,#142919,
#142920,#142921,#142922,#142923),.UNSPECIFIED.,.F.,.F.,(4,2,2,2,2,2,2,2,
4),(-1.59873750192417,-1.39837737144547,-1.19801724096678,-0.99869299596443,
-0.799368750962083,-0.600044505959736,-0.400720260957388,-0.200360130478694,
0.),.UNSPECIFIED.);
#4176=B_SPLINE_CURVE_WITH_KNOTS('',3,(#142924,#142925,#142926,#142927,#142928,
#142929,#142930,#142931,#142932,#142933,#142934,#142935,#142936,#142937,
#142938,#142939,#142940,#142941),.UNSPECIFIED.,.F.,.F.,(4,2,2,2,2,2,2,2,
4),(0.,0.197746522440287,0.395493044880574,0.59288416031001,0.790275275739446,
0.987666391168882,1.18505750659832,1.3828040290386,1.58055055147889),
 .UNSPECIFIED.);
#4177=B_SPLINE_CURVE_WITH_KNOTS('',3,(#142945,#142946,#142947,#142948,#142949,
#142950,#142951,#142952,#142953,#142954,#142955,#142956,#142957,#142958,
#142959,#142960,#142961,#142962),.UNSPECIFIED.,.F.,.F.,(4,2,2,2,2,2,2,2,
4),(1.59873750192417,1.79909763240286,1.99945776288156,2.1987820078839,
2.39810625288625,2.5974304978886,2.79675474289095,2.99711487336964,3.19747500384833),
 .UNSPECIFIED.);
#4178=B_SPLINE_CURVE_WITH_KNOTS('',3,(#142966,#142967,#142968,#142969,#142970,
#142971,#142972,#142973,#142974,#142975,#142976,#142977,#142978,#142979,
#142980,#142981,#142982,#142983),.UNSPECIFIED.,.F.,.F.,(4,2,2,2,2,2,2,2,
4),(3.16110110295778,3.35884762539807,3.55659414783836,3.75398526326779,
3.95137637869723,4.14876749412666,4.3461586095561,4.54390513199639,4.74165165443667),
 .UNSPECIFIED.);
#4179=B_SPLINE_CURVE_WITH_KNOTS('',3,(#142984,#142985,#142986,#142987,#142988,
#142989,#142990,#142991,#142992,#142993,#142994,#142995,#142996,#142997,
#142998,#142999,#143000,#143001),.UNSPECIFIED.,.F.,.F.,(4,2,2,2,2,2,2,2,
4),(1.58055055147889,1.77829707391918,1.97604359635947,2.1734347117889,
2.37082582721834,2.56821694264777,2.76560805807721,2.9633545805175,3.16110110295778),
 .UNSPECIFIED.);
#4180=B_SPLINE_CURVE_WITH_KNOTS('',3,(#143002,#143003,#143004,#143005,#143006,
#143007,#143008,#143009,#143010,#143011,#143012,#143013,#143014,#143015,
#143016,#143017,#143018,#143019),.UNSPECIFIED.,.F.,.F.,(4,2,2,2,2,2,2,2,
4),(3.19747500384833,3.39783513432703,3.59819526480572,3.79751950980807,
3.99684375481042,4.19616799981276,4.39549224481511,4.59585237529381,4.7962125057725),
 .UNSPECIFIED.);
#4181=B_SPLINE_CURVE_WITH_KNOTS('',3,(#143023,#143024,#143025,#143026,#143027,
#143028,#143029,#143030,#143031,#143032,#143033,#143034,#143035,#143036,
#143037,#143038,#143039,#143040,#143041),.UNSPECIFIED.,.F.,.F.,(4,2,2,2,
3,2,2,2,4),(-0.790275275739451,-0.592884160310013,-0.395493044880575,-0.197746522440287,
0.,0.197746522440287,0.395493044880575,0.592884160310013,0.790275275739451),
 .UNSPECIFIED.);
#4182=B_SPLINE_CURVE_WITH_KNOTS('',3,(#143045,#143046,#143047,#143048,#143049,
#143050,#143051,#143052,#143053,#143054,#143055,#143056,#143057,#143058,
#143059,#143060,#143061,#143062,#143063),.UNSPECIFIED.,.F.,.F.,(4,2,2,2,
3,2,2,2,4),(-0.799368750962089,-0.600044505959739,-0.400720260957389,-0.200360130478695,
0.,0.200360130478694,0.400720260957389,0.600044505959739,0.799368750962089),
 .UNSPECIFIED.);
#4183=B_SPLINE_CURVE_WITH_KNOTS('',3,(#143064,#143065,#143066,#143067,#143068,
#143069,#143070,#143071,#143072,#143073,#143074,#143075,#143076,#143077,
#143078,#143079,#143080,#143081),.UNSPECIFIED.,.F.,.F.,(4,2,2,2,2,2,2,2,
4),(-2.39810625288627,-2.19878200788392,-1.99945776288157,-1.79909763240287,
-1.59873750192418,-1.39837737144548,-1.19801724096679,-0.998692995964438,
-0.799368750962089),.UNSPECIFIED.);
#4184=B_SPLINE_CURVE_WITH_KNOTS('',3,(#143082,#143083,#143084,#143085,#143086,
#143087,#143088,#143089,#143090,#143091,#143092,#143093,#143094,#143095,
#143096,#143097,#143098,#143099),.UNSPECIFIED.,.F.,.F.,(4,2,2,2,2,2,2,2,
4),(0.790275275739451,0.987666391168889,1.18505750659833,1.38280402903861,
1.5805505514789,1.77829707391919,1.97604359635948,2.17343471178891,2.37082582721835),
 .UNSPECIFIED.);
#4185=B_SPLINE_CURVE_WITH_KNOTS('',3,(#143103,#143104,#143105,#143106,#143107,
#143108,#143109,#143110,#143111,#143112,#143113,#143114,#143115,#143116,
#143117,#143118,#143119,#143120,#143121),.UNSPECIFIED.,.F.,.F.,(4,2,2,2,
3,2,2,2,4),(2.39810625288627,2.59743049788862,2.79675474289097,2.99711487336966,
3.19747500384836,3.39783513432705,3.59819526480574,3.79751950980809,3.99684375481044),
 .UNSPECIFIED.);
#4186=B_SPLINE_CURVE_WITH_KNOTS('',3,(#143125,#143126,#143127,#143128,#143129,
#143130,#143131,#143132,#143133,#143134,#143135,#143136,#143137,#143138,
#143139,#143140,#143141,#143142,#143143),.UNSPECIFIED.,.F.,.F.,(4,2,2,2,
3,2,2,2,4),(2.37082582721835,2.56821694264779,2.76560805807723,2.96335458051752,
3.1611011029578,3.35884762539809,3.55659414783838,3.75398526326782,3.95137637869726),
 .UNSPECIFIED.);
#4187=B_SPLINE_CURVE_WITH_KNOTS('',3,(#143144,#143145,#143146,#143147,#143148,
#143149,#143150,#143151,#143152,#143153,#143154,#143155,#143156,#143157,
#143158,#143159,#143160,#143161),.UNSPECIFIED.,.F.,.F.,(4,2,2,2,2,2,2,2,
4),(0.790275275739451,0.987666391168889,1.18505750659833,1.38280402903861,
1.5805505514789,1.77829707391919,1.97604359635948,2.17343471178892,2.37082582721835),
 .UNSPECIFIED.);
#4188=B_SPLINE_CURVE_WITH_KNOTS('',3,(#143162,#143163,#143164,#143165,#143166,
#143167,#143168,#143169,#143170,#143171,#143172,#143173,#143174,#143175,
#143176,#143177,#143178,#143179),.UNSPECIFIED.,.F.,.F.,(4,2,2,2,2,2,2,2,
4),(3.99684375481044,4.19616799981279,4.39549224481514,4.59585237529384,
4.79621250577253,4.99657263625123,5.19693276672992,5.39625701173227,5.59558125673462),
 .UNSPECIFIED.);
#4189=B_SPLINE_CURVE_WITH_KNOTS('',3,(#144268,#144269,#144270,#144271,#144272,
#144273,#144274,#144275,#144276,#144277,#144278,#144279,#144280,#144281,
#144282,#144283,#144284,#144285,#144286,#144287,#144288,#144289,#144290,
#144291,#144292,#144293),.UNSPECIFIED.,.F.,.F.,(4,2,2,2,2,2,2,2,2,2,2,2,
4),(-13.8814766639242,-12.963099391817,-11.6984193910095,-10.4333774964113,
-9.16809598401541,-7.90278570433247,-6.63757145246671,-5.37278587819109,
-4.10915141819608,-2.84701293295869,-1.58416264486531,-0.792436008190626,
0.),.UNSPECIFIED.);
#4190=B_SPLINE_CURVE_WITH_KNOTS('',3,(#144299,#144300,#144301,#144302,#144303,
#144304,#144305,#144306,#144307,#144308,#144309,#144310,#144311,#144312,
#144313,#144314,#144315,#144316),.UNSPECIFIED.,.F.,.F.,(4,2,2,2,2,2,2,2,
4),(0.784365106334379,0.980404435697066,1.17644376505975,1.37258698886426,
1.56873021266876,1.76487343647326,1.96101666027776,2.15705598964045,2.35309531900314),
 .UNSPECIFIED.);
#4191=B_SPLINE_CURVE_WITH_KNOTS('',3,(#144319,#144320,#144321,#144322,#144323,
#144324,#144325,#144326,#144327,#144328,#144329,#144330,#144331,#144332,
#144333,#144334,#144335,#144336),.UNSPECIFIED.,.F.,.F.,(4,2,2,2,2,2,2,2,
4),(1.56873021266875,1.76487343647325,1.96101666027775,2.15705598964044,
2.35309531900312,2.54913464836581,2.74517397772849,2.94131720153299,3.1374604253375),
 .UNSPECIFIED.);
#4192=B_SPLINE_CURVE_WITH_KNOTS('',3,(#144337,#144338,#144339,#144340,#144341,
#144342,#144343,#144344,#144345,#144346,#144347,#144348,#144349,#144350,
#144351,#144352,#144353,#144354),.UNSPECIFIED.,.F.,.F.,(4,2,2,2,2,2,2,2,
4),(3.1374604253375,3.333603649142,3.5297468729465,3.72578620230918,3.92182553167187,
4.11786486103455,4.31390419039724,4.51004741420174,4.70619063800624),
 .UNSPECIFIED.);
#4193=B_SPLINE_CURVE_WITH_KNOTS('',3,(#144357,#144358,#144359,#144360,#144361,
#144362,#144363,#144364,#144365,#144366,#144367,#144368,#144369,#144370,
#144371,#144372,#144373,#144374),.UNSPECIFIED.,.F.,.F.,(4,2,2,2,2,2,2,2,
4),(-1.56873021266875,-1.37258698886425,-1.17644376505974,-0.980404435697059,
-0.784365106334374,-0.588325776971689,-0.392286447609003,-0.196143223804502,
0.),.UNSPECIFIED.);
#4194=B_SPLINE_CURVE_WITH_KNOTS('',3,(#144375,#144376,#144377,#144378,#144379,
#144380,#144381,#144382,#144383,#144384,#144385,#144386,#144387,#144388,
#144389,#144390,#144391,#144392),.UNSPECIFIED.,.F.,.F.,(4,2,2,2,2,2,2,2,
4),(0.,0.196143223804502,0.392286447609004,0.588325776971689,0.784365106334374,
0.980404435697059,1.17644376505974,1.37258698886425,1.56873021266875),
 .UNSPECIFIED.);
#4195=B_SPLINE_CURVE_WITH_KNOTS('',3,(#144397,#144398,#144399,#144400,#144401,
#144402,#144403,#144404,#144405,#144406,#144407,#144408,#144409,#144410,
#144411,#144412,#144413,#144414,#144415,#144416,#144417,#144418,#144419,
#144420,#144421,#144422),.UNSPECIFIED.,.F.,.F.,(4,2,2,2,2,2,2,2,2,2,2,2,
4),(-27.7692554578402,-26.8737799915245,-25.608769554275,-24.3432221416514,
-23.0773813467393,-21.8113780103894,-20.5453898616053,-19.2795959206261,
-18.014467770055,-16.7509292170372,-15.4895459533869,-14.2270583969213,
-13.8814766639242),.UNSPECIFIED.);
#4196=B_SPLINE_CURVE_WITH_KNOTS('',3,(#144423,#144424,#144425,#144426,#144427,
#144428,#144429,#144430,#144431,#144432,#144433,#144434,#144435,#144436,
#144437,#144438,#144439,#144440,#144441),.UNSPECIFIED.,.F.,.F.,(4,2,2,2,
3,2,2,2,4),(2.35309531900314,2.54913464836582,2.74517397772851,2.94131720153301,
3.13746042533751,3.33360364914202,3.52974687294652,3.72578620230921,3.92182553167189),
 .UNSPECIFIED.);
#4197=B_SPLINE_CURVE_WITH_KNOTS('',3,(#144442,#144443,#144444,#144445,#144446,
#144447,#144448,#144449,#144450,#144451,#144452,#144453,#144454,#144455,
#144456,#144457,#144458,#144459,#144460,#144461,#144462,#144463,#144464,
#144465,#144466,#144467),.UNSPECIFIED.,.F.,.F.,(4,2,2,2,2,2,2,2,2,2,2,2,
4),(-104.015874542983,-103.240957296345,-102.466440663735,-101.207072089471,
-99.9489235979378,-98.6882843547007,-97.425630439723,-96.1620642931025,
-94.8981892506107,-93.6342617969183,-92.3704234079043,-91.1068430913151,
-90.1604031166725),.UNSPECIFIED.);
#4198=B_SPLINE_CURVE_WITH_KNOTS('',3,(#144470,#144471,#144472,#144473,#144474,
#144475,#144476,#144477,#144478,#144479,#144480,#144481,#144482,#144483,
#144484,#144485,#144486,#144487,#144488),.UNSPECIFIED.,.F.,.F.,(4,2,2,2,
3,2,2,2,4),(-0.784365106334379,-0.588325776971691,-0.392286447609004,-0.196143223804502,
0.,0.196143223804502,0.392286447609004,0.588325776971692,0.784365106334379),
 .UNSPECIFIED.);
#4199=B_SPLINE_CURVE_WITH_KNOTS('',3,(#144489,#144490,#144491,#144492,#144493,
#144494,#144495,#144496,#144497,#144498,#144499,#144500,#144501,#144502,
#144503,#144504,#144505,#144506),.UNSPECIFIED.,.F.,.F.,(4,2,2,2,2,2,2,2,
4),(0.784365106334379,0.980404435697066,1.17644376505975,1.37258698886426,
1.56873021266876,1.76487343647326,1.96101666027776,2.15705598964045,2.35309531900314),
 .UNSPECIFIED.);
#4200=B_SPLINE_CURVE_WITH_KNOTS('',3,(#144511,#144512,#144513,#144514,#144515,
#144516,#144517,#144518,#144519,#144520,#144521,#144522,#144523,#144524,
#144525,#144526,#144527,#144528,#144529,#144530,#144531,#144532,#144533,
#144534,#144535,#144536),.UNSPECIFIED.,.F.,.F.,(4,2,2,2,2,2,2,2,2,2,2,2,
4),(-41.6372629980801,-40.7664022234293,-39.5041738810512,-38.2411203720136,
-36.9776617236179,-35.7139513451538,-34.4501697796324,-33.1864522471623,
-31.9230767454262,-30.6606810056365,-29.3994174888209,-28.1376783293277,
-27.7692554578402),.UNSPECIFIED.);
#4201=B_SPLINE_CURVE_WITH_KNOTS('',3,(#144537,#144538,#144539,#144540,#144541,
#144542,#144543,#144544,#144545,#144546,#144547,#144548,#144549,#144550,
#144551,#144552,#144553,#144554,#144555,#144556,#144557,#144558,#144559,
#144560,#144561,#144562),.UNSPECIFIED.,.F.,.F.,(4,2,2,2,2,2,2,2,2,2,2,2,
4),(-90.1604031166725,-89.8436895134744,-88.5814107402185,-87.3208827048715,
-86.0612546066959,-84.7998510025023,-83.537157629253,-82.2739624099999,
-81.0106422304456,-79.7473270963416,-78.4842338503542,-77.2214744103415,
-76.2990316115284),.UNSPECIFIED.);
#4202=B_SPLINE_CURVE_WITH_KNOTS('',3,(#144567,#144568,#144569,#144570,#144571,
#144572,#144573,#144574,#144575,#144576,#144577,#144578,#144579,#144580,
#144581,#144582,#144583,#144584,#144585,#144586,#144587,#144588,#144589,
#144590,#144591,#144592),.UNSPECIFIED.,.F.,.F.,(4,2,2,2,2,2,2,2,2,2,2,2,
4),(-55.4993512071467,-54.6513921073566,-53.3902342683282,-52.1278116316948,
-50.8647759569511,-49.6014201273275,-48.3378604563596,-47.0743011025923,
-45.8108853500451,-44.5480169787744,-43.2865230918552,-42.0269684623869,
-41.6372629980801),.UNSPECIFIED.);
#4203=B_SPLINE_CURVE_WITH_KNOTS('',3,(#144593,#144594,#144595,#144596,#144597,
#144598,#144599,#144600,#144601,#144602,#144603,#144604,#144605,#144606,
#144607,#144608,#144609,#144610,#144611,#144612,#144613,#144614,#144615,
#144616,#144617,#144618),.UNSPECIFIED.,.F.,.F.,(4,2,2,2,2,2,2,2,2,2,2,2,
4),(-76.2990316115284,-75.9593645087416,-74.6985903757287,-73.4389646676771,
-72.177047042093,-70.9133659385421,-69.6489198280436,-68.3842346083183,
-67.1195201876227,-65.85493675867,-64.5906295488055,-63.3268076944692,-62.4266886913099),
 .UNSPECIFIED.);
#4204=B_SPLINE_CURVE_WITH_KNOTS('',3,(#144623,#144624,#144625,#144626,#144627,
#144628,#144629,#144630,#144631,#144632,#144633,#144634,#144635,#144636,
#144637,#144638,#144639,#144640,#144641,#144642,#144643,#144644,#144645,
#144646,#144647,#144648),.UNSPECIFIED.,.F.,.F.,(4,2,2,2,2,2,2,2,2,2,2,2,
4),(-69.3801191133633,-68.5536951873574,-67.292001693102,-66.0284301208769,
-64.7639112991888,-63.4989332139754,-62.2336870563708,-60.9683277594848,
-59.7030069572755,-58.4379539740317,-57.1737276963798,-55.9113714686727,
-55.4993512071467),.UNSPECIFIED.);
#4205=B_SPLINE_CURVE_WITH_KNOTS('',3,(#144649,#144650,#144651,#144652,#144653,
#144654,#144655,#144656,#144657,#144658,#144659,#144660,#144661,#144662,
#144663,#144664,#144665,#144666,#144667,#144668,#144669,#144670,#144671,
#144672,#144673,#144674),.UNSPECIFIED.,.F.,.F.,(4,2,2,2,2,2,2,2,2,2,2,2,
4),(-62.4266886913099,-62.0639896504061,-60.8031471476672,-59.5429544790536,
-58.281360404511,-57.0186615159492,-55.7555575129026,-54.4923663240911,
-53.2292146600348,-51.9663050678705,-50.7032610542343,-49.4407596448874,
-48.5661368651097),.UNSPECIFIED.);
#4206=B_SPLINE_CURVE_WITH_KNOTS('',3,(#144679,#144680,#144681,#144682,#144683,
#144684,#144685,#144686,#144687,#144688,#144689,#144690,#144691,#144692,
#144693,#144694,#144695,#144696,#144697,#144698,#144699,#144700,#144701,
#144702,#144703,#144704),.UNSPECIFIED.,.F.,.F.,(4,2,2,2,2,2,2,2,2,2,2,2,
4),(-83.2500328628607,-82.4481533960685,-81.1876171552324,-79.9253065699082,
-78.6617065326316,-77.3976049520614,-76.1333785891597,-74.8691703087574,
-73.6049410691841,-72.3408142660145,-71.0771325954068,-69.8146334354338,
-69.3801191133633),.UNSPECIFIED.);
#4207=B_SPLINE_CURVE_WITH_KNOTS('',3,(#144705,#144706,#144707,#144708,#144709,
#144710,#144711,#144712,#144713,#144714,#144715,#144716,#144717,#144718,
#144719,#144720,#144721,#144722,#144723,#144724,#144725,#144726,#144727,
#144728,#144729,#144730),.UNSPECIFIED.,.F.,.F.,(4,2,2,2,2,2,2,2,2,2,2,2,
4),(-48.5661368651097,-48.1796237958336,-46.9204103396194,-45.6601967379575,
-44.3983128950498,-43.1355993319228,-41.8724786857766,-40.6091057824071,
-39.3456599380502,-38.082276908884,-36.8192324431946,-35.5571606562185,
-34.7056572650582),.UNSPECIFIED.);
#4208=B_SPLINE_CURVE_WITH_KNOTS('',3,(#144735,#144736,#144737,#144738,#144739,
#144740,#144741,#144742,#144743,#144744,#144745,#144746,#144747,#144748,
#144749,#144750,#144751,#144752,#144753,#144754,#144755,#144756,#144757,
#144758,#144759,#144760),.UNSPECIFIED.,.F.,.F.,(4,2,2,2,2,2,2,2,2,2,2,2,
4),(-97.1232537091924,-96.3443719127046,-95.0853105232451,-93.8237579151547,
-92.5601908545606,-91.295711898233,-90.0309243056691,-88.7660844304284,
-87.5013339520407,-86.2368418327317,-84.9727770982929,-83.7095885668981,
-83.2500328628607),.UNSPECIFIED.);
#4209=B_SPLINE_CURVE_WITH_KNOTS('',3,(#144761,#144762,#144763,#144764,#144765,
#144766,#144767,#144768,#144769,#144770,#144771,#144772,#144773,#144774,
#144775,#144776,#144777,#144778,#144779,#144780,#144781,#144782,#144783,
#144784,#144785,#144786),.UNSPECIFIED.,.F.,.F.,(4,2,2,2,2,2,2,2,2,2,2,2,
4),(-34.7056572650582,-34.2962056922594,-33.0347847958924,-31.771194527919,
-30.5064860259869,-29.2412375641598,-27.9756947285637,-26.7099875939099,
-25.4442949200012,-24.1787940187062,-22.9139533339695,-21.6506922260116,
-20.8210363596471),.UNSPECIFIED.);
#4210=B_SPLINE_CURVE_WITH_KNOTS('',3,(#144791,#144792,#144793,#144794,#144795,
#144796,#144797,#144798,#144799,#144800,#144801,#144802,#144803,#144804,
#144805,#144806,#144807,#144808,#144809,#144810,#144811,#144812,#144813,
#144814,#144815,#144816),.UNSPECIFIED.,.F.,.F.,(4,2,2,2,2,2,2,2,2,2,2,2,
4),(-110.967977009243,-109.972570106527,-108.957916406404,-107.699758598375,
-106.439527248507,-105.177806722715,-103.915475803826,-102.652974563524,
-101.390465164933,-100.128136116833,-98.8661109187615,-97.6046537650016,
-97.1232537091924),.UNSPECIFIED.);
#4211=B_SPLINE_CURVE_WITH_KNOTS('',3,(#144817,#144818,#144819,#144820,#144821,
#144822,#144823,#144824,#144825,#144826,#144827,#144828,#144829,#144830,
#144831,#144832,#144833,#144834,#144835,#144836,#144837,#144838,#144839,
#144840,#144841,#144842),.UNSPECIFIED.,.F.,.F.,(4,2,2,2,2,2,2,2,2,2,2,2,
4),(-20.8210363596471,-20.3895782821617,-19.1273626285183,-17.863667873144,
-16.5992480081042,-15.3344646086074,-14.0694411584903,-12.8043870765627,
-11.5394274728486,-10.2748924628399,-9.01150060417685,-7.74958849211455,
-6.94140314827258),.UNSPECIFIED.);
#4212=B_SPLINE_CURVE_WITH_KNOTS('',3,(#144848,#144849,#144850,#144851,#144852,
#144853,#144854,#144855,#144856,#144857,#144858,#144859,#144860,#144861,
#144862,#144863,#144864,#144865,#144866,#144867,#144868,#144869,#144870,
#144871,#144872,#144873),.UNSPECIFIED.,.F.,.F.,(4,2,2,2,2,2,2,2,2,2,2,2,
4),(192.908593634536,193.053216493834,194.838241605474,196.624309799068,
198.409265218689,200.19376370034,201.978838598696,203.764512861769,205.549513185926,
207.334220267435,209.119842173418,210.904778060657,212.697004771953),
 .UNSPECIFIED.);
#4213=B_SPLINE_CURVE_WITH_KNOTS('',3,(#144876,#144877,#144878,#144879,#144880,
#144881,#144882,#144883,#144884,#144885,#144886,#144887,#144888,#144889,
#144890,#144891,#144892,#144893,#144894,#144895,#144896,#144897,#144898,
#144899),.UNSPECIFIED.,.F.,.F.,(4,2,2,2,2,2,2,2,2,2,2,4),(9.99999989108212E-7,
1.6769694808229,3.35394573760072,5.14001215222226,6.92611120726754,8.71152346455622,
10.4972993356259,12.2838558739946,14.0693244115025,15.8542458178252,17.6397062809234,
18.9650896985654),.UNSPECIFIED.);
#4214=B_SPLINE_CURVE_WITH_KNOTS('',3,(#144904,#144905,#144906,#144907,#144908,
#144909,#144910,#144911,#144912,#144913,#144914,#144915,#144916,#144917,
#144918,#144919,#144920,#144921,#144922,#144923,#144924,#144925,#144926,
#144927,#144928,#144929,#144930,#144931,#144932,#144933,#144934,#144935),
 .UNSPECIFIED.,.F.,.F.,(4,2,2,2,2,2,2,2,2,2,2,2,2,2,2,4),(166.298715258511,
168.062704889159,169.846980296724,171.632329207268,173.416900833311,175.201110861311,
176.986013726065,178.770866342029,180.555131335309,182.339939547942,184.126158497811,
185.911539890777,187.696514469877,189.482090107986,191.267970458966,192.908593634536),
 .UNSPECIFIED.);
#4215=B_SPLINE_CURVE_WITH_KNOTS('',3,(#144936,#144937,#144938,#144939,#144940,
#144941,#144942,#144943,#144944,#144945,#144946,#144947,#144948,#144949,
#144950,#144951,#144952,#144953,#144954,#144955,#144956,#144957,#144958,
#144959,#144960,#144961,#144962,#144963,#144964,#144965,#144966,#144967,
#144968,#144969),.UNSPECIFIED.,.F.,.F.,(4,2,2,2,2,2,2,2,2,2,2,2,2,2,2,2,
4),(18.9650896985654,19.425618542153,21.2106941659649,22.996095123781,24.7822019761817,
26.5675394095681,28.3523130129014,30.137572813644,31.9237070575206,33.7088671994476,
35.4942868404638,37.2803639611839,39.0659738961904,40.850996381668,42.6364531786856,
44.4232157048341,45.5834444085454),.UNSPECIFIED.);
#4216=B_SPLINE_CURVE_WITH_KNOTS('',3,(#144974,#144975,#144976,#144977,#144978,
#144979,#144980,#144981,#144982,#144983,#144984,#144985,#144986,#144987,
#144988,#144989,#144990,#144991,#144992,#144993,#144994,#144995,#144996,
#144997,#144998,#144999,#145000,#145001,#145002,#145003,#145004,#145005,
#145006,#145007),.UNSPECIFIED.,.F.,.F.,(4,2,2,2,2,2,2,2,2,2,2,2,2,2,2,2,
4),(139.698460362937,141.298680190492,143.082542874683,144.866993668424,
146.651898927764,148.436148802202,150.220142419869,152.00511492784,153.789195633697,
155.572792685623,157.35695409508,159.141871394973,160.926086686371,162.709978269322,
164.494712074918,166.278976729113,166.298715258511),.UNSPECIFIED.);
#4217=B_SPLINE_CURVE_WITH_KNOTS('',3,(#145008,#145009,#145010,#145011,#145012,
#145013,#145014,#145015,#145016,#145017,#145018,#145019,#145020,#145021,
#145022,#145023,#145024,#145025,#145026,#145027,#145028,#145029,#145030,
#145031,#145032,#145033,#145034,#145035,#145036,#145037,#145038,#145039,
#145040,#145041),.UNSPECIFIED.,.F.,.F.,(4,2,2,2,2,2,2,2,2,2,2,2,2,2,2,2,
4),(45.5834444085454,46.2088841699579,47.9947463716619,49.7812231812246,
51.5675223476345,53.3532100307112,55.1392838945247,56.9261710618272,58.7117996117417,
60.496884827521,62.2825356237994,64.0684233445439,65.853549939962,67.6390203919217,
69.4252366706261,71.2113397224562,72.2052309313631),.UNSPECIFIED.);
#4218=B_SPLINE_CURVE_WITH_KNOTS('',3,(#145046,#145047,#145048,#145049,#145050,
#145051,#145052,#145053,#145054,#145055,#145056,#145057,#145058,#145059,
#145060,#145061,#145062,#145063,#145064,#145065,#145066,#145067,#145068,
#145069,#145070,#145071,#145072,#145073,#145074,#145075,#145076,#145077,
#145078,#145079),.UNSPECIFIED.,.F.,.F.,(4,2,2,2,2,2,2,2,2,2,2,2,2,2,2,2,
4),(113.09235101392,114.52775166222,116.312097574426,118.096101456626,119.880872306608,
121.665388745755,123.449342109569,125.23383862757,127.019578752594,128.804508600531,
130.589054425226,132.374213279577,134.15953667438,135.944247806099,137.728767737168,
139.514385601497,139.698460362937),.UNSPECIFIED.);
#4219=B_SPLINE_CURVE_WITH_KNOTS('',3,(#145080,#145081,#145082,#145083,#145084,
#145085,#145086,#145087,#145088,#145089,#145090,#145091,#145092,#145093,
#145094,#145095,#145096,#145097,#145098,#145099,#145100,#145101,#145102,
#145103,#145104,#145105,#145106,#145107,#145108,#145109,#145110,#145111,
#145112,#145113),.UNSPECIFIED.,.F.,.F.,(4,2,2,2,2,2,2,2,2,2,2,2,2,2,2,2,
4),(72.2052309313631,72.9965317100158,74.7812420564402,76.5665180619611,
78.3525368904608,80.1378568580769,81.9228543667527,83.7087009217182,85.49405960617,
87.2788837652769,89.0642560350252,90.8506881535951,92.6363455201069,94.421642900023,
96.2076402994364,97.9935690491882,98.8223876750889),.UNSPECIFIED.);
#4220=B_SPLINE_CURVE_WITH_KNOTS('',3,(#145118,#145119,#145120,#145121,#145122,
#145123,#145124,#145125,#145126,#145127,#145128,#145129,#145130,#145131,
#145132,#145133,#145134,#145135,#145136,#145137,#145138,#145139,#145140,
#145141,#145142,#145143,#145144,#145145,#145146,#145147,#145148,#145149,
#145150,#145151),.UNSPECIFIED.,.F.,.F.,(4,2,2,2,2,2,2,2,2,2,2,2,2,2,2,2,
4),(86.4916057697223,87.7620179914404,89.5470742844118,91.3314954032844,
93.1156939706259,94.9009319839527,96.6850691658659,98.4687482426107,100.253002836542,
102.037864510603,103.822051617035,105.605943517478,107.390746196952,109.174874371702,
110.958491782147,112.74266354629,113.09235101392),.UNSPECIFIED.);
#4221=B_SPLINE_CURVE_WITH_KNOTS('',3,(#145152,#145153,#145154,#145155,#145156,
#145157,#145158,#145159,#145160,#145161,#145162,#145163,#145164,#145165,
#145166,#145167,#145168,#145169,#145170,#145171,#145172,#145173,#145174,
#145175,#145176,#145177,#145178,#145179,#145180,#145181,#145182,#145183,
#145184,#145185),.UNSPECIFIED.,.F.,.F.,(4,2,2,2,2,2,2,2,2,2,2,2,2,2,2,2,
4),(98.8223876750889,99.778911980072,101.564798285203,103.352080954802,
105.138527824139,106.924569725461,108.711214082261,110.498150768372,112.284454663544,
114.070540322883,115.857674832274,117.643677117955,119.429224455379,121.215349595913,
123.002061348891,124.78810032242,125.451829625253),.UNSPECIFIED.);
#4222=B_SPLINE_CURVE_WITH_KNOTS('',3,(#145190,#145191,#145192,#145193,#145194,
#145195,#145196,#145197,#145198,#145199,#145200,#145201,#145202,#145203,
#145204,#145205,#145206,#145207,#145208,#145209,#145210,#145211,#145212,
#145213,#145214,#145215,#145216,#145217,#145218,#145219,#145220,#145221,
#145222,#145223),.UNSPECIFIED.,.F.,.F.,(4,2,2,2,2,2,2,2,2,2,2,2,2,2,2,2,
4),(59.8786188341278,60.9848711462809,62.7699607377911,64.5544747957343,
66.3394477240105,68.1255174331873,69.9105484752843,71.695958346319,73.4810053395191,
75.2667414148746,77.0524382847678,78.8375459582976,80.6224879685026,82.408578192017,
84.1931300109447,85.9772739287588,86.4916057697223),.UNSPECIFIED.);
#4223=B_SPLINE_CURVE_WITH_KNOTS('',3,(#145224,#145225,#145226,#145227,#145228,
#145229,#145230,#145231,#145232,#145233,#145234,#145235,#145236,#145237,
#145238,#145239,#145240,#145241,#145242,#145243,#145244,#145245,#145246,
#145247,#145248,#145249,#145250,#145251,#145252,#145253,#145254,#145255,
#145256,#145257),.UNSPECIFIED.,.F.,.F.,(4,2,2,2,2,2,2,2,2,2,2,2,2,2,2,2,
4),(125.451829625253,126.573849309195,128.360519589848,130.146485042424,
131.931942914064,133.71795694799,135.504866056864,137.29103750207,139.076869212986,
140.863479157537,142.64980507424,144.435570928966,146.221880827012,148.009412023174,
149.796136365143,151.582479454181,152.081568540232),.UNSPECIFIED.);
#4224=B_SPLINE_CURVE_WITH_KNOTS('',3,(#145262,#145263,#145264,#145265,#145266,
#145267,#145268,#145269,#145270,#145271,#145272,#145273,#145274,#145275,
#145276,#145277,#145278,#145279,#145280,#145281,#145282,#145283,#145284,
#145285,#145286,#145287,#145288,#145289,#145290,#145291,#145292,#145293,
#145294,#145295),.UNSPECIFIED.,.F.,.F.,(4,2,2,2,2,2,2,2,2,2,2,2,2,2,2,2,
4),(33.2649250020999,34.2056820368628,35.9922701244673,37.777610445128,
39.5624073988762,41.3477682347804,43.1333791648598,44.9182243539491,46.7034121380009,
48.4893432713056,50.2743542552732,52.0588108074829,53.8437789249438,55.6294173890104,
57.4141460993981,59.1991709946284,59.8786188341278),.UNSPECIFIED.);
#4225=B_SPLINE_CURVE_WITH_KNOTS('',3,(#145296,#145297,#145298,#145299,#145300,
#145301,#145302,#145303,#145304,#145305,#145306,#145307,#145308,#145309,
#145310,#145311,#145312,#145313,#145314,#145315,#145316,#145317,#145318,
#145319,#145320,#145321,#145322,#145323,#145324,#145325,#145326,#145327,
#145328,#145329),.UNSPECIFIED.,.F.,.F.,(4,2,2,2,2,2,2,2,2,2,2,2,2,2,2,2,
4),(152.081568540232,153.369447222936,155.156550264893,156.943043698927,
158.729349687956,160.516762242765,162.3028195186,164.088447986099,165.874666880246,
167.661320055741,169.44732000726,171.233068513856,173.019805839672,174.80562058442,
176.590954903103,178.376855652217,178.710809555564),.UNSPECIFIED.);
#4226=B_SPLINE_CURVE_WITH_KNOTS('',3,(#145334,#145335,#145336,#145337,#145338,
#145339,#145340,#145341,#145342,#145343,#145344,#145345,#145346,#145347,
#145348,#145349,#145350,#145351,#145352,#145353,#145354,#145355,#145356,
#145357,#145358,#145359,#145360,#145361,#145362,#145363,#145364,#145365,
#145366,#145367),.UNSPECIFIED.,.F.,.F.,(4,2,2,2,2,2,2,2,2,2,2,2,2,2,2,2,
4),(6.64837408914975,7.42331429784298,9.20825051621213,10.9940744495241,
12.7789203869486,14.5640234744708,16.3497826803808,18.135084081717,19.9197973552195,
21.7049432734423,23.491408467138,25.2767763535493,27.0623361352787,28.8485089624496,
30.6345131361714,32.4199052440002,33.2649250020999),.UNSPECIFIED.);
#4227=B_SPLINE_CURVE_WITH_KNOTS('',3,(#145368,#145369,#145370,#145371,#145372,
#145373,#145374,#145375,#145376,#145377,#145378,#145379,#145380,#145381,
#145382,#145383,#145384,#145385,#145386,#145387,#145388,#145389,#145390,
#145391,#145392,#145393,#145394,#145395,#145396,#145397,#145398,#145399,
#145400,#145401),.UNSPECIFIED.,.F.,.F.,(4,2,2,2,2,2,2,2,2,2,2,2,2,2,2,2,
4),(178.710809555564,180.163491400479,181.949430198385,183.7350472835,185.521517466646,
187.307488583991,189.092926368585,190.878912779111,192.665950859082,194.452215734871,
196.238121590287,198.024731740104,199.81126223008,201.597207998778,203.383697238931,
205.171574228893,205.339933575319),.UNSPECIFIED.);
#4228=B_SPLINE_CURVE_WITH_KNOTS('',3,(#145406,#145407,#145408,#145409,#145410,
#145411,#145412,#145413,#145414,#145415,#145416,#145417,#145418,#145419,
#145420,#145421,#145422,#145423),.UNSPECIFIED.,.F.,.F.,(4,2,2,2,2,2,2,2,
4),(0.,0.197658290162167,0.395316580324333,0.59263683604877,0.789957091773207,
0.987277347497643,1.18459760322208,1.38225589338425,1.57991418354641),
 .UNSPECIFIED.);
#4229=B_SPLINE_CURVE_WITH_KNOTS('',3,(#145424,#145425,#145426,#145427,#145428,
#145429,#145430,#145431,#145432,#145433,#145434,#145435,#145436,#145437,
#145438,#145439,#145440,#145441),.UNSPECIFIED.,.F.,.F.,(4,2,2,2,2,2,2,2,
4),(-1.57991418354641,-1.38225589338425,-1.18459760322208,-0.987277347497643,
-0.789957091773207,-0.59263683604877,-0.395316580324333,-0.197658290162167,
0.),.UNSPECIFIED.);
#4230=B_SPLINE_CURVE_WITH_KNOTS('',3,(#145445,#145446,#145447,#145448,#145449,
#145450,#145451,#145452,#145453,#145454,#145455,#145456,#145457,#145458,
#145459,#145460,#145461,#145462),.UNSPECIFIED.,.F.,.F.,(4,2,2,2,2,2,2,2,
4),(1.57991418354641,1.77757247370858,1.97523076387075,2.17255101959518,
2.36987127531962,2.56719153104406,2.76451178676849,2.96217007693066,3.15982836709283),
 .UNSPECIFIED.);
#4231=B_SPLINE_CURVE_WITH_KNOTS('',3,(#145464,#145465,#145466,#145467,#145468,
#145469,#145470,#145471,#145472,#145473,#145474,#145475,#145476,#145477,
#145478,#145479,#145480,#145481),.UNSPECIFIED.,.F.,.F.,(4,2,2,2,2,2,2,2,
4),(3.15982836709283,3.357486657255,3.55514494741716,3.7524652031416,3.94978545886604,
4.14710571459047,4.34442597031491,4.54208426047708,4.73974255063924),
 .UNSPECIFIED.);
#4232=B_SPLINE_CURVE_WITH_KNOTS('',3,(#145486,#145487,#145488,#145489,#145490,
#145491,#145492,#145493,#145494,#145495,#145496,#145497,#145498,#145499,
#145500,#145501,#145502,#145503,#145504),.UNSPECIFIED.,.F.,.F.,(4,2,2,2,
3,2,2,2,4),(-0.789957091773212,-0.592636836048773,-0.395316580324334,-0.197658290162167,
0.,0.197658290162167,0.395316580324334,0.592636836048773,0.789957091773212),
 .UNSPECIFIED.);
#4233=B_SPLINE_CURVE_WITH_KNOTS('',3,(#145505,#145506,#145507,#145508,#145509,
#145510,#145511,#145512,#145513,#145514,#145515,#145516,#145517,#145518,
#145519,#145520,#145521,#145522),.UNSPECIFIED.,.F.,.F.,(4,2,2,2,2,2,2,2,
4),(-2.36987127531964,-2.1725510195952,-1.97523076387076,-1.77757247370859,
-1.57991418354642,-1.38225589338426,-1.18459760322209,-0.987277347497651,
-0.789957091773212),.UNSPECIFIED.);
#4234=B_SPLINE_CURVE_WITH_KNOTS('',3,(#145526,#145527,#145528,#145529,#145530,
#145531,#145532,#145533,#145534,#145535,#145536,#145537,#145538,#145539,
#145540,#145541,#145542,#145543,#145544),.UNSPECIFIED.,.F.,.F.,(4,2,2,2,
3,2,2,2,4),(2.36987127531964,2.56719153104407,2.76451178676851,2.96217007693068,
3.15982836709285,3.35748665725501,3.55514494741718,3.75246520314162,3.94978545886606),
 .UNSPECIFIED.);
#4235=B_SPLINE_CURVE_WITH_KNOTS('',3,(#145546,#145547,#145548,#145549,#145550,
#145551,#145552,#145553,#145554,#145555,#145556,#145557,#145558,#145559,
#145560,#145561,#145562,#145563),.UNSPECIFIED.,.F.,.F.,(4,2,2,2,2,2,2,2,
4),(3.94978545886606,4.1471057145905,4.34442597031494,4.5420842604771,4.73974255063927,
4.93740084080144,5.13505913096361,5.33237938668804,5.52969964241248),
 .UNSPECIFIED.);
#4236=B_SPLINE_CURVE_WITH_KNOTS('',3,(#145566,#145567,#145568,#145569,#145570,
#145571,#145572,#145573,#145574,#145575),.UNSPECIFIED.,.F.,.F.,(4,2,2,2,
4),(205.339933575319,206.958616507017,208.745254927296,210.371885430349,
211.997838068529),.UNSPECIFIED.);
#4237=B_SPLINE_CURVE_WITH_KNOTS('',3,(#145578,#145579,#145580,#145581,#145582,
#145583,#145584,#145585,#145586,#145587,#145588,#145589),.UNSPECIFIED.,
 .F.,.F.,(4,2,2,2,2,4),(0.,1.03389160214753,2.06807064969959,3.85384635032225,
5.6388625243884,6.64837408914975),.UNSPECIFIED.);
#4238=B_SPLINE_CURVE_WITH_KNOTS('',3,(#145592,#145593,#145594,#145595,#145596,
#145597,#145598,#145599,#145600,#145601,#145602,#145603,#145604,#145605,
#145606,#145607),.UNSPECIFIED.,.F.,.F.,(4,2,2,2,2,2,2,4),(-6.94140314827258,
-6.4869752748672,-5.22243205186437,-3.95691169732814,-2.69091834975448,
-1.42465254456224,-0.71276813162599,0.),.UNSPECIFIED.);
#4239=B_SPLINE_CURVE_WITH_KNOTS('',3,(#145609,#145610,#145611,#145612,#145613,
#145614,#145615,#145616,#145617,#145618,#145619,#145620,#145621,#145622,
#145623,#145624,#145625,#145626,#145627,#145628,#145629,#145630,#145631,
#145632,#145633,#145634,#145635,#145636,#145637,#145638,#145639,#145640,
#145641,#145642,#145643,#145644,#145645,#145646,#145647,#145648,#145649,
#145650,#145651,#145652,#145653,#145654,#145655,#145656,#145657,#145658,
#145659,#145660,#145661,#145662,#145663,#145664,#145665,#145666,#145667,
#145668,#145669,#145670,#145671,#145672,#145673,#145674,#145675,#145676,
#145677,#145678,#145679,#145680,#145681,#145682,#145683,#145684,#145685,
#145686,#145687,#145688,#145689,#145690,#145691,#145692,#145693,#145694,
#145695,#145696,#145697,#145698,#145699,#145700,#145701,#145702,#145703,
#145704,#145705,#145706,#145707,#145708,#145709,#145710,#145711,#145712,
#145713,#145714,#145715,#145716,#145717,#145718,#145719,#145720,#145721,
#145722,#145723,#145724,#145725,#145726,#145727,#145728,#145729,#145730,
#145731,#145732,#145733,#145734,#145735,#145736,#145737,#145738,#145739,
#145740,#145741,#145742,#145743,#145744,#145745,#145746,#145747,#145748,
#145749,#145750,#145751,#145752,#145753,#145754,#145755,#145756,#145757,
#145758,#145759,#145760,#145761,#145762,#145763,#145764,#145765,#145766,
#145767,#145768,#145769,#145770,#145771,#145772,#145773,#145774,#145775,
#145776,#145777,#145778,#145779,#145780,#145781,#145782,#145783,#145784,
#145785,#145786,#145787,#145788,#145789,#145790,#145791,#145792,#145793,
#145794,#145795,#145796,#145797,#145798,#145799,#145800,#145801),
 .UNSPECIFIED.,.F.,.F.,(4,3,3,3,3,3,3,3,3,3,3,3,3,3,3,3,3,3,3,3,3,3,3,3,
3,3,3,3,3,3,3,3,3,3,3,3,3,3,3,3,3,3,3,3,3,3,3,3,3,3,3,3,3,3,3,3,3,3,3,3,
3,3,3,3,4),(0.25356579115215,0.253868242204076,0.254170595365822,0.254472068163607,
0.254559994575927,0.254862017366658,0.255174497215665,0.255486977064673,
0.25555456294769,0.25584417182401,0.256133884295542,0.256422820807404,0.256548943572741,
0.256837945950334,0.257127769386952,0.257408162977196,0.257543416604553,
0.257823699925624,0.258104255128538,0.258384192910332,0.258537766343908,
0.258817699141702,0.259098358149039,0.259329348889719,0.25953227603482,
0.259805885422422,0.260079864682975,0.260353333221958,0.260526494633499,
0.260800011386373,0.261074159864624,0.261250534802241,0.26152110805456,
0.261790065895994,0.262059439700215,0.262328354529141,0.262515160885892,
0.262784212260444,0.263053826468364,0.263171720714764,0.263438131643026,
0.263509893617797,0.263775819121753,0.264042173628218,0.264308080258592,
0.264503796454098,0.264769929002005,0.26503658597714,0.265092906627287,
0.265357824185491,0.265498626097877,0.265762894912191,0.266027586277107,
0.266291815112806,0.266492429976106,0.266757448196561,0.26701409253981,
0.267278657447202,0.267487309531408,0.267751167693691,0.268015432145765,
0.268279206795948,0.268481085740995,0.268745635122929,0.268935278452333),
 .UNSPECIFIED.);
#4240=B_SPLINE_CURVE_WITH_KNOTS('',3,(#145804,#145805,#145806,#145807),
 .UNSPECIFIED.,.F.,.F.,(4,4),(-110.988356064082,-110.967977009243),
 .UNSPECIFIED.);
#4241=B_SPLINE_CURVE_WITH_KNOTS('',3,(#154415,#154416,#154417,#154418,#154419,
#154420),.UNSPECIFIED.,.F.,.F.,(4,2,4),(9.99999997214368E-7,1.050385970465,
2.09906864072777),.UNSPECIFIED.);
#4242=B_SPLINE_CURVE_WITH_KNOTS('',3,(#162556,#162557,#162558,#162559,#162560,
#162561),.UNSPECIFIED.,.F.,.F.,(4,2,4),(0.,0.152399999790679,0.304800000000001),
 .UNSPECIFIED.);
#4243=B_SPLINE_CURVE_WITH_KNOTS('',3,(#167156,#167157,#167158,#167159,#167160,
#167161,#167162,#167163,#167164,#167165),.UNSPECIFIED.,.F.,.F.,(4,2,2,2,
4),(0.06129084465535,0.0663539220633962,0.0872647966493331,0.10817567123527,
0.113238748643028),.UNSPECIFIED.);
#4244=B_SPLINE_CURVE_WITH_KNOTS('',3,(#167169,#167170,#167171,#167172,#167173,
#167174,#167175,#167176,#167177,#167178),.UNSPECIFIED.,.F.,.F.,(4,2,2,2,
4),(0.21714824555634,0.222211322964386,0.243122197550323,0.26403307213626,
0.269096149544019),.UNSPECIFIED.);
#4245=B_SPLINE_CURVE_WITH_KNOTS('',3,(#167205,#167206,#167207,#167208,#167209,
#167210,#167211,#167212,#167213,#167214),.UNSPECIFIED.,.F.,.F.,(4,2,2,2,
4),(-0.113238748643028,-0.10817567123527,-0.0872647966493331,-0.0663539220633962,
-0.0612908446553502),.UNSPECIFIED.);
#4246=B_SPLINE_CURVE_WITH_KNOTS('',3,(#167271,#167272,#167273,#167274,#167275,
#167276,#167277,#167278,#167279,#167280),.UNSPECIFIED.,.F.,.F.,(4,2,2,2,
4),(-0.113238748643275,-0.10817567123527,-0.0872647966493331,-0.0663539220633962,
-0.061290844655351),.UNSPECIFIED.);
#4247=B_SPLINE_CURVE_WITH_KNOTS('',3,(#167290,#167291,#167292,#167293,#167294,
#167295,#167296,#167297,#167298,#167299),.UNSPECIFIED.,.F.,.F.,(4,2,2,2,
4),(-0.113238748643028,-0.10817567123527,-0.0872647966493333,-0.0663539220633963,
-0.061290844655349),.UNSPECIFIED.);
#4248=B_SPLINE_CURVE_WITH_KNOTS('',3,(#167309,#167310,#167311,#167312,#167313,
#167314,#167315,#167316,#167317,#167318),.UNSPECIFIED.,.F.,.F.,(4,2,2,2,
4),(-0.113238748643316,-0.10817567123527,-0.0872647966493333,-0.0663539220633963,
-0.0612908446553511),.UNSPECIFIED.);
#4249=B_SPLINE_CURVE_WITH_KNOTS('',3,(#167328,#167329,#167330,#167331,#167332,
#167333,#167334,#167335,#167336,#167337),.UNSPECIFIED.,.F.,.F.,(4,2,2,2,
4),(-0.113238748643028,-0.10817567123527,-0.0872647966493333,-0.0663539220633963,
-0.0612908446553899),.UNSPECIFIED.);
#4250=B_SPLINE_CURVE_WITH_KNOTS('',3,(#167358,#167359,#167360,#167361,#167362,
#167363,#167364,#167365,#167366,#167367),.UNSPECIFIED.,.F.,.F.,(4,2,2,2,
4),(-0.269096149544267,-0.26403307213626,-0.243122197550323,-0.222211322964386,
-0.21714824555634),.UNSPECIFIED.);
#4251=B_SPLINE_CURVE_WITH_KNOTS('',3,(#167377,#167378,#167379,#167380,#167381,
#167382,#167383,#167384,#167385,#167386),.UNSPECIFIED.,.F.,.F.,(4,2,2,2,
4),(-0.269096149544016,-0.26403307213626,-0.243122197550323,-0.222211322964386,
-0.217148245556339),.UNSPECIFIED.);
#4252=B_SPLINE_CURVE_WITH_KNOTS('',3,(#167396,#167397,#167398,#167399,#167400,
#167401,#167402,#167403,#167404,#167405),.UNSPECIFIED.,.F.,.F.,(4,2,2,2,
4),(-0.269096149544018,-0.26403307213626,-0.243122197550323,-0.222211322964386,
-0.21714824555634),.UNSPECIFIED.);
#4253=B_SPLINE_CURVE_WITH_KNOTS('',3,(#167415,#167416,#167417,#167418,#167419,
#167420,#167421,#167422,#167423,#167424),.UNSPECIFIED.,.F.,.F.,(4,2,2,2,
4),(-0.269096149544306,-0.26403307213626,-0.243122197550323,-0.222211322964386,
-0.21714824555634),.UNSPECIFIED.);
#4254=B_SPLINE_CURVE_WITH_KNOTS('',3,(#167434,#167435,#167436,#167437,#167438,
#167439,#167440,#167441,#167442,#167443),.UNSPECIFIED.,.F.,.F.,(4,2,2,2,
4),(-0.269096149544019,-0.26403307213626,-0.243122197550323,-0.222211322964386,
-0.217148245556379),.UNSPECIFIED.);
#4255=B_SPLINE_CURVE_WITH_KNOTS('',3,(#167669,#167670,#167671,#167672,#167673,
#167674,#167675,#167676,#167677,#167678,#167679,#167680,#167681,#167682,
#167683,#167684,#167685,#167686,#167687,#167688,#167689,#167690,#167691,
#167692,#167693,#167694,#167695,#167696,#167697,#167698,#167699,#167700,
#167701,#167702,#167703,#167704,#167705,#167706,#167707,#167708,#167709,
#167710,#167711),.UNSPECIFIED.,.F.,.F.,(4,3,3,3,3,3,3,3,3,3,3,3,3,3,4),
(1.00966327312713E-18,1.12890698065757E-5,7.65259667098946E-5,0.000102837507928451,
0.000112544869199196,0.000130746171581843,0.000194450729921106,0.000226303009090737,
0.000242229148675553,0.000258155288260369,0.000258291104876507,0.00032765463360993,
0.000399363990826254,0.00046970928517733,0.000516310576520721),
 .UNSPECIFIED.);
#4256=B_SPLINE_CURVE_WITH_KNOTS('',3,(#167719,#167720,#167721,#167722,#167723,
#167724,#167725,#167726,#167727,#167728,#167729,#167730,#167731,#167732,
#167733,#167734,#167735,#167736,#167737,#167738,#167739,#167740,#167741,
#167742,#167743,#167744,#167745,#167746,#167747,#167748,#167749,#167750,
#167751,#167752,#167753,#167754,#167755,#167756,#167757,#167758),
 .UNSPECIFIED.,.F.,.F.,(4,3,3,3,3,3,3,3,3,3,3,3,3,4),(1.20009527741861E-17,
6.84564250799994E-5,0.000138288406590926,0.000205407478924308,0.000256966021225851,
0.000257101146970264,0.000271589374668168,0.00035221306761286,0.000388398097499794,
0.000404123622054885,0.000459162957997706,0.000486682625969117,0.000500442459954822,
0.000514202293940527),.UNSPECIFIED.);
#4257=B_SPLINE_CURVE_WITH_KNOTS('',3,(#167762,#167763,#167764,#167765,#167766,
#167767,#167768,#167769,#167770,#167771,#167772,#167773,#167774,#167775,
#167776,#167777,#167778,#167779,#167780,#167781,#167782,#167783,#167784,
#167785,#167786,#167787,#167788,#167789,#167790,#167791,#167792,#167793,
#167794,#167795,#167796,#167797,#167798,#167799,#167800,#167801,#167802,
#167803,#167804),.UNSPECIFIED.,.F.,.F.,(4,3,3,3,3,3,3,3,3,3,3,3,3,3,4),
(8.67361737988403E-19,1.12890698065828E-5,7.65259666997707E-5,0.000102837507928519,
0.00011254486919926,0.000130746171581899,0.000194450729921135,0.000226303009090753,
0.000242229148675562,0.000258155288260372,0.000258291104876513,0.000327654633625812,
0.000399363990857997,0.000469709285222688,0.000516310576520742),
 .UNSPECIFIED.);
#4258=B_SPLINE_CURVE_WITH_KNOTS('',3,(#167812,#167813,#167814,#167815,#167816,
#167817,#167818,#167819,#167820,#167821,#167822,#167823,#167824,#167825,
#167826,#167827,#167828,#167829,#167830,#167831,#167832,#167833,#167834,
#167835,#167836,#167837,#167838,#167839,#167840,#167841,#167842,#167843,
#167844,#167845,#167846,#167847,#167848,#167849,#167850,#167851),
 .UNSPECIFIED.,.F.,.F.,(4,3,3,3,3,3,3,3,3,3,3,3,3,4),(0.,6.84564250830358E-5,
0.00013828840659705,0.000205407478933295,0.000256966021225846,0.000257101146970262,
0.000271589374668165,0.000352213067609841,0.000388398097499827,0.000404123622054914,
0.000459162957997719,0.000486682625969121,0.000500442459954823,0.000514202293940524),
 .UNSPECIFIED.);
#4259=B_SPLINE_CURVE_WITH_KNOTS('',3,(#167855,#167856,#167857,#167858,#167859,
#167860,#167861,#167862,#167863,#167864,#167865,#167866,#167867,#167868,
#167869,#167870,#167871,#167872,#167873,#167874,#167875,#167876,#167877,
#167878,#167879,#167880,#167881,#167882,#167883,#167884,#167885,#167886,
#167887,#167888,#167889,#167890,#167891,#167892,#167893,#167894,#167895,
#167896,#167897),.UNSPECIFIED.,.F.,.F.,(4,3,3,3,3,3,3,3,3,3,3,3,3,3,4),
(1.73472347597681E-18,1.12890698065783E-5,7.65259667045031E-5,0.000102837507928451,
0.000112544869199196,0.000130746171581843,0.000194450729921108,0.00022630300909074,
0.000242229148675556,0.000258155288260373,0.000258291104876516,0.000327654633619643,
0.000399363990846141,0.000469709285206287,0.000516310576520743),
 .UNSPECIFIED.);
#4260=B_SPLINE_CURVE_WITH_KNOTS('',3,(#167905,#167906,#167907,#167908,#167909,
#167910,#167911,#167912,#167913,#167914,#167915,#167916,#167917,#167918,
#167919,#167920,#167921,#167922,#167923,#167924,#167925,#167926,#167927,
#167928,#167929,#167930,#167931,#167932,#167933,#167934,#167935,#167936,
#167937,#167938,#167939,#167940,#167941,#167942,#167943,#167944),
 .UNSPECIFIED.,.F.,.F.,(4,3,3,3,3,3,3,3,3,3,3,3,3,4),(0.,6.84564250848561E-5,
0.000138288406600877,0.00020540747893902,0.000256966021225847,0.00025710114697026,
0.00027158937466817,0.000352213067607056,0.000388398097499874,0.000404123622054955,
0.000459162957997738,0.000486682625969129,0.000500442459954825,0.000514202293940521),
 .UNSPECIFIED.);
#4261=B_SPLINE_CURVE_WITH_KNOTS('',3,(#167948,#167949,#167950,#167951,#167952,
#167953,#167954,#167955,#167956,#167957,#167958,#167959,#167960,#167961,
#167962,#167963,#167964,#167965,#167966,#167967,#167968,#167969,#167970,
#167971,#167972,#167973,#167974,#167975,#167976,#167977,#167978,#167979,
#167980,#167981,#167982,#167983,#167984,#167985,#167986,#167987,#167988,
#167989,#167990),.UNSPECIFIED.,.F.,.F.,(4,3,3,3,3,3,3,3,3,3,3,3,3,3,4),
(0.,1.12890698065866E-5,7.65259667154617E-5,0.000102837507928558,0.000112544869199297,
0.000130746171581931,0.000194450729921151,0.000226303009090762,0.000242229148675567,
0.000258155288260372,0.000258291104876507,0.000327654633617086,0.000399363990840721,
0.000469709285197883,0.000516310576520743),.UNSPECIFIED.);
#4262=B_SPLINE_CURVE_WITH_KNOTS('',3,(#167998,#167999,#168000,#168001,#168002,
#168003,#168004,#168005,#168006,#168007,#168008,#168009,#168010,#168011,
#168012,#168013,#168014,#168015,#168016,#168017,#168018,#168019,#168020,
#168021,#168022,#168023,#168024,#168025,#168026,#168027,#168028,#168029,
#168030,#168031,#168032,#168033,#168034,#168035,#168036,#168037),
 .UNSPECIFIED.,.F.,.F.,(4,3,3,3,3,3,3,3,3,3,3,3,3,4),(0.,6.84564250816342E-5,
0.000138288406594322,0.000205407478929741,0.000256966021225855,0.000257101146970265,
0.000271589374668173,0.000352213067599976,0.000388398097499811,0.0004041236220549,
0.000459162957997715,0.000486682625969123,0.000500442459954826,0.00051420229394053),
 .UNSPECIFIED.);
#4263=B_SPLINE_CURVE_WITH_KNOTS('',3,(#168041,#168042,#168043,#168044,#168045,
#168046,#168047,#168048,#168049,#168050,#168051,#168052,#168053,#168054,
#168055,#168056,#168057,#168058,#168059,#168060,#168061,#168062,#168063,
#168064,#168065,#168066,#168067,#168068,#168069,#168070,#168071,#168072,
#168073,#168074,#168075,#168076,#168077,#168078,#168079,#168080,#168081,
#168082,#168083),.UNSPECIFIED.,.F.,.F.,(4,3,3,3,3,3,3,3,3,3,3,3,3,3,4),
(3.46944695195361E-18,1.12890698065793E-5,7.65259667061472E-5,0.000102837507928427,
0.000112544869199174,0.000130746171581824,0.000194450729921099,0.000226303009090737,
0.000242229148675555,0.000258155288260374,0.000258291104876507,0.000327654633615792,
0.000399363990838126,0.000469709285194437,0.000516310576520745),
 .UNSPECIFIED.);
#4264=B_SPLINE_CURVE_WITH_KNOTS('',3,(#168091,#168092,#168093,#168094,#168095,
#168096,#168097,#168098,#168099,#168100,#168101,#168102,#168103,#168104,
#168105,#168106,#168107,#168108,#168109,#168110,#168111,#168112,#168113,
#168114,#168115,#168116,#168117,#168118,#168119,#168120,#168121,#168122,
#168123,#168124,#168125,#168126,#168127,#168128,#168129,#168130),
 .UNSPECIFIED.,.F.,.F.,(4,3,3,3,3,3,3,3,3,3,3,3,3,4),(0.,6.84564250791255E-5,
0.000138288406588817,0.000205407478920826,0.000256966021225839,0.000257101146970257,
0.000271589374668167,0.000352213067604686,0.00038839809749988,0.00040412362205496,
0.000459162957997741,0.000486682625969131,0.000500442459954827,0.000514202293940522),
 .UNSPECIFIED.);
#4265=B_SPLINE_CURVE_WITH_KNOTS('',3,(#168134,#168135,#168136,#168137,#168138,
#168139,#168140,#168141,#168142,#168143,#168144,#168145,#168146,#168147,
#168148,#168149,#168150,#168151,#168152,#168153,#168154,#168155,#168156,
#168157,#168158,#168159,#168160,#168161,#168162,#168163,#168164,#168165,
#168166,#168167,#168168,#168169,#168170,#168171,#168172,#168173,#168174,
#168175,#168176),.UNSPECIFIED.,.F.,.F.,(4,3,3,3,3,3,3,3,3,3,3,3,3,3,4),
(0.,1.128906980658E-5,7.65259667055946E-5,0.000102837507928488,0.000112544869199231,
0.000130746171581874,0.000194450729921126,0.000226303009090752,0.000242229148675565,
0.000258155288260378,0.00025829110487652,0.000327654633621028,0.000399363990848623,
0.000469709285209461,0.000516310576520755),.UNSPECIFIED.);
#4266=B_SPLINE_CURVE_WITH_KNOTS('',3,(#168184,#168185,#168186,#168187,#168188,
#168189,#168190,#168191,#168192,#168193,#168194,#168195,#168196,#168197,
#168198,#168199,#168200,#168201,#168202,#168203,#168204,#168205,#168206,
#168207,#168208,#168209,#168210,#168211,#168212,#168213,#168214,#168215,
#168216,#168217,#168218,#168219,#168220,#168221,#168222,#168223),
 .UNSPECIFIED.,.F.,.F.,(4,3,3,3,3,3,3,3,3,3,3,3,3,4),(0.,6.84564250797382E-5,
0.000138288406590481,0.000205407478923822,0.00025696602122586,0.000257101146970262,
0.000271589374668168,0.000352213067609828,0.000388398097499862,0.000404123622054945,
0.000459162957997734,0.000486682625969129,0.000500442459954826,0.000514202293940523),
 .UNSPECIFIED.);
#4267=B_SPLINE_CURVE_WITH_KNOTS('',3,(#168227,#168228,#168229,#168230,#168231,
#168232,#168233,#168234,#168235,#168236,#168237,#168238,#168239,#168240,
#168241,#168242,#168243,#168244,#168245,#168246,#168247,#168248,#168249,
#168250,#168251,#168252,#168253,#168254,#168255,#168256,#168257,#168258,
#168259,#168260,#168261,#168262,#168263,#168264,#168265,#168266,#168267,
#168268,#168269),.UNSPECIFIED.,.F.,.F.,(4,3,3,3,3,3,3,3,3,3,3,3,3,3,4),
(0.,1.12890698065866E-5,7.65259667026273E-5,0.000102837507928552,0.000112544869199291,
0.000130746171581927,0.000194450729921151,0.000226303009090764,0.00024222914867557,
0.000258155288260376,0.000258291104876516,0.000327654633619408,0.000399363990846113,
0.000469709285207155,0.000516310576520752),.UNSPECIFIED.);
#4268=B_SPLINE_CURVE_WITH_KNOTS('',3,(#168277,#168278,#168279,#168280,#168281,
#168282,#168283,#168284,#168285,#168286,#168287,#168288,#168289,#168290,
#168291,#168292,#168293,#168294,#168295,#168296,#168297,#168298,#168299,
#168300,#168301,#168302,#168303,#168304,#168305,#168306,#168307,#168308,
#168309,#168310,#168311,#168312,#168313,#168314,#168315,#168316),
 .UNSPECIFIED.,.F.,.F.,(4,3,3,3,3,3,3,3,3,3,3,3,3,4),(0.,6.84564250840846E-5,
0.000138288406599155,0.00020540747893674,0.000256966021225868,0.000257101146970265,
0.000271589374668158,0.000352213067593023,0.000388398097499727,0.000404123622054827,
0.000459162957997679,0.000486682625969105,0.000500442459954818,0.000514202293940531),
 .UNSPECIFIED.);
#4269=B_SPLINE_CURVE_WITH_KNOTS('',3,(#168320,#168321,#168322,#168323,#168324,
#168325,#168326,#168327,#168328,#168329,#168330,#168331,#168332,#168333,
#168334,#168335,#168336,#168337,#168338,#168339,#168340,#168341,#168342,
#168343,#168344,#168345,#168346,#168347,#168348,#168349,#168350,#168351,
#168352,#168353,#168354,#168355,#168356,#168357,#168358,#168359,#168360,
#168361,#168362),.UNSPECIFIED.,.F.,.F.,(4,3,3,3,3,3,3,3,3,3,3,3,3,3,4),
(0.,1.12890698065756E-5,7.65259666974363E-5,0.000102837507928435,0.000112544869199181,
0.000130746171581831,0.000194450729921105,0.000226303009090742,0.00024222914867556,
0.000258155288260379,0.000258291104876533,0.000327654633620618,0.000399363990848227,
0.000469709285210271,0.000516310576520758),.UNSPECIFIED.);
#4270=B_SPLINE_CURVE_WITH_KNOTS('',3,(#168370,#168371,#168372,#168373,#168374,
#168375,#168376,#168377,#168378,#168379,#168380,#168381,#168382,#168383,
#168384,#168385,#168386,#168387,#168388,#168389,#168390,#168391,#168392,
#168393,#168394,#168395,#168396,#168397,#168398,#168399,#168400,#168401,
#168402,#168403,#168404,#168405,#168406,#168407,#168408,#168409),
 .UNSPECIFIED.,.F.,.F.,(4,3,3,3,3,3,3,3,3,3,3,3,3,4),(0.,6.84564250769302E-5,
0.000138288406583924,0.000205407478911775,0.000256966021225856,0.000257101146970262,
0.000271589374668158,0.000352213067622837,0.000388398097499689,0.000404123622054793,
0.000459162957997659,0.000486682625969092,0.000500442459954808,0.000514202293940524),
 .UNSPECIFIED.);
#4271=B_SPLINE_CURVE_WITH_KNOTS('',3,(#168413,#168414,#168415,#168416,#168417,
#168418,#168419,#168420,#168421,#168422,#168423,#168424,#168425,#168426,
#168427,#168428,#168429,#168430,#168431,#168432,#168433,#168434,#168435,
#168436,#168437,#168438,#168439,#168440,#168441,#168442,#168443,#168444,
#168445,#168446,#168447,#168448,#168449,#168450,#168451,#168452,#168453,
#168454,#168455),.UNSPECIFIED.,.F.,.F.,(4,3,3,3,3,3,3,3,3,3,3,3,3,3,4),
(0.,1.12890698065816E-5,7.65259666866503E-5,0.000102837507928537,0.000112544869199277,
0.000130746171581913,0.000194450729921141,0.000226303009090755,0.000242229148675562,
0.000258155288260369,0.000258291104876509,0.00032765463362347,0.000399363990852578,
0.000469709285214009,0.000516310576520738),.UNSPECIFIED.);
#4272=B_SPLINE_CURVE_WITH_KNOTS('',3,(#168463,#168464,#168465,#168466,#168467,
#168468,#168469,#168470,#168471,#168472,#168473,#168474,#168475,#168476,
#168477,#168478,#168479,#168480,#168481,#168482,#168483,#168484,#168485,
#168486,#168487,#168488,#168489,#168490,#168491,#168492,#168493,#168494,
#168495,#168496,#168497,#168498,#168499,#168500,#168501,#168502),
 .UNSPECIFIED.,.F.,.F.,(4,3,3,3,3,3,3,3,3,3,3,3,3,4),(0.,6.845642508705E-5,
0.000138288406605506,0.000205407478946818,0.000256966021225846,0.000257101146970255,
0.00027158937466815,0.00035221306759162,0.000388398097499678,0.000404123622054782,
0.000459162957997647,0.000486682625969079,0.000500442459954795,0.000514202293940511),
 .UNSPECIFIED.);
#4273=B_SPLINE_CURVE_WITH_KNOTS('',3,(#168506,#168507,#168508,#168509,#168510,
#168511,#168512,#168513,#168514,#168515,#168516,#168517,#168518,#168519,
#168520,#168521,#168522,#168523,#168524,#168525,#168526,#168527,#168528,
#168529,#168530,#168531,#168532,#168533,#168534,#168535,#168536,#168537,
#168538,#168539,#168540,#168541,#168542,#168543,#168544,#168545,#168546,
#168547,#168548),.UNSPECIFIED.,.F.,.F.,(4,3,3,3,3,3,3,3,3,3,3,3,3,3,4),
(0.,1.12890698065805E-5,7.65259667089018E-5,0.000102837507928513,0.000112544869199254,
0.000130746171581893,0.000194450729921131,0.00022630300909075,0.000242229148675559,
0.000258155288260369,0.00025829110487651,0.000327654633617099,0.000399363990841473,
0.000469709285200287,0.000516310576520737),.UNSPECIFIED.);
#4274=B_SPLINE_CURVE_WITH_KNOTS('',3,(#168556,#168557,#168558,#168559,#168560,
#168561,#168562,#168563,#168564,#168565,#168566,#168567,#168568,#168569,
#168570,#168571,#168572,#168573,#168574,#168575,#168576,#168577,#168578,
#168579,#168580,#168581,#168582,#168583,#168584,#168585,#168586,#168587,
#168588,#168589,#168590,#168591,#168592,#168593,#168594,#168595),
 .UNSPECIFIED.,.F.,.F.,(4,3,3,3,3,3,3,3,3,3,3,3,3,4),(0.,6.84564250895596E-5,
0.000138288406609849,0.000205407478950599,0.000256966021225854,0.000257101146970263,
0.000271589374668168,0.000352213067611649,0.000388398097499792,0.000404123622054883,
0.000459162957997705,0.000486682625969115,0.00050044245995482,0.000514202293940526),
 .UNSPECIFIED.);
#4275=B_SPLINE_CURVE_WITH_KNOTS('',3,(#168599,#168600,#168601,#168602,#168603,
#168604,#168605,#168606,#168607,#168608,#168609,#168610,#168611,#168612,
#168613,#168614,#168615,#168616,#168617,#168618,#168619,#168620,#168621,
#168622,#168623,#168624,#168625,#168626,#168627,#168628,#168629,#168630,
#168631,#168632,#168633,#168634,#168635,#168636,#168637,#168638,#168639,
#168640,#168641),.UNSPECIFIED.,.F.,.F.,(4,3,3,3,3,3,3,3,3,3,3,3,3,3,4),
(0.,1.12890698065891E-5,7.65259667078449E-5,0.000102837507928607,0.000112544869199342,
0.000130746171581971,0.000194450729921172,0.000226303009090772,0.000242229148675572,
0.000258155288260373,0.000258291104876515,0.000327654633617038,0.000399363990840811,
0.000469709285198597,0.000516310576520745),.UNSPECIFIED.);
#4276=B_SPLINE_CURVE_WITH_KNOTS('',3,(#168649,#168650,#168651,#168652,#168653,
#168654,#168655,#168656,#168657,#168658,#168659,#168660,#168661,#168662,
#168663,#168664,#168665,#168666,#168667,#168668,#168669,#168670,#168671,
#168672,#168673,#168674,#168675,#168676,#168677,#168678,#168679,#168680,
#168681,#168682,#168683,#168684,#168685,#168686,#168687,#168688),
 .UNSPECIFIED.,.F.,.F.,(4,3,3,3,3,3,3,3,3,3,3,3,3,4),(0.,6.84564250838755E-5,
0.000138288406598415,0.00020540747893465,0.000256966021225841,0.000257101146970261,
0.000271589374668164,0.0003522130676064,0.000388398097499832,0.000404123622054918,
0.000459162957997721,0.000486682625969122,0.000500442459954822,0.000514202293940523),
 .UNSPECIFIED.);
#4277=B_SPLINE_CURVE_WITH_KNOTS('',3,(#168692,#168693,#168694,#168695,#168696,
#168697,#168698,#168699,#168700,#168701,#168702,#168703,#168704,#168705,
#168706,#168707,#168708,#168709,#168710,#168711,#168712,#168713,#168714,
#168715,#168716,#168717,#168718,#168719,#168720,#168721,#168722,#168723,
#168724,#168725,#168726,#168727,#168728,#168729,#168730,#168731,#168732,
#168733,#168734),.UNSPECIFIED.,.F.,.F.,(4,3,3,3,3,3,3,3,3,3,3,3,3,3,4),
(0.,1.12890698065788E-5,7.65259667132543E-5,0.000102837507928489,0.000112544869199232,
0.000130746171581874,0.000194450729921125,0.00022630300909075,0.000242229148675562,
0.000258155288260375,0.000258291104876516,0.000327654633612138,0.000399363990830831,
0.000469709285183981,0.00051631057652075),.UNSPECIFIED.);
#4278=B_SPLINE_CURVE_WITH_KNOTS('',3,(#168742,#168743,#168744,#168745,#168746,
#168747,#168748,#168749,#168750,#168751,#168752,#168753,#168754,#168755,
#168756,#168757,#168758,#168759,#168760,#168761,#168762,#168763,#168764,
#168765,#168766,#168767,#168768,#168769,#168770,#168771,#168772,#168773,
#168774,#168775,#168776,#168777,#168778,#168779,#168780,#168781),
 .UNSPECIFIED.,.F.,.F.,(4,3,3,3,3,3,3,3,3,3,3,3,3,4),(0.,6.84564250765995E-5,
0.000138288406584294,0.000205407478915326,0.000256966021225849,0.000257101146970262,
0.000271589374668161,0.000352213067601591,0.000388398097499769,0.000404123622054863,
0.000459162957997693,0.000486682625969109,0.000500442459954816,0.000514202293940524),
 .UNSPECIFIED.);
#4279=B_SPLINE_CURVE_WITH_KNOTS('',3,(#168785,#168786,#168787,#168788,#168789,
#168790,#168791,#168792,#168793,#168794,#168795,#168796,#168797,#168798,
#168799,#168800,#168801,#168802,#168803,#168804,#168805,#168806,#168807,
#168808,#168809,#168810,#168811,#168812,#168813,#168814,#168815,#168816,
#168817,#168818,#168819,#168820,#168821,#168822,#168823,#168824,#168825,
#168826,#168827),.UNSPECIFIED.,.F.,.F.,(4,3,3,3,3,3,3,3,3,3,3,3,3,3,4),
(3.46944695195361E-18,1.12890698065869E-5,7.65259667025008E-5,0.000102837507928517,
0.000112544869199258,0.000130746171581898,0.000194450729921137,0.000226303009090756,
0.000242229148675566,0.000258155288260376,0.000258291104876511,0.000327654633609564,
0.000399363990824879,0.000469709285174596,0.000516310576520748),
 .UNSPECIFIED.);
#4280=B_SPLINE_CURVE_WITH_KNOTS('',3,(#168835,#168836,#168837,#168838,#168839,
#168840,#168841,#168842,#168843,#168844,#168845,#168846,#168847,#168848,
#168849,#168850,#168851,#168852,#168853,#168854,#168855,#168856,#168857,
#168858,#168859,#168860,#168861,#168862,#168863,#168864,#168865,#168866,
#168867,#168868,#168869,#168870,#168871,#168872,#168873,#168874),
 .UNSPECIFIED.,.F.,.F.,(4,3,3,3,3,3,3,3,3,3,3,3,3,4),(0.,6.84564250797669E-5,
0.000138288406590498,0.000205407478924127,0.000256966021225838,0.000257101146970264,
0.000271589374668166,0.000352213067600068,0.000388398097499821,0.00040412362205491,
0.000459162957997718,0.000486682625969123,0.000500442459954825,0.000514202293940527),
 .UNSPECIFIED.);
#4281=B_SPLINE_CURVE_WITH_KNOTS('',3,(#168878,#168879,#168880,#168881,#168882,
#168883,#168884,#168885,#168886,#168887,#168888,#168889,#168890,#168891,
#168892,#168893,#168894,#168895,#168896,#168897,#168898,#168899,#168900,
#168901,#168902,#168903,#168904,#168905,#168906,#168907,#168908,#168909,
#168910,#168911,#168912,#168913,#168914,#168915,#168916,#168917,#168918,
#168919,#168920),.UNSPECIFIED.,.F.,.F.,(4,3,3,3,3,3,3,3,3,3,3,3,3,3,4),
(1.73472347597681E-18,1.12890698065832E-5,7.65259667045979E-5,0.000102837507928536,
0.000112544869199276,0.000130746171581912,0.00019445072992114,0.000226303009090754,
0.000242229148675561,0.000258155288260368,0.000258291104876511,0.000327654633615822,
0.000399363990838075,0.000469709285194198,0.000516310576520735),
 .UNSPECIFIED.);
#4282=B_SPLINE_CURVE_WITH_KNOTS('',3,(#168928,#168929,#168930,#168931,#168932,
#168933,#168934,#168935,#168936,#168937,#168938,#168939,#168940,#168941,
#168942,#168943,#168944,#168945,#168946,#168947,#168948,#168949,#168950,
#168951,#168952,#168953,#168954,#168955,#168956,#168957,#168958,#168959,
#168960,#168961,#168962,#168963,#168964,#168965,#168966,#168967),
 .UNSPECIFIED.,.F.,.F.,(4,3,3,3,3,3,3,3,3,3,3,3,3,4),(0.,6.84564250822334E-5,
0.000138288406595693,0.000205407478931659,0.000256966021225854,0.000257101146970264,
0.000271589374668166,0.000352213067615386,0.000388398097499783,0.000404123622054876,
0.000459162957997701,0.000486682625969114,0.000500442459954821,0.000514202293940527),
 .UNSPECIFIED.);
#4283=B_SPLINE_CURVE_WITH_KNOTS('',3,(#168971,#168972,#168973,#168974,#168975,
#168976,#168977,#168978,#168979,#168980,#168981,#168982,#168983,#168984,
#168985,#168986,#168987,#168988,#168989,#168990,#168991,#168992,#168993,
#168994,#168995,#168996,#168997,#168998,#168999,#169000,#169001,#169002,
#169003,#169004,#169005,#169006,#169007,#169008,#169009,#169010,#169011,
#169012,#169013),.UNSPECIFIED.,.F.,.F.,(4,3,3,3,3,3,3,3,3,3,3,3,3,3,4),
(0.,1.12890698065817E-5,7.652596670597E-5,0.000102837507928492,0.000112544869199235,
0.000130746171581877,0.000194450729921126,0.00022630300909075,0.000242229148675562,
0.000258155288260375,0.000258291104876527,0.000327654633612159,0.000399363990830566,
0.000469709285183404,0.000516310576520749),.UNSPECIFIED.);
#4284=B_SPLINE_CURVE_WITH_KNOTS('',3,(#169021,#169022,#169023,#169024,#169025,
#169026,#169027,#169028,#169029,#169030,#169031,#169032,#169033,#169034,
#169035,#169036,#169037,#169038,#169039,#169040,#169041,#169042,#169043,
#169044,#169045,#169046,#169047,#169048,#169049,#169050,#169051,#169052,
#169053,#169054,#169055,#169056,#169057,#169058,#169059,#169060),
 .UNSPECIFIED.,.F.,.F.,(4,3,3,3,3,3,3,3,3,3,3,3,3,4),(0.,6.84564250761049E-5,
0.00013828840658303,0.000205407478912784,0.000256966021225849,0.000257101146970261,
0.000271589374668167,0.000352213067604775,0.000388398097499802,0.000404123622054892,
0.000459162957997707,0.000486682625969115,0.000500442459954818,0.000514202293940522),
 .UNSPECIFIED.);
#4285=B_SPLINE_CURVE_WITH_KNOTS('',3,(#169064,#169065,#169066,#169067,#169068,
#169069,#169070,#169071,#169072,#169073,#169074,#169075,#169076,#169077,
#169078,#169079,#169080,#169081,#169082,#169083,#169084,#169085,#169086,
#169087,#169088,#169089,#169090,#169091,#169092,#169093,#169094,#169095,
#169096,#169097,#169098,#169099,#169100,#169101,#169102,#169103,#169104,
#169105,#169106),.UNSPECIFIED.,.F.,.F.,(4,3,3,3,3,3,3,3,3,3,3,3,3,3,4),
(0.,1.12890698065779E-5,7.65259667127145E-5,0.000102837507928481,0.000112544869199224,
0.000130746171581867,0.000194450729921117,0.000226303009090742,0.000242229148675555,
0.000258155288260368,0.000258291104876507,0.000327654633610104,0.000399363990826758,
0.000469709285178193,0.000516310576520735),.UNSPECIFIED.);
#4286=B_SPLINE_CURVE_WITH_KNOTS('',3,(#169114,#169115,#169116,#169117,#169118,
#169119,#169120,#169121,#169122,#169123,#169124,#169125,#169126,#169127,
#169128,#169129,#169130,#169131,#169132,#169133,#169134,#169135,#169136,
#169137,#169138,#169139,#169140,#169141,#169142,#169143,#169144,#169145,
#169146,#169147,#169148,#169149,#169150,#169151,#169152,#169153),
 .UNSPECIFIED.,.F.,.F.,(4,3,3,3,3,3,3,3,3,3,3,3,3,4),(0.,6.84564250890086E-5,
0.000138288406609153,0.000205407478951144,0.000256966021225856,0.000257101146970263,
0.000271589374668163,0.00035221306760415,0.000388398097499778,0.000404123622054872,
0.000459162957997699,0.000486682625969112,0.000500442459954819,0.000514202293940526),
 .UNSPECIFIED.);
#4287=B_SPLINE_CURVE_WITH_KNOTS('',3,(#169157,#169158,#169159,#169160,#169161,
#169162,#169163,#169164,#169165,#169166,#169167,#169168,#169169,#169170,
#169171,#169172,#169173,#169174,#169175,#169176,#169177,#169178,#169179,
#169180,#169181,#169182,#169183,#169184,#169185,#169186,#169187,#169188,
#169189,#169190,#169191,#169192,#169193,#169194,#169195,#169196,#169197,
#169198,#169199),.UNSPECIFIED.,.F.,.F.,(4,3,3,3,3,3,3,3,3,3,3,3,3,3,4),
(8.67361737988404E-19,1.12890698065823E-5,7.65259666978494E-5,0.000102837507928528,
0.000112544869199268,0.000130746171581906,0.000194450729921138,0.000226303009090754,
0.000242229148675562,0.000258155288260371,0.0002582911048765,0.000327654633618696,
0.000399363990843831,0.000469709285202593,0.00051631057652074),
 .UNSPECIFIED.);
#4288=B_SPLINE_CURVE_WITH_KNOTS('',3,(#169207,#169208,#169209,#169210,#169211,
#169212,#169213,#169214,#169215,#169216,#169217,#169218,#169219,#169220,
#169221,#169222,#169223,#169224,#169225,#169226,#169227,#169228,#169229,
#169230,#169231,#169232,#169233,#169234,#169235,#169236,#169237,#169238,
#169239,#169240,#169241,#169242,#169243,#169244,#169245,#169246),
 .UNSPECIFIED.,.F.,.F.,(4,3,3,3,3,3,3,3,3,3,3,3,3,4),(0.,6.84564250864531E-5,
0.000138288406604524,0.000205407478945309,0.000256966021225842,0.000257101146970264,
0.000271589374668167,0.00035221306760789,0.000388398097499815,0.000404123622054904,
0.000459162957997716,0.000486682625969122,0.000500442459954825,0.000514202293940528),
 .UNSPECIFIED.);
#4289=B_SPLINE_CURVE_WITH_KNOTS('',3,(#169250,#169251,#169252,#169253,#169254,
#169255,#169256,#169257,#169258,#169259,#169260,#169261,#169262,#169263,
#169264,#169265,#169266,#169267,#169268,#169269,#169270,#169271,#169272,
#169273,#169274,#169275,#169276,#169277,#169278,#169279,#169280,#169281,
#169282,#169283,#169284,#169285,#169286,#169287,#169288,#169289,#169290,
#169291,#169292),.UNSPECIFIED.,.F.,.F.,(4,3,3,3,3,3,3,3,3,3,3,3,3,3,4),
(1.73472347597681E-18,1.12890698065862E-5,7.652596670712E-5,0.000102837507928532,
0.000112544869199272,0.000130746171581909,0.000194450729921137,0.000226303009090752,
0.000242229148675559,0.000258155288260366,0.000258291104876512,0.000327654633614979,
0.000399363990836396,0.000469709285192041,0.00051631057652073),
 .UNSPECIFIED.);
#4290=B_SPLINE_CURVE_WITH_KNOTS('',3,(#169300,#169301,#169302,#169303,#169304,
#169305,#169306,#169307,#169308,#169309,#169310,#169311,#169312,#169313,
#169314,#169315,#169316,#169317,#169318,#169319,#169320,#169321,#169322,
#169323,#169324,#169325,#169326,#169327,#169328,#169329,#169330,#169331,
#169332,#169333,#169334,#169335,#169336,#169337,#169338,#169339),
 .UNSPECIFIED.,.F.,.F.,(4,3,3,3,3,3,3,3,3,3,3,3,3,4),(0.,6.84564250871121E-5,
0.000138288406605608,0.000205407478946803,0.000256966021225858,0.000257101146970267,
0.000271589374668171,0.000352213067596241,0.000388398097499807,0.000404123622054898,
0.000459162957997716,0.000486682625969125,0.000500442459954829,0.000514202293940534),
 .UNSPECIFIED.);
#4291=B_SPLINE_CURVE_WITH_KNOTS('',3,(#169343,#169344,#169345,#169346,#169347,
#169348,#169349,#169350,#169351,#169352,#169353,#169354,#169355,#169356,
#169357,#169358,#169359,#169360,#169361,#169362,#169363,#169364,#169365,
#169366,#169367,#169368,#169369,#169370,#169371,#169372,#169373,#169374,
#169375,#169376,#169377,#169378,#169379,#169380,#169381,#169382,#169383,
#169384,#169385),.UNSPECIFIED.,.F.,.F.,(4,3,3,3,3,3,3,3,3,3,3,3,3,3,4),
(0.,1.12890698065804E-5,7.65259666985084E-5,0.000102837507928506,0.000112544869199248,
0.000130746171581889,0.000194450729921132,0.000226303009090753,0.000242229148675564,
0.000258155288260375,0.000258291104876532,0.000327654633619549,0.000399363990845382,
0.000469709285204578,0.00051631057652075),.UNSPECIFIED.);
#4292=B_SPLINE_CURVE_WITH_KNOTS('',3,(#169393,#169394,#169395,#169396,#169397,
#169398,#169399,#169400,#169401,#169402,#169403,#169404,#169405,#169406,
#169407,#169408,#169409,#169410,#169411,#169412,#169413,#169414,#169415,
#169416,#169417,#169418,#169419,#169420,#169421,#169422,#169423,#169424,
#169425,#169426,#169427,#169428,#169429,#169430,#169431,#169432),
 .UNSPECIFIED.,.F.,.F.,(4,3,3,3,3,3,3,3,3,3,3,3,3,4),(0.,6.84564250843184E-5,
0.000138288406599641,0.000205407478937078,0.000256966021225852,0.000257101146970261,
0.000271589374668166,0.000352213067604727,0.000388398097499781,0.000404123622054874,
0.000459162957997697,0.000486682625969109,0.000500442459954815,0.000514202293940521),
 .UNSPECIFIED.);
#4293=B_SPLINE_CURVE_WITH_KNOTS('',3,(#169436,#169437,#169438,#169439,#169440,
#169441,#169442,#169443,#169444,#169445,#169446,#169447,#169448,#169449,
#169450,#169451,#169452,#169453,#169454,#169455,#169456,#169457,#169458,
#169459,#169460,#169461,#169462,#169463,#169464,#169465,#169466,#169467,
#169468,#169469,#169470,#169471,#169472,#169473,#169474,#169475,#169476,
#169477,#169478),.UNSPECIFIED.,.F.,.F.,(4,3,3,3,3,3,3,3,3,3,3,3,3,3,4),
(0.,1.12890698065816E-5,7.65259667114556E-5,0.000102837507928525,0.000112544869199266,
0.000130746171581904,0.00019445072992114,0.000226303009090757,0.000242229148675566,
0.000258155288260375,0.000258291104876523,0.00032765463361819,0.000399363990843023,
0.000469709285201166,0.000516310576520736),.UNSPECIFIED.);
#4294=B_SPLINE_CURVE_WITH_KNOTS('',3,(#169486,#169487,#169488,#169489,#169490,
#169491,#169492,#169493,#169494,#169495,#169496,#169497,#169498,#169499,
#169500,#169501,#169502,#169503,#169504,#169505,#169506,#169507,#169508,
#169509,#169510,#169511,#169512,#169513,#169514,#169515,#169516,#169517,
#169518,#169519,#169520,#169521,#169522,#169523,#169524,#169525),
 .UNSPECIFIED.,.F.,.F.,(4,3,3,3,3,3,3,3,3,3,3,3,3,4),(0.,6.8456425074579E-5,
0.000138288406580344,0.000205407478909642,0.000256966021225861,0.000257101146970265,
0.00027158937466816,0.000352213067612298,0.000388398097499719,0.00040412362205482,
0.000459162957997671,0.000486682625969096,0.000500442459954809,0.000514202293940522),
 .UNSPECIFIED.);
#4295=B_SPLINE_CURVE_WITH_KNOTS('',3,(#169529,#169530,#169531,#169532,#169533,
#169534,#169535,#169536,#169537,#169538,#169539,#169540,#169541,#169542,
#169543,#169544,#169545,#169546,#169547,#169548,#169549,#169550,#169551,
#169552,#169553,#169554,#169555,#169556,#169557,#169558,#169559,#169560,
#169561,#169562,#169563,#169564,#169565,#169566,#169567,#169568,#169569,
#169570,#169571),.UNSPECIFIED.,.F.,.F.,(4,3,3,3,3,3,3,3,3,3,3,3,3,3,4),
(0.,1.12890698065828E-5,7.6525966717577E-5,0.000102837507928482,0.000112544869199225,
0.000130746171581869,0.000194450729921122,0.000226303009090749,0.000242229148675563,
0.000258155288260376,0.000258291104876513,0.000327654633621626,0.000399363990850335,
0.000469709285212286,0.000516310576520752),.UNSPECIFIED.);
#4296=B_SPLINE_CURVE_WITH_KNOTS('',3,(#169579,#169580,#169581,#169582,#169583,
#169584,#169585,#169586,#169587,#169588,#169589,#169590,#169591,#169592,
#169593,#169594,#169595,#169596,#169597,#169598,#169599,#169600,#169601,
#169602,#169603,#169604,#169605,#169606,#169607,#169608,#169609,#169610,
#169611,#169612,#169613,#169614,#169615,#169616,#169617,#169618),
 .UNSPECIFIED.,.F.,.F.,(4,3,3,3,3,3,3,3,3,3,3,3,3,4),(0.,6.84564250758689E-5,
0.000138288406581853,0.000205407478909165,0.000256966021225856,0.00025710114697026,
0.000271589374668164,0.00035221306760689,0.000388398097499763,0.000404123622054857,
0.000459162957997689,0.000486682625969104,0.000500442459954812,0.00051420229394052),
 .UNSPECIFIED.);
#4297=B_SPLINE_CURVE_WITH_KNOTS('',3,(#169622,#169623,#169624,#169625,#169626,
#169627,#169628,#169629,#169630,#169631,#169632,#169633,#169634,#169635,
#169636,#169637,#169638,#169639,#169640,#169641,#169642,#169643,#169644,
#169645,#169646,#169647,#169648,#169649,#169650,#169651,#169652,#169653,
#169654,#169655,#169656,#169657,#169658,#169659,#169660,#169661,#169662,
#169663,#169664),.UNSPECIFIED.,.F.,.F.,(4,3,3,3,3,3,3,3,3,3,3,3,3,3,4),
(0.,1.12890698065862E-5,7.65259667010518E-5,0.000102837507928541,0.00011254486919928,
0.000130746171581917,0.000194450729921143,0.000226303009090756,0.000242229148675563,
0.000258155288260369,0.000258291104876529,0.000327654633612457,0.000399363990831282,
0.000469709285184427,0.000516310576520739),.UNSPECIFIED.);
#4298=B_SPLINE_CURVE_WITH_KNOTS('',3,(#169672,#169673,#169674,#169675,#169676,
#169677,#169678,#169679,#169680,#169681,#169682,#169683,#169684,#169685,
#169686,#169687,#169688,#169689,#169690,#169691,#169692,#169693,#169694,
#169695,#169696,#169697,#169698,#169699,#169700,#169701,#169702,#169703,
#169704,#169705,#169706,#169707,#169708,#169709,#169710,#169711),
 .UNSPECIFIED.,.F.,.F.,(4,3,3,3,3,3,3,3,3,3,3,3,3,4),(0.,6.84564250843761E-5,
0.000138288406600102,0.000205407478938898,0.00025696602122586,0.000257101146970268,
0.000271589374668179,0.000352213067592679,0.000388398097499883,0.000404123622054964,
0.00045916295799775,0.000486682625969143,0.000500442459954839,0.000514202293940536),
 .UNSPECIFIED.);
#4299=B_SPLINE_CURVE_WITH_KNOTS('',3,(#169715,#169716,#169717,#169718,#169719,
#169720,#169721,#169722,#169723,#169724,#169725,#169726,#169727,#169728,
#169729,#169730,#169731,#169732,#169733,#169734,#169735,#169736,#169737,
#169738,#169739,#169740,#169741,#169742,#169743,#169744,#169745,#169746,
#169747,#169748,#169749,#169750,#169751,#169752,#169753,#169754,#169755,
#169756,#169757),.UNSPECIFIED.,.F.,.F.,(4,3,3,3,3,3,3,3,3,3,3,3,3,3,4),
(0.,1.12890698065796E-5,7.65259666991178E-5,0.000102837507928466,0.000112544869199211,
0.000130746171581857,0.000194450729921119,0.000226303009090749,0.000242229148675565,
0.00025815528826038,0.000258291104876507,0.000327654633623256,0.000399363990854542,
0.000469709285220818,0.000516310576520761),.UNSPECIFIED.);
#4300=B_SPLINE_CURVE_WITH_KNOTS('',3,(#169765,#169766,#169767,#169768,#169769,
#169770,#169771,#169772,#169773,#169774,#169775,#169776,#169777,#169778,
#169779,#169780,#169781,#169782,#169783,#169784,#169785,#169786,#169787,
#169788,#169789,#169790,#169791,#169792,#169793,#169794,#169795,#169796,
#169797,#169798,#169799,#169800,#169801,#169802,#169803,#169804),
 .UNSPECIFIED.,.F.,.F.,(4,3,3,3,3,3,3,3,3,3,3,3,3,4),(0.,6.8456425090809E-5,
0.000138288406613196,0.00020540747895784,0.000256966021225841,0.000257101146970264,
0.000271589374668169,0.000352213067601343,0.000388398097499806,0.000404123622054896,
0.000459162957997712,0.00048668262596912,0.000500442459954824,0.000514202293940528),
 .UNSPECIFIED.);
#4301=B_SPLINE_CURVE_WITH_KNOTS('',3,(#169808,#169809,#169810,#169811,#169812,
#169813,#169814,#169815,#169816,#169817,#169818,#169819,#169820,#169821,
#169822,#169823,#169824,#169825,#169826,#169827,#169828,#169829,#169830,
#169831,#169832,#169833,#169834,#169835,#169836,#169837,#169838,#169839,
#169840,#169841,#169842,#169843,#169844,#169845,#169846,#169847,#169848,
#169849,#169850),.UNSPECIFIED.,.F.,.F.,(4,3,3,3,3,3,3,3,3,3,3,3,3,3,4),
(0.,1.12890698065837E-5,7.65259666927835E-5,0.000102837507928546,0.000112544869199286,
0.000130746171581922,0.000194450729921148,0.000226303009090761,0.000242229148675567,
0.000258155288260374,0.000258291104876513,0.000327654633617415,0.000399363990840611,
0.000469709285196912,0.000516310576520748),.UNSPECIFIED.);
#4302=B_SPLINE_CURVE_WITH_KNOTS('',3,(#169858,#169859,#169860,#169861,#169862,
#169863,#169864,#169865,#169866,#169867,#169868,#169869,#169870,#169871,
#169872,#169873,#169874,#169875,#169876,#169877,#169878,#169879,#169880,
#169881,#169882,#169883,#169884,#169885,#169886,#169887,#169888,#169889,
#169890,#169891,#169892,#169893,#169894,#169895,#169896,#169897),
 .UNSPECIFIED.,.F.,.F.,(4,3,3,3,3,3,3,3,3,3,3,3,3,4),(0.,6.84564250857982E-5,
0.000138288406602572,0.000205407478941416,0.000256966021225879,0.000257101146970264,
0.000271589374668177,0.000352213067604349,0.000388398097499876,0.000404123622054957,
0.000459162957997742,0.000486682625969135,0.000500442459954831,0.000514202293940528),
 .UNSPECIFIED.);
#4303=B_SPLINE_CURVE_WITH_KNOTS('',3,(#169901,#169902,#169903,#169904,#169905,
#169906,#169907,#169908,#169909,#169910,#169911,#169912,#169913,#169914,
#169915,#169916,#169917,#169918,#169919,#169920,#169921,#169922,#169923,
#169924,#169925,#169926,#169927,#169928,#169929,#169930,#169931,#169932,
#169933,#169934,#169935,#169936,#169937,#169938,#169939,#169940,#169941,
#169942,#169943),.UNSPECIFIED.,.F.,.F.,(4,3,3,3,3,3,3,3,3,3,3,3,3,3,4),
(0.,1.12890698065829E-5,7.6525966704634E-5,0.00010283750792853,0.000112544869199271,
0.000130746171581909,0.000194450729921141,0.000226303009090758,0.000242229148675566,
0.000258155288260374,0.000258291104876519,0.000327654633610232,0.000399363990826456,
0.000469709285177114,0.000516310576520749),.UNSPECIFIED.);
#4304=B_SPLINE_CURVE_WITH_KNOTS('',3,(#169951,#169952,#169953,#169954,#169955,
#169956,#169957,#169958,#169959,#169960,#169961,#169962,#169963,#169964,
#169965,#169966,#169967,#169968,#169969,#169970,#169971,#169972,#169973,
#169974,#169975,#169976,#169977,#169978,#169979,#169980,#169981,#169982,
#169983,#169984,#169985,#169986,#169987,#169988,#169989,#169990),
 .UNSPECIFIED.,.F.,.F.,(4,3,3,3,3,3,3,3,3,3,3,3,3,4),(0.,6.84564250862363E-5,
0.00013828840660365,0.000205407478943243,0.000256966021225853,0.000257101146970269,
0.000271589374668181,0.000352213067603087,0.000388398097499869,0.000404123622054952,
0.000459162957997745,0.000486682625969141,0.000500442459954839,0.000514202293940537),
 .UNSPECIFIED.);
#4305=B_SPLINE_CURVE_WITH_KNOTS('',3,(#169994,#169995,#169996,#169997,#169998,
#169999,#170000,#170001,#170002,#170003,#170004,#170005,#170006,#170007,
#170008,#170009,#170010,#170011,#170012,#170013,#170014,#170015,#170016,
#170017,#170018,#170019,#170020,#170021,#170022,#170023,#170024,#170025,
#170026,#170027,#170028,#170029,#170030,#170031,#170032,#170033,#170034,
#170035,#170036),.UNSPECIFIED.,.F.,.F.,(4,3,3,3,3,3,3,3,3,3,3,3,3,3,4),
(0.,1.12890698065816E-5,7.65259667227941E-5,0.000102837507928512,0.000112544869199253,
0.000130746171581893,0.000194450729921135,0.000226303009090755,0.000242229148675565,
0.000258155288260376,0.000258291104876516,0.000327654633614687,0.000399363990836629,
0.00046970928519338,0.000516310576520744),.UNSPECIFIED.);
#4306=B_SPLINE_CURVE_WITH_KNOTS('',3,(#170044,#170045,#170046,#170047,#170048,
#170049,#170050,#170051,#170052,#170053,#170054,#170055,#170056,#170057,
#170058,#170059,#170060,#170061,#170062,#170063,#170064,#170065,#170066,
#170067,#170068,#170069,#170070,#170071,#170072,#170073,#170074,#170075,
#170076,#170077,#170078,#170079,#170080,#170081,#170082,#170083),
 .UNSPECIFIED.,.F.,.F.,(4,3,3,3,3,3,3,3,3,3,3,3,3,4),(0.,6.84564250861885E-5,
0.000138288406603737,0.00020540747894416,0.000256966021225845,0.000257101146970264,
0.000271589374668171,0.000352213067589949,0.000388398097499864,0.000404123622054947,
0.000459162957997737,0.000486682625969132,0.00050044245995483,0.000514202293940528),
 .UNSPECIFIED.);
#4307=B_SPLINE_CURVE_WITH_KNOTS('',3,(#170087,#170088,#170089,#170090,#170091,
#170092,#170093,#170094,#170095,#170096,#170097,#170098,#170099,#170100,
#170101,#170102,#170103,#170104,#170105,#170106,#170107,#170108,#170109,
#170110,#170111,#170112,#170113,#170114,#170115,#170116,#170117,#170118,
#170119,#170120,#170121,#170122,#170123,#170124,#170125,#170126,#170127,
#170128,#170129),.UNSPECIFIED.,.F.,.F.,(4,3,3,3,3,3,3,3,3,3,3,3,3,3,4),
(0.,1.12890698065835E-5,7.65259666994345E-5,0.0001028375079285,0.000112544869199242,
0.000130746171581883,0.000194450729921126,0.000226303009090747,0.000242229148675558,
0.000258155288260369,0.00025829110487652,0.000327654633625233,0.000399363990857316,
0.000469709285222563,0.000516310576520737),.UNSPECIFIED.);
#4308=B_SPLINE_CURVE_WITH_KNOTS('',3,(#170137,#170138,#170139,#170140,#170141,
#170142,#170143,#170144,#170145,#170146,#170147,#170148,#170149,#170150,
#170151,#170152,#170153,#170154,#170155,#170156,#170157,#170158,#170159,
#170160,#170161,#170162,#170163,#170164,#170165,#170166,#170167,#170168,
#170169,#170170,#170171,#170172,#170173,#170174,#170175,#170176),
 .UNSPECIFIED.,.F.,.F.,(4,3,3,3,3,3,3,3,3,3,3,3,3,4),(0.,6.84564250829992E-5,
0.000138288406596676,0.000205407478932091,0.000256966021225855,0.000257101146970265,
0.000271589374668167,0.00035221306760733,0.000388398097499791,0.000404123622054884,
0.000459162957997707,0.000486682625969119,0.000500442459954825,0.000514202293940531),
 .UNSPECIFIED.);
#4309=B_SPLINE_CURVE_WITH_KNOTS('',3,(#170180,#170181,#170182,#170183,#170184,
#170185,#170186,#170187,#170188,#170189,#170190,#170191,#170192,#170193,
#170194,#170195,#170196,#170197,#170198,#170199,#170200,#170201,#170202,
#170203,#170204,#170205,#170206,#170207,#170208,#170209,#170210,#170211,
#170212,#170213,#170214,#170215,#170216,#170217,#170218,#170219,#170220,
#170221,#170222),.UNSPECIFIED.,.F.,.F.,(4,3,3,3,3,3,3,3,3,3,3,3,3,3,4),
(0.,1.12890698065865E-5,7.65259667007628E-5,0.000102837507928553,0.000112544869199292,
0.000130746171581927,0.000194450729921151,0.000226303009090763,0.000242229148675569,
0.000258155288260375,0.000258291104876515,0.000327654633620995,0.000399363990848543,
0.00046970928520939,0.00051631057652075),.UNSPECIFIED.);
#4310=B_SPLINE_CURVE_WITH_KNOTS('',3,(#170230,#170231,#170232,#170233,#170234,
#170235,#170236,#170237,#170238,#170239,#170240,#170241,#170242,#170243,
#170244,#170245,#170246,#170247,#170248,#170249,#170250,#170251,#170252,
#170253,#170254,#170255,#170256,#170257,#170258,#170259,#170260,#170261,
#170262,#170263,#170264,#170265,#170266,#170267,#170268,#170269),
 .UNSPECIFIED.,.F.,.F.,(4,3,3,3,3,3,3,3,3,3,3,3,3,4),(0.,6.84564250862226E-5,
0.000138288406603668,0.000205407478943698,0.00025696602122584,0.000257101146970262,
0.000271589374668167,0.000352213067598809,0.000388398097499793,0.000404123622054884,
0.000459162957997704,0.000486682625969114,0.000500442459954819,0.000514202293940524),
 .UNSPECIFIED.);
#4311=B_SPLINE_CURVE_WITH_KNOTS('',3,(#170273,#170274,#170275,#170276,#170277,
#170278,#170279,#170280,#170281,#170282,#170283,#170284,#170285,#170286,
#170287,#170288,#170289,#170290,#170291,#170292,#170293,#170294,#170295,
#170296,#170297,#170298,#170299,#170300,#170301,#170302,#170303,#170304,
#170305,#170306,#170307,#170308,#170309,#170310,#170311,#170312,#170313,
#170314,#170315),.UNSPECIFIED.,.F.,.F.,(4,3,3,3,3,3,3,3,3,3,3,3,3,3,4),
(0.,1.1289069806586E-5,7.65259667026302E-5,0.000102837507928521,0.000112544869199262,
0.000130746171581899,0.000194450729921131,0.000226303009090747,0.000242229148675555,
0.000258155288260363,0.000258291104876498,0.000327654633617347,0.000399363990841111,
0.000469709285198713,0.000516310576520727),.UNSPECIFIED.);
#4312=B_SPLINE_CURVE_WITH_KNOTS('',3,(#170323,#170324,#170325,#170326,#170327,
#170328,#170329,#170330,#170331,#170332,#170333,#170334,#170335,#170336,
#170337,#170338,#170339,#170340,#170341,#170342,#170343,#170344,#170345,
#170346,#170347,#170348,#170349,#170350,#170351,#170352,#170353,#170354,
#170355,#170356,#170357,#170358,#170359,#170360,#170361,#170362),
 .UNSPECIFIED.,.F.,.F.,(4,3,3,3,3,3,3,3,3,3,3,3,3,4),(0.,6.84564250893229E-5,
0.000138288406610045,0.000205407478953388,0.000256966021225841,0.000257101146970263,
0.00027158937466816,0.000352213067592389,0.000388398097499739,0.000404123622054837,
0.000459162957997681,0.000486682625969103,0.000500442459954814,0.000514202293940525),
 .UNSPECIFIED.);
#4313=B_SPLINE_CURVE_WITH_KNOTS('',3,(#170366,#170367,#170368,#170369,#170370,
#170371,#170372,#170373,#170374,#170375,#170376,#170377,#170378,#170379,
#170380,#170381,#170382,#170383,#170384,#170385,#170386,#170387,#170388,
#170389,#170390,#170391,#170392,#170393,#170394,#170395,#170396,#170397,
#170398,#170399,#170400,#170401,#170402,#170403,#170404,#170405,#170406,
#170407,#170408),.UNSPECIFIED.,.F.,.F.,(4,3,3,3,3,3,3,3,3,3,3,3,3,3,4),
(0.,1.12890698065853E-5,7.6525966706682E-5,0.000102837507928526,0.000112544869199267,
0.000130746171581906,0.000194450729921142,0.00022630300909076,0.000242229148675569,
0.000258155288260379,0.000258291104876522,0.000327654633611439,0.000399363990829307,
0.000469709285181712,0.000516310576520757),.UNSPECIFIED.);
#4314=B_SPLINE_CURVE_WITH_KNOTS('',3,(#170415,#170416,#170417,#170418,#170419,
#170420,#170421,#170422,#170423,#170424,#170425,#170426,#170427,#170428,
#170429,#170430,#170431,#170432,#170433,#170434,#170435,#170436,#170437,
#170438,#170439,#170440,#170441,#170442,#170443,#170444,#170445,#170446,
#170447,#170448,#170449,#170450,#170451,#170452,#170453,#170454),
 .UNSPECIFIED.,.F.,.F.,(4,3,3,3,3,3,3,3,3,3,3,3,3,4),(0.,6.84564250828479E-5,
0.000138288406596811,0.000205407478933446,0.000256966021225857,0.000257101146970263,
0.000271589374668171,0.000352213067600988,0.000388398097499851,0.000404123622054936,
0.000459162957997731,0.000486682625969128,0.000500442459954827,0.000514202293940526),
 .UNSPECIFIED.);
#4315=B_SPLINE_CURVE_WITH_KNOTS('',3,(#170457,#170458,#170459,#170460,#170461,
#170462,#170463,#170464,#170465,#170466,#170467,#170468,#170469,#170470,
#170471,#170472,#170473,#170474,#170475,#170476,#170477,#170478,#170479,
#170480,#170481,#170482,#170483,#170484,#170485,#170486,#170487,#170488,
#170489,#170490,#170491,#170492,#170493,#170494,#170495,#170496,#170497,
#170498,#170499),.UNSPECIFIED.,.F.,.F.,(4,3,3,3,3,3,3,3,3,3,3,3,3,3,4),
(0.,1.1289069806584E-5,7.65259667159113E-5,0.000102837507928536,0.000112544869199276,
0.000130746171581913,0.000194450729921141,0.000226303009090755,0.000242229148675562,
0.000258155288260369,0.000258291104876519,0.000327654633610196,0.000399363990826946,
0.000469709285178442,0.000516310576520737),.UNSPECIFIED.);
#4316=B_SPLINE_CURVE_WITH_KNOTS('',3,(#170507,#170508,#170509,#170510,#170511,
#170512,#170513,#170514,#170515,#170516,#170517,#170518,#170519,#170520,
#170521,#170522,#170523,#170524,#170525,#170526,#170527,#170528,#170529,
#170530,#170531,#170532,#170533,#170534,#170535,#170536,#170537,#170538,
#170539,#170540,#170541,#170542,#170543,#170544,#170545,#170546),
 .UNSPECIFIED.,.F.,.F.,(4,3,3,3,3,3,3,3,3,3,3,3,3,4),(0.,6.84564250954211E-5,
0.000138288406622434,0.000205407478971246,0.000256966021225848,0.000257101146970262,
0.000271589374668172,0.000352213067604716,0.000388398097499863,0.000404123622054945,
0.000459162957997735,0.000486682625969129,0.000500442459954827,0.000514202293940524),
 .UNSPECIFIED.);
#4317=B_SPLINE_CURVE_WITH_KNOTS('',3,(#170550,#170551,#170552,#170553,#170554,
#170555,#170556,#170557,#170558,#170559,#170560,#170561,#170562,#170563,
#170564,#170565,#170566,#170567,#170568,#170569,#170570,#170571,#170572,
#170573,#170574,#170575,#170576,#170577,#170578,#170579,#170580,#170581,
#170582,#170583,#170584,#170585,#170586,#170587,#170588,#170589,#170590,
#170591,#170592),.UNSPECIFIED.,.F.,.F.,(4,3,3,3,3,3,3,3,3,3,3,3,3,3,4),
(0.,1.1289069806583E-5,7.65259667103485E-5,0.000102837507928521,0.000112544869199261,
0.0001307461715819,0.000194450729921134,0.000226303009090751,0.00024222914867556,
0.000258155288260369,0.000258291104876502,0.000327654633618343,0.000399363990843429,
0.000469709285202199,0.000516310576520737),.UNSPECIFIED.);
#4318=B_SPLINE_CURVE_WITH_KNOTS('',3,(#170600,#170601,#170602,#170603,#170604,
#170605,#170606,#170607,#170608,#170609,#170610,#170611,#170612,#170613,
#170614,#170615,#170616,#170617,#170618,#170619,#170620,#170621,#170622,
#170623,#170624,#170625,#170626,#170627,#170628,#170629,#170630,#170631,
#170632,#170633,#170634,#170635,#170636,#170637,#170638,#170639),
 .UNSPECIFIED.,.F.,.F.,(4,3,3,3,3,3,3,3,3,3,3,3,3,4),(0.,6.84564250890799E-5,
0.000138288406609806,0.000205407478953346,0.000256966021225843,0.000257101146970264,
0.00027158937466816,0.000352213067600159,0.000388398097499754,0.00040412362205485,
0.000459162957997689,0.000486682625969108,0.000500442459954818,0.000514202293940527),
 .UNSPECIFIED.);
#4319=B_SPLINE_CURVE_WITH_KNOTS('',3,(#170643,#170644,#170645,#170646,#170647,
#170648,#170649,#170650,#170651,#170652,#170653,#170654,#170655,#170656,
#170657,#170658,#170659,#170660,#170661,#170662,#170663,#170664,#170665,
#170666,#170667,#170668,#170669,#170670,#170671,#170672,#170673,#170674,
#170675,#170676,#170677,#170678,#170679,#170680,#170681,#170682,#170683,
#170684,#170685),.UNSPECIFIED.,.F.,.F.,(4,3,3,3,3,3,3,3,3,3,3,3,3,3,4),
(0.,1.12890698065784E-5,7.65259667110566E-5,0.000102837507928478,0.000112544869199221,
0.000130746171581864,0.000194450729921115,0.00022630300909074,0.000242229148675553,
0.000258155288260366,0.000258291104876503,0.000327654633619958,0.000399363990846323,
0.000469709285205513,0.000516310576520731),.UNSPECIFIED.);
#4320=B_SPLINE_CURVE_WITH_KNOTS('',3,(#170693,#170694,#170695,#170696,#170697,
#170698,#170699,#170700,#170701,#170702,#170703,#170704,#170705,#170706,
#170707,#170708,#170709,#170710,#170711,#170712,#170713,#170714,#170715,
#170716,#170717,#170718,#170719,#170720,#170721,#170722,#170723,#170724,
#170725,#170726,#170727,#170728,#170729,#170730,#170731,#170732),
 .UNSPECIFIED.,.F.,.F.,(4,3,3,3,3,3,3,3,3,3,3,3,3,4),(0.,6.84564250865478E-5,
0.000138288406603928,0.000205407478942991,0.000256966021225854,0.00025710114697026,
0.000271589374668167,0.000352213067606407,0.000388398097499869,0.000404123622054951,
0.000459162957997736,0.000486682625969128,0.000500442459954825,0.000514202293940521),
 .UNSPECIFIED.);
#4321=B_SPLINE_CURVE_WITH_KNOTS('',3,(#170736,#170737,#170738,#170739,#170740,
#170741,#170742,#170743,#170744,#170745,#170746,#170747,#170748,#170749,
#170750,#170751,#170752,#170753,#170754,#170755,#170756,#170757,#170758,
#170759,#170760,#170761,#170762,#170763,#170764,#170765,#170766,#170767,
#170768,#170769,#170770,#170771,#170772,#170773,#170774,#170775,#170776,
#170777,#170778),.UNSPECIFIED.,.F.,.F.,(4,3,3,3,3,3,3,3,3,3,3,3,3,3,4),
(0.,1.12890698065819E-5,7.65259667075592E-5,0.000102837507928482,0.000112544869199225,
0.000130746171581869,0.000194450729921122,0.000226303009090748,0.000242229148675561,
0.000258155288260374,0.000258291104876516,0.000327654633605226,0.000399363990816631,
0.000469709285163391,0.000516310576520749),.UNSPECIFIED.);
#4322=B_SPLINE_CURVE_WITH_KNOTS('',3,(#170786,#170787,#170788,#170789,#170790,
#170791,#170792,#170793,#170794,#170795,#170796,#170797,#170798,#170799,
#170800,#170801,#170802,#170803,#170804,#170805,#170806,#170807,#170808,
#170809,#170810,#170811,#170812,#170813,#170814,#170815,#170816,#170817,
#170818,#170819,#170820,#170821,#170822,#170823,#170824,#170825),
 .UNSPECIFIED.,.F.,.F.,(4,3,3,3,3,3,3,3,3,3,3,3,3,4),(0.,6.84564250871706E-5,
0.000138288406605827,0.000205407478946739,0.000256966021225855,0.000257101146970261,
0.000271589374668165,0.000352213067617463,0.000388398097499751,0.000404123622054848,
0.000459162957997684,0.000486682625969103,0.000500442459954812,0.000514202293940521),
 .UNSPECIFIED.);
#4323=B_SPLINE_CURVE_WITH_KNOTS('',3,(#170829,#170830,#170831,#170832,#170833,
#170834,#170835,#170836,#170837,#170838,#170839,#170840,#170841,#170842,
#170843,#170844,#170845,#170846,#170847,#170848,#170849,#170850,#170851,
#170852,#170853,#170854,#170855,#170856,#170857,#170858,#170859,#170860,
#170861,#170862,#170863,#170864,#170865,#170866,#170867,#170868,#170869,
#170870,#170871),.UNSPECIFIED.,.F.,.F.,(4,3,3,3,3,3,3,3,3,3,3,3,3,3,4),
(0.,1.12890698065823E-5,7.65259667154223E-5,0.000102837507928501,0.000112544869199243,
0.000130746171581885,0.000194450729921131,0.000226303009090754,0.000242229148675565,
0.000258155288260377,0.000258291104876513,0.000327654633611621,0.000399363990829974,
0.000469709285183087,0.000516310576520753),.UNSPECIFIED.);
#4324=B_SPLINE_CURVE_WITH_KNOTS('',3,(#170879,#170880,#170881,#170882,#170883,
#170884,#170885,#170886,#170887,#170888,#170889,#170890,#170891,#170892,
#170893,#170894,#170895,#170896,#170897,#170898,#170899,#170900,#170901,
#170902,#170903,#170904,#170905,#170906,#170907,#170908,#170909,#170910,
#170911,#170912,#170913,#170914,#170915,#170916,#170917,#170918),
 .UNSPECIFIED.,.F.,.F.,(4,3,3,3,3,3,3,3,3,3,3,3,3,4),(0.,6.84564250850767E-5,
0.000138288406600822,0.000205407478937571,0.000256966021225869,0.000257101146970269,
0.00027158937466817,0.000352213067610346,0.000388398097499747,0.000404123622054845,
0.000459162957997688,0.000486682625969109,0.00050044245995482,0.000514202293940531),
 .UNSPECIFIED.);
#4325=B_SPLINE_CURVE_WITH_KNOTS('',3,(#170922,#170923,#170924,#170925,#170926,
#170927,#170928,#170929,#170930,#170931,#170932,#170933,#170934,#170935,
#170936,#170937,#170938,#170939,#170940,#170941,#170942,#170943,#170944,
#170945,#170946,#170947,#170948,#170949,#170950,#170951,#170952,#170953,
#170954,#170955,#170956,#170957,#170958,#170959,#170960,#170961,#170962,
#170963,#170964),.UNSPECIFIED.,.F.,.F.,(4,3,3,3,3,3,3,3,3,3,3,3,3,3,4),
(0.,1.12890698065787E-5,7.65259667143295E-5,0.00010283750792846,0.000112544869199205,
0.000130746171581851,0.000194450729921113,0.000226303009090744,0.000242229148675559,
0.000258155288260375,0.00025829110487651,0.000327654633621617,0.000399363990849291,
0.000469709285208686,0.00051631057652075),.UNSPECIFIED.);
#4326=B_SPLINE_CURVE_WITH_KNOTS('',3,(#170972,#170973,#170974,#170975,#170976,
#170977,#170978,#170979,#170980,#170981,#170982,#170983,#170984,#170985,
#170986,#170987,#170988,#170989,#170990,#170991,#170992,#170993,#170994,
#170995,#170996,#170997,#170998,#170999,#171000,#171001,#171002,#171003,
#171004,#171005,#171006,#171007,#171008,#171009,#171010,#171011),
 .UNSPECIFIED.,.F.,.F.,(4,3,3,3,3,3,3,3,3,3,3,3,3,4),(0.,6.84564250915387E-5,
0.00013828840661381,0.000205407478957333,0.00025696602122584,0.000257101146970264,
0.000271589374668166,0.000352213067592918,0.000388398097499716,0.000404123622054817,
0.000459162957997673,0.000486682625969101,0.000500442459954815,0.000514202293940529),
 .UNSPECIFIED.);
#4327=B_SPLINE_CURVE_WITH_KNOTS('',3,(#171015,#171016,#171017,#171018,#171019,
#171020,#171021,#171022,#171023,#171024,#171025,#171026,#171027,#171028,
#171029,#171030,#171031,#171032,#171033,#171034,#171035,#171036,#171037,
#171038,#171039,#171040,#171041,#171042,#171043,#171044,#171045,#171046,
#171047,#171048,#171049,#171050,#171051,#171052,#171053,#171054,#171055,
#171056,#171057),.UNSPECIFIED.,.F.,.F.,(4,3,3,3,3,3,3,3,3,3,3,3,3,3,4),
(0.,1.128906980658E-5,7.65259667093686E-5,0.00010283750792849,0.000112544869199233,
0.000130746171581876,0.000194450729921126,0.000226303009090751,0.000242229148675563,
0.000258155288260376,0.000258291104876518,0.00032765463361249,0.000399363990831544,
0.000469709285185222,0.000516310576520752),.UNSPECIFIED.);
#4328=B_SPLINE_CURVE_WITH_KNOTS('',3,(#171065,#171066,#171067,#171068,#171069,
#171070,#171071,#171072,#171073,#171074,#171075,#171076,#171077,#171078,
#171079,#171080,#171081,#171082,#171083,#171084,#171085,#171086,#171087,
#171088,#171089,#171090,#171091,#171092,#171093,#171094,#171095,#171096,
#171097,#171098,#171099,#171100,#171101,#171102,#171103,#171104),
 .UNSPECIFIED.,.F.,.F.,(4,3,3,3,3,3,3,3,3,3,3,3,3,4),(0.,6.84564250730484E-5,
0.000138288406575729,0.000205407478898954,0.000256966021225863,0.000257101146970266,
0.000271589374668165,0.000352213067626712,0.000388398097499794,0.000404123622054886,
0.000459162957997709,0.00048668262596912,0.000500442459954826,0.000514202293940531),
 .UNSPECIFIED.);
#4329=B_SPLINE_CURVE_WITH_KNOTS('',3,(#171108,#171109,#171110,#171111,#171112,
#171113,#171114,#171115,#171116,#171117,#171118,#171119,#171120,#171121,
#171122,#171123,#171124,#171125,#171126,#171127,#171128,#171129,#171130,
#171131,#171132,#171133,#171134,#171135,#171136,#171137,#171138,#171139,
#171140,#171141,#171142,#171143,#171144,#171145,#171146,#171147,#171148,
#171149,#171150),.UNSPECIFIED.,.F.,.F.,(4,3,3,3,3,3,3,3,3,3,3,3,3,3,4),
(0.,1.12890698065735E-5,7.65259666964498E-5,0.000102837507928437,0.000112544869199182,
0.000130746171581831,0.000194450729921099,0.000226303009090734,0.000242229148675551,
0.000258155288260368,0.000258291104876531,0.000327654633628666,0.00039936399086441,
0.000469709285233363,0.000516310576520736),.UNSPECIFIED.);
#4330=B_SPLINE_CURVE_WITH_KNOTS('',3,(#171158,#171159,#171160,#171161,#171162,
#171163,#171164,#171165,#171166,#171167,#171168,#171169,#171170,#171171,
#171172,#171173,#171174,#171175,#171176,#171177,#171178,#171179,#171180,
#171181,#171182,#171183,#171184,#171185,#171186,#171187,#171188,#171189,
#171190,#171191,#171192,#171193,#171194,#171195,#171196,#171197),
 .UNSPECIFIED.,.F.,.F.,(4,3,3,3,3,3,3,3,3,3,3,3,3,4),(0.,6.84564250925084E-5,
0.000138288406615908,0.000205407478960095,0.000256966021225855,0.000257101146970265,
0.000271589374668168,0.000352213067604673,0.000388398097499809,0.000404123622054899,
0.000459162957997714,0.000486682625969122,0.000500442459954826,0.00051420229394053),
 .UNSPECIFIED.);
#4331=B_SPLINE_CURVE_WITH_KNOTS('',3,(#171201,#171202,#171203,#171204,#171205,
#171206,#171207,#171208,#171209,#171210,#171211,#171212,#171213,#171214,
#171215,#171216,#171217,#171218,#171219,#171220,#171221,#171222,#171223,
#171224,#171225,#171226,#171227,#171228,#171229,#171230,#171231,#171232,
#171233,#171234,#171235,#171236,#171237,#171238,#171239,#171240,#171241,
#171242,#171243),.UNSPECIFIED.,.F.,.F.,(4,3,3,3,3,3,3,3,3,3,3,3,3,3,4),
(0.,1.12890698065805E-5,7.65259667133678E-5,0.000102837507928527,0.000112544869199267,
0.000130746171581905,0.000194450729921139,0.000226303009090756,0.000242229148675565,
0.000258155288260373,0.000258291104876516,0.000327654633621551,0.00039936399085004,
0.000469709285212181,0.000516310576520747),.UNSPECIFIED.);
#4332=B_SPLINE_CURVE_WITH_KNOTS('',3,(#171251,#171252,#171253,#171254,#171255,
#171256,#171257,#171258,#171259,#171260,#171261,#171262,#171263,#171264,
#171265,#171266,#171267,#171268,#171269,#171270,#171271,#171272,#171273,
#171274,#171275,#171276,#171277,#171278,#171279,#171280,#171281,#171282,
#171283,#171284,#171285,#171286,#171287,#171288,#171289,#171290),
 .UNSPECIFIED.,.F.,.F.,(4,3,3,3,3,3,3,3,3,3,3,3,3,4),(0.,6.84564250780475E-5,
0.000138288406587184,0.000205407478918763,0.000256966021225858,0.000257101146970266,
0.000271589374668172,0.000352213067616118,0.000388398097499824,0.000404123622054913,
0.000459162957997722,0.000486682625969127,0.000500442459954829,0.000514202293940532),
 .UNSPECIFIED.);
#4333=B_SPLINE_CURVE_WITH_KNOTS('',3,(#171294,#171295,#171296,#171297,#171298,
#171299,#171300,#171301,#171302,#171303,#171304,#171305,#171306,#171307,
#171308,#171309,#171310,#171311,#171312,#171313,#171314,#171315,#171316,
#171317,#171318,#171319,#171320,#171321,#171322,#171323,#171324,#171325,
#171326,#171327,#171328,#171329,#171330,#171331,#171332,#171333,#171334,
#171335,#171336),.UNSPECIFIED.,.F.,.F.,(4,3,3,3,3,3,3,3,3,3,3,3,3,3,4),
(0.,1.12890698065829E-5,7.6525966699166E-5,0.000102837507928514,0.000112544869199255,
0.000130746171581894,0.000194450729921133,0.000226303009090753,0.000242229148675562,
0.000258155288260372,0.00025829110487651,0.0003276546336249,0.000399363990855324,
0.000469709285217151,0.000516310576520744),.UNSPECIFIED.);
#4334=B_SPLINE_CURVE_WITH_KNOTS('',3,(#171344,#171345,#171346,#171347,#171348,
#171349,#171350,#171351,#171352,#171353,#171354,#171355,#171356,#171357,
#171358,#171359,#171360,#171361,#171362,#171363,#171364,#171365,#171366,
#171367,#171368,#171369,#171370,#171371,#171372,#171373,#171374,#171375,
#171376,#171377,#171378,#171379,#171380,#171381,#171382,#171383),
 .UNSPECIFIED.,.F.,.F.,(4,3,3,3,3,3,3,3,3,3,3,3,3,4),(1.34144585567483E-17,
6.84564250925487E-5,0.000138288406616583,0.000205407478962631,0.000256966021225856,
0.000257101146970265,0.000271589374668168,0.00035221306759979,0.000388398097499808,
0.000404123622054899,0.000459162957997714,0.000486682625969122,0.000500442459954826,
0.00051420229394053),.UNSPECIFIED.);
#4335=B_SPLINE_CURVE_WITH_KNOTS('',3,(#171387,#171388,#171389,#171390,#171391,
#171392,#171393,#171394,#171395,#171396,#171397,#171398,#171399,#171400,
#171401,#171402,#171403,#171404,#171405,#171406,#171407,#171408,#171409,
#171410,#171411,#171412,#171413,#171414,#171415,#171416,#171417,#171418,
#171419,#171420,#171421,#171422,#171423,#171424,#171425,#171426,#171427,
#171428,#171429),.UNSPECIFIED.,.F.,.F.,(4,3,3,3,3,3,3,3,3,3,3,3,3,3,4),
(0.,1.12890698065832E-5,7.65259667081792E-5,0.000102837507928538,0.000112544869199278,
0.000130746171581915,0.000194450729921144,0.000226303009090759,0.000242229148675566,
0.000258155288260373,0.000258291104876514,0.000327654633623112,0.000399363990853129,
0.00046970928521632,0.000516310576520746),.UNSPECIFIED.);
#4336=B_SPLINE_CURVE_WITH_KNOTS('',3,(#171437,#171438,#171439,#171440,#171441,
#171442,#171443,#171444,#171445,#171446,#171447,#171448,#171449,#171450,
#171451,#171452,#171453,#171454,#171455,#171456,#171457,#171458,#171459,
#171460,#171461,#171462,#171463,#171464,#171465,#171466,#171467,#171468,
#171469,#171470,#171471,#171472,#171473,#171474,#171475,#171476),
 .UNSPECIFIED.,.F.,.F.,(4,3,3,3,3,3,3,3,3,3,3,3,3,4),(0.,6.84564250775598E-5,
0.000138288406585897,0.000205407478917233,0.000256966021225855,0.000257101146970263,
0.000271589374668167,0.000352213067595873,0.000388398097499834,0.000404123622054921,
0.000459162957997723,0.000486682625969125,0.000500442459954825,0.000514202293940526),
 .UNSPECIFIED.);
#4337=B_SPLINE_CURVE_WITH_KNOTS('',3,(#171480,#171481,#171482,#171483,#171484,
#171485,#171486,#171487,#171488,#171489,#171490,#171491,#171492,#171493,
#171494,#171495,#171496,#171497,#171498,#171499,#171500,#171501,#171502,
#171503,#171504,#171505,#171506,#171507,#171508,#171509,#171510,#171511,
#171512,#171513,#171514,#171515,#171516,#171517,#171518,#171519,#171520,
#171521,#171522),.UNSPECIFIED.,.F.,.F.,(4,3,3,3,3,3,3,3,3,3,3,3,3,3,4),
(0.,1.1289069806584E-5,7.65259667025282E-5,0.000102837507928508,0.00011254486919925,
0.000130746171581889,0.000194450729921128,0.000226303009090748,0.000242229148675557,
0.000258155288260367,0.000258291104876519,0.000327654633616274,0.000399363990838822,
0.000469709285195002,0.000516310576520734),.UNSPECIFIED.);
#4338=B_SPLINE_CURVE_WITH_KNOTS('',3,(#171530,#171531,#171532,#171533,#171534,
#171535,#171536,#171537,#171538,#171539,#171540,#171541,#171542,#171543,
#171544,#171545,#171546,#171547,#171548,#171549,#171550,#171551,#171552,
#171553,#171554,#171555,#171556,#171557,#171558,#171559,#171560,#171561,
#171562,#171563,#171564,#171565,#171566,#171567,#171568,#171569),
 .UNSPECIFIED.,.F.,.F.,(4,3,3,3,3,3,3,3,3,3,3,3,3,4),(0.,6.84564250757926E-5,
0.000138288406582254,0.000205407478911281,0.000256966021225868,0.000257101146970264,
0.00027158937466817,0.000352213067604392,0.000388398097499803,0.000404123622054894,
0.000459162957997711,0.00048668262596912,0.000500442459954824,0.000514202293940529),
 .UNSPECIFIED.);
#4339=B_SPLINE_CURVE_WITH_KNOTS('',3,(#171573,#171574,#171575,#171576,#171577,
#171578,#171579,#171580,#171581,#171582,#171583,#171584,#171585,#171586,
#171587,#171588,#171589,#171590,#171591,#171592,#171593,#171594,#171595,
#171596,#171597,#171598,#171599,#171600,#171601,#171602,#171603,#171604,
#171605,#171606,#171607,#171608,#171609,#171610,#171611,#171612,#171613,
#171614,#171615),.UNSPECIFIED.,.F.,.F.,(4,3,3,3,3,3,3,3,3,3,3,3,3,3,4),
(0.,1.12890698065807E-5,7.65259667028005E-5,0.000102837507928501,0.000112544869199243,
0.000130746171581885,0.00019445072992113,0.000226303009090753,0.000242229148675564,
0.000258155288260375,0.00025829110487652,0.000327654633608315,0.000399363990823035,
0.00046970928517307,0.00051631057652075),.UNSPECIFIED.);
#4340=B_SPLINE_CURVE_WITH_KNOTS('',3,(#171623,#171624,#171625,#171626,#171627,
#171628,#171629,#171630,#171631,#171632,#171633,#171634,#171635,#171636,
#171637,#171638,#171639,#171640,#171641,#171642,#171643,#171644,#171645,
#171646,#171647,#171648,#171649,#171650,#171651,#171652,#171653,#171654,
#171655,#171656,#171657,#171658,#171659,#171660,#171661,#171662),
 .UNSPECIFIED.,.F.,.F.,(4,3,3,3,3,3,3,3,3,3,3,3,3,4),(0.,6.84564250793529E-5,
0.000138288406589974,0.000205407478923682,0.000256966021225855,0.000257101146970264,
0.000271589374668171,0.000352213067612092,0.000388398097499841,0.000404123622054927,
0.000459162957997727,0.000486682625969127,0.000500442459954827,0.000514202293940527),
 .UNSPECIFIED.);
#4341=B_SPLINE_CURVE_WITH_KNOTS('',3,(#171666,#171667,#171668,#171669,#171670,
#171671,#171672,#171673,#171674,#171675,#171676,#171677,#171678,#171679,
#171680,#171681,#171682,#171683,#171684,#171685,#171686,#171687,#171688,
#171689,#171690,#171691,#171692,#171693,#171694,#171695,#171696,#171697,
#171698,#171699,#171700,#171701,#171702,#171703,#171704,#171705,#171706,
#171707,#171708),.UNSPECIFIED.,.F.,.F.,(4,3,3,3,3,3,3,3,3,3,3,3,3,3,4),
(1.73472347597681E-18,1.1289069806582E-5,7.65259666980292E-5,0.000102837507928463,
0.000112544869199207,0.000130746171581853,0.000194450729921112,0.000226303009090742,
0.000242229148675557,0.000258155288260371,0.00025829110487652,0.000327654633617188,
0.000399363990840792,0.00046970928519829,0.000516310576520741),
 .UNSPECIFIED.);
#4342=B_SPLINE_CURVE_WITH_KNOTS('',3,(#171716,#171717,#171718,#171719,#171720,
#171721,#171722,#171723,#171724,#171725,#171726,#171727,#171728,#171729,
#171730,#171731,#171732,#171733,#171734,#171735,#171736,#171737,#171738,
#171739,#171740,#171741,#171742,#171743,#171744,#171745,#171746,#171747,
#171748,#171749,#171750,#171751,#171752,#171753,#171754,#171755),
 .UNSPECIFIED.,.F.,.F.,(4,3,3,3,3,3,3,3,3,3,3,3,3,4),(0.,6.84564250891977E-5,
0.00013828840660983,0.000205407478953017,0.000256966021225848,0.000257101146970265,
0.000271589374668171,0.000352213067589024,0.000388398097499806,0.000404123622054896,
0.000459162957997713,0.000486682625969122,0.000500442459954826,0.000514202293940531),
 .UNSPECIFIED.);
#4343=B_SPLINE_CURVE_WITH_KNOTS('',3,(#171759,#171760,#171761,#171762,#171763,
#171764,#171765,#171766,#171767,#171768,#171769,#171770,#171771,#171772,
#171773,#171774,#171775,#171776,#171777,#171778,#171779,#171780,#171781,
#171782,#171783,#171784,#171785,#171786,#171787,#171788,#171789,#171790,
#171791,#171792,#171793,#171794,#171795,#171796,#171797,#171798,#171799,
#171800,#171801),.UNSPECIFIED.,.F.,.F.,(4,3,3,3,3,3,3,3,3,3,3,3,3,3,4),
(0.,1.12890698065773E-5,7.65259666988184E-5,0.000102837507928458,0.000112544869199202,
0.000130746171581848,0.00019445072992111,0.00022630300909074,0.000242229148675555,
0.000258155288260371,0.00025829110487651,0.000327654633612431,0.000399363990831073,
0.000469709285184065,0.000516310576520741),.UNSPECIFIED.);
#4344=B_SPLINE_CURVE_WITH_KNOTS('',3,(#171808,#171809,#171810,#171811,#171812,
#171813,#171814,#171815,#171816,#171817,#171818,#171819,#171820,#171821,
#171822,#171823,#171824,#171825,#171826,#171827,#171828,#171829,#171830,
#171831,#171832,#171833,#171834,#171835,#171836,#171837,#171838,#171839,
#171840,#171841,#171842,#171843,#171844,#171845,#171846,#171847),
 .UNSPECIFIED.,.F.,.F.,(4,3,3,3,3,3,3,3,3,3,3,3,3,4),(0.,6.84564250836823E-5,
0.000138288406598479,0.00020540747893587,0.000256966021225843,0.000257101146970263,
0.000271589374668168,0.000352213067600198,0.000388398097499801,0.000404123622054892,
0.000459162957997709,0.000486682625969117,0.000500442459954822,0.000514202293940526),
 .UNSPECIFIED.);
#4345=B_SPLINE_CURVE_WITH_KNOTS('',3,(#171849,#171850,#171851,#171852,#171853,
#171854,#171855,#171856,#171857,#171858,#171859,#171860,#171861,#171862,
#171863,#171864,#171865,#171866,#171867,#171868,#171869,#171870,#171871,
#171872,#171873,#171874,#171875,#171876,#171877,#171878,#171879,#171880,
#171881,#171882,#171883,#171884,#171885,#171886,#171887,#171888,#171889,
#171890,#171891),.UNSPECIFIED.,.F.,.F.,(4,3,3,3,3,3,3,3,3,3,3,3,3,3,4),
(0.,1.12890698065822E-5,7.65259667098589E-5,0.000102837507928504,0.000112544869199245,
0.000130746171581886,0.000194450729921127,0.000226303009090747,0.000242229148675558,
0.000258155288260368,0.000258291104876532,0.00032765463361062,0.000399363990827817,
0.00046970928517974,0.000516310576520736),.UNSPECIFIED.);
#4346=B_SPLINE_CURVE_WITH_KNOTS('',3,(#171899,#171900,#171901,#171902,#171903,
#171904,#171905,#171906,#171907,#171908,#171909,#171910,#171911,#171912,
#171913,#171914,#171915,#171916,#171917,#171918,#171919,#171920,#171921,
#171922,#171923,#171924,#171925,#171926,#171927,#171928,#171929,#171930,
#171931,#171932,#171933,#171934,#171935,#171936,#171937,#171938),
 .UNSPECIFIED.,.F.,.F.,(4,3,3,3,3,3,3,3,3,3,3,3,3,4),(1.21218245568944E-17,
6.8456425089051E-5,0.000138288406609231,0.000205407478951254,0.000256966021225852,
0.000257101146970263,0.000271589374668161,0.000352213067605418,0.000388398097499745,
0.000404123622054843,0.000459162957997685,0.000486682625969105,0.000500442459954816,
0.000514202293940526),.UNSPECIFIED.);
#4347=B_SPLINE_CURVE_WITH_KNOTS('',3,(#171942,#171943,#171944,#171945,#171946,
#171947,#171948,#171949,#171950,#171951,#171952,#171953,#171954,#171955,
#171956,#171957,#171958,#171959,#171960,#171961,#171962,#171963,#171964,
#171965,#171966,#171967,#171968,#171969,#171970,#171971,#171972,#171973,
#171974,#171975,#171976,#171977,#171978,#171979,#171980,#171981,#171982,
#171983,#171984),.UNSPECIFIED.,.F.,.F.,(4,3,3,3,3,3,3,3,3,3,3,3,3,3,4),
(0.,1.12890698065851E-5,7.65259667091874E-5,0.000102837507928538,0.000112544869199278,
0.000130746171581915,0.000194450729921143,0.000226303009090758,0.000242229148675565,
0.000258155288260372,0.000258291104876525,0.000327654633618784,0.000399363990844283,
0.000469709285203434,0.000516310576520733),.UNSPECIFIED.);
#4348=B_SPLINE_CURVE_WITH_KNOTS('',3,(#171992,#171993,#171994,#171995,#171996,
#171997,#171998,#171999,#172000,#172001,#172002,#172003,#172004,#172005,
#172006,#172007,#172008,#172009,#172010,#172011,#172012,#172013,#172014,
#172015,#172016,#172017,#172018,#172019,#172020,#172021,#172022,#172023,
#172024,#172025,#172026,#172027,#172028,#172029,#172030,#172031),
 .UNSPECIFIED.,.F.,.F.,(4,3,3,3,3,3,3,3,3,3,3,3,3,4),(0.,6.84564250868887E-5,
0.000138288406605147,0.000205407478945967,0.000256966021225847,0.000257101146970261,
0.000271589374668168,0.000352213067598293,0.000388398097499808,0.000404123622054897,
0.00045916295799771,0.000486682625969116,0.000500442459954819,0.000514202293940523),
 .UNSPECIFIED.);
#4349=B_SPLINE_CURVE_WITH_KNOTS('',3,(#172035,#172036,#172037,#172038,#172039,
#172040,#172041,#172042,#172043,#172044,#172045,#172046,#172047,#172048,
#172049,#172050,#172051,#172052,#172053,#172054,#172055,#172056,#172057,
#172058,#172059,#172060,#172061,#172062,#172063,#172064,#172065,#172066,
#172067,#172068,#172069,#172070,#172071,#172072,#172073,#172074,#172075,
#172076,#172077),.UNSPECIFIED.,.F.,.F.,(4,3,3,3,3,3,3,3,3,3,3,3,3,3,4),
(0.,1.12890698065767E-5,7.65259667144555E-5,0.000102837507928448,0.000112544869199193,
0.000130746171581841,0.000194450729921109,0.000226303009090742,0.000242229148675559,
0.000258155288260376,0.000258291104876509,0.00032765463361531,0.000399363990837435,
0.000469709285193806,0.000516310576520752),.UNSPECIFIED.);
#4350=B_SPLINE_CURVE_WITH_KNOTS('',3,(#172085,#172086,#172087,#172088,#172089,
#172090,#172091,#172092,#172093,#172094,#172095,#172096,#172097,#172098,
#172099,#172100,#172101,#172102,#172103,#172104,#172105,#172106,#172107,
#172108,#172109,#172110,#172111,#172112,#172113,#172114,#172115,#172116,
#172117,#172118,#172119,#172120,#172121,#172122,#172123,#172124),
 .UNSPECIFIED.,.F.,.F.,(4,3,3,3,3,3,3,3,3,3,3,3,3,4),(0.,6.84564250823883E-5,
0.000138288406596485,0.000205407478933699,0.000256966021225852,0.00025710114697026,
0.000271589374668168,0.000352213067613843,0.000388398097499785,0.000404123622054877,
0.000459162957997698,0.000486682625969109,0.000500442459954814,0.000514202293940519),
 .UNSPECIFIED.);
#4351=B_SPLINE_CURVE_WITH_KNOTS('',3,(#172128,#172129,#172130,#172131,#172132,
#172133,#172134,#172135,#172136,#172137,#172138,#172139,#172140,#172141,
#172142,#172143,#172144,#172145,#172146,#172147,#172148,#172149,#172150,
#172151,#172152,#172153,#172154,#172155,#172156,#172157,#172158,#172159,
#172160,#172161,#172162,#172163,#172164,#172165,#172166,#172167,#172168,
#172169,#172170),.UNSPECIFIED.,.F.,.F.,(4,3,3,3,3,3,3,3,3,3,3,3,3,3,4),
(0.,1.12890698065798E-5,7.65259667182735E-5,0.000102837507928502,0.000112544869199243,
0.000130746171581884,0.000194450729921128,0.00022630300909075,0.000242229148675561,
0.000258155288260372,0.000258291104876522,0.0003276546336074,0.000399363990821298,
0.000469709285170205,0.000516310576520743),.UNSPECIFIED.);
#4352=B_SPLINE_CURVE_WITH_KNOTS('',3,(#172178,#172179,#172180,#172181,#172182,
#172183,#172184,#172185,#172186,#172187,#172188,#172189,#172190,#172191,
#172192,#172193,#172194,#172195,#172196,#172197,#172198,#172199,#172200,
#172201,#172202,#172203,#172204,#172205,#172206,#172207,#172208,#172209,
#172210,#172211,#172212,#172213,#172214,#172215,#172216,#172217),
 .UNSPECIFIED.,.F.,.F.,(4,3,3,3,3,3,3,3,3,3,3,3,3,4),(0.,6.84564250862393E-5,
0.000138288406603796,0.000205407478943121,0.000256966021225849,0.00025710114697026,
0.000271589374668168,0.000352213067629227,0.000388398097499841,0.000404123622054926,
0.000459162957997723,0.000486682625969121,0.00050044245995482,0.000514202293940519),
 .UNSPECIFIED.);
#4353=B_SPLINE_CURVE_WITH_KNOTS('',3,(#172221,#172222,#172223,#172224,#172225,
#172226,#172227,#172228,#172229,#172230,#172231,#172232,#172233,#172234,
#172235,#172236,#172237,#172238,#172239,#172240,#172241,#172242,#172243,
#172244,#172245,#172246,#172247,#172248,#172249,#172250,#172251,#172252,
#172253,#172254,#172255,#172256,#172257,#172258,#172259,#172260,#172261,
#172262,#172263),.UNSPECIFIED.,.F.,.F.,(4,3,3,3,3,3,3,3,3,3,3,3,3,3,4),
(0.,1.12890698065779E-5,7.6525966711966E-5,0.000102837507928451,0.000112544869199195,
0.000130746171581842,0.000194450729921103,0.000226303009090734,0.00024222914867555,
0.000258155288260365,0.000258291104876504,0.000327654633616026,0.000399363990838618,
0.00046970928519519,0.00051631057652073),.UNSPECIFIED.);
#4354=B_SPLINE_CURVE_WITH_KNOTS('',3,(#172271,#172272,#172273,#172274,#172275,
#172276,#172277,#172278,#172279,#172280,#172281,#172282,#172283,#172284,
#172285,#172286,#172287,#172288,#172289,#172290,#172291,#172292,#172293,
#172294,#172295,#172296,#172297,#172298,#172299,#172300,#172301,#172302,
#172303,#172304,#172305,#172306,#172307,#172308,#172309,#172310),
 .UNSPECIFIED.,.F.,.F.,(4,3,3,3,3,3,3,3,3,3,3,3,3,4),(0.,6.84564250799927E-5,
0.000138288406590908,0.00020540747892476,0.000256966021225863,0.000257101146970264,
0.000271589374668162,0.000352213067603696,0.000388398097499727,0.000404123622054826,
0.000459162957997673,0.000486682625969097,0.000500442459954809,0.000514202293940521),
 .UNSPECIFIED.);
#4355=B_SPLINE_CURVE_WITH_KNOTS('',3,(#172314,#172315,#172316,#172317,#172318,
#172319,#172320,#172321,#172322,#172323,#172324,#172325,#172326,#172327,
#172328,#172329,#172330,#172331,#172332,#172333,#172334,#172335,#172336,
#172337,#172338,#172339,#172340,#172341,#172342,#172343,#172344,#172345,
#172346,#172347,#172348,#172349,#172350,#172351,#172352,#172353,#172354,
#172355,#172356),.UNSPECIFIED.,.F.,.F.,(4,3,3,3,3,3,3,3,3,3,3,3,3,3,4),
(0.,1.12890698065862E-5,7.65259667140177E-5,0.000102837507928526,0.000112544869199266,
0.000130746171581904,0.000194450729921138,0.000226303009090755,0.000242229148675563,
0.000258155288260372,0.000258291104876524,0.000327654633607696,0.000399363990821742,
0.000469709285170638,0.000516310576520743),.UNSPECIFIED.);
#4356=B_SPLINE_CURVE_WITH_KNOTS('',3,(#172364,#172365,#172366,#172367,#172368,
#172369,#172370,#172371,#172372,#172373,#172374,#172375,#172376,#172377,
#172378,#172379,#172380,#172381,#172382,#172383,#172384,#172385,#172386,
#172387,#172388,#172389,#172390,#172391,#172392,#172393,#172394,#172395,
#172396,#172397,#172398,#172399,#172400,#172401,#172402,#172403),
 .UNSPECIFIED.,.F.,.F.,(4,3,3,3,3,3,3,3,3,3,3,3,3,4),(0.,6.84564250927535E-5,
0.000138288406617572,0.000205407478965534,0.000256966021225856,0.000257101146970261,
0.000271589374668161,0.000352213067604348,0.000388398097499758,0.000404123622054853,
0.000459162957997688,0.000486682625969105,0.000500442459954814,0.000514202293940522),
 .UNSPECIFIED.);
#4357=B_SPLINE_CURVE_WITH_KNOTS('',3,(#172407,#172408,#172409,#172410,#172411,
#172412,#172413,#172414,#172415,#172416,#172417,#172418,#172419,#172420,
#172421,#172422,#172423,#172424,#172425,#172426,#172427,#172428,#172429,
#172430,#172431,#172432,#172433,#172434,#172435,#172436,#172437,#172438,
#172439,#172440,#172441,#172442,#172443,#172444,#172445,#172446,#172447,
#172448,#172449),.UNSPECIFIED.,.F.,.F.,(4,3,3,3,3,3,3,3,3,3,3,3,3,3,4),
(0.,1.12890698065764E-5,7.65259667099777E-5,0.00010283750792846,0.000112544869199204,
0.00013074617158185,0.000194450729921111,0.000226303009090741,0.000242229148675556,
0.000258155288260372,0.000258291104876515,0.000327654633618559,0.000399363990844535,
0.000469709285205091,0.000516310576520743),.UNSPECIFIED.);
#4358=B_SPLINE_CURVE_WITH_KNOTS('',3,(#172457,#172458,#172459,#172460,#172461,
#172462,#172463,#172464,#172465,#172466,#172467,#172468,#172469,#172470,
#172471,#172472,#172473,#172474,#172475,#172476,#172477,#172478,#172479,
#172480,#172481,#172482,#172483,#172484,#172485,#172486,#172487,#172488,
#172489,#172490,#172491,#172492,#172493,#172494,#172495,#172496),
 .UNSPECIFIED.,.F.,.F.,(4,3,3,3,3,3,3,3,3,3,3,3,3,4),(0.,6.84564250849387E-5,
0.000138288406600687,0.000205407478937706,0.000256966021225849,0.000257101146970271,
0.000271589374668183,0.000352213067620596,0.000388398097499899,0.000404123622054979,
0.00045916295799776,0.000486682625969151,0.000500442459954846,0.000514202293940541),
 .UNSPECIFIED.);
#4359=B_SPLINE_CURVE_WITH_KNOTS('',3,(#172500,#172501,#172502,#172503,#172504,
#172505,#172506,#172507,#172508,#172509,#172510,#172511,#172512,#172513,
#172514,#172515,#172516,#172517,#172518,#172519,#172520,#172521,#172522,
#172523,#172524,#172525,#172526,#172527,#172528,#172529,#172530,#172531,
#172532,#172533,#172534,#172535,#172536,#172537,#172538,#172539,#172540,
#172541,#172542),.UNSPECIFIED.,.F.,.F.,(4,3,3,3,3,3,3,3,3,3,3,3,3,3,4),
(0.,1.12890698065836E-5,7.65259666749699E-5,0.000102837507928543,0.000112544869199282,
0.000130746171581918,0.000194450729921143,0.000226303009090755,0.000242229148675561,
0.000258155288260367,0.000258291104876523,0.000327654633630791,0.000399363990867584,
0.000469709285236347,0.000516310576520735),.UNSPECIFIED.);
#4360=B_SPLINE_CURVE_WITH_KNOTS('',3,(#172550,#172551,#172552,#172553,#172554,
#172555,#172556,#172557,#172558,#172559,#172560,#172561,#172562,#172563,
#172564,#172565,#172566,#172567,#172568,#172569,#172570,#172571,#172572,
#172573,#172574,#172575,#172576,#172577,#172578,#172579,#172580,#172581,
#172582,#172583,#172584,#172585,#172586,#172587,#172588,#172589),
 .UNSPECIFIED.,.F.,.F.,(4,3,3,3,3,3,3,3,3,3,3,3,3,4),(0.,6.84564250792623E-5,
0.000138288406588807,0.000205407478919674,0.000256966021225846,0.000257101146970266,
0.000271589374668166,0.000352213067610283,0.000388398097499773,0.000404123622054868,
0.0004591629579977,0.000486682625969117,0.000500442459954825,0.000514202293940533),
 .UNSPECIFIED.);
#4361=B_SPLINE_CURVE_WITH_KNOTS('',3,(#172593,#172594,#172595,#172596,#172597,
#172598,#172599,#172600,#172601,#172602,#172603,#172604,#172605,#172606,
#172607,#172608,#172609,#172610,#172611,#172612,#172613,#172614,#172615,
#172616,#172617,#172618,#172619,#172620,#172621,#172622,#172623,#172624,
#172625,#172626,#172627,#172628,#172629,#172630,#172631,#172632,#172633,
#172634,#172635),.UNSPECIFIED.,.F.,.F.,(4,3,3,3,3,3,3,3,3,3,3,3,3,3,4),
(0.,1.12890698065765E-5,7.65259667163295E-5,0.000102837507928452,0.000112544869199197,
0.000130746171581844,0.000194450729921109,0.000226303009090742,0.000242229148675558,
0.000258155288260374,0.000258291104876519,0.0003276546336177,0.000399363990841842,
0.000469709285199261,0.000516310576520749),.UNSPECIFIED.);
#4362=B_SPLINE_CURVE_WITH_KNOTS('',3,(#172643,#172644,#172645,#172646,#172647,
#172648,#172649,#172650,#172651,#172652,#172653,#172654,#172655,#172656,
#172657,#172658,#172659,#172660,#172661,#172662,#172663,#172664,#172665,
#172666,#172667,#172668,#172669,#172670,#172671,#172672,#172673,#172674,
#172675,#172676,#172677,#172678,#172679,#172680,#172681,#172682),
 .UNSPECIFIED.,.F.,.F.,(4,3,3,3,3,3,3,3,3,3,3,3,3,4),(0.,6.84564250789114E-5,
0.000138288406589003,0.000205407478922446,0.000256966021225846,0.000257101146970262,
0.000271589374668163,0.000352213067604696,0.000388398097499755,0.000404123622054851,
0.000459162957997687,0.000486682625969105,0.000500442459954814,0.000514202293940523),
 .UNSPECIFIED.);
#4363=B_SPLINE_CURVE_WITH_KNOTS('',3,(#172686,#172687,#172688,#172689,#172690,
#172691,#172692,#172693,#172694,#172695,#172696,#172697,#172698,#172699,
#172700,#172701,#172702,#172703,#172704,#172705,#172706,#172707,#172708,
#172709,#172710,#172711,#172712,#172713,#172714,#172715,#172716,#172717,
#172718,#172719,#172720,#172721,#172722,#172723,#172724,#172725,#172726,
#172727,#172728),.UNSPECIFIED.,.F.,.F.,(4,3,3,3,3,3,3,3,3,3,3,3,3,3,4),
(0.,1.12890698065812E-5,7.65259666864815E-5,0.000102837507928512,0.000112544869199253,
0.000130746171581893,0.000194450729921133,0.000226303009090753,0.000242229148675563,
0.000258155288260373,0.000258291104876499,0.000327654633628822,0.000399363990862394,
0.000469709285225838,0.000516310576520746),.UNSPECIFIED.);
#4364=B_SPLINE_CURVE_WITH_KNOTS('',3,(#172736,#172737,#172738,#172739,#172740,
#172741,#172742,#172743,#172744,#172745,#172746,#172747,#172748,#172749,
#172750,#172751,#172752,#172753,#172754,#172755,#172756,#172757,#172758,
#172759,#172760,#172761,#172762,#172763,#172764,#172765,#172766,#172767,
#172768,#172769,#172770,#172771,#172772,#172773,#172774,#172775),
 .UNSPECIFIED.,.F.,.F.,(4,3,3,3,3,3,3,3,3,3,3,3,3,4),(0.,6.84564250929779E-5,
0.000138288406617422,0.000205407478963844,0.000256966021225864,0.000257101146970267,
0.000271589374668178,0.000352213067597606,0.00038839809749987,0.000404123622054953,
0.000459162957997743,0.000486682625969139,0.000500442459954836,0.000514202293940534),
 .UNSPECIFIED.);
#4365=B_SPLINE_CURVE_WITH_KNOTS('',3,(#172779,#172780,#172781,#172782,#172783,
#172784,#172785,#172786,#172787,#172788,#172789,#172790,#172791,#172792,
#172793,#172794,#172795,#172796,#172797,#172798,#172799,#172800,#172801,
#172802,#172803,#172804,#172805,#172806,#172807,#172808,#172809,#172810,
#172811,#172812,#172813,#172814,#172815,#172816,#172817,#172818,#172819,
#172820,#172821),.UNSPECIFIED.,.F.,.F.,(4,3,3,3,3,3,3,3,3,3,3,3,3,3,4),
(0.,1.12890698065804E-5,7.65259667067788E-5,0.000102837507928517,0.000112544869199258,
0.000130746171581896,0.000194450729921131,0.000226303009090748,0.000242229148675557,
0.000258155288260366,0.000258291104876526,0.00032765463362171,0.000399363990850038,
0.000469709285211668,0.000516310576520732),.UNSPECIFIED.);
#4366=B_SPLINE_CURVE_WITH_KNOTS('',3,(#172829,#172830,#172831,#172832,#172833,
#172834,#172835,#172836,#172837,#172838,#172839,#172840,#172841,#172842,
#172843,#172844,#172845,#172846,#172847,#172848,#172849,#172850,#172851,
#172852,#172853,#172854,#172855,#172856,#172857,#172858,#172859,#172860,
#172861,#172862,#172863,#172864,#172865,#172866,#172867,#172868),
 .UNSPECIFIED.,.F.,.F.,(4,3,3,3,3,3,3,3,3,3,3,3,3,4),(0.,6.84564250773449E-5,
0.000138288406585096,0.000205407478915048,0.000256966021225853,0.000257101146970262,
0.000271589374668166,0.000352213067599712,0.000388398097499801,0.000404123622054891,
0.000459162957997708,0.000486682625969116,0.00050044245995482,0.000514202293940524),
 .UNSPECIFIED.);
#4367=B_SPLINE_CURVE_WITH_KNOTS('',3,(#172872,#172873,#172874,#172875,#172876,
#172877,#172878,#172879,#172880,#172881,#172882,#172883,#172884,#172885,
#172886,#172887,#172888,#172889,#172890,#172891,#172892,#172893,#172894,
#172895,#172896,#172897,#172898,#172899,#172900,#172901,#172902,#172903,
#172904,#172905,#172906,#172907,#172908,#172909,#172910,#172911,#172912,
#172913,#172914),.UNSPECIFIED.,.F.,.F.,(4,3,3,3,3,3,3,3,3,3,3,3,3,3,4),
(0.,1.12890698065801E-5,7.6525966691684E-5,0.000102837507928504,0.000112544869199246,
0.000130746171581886,0.000194450729921128,0.000226303009090748,0.000242229148675559,
0.000258155288260369,0.000258291104876528,0.000327654633632161,0.000399363990871155,
0.000469709285242306,0.000516310576520738),.UNSPECIFIED.);
#4368=B_SPLINE_CURVE_WITH_KNOTS('',3,(#172922,#172923,#172924,#172925,#172926,
#172927,#172928,#172929,#172930,#172931,#172932,#172933,#172934,#172935,
#172936,#172937,#172938,#172939,#172940,#172941,#172942,#172943,#172944,
#172945,#172946,#172947,#172948,#172949,#172950,#172951,#172952,#172953,
#172954,#172955,#172956,#172957,#172958,#172959,#172960,#172961),
 .UNSPECIFIED.,.F.,.F.,(4,3,3,3,3,3,3,3,3,3,3,3,3,4),(0.,6.84564250807333E-5,
0.000138288406592608,0.000205407478927544,0.000256966021225847,0.000257101146970264,
0.000271589374668166,0.000352213067602011,0.000388398097499788,0.000404123622054881,
0.000459162957997704,0.000486682625969116,0.000500442459954822,0.000514202293940528),
 .UNSPECIFIED.);
#4369=B_SPLINE_CURVE_WITH_KNOTS('',3,(#172965,#172966,#172967,#172968,#172969,
#172970,#172971,#172972,#172973,#172974,#172975,#172976,#172977,#172978,
#172979,#172980,#172981,#172982,#172983,#172984,#172985,#172986,#172987,
#172988,#172989,#172990,#172991,#172992,#172993,#172994,#172995,#172996,
#172997,#172998,#172999,#173000,#173001,#173002,#173003,#173004,#173005,
#173006,#173007),.UNSPECIFIED.,.F.,.F.,(4,3,3,3,3,3,3,3,3,3,3,3,3,3,4),
(0.,1.12890698065848E-5,7.65259667016126E-5,0.00010283750792857,0.000112544869199308,
0.000130746171581941,0.000194450729921157,0.000226303009090765,0.000242229148675569,
0.000258155288260373,0.000258291104876515,0.000327654633612286,0.000399363990831393,
0.000469709285185608,0.000516310576520745),.UNSPECIFIED.);
#4370=B_SPLINE_CURVE_WITH_KNOTS('',3,(#173015,#173016,#173017,#173018,#173019,
#173020,#173021,#173022,#173023,#173024,#173025,#173026,#173027,#173028,
#173029,#173030,#173031,#173032,#173033,#173034,#173035,#173036,#173037,
#173038,#173039,#173040,#173041,#173042,#173043,#173044,#173045,#173046,
#173047,#173048,#173049,#173050,#173051,#173052,#173053,#173054),
 .UNSPECIFIED.,.F.,.F.,(4,3,3,3,3,3,3,3,3,3,3,3,3,4),(0.,6.8456425072981E-5,
0.000138288406576581,0.000205407478902633,0.000256966021225849,0.000257101146970262,
0.000271589374668165,0.000352213067615655,0.000388398097499802,0.000404123622054892,
0.000459162957997708,0.000486682625969116,0.00050044245995482,0.000514202293940524),
 .UNSPECIFIED.);
#4371=B_SPLINE_CURVE_WITH_KNOTS('',3,(#173058,#173059,#173060,#173061,#173062,
#173063,#173064,#173065,#173066,#173067,#173068,#173069,#173070,#173071,
#173072,#173073,#173074,#173075,#173076,#173077,#173078,#173079,#173080,
#173081,#173082,#173083,#173084,#173085,#173086,#173087,#173088,#173089,
#173090,#173091,#173092,#173093,#173094,#173095,#173096,#173097,#173098,
#173099,#173100),.UNSPECIFIED.,.F.,.F.,(4,3,3,3,3,3,3,3,3,3,3,3,3,3,4),
(1.73472347597681E-18,1.12890698065816E-5,7.65259667046772E-5,0.000102837507928469,
0.000112544869199213,0.000130746171581857,0.000194450729921112,0.000226303009090739,
0.000242229148675553,0.000258155288260367,0.000258291104876528,0.00032765463361615,
0.000399363990838513,0.000469709285194426,0.000516310576520732),
 .UNSPECIFIED.);
#4372=B_SPLINE_CURVE_WITH_KNOTS('',3,(#173108,#173109,#173110,#173111,#173112,
#173113,#173114,#173115,#173116,#173117,#173118,#173119,#173120,#173121,
#173122,#173123,#173124,#173125,#173126,#173127,#173128,#173129,#173130,
#173131,#173132,#173133,#173134,#173135,#173136,#173137,#173138,#173139,
#173140,#173141,#173142,#173143,#173144,#173145,#173146,#173147),
 .UNSPECIFIED.,.F.,.F.,(4,3,3,3,3,3,3,3,3,3,3,3,3,4),(0.,6.8456425082964E-5,
0.000138288406597018,0.000205407478933636,0.000256966021225847,0.000257101146970261,
0.000271589374668168,0.000352213067601968,0.000388398097499816,0.000404123622054904,
0.000459162957997713,0.000486682625969118,0.00050044245995482,0.000514202293940522),
 .UNSPECIFIED.);
#4373=B_SPLINE_CURVE_WITH_KNOTS('',3,(#173151,#173152,#173153,#173154,#173155,
#173156,#173157,#173158,#173159,#173160,#173161,#173162,#173163,#173164,
#173165,#173166,#173167,#173168,#173169,#173170,#173171,#173172,#173173,
#173174,#173175,#173176,#173177,#173178,#173179,#173180,#173181,#173182,
#173183,#173184,#173185,#173186,#173187,#173188,#173189,#173190,#173191,
#173192,#173193),.UNSPECIFIED.,.F.,.F.,(4,3,3,3,3,3,3,3,3,3,3,3,3,3,4),
(8.67361737988403E-19,1.1289069806576E-5,7.65259667049559E-5,0.00010283750792845,
0.000112544869199195,0.000130746171581841,0.000194450729921104,0.000226303009090735,
0.00024222914867555,0.000258155288260366,0.000258291104876504,0.000327654633611955,
0.000399363990830165,0.000469709285182823,0.000516310576520731),
 .UNSPECIFIED.);
#4374=B_SPLINE_CURVE_WITH_KNOTS('',3,(#173200,#173201,#173202,#173203,#173204,
#173205,#173206,#173207,#173208,#173209,#173210,#173211,#173212,#173213,
#173214,#173215,#173216,#173217,#173218,#173219,#173220,#173221,#173222,
#173223,#173224,#173225,#173226,#173227,#173228,#173229,#173230,#173231,
#173232,#173233,#173234,#173235,#173236,#173237,#173238,#173239),
 .UNSPECIFIED.,.F.,.F.,(4,3,3,3,3,3,3,3,3,3,3,3,3,4),(0.,6.84564250762055E-5,
0.000138288406583219,0.000205407478913333,0.000256966021225853,0.000257101146970262,
0.000271589374668166,0.000352213067595464,0.000388398097499808,0.000404123622054897,
0.00045916295799771,0.000486682625969117,0.00050044245995482,0.000514202293940523),
 .UNSPECIFIED.);
#4375=B_SPLINE_CURVE_WITH_KNOTS('',3,(#173242,#173243,#173244,#173245,#173246,
#173247,#173248,#173249,#173250,#173251,#173252,#173253,#173254,#173255,
#173256,#173257,#173258,#173259,#173260,#173261,#173262,#173263,#173264,
#173265,#173266,#173267,#173268,#173269,#173270,#173271,#173272,#173273,
#173274,#173275,#173276,#173277,#173278),.UNSPECIFIED.,.F.,.F.,(4,3,3,3,
3,3,3,3,3,3,3,3,4),(0.,1.12535551670963E-5,7.76936938449189E-5,0.000102513517961119,
0.000121879189824267,0.000189659041345284,0.000223548967105793,0.000257294099096092,
0.000257438892866302,0.000325720851757748,0.00039648677396,0.000466242707669274,
0.000514877785732603),.UNSPECIFIED.);
#4376=B_SPLINE_CURVE_WITH_KNOTS('',3,(#173286,#173287,#173288,#173289,#173290,
#173291,#173292,#173293,#173294,#173295,#173296,#173297,#173298,#173299,
#173300,#173301,#173302,#173303,#173304,#173305,#173306,#173307,#173308,
#173309,#173310,#173311,#173312,#173313,#173314,#173315,#173316,#173317,
#173318,#173319,#173320,#173321,#173322,#173323,#173324,#173325),
 .UNSPECIFIED.,.F.,.F.,(4,3,3,3,3,3,3,3,3,3,3,3,3,4),(0.,6.80370855381457E-5,
0.000137303169301757,0.00020363670666859,0.000256396220959708,0.000256540237295746,
0.000285209320207747,0.000342105100635664,0.000384776935956602,0.000400778874201954,
0.000456785658060685,0.000484789049990051,0.000498790745954733,0.000512792441919416),
 .UNSPECIFIED.);
#4377=B_SPLINE_CURVE_WITH_KNOTS('',3,(#173329,#173330,#173331,#173332,#173333,
#173334,#173335,#173336,#173337,#173338,#173339,#173340,#173341,#173342,
#173343,#173344,#173345,#173346,#173347,#173348,#173349,#173350,#173351,
#173352,#173353,#173354,#173355,#173356,#173357,#173358,#173359,#173360,
#173361,#173362,#173363,#173364,#173365),.UNSPECIFIED.,.F.,.F.,(4,3,3,3,
3,3,3,3,3,3,3,3,4),(0.,1.12535551670971E-5,7.76936938477942E-5,0.000102513517961123,
0.00012187918982427,0.000189659041345285,0.000223548967105792,0.000257294099096091,
0.000257438892866299,0.000325720851759598,0.000396486773963869,0.000466242707675107,
0.000514877785732599),.UNSPECIFIED.);
#4378=B_SPLINE_CURVE_WITH_KNOTS('',3,(#173373,#173374,#173375,#173376,#173377,
#173378,#173379,#173380,#173381,#173382,#173383,#173384,#173385,#173386,
#173387,#173388,#173389,#173390,#173391,#173392,#173393,#173394,#173395,
#173396,#173397,#173398,#173399,#173400,#173401,#173402,#173403,#173404,
#173405,#173406,#173407,#173408,#173409,#173410,#173411,#173412),
 .UNSPECIFIED.,.F.,.F.,(4,3,3,3,3,3,3,3,3,3,3,3,3,4),(0.,6.80370855340055E-5,
0.000137303169293596,0.000203636706656825,0.000256396220959708,0.000256540237295739,
0.000285209320207743,0.000342105100635661,0.0003847769359566,0.000400778874201951,
0.000456785658060683,0.000484789049990049,0.000498790745954732,0.000512792441919415),
 .UNSPECIFIED.);
#4379=B_SPLINE_CURVE_WITH_KNOTS('',3,(#173416,#173417,#173418,#173419,#173420,
#173421,#173422,#173423,#173424,#173425,#173426,#173427,#173428,#173429,
#173430,#173431,#173432,#173433,#173434,#173435,#173436,#173437,#173438,
#173439,#173440,#173441,#173442,#173443,#173444,#173445,#173446,#173447,
#173448,#173449,#173450,#173451,#173452),.UNSPECIFIED.,.F.,.F.,(4,3,3,3,
3,3,3,3,3,3,3,3,4),(0.,1.12535551671009E-5,7.76936938396507E-5,0.000102513517961129,
0.000121879189824276,0.000189659041345289,0.000223548967105796,0.000257294099096101,
0.000257438892866303,0.000325720851765454,0.000396486773975544,0.000466242707691564,
0.000514877785732606),.UNSPECIFIED.);
#4380=B_SPLINE_CURVE_WITH_KNOTS('',3,(#173460,#173461,#173462,#173463,#173464,
#173465,#173466,#173467,#173468,#173469,#173470,#173471,#173472,#173473,
#173474,#173475,#173476,#173477,#173478,#173479,#173480,#173481,#173482,
#173483,#173484,#173485,#173486,#173487,#173488,#173489,#173490,#173491,
#173492,#173493,#173494,#173495,#173496,#173497,#173498,#173499),
 .UNSPECIFIED.,.F.,.F.,(4,3,3,3,3,3,3,3,3,3,3,3,3,4),(0.,6.80370855356198E-5,
0.000137303169296276,0.000203636706659361,0.000256396220959709,0.000256540237295742,
0.000285209320207737,0.000342105100635657,0.000384776935956597,0.00040077887420195,
0.000456785658060683,0.00048478904999005,0.000498790745954734,0.000512792441919417),
 .UNSPECIFIED.);
#4381=B_SPLINE_CURVE_WITH_KNOTS('',3,(#173503,#173504,#173505,#173506,#173507,
#173508,#173509,#173510,#173511,#173512,#173513,#173514,#173515,#173516,
#173517,#173518,#173519,#173520,#173521,#173522,#173523,#173524,#173525,
#173526,#173527,#173528,#173529,#173530,#173531,#173532,#173533,#173534,
#173535,#173536,#173537,#173538,#173539),.UNSPECIFIED.,.F.,.F.,(4,3,3,3,
3,3,3,3,3,3,3,3,4),(0.,1.12535551670961E-5,7.76936938360982E-5,0.000102513517961078,
0.000121879189824231,0.000189659041345266,0.000223548967105784,0.000257294099096098,
0.000257438892866302,0.000325720851762349,0.000396486773968905,0.000466242707681605,
0.000514877785732604),.UNSPECIFIED.);
#4382=B_SPLINE_CURVE_WITH_KNOTS('',3,(#173547,#173548,#173549,#173550,#173551,
#173552,#173553,#173554,#173555,#173556,#173557,#173558,#173559,#173560,
#173561,#173562,#173563,#173564,#173565,#173566,#173567,#173568,#173569,
#173570,#173571,#173572,#173573,#173574,#173575,#173576,#173577,#173578,
#173579,#173580,#173581,#173582,#173583,#173584,#173585,#173586),
 .UNSPECIFIED.,.F.,.F.,(4,3,3,3,3,3,3,3,3,3,3,3,3,4),(0.,6.80370855416975E-5,
0.000137303169308508,0.00020363670667723,0.000256396220959707,0.000256540237295748,
0.000285209320207735,0.000342105100635654,0.000384776935956594,0.000400778874201947,
0.00045678565806068,0.000484789049990047,0.000498790745954731,0.000512792441919414),
 .UNSPECIFIED.);
#4383=B_SPLINE_CURVE_WITH_KNOTS('',3,(#173590,#173591,#173592,#173593,#173594,
#173595,#173596,#173597,#173598,#173599,#173600,#173601,#173602,#173603,
#173604,#173605,#173606,#173607,#173608,#173609,#173610,#173611,#173612,
#173613,#173614,#173615,#173616,#173617,#173618,#173619,#173620,#173621,
#173622,#173623,#173624,#173625,#173626),.UNSPECIFIED.,.F.,.F.,(4,3,3,3,
3,3,3,3,3,3,3,3,4),(0.,1.12535551670951E-5,7.76936938499772E-5,0.000102513517961046,
0.000121879189824203,0.000189659041345254,0.000223548967105779,0.000257294099096101,
0.000257438892866304,0.000325720851757687,0.000396486773959997,0.000466242707669562,
0.000514877785732608),.UNSPECIFIED.);
#4384=B_SPLINE_CURVE_WITH_KNOTS('',3,(#173634,#173635,#173636,#173637,#173638,
#173639,#173640,#173641,#173642,#173643,#173644,#173645,#173646,#173647,
#173648,#173649,#173650,#173651,#173652,#173653,#173654,#173655,#173656,
#173657,#173658,#173659,#173660,#173661,#173662,#173663,#173664,#173665,
#173666,#173667,#173668,#173669,#173670,#173671,#173672,#173673),
 .UNSPECIFIED.,.F.,.F.,(4,3,3,3,3,3,3,3,3,3,3,3,3,4),(0.,6.80370855321537E-5,
0.000137303169289407,0.000203636706649685,0.000256396220959712,0.000256540237295725,
0.000285209320207737,0.000342105100635658,0.0003847769359566,0.000400778874201953,
0.000456785658060688,0.000484789049990056,0.000498790745954739,0.000512792441919423),
 .UNSPECIFIED.);
#4385=B_SPLINE_CURVE_WITH_KNOTS('',3,(#173677,#173678,#173679,#173680,#173681,
#173682,#173683,#173684,#173685,#173686,#173687,#173688,#173689,#173690,
#173691,#173692,#173693,#173694,#173695,#173696,#173697,#173698,#173699,
#173700,#173701,#173702,#173703,#173704,#173705,#173706,#173707,#173708,
#173709,#173710,#173711,#173712,#173713),.UNSPECIFIED.,.F.,.F.,(4,3,3,3,
3,3,3,3,3,3,3,3,4),(0.,1.12535551670998E-5,7.76936938510011E-5,0.000102513517961135,
0.000121879189824282,0.000189659041345296,0.000223548967105803,0.000257294099096103,
0.00025743889286631,0.000325720851757794,0.000396486773960278,0.000466242707669978,
0.000514877785732619),.UNSPECIFIED.);
#4386=B_SPLINE_CURVE_WITH_KNOTS('',3,(#173721,#173722,#173723,#173724,#173725,
#173726,#173727,#173728,#173729,#173730,#173731,#173732,#173733,#173734,
#173735,#173736,#173737,#173738,#173739,#173740,#173741,#173742,#173743,
#173744,#173745,#173746,#173747,#173748,#173749,#173750,#173751,#173752,
#173753,#173754,#173755,#173756,#173757,#173758,#173759,#173760),
 .UNSPECIFIED.,.F.,.F.,(4,3,3,3,3,3,3,3,3,3,3,3,3,4),(0.,6.80370855402335E-5,
0.000137303169306136,0.000203636706675648,0.000256396220959704,0.000256540237295737,
0.000285209320207747,0.000342105100635662,0.000384776935956598,0.000400778874201949,
0.000456785658060679,0.000484789049990043,0.000498790745954725,0.000512792441919408),
 .UNSPECIFIED.);
#4387=B_SPLINE_CURVE_WITH_KNOTS('',3,(#173764,#173765,#173766,#173767,#173768,
#173769,#173770,#173771,#173772,#173773,#173774,#173775,#173776,#173777,
#173778,#173779,#173780,#173781,#173782,#173783,#173784,#173785,#173786,
#173787,#173788,#173789,#173790,#173791,#173792,#173793,#173794,#173795,
#173796,#173797,#173798,#173799,#173800),.UNSPECIFIED.,.F.,.F.,(4,3,3,3,
3,3,3,3,3,3,3,3,4),(0.,1.12535551670965E-5,7.76936938370593E-5,0.00010251351796113,
0.000121879189824277,0.000189659041345291,0.000223548967105798,0.000257294099096113,
0.000257438892866305,0.000325720851760076,0.000396486773964988,0.000466242707677394,
0.000514877785732611),.UNSPECIFIED.);
#4388=B_SPLINE_CURVE_WITH_KNOTS('',3,(#173808,#173809,#173810,#173811,#173812,
#173813,#173814,#173815,#173816,#173817,#173818,#173819,#173820,#173821,
#173822,#173823,#173824,#173825,#173826,#173827,#173828,#173829,#173830,
#173831,#173832,#173833,#173834,#173835,#173836,#173837,#173838,#173839,
#173840,#173841,#173842,#173843,#173844,#173845,#173846,#173847),
 .UNSPECIFIED.,.F.,.F.,(4,3,3,3,3,3,3,3,3,3,3,3,3,4),(0.,6.80370855329636E-5,
0.000137303169291043,0.000203636706652177,0.000256396220959708,0.000256540237295739,
0.000285209320207743,0.000342105100635661,0.0003847769359566,0.000400778874201952,
0.000456785658060685,0.000484789049990051,0.000498790745954734,0.000512792441919417),
 .UNSPECIFIED.);
#4389=B_SPLINE_CURVE_WITH_KNOTS('',3,(#173851,#173852,#173853,#173854,#173855,
#173856,#173857,#173858,#173859,#173860,#173861,#173862,#173863,#173864,
#173865,#173866,#173867,#173868,#173869,#173870,#173871,#173872,#173873,
#173874,#173875,#173876,#173877,#173878,#173879,#173880,#173881,#173882,
#173883,#173884,#173885,#173886,#173887),.UNSPECIFIED.,.F.,.F.,(4,3,3,3,
3,3,3,3,3,3,3,3,4),(0.,1.1253555167096E-5,7.7693693832872E-5,0.000102513517961065,
0.000121879189824221,0.000189659041345265,0.000223548967105787,0.000257294099096107,
0.000257438892866309,0.000325720851759186,0.000396486773962424,0.000466242707672148,
0.000514877785732618),.UNSPECIFIED.);
#4390=B_SPLINE_CURVE_WITH_KNOTS('',3,(#173895,#173896,#173897,#173898,#173899,
#173900,#173901,#173902,#173903,#173904,#173905,#173906,#173907,#173908,
#173909,#173910,#173911,#173912,#173913,#173914,#173915,#173916,#173917,
#173918,#173919,#173920,#173921,#173922,#173923,#173924,#173925,#173926,
#173927,#173928,#173929,#173930,#173931,#173932,#173933,#173934),
 .UNSPECIFIED.,.F.,.F.,(4,3,3,3,3,3,3,3,3,3,3,3,3,4),(0.,6.80370855426867E-5,
0.000137303169311313,0.000203636706683517,0.000256396220959705,0.00025654023729572,
0.000285209320207733,0.000342105100635652,0.000384776935956592,0.000400778874201944,
0.000456785658060677,0.000484789049990044,0.000498790745954727,0.00051279244191941),
 .UNSPECIFIED.);
#4391=B_SPLINE_CURVE_WITH_KNOTS('',3,(#173938,#173939,#173940,#173941,#173942,
#173943,#173944,#173945,#173946,#173947,#173948,#173949,#173950,#173951,
#173952,#173953,#173954,#173955,#173956,#173957,#173958,#173959,#173960,
#173961,#173962,#173963,#173964,#173965,#173966,#173967,#173968,#173969,
#173970,#173971,#173972,#173973,#173974),.UNSPECIFIED.,.F.,.F.,(4,3,3,3,
3,3,3,3,3,3,3,3,4),(0.,1.12535551670979E-5,7.76936938511101E-5,0.000102513517961128,
0.000121879189824275,0.000189659041345292,0.0002235489671058,0.000257294099096117,
0.000257438892866308,0.000325720851744255,0.000396486773933114,0.000466242707631399,
0.000514877785732617),.UNSPECIFIED.);
#4392=B_SPLINE_CURVE_WITH_KNOTS('',3,(#173982,#173983,#173984,#173985,#173986,
#173987,#173988,#173989,#173990,#173991,#173992,#173993,#173994,#173995,
#173996,#173997,#173998,#173999,#174000,#174001,#174002,#174003,#174004,
#174005,#174006,#174007,#174008,#174009,#174010,#174011,#174012,#174013,
#174014,#174015,#174016,#174017,#174018,#174019,#174020,#174021),
 .UNSPECIFIED.,.F.,.F.,(4,3,3,3,3,3,3,3,3,3,3,3,3,4),(0.,6.80370855405851E-5,
0.000137303169307101,0.000203636706677472,0.000256396220959704,0.00025654023729574,
0.000285209320207737,0.000342105100635655,0.000384776935956593,0.000400778874201945,
0.000456785658060677,0.000484789049990043,0.000498790745954726,0.000512792441919409),
 .UNSPECIFIED.);
#4393=B_SPLINE_CURVE_WITH_KNOTS('',3,(#174025,#174026,#174027,#174028,#174029,
#174030,#174031,#174032,#174033,#174034,#174035,#174036,#174037,#174038,
#174039,#174040,#174041,#174042,#174043,#174044,#174045,#174046,#174047,
#174048,#174049,#174050,#174051,#174052,#174053,#174054,#174055,#174056,
#174057,#174058,#174059,#174060,#174061),.UNSPECIFIED.,.F.,.F.,(4,3,3,3,
3,3,3,3,3,3,3,3,4),(0.,1.12535551670968E-5,7.76936938519756E-5,0.000102513517961092,
0.000121879189824243,0.000189659041345274,0.00022354896710579,0.000257294099096106,
0.000257438892866305,0.000325720851759131,0.000396486773963648,0.000466242707676064,
0.000514877785732611),.UNSPECIFIED.);
#4394=B_SPLINE_CURVE_WITH_KNOTS('',3,(#174069,#174070,#174071,#174072,#174073,
#174074,#174075,#174076,#174077,#174078,#174079,#174080,#174081,#174082,
#174083,#174084,#174085,#174086,#174087,#174088,#174089,#174090,#174091,
#174092,#174093,#174094,#174095,#174096,#174097,#174098,#174099,#174100,
#174101,#174102,#174103,#174104,#174105,#174106,#174107,#174108),
 .UNSPECIFIED.,.F.,.F.,(4,3,3,3,3,3,3,3,3,3,3,3,3,4),(0.,6.80370855443293E-5,
0.000137303169314145,0.000203636706686637,0.000256396220959703,0.000256540237295738,
0.000285209320207752,0.000342105100635665,0.0003847769359566,0.000400778874201951,
0.000456785658060678,0.000484789049990041,0.000498790745954723,0.000512792441919405),
 .UNSPECIFIED.);
#4395=B_SPLINE_CURVE_WITH_KNOTS('',3,(#174112,#174113,#174114,#174115,#174116,
#174117,#174118,#174119,#174120,#174121,#174122,#174123,#174124,#174125,
#174126,#174127,#174128,#174129,#174130,#174131,#174132,#174133,#174134,
#174135,#174136,#174137,#174138,#174139,#174140,#174141,#174142,#174143,
#174144,#174145,#174146,#174147,#174148),.UNSPECIFIED.,.F.,.F.,(4,3,3,3,
3,3,3,3,3,3,3,3,4),(0.,1.12535551670953E-5,7.76936938441846E-5,0.000102513517961061,
0.000121879189824217,0.000189659041345262,0.000223548967105784,0.000257294099096109,
0.000257438892866307,0.000325720851756007,0.000396486773956202,0.000466242707663296,
0.000514877785732614),.UNSPECIFIED.);
#4396=B_SPLINE_CURVE_WITH_KNOTS('',3,(#174156,#174157,#174158,#174159,#174160,
#174161,#174162,#174163,#174164,#174165,#174166,#174167,#174168,#174169,
#174170,#174171,#174172,#174173,#174174,#174175,#174176,#174177,#174178,
#174179,#174180,#174181,#174182,#174183,#174184,#174185,#174186,#174187,
#174188,#174189,#174190,#174191,#174192,#174193,#174194,#174195),
 .UNSPECIFIED.,.F.,.F.,(4,3,3,3,3,3,3,3,3,3,3,3,3,4),(0.,6.80370855340898E-5,
0.00013730316929358,0.000203636706656239,0.000256396220959703,0.000256540237295742,
0.000285209320207727,0.000342105100635647,0.000384776935956586,0.000400778874201939,
0.000456785658060672,0.000484789049990039,0.000498790745954723,0.000512792441919406),
 .UNSPECIFIED.);
#4397=B_SPLINE_CURVE_WITH_KNOTS('',3,(#174199,#174200,#174201,#174202,#174203,
#174204,#174205,#174206,#174207,#174208,#174209,#174210,#174211,#174212,
#174213,#174214,#174215,#174216,#174217,#174218,#174219,#174220,#174221,
#174222,#174223,#174224,#174225,#174226,#174227,#174228,#174229,#174230,
#174231,#174232,#174233,#174234,#174235),.UNSPECIFIED.,.F.,.F.,(4,3,3,3,
3,3,3,3,3,3,3,3,4),(0.,1.12535551670914E-5,7.76936938407497E-5,0.000102513517961058,
0.000121879189824214,0.000189659041345258,0.00022354896710578,0.000257294099096095,
0.000257438892866303,0.000325720851759145,0.00039648677396219,0.000466242707671321,
0.000514877785732594),.UNSPECIFIED.);
#4398=B_SPLINE_CURVE_WITH_KNOTS('',3,(#174243,#174244,#174245,#174246,#174247,
#174248,#174249,#174250,#174251,#174252,#174253,#174254,#174255,#174256,
#174257,#174258,#174259,#174260,#174261,#174262,#174263,#174264,#174265,
#174266,#174267,#174268,#174269,#174270,#174271,#174272,#174273,#174274,
#174275,#174276,#174277,#174278,#174279,#174280,#174281,#174282),
 .UNSPECIFIED.,.F.,.F.,(4,3,3,3,3,3,3,3,3,3,3,3,3,4),(0.,6.80370855425274E-5,
0.000137303169310403,0.000203636706680631,0.000256396220959705,0.000256540237295745,
0.000285209320207746,0.000342105100635662,0.000384776935956599,0.000400778874201951,
0.000456785658060681,0.000484789049990046,0.000498790745954728,0.000512792441919411),
 .UNSPECIFIED.);
#4399=B_SPLINE_CURVE_WITH_KNOTS('',3,(#174286,#174287,#174288,#174289,#174290,
#174291,#174292,#174293,#174294,#174295,#174296,#174297,#174298,#174299,
#174300,#174301,#174302,#174303,#174304,#174305,#174306,#174307,#174308,
#174309,#174310,#174311,#174312,#174313,#174314,#174315,#174316,#174317,
#174318,#174319,#174320,#174321,#174322),.UNSPECIFIED.,.F.,.F.,(4,3,3,3,
3,3,3,3,3,3,3,3,4),(0.,1.12535551670943E-5,7.76936938459712E-5,0.000102513517961047,
0.000121879189824205,0.000189659041345256,0.000223548967105781,0.000257294099096093,
0.000257438892866307,0.000325720851750959,0.000396486773946435,0.000466242707650226,
0.000514877785732613),.UNSPECIFIED.);
#4400=B_SPLINE_CURVE_WITH_KNOTS('',3,(#174330,#174331,#174332,#174333,#174334,
#174335,#174336,#174337,#174338,#174339,#174340,#174341,#174342,#174343,
#174344,#174345,#174346,#174347,#174348,#174349,#174350,#174351,#174352,
#174353,#174354,#174355,#174356,#174357,#174358,#174359,#174360,#174361,
#174362,#174363,#174364,#174365,#174366,#174367,#174368,#174369),
 .UNSPECIFIED.,.F.,.F.,(4,3,3,3,3,3,3,3,3,3,3,3,3,4),(0.,6.80370855416932E-5,
0.000137303169308873,0.000203636706679008,0.000256396220959704,0.000256540237295732,
0.000285209320207732,0.000342105100635651,0.00038477693595659,0.000400778874201943,
0.000456785658060676,0.000484789049990042,0.000498790745954725,0.000512792441919408),
 .UNSPECIFIED.);
#4401=B_SPLINE_CURVE_WITH_KNOTS('',3,(#174373,#174374,#174375,#174376,#174377,
#174378,#174379,#174380,#174381,#174382,#174383,#174384,#174385,#174386,
#174387,#174388,#174389,#174390,#174391,#174392,#174393,#174394,#174395,
#174396,#174397,#174398,#174399,#174400,#174401,#174402,#174403,#174404,
#174405,#174406,#174407,#174408,#174409),.UNSPECIFIED.,.F.,.F.,(4,3,3,3,
3,3,3,3,3,3,3,3,4),(0.,1.12535551670975E-5,7.76936938474744E-5,0.000102513517961061,
0.000121879189824216,0.000189659041345261,0.000223548967105783,0.000257294099096097,
0.000257438892866305,0.00032572085175803,0.000396486773960401,0.000466242707669455,
0.00051487778573261),.UNSPECIFIED.);
#4402=B_SPLINE_CURVE_WITH_KNOTS('',3,(#174417,#174418,#174419,#174420,#174421,
#174422,#174423,#174424,#174425,#174426,#174427,#174428,#174429,#174430,
#174431,#174432,#174433,#174434,#174435,#174436,#174437,#174438,#174439,
#174440,#174441,#174442,#174443,#174444,#174445,#174446,#174447,#174448,
#174449,#174450,#174451,#174452,#174453,#174454,#174455,#174456),
 .UNSPECIFIED.,.F.,.F.,(4,3,3,3,3,3,3,3,3,3,3,3,3,4),(0.,6.80370855424907E-5,
0.0001373031693105,0.000203636706681343,0.000256396220959704,0.000256540237295739,
0.000285209320207733,0.000342105100635651,0.000384776935956591,0.000400778874201943,
0.000456785658060675,0.000484789049990042,0.000498790745954725,0.000512792441919408),
 .UNSPECIFIED.);
#4403=B_SPLINE_CURVE_WITH_KNOTS('',3,(#174460,#174461,#174462,#174463,#174464,
#174465,#174466,#174467,#174468,#174469,#174470,#174471,#174472,#174473,
#174474,#174475,#174476,#174477,#174478,#174479,#174480,#174481,#174482,
#174483,#174484,#174485,#174486,#174487,#174488,#174489,#174490,#174491,
#174492,#174493,#174494,#174495,#174496),.UNSPECIFIED.,.F.,.F.,(4,3,3,3,
3,3,3,3,3,3,3,3,4),(0.,1.12535551670997E-5,7.76936938476196E-5,0.000102513517961137,
0.000121879189824283,0.000189659041345294,0.0002235489671058,0.000257294099096102,
0.000257438892866305,0.000325720851755202,0.000396486773954731,0.000466242707661486,
0.000514877785732611),.UNSPECIFIED.);
#4404=B_SPLINE_CURVE_WITH_KNOTS('',3,(#174504,#174505,#174506,#174507,#174508,
#174509,#174510,#174511,#174512,#174513,#174514,#174515,#174516,#174517,
#174518,#174519,#174520,#174521,#174522,#174523,#174524,#174525,#174526,
#174527,#174528,#174529,#174530,#174531,#174532,#174533,#174534,#174535,
#174536,#174537,#174538,#174539,#174540,#174541,#174542,#174543),
 .UNSPECIFIED.,.F.,.F.,(4,3,3,3,3,3,3,3,3,3,3,3,3,4),(0.,6.80370855428342E-5,
0.000137303169311103,0.000203636706682138,0.000256396220959707,0.000256540237295733,
0.000285209320207737,0.000342105100635656,0.000384776935956596,0.000400778874201948,
0.000456785658060681,0.000484789049990048,0.000498790745954731,0.000512792441919414),
 .UNSPECIFIED.);
#4405=B_SPLINE_CURVE_WITH_KNOTS('',3,(#174547,#174548,#174549,#174550,#174551,
#174552,#174553,#174554,#174555,#174556,#174557,#174558,#174559,#174560,
#174561,#174562,#174563,#174564,#174565,#174566,#174567,#174568,#174569,
#174570,#174571,#174572,#174573,#174574,#174575,#174576,#174577,#174578,
#174579,#174580,#174581,#174582,#174583),.UNSPECIFIED.,.F.,.F.,(4,3,3,3,
3,3,3,3,3,3,3,3,4),(0.,1.12535551670975E-5,7.7693693847771E-5,0.00010251351796109,
0.000121879189824242,0.000189659041345272,0.000223548967105788,0.000257294099096109,
0.000257438892866303,0.000325720851758554,0.000396486773961584,0.00046624270767156,
0.000514877785732606),.UNSPECIFIED.);
#4406=B_SPLINE_CURVE_WITH_KNOTS('',3,(#174591,#174592,#174593,#174594,#174595,
#174596,#174597,#174598,#174599,#174600,#174601,#174602,#174603,#174604,
#174605,#174606,#174607,#174608,#174609,#174610,#174611,#174612,#174613,
#174614,#174615,#174616,#174617,#174618,#174619,#174620,#174621,#174622,
#174623,#174624,#174625,#174626,#174627,#174628,#174629,#174630),
 .UNSPECIFIED.,.F.,.F.,(4,3,3,3,3,3,3,3,3,3,3,3,3,4),(0.,6.80370855342209E-5,
0.000137303169293638,0.00020363670665596,0.000256396220959704,0.000256540237295741,
0.000285209320207738,0.000342105100635655,0.000384776935956594,0.000400778874201945,
0.000456785658060677,0.000484789049990042,0.000498790745954725,0.000512792441919408),
 .UNSPECIFIED.);
#4407=B_SPLINE_CURVE_WITH_KNOTS('',3,(#174634,#174635,#174636,#174637,#174638,
#174639,#174640,#174641,#174642,#174643,#174644,#174645,#174646,#174647,
#174648,#174649,#174650,#174651,#174652,#174653,#174654,#174655,#174656,
#174657,#174658,#174659,#174660,#174661,#174662,#174663,#174664,#174665,
#174666,#174667,#174668,#174669,#174670),.UNSPECIFIED.,.F.,.F.,(4,3,3,3,
3,3,3,3,3,3,3,3,4),(0.,1.12535551670985E-5,7.76936938451044E-5,0.000102513517961084,
0.000121879189824236,0.000189659041345269,0.000223548967105785,0.000257294099096095,
0.000257438892866301,0.000325720851759207,0.000396486773962963,0.000466242707673494,
0.000514877785732603),.UNSPECIFIED.);
#4408=B_SPLINE_CURVE_WITH_KNOTS('',3,(#174678,#174679,#174680,#174681,#174682,
#174683,#174684,#174685,#174686,#174687,#174688,#174689,#174690,#174691,
#174692,#174693,#174694,#174695,#174696,#174697,#174698,#174699,#174700,
#174701,#174702,#174703,#174704,#174705,#174706,#174707,#174708,#174709,
#174710,#174711,#174712,#174713,#174714,#174715,#174716,#174717),
 .UNSPECIFIED.,.F.,.F.,(4,3,3,3,3,3,3,3,3,3,3,3,3,4),(0.,6.80370855408533E-5,
0.000137303169307367,0.000203636706676852,0.000256396220959703,0.000256540237295735,
0.000285209320207737,0.000342105100635654,0.000384776935956592,0.000400778874201944,
0.000456785658060675,0.000484789049990041,0.000498790745954724,0.000512792441919407),
 .UNSPECIFIED.);
#4409=B_SPLINE_CURVE_WITH_KNOTS('',3,(#174721,#174722,#174723,#174724,#174725,
#174726,#174727,#174728,#174729,#174730,#174731,#174732,#174733,#174734,
#174735,#174736,#174737,#174738,#174739,#174740,#174741,#174742,#174743,
#174744,#174745,#174746,#174747,#174748,#174749,#174750,#174751,#174752,
#174753,#174754,#174755,#174756,#174757),.UNSPECIFIED.,.F.,.F.,(4,3,3,3,
3,3,3,3,3,3,3,3,4),(0.,1.12535551670974E-5,7.76936938464889E-5,0.000102513517961109,
0.000121879189824259,0.000189659041345283,0.000223548967105796,0.00025729409909611,
0.000257438892866308,0.000325720851760378,0.000396486773965212,0.000466242707676601,
0.000514877785732616),.UNSPECIFIED.);
#4410=B_SPLINE_CURVE_WITH_KNOTS('',3,(#174765,#174766,#174767,#174768,#174769,
#174770,#174771,#174772,#174773,#174774,#174775,#174776,#174777,#174778,
#174779,#174780,#174781,#174782,#174783,#174784,#174785,#174786,#174787,
#174788,#174789,#174790,#174791,#174792,#174793,#174794,#174795,#174796,
#174797,#174798,#174799,#174800,#174801,#174802,#174803,#174804),
 .UNSPECIFIED.,.F.,.F.,(4,3,3,3,3,3,3,3,3,3,3,3,3,4),(0.,6.80370855403097E-5,
0.000137303169305359,0.000203636706671983,0.000256396220959709,0.000256540237295736,
0.000285209320207733,0.000342105100635654,0.000384776935956595,0.000400778874201948,
0.000456785658060682,0.00048478904999005,0.000498790745954733,0.000512792441919417),
 .UNSPECIFIED.);
#4411=B_SPLINE_CURVE_WITH_KNOTS('',3,(#174808,#174809,#174810,#174811,#174812,
#174813,#174814,#174815,#174816,#174817,#174818,#174819,#174820,#174821,
#174822,#174823,#174824,#174825,#174826,#174827,#174828,#174829,#174830,
#174831,#174832,#174833,#174834,#174835,#174836,#174837,#174838,#174839,
#174840,#174841,#174842,#174843,#174844),.UNSPECIFIED.,.F.,.F.,(4,3,3,3,
3,3,3,3,3,3,3,3,4),(0.,1.12535551670966E-5,7.76936938395229E-5,0.000102513517961087,
0.00012187918982424,0.000189659041345274,0.00022354896710579,0.00025729409909612,
0.000257438892866307,0.000325720851748994,0.000396486773942172,0.000466242707643575,
0.000514877785732614),.UNSPECIFIED.);
#4412=B_SPLINE_CURVE_WITH_KNOTS('',3,(#174852,#174853,#174854,#174855,#174856,
#174857,#174858,#174859,#174860,#174861,#174862,#174863,#174864,#174865,
#174866,#174867,#174868,#174869,#174870,#174871,#174872,#174873,#174874,
#174875,#174876,#174877,#174878,#174879,#174880,#174881,#174882,#174883,
#174884,#174885,#174886,#174887,#174888,#174889,#174890,#174891),
 .UNSPECIFIED.,.F.,.F.,(4,3,3,3,3,3,3,3,3,3,3,3,3,4),(0.,6.80370855330231E-5,
0.000137303169291361,0.000203636706653042,0.000256396220959707,0.000256540237295735,
0.000285209320207733,0.000342105100635653,0.000384776935956594,0.000400778874201946,
0.00045678565806068,0.000484789049990047,0.00049879074595473,0.000512792441919414),
 .UNSPECIFIED.);
#4413=B_SPLINE_CURVE_WITH_KNOTS('',3,(#174895,#174896,#174897,#174898,#174899,
#174900,#174901,#174902,#174903,#174904,#174905,#174906,#174907,#174908,
#174909,#174910,#174911,#174912,#174913,#174914,#174915,#174916,#174917,
#174918,#174919,#174920,#174921,#174922,#174923,#174924,#174925,#174926,
#174927,#174928,#174929,#174930,#174931),.UNSPECIFIED.,.F.,.F.,(4,3,3,3,
3,3,3,3,3,3,3,3,4),(0.,1.12535551670998E-5,7.76936938476081E-5,0.000102513517961124,
0.000121879189824272,0.000189659041345288,0.000223548967105796,0.000257294099096119,
0.000257438892866305,0.000325720851753445,0.000396486773950165,0.000466242707652896,
0.000514877785732609),.UNSPECIFIED.);
#4414=B_SPLINE_CURVE_WITH_KNOTS('',3,(#174939,#174940,#174941,#174942,#174943,
#174944,#174945,#174946,#174947,#174948,#174949,#174950,#174951,#174952,
#174953,#174954,#174955,#174956,#174957,#174958,#174959,#174960,#174961,
#174962,#174963,#174964,#174965,#174966,#174967,#174968,#174969,#174970,
#174971,#174972,#174973,#174974,#174975,#174976,#174977,#174978),
 .UNSPECIFIED.,.F.,.F.,(4,3,3,3,3,3,3,3,3,3,3,3,3,4),(0.,6.80370855325344E-5,
0.000137303169290103,0.000203636706650601,0.000256396220959707,0.000256540237295731,
0.000285209320207729,0.00034210510063565,0.000384776935956591,0.000400778874201944,
0.000456785658060678,0.000484789049990046,0.00049879074595473,0.000512792441919413),
 .UNSPECIFIED.);
#4415=B_SPLINE_CURVE_WITH_KNOTS('',3,(#174982,#174983,#174984,#174985,#174986,
#174987,#174988,#174989,#174990,#174991,#174992,#174993,#174994,#174995,
#174996,#174997,#174998,#174999,#175000,#175001,#175002,#175003,#175004,
#175005,#175006,#175007,#175008,#175009,#175010,#175011,#175012,#175013,
#175014,#175015,#175016,#175017,#175018),.UNSPECIFIED.,.F.,.F.,(4,3,3,3,
3,3,3,3,3,3,3,3,4),(0.,1.12535551670955E-5,7.76936938495978E-5,0.000102513517961049,
0.000121879189824206,0.000189659041345252,0.000223548967105776,0.000257294099096094,
0.000257438892866299,0.000325720851750144,0.000396486773944257,0.000466242707645802,
0.000514877785732598),.UNSPECIFIED.);
#4416=B_SPLINE_CURVE_WITH_KNOTS('',3,(#175026,#175027,#175028,#175029,#175030,
#175031,#175032,#175033,#175034,#175035,#175036,#175037,#175038,#175039,
#175040,#175041,#175042,#175043,#175044,#175045,#175046,#175047,#175048,
#175049,#175050,#175051,#175052,#175053,#175054,#175055,#175056,#175057,
#175058,#175059,#175060,#175061,#175062,#175063,#175064,#175065),
 .UNSPECIFIED.,.F.,.F.,(4,3,3,3,3,3,3,3,3,3,3,3,3,4),(0.,6.80370855436682E-5,
0.000137303169312912,0.00020363670668485,0.00025639622095971,0.000256540237295729,
0.000285209320207753,0.00034210510063567,0.000384776935956608,0.000400778874201959,
0.00045678565806069,0.000484789049990056,0.000498790745954738,0.000512792441919421),
 .UNSPECIFIED.);
#4417=B_SPLINE_CURVE_WITH_KNOTS('',3,(#175069,#175070,#175071,#175072,#175073,
#175074,#175075,#175076,#175077,#175078,#175079,#175080,#175081,#175082,
#175083,#175084,#175085,#175086,#175087,#175088,#175089,#175090,#175091,
#175092,#175093,#175094,#175095,#175096,#175097,#175098,#175099,#175100,
#175101,#175102,#175103,#175104,#175105),.UNSPECIFIED.,.F.,.F.,(4,3,3,3,
3,3,3,3,3,3,3,3,4),(0.,1.12535551670953E-5,7.76936938401081E-5,0.000102513517961066,
0.00012187918982422,0.000189659041345261,0.000223548967105781,0.000257294099096089,
0.000257438892866301,0.000325720851764136,0.000396486773972714,0.000466242707687174,
0.000514877785732603),.UNSPECIFIED.);
#4418=B_SPLINE_CURVE_WITH_KNOTS('',3,(#175113,#175114,#175115,#175116,#175117,
#175118,#175119,#175120,#175121,#175122,#175123,#175124,#175125,#175126,
#175127,#175128,#175129,#175130,#175131,#175132,#175133,#175134,#175135,
#175136,#175137,#175138,#175139,#175140,#175141,#175142,#175143,#175144,
#175145,#175146,#175147,#175148,#175149,#175150,#175151,#175152),
 .UNSPECIFIED.,.F.,.F.,(4,3,3,3,3,3,3,3,3,3,3,3,3,4),(0.,6.80370855328581E-5,
0.000137303169290931,0.000203636706652317,0.000256396220959702,0.000256540237295726,
0.000285209320207734,0.000342105100635652,0.00038477693595659,0.000400778874201942,
0.000456785658060673,0.000484789049990039,0.000498790745954722,0.000512792441919405),
 .UNSPECIFIED.);
#4419=B_SPLINE_CURVE_WITH_KNOTS('',3,(#175156,#175157,#175158,#175159,#175160,
#175161,#175162,#175163,#175164,#175165,#175166,#175167,#175168,#175169,
#175170,#175171,#175172,#175173,#175174,#175175,#175176,#175177,#175178,
#175179,#175180,#175181,#175182,#175183,#175184,#175185,#175186,#175187,
#175188,#175189,#175190,#175191,#175192),.UNSPECIFIED.,.F.,.F.,(4,3,3,3,
3,3,3,3,3,3,3,3,4),(0.,1.12535551670997E-5,7.76936938475713E-5,0.00010251351796112,
0.000121879189824268,0.000189659041345287,0.000223548967105797,0.000257294099096103,
0.000257438892866306,0.000325720851765822,0.000396486773977161,0.000466242707695556,
0.000514877785732613),.UNSPECIFIED.);
#4420=B_SPLINE_CURVE_WITH_KNOTS('',3,(#175200,#175201,#175202,#175203,#175204,
#175205,#175206,#175207,#175208,#175209,#175210,#175211,#175212,#175213,
#175214,#175215,#175216,#175217,#175218,#175219,#175220,#175221,#175222,
#175223,#175224,#175225,#175226,#175227,#175228,#175229,#175230,#175231,
#175232,#175233,#175234,#175235,#175236,#175237,#175238,#175239),
 .UNSPECIFIED.,.F.,.F.,(4,3,3,3,3,3,3,3,3,3,3,3,3,4),(0.,6.80370855398214E-5,
0.000137303169304995,0.00020363670667273,0.000256396220959706,0.000256540237295733,
0.000285209320207728,0.000342105100635649,0.00038477693595659,0.000400778874201943,
0.000456785658060678,0.000484789049990045,0.000498790745954729,0.000512792441919412),
 .UNSPECIFIED.);
#4421=B_SPLINE_CURVE_WITH_KNOTS('',3,(#175243,#175244,#175245,#175246,#175247,
#175248,#175249,#175250,#175251,#175252,#175253,#175254,#175255,#175256,
#175257,#175258,#175259,#175260,#175261,#175262,#175263,#175264,#175265,
#175266,#175267,#175268,#175269,#175270,#175271,#175272,#175273,#175274,
#175275,#175276,#175277,#175278,#175279),.UNSPECIFIED.,.F.,.F.,(4,3,3,3,
3,3,3,3,3,3,3,3,4),(0.,1.12535551670982E-5,7.76936938418339E-5,0.000102513517961084,
0.000121879189824238,0.000189659041345274,0.000223548967105792,0.000257294099096109,
0.000257438892866311,0.000325720851765796,0.000396486773976165,0.000466242707692333,
0.000514877785732621),.UNSPECIFIED.);
#4422=B_SPLINE_CURVE_WITH_KNOTS('',3,(#175287,#175288,#175289,#175290,#175291,
#175292,#175293,#175294,#175295,#175296,#175297,#175298,#175299,#175300,
#175301,#175302,#175303,#175304,#175305,#175306,#175307,#175308,#175309,
#175310,#175311,#175312,#175313,#175314,#175315,#175316,#175317,#175318,
#175319,#175320,#175321,#175322,#175323,#175324,#175325,#175326),
 .UNSPECIFIED.,.F.,.F.,(4,3,3,3,3,3,3,3,3,3,3,3,3,4),(0.,6.80370855336509E-5,
0.000137303169291916,0.000203636706652182,0.000256396220959706,0.000256540237295742,
0.000285209320207705,0.000342105100635632,0.000384776935956577,0.000400778874201931,
0.000456785658060672,0.000484789049990042,0.000498790745954727,0.000512792441919412),
 .UNSPECIFIED.);
#4423=B_SPLINE_CURVE_WITH_KNOTS('',3,(#175330,#175331,#175332,#175333,#175334,
#175335,#175336,#175337,#175338,#175339,#175340,#175341,#175342,#175343,
#175344,#175345,#175346,#175347,#175348,#175349,#175350,#175351,#175352,
#175353,#175354,#175355,#175356,#175357,#175358,#175359,#175360,#175361,
#175362,#175363,#175364,#175365,#175366),.UNSPECIFIED.,.F.,.F.,(4,3,3,3,
3,3,3,3,3,3,3,3,4),(0.,1.12535551671027E-5,7.76936938492863E-5,0.000102513517961115,
0.000121879189824264,0.000189659041345283,0.000223548967105793,0.000257294099096098,
0.000257438892866303,0.000325720851756605,0.00039648677395862,0.000466242707669241,
0.000514877785732606),.UNSPECIFIED.);
#4424=B_SPLINE_CURVE_WITH_KNOTS('',3,(#175374,#175375,#175376,#175377,#175378,
#175379,#175380,#175381,#175382,#175383,#175384,#175385,#175386,#175387,
#175388,#175389,#175390,#175391,#175392,#175393,#175394,#175395,#175396,
#175397,#175398,#175399,#175400,#175401,#175402,#175403,#175404,#175405,
#175406,#175407,#175408,#175409,#175410,#175411,#175412,#175413),
 .UNSPECIFIED.,.F.,.F.,(4,3,3,3,3,3,3,3,3,3,3,3,3,4),(0.,6.80370855510928E-5,
0.000137303169327734,0.000203636706706446,0.000256396220959707,0.000256540237295735,
0.000285209320207741,0.000342105100635659,0.000384776935956598,0.00040077887420195,
0.000456785658060681,0.000484789049990047,0.00049879074595473,0.000512792441919413),
 .UNSPECIFIED.);
#4425=B_SPLINE_CURVE_WITH_KNOTS('',3,(#175417,#175418,#175419,#175420,#175421,
#175422,#175423,#175424,#175425,#175426,#175427,#175428,#175429,#175430,
#175431,#175432,#175433,#175434,#175435,#175436,#175437,#175438,#175439,
#175440,#175441,#175442,#175443,#175444,#175445,#175446,#175447,#175448,
#175449,#175450,#175451,#175452,#175453),.UNSPECIFIED.,.F.,.F.,(4,3,3,3,
3,3,3,3,3,3,3,3,4),(0.,1.12535551671005E-5,7.7693693864023E-5,0.000102513517961177,
0.000121879189824318,0.000189659041345312,0.000223548967105808,0.000257294099096088,
0.000257438892866305,0.00032572085175239,0.000396486773948841,0.00046624270765219,
0.00051487778573261),.UNSPECIFIED.);
#4426=B_SPLINE_CURVE_WITH_KNOTS('',3,(#175461,#175462,#175463,#175464,#175465,
#175466,#175467,#175468,#175469,#175470,#175471,#175472,#175473,#175474,
#175475,#175476,#175477,#175478,#175479,#175480,#175481,#175482,#175483,
#175484,#175485,#175486,#175487,#175488,#175489,#175490,#175491,#175492,
#175493,#175494,#175495,#175496,#175497,#175498,#175499,#175500),
 .UNSPECIFIED.,.F.,.F.,(4,3,3,3,3,3,3,3,3,3,3,3,3,4),(0.,6.80370855290005E-5,
0.000137303169282125,0.000203636706636526,0.000256396220959704,0.000256540237295738,
0.000285209320207738,0.000342105100635655,0.000384776935956594,0.000400778874201945,
0.000456785658060677,0.000484789049990042,0.000498790745954725,0.000512792441919408),
 .UNSPECIFIED.);
#4427=B_SPLINE_CURVE_WITH_KNOTS('',3,(#175504,#175505,#175506,#175507,#175508,
#175509,#175510,#175511,#175512,#175513,#175514,#175515,#175516,#175517,
#175518,#175519,#175520,#175521,#175522,#175523,#175524,#175525,#175526,
#175527,#175528,#175529,#175530,#175531,#175532,#175533,#175534,#175535,
#175536,#175537,#175538,#175539,#175540),.UNSPECIFIED.,.F.,.F.,(4,3,3,3,
3,3,3,3,3,3,3,3,4),(0.,1.12535551670973E-5,7.76936938483821E-5,0.000102513517961069,
0.000121879189824223,0.000189659041345262,0.000223548967105782,0.000257294099096089,
0.000257438892866301,0.000325720851754469,0.000396486773953083,0.000466242707658755,
0.000514877785732602),.UNSPECIFIED.);
#4428=B_SPLINE_CURVE_WITH_KNOTS('',3,(#175548,#175549,#175550,#175551,#175552,
#175553,#175554,#175555,#175556,#175557,#175558,#175559,#175560,#175561,
#175562,#175563,#175564,#175565,#175566,#175567,#175568,#175569,#175570,
#175571,#175572,#175573,#175574,#175575,#175576,#175577,#175578,#175579,
#175580,#175581,#175582,#175583,#175584,#175585,#175586,#175587),
 .UNSPECIFIED.,.F.,.F.,(4,3,3,3,3,3,3,3,3,3,3,3,3,4),(0.,6.80370855443474E-5,
0.000137303169313637,0.00020363670668462,0.000256396220959708,0.000256540237295739,
0.000285209320207743,0.000342105100635661,0.0003847769359566,0.000400778874201952,
0.000456785658060683,0.000484789049990049,0.000498790745954732,0.000512792441919415),
 .UNSPECIFIED.);
#4429=B_SPLINE_CURVE_WITH_KNOTS('',3,(#175591,#175592,#175593,#175594,#175595,
#175596,#175597,#175598,#175599,#175600,#175601,#175602,#175603,#175604,
#175605,#175606,#175607,#175608,#175609,#175610,#175611,#175612,#175613,
#175614,#175615,#175616,#175617,#175618,#175619,#175620,#175621,#175622,
#175623,#175624,#175625,#175626,#175627),.UNSPECIFIED.,.F.,.F.,(4,3,3,3,
3,3,3,3,3,3,3,3,4),(0.,1.12535551670978E-5,7.76936938552473E-5,0.000102513517961072,
0.000121879189824226,0.000189659041345266,0.000223548967105787,0.000257294099096106,
0.000257438892866307,0.000325720851749875,0.000396486773943902,0.000466242707645584,
0.000514877785732614),.UNSPECIFIED.);
#4430=B_SPLINE_CURVE_WITH_KNOTS('',3,(#175635,#175636,#175637,#175638,#175639,
#175640,#175641,#175642,#175643,#175644,#175645,#175646,#175647,#175648,
#175649,#175650,#175651,#175652,#175653,#175654,#175655,#175656,#175657,
#175658,#175659,#175660,#175661,#175662,#175663,#175664,#175665,#175666,
#175667,#175668,#175669,#175670,#175671,#175672,#175673,#175674),
 .UNSPECIFIED.,.F.,.F.,(4,3,3,3,3,3,3,3,3,3,3,3,3,4),(0.,6.80370855381467E-5,
0.000137303169301509,0.000203636706667771,0.000256396220959704,0.000256540237295722,
0.000285209320207738,0.000342105100635655,0.000384776935956594,0.000400778874201945,
0.000456785658060677,0.000484789049990042,0.000498790745954725,0.000512792441919408),
 .UNSPECIFIED.);
#4431=B_SPLINE_CURVE_WITH_KNOTS('',3,(#175678,#175679,#175680,#175681,#175682,
#175683,#175684,#175685,#175686,#175687,#175688,#175689,#175690,#175691,
#175692,#175693,#175694,#175695,#175696,#175697,#175698,#175699,#175700,
#175701,#175702,#175703,#175704,#175705,#175706,#175707,#175708,#175709,
#175710,#175711,#175712,#175713,#175714),.UNSPECIFIED.,.F.,.F.,(4,3,3,3,
3,3,3,3,3,3,3,3,4),(0.,1.12535551670998E-5,7.76936938400932E-5,0.000102513517961126,
0.000121879189824273,0.000189659041345289,0.000223548967105797,0.000257294099096098,
0.000257438892866305,0.000325720851765772,0.000396486773975871,0.000466242707691754,
0.00051487778573261),.UNSPECIFIED.);
#4432=B_SPLINE_CURVE_WITH_KNOTS('',3,(#175722,#175723,#175724,#175725,#175726,
#175727,#175728,#175729,#175730,#175731,#175732,#175733,#175734,#175735,
#175736,#175737,#175738,#175739,#175740,#175741,#175742,#175743,#175744,
#175745,#175746,#175747,#175748,#175749,#175750,#175751,#175752,#175753,
#175754,#175755,#175756,#175757,#175758,#175759,#175760,#175761),
 .UNSPECIFIED.,.F.,.F.,(4,3,3,3,3,3,3,3,3,3,3,3,3,4),(0.,6.80370855358042E-5,
0.000137303169296868,0.000203636706660701,0.000256396220959706,0.000256540237295732,
0.00028520932020774,0.000342105100635658,0.000384776935956596,0.000400778874201948,
0.00045678565806068,0.000484789049990046,0.000498790745954728,0.000512792441919411),
 .UNSPECIFIED.);
#4433=B_SPLINE_CURVE_WITH_KNOTS('',3,(#175765,#175766,#175767,#175768,#175769,
#175770,#175771,#175772,#175773,#175774,#175775,#175776,#175777,#175778,
#175779,#175780,#175781,#175782,#175783,#175784,#175785,#175786,#175787,
#175788,#175789,#175790,#175791,#175792,#175793,#175794,#175795,#175796,
#175797,#175798,#175799,#175800,#175801),.UNSPECIFIED.,.F.,.F.,(4,3,3,3,
3,3,3,3,3,3,3,3,4),(0.,1.12535551671032E-5,7.76936938466288E-5,0.000102513517961138,
0.000121879189824284,0.000189659041345294,0.000223548967105799,0.000257294099096093,
0.000257438892866304,0.000325720851754854,0.000396486773954175,0.000466242707660958,
0.000514877785732608),.UNSPECIFIED.);
#4434=B_SPLINE_CURVE_WITH_KNOTS('',3,(#175809,#175810,#175811,#175812,#175813,
#175814,#175815,#175816,#175817,#175818,#175819,#175820,#175821,#175822,
#175823,#175824,#175825,#175826,#175827,#175828,#175829,#175830,#175831,
#175832,#175833,#175834,#175835,#175836,#175837,#175838,#175839,#175840,
#175841,#175842,#175843,#175844,#175845,#175846,#175847,#175848),
 .UNSPECIFIED.,.F.,.F.,(4,3,3,3,3,3,3,3,3,3,3,3,3,4),(0.,6.8037085539341E-5,
0.000137303169304,0.000203636706671485,0.000256396220959705,0.000256540237295733,
0.000285209320207739,0.000342105100635656,0.000384776935956594,0.000400778874201946,
0.000456785658060678,0.000484789049990043,0.000498790745954726,0.000512792441919409),
 .UNSPECIFIED.);
#4435=B_SPLINE_CURVE_WITH_KNOTS('',3,(#175855,#175856,#175857,#175858,#175859,
#175860,#175861,#175862,#175863,#175864,#175865,#175866,#175867,#175868,
#175869,#175870,#175871,#175872,#175873,#175874,#175875,#175876,#175877,
#175878,#175879,#175880,#175881,#175882,#175883,#175884,#175885,#175886,
#175887,#175888,#175889,#175890,#175891),.UNSPECIFIED.,.F.,.F.,(4,3,3,3,
3,3,3,3,3,3,3,3,4),(0.,1.12535551671012E-5,7.76936938518268E-5,0.000102513517961145,
0.00012187918982429,0.000189659041345297,0.000223548967105801,0.000257294099096108,
0.000257438892866305,0.000325720851757891,0.000396486773960361,0.000466242707669812,
0.00051487778573261),.UNSPECIFIED.);
#4436=B_SPLINE_CURVE_WITH_KNOTS('',3,(#175899,#175900,#175901,#175902,#175903,
#175904,#175905,#175906,#175907,#175908,#175909,#175910,#175911,#175912,
#175913,#175914,#175915,#175916,#175917,#175918,#175919,#175920,#175921,
#175922,#175923,#175924,#175925,#175926,#175927,#175928,#175929,#175930,
#175931,#175932,#175933,#175934,#175935,#175936,#175937,#175938),
 .UNSPECIFIED.,.F.,.F.,(4,3,3,3,3,3,3,3,3,3,3,3,3,4),(0.,6.8037085541032E-5,
0.000137303169307532,0.000203636706676779,0.000256396220959702,0.00025654023729573,
0.000285209320207736,0.000342105100635653,0.000384776935956591,0.000400778874201943,
0.000456785658060674,0.000484789049990039,0.000498790745954722,0.000512792441919405),
 .UNSPECIFIED.);
#4437=B_SPLINE_CURVE_WITH_KNOTS('',3,(#175942,#175943,#175944,#175945,#175946,
#175947,#175948,#175949,#175950,#175951,#175952,#175953,#175954,#175955,
#175956,#175957,#175958,#175959,#175960,#175961,#175962,#175963,#175964,
#175965,#175966,#175967,#175968,#175969,#175970,#175971,#175972,#175973,
#175974,#175975,#175976,#175977,#175978),.UNSPECIFIED.,.F.,.F.,(4,3,3,3,
3,3,3,3,3,3,3,3,4),(0.,1.1253555167099E-5,7.76936938452608E-5,0.000102513517961139,
0.000121879189824284,0.000189659041345294,0.000223548967105799,0.00025729409909611,
0.000257438892866304,0.000325720851760016,0.000396486773964437,0.000466242707675329,
0.000514877785732608),.UNSPECIFIED.);
#4438=B_SPLINE_CURVE_WITH_KNOTS('',3,(#175986,#175987,#175988,#175989,#175990,
#175991,#175992,#175993,#175994,#175995,#175996,#175997,#175998,#175999,
#176000,#176001,#176002,#176003,#176004,#176005,#176006,#176007,#176008,
#176009,#176010,#176011,#176012,#176013,#176014,#176015,#176016,#176017,
#176018,#176019,#176020,#176021,#176022,#176023,#176024,#176025),
 .UNSPECIFIED.,.F.,.F.,(4,3,3,3,3,3,3,3,3,3,3,3,3,4),(0.,6.80370855344135E-5,
0.000137303169294105,0.000203636706657015,0.000256396220959704,0.000256540237295728,
0.000285209320207741,0.000342105100635657,0.000384776935956595,0.000400778874201946,
0.000456785658060677,0.000484789049990042,0.000498790745954725,0.000512792441919407),
 .UNSPECIFIED.);
#4439=B_SPLINE_CURVE_WITH_KNOTS('',3,(#176029,#176030,#176031,#176032,#176033,
#176034,#176035,#176036,#176037,#176038,#176039,#176040,#176041,#176042,
#176043,#176044,#176045,#176046,#176047,#176048,#176049,#176050,#176051,
#176052,#176053,#176054,#176055,#176056,#176057,#176058,#176059,#176060,
#176061,#176062,#176063,#176064,#176065),.UNSPECIFIED.,.F.,.F.,(4,3,3,3,
3,3,3,3,3,3,3,3,4),(0.,1.12535551670998E-5,7.76936938473757E-5,0.000102513517961127,
0.000121879189824274,0.000189659041345289,0.000223548967105796,0.000257294099096108,
0.000257438892866304,0.000325720851760781,0.000396486773966304,0.000466242707678675,
0.000514877785732608),.UNSPECIFIED.);
#4440=B_SPLINE_CURVE_WITH_KNOTS('',3,(#176073,#176074,#176075,#176076,#176077,
#176078,#176079,#176080,#176081,#176082,#176083,#176084,#176085,#176086,
#176087,#176088,#176089,#176090,#176091,#176092,#176093,#176094,#176095,
#176096,#176097,#176098,#176099,#176100,#176101,#176102,#176103,#176104,
#176105,#176106,#176107,#176108,#176109,#176110,#176111,#176112),
 .UNSPECIFIED.,.F.,.F.,(4,3,3,3,3,3,3,3,3,3,3,3,3,4),(0.,6.80370855324475E-5,
0.000137303169290076,0.000203636706650847,0.000256396220959707,0.000256540237295739,
0.000285209320207734,0.000342105100635654,0.000384776935956594,0.000400778874201946,
0.00045678565806068,0.000484789049990047,0.00049879074595473,0.000512792441919413),
 .UNSPECIFIED.);
#4441=B_SPLINE_CURVE_WITH_KNOTS('',3,(#176116,#176117,#176118,#176119,#176120,
#176121,#176122,#176123,#176124,#176125,#176126,#176127,#176128,#176129,
#176130,#176131,#176132,#176133,#176134,#176135,#176136,#176137,#176138,
#176139,#176140,#176141,#176142,#176143,#176144,#176145,#176146,#176147,
#176148,#176149,#176150,#176151,#176152),.UNSPECIFIED.,.F.,.F.,(4,3,3,3,
3,3,3,3,3,3,3,3,4),(0.,1.12535551671022E-5,7.7693693845666E-5,0.00010251351796117,
0.000121879189824311,0.000189659041345307,0.000223548967105805,0.000257294099096107,
0.000257438892866303,0.00032572085175553,0.000396486773955308,0.00046624270766216,
0.000514877785732605),.UNSPECIFIED.);
#4442=B_SPLINE_CURVE_WITH_KNOTS('',3,(#176160,#176161,#176162,#176163,#176164,
#176165,#176166,#176167,#176168,#176169,#176170,#176171,#176172,#176173,
#176174,#176175,#176176,#176177,#176178,#176179,#176180,#176181,#176182,
#176183,#176184,#176185,#176186,#176187,#176188,#176189,#176190,#176191,
#176192,#176193,#176194,#176195,#176196,#176197,#176198,#176199),
 .UNSPECIFIED.,.F.,.F.,(4,3,3,3,3,3,3,3,3,3,3,3,3,4),(0.,6.8037085543224E-5,
0.000137303169311952,0.000203636706683699,0.000256396220959705,0.000256540237295732,
0.000285209320207731,0.00034210510063565,0.00038477693595659,0.000400778874201943,
0.000456785658060676,0.000484789049990043,0.000498790745954727,0.00051279244191941),
 .UNSPECIFIED.);
#4443=B_SPLINE_CURVE_WITH_KNOTS('',3,(#176203,#176204,#176205,#176206,#176207,
#176208,#176209,#176210,#176211,#176212,#176213,#176214,#176215,#176216,
#176217,#176218,#176219,#176220,#176221,#176222,#176223,#176224,#176225,
#176226,#176227,#176228,#176229,#176230,#176231,#176232,#176233,#176234,
#176235,#176236,#176237,#176238,#176239),.UNSPECIFIED.,.F.,.F.,(4,3,3,3,
3,3,3,3,3,3,3,3,4),(0.,1.12535551671005E-5,7.7693693841547E-5,0.000102513517961162,
0.000121879189824305,0.000189659041345307,0.000223548967105808,0.000257294099096097,
0.000257438892866309,0.000325720851762212,0.000396486773968726,0.000466242707681267,
0.000514877785732617),.UNSPECIFIED.);
#4444=B_SPLINE_CURVE_WITH_KNOTS('',3,(#176247,#176248,#176249,#176250,#176251,
#176252,#176253,#176254,#176255,#176256,#176257,#176258,#176259,#176260,
#176261,#176262,#176263,#176264,#176265,#176266,#176267,#176268,#176269,
#176270,#176271,#176272,#176273,#176274,#176275,#176276,#176277,#176278,
#176279,#176280,#176281,#176282,#176283,#176284,#176285,#176286),
 .UNSPECIFIED.,.F.,.F.,(4,3,3,3,3,3,3,3,3,3,3,3,3,4),(0.,6.80370855366589E-5,
0.000137303169298556,0.00020363670666332,0.000256396220959708,0.000256540237295731,
0.000285209320207723,0.000342105100635647,0.000384776935956589,0.000400778874201942,
0.000456785658060679,0.000484789049990048,0.000498790745954732,0.000512792441919417),
 .UNSPECIFIED.);
#4445=B_SPLINE_CURVE_WITH_KNOTS('',3,(#176290,#176291,#176292,#176293,#176294,
#176295,#176296,#176297,#176298,#176299,#176300,#176301,#176302,#176303,
#176304,#176305,#176306,#176307,#176308,#176309,#176310,#176311,#176312,
#176313,#176314,#176315,#176316,#176317,#176318,#176319,#176320,#176321,
#176322,#176323,#176324,#176325,#176326),.UNSPECIFIED.,.F.,.F.,(4,3,3,3,
3,3,3,3,3,3,3,3,4),(0.,1.12535551670983E-5,7.76936938510176E-5,0.000102513517961093,
0.000121879189824245,0.000189659041345275,0.00022354896710579,0.000257294099096106,
0.000257438892866305,0.00032572085175851,0.000396486773961158,0.000466242707670101,
0.0005148777857326),.UNSPECIFIED.);
#4446=B_SPLINE_CURVE_WITH_KNOTS('',3,(#176334,#176335,#176336,#176337,#176338,
#176339,#176340,#176341,#176342,#176343,#176344,#176345,#176346,#176347,
#176348,#176349,#176350,#176351,#176352,#176353,#176354,#176355,#176356,
#176357,#176358,#176359,#176360,#176361,#176362,#176363,#176364,#176365,
#176366,#176367,#176368,#176369,#176370,#176371,#176372,#176373),
 .UNSPECIFIED.,.F.,.F.,(4,3,3,3,3,3,3,3,3,3,3,3,3,4),(0.,6.80370855381278E-5,
0.000137303169302431,0.000203636706670777,0.000256396220959703,0.000256540237295731,
0.000285209320207733,0.000342105100635651,0.00038477693595659,0.000400778874201942,
0.000456785658060674,0.00048478904999004,0.000498790745954723,0.000512792441919405),
 .UNSPECIFIED.);
#4447=B_SPLINE_CURVE_WITH_KNOTS('',3,(#176377,#176378,#176379,#176380,#176381,
#176382,#176383,#176384,#176385,#176386,#176387,#176388,#176389,#176390,
#176391,#176392,#176393,#176394,#176395,#176396,#176397,#176398,#176399,
#176400,#176401,#176402,#176403,#176404,#176405,#176406,#176407,#176408,
#176409,#176410,#176411,#176412,#176413),.UNSPECIFIED.,.F.,.F.,(4,3,3,3,
3,3,3,3,3,3,3,3,4),(0.,1.12535551671016E-5,7.76936938479796E-5,0.000102513517961101,
0.000121879189824252,0.000189659041345279,0.000223548967105792,0.000257294099096099,
0.000257438892866305,0.000325720851745948,0.000396486773936273,0.000466242707635578,
0.000514877785732611),.UNSPECIFIED.);
#4448=B_SPLINE_CURVE_WITH_KNOTS('',3,(#176421,#176422,#176423,#176424,#176425,
#176426,#176427,#176428,#176429,#176430,#176431,#176432,#176433,#176434,
#176435,#176436,#176437,#176438,#176439,#176440,#176441,#176442,#176443,
#176444,#176445,#176446,#176447,#176448,#176449,#176450,#176451,#176452,
#176453,#176454,#176455,#176456,#176457,#176458,#176459,#176460),
 .UNSPECIFIED.,.F.,.F.,(4,3,3,3,3,3,3,3,3,3,3,3,3,4),(0.,6.80370855407977E-5,
0.0001373031693065,0.00020363670667411,0.000256396220959709,0.00025654023729572,
0.000285209320207748,0.000342105100635665,0.000384776935956604,0.000400778874201955,
0.000456785658060687,0.000484789049990053,0.000498790745954735,0.000512792441919418),
 .UNSPECIFIED.);
#4449=B_SPLINE_CURVE_WITH_KNOTS('',3,(#176464,#176465,#176466,#176467,#176468,
#176469,#176470,#176471,#176472,#176473,#176474,#176475,#176476,#176477,
#176478,#176479,#176480,#176481,#176482,#176483,#176484,#176485,#176486,
#176487,#176488,#176489,#176490,#176491,#176492,#176493,#176494,#176495,
#176496,#176497,#176498,#176499,#176500),.UNSPECIFIED.,.F.,.F.,(4,3,3,3,
3,3,3,3,3,3,3,3,4),(0.,1.12535551671054E-5,7.76936938616112E-5,0.000102513517961212,
0.000121879189824349,0.000189659041345329,0.00022354896710582,0.00025729409909611,
0.00025743889286631,0.000325720851754512,0.000396486773953998,0.000466242707661241,
0.00051487778573262),.UNSPECIFIED.);
#4450=B_SPLINE_CURVE_WITH_KNOTS('',3,(#176508,#176509,#176510,#176511,#176512,
#176513,#176514,#176515,#176516,#176517,#176518,#176519,#176520,#176521,
#176522,#176523,#176524,#176525,#176526,#176527,#176528,#176529,#176530,
#176531,#176532,#176533,#176534,#176535,#176536,#176537,#176538,#176539,
#176540,#176541,#176542,#176543,#176544,#176545,#176546,#176547),
 .UNSPECIFIED.,.F.,.F.,(4,3,3,3,3,3,3,3,3,3,3,3,3,4),(0.,6.80370855414931E-5,
0.000137303169307904,0.000203636706675899,0.000256396220959702,0.000256540237295727,
0.00028520932020771,0.000342105100635634,0.000384776935956576,0.00040077887420193,
0.000456785658060667,0.000484789049990036,0.00049879074595472,0.000512792441919405),
 .UNSPECIFIED.);
#4451=B_SPLINE_CURVE_WITH_KNOTS('',3,(#176551,#176552,#176553,#176554,#176555,
#176556,#176557,#176558,#176559,#176560,#176561,#176562,#176563,#176564,
#176565,#176566,#176567,#176568,#176569,#176570,#176571,#176572,#176573,
#176574,#176575,#176576,#176577,#176578,#176579,#176580,#176581,#176582,
#176583,#176584,#176585,#176586,#176587),.UNSPECIFIED.,.F.,.F.,(4,3,3,3,
3,3,3,3,3,3,3,3,4),(0.,1.12535551671044E-5,7.76936938352556E-5,0.000102513517961147,
0.000121879189824292,0.000189659041345301,0.000223548967105805,0.000257294099096117,
0.00025743889286631,0.000325720851753075,0.000396486773950483,0.000466242707655942,
0.000514877785732619),.UNSPECIFIED.);
#4452=B_SPLINE_CURVE_WITH_KNOTS('',3,(#176595,#176596,#176597,#176598,#176599,
#176600,#176601,#176602,#176603,#176604,#176605,#176606,#176607,#176608,
#176609,#176610,#176611,#176612,#176613,#176614,#176615,#176616,#176617,
#176618,#176619,#176620,#176621,#176622,#176623,#176624,#176625,#176626,
#176627,#176628,#176629,#176630,#176631,#176632,#176633,#176634),
 .UNSPECIFIED.,.F.,.F.,(4,3,3,3,3,3,3,3,3,3,3,3,3,4),(0.,6.80370855377875E-5,
0.000137303169301054,0.000203636706667488,0.000256396220959705,0.00025654023729572,
0.000285209320207726,0.000342105100635647,0.000384776935956588,0.00040077887420194,
0.000456785658060675,0.000484789049990043,0.000498790745954726,0.00051279244191941),
 .UNSPECIFIED.);
#4453=B_SPLINE_CURVE_WITH_KNOTS('',3,(#176638,#176639,#176640,#176641,#176642,
#176643,#176644,#176645,#176646,#176647,#176648,#176649,#176650,#176651,
#176652,#176653,#176654,#176655,#176656,#176657,#176658,#176659,#176660,
#176661,#176662,#176663,#176664,#176665,#176666,#176667,#176668,#176669,
#176670,#176671,#176672,#176673,#176674),.UNSPECIFIED.,.F.,.F.,(4,3,3,3,
3,3,3,3,3,3,3,3,4),(0.,1.12535551671036E-5,7.76936938472083E-5,0.000102513517961145,
0.00012187918982429,0.000189659041345296,0.000223548967105799,0.000257294099096105,
0.000257438892866302,0.000325720851742521,0.000396486773928871,0.000466242707623768,
0.000514877785732603),.UNSPECIFIED.);
#4454=B_SPLINE_CURVE_WITH_KNOTS('',3,(#176682,#176683,#176684,#176685,#176686,
#176687,#176688,#176689,#176690,#176691,#176692,#176693,#176694,#176695,
#176696,#176697,#176698,#176699,#176700,#176701,#176702,#176703,#176704,
#176705,#176706,#176707,#176708,#176709,#176710,#176711,#176712,#176713,
#176714,#176715,#176716,#176717,#176718,#176719,#176720,#176721),
 .UNSPECIFIED.,.F.,.F.,(4,3,3,3,3,3,3,3,3,3,3,3,3,4),(0.,6.80370855369261E-5,
0.000137303169298902,0.000203636706663393,0.000256396220959703,0.000256540237295733,
0.000285209320207716,0.000342105100635638,0.00038477693595658,0.000400778874201934,
0.00045678565806067,0.000484789049990038,0.000498790745954722,0.000512792441919406),
 .UNSPECIFIED.);
#4455=B_SPLINE_CURVE_WITH_KNOTS('',3,(#176725,#176726,#176727,#176728,#176729,
#176730,#176731,#176732,#176733,#176734,#176735,#176736,#176737,#176738,
#176739,#176740,#176741,#176742,#176743,#176744,#176745,#176746,#176747,
#176748,#176749,#176750,#176751,#176752,#176753,#176754,#176755,#176756,
#176757,#176758,#176759,#176760,#176761),.UNSPECIFIED.,.F.,.F.,(4,3,3,3,
3,3,3,3,3,3,3,3,4),(0.,1.12535551670904E-5,7.76936938439903E-5,0.00010251351796104,
0.000121879189824199,0.000189659041345254,0.000223548967105781,0.000257294099096101,
0.000257438892866308,0.000325720851761651,0.000396486773967453,0.000466242707679148,
0.000514877785732617),.UNSPECIFIED.);
#4456=B_SPLINE_CURVE_WITH_KNOTS('',3,(#176769,#176770,#176771,#176772,#176773,
#176774,#176775,#176776,#176777,#176778,#176779,#176780,#176781,#176782,
#176783,#176784,#176785,#176786,#176787,#176788,#176789,#176790,#176791,
#176792,#176793,#176794,#176795,#176796,#176797,#176798,#176799,#176800,
#176801,#176802,#176803,#176804,#176805,#176806,#176807,#176808),
 .UNSPECIFIED.,.F.,.F.,(4,3,3,3,3,3,3,3,3,3,3,3,3,4),(0.,6.80370855361831E-5,
0.000137303169297157,0.000203636706660255,0.000256396220959701,0.000256540237295729,
0.000285209320207742,0.000342105100635657,0.000384776935956594,0.000400778874201945,
0.000456785658060674,0.000484789049990038,0.00049879074595472,0.000512792441919403),
 .UNSPECIFIED.);
#4457=B_SPLINE_CURVE_WITH_KNOTS('',3,(#176812,#176813,#176814,#176815,#176816,
#176817,#176818,#176819,#176820,#176821,#176822,#176823,#176824,#176825,
#176826,#176827,#176828,#176829,#176830,#176831,#176832,#176833,#176834,
#176835,#176836,#176837,#176838,#176839,#176840,#176841,#176842,#176843,
#176844,#176845,#176846,#176847,#176848),.UNSPECIFIED.,.F.,.F.,(4,3,3,3,
3,3,3,3,3,3,3,3,4),(0.,1.12535551671015E-5,7.76936938530422E-5,0.00010251351796114,
0.000121879189824285,0.00018965904134529,0.000223548967105792,0.000257294099096101,
0.000257438892866295,0.000325720851754998,0.000396486773954111,0.000466242707659906,
0.00051487778573259),.UNSPECIFIED.);
#4458=B_SPLINE_CURVE_WITH_KNOTS('',3,(#176856,#176857,#176858,#176859,#176860,
#176861,#176862,#176863,#176864,#176865,#176866,#176867,#176868,#176869,
#176870,#176871,#176872,#176873,#176874,#176875,#176876,#176877,#176878,
#176879,#176880,#176881,#176882,#176883,#176884,#176885,#176886,#176887,
#176888,#176889,#176890,#176891,#176892,#176893,#176894,#176895),
 .UNSPECIFIED.,.F.,.F.,(4,3,3,3,3,3,3,3,3,3,3,3,3,4),(0.,6.80370855425714E-5,
0.000137303169310326,0.000203636706679929,0.000256396220959705,0.000256540237295739,
0.000285209320207736,0.000342105100635654,0.000384776935956593,0.000400778874201945,
0.000456785658060677,0.000484789049990043,0.000498790745954727,0.00051279244191941),
 .UNSPECIFIED.);
#4459=B_SPLINE_CURVE_WITH_KNOTS('',3,(#176899,#176900,#176901,#176902,#176903,
#176904,#176905,#176906,#176907,#176908,#176909,#176910,#176911,#176912,
#176913,#176914,#176915,#176916,#176917,#176918,#176919,#176920,#176921,
#176922,#176923,#176924,#176925,#176926,#176927,#176928,#176929,#176930,
#176931,#176932,#176933,#176934,#176935),.UNSPECIFIED.,.F.,.F.,(4,3,3,3,
3,3,3,3,3,3,3,3,4),(0.,1.12535551670989E-5,7.76936938471546E-5,0.00010251351796113,
0.000121879189824276,0.00018965904134529,0.000223548967105796,0.00025729409909611,
0.000257438892866303,0.000325720851757156,0.000396486773958549,0.000466242707666787,
0.000514877785732606),.UNSPECIFIED.);
#4460=B_SPLINE_CURVE_WITH_KNOTS('',3,(#176943,#176944,#176945,#176946,#176947,
#176948,#176949,#176950,#176951,#176952,#176953,#176954,#176955,#176956,
#176957,#176958,#176959,#176960,#176961,#176962,#176963,#176964,#176965,
#176966,#176967,#176968,#176969,#176970,#176971,#176972,#176973,#176974,
#176975,#176976,#176977,#176978,#176979,#176980,#176981,#176982),
 .UNSPECIFIED.,.F.,.F.,(4,3,3,3,3,3,3,3,3,3,3,3,3,4),(0.,6.80370855337926E-5,
0.000137303169293006,0.00020363670665551,0.000256396220959705,0.000256540237295733,
0.000285209320207729,0.000342105100635649,0.000384776935956589,0.000400778874201942,
0.000456785658060675,0.000484789049990042,0.000498790745954726,0.000512792441919409),
 .UNSPECIFIED.);
#4461=B_SPLINE_CURVE_WITH_KNOTS('',3,(#176986,#176987,#176988,#176989,#176990,
#176991,#176992,#176993,#176994,#176995,#176996,#176997,#176998,#176999,
#177000,#177001,#177002,#177003,#177004,#177005,#177006,#177007,#177008,
#177009,#177010,#177011,#177012,#177013,#177014,#177015,#177016,#177017,
#177018,#177019,#177020,#177021,#177022),.UNSPECIFIED.,.F.,.F.,(4,3,3,3,
3,3,3,3,3,3,3,3,4),(0.,1.12535551671055E-5,7.76936938444389E-5,0.000102513517961177,
0.000121879189824318,0.000189659041345312,0.000223548967105809,0.000257294099096115,
0.000257438892866307,0.000325720851758166,0.000396486773960672,0.00046624270767006,
0.000514877785732613),.UNSPECIFIED.);
#4462=B_SPLINE_CURVE_WITH_KNOTS('',3,(#177030,#177031,#177032,#177033,#177034,
#177035,#177036,#177037,#177038,#177039,#177040,#177041,#177042,#177043,
#177044,#177045,#177046,#177047,#177048,#177049,#177050,#177051,#177052,
#177053,#177054,#177055,#177056,#177057,#177058,#177059,#177060,#177061,
#177062,#177063,#177064,#177065,#177066,#177067,#177068,#177069),
 .UNSPECIFIED.,.F.,.F.,(4,3,3,3,3,3,3,3,3,3,3,3,3,4),(0.,6.80370855295494E-5,
0.000137303169284071,0.000203636706641568,0.000256396220959705,0.000256540237295731,
0.000285209320207737,0.000342105100635655,0.000384776935956594,0.000400778874201946,
0.000456785658060678,0.000484789049990043,0.000498790745954726,0.000512792441919409),
 .UNSPECIFIED.);
#4463=B_SPLINE_CURVE_WITH_KNOTS('',3,(#177073,#177074,#177075,#177076,#177077,
#177078,#177079,#177080,#177081,#177082,#177083,#177084,#177085,#177086,
#177087,#177088,#177089,#177090,#177091,#177092,#177093,#177094,#177095,
#177096,#177097,#177098,#177099,#177100,#177101,#177102,#177103,#177104,
#177105,#177106,#177107,#177108,#177109),.UNSPECIFIED.,.F.,.F.,(4,3,3,3,
3,3,3,3,3,3,3,3,4),(0.,1.12535551670975E-5,7.76936938472089E-5,0.000102513517961106,
0.000121879189824256,0.00018965904134528,0.000223548967105792,0.000257294099096117,
0.000257438892866304,0.000325720851759813,0.000396486773964141,0.000466242707675212,
0.000514877785732608),.UNSPECIFIED.);
#4464=B_SPLINE_CURVE_WITH_KNOTS('',3,(#177116,#177117,#177118,#177119,#177120,
#177121,#177122,#177123,#177124,#177125,#177126,#177127,#177128,#177129,
#177130,#177131,#177132,#177133,#177134,#177135,#177136,#177137,#177138,
#177139,#177140,#177141,#177142,#177143,#177144,#177145,#177146,#177147,
#177148,#177149,#177150,#177151,#177152,#177153,#177154,#177155),
 .UNSPECIFIED.,.F.,.F.,(4,3,3,3,3,3,3,3,3,3,3,3,3,4),(0.,6.80370855426575E-5,
0.000137303169310749,0.000203636706681619,0.000256396220959708,0.00025654023729573,
0.000285209320207732,0.000342105100635653,0.000384776935956594,0.000400778874201947,
0.000456785658060682,0.000484789049990049,0.000498790745954733,0.000512792441919416),
 .UNSPECIFIED.);
#4465=B_SPLINE_CURVE_WITH_KNOTS('',3,(#177157,#177158,#177159,#177160,#177161,
#177162,#177163,#177164,#177165,#177166,#177167,#177168,#177169,#177170,
#177171,#177172,#177173,#177174,#177175,#177176,#177177,#177178,#177179,
#177180,#177181,#177182,#177183,#177184,#177185,#177186,#177187,#177188,
#177189,#177190,#177191,#177192,#177193),.UNSPECIFIED.,.F.,.F.,(4,3,3,3,
3,3,3,3,3,3,3,3,4),(0.,1.12535551670974E-5,7.76936938451676E-5,0.000102513517961093,
0.000121879189824244,0.000189659041345273,0.000223548967105788,0.000257294099096101,
0.000257438892866302,0.000325720851758372,0.000396486773961206,0.000466242707671043,
0.000514877785732605),.UNSPECIFIED.);
#4466=B_SPLINE_CURVE_WITH_KNOTS('',3,(#177201,#177202,#177203,#177204,#177205,
#177206,#177207,#177208,#177209,#177210,#177211,#177212,#177213,#177214,
#177215,#177216,#177217,#177218,#177219,#177220,#177221,#177222,#177223,
#177224,#177225,#177226,#177227,#177228,#177229,#177230,#177231,#177232,
#177233,#177234,#177235,#177236,#177237,#177238,#177239,#177240),
 .UNSPECIFIED.,.F.,.F.,(4,3,3,3,3,3,3,3,3,3,3,3,3,4),(0.,6.80370855381835E-5,
0.000137303169301825,0.000203636706668595,0.000256396220959707,0.00025654023729572,
0.000285209320207731,0.000342105100635652,0.000384776935956593,0.000400778874201946,
0.00045678565806068,0.000484789049990048,0.000498790745954731,0.000512792441919415),
 .UNSPECIFIED.);
#4467=B_SPLINE_CURVE_WITH_KNOTS('',3,(#177244,#177245,#177246,#177247,#177248,
#177249,#177250,#177251,#177252,#177253,#177254,#177255,#177256,#177257,
#177258,#177259,#177260,#177261,#177262,#177263,#177264,#177265,#177266,
#177267,#177268,#177269,#177270,#177271,#177272,#177273,#177274,#177275,
#177276,#177277,#177278,#177279,#177280),.UNSPECIFIED.,.F.,.F.,(4,3,3,3,
3,3,3,3,3,3,3,3,4),(0.,1.12535551670995E-5,7.76936938489843E-5,0.000102513517961118,
0.000121879189824266,0.000189659041345285,0.000223548967105795,0.000257294099096108,
0.000257438892866304,0.00032572085175959,0.00039648677396363,0.000466242707674216,
0.000514877785732608),.UNSPECIFIED.);
#4468=B_SPLINE_CURVE_WITH_KNOTS('',3,(#177288,#177289,#177290,#177291,#177292,
#177293,#177294,#177295,#177296,#177297,#177298,#177299,#177300,#177301,
#177302,#177303,#177304,#177305,#177306,#177307,#177308,#177309,#177310,
#177311,#177312,#177313,#177314,#177315,#177316,#177317,#177318,#177319,
#177320,#177321,#177322,#177323,#177324,#177325,#177326,#177327),
 .UNSPECIFIED.,.F.,.F.,(4,3,3,3,3,3,3,3,3,3,3,3,3,4),(0.,6.80370855408551E-5,
0.000137303169307171,0.000203636706676362,0.000256396220959704,0.00025654023729573,
0.000285209320207735,0.000342105100635653,0.000384776935956592,0.000400778874201944,
0.000456785658060676,0.000484789049990042,0.000498790745954725,0.000512792441919408),
 .UNSPECIFIED.);
#4469=B_SPLINE_CURVE_WITH_KNOTS('',3,(#177331,#177332,#177333,#177334,#177335,
#177336,#177337,#177338,#177339,#177340,#177341,#177342,#177343,#177344,
#177345,#177346,#177347,#177348,#177349,#177350,#177351,#177352,#177353,
#177354,#177355,#177356,#177357,#177358,#177359,#177360,#177361,#177362,
#177363,#177364,#177365,#177366,#177367),.UNSPECIFIED.,.F.,.F.,(4,3,3,3,
3,3,3,3,3,3,3,3,4),(0.,1.12535551671002E-5,7.7693693839773E-5,0.000102513517961098,
0.000121879189824249,0.000189659041345276,0.00022354896710579,0.000257294099096113,
0.000257438892866304,0.00032572085175236,0.000396486773948729,0.000466242707652564,
0.000514877785732609),.UNSPECIFIED.);
#4470=B_SPLINE_CURVE_WITH_KNOTS('',3,(#177375,#177376,#177377,#177378,#177379,
#177380,#177381,#177382,#177383,#177384,#177385,#177386,#177387,#177388,
#177389,#177390,#177391,#177392,#177393,#177394,#177395,#177396,#177397,
#177398,#177399,#177400,#177401,#177402,#177403,#177404,#177405,#177406,
#177407,#177408,#177409,#177410,#177411,#177412,#177413,#177414),
 .UNSPECIFIED.,.F.,.F.,(4,3,3,3,3,3,3,3,3,3,3,3,3,4),(0.,6.80370855356796E-5,
0.000137303169296129,0.000203636706658719,0.000256396220959703,0.000256540237295748,
0.00028520932020774,0.000342105100635656,0.000384776935956594,0.000400778874201945,
0.000456785658060676,0.000484789049990041,0.000498790745954723,0.000512792441919406),
 .UNSPECIFIED.);
#4471=B_SPLINE_CURVE_WITH_KNOTS('',3,(#177418,#177419,#177420,#177421,#177422,
#177423,#177424,#177425,#177426,#177427,#177428,#177429,#177430,#177431,
#177432,#177433,#177434,#177435,#177436,#177437,#177438,#177439,#177440,
#177441,#177442,#177443,#177444,#177445,#177446,#177447,#177448,#177449,
#177450,#177451,#177452,#177453,#177454),.UNSPECIFIED.,.F.,.F.,(4,3,3,3,
3,3,3,3,3,3,3,3,4),(0.,1.12535551670962E-5,7.76936938524064E-5,0.000102513517961067,
0.000121879189824222,0.000189659041345266,0.000223548967105787,0.000257294099096103,
0.000257438892866309,0.000325720851742739,0.000396486773928982,0.000466242707623088,
0.000514877785732618),.UNSPECIFIED.);
#4472=B_SPLINE_CURVE_WITH_KNOTS('',3,(#177462,#177463,#177464,#177465,#177466,
#177467,#177468,#177469,#177470,#177471,#177472,#177473,#177474,#177475,
#177476,#177477,#177478,#177479,#177480,#177481,#177482,#177483,#177484,
#177485,#177486,#177487,#177488,#177489,#177490,#177491,#177492,#177493,
#177494,#177495,#177496,#177497,#177498,#177499,#177500,#177501),
 .UNSPECIFIED.,.F.,.F.,(4,3,3,3,3,3,3,3,3,3,3,3,3,4),(0.,6.8037085537137E-5,
0.000137303169299574,0.000203636706665128,0.000256396220959701,0.000256540237295749,
0.000285209320207748,0.000342105100635662,0.000384776935956597,0.000400778874201948,
0.000456785658060675,0.000484789049990039,0.000498790745954721,0.000512792441919403),
 .UNSPECIFIED.);
#4473=B_SPLINE_CURVE_WITH_KNOTS('',3,(#177505,#177506,#177507,#177508,#177509,
#177510,#177511,#177512,#177513,#177514,#177515,#177516,#177517,#177518,
#177519,#177520,#177521,#177522,#177523,#177524,#177525,#177526,#177527,
#177528,#177529,#177530,#177531,#177532,#177533,#177534,#177535,#177536,
#177537,#177538,#177539,#177540,#177541),.UNSPECIFIED.,.F.,.F.,(4,3,3,3,
3,3,3,3,3,3,3,3,4),(0.,1.12535551670965E-5,7.76936938401387E-5,0.000102513517961103,
0.000121879189824253,0.00018965904134528,0.000223548967105793,0.000257294099096109,
0.000257438892866306,0.000325720851768072,0.000396486773980999,0.00046624270769989,
0.000514877785732612),.UNSPECIFIED.);
#4474=B_SPLINE_CURVE_WITH_KNOTS('',3,(#177549,#177550,#177551,#177552,#177553,
#177554,#177555,#177556,#177557,#177558,#177559,#177560,#177561,#177562,
#177563,#177564,#177565,#177566,#177567,#177568,#177569,#177570,#177571,
#177572,#177573,#177574,#177575,#177576,#177577,#177578,#177579,#177580,
#177581,#177582,#177583,#177584,#177585,#177586,#177587,#177588),
 .UNSPECIFIED.,.F.,.F.,(4,3,3,3,3,3,3,3,3,3,3,3,3,4),(0.,6.80370855398071E-5,
0.000137303169305327,0.000203636706674421,0.000256396220959704,0.000256540237295728,
0.000285209320207732,0.000342105100635651,0.00038477693595659,0.000400778874201942,
0.000456785658060675,0.000484789049990041,0.000498790745954725,0.000512792441919408),
 .UNSPECIFIED.);
#4475=B_SPLINE_CURVE_WITH_KNOTS('',3,(#177592,#177593,#177594,#177595,#177596,
#177597,#177598,#177599,#177600,#177601,#177602,#177603,#177604,#177605,
#177606,#177607,#177608,#177609,#177610,#177611,#177612,#177613,#177614,
#177615,#177616,#177617,#177618,#177619,#177620,#177621,#177622,#177623,
#177624,#177625,#177626,#177627,#177628),.UNSPECIFIED.,.F.,.F.,(4,3,3,3,
3,3,3,3,3,3,3,3,4),(0.,1.12535551670948E-5,7.76936938452495E-5,0.000102513517961045,
0.000121879189824203,0.000189659041345256,0.000223548967105782,0.000257294099096104,
0.000257438892866309,0.0003257208517583,0.000396486773960412,0.000466242707668339,
0.000514877785732617),.UNSPECIFIED.);
#4476=B_SPLINE_CURVE_WITH_KNOTS('',3,(#177636,#177637,#177638,#177639,#177640,
#177641,#177642,#177643,#177644,#177645,#177646,#177647,#177648,#177649,
#177650,#177651,#177652,#177653,#177654,#177655,#177656,#177657,#177658,
#177659,#177660,#177661,#177662,#177663,#177664,#177665,#177666,#177667,
#177668,#177669,#177670,#177671,#177672,#177673,#177674,#177675),
 .UNSPECIFIED.,.F.,.F.,(4,3,3,3,3,3,3,3,3,3,3,3,3,4),(0.,6.80370855368213E-5,
0.00013730316929917,0.000203636706664817,0.000256396220959701,0.000256540237295725,
0.000285209320207718,0.000342105100635639,0.00038477693595658,0.000400778874201932,
0.000456785658060667,0.000484789049990034,0.000498790745954718,0.000512792441919401),
 .UNSPECIFIED.);
#4477=B_SPLINE_CURVE_WITH_KNOTS('',3,(#177679,#177680,#177681,#177682,#177683,
#177684,#177685,#177686,#177687,#177688,#177689,#177690,#177691,#177692,
#177693,#177694,#177695,#177696,#177697,#177698,#177699,#177700,#177701,
#177702,#177703,#177704,#177705,#177706,#177707,#177708,#177709,#177710,
#177711,#177712,#177713,#177714,#177715),.UNSPECIFIED.,.F.,.F.,(4,3,3,3,
3,3,3,3,3,3,3,3,4),(0.,1.12535551670986E-5,7.76936938620434E-5,0.000102513517961113,
0.000121879189824263,0.000189659041345287,0.000223548967105799,0.000257294099096108,
0.000257438892866311,0.000325720851745853,0.000396486773936162,0.000466242707634991,
0.000514877785732623),.UNSPECIFIED.);
#4478=B_SPLINE_CURVE_WITH_KNOTS('',3,(#177723,#177724,#177725,#177726,#177727,
#177728,#177729,#177730,#177731,#177732,#177733,#177734,#177735,#177736,
#177737,#177738,#177739,#177740,#177741,#177742,#177743,#177744,#177745,
#177746,#177747,#177748,#177749,#177750,#177751,#177752,#177753,#177754,
#177755,#177756,#177757,#177758,#177759,#177760,#177761,#177762),
 .UNSPECIFIED.,.F.,.F.,(4,3,3,3,3,3,3,3,3,3,3,3,3,4),(0.,6.80370855419168E-5,
0.000137303169309447,0.000203636706680337,0.000256396220959704,0.000256540237295742,
0.000285209320207732,0.000342105100635651,0.00038477693595659,0.000400778874201942,
0.000456785658060675,0.000484789049990041,0.000498790745954724,0.000512792441919408),
 .UNSPECIFIED.);
#4479=B_SPLINE_CURVE_WITH_KNOTS('',3,(#177766,#177767,#177768,#177769,#177770,
#177771,#177772,#177773,#177774,#177775,#177776,#177777,#177778,#177779,
#177780,#177781,#177782,#177783,#177784,#177785,#177786,#177787,#177788,
#177789,#177790,#177791,#177792,#177793,#177794,#177795,#177796,#177797,
#177798,#177799,#177800,#177801,#177802),.UNSPECIFIED.,.F.,.F.,(4,3,3,3,
3,3,3,3,3,3,3,3,4),(0.,1.12535551670945E-5,7.76936938530435E-5,0.000102513517961046,
0.000121879189824204,0.000189659041345257,0.000223548967105783,0.0002572940990961,
0.000257438892866309,0.000325720851758386,0.000396486773961598,0.000466242707672009,
0.000514877785732619),.UNSPECIFIED.);
#4480=B_SPLINE_CURVE_WITH_KNOTS('',3,(#177810,#177811,#177812,#177813,#177814,
#177815,#177816,#177817,#177818,#177819,#177820,#177821,#177822,#177823,
#177824,#177825,#177826,#177827,#177828,#177829,#177830,#177831,#177832,
#177833,#177834,#177835,#177836,#177837,#177838,#177839,#177840,#177841,
#177842,#177843,#177844,#177845,#177846,#177847,#177848,#177849),
 .UNSPECIFIED.,.F.,.F.,(4,3,3,3,3,3,3,3,3,3,3,3,3,4),(0.,6.80370855335525E-5,
0.000137303169292306,0.000203636706653932,0.00025639622095971,0.000256540237295747,
0.000285209320207735,0.000342105100635656,0.000384776935956597,0.00040077887420195,
0.000456785658060685,0.000484789049990053,0.000498790745954737,0.00051279244191942),
 .UNSPECIFIED.);
#4481=B_SPLINE_CURVE_WITH_KNOTS('',3,(#177853,#177854,#177855,#177856,#177857,
#177858,#177859,#177860,#177861,#177862,#177863,#177864,#177865,#177866,
#177867,#177868,#177869,#177870,#177871,#177872,#177873,#177874,#177875,
#177876,#177877,#177878,#177879,#177880,#177881,#177882,#177883,#177884,
#177885,#177886,#177887,#177888,#177889),.UNSPECIFIED.,.F.,.F.,(4,3,3,3,
3,3,3,3,3,3,3,3,4),(0.,1.12535551670982E-5,7.76936938420302E-5,0.000102513517961121,
0.000121879189824269,0.000189659041345284,0.000223548967105792,0.00025729409909609,
0.000257438892866299,0.000325720851756146,0.000396486773955559,0.000466242707660611,
0.000514877785732599),.UNSPECIFIED.);
#4482=B_SPLINE_CURVE_WITH_KNOTS('',3,(#177897,#177898,#177899,#177900,#177901,
#177902,#177903,#177904,#177905,#177906,#177907,#177908,#177909,#177910,
#177911,#177912,#177913,#177914,#177915,#177916,#177917,#177918,#177919,
#177920,#177921,#177922,#177923,#177924,#177925,#177926,#177927,#177928,
#177929,#177930,#177931,#177932,#177933,#177934,#177935,#177936),
 .UNSPECIFIED.,.F.,.F.,(4,3,3,3,3,3,3,3,3,3,3,3,3,4),(0.,6.80370855388716E-5,
0.000137303169302875,0.00020363670666931,0.000256396220959701,0.000256540237295736,
0.000285209320207724,0.000342105100635644,0.000384776935956583,0.000400778874201936,
0.000456785658060669,0.000484789049990036,0.000498790745954719,0.000512792441919403),
 .UNSPECIFIED.);
#4483=B_SPLINE_CURVE_WITH_KNOTS('',3,(#177940,#177941,#177942,#177943,#177944,
#177945,#177946,#177947,#177948,#177949,#177950,#177951,#177952,#177953,
#177954,#177955,#177956,#177957,#177958,#177959,#177960,#177961,#177962,
#177963,#177964,#177965,#177966,#177967,#177968,#177969,#177970,#177971,
#177972,#177973,#177974,#177975,#177976),.UNSPECIFIED.,.F.,.F.,(4,3,3,3,
3,3,3,3,3,3,3,3,4),(0.,1.12535551670968E-5,7.76936938432487E-5,0.000102513517961121,
0.000121879189824269,0.000189659041345286,0.000223548967105795,0.000257294099096113,
0.000257438892866304,0.000325720851757511,0.000396486773960315,0.000466242707671397,
0.000514877785732607),.UNSPECIFIED.);
#4484=B_SPLINE_CURVE_WITH_KNOTS('',3,(#177984,#177985,#177986,#177987,#177988,
#177989,#177990,#177991,#177992,#177993,#177994,#177995,#177996,#177997,
#177998,#177999,#178000,#178001,#178002,#178003,#178004,#178005,#178006,
#178007,#178008,#178009,#178010,#178011,#178012,#178013,#178014,#178015,
#178016,#178017,#178018,#178019,#178020,#178021,#178022,#178023),
 .UNSPECIFIED.,.F.,.F.,(4,3,3,3,3,3,3,3,3,3,3,3,3,4),(0.,6.80370855309538E-5,
0.00013730316928727,0.000203636706647231,0.000256396220959712,0.000256540237295743,
0.000285209320207748,0.000342105100635667,0.000384776935956606,0.000400778874201958,
0.000456785658060691,0.000484789049990057,0.000498790745954741,0.000512792441919424),
 .UNSPECIFIED.);
#4485=B_SPLINE_CURVE_WITH_KNOTS('',3,(#178027,#178028,#178029,#178030,#178031,
#178032,#178033,#178034,#178035,#178036,#178037,#178038,#178039,#178040,
#178041,#178042,#178043,#178044,#178045,#178046,#178047,#178048,#178049,
#178050,#178051,#178052,#178053,#178054,#178055,#178056,#178057,#178058,
#178059,#178060,#178061,#178062,#178063),.UNSPECIFIED.,.F.,.F.,(4,3,3,3,
3,3,3,3,3,3,3,3,4),(0.,1.12535551670983E-5,7.76936938367873E-5,0.000102513517961129,
0.000121879189824276,0.000189659041345291,0.000223548967105798,0.000257294099096089,
0.000257438892866305,0.000325720851750639,0.000396486773945176,0.000466242707647004,
0.00051487778573261),.UNSPECIFIED.);
#4486=B_SPLINE_CURVE_WITH_KNOTS('',3,(#178071,#178072,#178073,#178074,#178075,
#178076,#178077,#178078,#178079,#178080,#178081,#178082,#178083,#178084,
#178085,#178086,#178087,#178088,#178089,#178090,#178091,#178092,#178093,
#178094,#178095,#178096,#178097,#178098,#178099,#178100,#178101,#178102,
#178103,#178104,#178105,#178106,#178107,#178108,#178109,#178110),
 .UNSPECIFIED.,.F.,.F.,(4,3,3,3,3,3,3,3,3,3,3,3,3,4),(0.,6.80370855382641E-5,
0.000137303169301827,0.000203636706668335,0.000256396220959708,0.000256540237295738,
0.000285209320207749,0.000342105100635665,0.000384776935956603,0.000400778874201954,
0.000456785658060685,0.00048478904999005,0.000498790745954732,0.000512792441919415),
 .UNSPECIFIED.);
#4487=B_SPLINE_CURVE_WITH_KNOTS('',3,(#178114,#178115,#178116,#178117,#178118,
#178119,#178120,#178121,#178122,#178123,#178124,#178125,#178126,#178127,
#178128,#178129,#178130,#178131,#178132,#178133,#178134,#178135,#178136,
#178137,#178138,#178139,#178140,#178141,#178142,#178143,#178144,#178145,
#178146,#178147,#178148,#178149,#178150),.UNSPECIFIED.,.F.,.F.,(4,3,3,3,
3,3,3,3,3,3,3,3,4),(0.,1.12535551670954E-5,7.769369383202E-5,0.000102513517961085,
0.000121879189824237,0.00018965904134527,0.000223548967105787,0.000257294099096099,
0.000257438892866304,0.000325720851760152,0.000396486773964489,0.000466242707675398,
0.000514877785732607),.UNSPECIFIED.);
#4488=B_SPLINE_CURVE_WITH_KNOTS('',3,(#178158,#178159,#178160,#178161,#178162,
#178163,#178164,#178165,#178166,#178167,#178168,#178169,#178170,#178171,
#178172,#178173,#178174,#178175,#178176,#178177,#178178,#178179,#178180,
#178181,#178182,#178183,#178184,#178185,#178186,#178187,#178188,#178189,
#178190,#178191,#178192,#178193,#178194,#178195,#178196,#178197),
 .UNSPECIFIED.,.F.,.F.,(4,3,3,3,3,3,3,3,3,3,3,3,3,4),(0.,6.80370855357845E-5,
0.000137303169296545,0.000203636706659477,0.000256396220959712,0.000256540237295743,
0.000285209320207756,0.000342105100635673,0.000384776935956611,0.000400778874201962,
0.000456785658060693,0.000484789049990058,0.000498790745954741,0.000512792441919424),
 .UNSPECIFIED.);
#4489=B_SPLINE_CURVE_WITH_KNOTS('',3,(#178201,#178202,#178203,#178204,#178205,
#178206,#178207,#178208,#178209,#178210,#178211,#178212,#178213,#178214,
#178215,#178216,#178217,#178218,#178219,#178220,#178221,#178222,#178223,
#178224,#178225,#178226,#178227,#178228,#178229,#178230,#178231,#178232,
#178233,#178234,#178235,#178236,#178237),.UNSPECIFIED.,.F.,.F.,(4,3,3,3,
3,3,3,3,3,3,3,3,4),(0.,1.12535551670973E-5,7.76936938384776E-5,0.000102513517961114,
0.000121879189824263,0.000189659041345285,0.000223548967105795,0.000257294099096104,
0.000257438892866306,0.000325720851762052,0.000396486773967539,0.000466242707677798,
0.000514877785732612),.UNSPECIFIED.);
#4490=B_SPLINE_CURVE_WITH_KNOTS('',3,(#178245,#178246,#178247,#178248,#178249,
#178250,#178251,#178252,#178253,#178254,#178255,#178256,#178257,#178258,
#178259,#178260,#178261,#178262,#178263,#178264,#178265,#178266,#178267,
#178268,#178269,#178270,#178271,#178272,#178273,#178274,#178275,#178276,
#178277,#178278,#178279,#178280,#178281,#178282,#178283,#178284),
 .UNSPECIFIED.,.F.,.F.,(4,3,3,3,3,3,3,3,3,3,3,3,3,4),(0.,6.80370855448908E-5,
0.00013730316931562,0.000203636706689471,0.000256396220959709,0.000256540237295741,
0.000285209320207744,0.000342105100635662,0.000384776935956601,0.000400778874201953,
0.000456785658060685,0.000484789049990051,0.000498790745954734,0.000512792441919417),
 .UNSPECIFIED.);
#4491=B_SPLINE_CURVE_WITH_KNOTS('',3,(#178288,#178289,#178290,#178291,#178292,
#178293,#178294,#178295,#178296,#178297,#178298,#178299,#178300,#178301,
#178302,#178303,#178304,#178305,#178306,#178307,#178308,#178309,#178310,
#178311,#178312,#178313,#178314,#178315,#178316,#178317,#178318,#178319,
#178320,#178321,#178322,#178323,#178324),.UNSPECIFIED.,.F.,.F.,(4,3,3,3,
3,3,3,3,3,3,3,3,4),(0.,1.12535551670965E-5,7.7693693850504E-5,0.000102513517961145,
0.00012187918982429,0.000189659041345294,0.000223548967105797,0.000257294099096094,
0.000257438892866299,0.000325720851758731,0.000396486773961765,0.000466242707671255,
0.000514877785732599),.UNSPECIFIED.);
#4492=B_SPLINE_CURVE_WITH_KNOTS('',3,(#178332,#178333,#178334,#178335,#178336,
#178337,#178338,#178339,#178340,#178341,#178342,#178343,#178344,#178345,
#178346,#178347,#178348,#178349,#178350,#178351,#178352,#178353,#178354,
#178355,#178356,#178357,#178358,#178359,#178360,#178361,#178362,#178363,
#178364,#178365,#178366,#178367,#178368,#178369,#178370,#178371),
 .UNSPECIFIED.,.F.,.F.,(4,3,3,3,3,3,3,3,3,3,3,3,3,4),(0.,6.80370855381794E-5,
0.000137303169301656,0.000203636706667918,0.000256396220959708,0.000256540237295746,
0.000285209320207746,0.000342105100635663,0.000384776935956602,0.000400778874201954,
0.000456785658060685,0.000484789049990051,0.000498790745954734,0.000512792441919417),
 .UNSPECIFIED.);
#4493=B_SPLINE_CURVE_WITH_KNOTS('',3,(#178375,#178376,#178377,#178378,#178379,
#178380,#178381,#178382,#178383,#178384,#178385,#178386,#178387,#178388,
#178389,#178390,#178391,#178392,#178393,#178394,#178395,#178396,#178397,
#178398,#178399,#178400,#178401,#178402,#178403,#178404,#178405,#178406,
#178407,#178408,#178409,#178410,#178411),.UNSPECIFIED.,.F.,.F.,(4,3,3,3,
3,3,3,3,3,3,3,3,4),(0.,1.12535551670961E-5,7.76936938492663E-5,0.000102513517961084,
0.000121879189824237,0.00018965904134527,0.000223548967105786,0.000257294099096085,
0.000257438892866303,0.000325720851754593,0.00039648677395353,0.000466242707659808,
0.000514877785732606),.UNSPECIFIED.);
#4494=B_SPLINE_CURVE_WITH_KNOTS('',3,(#178418,#178419,#178420,#178421,#178422,
#178423,#178424,#178425,#178426,#178427,#178428,#178429,#178430,#178431,
#178432,#178433,#178434,#178435,#178436,#178437,#178438,#178439,#178440,
#178441,#178442,#178443,#178444,#178445,#178446,#178447,#178448,#178449,
#178450,#178451,#178452,#178453,#178454,#178455,#178456,#178457),
 .UNSPECIFIED.,.F.,.F.,(4,3,3,3,3,3,3,3,3,3,3,3,3,4),(0.,6.80370855321557E-5,
0.000137303169289422,0.000203636706649785,0.000256396220959709,0.000256540237295743,
0.000285209320207743,0.000342105100635662,0.000384776935956601,0.000400778874201953,
0.000456785658060685,0.000484789049990051,0.000498790745954734,0.000512792441919417),
 .UNSPECIFIED.);
#4495=B_SPLINE_CURVE_WITH_KNOTS('',3,(#182071,#182072,#182073,#182074,#182075,
#182076,#182077,#182078,#182079,#182080,#182081,#182082,#182083,#182084,
#182085,#182086,#182087,#182088,#182089,#182090,#182091,#182092,#182093,
#182094,#182095,#182096,#182097,#182098,#182099,#182100,#182101,#182102,
#182103,#182104,#182105,#182106,#182107,#182108,#182109,#182110,#182111,
#182112,#182113,#182114,#182115,#182116,#182117,#182118,#182119,#182120,
#182121,#182122),.UNSPECIFIED.,.F.,.F.,(4,3,3,3,3,3,3,3,3,3,3,3,3,3,3,3,
3,4),(0.,4.3070623787495E-5,8.47417087705792E-5,0.000124159989206991,0.000160467076291534,
0.0001709983821167,0.000182414994733782,0.000213747977645871,0.000242415955902806,
0.000256497573175043,0.000259169422895616,0.000261757777312422,0.000289965130403398,
0.000301877270772904,0.000321937017503146,0.000326951954185706,0.000334474359209546,
0.000341996764233387),.UNSPECIFIED.);
#4496=B_SPLINE_CURVE_WITH_KNOTS('',3,(#182123,#182124,#182125,#182126,#182127,
#182128,#182129,#182130,#182131,#182132,#182133,#182134,#182135,#182136,
#182137,#182138,#182139,#182140,#182141,#182142,#182143,#182144,#182145,
#182146,#182147,#182148,#182149,#182150,#182151,#182152,#182153,#182154,
#182155,#182156,#182157,#182158,#182159,#182160,#182161,#182162,#182163,
#182164,#182165,#182166,#182167,#182168,#182169,#182170,#182171,#182172,
#182173,#182174),.UNSPECIFIED.,.F.,.F.,(4,3,3,3,3,3,3,3,3,3,3,3,3,3,3,3,
3,4),(0.,2.58457451675486E-5,4.25394446196056E-5,6.4665986968724E-5,7.57292581432831E-5,
8.12608937305627E-5,8.26438026273826E-5,8.67925293178423E-5,0.000116015624428002,
0.000130188793976763,0.000151886926306224,0.00016196365121129,0.000162735992470954,
0.000173585058635685,0.000212487880460513,0.000255238173511739,0.000301397761149341,
0.000347170117271356),.UNSPECIFIED.);
#4497=B_SPLINE_CURVE_WITH_KNOTS('',3,(#182176,#182177,#182178,#182179,#182180,
#182181,#182182,#182183,#182184,#182185,#182186,#182187,#182188,#182189,
#182190,#182191,#182192,#182193,#182194,#182195,#182196,#182197,#182198,
#182199,#182200,#182201,#182202,#182203,#182204,#182205,#182206,#182207,
#182208,#182209,#182210,#182211,#182212,#182213,#182214,#182215,#182216,
#182217,#182218,#182219,#182220,#182221),.UNSPECIFIED.,.F.,.F.,(4,3,3,3,
3,3,3,3,3,3,3,3,3,3,3,4),(3.3881317890172E-21,2.57218161986703E-5,4.21568322567895E-5,
6.4587331461705E-5,7.58025810641627E-5,8.14102058653916E-5,8.28121120656988E-5,
8.70178306666205E-5,0.000116081955657568,0.000130526745999931,0.00016239411102205,
0.000174035661333241,0.000213138396956876,0.000256116935431032,0.000302406662851701,
0.000348071322666469),.UNSPECIFIED.);
#4498=B_SPLINE_CURVE_WITH_KNOTS('',3,(#182222,#182223,#182224,#182225,#182226,
#182227,#182228,#182229,#182230,#182231,#182232,#182233,#182234,#182235,
#182236,#182237,#182238,#182239,#182240,#182241,#182242,#182243,#182244,
#182245,#182246,#182247,#182248,#182249,#182250,#182251,#182252,#182253,
#182254,#182255,#182256,#182257,#182258,#182259,#182260,#182261,#182262,
#182263,#182264,#182265,#182266,#182267,#182268,#182269,#182270,#182271,
#182272,#182273),.UNSPECIFIED.,.F.,.F.,(4,3,3,3,3,3,3,3,3,3,3,3,3,3,3,3,
3,4),(0.,4.29652152163274E-5,8.4451910753757E-5,0.000123669830865422,0.000159788877358504,
0.000170558847912626,0.000181218775907166,0.000181960046452408,0.000214460062643432,
0.000244755726198055,0.000255838271868945,0.00025850325386758,0.000261084955178757,
0.000289370476647835,0.000301101325502011,0.000321109510663637,0.000331113603244451,
0.000341117695825264),.UNSPECIFIED.);
#4499=B_SPLINE_CURVE_WITH_KNOTS('',3,(#185956,#185957,#185958,#185959,#185960,
#185961,#185962,#185963,#185964,#185965,#185966,#185967,#185968,#185969,
#185970,#185971,#185972,#185973,#185974,#185975,#185976,#185977,#185978,
#185979,#185980,#185981,#185982,#185983,#185984,#185985,#185986,#185987,
#185988,#185989,#185990,#185991,#185992,#185993,#185994,#185995,#185996,
#185997,#185998,#185999,#186000,#186001,#186002,#186003,#186004,#186005,
#186006,#186007),.UNSPECIFIED.,.F.,.F.,(4,3,3,3,3,3,3,3,3,3,3,3,3,3,3,3,
3,4),(0.,4.30706237904622E-5,8.47417087758447E-5,0.000124159989214271,0.000160467076301093,
0.00017099838211669,0.000182414994733772,0.000213747977645865,0.000242415955903934,
0.00025649757317504,0.000259169422895614,0.000261757777312419,0.000289965130401458,
0.000301877270772905,0.000321937017503148,0.000326951954185709,0.00033447435920955,
0.000341996764233391),.UNSPECIFIED.);
#4500=B_SPLINE_CURVE_WITH_KNOTS('',3,(#186008,#186009,#186010,#186011,#186012,
#186013,#186014,#186015,#186016,#186017,#186018,#186019,#186020,#186021,
#186022,#186023,#186024,#186025,#186026,#186027,#186028,#186029,#186030,
#186031,#186032,#186033,#186034,#186035,#186036,#186037,#186038,#186039,
#186040,#186041,#186042,#186043,#186044,#186045,#186046,#186047,#186048,
#186049,#186050,#186051,#186052,#186053,#186054,#186055,#186056,#186057,
#186058,#186059),.UNSPECIFIED.,.F.,.F.,(4,3,3,3,3,3,3,3,3,3,3,3,3,3,3,3,
3,4),(8.67361737988404E-19,2.58457451683905E-5,4.25394446195019E-5,6.4665986968671E-5,
7.57292581432556E-5,8.12608937305479E-5,8.26438026273709E-5,8.67925293178401E-5,
0.000116015624426893,0.00013018879397676,0.00015188692630622,0.000161963651211285,
0.00016273599247095,0.000173585058635679,0.000212487880462509,0.000255238173515559,
0.000301397761155017,0.000347170117271358),.UNSPECIFIED.);
#4501=B_SPLINE_CURVE_WITH_KNOTS('',3,(#186061,#186062,#186063,#186064,#186065,
#186066,#186067,#186068,#186069,#186070,#186071,#186072,#186073,#186074,
#186075,#186076,#186077,#186078,#186079,#186080,#186081,#186082,#186083,
#186084,#186085,#186086,#186087,#186088,#186089,#186090,#186091,#186092,
#186093,#186094,#186095,#186096,#186097,#186098,#186099,#186100,#186101,
#186102,#186103,#186104,#186105,#186106),.UNSPECIFIED.,.F.,.F.,(4,3,3,3,
3,3,3,3,3,3,3,3,3,3,3,4),(0.,2.57218162004654E-5,4.21568322569402E-5,6.4587331461781E-5,
7.58025810642015E-5,8.14102058654117E-5,8.28121120657143E-5,8.7017830666622E-5,
0.000116081955658923,0.000130526745999929,0.000162394111022053,0.000174035661333236,
0.000213138396959096,0.000256116935435479,0.000302406662858657,0.000348071322666466),
 .UNSPECIFIED.);
#4502=B_SPLINE_CURVE_WITH_KNOTS('',3,(#186107,#186108,#186109,#186110,#186111,
#186112,#186113,#186114,#186115,#186116,#186117,#186118,#186119,#186120,
#186121,#186122,#186123,#186124,#186125,#186126,#186127,#186128,#186129,
#186130,#186131,#186132,#186133,#186134,#186135,#186136,#186137,#186138,
#186139,#186140,#186141,#186142,#186143,#186144,#186145,#186146,#186147,
#186148,#186149,#186150,#186151,#186152,#186153,#186154,#186155,#186156,
#186157,#186158),.UNSPECIFIED.,.F.,.F.,(4,3,3,3,3,3,3,3,3,3,3,3,3,3,3,3,
3,4),(0.,4.29652152126473E-5,8.44519107477571E-5,0.000123669830857838,0.000159788877349733,
0.000170558847912618,0.000181218775907158,0.000181960046452388,0.000214460062643972,
0.000244755726199678,0.00025583827186894,0.000258503253867575,0.000261084955178752,
0.000289370476647328,0.000301101325502007,0.000321109510663634,0.000331113603244448,
0.000341117695825262),.UNSPECIFIED.);
#4503=B_SPLINE_CURVE_WITH_KNOTS('',3,(#186160,#186161,#186162,#186163,#186164,
#186165,#186166,#186167,#186168,#186169,#186170,#186171,#186172,#186173,
#186174,#186175,#186176,#186177,#186178,#186179,#186180,#186181,#186182,
#186183,#186184,#186185,#186186,#186187,#186188,#186189,#186190,#186191,
#186192,#186193,#186194,#186195,#186196,#186197,#186198,#186199,#186200,
#186201,#186202,#186203,#186204,#186205,#186206,#186207,#186208,#186209,
#186210,#186211),.UNSPECIFIED.,.F.,.F.,(4,3,3,3,3,3,3,3,3,3,3,3,3,3,3,3,
3,4),(0.,4.30706237869498E-5,8.47417087696762E-5,0.000124159989205771,0.000160467076290074,
0.000170998382116688,0.000182414994733765,0.000213747977645863,0.000242415955902775,
0.000256497573175039,0.000259169422895612,0.000261757777312418,0.000289965130403254,
0.000301877270772904,0.000321937017503147,0.000326951954185708,0.000334474359209549,
0.00034199676423339),.UNSPECIFIED.);
#4504=B_SPLINE_CURVE_WITH_KNOTS('',3,(#186212,#186213,#186214,#186215,#186216,
#186217,#186218,#186219,#186220,#186221,#186222,#186223,#186224,#186225,
#186226,#186227,#186228,#186229,#186230,#186231,#186232,#186233,#186234,
#186235,#186236,#186237,#186238,#186239,#186240,#186241,#186242,#186243,
#186244,#186245,#186246,#186247,#186248,#186249,#186250,#186251,#186252,
#186253,#186254,#186255,#186256,#186257,#186258,#186259,#186260,#186261,
#186262,#186263),.UNSPECIFIED.,.F.,.F.,(4,3,3,3,3,3,3,3,3,3,3,3,3,3,3,3,
3,4),(0.,2.58457451680011E-5,4.25394446195326E-5,6.46659869686882E-5,7.5729258143266E-5,
8.12608937305549E-5,8.26438026273771E-5,8.67925293178438E-5,0.000116015624426372,
0.000130188793976766,0.000151886926306227,0.000161963651211297,0.000162735992470957,
0.000173585058635688,0.000212487880459008,0.000255238173508161,0.00030139776114258,
0.000347170117271372),.UNSPECIFIED.);
#4505=B_SPLINE_CURVE_WITH_KNOTS('',3,(#186265,#186266,#186267,#186268,#186269,
#186270,#186271,#186272,#186273,#186274,#186275,#186276,#186277,#186278,
#186279,#186280,#186281,#186282,#186283,#186284,#186285,#186286,#186287,
#186288,#186289,#186290,#186291,#186292,#186293,#186294,#186295,#186296,
#186297,#186298,#186299,#186300,#186301,#186302,#186303,#186304,#186305,
#186306,#186307,#186308,#186309,#186310),.UNSPECIFIED.,.F.,.F.,(4,3,3,3,
3,3,3,3,3,3,3,3,3,3,3,4),(1.73472347597681E-18,2.57218161995936E-5,4.21568322567643E-5,
6.45873314616834E-5,7.5802581064143E-5,8.14102058653728E-5,8.28121120656802E-5,
8.70178306666025E-5,0.000116081955658033,0.000130526745999903,0.000162394111022011,
0.000174035661333203,0.000213138396957744,0.000256116935432899,0.000302406662854991,
0.000348071322666432),.UNSPECIFIED.);
#4506=B_SPLINE_CURVE_WITH_KNOTS('',3,(#186311,#186312,#186313,#186314,#186315,
#186316,#186317,#186318,#186319,#186320,#186321,#186322,#186323,#186324,
#186325,#186326,#186327,#186328,#186329,#186330,#186331,#186332,#186333,
#186334,#186335,#186336,#186337,#186338,#186339,#186340,#186341,#186342,
#186343,#186344,#186345,#186346,#186347,#186348,#186349,#186350,#186351,
#186352,#186353,#186354,#186355,#186356,#186357,#186358,#186359,#186360,
#186361,#186362),.UNSPECIFIED.,.F.,.F.,(4,3,3,3,3,3,3,3,3,3,3,3,3,3,3,3,
3,4),(0.,4.2965215218261E-5,8.44519107571648E-5,0.00012366983086999,0.000159788877364278,
0.000170558847912618,0.000181218775907157,0.000181960046452381,0.000214460062644312,
0.000244755726200678,0.000255838271868933,0.000258503253867568,0.000261084955178745,
0.000289370476645579,0.000301101325501997,0.000321109510663622,0.000331113603244435,
0.000341117695825248),.UNSPECIFIED.);
#4507=B_SPLINE_CURVE_WITH_KNOTS('',3,(#186364,#186365,#186366,#186367,#186368,
#186369,#186370,#186371,#186372,#186373,#186374,#186375,#186376,#186377,
#186378,#186379,#186380,#186381,#186382,#186383,#186384,#186385,#186386,
#186387,#186388,#186389,#186390,#186391,#186392,#186393,#186394,#186395,
#186396,#186397,#186398,#186399,#186400,#186401,#186402,#186403,#186404,
#186405,#186406,#186407,#186408,#186409,#186410,#186411,#186412,#186413,
#186414,#186415),.UNSPECIFIED.,.F.,.F.,(4,3,3,3,3,3,3,3,3,3,3,3,3,3,3,3,
3,4),(9.81307786677359E-18,4.30706237872886E-5,8.47417087703267E-5,0.000124159989206749,
0.000160467076291443,0.000170998382116702,0.000182414994733785,0.000213747977645874,
0.000242415955904002,0.000256497573175045,0.000259169422895618,0.000261757777312424,
0.000289965130402902,0.000301877270772906,0.000321937017503147,0.000326951954185707,
0.000334474359209548,0.000341996764233388),.UNSPECIFIED.);
#4508=B_SPLINE_CURVE_WITH_KNOTS('',3,(#186416,#186417,#186418,#186419,#186420,
#186421,#186422,#186423,#186424,#186425,#186426,#186427,#186428,#186429,
#186430,#186431,#186432,#186433,#186434,#186435,#186436,#186437,#186438,
#186439,#186440,#186441,#186442,#186443,#186444,#186445,#186446,#186447,
#186448,#186449,#186450,#186451,#186452,#186453,#186454,#186455,#186456,
#186457,#186458,#186459,#186460,#186461,#186462,#186463,#186464,#186465,
#186466,#186467),.UNSPECIFIED.,.F.,.F.,(4,3,3,3,3,3,3,3,3,3,3,3,3,3,3,3,
3,4),(0.,2.58457451681907E-5,4.25394446194808E-5,6.46659869686619E-5,7.57292581432524E-5,
8.12608937305477E-5,8.26438026273715E-5,8.67925293178429E-5,0.000116015624427697,
0.000130188793976764,0.000151886926306225,0.000161963651211284,0.000162735992470955,
0.000173585058635686,0.000212487880460992,0.000255238173511379,0.000301397761145688,
0.000347170117271377),.UNSPECIFIED.);
#4509=B_SPLINE_CURVE_WITH_KNOTS('',3,(#186469,#186470,#186471,#186472,#186473,
#186474,#186475,#186476,#186477,#186478,#186479,#186480,#186481,#186482,
#186483,#186484,#186485,#186486,#186487,#186488,#186489,#186490,#186491,
#186492,#186493,#186494,#186495,#186496,#186497,#186498,#186499,#186500,
#186501,#186502,#186503,#186504,#186505,#186506,#186507,#186508,#186509,
#186510,#186511,#186512,#186513,#186514),.UNSPECIFIED.,.F.,.F.,(4,3,3,3,
3,3,3,3,3,3,3,3,3,3,3,4),(0.,2.57218161996713E-5,4.2156832256742E-5,6.45873314616798E-5,
7.58025810641487E-5,8.14102058653831E-5,8.28121120656917E-5,8.70178306666176E-5,
0.000116081955658986,0.000130526745999926,0.000162394111022057,0.000174035661333235,
0.000213138396960236,0.000256116935437692,0.000302406662861853,0.000348071322666466),
 .UNSPECIFIED.);
#4510=B_SPLINE_CURVE_WITH_KNOTS('',3,(#186515,#186516,#186517,#186518,#186519,
#186520,#186521,#186522,#186523,#186524,#186525,#186526,#186527,#186528,
#186529,#186530,#186531,#186532,#186533,#186534,#186535,#186536,#186537,
#186538,#186539,#186540,#186541,#186542,#186543,#186544,#186545,#186546,
#186547,#186548,#186549,#186550,#186551,#186552,#186553,#186554,#186555,
#186556,#186557,#186558,#186559,#186560,#186561,#186562,#186563,#186564,
#186565,#186566),.UNSPECIFIED.,.F.,.F.,(4,3,3,3,3,3,3,3,3,3,3,3,3,3,3,3,
3,4),(0.,4.29652152153032E-5,8.44519107518936E-5,0.000123669830862718,0.000159788877354853,
0.000170558847912617,0.000181218775907157,0.000181960046452383,0.000214460062643983,
0.000244755726199726,0.00025583827186894,0.000258503253867575,0.000261084955178752,
0.000289370476647621,0.000301101325502007,0.000321109510663635,0.000331113603244448,
0.000341117695825262),.UNSPECIFIED.);
#4511=B_SPLINE_CURVE_WITH_KNOTS('',3,(#186568,#186569,#186570,#186571,#186572,
#186573,#186574,#186575,#186576,#186577,#186578,#186579,#186580,#186581,
#186582,#186583,#186584,#186585,#186586,#186587,#186588,#186589,#186590,
#186591,#186592,#186593,#186594,#186595,#186596,#186597,#186598,#186599,
#186600,#186601,#186602,#186603,#186604,#186605,#186606,#186607,#186608,
#186609,#186610,#186611,#186612,#186613,#186614,#186615,#186616,#186617,
#186618,#186619),.UNSPECIFIED.,.F.,.F.,(4,3,3,3,3,3,3,3,3,3,3,3,3,3,3,3,
3,4),(0.,4.30706237883116E-5,8.4741708772137E-5,0.000124159989209315,0.000160467076294801,
0.000170998382116688,0.000182414994733781,0.000213747977645863,0.000242415955903352,
0.000256497573175038,0.000259169422895611,0.000261757777312417,0.000289965130402052,
0.000301877270772902,0.000321937017503145,0.000326951954185706,0.000334474359209547,
0.000341996764233388),.UNSPECIFIED.);
#4512=B_SPLINE_CURVE_WITH_KNOTS('',3,(#186620,#186621,#186622,#186623,#186624,
#186625,#186626,#186627,#186628,#186629,#186630,#186631,#186632,#186633,
#186634,#186635,#186636,#186637,#186638,#186639,#186640,#186641,#186642,
#186643,#186644,#186645,#186646,#186647,#186648,#186649,#186650,#186651,
#186652,#186653,#186654,#186655,#186656,#186657,#186658,#186659,#186660,
#186661,#186662,#186663,#186664,#186665,#186666,#186667,#186668,#186669,
#186670,#186671),.UNSPECIFIED.,.F.,.F.,(4,3,3,3,3,3,3,3,3,3,3,3,3,3,3,3,
3,4),(0.,2.58457451672917E-5,4.25394446196108E-5,6.46659869687248E-5,7.57292581432817E-5,
8.12608937305602E-5,8.26438026273798E-5,8.67925293178387E-5,0.000116015624427758,
0.000130188793976758,0.000151886926306218,0.000161963651211268,0.000162735992470948,
0.000173585058635677,0.000212487880459398,0.00025523817350879,0.000301397761142968,
0.000347170117271355),.UNSPECIFIED.);
#4513=B_SPLINE_CURVE_WITH_KNOTS('',3,(#186673,#186674,#186675,#186676,#186677,
#186678,#186679,#186680,#186681,#186682,#186683,#186684,#186685,#186686,
#186687,#186688,#186689,#186690,#186691,#186692,#186693,#186694,#186695,
#186696,#186697,#186698,#186699,#186700,#186701,#186702,#186703,#186704,
#186705,#186706,#186707,#186708,#186709,#186710,#186711,#186712,#186713,
#186714,#186715,#186716,#186717,#186718),.UNSPECIFIED.,.F.,.F.,(4,3,3,3,
3,3,3,3,3,3,3,3,3,3,3,4),(3.46944695195361E-18,2.57218161983717E-5,4.21568322568919E-5,
6.45873314617591E-5,7.58025810641928E-5,8.14102058654096E-5,8.28121120657138E-5,
8.70178306666264E-5,0.000116081955657765,0.000130526745999938,0.000162394111022065,
0.000174035661333249,0.000213138396958737,0.000256116935434866,0.000302406662858167,
0.000348071322666474),.UNSPECIFIED.);
#4514=B_SPLINE_CURVE_WITH_KNOTS('',3,(#186719,#186720,#186721,#186722,#186723,
#186724,#186725,#186726,#186727,#186728,#186729,#186730,#186731,#186732,
#186733,#186734,#186735,#186736,#186737,#186738,#186739,#186740,#186741,
#186742,#186743,#186744,#186745,#186746,#186747,#186748,#186749,#186750,
#186751,#186752,#186753,#186754,#186755,#186756,#186757,#186758,#186759,
#186760,#186761,#186762,#186763,#186764,#186765,#186766,#186767,#186768,
#186769,#186770),.UNSPECIFIED.,.F.,.F.,(4,3,3,3,3,3,3,3,3,3,3,3,3,3,3,3,
3,4),(0.,4.29652152163865E-5,8.4451910753883E-5,0.000123669830865533,0.000159788877358621,
0.000170558847912619,0.000181218775907159,0.000181960046452386,0.000214460062643117,
0.000244755726196957,0.000255838271868941,0.000258503253867576,0.000261084955178754,
0.000289370476648858,0.000301101325502009,0.000321109510663636,0.00033111360324445,
0.000341117695825264),.UNSPECIFIED.);
#4515=B_SPLINE_CURVE_WITH_KNOTS('',3,(#186772,#186773,#186774,#186775,#186776,
#186777,#186778,#186779,#186780,#186781,#186782,#186783,#186784,#186785,
#186786,#186787,#186788,#186789,#186790,#186791,#186792,#186793,#186794,
#186795,#186796,#186797,#186798,#186799,#186800,#186801,#186802,#186803,
#186804,#186805,#186806,#186807,#186808,#186809,#186810,#186811,#186812,
#186813,#186814,#186815,#186816,#186817,#186818,#186819,#186820,#186821,
#186822,#186823),.UNSPECIFIED.,.F.,.F.,(4,3,3,3,3,3,3,3,3,3,3,3,3,3,3,3,
3,4),(0.,4.30706237866878E-5,8.47417087690751E-5,0.000124159989204751,0.000160467076288489,
0.000170998382116703,0.000182414994733785,0.000213747977645875,0.000242415955903625,
0.000256497573175048,0.000259169422895621,0.000261757777312427,0.000289965130402839,
0.00030187727077291,0.000321937017503152,0.000326951954185712,0.000334474359209553,
0.000341996764233393),.UNSPECIFIED.);
#4516=B_SPLINE_CURVE_WITH_KNOTS('',3,(#186824,#186825,#186826,#186827,#186828,
#186829,#186830,#186831,#186832,#186833,#186834,#186835,#186836,#186837,
#186838,#186839,#186840,#186841,#186842,#186843,#186844,#186845,#186846,
#186847,#186848,#186849,#186850,#186851,#186852,#186853,#186854,#186855,
#186856,#186857,#186858,#186859,#186860,#186861,#186862,#186863,#186864,
#186865,#186866,#186867,#186868,#186869,#186870,#186871,#186872,#186873,
#186874,#186875),.UNSPECIFIED.,.F.,.F.,(4,3,3,3,3,3,3,3,3,3,3,3,3,3,3,3,
3,4),(3.46944695195361E-18,2.58457451665415E-5,4.25394446196409E-5,6.4665986968742E-5,
7.57292581432925E-5,8.12608937305678E-5,8.26438026273866E-5,8.67925293178431E-5,
0.000116015624427815,0.000130188793976763,0.000151886926306223,0.000161963651211269,
0.000162735992470953,0.000173585058635683,0.000212487880462884,0.000255238173515455,
0.000301397761152582,0.000347170117271373),.UNSPECIFIED.);
#4517=B_SPLINE_CURVE_WITH_KNOTS('',3,(#186877,#186878,#186879,#186880,#186881,
#186882,#186883,#186884,#186885,#186886,#186887,#186888,#186889,#186890,
#186891,#186892,#186893,#186894,#186895,#186896,#186897,#186898,#186899,
#186900,#186901,#186902,#186903,#186904,#186905,#186906,#186907,#186908,
#186909,#186910,#186911,#186912,#186913,#186914,#186915,#186916,#186917,
#186918,#186919,#186920,#186921,#186922),.UNSPECIFIED.,.F.,.F.,(4,3,3,3,
3,3,3,3,3,3,3,3,3,3,3,4),(0.,2.57218162001907E-5,4.21568322567731E-5,6.45873314616956E-5,
7.58025810641568E-5,8.14102058653875E-5,8.28121120656951E-5,8.70178306666181E-5,
0.000116081955658954,0.000130526745999927,0.000162394111022066,0.000174035661333236,
0.000213138396957247,0.000256116935431918,0.000302406662853574,0.00034807132266646),
 .UNSPECIFIED.);
#4518=B_SPLINE_CURVE_WITH_KNOTS('',3,(#186923,#186924,#186925,#186926,#186927,
#186928,#186929,#186930,#186931,#186932,#186933,#186934,#186935,#186936,
#186937,#186938,#186939,#186940,#186941,#186942,#186943,#186944,#186945,
#186946,#186947,#186948,#186949,#186950,#186951,#186952,#186953,#186954,
#186955,#186956,#186957,#186958,#186959,#186960,#186961,#186962,#186963,
#186964,#186965,#186966,#186967,#186968,#186969,#186970,#186971,#186972,
#186973,#186974),.UNSPECIFIED.,.F.,.F.,(4,3,3,3,3,3,3,3,3,3,3,3,3,3,3,3,
3,4),(0.,4.29652152201144E-5,8.44519107599058E-5,0.000123669830872989,0.000159788877367001,
0.000170558847912645,0.000181218775907183,0.000181960046452432,0.000214460062643515,
0.000244755726198189,0.000255838271868953,0.000258503253867588,0.000261084955178765,
0.000289370476647358,0.000301101325502013,0.000321109510663637,0.000331113603244449,
0.000341117695825262),.UNSPECIFIED.);
#4519=B_SPLINE_CURVE_WITH_KNOTS('',3,(#186976,#186977,#186978,#186979,#186980,
#186981,#186982,#186983,#186984,#186985,#186986,#186987,#186988,#186989,
#186990,#186991,#186992,#186993,#186994,#186995,#186996,#186997,#186998,
#186999,#187000,#187001,#187002,#187003,#187004,#187005,#187006,#187007,
#187008,#187009,#187010,#187011,#187012,#187013,#187014,#187015,#187016,
#187017,#187018,#187019,#187020,#187021,#187022,#187023,#187024,#187025,
#187026,#187027),.UNSPECIFIED.,.F.,.F.,(4,3,3,3,3,3,3,3,3,3,3,3,3,3,3,3,
3,4),(1.20185167898973E-17,4.30706237879685E-5,8.4741708771448E-5,0.000124159989208214,
0.000160467076293205,0.000170998382116688,0.000182414994733758,0.000213747977645861,
0.000242415955904577,0.000256497573175034,0.000259169422895607,0.000261757777312412,
0.000289965130402962,0.000301877270772896,0.000321937017503138,0.000326951954185698,
0.000334474359209539,0.00034199676423338),.UNSPECIFIED.);
#4520=B_SPLINE_CURVE_WITH_KNOTS('',3,(#187028,#187029,#187030,#187031,#187032,
#187033,#187034,#187035,#187036,#187037,#187038,#187039,#187040,#187041,
#187042,#187043,#187044,#187045,#187046,#187047,#187048,#187049,#187050,
#187051,#187052,#187053,#187054,#187055,#187056,#187057,#187058,#187059,
#187060,#187061,#187062,#187063,#187064,#187065,#187066,#187067,#187068,
#187069,#187070,#187071,#187072,#187073,#187074,#187075,#187076,#187077,
#187078,#187079),.UNSPECIFIED.,.F.,.F.,(4,3,3,3,3,3,3,3,3,3,3,3,3,3,3,3,
3,4),(0.,2.58457451685695E-5,4.25394446195858E-5,6.46659869687149E-5,7.57292581432795E-5,
8.12608937305618E-5,8.26438026273824E-5,8.67925293178441E-5,0.000116015624427412,
0.000130188793976766,0.000151886926306227,0.000161963651211282,0.000162735992470958,
0.000173585058635688,0.000212487880459148,0.000255238173507998,0.000301397761141145,
0.000347170117271364),.UNSPECIFIED.);
#4521=B_SPLINE_CURVE_WITH_KNOTS('',3,(#187081,#187082,#187083,#187084,#187085,
#187086,#187087,#187088,#187089,#187090,#187091,#187092,#187093,#187094,
#187095,#187096,#187097,#187098,#187099,#187100,#187101,#187102,#187103,
#187104,#187105,#187106,#187107,#187108,#187109,#187110,#187111,#187112,
#187113,#187114,#187115,#187116,#187117,#187118,#187119,#187120,#187121,
#187122,#187123,#187124,#187125,#187126),.UNSPECIFIED.,.F.,.F.,(4,3,3,3,
3,3,3,3,3,3,3,3,3,3,3,4),(0.,2.57218162002906E-5,4.2156832256782E-5,6.4587331461703E-5,
7.58025810641635E-5,8.14102058653938E-5,8.28121120657014E-5,8.70178306666241E-5,
0.0001160819556579,0.000130526745999936,0.000162394111022055,0.000174035661333248,
0.000213138396956627,0.00025611693543044,0.000302406662850497,0.000348071322666479),
 .UNSPECIFIED.);
#4522=B_SPLINE_CURVE_WITH_KNOTS('',3,(#187127,#187128,#187129,#187130,#187131,
#187132,#187133,#187134,#187135,#187136,#187137,#187138,#187139,#187140,
#187141,#187142,#187143,#187144,#187145,#187146,#187147,#187148,#187149,
#187150,#187151,#187152,#187153,#187154,#187155,#187156,#187157,#187158,
#187159,#187160,#187161,#187162,#187163,#187164,#187165,#187166,#187167,
#187168,#187169,#187170,#187171,#187172,#187173,#187174,#187175,#187176,
#187177,#187178),.UNSPECIFIED.,.F.,.F.,(4,3,3,3,3,3,3,3,3,3,3,3,3,3,3,3,
3,4),(0.,4.29652152158326E-5,8.4451910753004E-5,0.000123669830864426,0.0001597888773574,
0.000170558847912627,0.000181218775907167,0.000181960046452397,0.000214460062643843,
0.000244755726198955,0.000255838271868947,0.000258503253867582,0.00026108495517876,
0.000289370476648254,0.000301101325502013,0.00032110951066364,0.000331113603244453,
0.000341117695825267),.UNSPECIFIED.);
#4523=B_SPLINE_CURVE_WITH_KNOTS('',3,(#187180,#187181,#187182,#187183,#187184,
#187185,#187186,#187187,#187188,#187189,#187190,#187191,#187192,#187193,
#187194,#187195,#187196,#187197,#187198,#187199,#187200,#187201,#187202,
#187203,#187204,#187205,#187206,#187207,#187208,#187209,#187210,#187211,
#187212,#187213,#187214,#187215,#187216,#187217,#187218,#187219,#187220,
#187221,#187222,#187223,#187224,#187225,#187226,#187227,#187228,#187229,
#187230,#187231),.UNSPECIFIED.,.F.,.F.,(4,3,3,3,3,3,3,3,3,3,3,3,3,3,3,3,
3,4),(0.,4.30706237868942E-5,8.474170876963E-5,0.000124159989205747,0.000160467076290168,
0.000170998382116697,0.000182414994733784,0.000213747977645871,0.000242415955904234,
0.000256497573175044,0.000259169422895617,0.000261757777312423,0.000289965130401751,
0.000301877270772907,0.000321937017503149,0.000326951954185709,0.00033447435920955,
0.000341996764233391),.UNSPECIFIED.);
#4524=B_SPLINE_CURVE_WITH_KNOTS('',3,(#187232,#187233,#187234,#187235,#187236,
#187237,#187238,#187239,#187240,#187241,#187242,#187243,#187244,#187245,
#187246,#187247,#187248,#187249,#187250,#187251,#187252,#187253,#187254,
#187255,#187256,#187257,#187258,#187259,#187260,#187261,#187262,#187263,
#187264,#187265,#187266,#187267,#187268,#187269,#187270,#187271,#187272,
#187273,#187274,#187275,#187276,#187277,#187278,#187279,#187280,#187281,
#187282,#187283),.UNSPECIFIED.,.F.,.F.,(4,3,3,3,3,3,3,3,3,3,3,3,3,3,3,3,
3,4),(0.,2.58457451695845E-5,4.25394446195289E-5,6.46659869686875E-5,7.57292581432667E-5,
8.12608937305564E-5,8.26438026273788E-5,8.6792529317846E-5,0.000116015624427563,
0.000130188793976769,0.000151886926306231,0.000161963651211295,0.000162735992470961,
0.000173585058635692,0.000212487880462759,0.00025523817351527,0.000301397761152659,
0.000347170117271367),.UNSPECIFIED.);
#4525=B_SPLINE_CURVE_WITH_KNOTS('',3,(#187285,#187286,#187287,#187288,#187289,
#187290,#187291,#187292,#187293,#187294,#187295,#187296,#187297,#187298,
#187299,#187300,#187301,#187302,#187303,#187304,#187305,#187306,#187307,
#187308,#187309,#187310,#187311,#187312,#187313,#187314,#187315,#187316,
#187317,#187318,#187319,#187320,#187321,#187322,#187323,#187324,#187325,
#187326,#187327,#187328,#187329,#187330),.UNSPECIFIED.,.F.,.F.,(4,3,3,3,
3,3,3,3,3,3,3,3,3,3,3,4),(0.,2.57218161974927E-5,4.21568322567519E-5,6.45873314616843E-5,
7.58025810641505E-5,8.14102058653837E-5,8.28121120656919E-5,8.70178306666168E-5,
0.000116081955657236,0.000130526745999925,0.000162394111022051,0.000174035661333234,
0.000213138396959219,0.000256116935435569,0.000302406662858305,0.000348071322666466),
 .UNSPECIFIED.);
#4526=B_SPLINE_CURVE_WITH_KNOTS('',3,(#187331,#187332,#187333,#187334,#187335,
#187336,#187337,#187338,#187339,#187340,#187341,#187342,#187343,#187344,
#187345,#187346,#187347,#187348,#187349,#187350,#187351,#187352,#187353,
#187354,#187355,#187356,#187357,#187358,#187359,#187360,#187361,#187362,
#187363,#187364,#187365,#187366,#187367,#187368,#187369,#187370,#187371,
#187372,#187373,#187374,#187375,#187376,#187377,#187378,#187379,#187380,
#187381,#187382),.UNSPECIFIED.,.F.,.F.,(4,3,3,3,3,3,3,3,3,3,3,3,3,3,3,3,
3,4),(0.,4.29652152193347E-5,8.4451910758867E-5,0.000123669830872074,0.000159788877366483,
0.000170558847912628,0.000181218775907168,0.000181960046452402,0.000214460062643761,
0.00024475572619894,0.000255838271868948,0.000258503253867583,0.000261084955178761,
0.00028937047664693,0.000301101325502014,0.000321109510663641,0.000331113603244454,
0.000341117695825268),.UNSPECIFIED.);
#4527=B_SPLINE_CURVE_WITH_KNOTS('',3,(#187384,#187385,#187386,#187387,#187388,
#187389,#187390,#187391,#187392,#187393,#187394,#187395,#187396,#187397,
#187398,#187399,#187400,#187401,#187402,#187403,#187404,#187405,#187406,
#187407,#187408,#187409,#187410,#187411,#187412,#187413,#187414,#187415,
#187416,#187417,#187418,#187419,#187420,#187421,#187422,#187423,#187424,
#187425,#187426,#187427,#187428,#187429,#187430,#187431,#187432,#187433,
#187434,#187435),.UNSPECIFIED.,.F.,.F.,(4,3,3,3,3,3,3,3,3,3,3,3,3,3,3,3,
3,4),(0.,4.30706237884788E-5,8.47417087722986E-5,0.000124159989209235,0.000160467076294441,
0.000170998382116698,0.00018241499473378,0.000213747977645868,0.000242415955903622,
0.000256497573175039,0.000259169422895612,0.000261757777312418,0.000289965130403898,
0.000301877270772899,0.00032193701750314,0.0003269519541857,0.00033447435920954,
0.00034199676423338),.UNSPECIFIED.);
#4528=B_SPLINE_CURVE_WITH_KNOTS('',3,(#187436,#187437,#187438,#187439,#187440,
#187441,#187442,#187443,#187444,#187445,#187446,#187447,#187448,#187449,
#187450,#187451,#187452,#187453,#187454,#187455,#187456,#187457,#187458,
#187459,#187460,#187461,#187462,#187463,#187464,#187465,#187466,#187467,
#187468,#187469,#187470,#187471,#187472,#187473,#187474,#187475,#187476,
#187477,#187478,#187479,#187480,#187481,#187482,#187483,#187484,#187485,
#187486,#187487),.UNSPECIFIED.,.F.,.F.,(4,3,3,3,3,3,3,3,3,3,3,3,3,3,3,3,
3,4),(0.,2.58457451704755E-5,4.25394446194672E-5,6.46659869686538E-5,7.57292581432472E-5,
8.12608937305438E-5,8.2643802627368E-5,8.67925293178405E-5,0.000116015624427198,
0.000130188793976761,0.000151886926306221,0.000161963651211268,0.000162735992470951,
0.000173585058635681,0.000212487880458066,0.000255238173506561,0.000301397761140657,
0.000347170117271375),.UNSPECIFIED.);
#4529=B_SPLINE_CURVE_WITH_KNOTS('',3,(#187489,#187490,#187491,#187492,#187493,
#187494,#187495,#187496,#187497,#187498,#187499,#187500,#187501,#187502,
#187503,#187504,#187505,#187506,#187507,#187508,#187509,#187510,#187511,
#187512,#187513,#187514,#187515,#187516,#187517,#187518,#187519,#187520,
#187521,#187522,#187523,#187524,#187525,#187526,#187527,#187528,#187529,
#187530,#187531,#187532,#187533,#187534),.UNSPECIFIED.,.F.,.F.,(4,3,3,3,
3,3,3,3,3,3,3,3,3,3,3,4),(0.,2.57218162000528E-5,4.2156832256754E-5,6.45873314616856E-5,
7.58025810641514E-5,8.14102058653844E-5,8.28121120656926E-5,8.70178306666173E-5,
0.00011608195565755,0.000130526745999926,0.000162394111022041,0.000174035661333235,
0.000213138396956922,0.000256116935431229,0.000302406662852368,0.000348071322666458),
 .UNSPECIFIED.);
#4530=B_SPLINE_CURVE_WITH_KNOTS('',3,(#187535,#187536,#187537,#187538,#187539,
#187540,#187541,#187542,#187543,#187544,#187545,#187546,#187547,#187548,
#187549,#187550,#187551,#187552,#187553,#187554,#187555,#187556,#187557,
#187558,#187559,#187560,#187561,#187562,#187563,#187564,#187565,#187566,
#187567,#187568,#187569,#187570,#187571,#187572,#187573,#187574,#187575,
#187576,#187577,#187578,#187579,#187580,#187581,#187582,#187583,#187584,
#187585,#187586),.UNSPECIFIED.,.F.,.F.,(4,3,3,3,3,3,3,3,3,3,3,3,3,3,3,3,
3,4),(0.,4.29652152177208E-5,8.44519107561497E-5,0.000123669830868545,0.000159788877362415,
0.00017055884791262,0.00018121877590716,0.000181960046452397,0.000214460062643471,
0.000244755726198109,0.000255838271868942,0.000258503253867577,0.000261084955178755,
0.000289370476648085,0.00030110132550201,0.000321109510663637,0.000331113603244451,
0.000341117695825265),.UNSPECIFIED.);
#4531=B_SPLINE_CURVE_WITH_KNOTS('',3,(#187588,#187589,#187590,#187591,#187592,
#187593,#187594,#187595,#187596,#187597,#187598,#187599,#187600,#187601,
#187602,#187603,#187604,#187605,#187606,#187607,#187608,#187609,#187610,
#187611,#187612,#187613,#187614,#187615,#187616,#187617,#187618,#187619,
#187620,#187621,#187622,#187623,#187624,#187625,#187626,#187627,#187628,
#187629,#187630,#187631,#187632,#187633,#187634,#187635,#187636,#187637,
#187638,#187639),.UNSPECIFIED.,.F.,.F.,(4,3,3,3,3,3,3,3,3,3,3,3,3,3,3,3,
3,4),(0.,4.30706237855123E-5,8.47417087672605E-5,0.000124159989202624,0.000160467076286203,
0.000170998382116679,0.000182414994733753,0.000213747977645857,0.000242415955904274,
0.000256497573175035,0.000259169422895609,0.000261757777312415,0.000289965130404309,
0.000301877270772903,0.000321937017503147,0.000326951954185708,0.00033447435920955,
0.000341996764233392),.UNSPECIFIED.);
#4532=B_SPLINE_CURVE_WITH_KNOTS('',3,(#187640,#187641,#187642,#187643,#187644,
#187645,#187646,#187647,#187648,#187649,#187650,#187651,#187652,#187653,
#187654,#187655,#187656,#187657,#187658,#187659,#187660,#187661,#187662,
#187663,#187664,#187665,#187666,#187667,#187668,#187669,#187670,#187671,
#187672,#187673,#187674,#187675,#187676,#187677,#187678,#187679,#187680,
#187681,#187682,#187683,#187684,#187685,#187686,#187687,#187688,#187689,
#187690,#187691),.UNSPECIFIED.,.F.,.F.,(4,3,3,3,3,3,3,3,3,3,3,3,3,3,3,3,
3,4),(6.93889390390723E-18,2.58457451683063E-5,4.25394446195843E-5,6.46659869687167E-5,
7.57292581432828E-5,8.12608937305659E-5,8.26438026273867E-5,8.6792529317849E-5,
0.000116015624427382,0.00013018879397677,0.000151886926306231,0.000161963651211302,
0.000162735992470961,0.000173585058635691,0.000212487880461466,0.000255238173511805,
0.000301397761145146,0.000347170117271358),.UNSPECIFIED.);
#4533=B_SPLINE_CURVE_WITH_KNOTS('',3,(#187693,#187694,#187695,#187696,#187697,
#187698,#187699,#187700,#187701,#187702,#187703,#187704,#187705,#187706,
#187707,#187708,#187709,#187710,#187711,#187712,#187713,#187714,#187715,
#187716,#187717,#187718,#187719,#187720,#187721,#187722,#187723,#187724,
#187725,#187726,#187727,#187728,#187729,#187730,#187731,#187732,#187733,
#187734,#187735,#187736,#187737,#187738),.UNSPECIFIED.,.F.,.F.,(4,3,3,3,
3,3,3,3,3,3,3,3,3,3,3,4),(6.93889390390723E-18,2.57218161972534E-5,4.2156832256757E-5,
6.458733146169E-5,7.58025810641566E-5,8.14102058653898E-5,8.28121120656981E-5,
8.70178306666231E-5,0.000116081955657329,0.000130526745999931,0.000162394111022074,
0.000174035661333239,0.000213138396957694,0.000256116935432815,0.000302406662854965,
0.000348071322666459),.UNSPECIFIED.);
#4534=B_SPLINE_CURVE_WITH_KNOTS('',3,(#187739,#187740,#187741,#187742,#187743,
#187744,#187745,#187746,#187747,#187748,#187749,#187750,#187751,#187752,
#187753,#187754,#187755,#187756,#187757,#187758,#187759,#187760,#187761,
#187762,#187763,#187764,#187765,#187766,#187767,#187768,#187769,#187770,
#187771,#187772,#187773,#187774,#187775,#187776,#187777,#187778,#187779,
#187780,#187781,#187782,#187783,#187784,#187785,#187786,#187787,#187788,
#187789,#187790),.UNSPECIFIED.,.F.,.F.,(4,3,3,3,3,3,3,3,3,3,3,3,3,3,3,3,
3,4),(0.,4.2965215221334E-5,8.44519107622145E-5,0.000123669830876504,0.000159788877371945,
0.000170558847912634,0.000181218775907173,0.000181960046452426,0.000214460062644004,
0.0002447557261995,0.000255838271868948,0.000258503253867583,0.000261084955178761,
0.000289370476645958,0.000301101325502012,0.000321109510663638,0.000331113603244451,
0.000341117695825263),.UNSPECIFIED.);
#4535=B_SPLINE_CURVE_WITH_KNOTS('',3,(#187792,#187793,#187794,#187795,#187796,
#187797,#187798,#187799,#187800,#187801,#187802,#187803,#187804,#187805,
#187806,#187807,#187808,#187809,#187810,#187811,#187812,#187813,#187814,
#187815,#187816,#187817,#187818,#187819,#187820,#187821,#187822,#187823,
#187824,#187825,#187826,#187827,#187828,#187829,#187830,#187831,#187832,
#187833,#187834,#187835,#187836,#187837,#187838,#187839,#187840,#187841,
#187842,#187843),.UNSPECIFIED.,.F.,.F.,(4,3,3,3,3,3,3,3,3,3,3,3,3,3,3,3,
3,4),(0.,4.30706237842057E-5,8.47417087648121E-5,0.000124159989199012,0.000160467076281244,
0.000170998382116703,0.000182414994733766,0.000213747977645878,0.00024241595590268,
0.000256497573175052,0.000259169422895626,0.000261757777312431,0.000289965130404317,
0.000301877270772916,0.000321937017503159,0.00032695195418572,0.000334474359209561,
0.000341996764233402),.UNSPECIFIED.);
#4536=B_SPLINE_CURVE_WITH_KNOTS('',3,(#187844,#187845,#187846,#187847,#187848,
#187849,#187850,#187851,#187852,#187853,#187854,#187855,#187856,#187857,
#187858,#187859,#187860,#187861,#187862,#187863,#187864,#187865,#187866,
#187867,#187868,#187869,#187870,#187871,#187872,#187873,#187874,#187875,
#187876,#187877,#187878,#187879,#187880,#187881,#187882,#187883,#187884,
#187885,#187886,#187887,#187888,#187889,#187890,#187891,#187892,#187893,
#187894,#187895),.UNSPECIFIED.,.F.,.F.,(4,3,3,3,3,3,3,3,3,3,3,3,3,3,3,3,
3,4),(3.46944695195361E-18,2.58457451697369E-5,4.25394446196474E-5,6.46659869687486E-5,
7.57292581432992E-5,8.12608937305745E-5,8.26438026273933E-5,8.67925293178498E-5,
0.0001160156244268,0.000130188793976773,0.000151886926306235,0.000161963651211278,
0.000162735992470965,0.000173585058635696,0.000212487880457896,0.000255238173505114,
0.000301397761135914,0.000347170117271375),.UNSPECIFIED.);
#4537=B_SPLINE_CURVE_WITH_KNOTS('',3,(#187897,#187898,#187899,#187900,#187901,
#187902,#187903,#187904,#187905,#187906,#187907,#187908,#187909,#187910,
#187911,#187912,#187913,#187914,#187915,#187916,#187917,#187918,#187919,
#187920,#187921,#187922,#187923,#187924,#187925,#187926,#187927,#187928,
#187929,#187930,#187931,#187932,#187933,#187934,#187935,#187936,#187937,
#187938,#187939,#187940,#187941,#187942),.UNSPECIFIED.,.F.,.F.,(4,3,3,3,
3,3,3,3,3,3,3,3,3,3,3,4),(0.,2.57218161993105E-5,4.21568322568682E-5,6.45873314617395E-5,
7.58025810641752E-5,8.1410205865393E-5,8.28121120656975E-5,8.70178306666108E-5,
0.000116081955657196,0.000130526745999916,0.000162394111022044,0.000174035661333222,
0.000213138396958914,0.000256116935435134,0.000302406662858135,0.000348071322666431),
 .UNSPECIFIED.);
#4538=B_SPLINE_CURVE_WITH_KNOTS('',3,(#187943,#187944,#187945,#187946,#187947,
#187948,#187949,#187950,#187951,#187952,#187953,#187954,#187955,#187956,
#187957,#187958,#187959,#187960,#187961,#187962,#187963,#187964,#187965,
#187966,#187967,#187968,#187969,#187970,#187971,#187972,#187973,#187974,
#187975,#187976,#187977,#187978,#187979,#187980,#187981,#187982,#187983,
#187984,#187985,#187986,#187987,#187988,#187989,#187990,#187991,#187992,
#187993,#187994),.UNSPECIFIED.,.F.,.F.,(4,3,3,3,3,3,3,3,3,3,3,3,3,3,3,3,
3,4),(0.,4.29652152131072E-5,8.44519107485544E-5,0.000123669830858988,0.000159788877351408,
0.000170558847912628,0.000181218775907167,0.00018196004645239,0.000214460062642862,
0.000244755726196479,0.00025583827186894,0.000258503253867575,0.000261084955178753,
0.000289370476649787,0.000301101325502002,0.000321109510663627,0.00033111360324444,
0.000341117695825252),.UNSPECIFIED.);
#4539=B_SPLINE_CURVE_WITH_KNOTS('',3,(#187996,#187997,#187998,#187999,#188000,
#188001,#188002,#188003,#188004,#188005,#188006,#188007,#188008,#188009,
#188010,#188011,#188012,#188013,#188014,#188015,#188016,#188017,#188018,
#188019,#188020,#188021,#188022,#188023,#188024,#188025,#188026,#188027,
#188028,#188029,#188030,#188031,#188032,#188033,#188034,#188035,#188036,
#188037,#188038,#188039,#188040,#188041,#188042,#188043,#188044,#188045,
#188046,#188047),.UNSPECIFIED.,.F.,.F.,(4,3,3,3,3,3,3,3,3,3,3,3,3,3,3,3,
3,4),(0.,4.30706237861054E-5,8.47417087681986E-5,0.000124159989203905,0.000160467076287747,
0.000170998382116685,0.000182414994733779,0.000213747977645861,0.000242415955902392,
0.000256497573175037,0.000259169422895611,0.000261757777312416,0.000289965130404567,
0.000301877270772903,0.000321937017503146,0.000326951954185707,0.000334474359209548,
0.000341996764233389),.UNSPECIFIED.);
#4540=B_SPLINE_CURVE_WITH_KNOTS('',3,(#188048,#188049,#188050,#188051,#188052,
#188053,#188054,#188055,#188056,#188057,#188058,#188059,#188060,#188061,
#188062,#188063,#188064,#188065,#188066,#188067,#188068,#188069,#188070,
#188071,#188072,#188073,#188074,#188075,#188076,#188077,#188078,#188079,
#188080,#188081,#188082,#188083,#188084,#188085,#188086,#188087,#188088,
#188089,#188090,#188091,#188092,#188093,#188094,#188095,#188096,#188097,
#188098,#188099),.UNSPECIFIED.,.F.,.F.,(4,3,3,3,3,3,3,3,3,3,3,3,3,3,3,3,
3,4),(3.46944695195361E-18,2.58457451678929E-5,4.25394446195445E-5,6.46659869686953E-5,
7.57292581432707E-5,8.12608937305584E-5,8.26438026273803E-5,8.67925293178461E-5,
0.000116015624426703,0.000130188793976767,0.000151886926306228,0.000161963651211296,
0.000162735992470958,0.000173585058635689,0.00021248788045957,0.000255238173508425,
0.000301397761140786,0.000347170117271359),.UNSPECIFIED.);
#4541=B_SPLINE_CURVE_WITH_KNOTS('',3,(#188101,#188102,#188103,#188104,#188105,
#188106,#188107,#188108,#188109,#188110,#188111,#188112,#188113,#188114,
#188115,#188116,#188117,#188118,#188119,#188120,#188121,#188122,#188123,
#188124,#188125,#188126,#188127,#188128,#188129,#188130,#188131,#188132,
#188133,#188134,#188135,#188136,#188137,#188138,#188139,#188140,#188141,
#188142,#188143,#188144,#188145,#188146),.UNSPECIFIED.,.F.,.F.,(4,3,3,3,
3,3,3,3,3,3,3,3,3,3,3,4),(0.,2.57218162010215E-5,4.21568322568023E-5,6.45873314617128E-5,
7.5802581064168E-5,8.14102058653956E-5,8.28121120657025E-5,8.70178306666232E-5,
0.000116081955658569,0.000130526745999935,0.000162394111022054,0.000174035661333246,
0.000213138396958572,0.000256116935434451,0.000302406662857123,0.000348071322666499),
 .UNSPECIFIED.);
#4542=B_SPLINE_CURVE_WITH_KNOTS('',3,(#188147,#188148,#188149,#188150,#188151,
#188152,#188153,#188154,#188155,#188156,#188157,#188158,#188159,#188160,
#188161,#188162,#188163,#188164,#188165,#188166,#188167,#188168,#188169,
#188170,#188171,#188172,#188173,#188174,#188175,#188176,#188177,#188178,
#188179,#188180,#188181,#188182,#188183,#188184,#188185,#188186,#188187,
#188188,#188189,#188190,#188191,#188192,#188193,#188194,#188195,#188196,
#188197,#188198),.UNSPECIFIED.,.F.,.F.,(4,3,3,3,3,3,3,3,3,3,3,3,3,3,3,3,
3,4),(0.,4.2965215210667E-5,8.44519107445277E-5,0.000123669830853843,0.000159788877345156,
0.000170558847912632,0.000181218775907172,0.000181960046452383,0.000214460062643245,
0.000244755726197489,0.000255838271868954,0.000258503253867589,0.000261084955178766,
0.000289370476648082,0.000301101325502021,0.000321109510663648,0.000331113603244462,
0.000341117695825276),.UNSPECIFIED.);
#4543=B_SPLINE_CURVE_WITH_KNOTS('',3,(#188200,#188201,#188202,#188203,#188204,
#188205,#188206,#188207,#188208,#188209,#188210,#188211,#188212,#188213,
#188214,#188215,#188216,#188217,#188218,#188219,#188220,#188221,#188222,
#188223,#188224,#188225,#188226,#188227,#188228,#188229,#188230,#188231,
#188232,#188233,#188234,#188235,#188236,#188237,#188238,#188239,#188240,
#188241,#188242,#188243,#188244,#188245,#188246,#188247,#188248,#188249,
#188250,#188251),.UNSPECIFIED.,.F.,.F.,(4,3,3,3,3,3,3,3,3,3,3,3,3,3,3,3,
3,4),(0.,4.30706237856851E-5,8.47417087672796E-5,0.000124159989202264,0.000160467076285325,
0.000170998382116702,0.000182414994733779,0.000213747977645874,0.000242415955903721,
0.000256497573175046,0.00025916942289562,0.000261757777312425,0.000289965130403,
0.000301877270772908,0.000321937017503149,0.00032695195418571,0.00033447435920955,
0.000341996764233391),.UNSPECIFIED.);
#4544=B_SPLINE_CURVE_WITH_KNOTS('',3,(#188252,#188253,#188254,#188255,#188256,
#188257,#188258,#188259,#188260,#188261,#188262,#188263,#188264,#188265,
#188266,#188267,#188268,#188269,#188270,#188271,#188272,#188273,#188274,
#188275,#188276,#188277,#188278,#188279,#188280,#188281,#188282,#188283,
#188284,#188285,#188286,#188287,#188288,#188289,#188290,#188291,#188292,
#188293,#188294,#188295,#188296,#188297,#188298,#188299,#188300,#188301,
#188302,#188303),.UNSPECIFIED.,.F.,.F.,(4,3,3,3,3,3,3,3,3,3,3,3,3,3,3,3,
3,4),(3.46944695195361E-18,2.58457451677859E-5,4.2539444619544E-5,6.46659869686969E-5,
7.57292581432733E-5,8.12608937305615E-5,8.26438026273836E-5,8.67925293178497E-5,
0.000116015624427814,0.000130188793976773,0.000151886926306234,0.000161963651211293,
0.000162735992470965,0.000173585058635696,0.00021248788046203,0.000255238173515158,
0.000301397761155678,0.000347170117271372),.UNSPECIFIED.);
#4545=B_SPLINE_CURVE_WITH_KNOTS('',3,(#188305,#188306,#188307,#188308,#188309,
#188310,#188311,#188312,#188313,#188314,#188315,#188316,#188317,#188318,
#188319,#188320,#188321,#188322,#188323,#188324,#188325,#188326,#188327,
#188328,#188329,#188330,#188331,#188332,#188333,#188334,#188335,#188336,
#188337,#188338,#188339,#188340,#188341,#188342,#188343,#188344,#188345,
#188346,#188347,#188348,#188349,#188350),.UNSPECIFIED.,.F.,.F.,(4,3,3,3,
3,3,3,3,3,3,3,3,3,3,3,4),(0.,2.57218161992883E-5,4.21568322568875E-5,6.45873314617512E-5,
7.5802581064183E-5,8.14102058653989E-5,8.28121120657029E-5,8.70178306666148E-5,
0.000116081955658576,0.000130526745999922,0.00016239411102203,0.00017403566133323,
0.000213138396955947,0.000256116935429326,0.000302406662849522,0.000348071322666453),
 .UNSPECIFIED.);
#4546=B_SPLINE_CURVE_WITH_KNOTS('',3,(#188351,#188352,#188353,#188354,#188355,
#188356,#188357,#188358,#188359,#188360,#188361,#188362,#188363,#188364,
#188365,#188366,#188367,#188368,#188369,#188370,#188371,#188372,#188373,
#188374,#188375,#188376,#188377,#188378,#188379,#188380,#188381,#188382,
#188383,#188384,#188385,#188386,#188387,#188388,#188389,#188390,#188391,
#188392,#188393,#188394,#188395,#188396,#188397,#188398,#188399,#188400,
#188401,#188402),.UNSPECIFIED.,.F.,.F.,(4,3,3,3,3,3,3,3,3,3,3,3,3,3,3,3,
3,4),(0.,4.29652152159528E-5,8.44519107530115E-5,0.000123669830864204,0.000159788877356665,
0.000170558847912628,0.000181218775907167,0.000181960046452395,0.000214460062643637,
0.000244755726198709,0.00025583827186894,0.000258503253867575,0.000261084955178752,
0.000289370476647891,0.000301101325502002,0.000321109510663627,0.00033111360324444,
0.000341117695825252),.UNSPECIFIED.);
#4547=B_SPLINE_CURVE_WITH_KNOTS('',3,(#188404,#188405,#188406,#188407,#188408,
#188409,#188410,#188411,#188412,#188413,#188414,#188415,#188416,#188417,
#188418,#188419,#188420,#188421,#188422,#188423,#188424,#188425,#188426,
#188427,#188428,#188429,#188430,#188431,#188432,#188433,#188434,#188435,
#188436,#188437,#188438,#188439,#188440,#188441,#188442,#188443,#188444,
#188445,#188446,#188447,#188448,#188449,#188450,#188451,#188452,#188453,
#188454,#188455),.UNSPECIFIED.,.F.,.F.,(4,3,3,3,3,3,3,3,3,3,3,3,3,3,3,3,
3,4),(0.,4.3070623787178E-5,8.47417087700662E-5,0.000124159989206384,0.000160467076290823,
0.000170998382116695,0.000182414994733763,0.000213747977645866,0.000242415955903335,
0.000256497573175037,0.00025916942289561,0.000261757777312416,0.000289965130403811,
0.000301877270772898,0.000321937017503139,0.000326951954185699,0.00033447435920954,
0.00034199676423338),.UNSPECIFIED.);
#4548=B_SPLINE_CURVE_WITH_KNOTS('',3,(#188456,#188457,#188458,#188459,#188460,
#188461,#188462,#188463,#188464,#188465,#188466,#188467,#188468,#188469,
#188470,#188471,#188472,#188473,#188474,#188475,#188476,#188477,#188478,
#188479,#188480,#188481,#188482,#188483,#188484,#188485,#188486,#188487,
#188488,#188489,#188490,#188491,#188492,#188493,#188494,#188495,#188496,
#188497,#188498,#188499,#188500,#188501,#188502,#188503,#188504,#188505,
#188506,#188507),.UNSPECIFIED.,.F.,.F.,(4,3,3,3,3,3,3,3,3,3,3,3,3,3,3,3,
3,4),(0.,2.58457451688714E-5,4.25394446196352E-5,6.46659869687418E-5,7.5729258143295E-5,
8.12608937305717E-5,8.26438026273908E-5,8.67925293178483E-5,0.000116015624427734,
0.000130188793976772,0.000151886926306235,0.000161963651211294,0.000162735992470966,
0.000173585058635697,0.000212487880462616,0.000255238173515711,0.000301397761155049,
0.000347170117271365),.UNSPECIFIED.);
#4549=B_SPLINE_CURVE_WITH_KNOTS('',3,(#188509,#188510,#188511,#188512,#188513,
#188514,#188515,#188516,#188517,#188518,#188519,#188520,#188521,#188522,
#188523,#188524,#188525,#188526,#188527,#188528,#188529,#188530,#188531,
#188532,#188533,#188534,#188535,#188536,#188537,#188538,#188539,#188540,
#188541,#188542,#188543,#188544,#188545,#188546,#188547,#188548,#188549,
#188550,#188551,#188552,#188553,#188554),.UNSPECIFIED.,.F.,.F.,(4,3,3,3,
3,3,3,3,3,3,3,3,3,3,3,4),(0.,2.57218162002632E-5,4.21568322568512E-5,6.45873314617311E-5,
7.58025810641711E-5,8.1410205865391E-5,8.2812112065696E-5,8.7017830666611E-5,
0.000116081955658825,0.000130526745999917,0.000162394111022047,0.000174035661333222,
0.000213138396959396,0.000256116935436168,0.000302406662860064,0.000348071322666447),
 .UNSPECIFIED.);
#4550=B_SPLINE_CURVE_WITH_KNOTS('',3,(#188555,#188556,#188557,#188558,#188559,
#188560,#188561,#188562,#188563,#188564,#188565,#188566,#188567,#188568,
#188569,#188570,#188571,#188572,#188573,#188574,#188575,#188576,#188577,
#188578,#188579,#188580,#188581,#188582,#188583,#188584,#188585,#188586,
#188587,#188588,#188589,#188590,#188591,#188592,#188593,#188594,#188595,
#188596,#188597,#188598,#188599,#188600,#188601,#188602,#188603,#188604,
#188605,#188606),.UNSPECIFIED.,.F.,.F.,(4,3,3,3,3,3,3,3,3,3,3,3,3,3,3,3,
3,4),(0.,4.29652152163955E-5,8.44519107540137E-5,0.000123669830865945,0.000159788877359403,
0.000170558847912639,0.000181218775907178,0.00018196004645242,0.00021446006264403,
0.000244755726199579,0.000255838271868947,0.000258503253867582,0.000261084955178759,
0.0002893704766472,0.000301101325502007,0.000321109510663631,0.000331113603244444,
0.000341117695825256),.UNSPECIFIED.);
#4551=B_SPLINE_CURVE_WITH_KNOTS('',3,(#188608,#188609,#188610,#188611,#188612,
#188613,#188614,#188615,#188616,#188617,#188618,#188619,#188620,#188621,
#188622,#188623,#188624,#188625,#188626,#188627,#188628,#188629,#188630,
#188631,#188632,#188633,#188634,#188635,#188636,#188637,#188638,#188639,
#188640,#188641,#188642,#188643,#188644,#188645,#188646,#188647,#188648,
#188649,#188650,#188651,#188652,#188653,#188654,#188655,#188656,#188657,
#188658,#188659),.UNSPECIFIED.,.F.,.F.,(4,3,3,3,3,3,3,3,3,3,3,3,3,3,3,3,
3,4),(0.,4.30706237872259E-5,8.47417087700833E-5,0.000124159989206224,0.000160467076290431,
0.000170998382116682,0.000182414994733756,0.000213747977645859,0.000242415955905012,
0.000256497573175035,0.000259169422895609,0.000261757777312414,0.000289965130402064,
0.000301877270772901,0.000321937017503145,0.000326951954185706,0.000334474359209547,
0.000341996764233389),.UNSPECIFIED.);
#4552=B_SPLINE_CURVE_WITH_KNOTS('',3,(#188660,#188661,#188662,#188663,#188664,
#188665,#188666,#188667,#188668,#188669,#188670,#188671,#188672,#188673,
#188674,#188675,#188676,#188677,#188678,#188679,#188680,#188681,#188682,
#188683,#188684,#188685,#188686,#188687,#188688,#188689,#188690,#188691,
#188692,#188693,#188694,#188695,#188696,#188697,#188698,#188699,#188700,
#188701,#188702,#188703,#188704,#188705,#188706,#188707,#188708,#188709,
#188710,#188711),.UNSPECIFIED.,.F.,.F.,(4,3,3,3,3,3,3,3,3,3,3,3,3,3,3,3,
3,4),(0.,2.58457451680095E-5,4.2539444619618E-5,6.46659869687305E-5,7.57292581432868E-5,
8.12608937305649E-5,8.26438026273845E-5,8.67925293178431E-5,0.000116015624426959,
0.000130188793976765,0.000151886926306225,0.000161963651211284,0.000162735992470956,
0.000173585058635686,0.000212487880456419,0.000255238173500689,0.000301397761125226,
0.000347170117271373),.UNSPECIFIED.);
#4553=B_SPLINE_CURVE_WITH_KNOTS('',3,(#188713,#188714,#188715,#188716,#188717,
#188718,#188719,#188720,#188721,#188722,#188723,#188724,#188725,#188726,
#188727,#188728,#188729,#188730,#188731,#188732,#188733,#188734,#188735,
#188736,#188737,#188738,#188739,#188740,#188741,#188742,#188743,#188744,
#188745,#188746,#188747,#188748,#188749,#188750,#188751,#188752,#188753,
#188754,#188755,#188756,#188757,#188758),.UNSPECIFIED.,.F.,.F.,(4,3,3,3,
3,3,3,3,3,3,3,3,3,3,3,4),(8.67361737988404E-19,2.57218162009145E-5,4.21568322566762E-5,
6.45873314616513E-5,7.58025810641389E-5,8.14102058653827E-5,8.28121120656936E-5,
8.70178306666264E-5,0.000116081955658878,0.000130526745999939,0.000162394111022056,
0.000174035661333252,0.000213138396958378,0.000256116935433806,0.000302406662855308,
0.000348071322666491),.UNSPECIFIED.);
#4554=B_SPLINE_CURVE_WITH_KNOTS('',3,(#188759,#188760,#188761,#188762,#188763,
#188764,#188765,#188766,#188767,#188768,#188769,#188770,#188771,#188772,
#188773,#188774,#188775,#188776,#188777,#188778,#188779,#188780,#188781,
#188782,#188783,#188784,#188785,#188786,#188787,#188788,#188789,#188790,
#188791,#188792,#188793,#188794,#188795,#188796,#188797,#188798,#188799,
#188800,#188801,#188802,#188803,#188804,#188805,#188806,#188807,#188808,
#188809,#188810),.UNSPECIFIED.,.F.,.F.,(4,3,3,3,3,3,3,3,3,3,3,3,3,3,3,3,
3,4),(0.,4.29652152202514E-5,8.4451910759941E-5,0.000123669830872665,0.000159788877366079,
0.000170558847912629,0.000181218775907169,0.000181960046452395,0.000214460062643499,
0.000244755726198446,0.000255838271868949,0.000258503253867584,0.000261084955178762,
0.000289370476647764,0.000301101325502016,0.000321109510663643,0.000331113603244456,
0.00034111769582527),.UNSPECIFIED.);
#4555=B_SPLINE_CURVE_WITH_KNOTS('',3,(#188812,#188813,#188814,#188815,#188816,
#188817,#188818,#188819,#188820,#188821,#188822,#188823,#188824,#188825,
#188826,#188827,#188828,#188829,#188830,#188831,#188832,#188833,#188834,
#188835,#188836,#188837,#188838,#188839,#188840,#188841,#188842,#188843,
#188844,#188845,#188846,#188847,#188848,#188849,#188850,#188851,#188852,
#188853,#188854,#188855,#188856,#188857,#188858,#188859,#188860,#188861,
#188862,#188863),.UNSPECIFIED.,.F.,.F.,(4,3,3,3,3,3,3,3,3,3,3,3,3,3,3,3,
3,4),(5.96311194867027E-19,4.3070623785328E-5,8.47417087668814E-5,0.000124159989202045,
0.000160467076285363,0.000170998382116684,0.000182414994733754,0.000213747977645859,
0.000242415955902855,0.000256497573175034,0.000259169422895607,0.000261757777312412,
0.000289965130403962,0.000301877270772898,0.00032193701750314,0.000326951954185701,
0.000334474359209542,0.000341996764233383),.UNSPECIFIED.);
#4556=B_SPLINE_CURVE_WITH_KNOTS('',3,(#188864,#188865,#188866,#188867,#188868,
#188869,#188870,#188871,#188872,#188873,#188874,#188875,#188876,#188877,
#188878,#188879,#188880,#188881,#188882,#188883,#188884,#188885,#188886,
#188887,#188888,#188889,#188890,#188891,#188892,#188893,#188894,#188895,
#188896,#188897,#188898,#188899,#188900,#188901,#188902,#188903,#188904,
#188905,#188906,#188907,#188908,#188909,#188910,#188911,#188912,#188913,
#188914,#188915),.UNSPECIFIED.,.F.,.F.,(4,3,3,3,3,3,3,3,3,3,3,3,3,3,3,3,
3,4),(2.76132740804902E-19,2.58457451672193E-5,4.25394446196239E-5,6.46659869687285E-5,
7.57292581432808E-5,8.1260893730557E-5,8.2643802627376E-5,8.67925293178331E-5,
0.000116015624427903,0.00013018879397675,0.000151886926306208,0.000161963651211269,
0.000162735992470937,0.000173585058635666,0.000212487880463427,0.000255238173517339,
0.000301397761157609,0.000347170117271358),.UNSPECIFIED.);
#4557=B_SPLINE_CURVE_WITH_KNOTS('',3,(#188917,#188918,#188919,#188920,#188921,
#188922,#188923,#188924,#188925,#188926,#188927,#188928,#188929,#188930,
#188931,#188932,#188933,#188934,#188935,#188936,#188937,#188938,#188939,
#188940,#188941,#188942,#188943,#188944,#188945,#188946,#188947,#188948,
#188949,#188950,#188951,#188952,#188953,#188954,#188955,#188956,#188957,
#188958,#188959,#188960,#188961,#188962),.UNSPECIFIED.,.F.,.F.,(4,3,3,3,
3,3,3,3,3,3,3,3,3,3,3,4),(2.74438674910393E-19,2.57218161992784E-5,4.21568322568869E-5,
6.45873314617526E-5,7.58025810641854E-5,8.14102058654018E-5,8.2812112065706E-5,
8.70178306666183E-5,0.000116081955658528,0.000130526745999927,0.000162394111022038,
0.000174035661333236,0.000213138396956903,0.000256116935431176,0.000302406662852235,
0.000348071322666485),.UNSPECIFIED.);
#4558=B_SPLINE_CURVE_WITH_KNOTS('',3,(#188963,#188964,#188965,#188966,#188967,
#188968,#188969,#188970,#188971,#188972,#188973,#188974,#188975,#188976,
#188977,#188978,#188979,#188980,#188981,#188982,#188983,#188984,#188985,
#188986,#188987,#188988,#188989,#188990,#188991,#188992,#188993,#188994,
#188995,#188996,#188997,#188998,#188999,#189000,#189001,#189002,#189003,
#189004,#189005,#189006,#189007,#189008,#189009,#189010,#189011,#189012,
#189013,#189014),.UNSPECIFIED.,.F.,.F.,(4,3,3,3,3,3,3,3,3,3,3,3,3,3,3,3,
3,4),(0.,4.29652152157141E-5,8.44519107528248E-5,0.000123669830864298,0.000159788877357386,
0.000170558847912639,0.000181218775907179,0.000181960046452421,0.000214460062643711,
0.000244755726198599,0.000255838271868953,0.000258503253867588,0.000261084955178765,
0.000289370476647698,0.000301101325502016,0.000321109510663641,0.000331113603244454,
0.000341117695825267),.UNSPECIFIED.);
#4559=B_SPLINE_CURVE_WITH_KNOTS('',3,(#189016,#189017,#189018,#189019,#189020,
#189021,#189022,#189023,#189024,#189025,#189026,#189027,#189028,#189029,
#189030,#189031,#189032,#189033,#189034,#189035,#189036,#189037,#189038,
#189039,#189040,#189041,#189042,#189043,#189044,#189045,#189046,#189047,
#189048,#189049,#189050,#189051,#189052,#189053,#189054,#189055,#189056,
#189057,#189058,#189059,#189060,#189061,#189062,#189063,#189064,#189065,
#189066,#189067),.UNSPECIFIED.,.F.,.F.,(4,3,3,3,3,3,3,3,3,3,3,3,3,3,3,3,
3,4),(0.,4.30706237863024E-5,8.47417087684952E-5,0.000124159989204232,0.000160467076288062,
0.000170998382116688,0.000182414994733777,0.000213747977645863,0.000242415955901826,
0.000256497573175038,0.000259169422895611,0.000261757777312417,0.000289965130404822,
0.000301877270772903,0.000321937017503145,0.000326951954185706,0.000334474359209547,
0.000341996764233388),.UNSPECIFIED.);
#4560=B_SPLINE_CURVE_WITH_KNOTS('',3,(#189068,#189069,#189070,#189071,#189072,
#189073,#189074,#189075,#189076,#189077,#189078,#189079,#189080,#189081,
#189082,#189083,#189084,#189085,#189086,#189087,#189088,#189089,#189090,
#189091,#189092,#189093,#189094,#189095,#189096,#189097,#189098,#189099,
#189100,#189101,#189102,#189103,#189104,#189105,#189106,#189107,#189108,
#189109,#189110,#189111,#189112,#189113,#189114,#189115,#189116,#189117,
#189118,#189119),.UNSPECIFIED.,.F.,.F.,(4,3,3,3,3,3,3,3,3,3,3,3,3,3,3,3,
3,4),(0.,2.58457451673335E-5,4.25394446194833E-5,6.46659869686626E-5,7.57292581432522E-5,
8.12608937305471E-5,8.26438026273708E-5,8.67925293178419E-5,0.000116015624427352,
0.000130188793976763,0.000151886926306223,0.000161963651211264,0.000162735992470954,
0.000173585058635684,0.000212487880460423,0.000255238173509651,0.000301397761141473,
0.000347170117271379),.UNSPECIFIED.);
#4561=B_SPLINE_CURVE_WITH_KNOTS('',3,(#189121,#189122,#189123,#189124,#189125,
#189126,#189127,#189128,#189129,#189130,#189131,#189132,#189133,#189134,
#189135,#189136,#189137,#189138,#189139,#189140,#189141,#189142,#189143,
#189144,#189145,#189146,#189147,#189148,#189149,#189150,#189151,#189152,
#189153,#189154,#189155,#189156,#189157,#189158,#189159,#189160,#189161,
#189162,#189163,#189164,#189165,#189166),.UNSPECIFIED.,.F.,.F.,(4,3,3,3,
3,3,3,3,3,3,3,3,3,3,3,4),(0.,2.57218161990161E-5,4.21568322567036E-5,6.45873314616669E-5,
7.58025810641486E-5,8.14102058653895E-5,8.28121120656997E-5,8.70178306666303E-5,
0.000116081955657631,0.000130526745999942,0.000162394111022068,0.000174035661333253,
0.000213138396958698,0.00025611693543461,0.000302406662857067,0.000348071322666475),
 .UNSPECIFIED.);
#4562=B_SPLINE_CURVE_WITH_KNOTS('',3,(#189167,#189168,#189169,#189170,#189171,
#189172,#189173,#189174,#189175,#189176,#189177,#189178,#189179,#189180,
#189181,#189182,#189183,#189184,#189185,#189186,#189187,#189188,#189189,
#189190,#189191,#189192,#189193,#189194,#189195,#189196,#189197,#189198,
#189199,#189200,#189201,#189202,#189203,#189204,#189205,#189206,#189207,
#189208,#189209,#189210,#189211,#189212,#189213,#189214,#189215,#189216,
#189217,#189218),.UNSPECIFIED.,.F.,.F.,(4,3,3,3,3,3,3,3,3,3,3,3,3,3,3,3,
3,4),(0.,4.29652152166112E-5,8.44519107541718E-5,0.000123669830865709,0.00015978887735854,
0.00017055884791262,0.000181218775907161,0.000181960046452391,0.000214460062643901,
0.000244755726199277,0.000255838271868943,0.000258503253867579,0.000261084955178756,
0.000289370476647179,0.000301101325502011,0.000321109510663639,0.000331113603244453,
0.000341117695825267),.UNSPECIFIED.);
#4563=B_SPLINE_CURVE_WITH_KNOTS('',3,(#189220,#189221,#189222,#189223,#189224,
#189225,#189226,#189227,#189228,#189229,#189230,#189231,#189232,#189233,
#189234,#189235,#189236,#189237,#189238,#189239,#189240,#189241,#189242,
#189243,#189244,#189245,#189246,#189247,#189248,#189249,#189250,#189251,
#189252,#189253,#189254,#189255,#189256,#189257,#189258,#189259,#189260,
#189261,#189262,#189263,#189264,#189265,#189266,#189267,#189268,#189269,
#189270,#189271),.UNSPECIFIED.,.F.,.F.,(4,3,3,3,3,3,3,3,3,3,3,3,3,3,3,3,
3,4),(0.,4.3070623786285E-5,8.47417087683859E-5,0.000124159989203828,0.000160467076287352,
0.000170998382116686,0.000182414994733794,0.00021374797764586,0.000242415955901968,
0.000256497573175035,0.000259169422895608,0.000261757777312414,0.000289965130404094,
0.000301877270772899,0.000321937017503141,0.000326951954185702,0.000334474359209543,
0.000341996764233384),.UNSPECIFIED.);
#4564=B_SPLINE_CURVE_WITH_KNOTS('',3,(#189272,#189273,#189274,#189275,#189276,
#189277,#189278,#189279,#189280,#189281,#189282,#189283,#189284,#189285,
#189286,#189287,#189288,#189289,#189290,#189291,#189292,#189293,#189294,
#189295,#189296,#189297,#189298,#189299,#189300,#189301,#189302,#189303,
#189304,#189305,#189306,#189307,#189308,#189309,#189310,#189311,#189312,
#189313,#189314,#189315,#189316,#189317,#189318,#189319,#189320,#189321,
#189322,#189323),.UNSPECIFIED.,.F.,.F.,(4,3,3,3,3,3,3,3,3,3,3,3,3,3,3,3,
3,4),(0.,2.58457451685046E-5,4.25394446195917E-5,6.46659869687147E-5,7.57292581432762E-5,
8.12608937305569E-5,8.26438026273771E-5,8.67925293178377E-5,0.000116015624427896,
0.000130188793976757,0.000151886926306216,0.000161963651211271,0.000162735992470946,
0.000173585058635675,0.000212487880458822,0.000255238173506331,0.000301397761136081,
0.000347170117271363),.UNSPECIFIED.);
#4565=B_SPLINE_CURVE_WITH_KNOTS('',3,(#189325,#189326,#189327,#189328,#189329,
#189330,#189331,#189332,#189333,#189334,#189335,#189336,#189337,#189338,
#189339,#189340,#189341,#189342,#189343,#189344,#189345,#189346,#189347,
#189348,#189349,#189350,#189351,#189352,#189353,#189354,#189355,#189356,
#189357,#189358,#189359,#189360,#189361,#189362,#189363,#189364,#189365,
#189366,#189367,#189368,#189369,#189370),.UNSPECIFIED.,.F.,.F.,(4,3,3,3,
3,3,3,3,3,3,3,3,3,3,3,4),(0.,2.57218162002362E-5,4.21568322566886E-5,6.45873314616546E-5,
7.58025810641376E-5,8.14102058653791E-5,8.28121120656895E-5,8.70178306666206E-5,
0.000116081955657556,0.000130526745999931,0.000162394111022038,0.000174035661333241,
0.000213138396957546,0.000256116935432267,0.000302406662853359,0.000348071322666503),
 .UNSPECIFIED.);
#4566=B_SPLINE_CURVE_WITH_KNOTS('',3,(#189371,#189372,#189373,#189374,#189375,
#189376,#189377,#189378,#189379,#189380,#189381,#189382,#189383,#189384,
#189385,#189386,#189387,#189388,#189389,#189390,#189391,#189392,#189393,
#189394,#189395,#189396,#189397,#189398,#189399,#189400,#189401,#189402,
#189403,#189404,#189405,#189406,#189407,#189408,#189409,#189410,#189411,
#189412,#189413,#189414,#189415,#189416,#189417,#189418,#189419,#189420,
#189421,#189422),.UNSPECIFIED.,.F.,.F.,(4,3,3,3,3,3,3,3,3,3,3,3,3,3,3,3,
3,4),(0.,4.29652152209911E-5,8.44519107613256E-5,0.000123669830874747,0.00015978887736901,
0.000170558847912628,0.000181218775907169,0.000181960046452397,0.000214460062644086,
0.000244755726200129,0.00025583827186895,0.000258503253867585,0.000261084955178762,
0.000289370476647124,0.000301101325502017,0.000321109510663644,0.000331113603244457,
0.000341117695825271),.UNSPECIFIED.);
#4567=B_SPLINE_CURVE_WITH_KNOTS('',3,(#189424,#189425,#189426,#189427,#189428,
#189429,#189430,#189431,#189432,#189433,#189434,#189435,#189436,#189437,
#189438,#189439,#189440,#189441,#189442,#189443,#189444,#189445,#189446,
#189447,#189448,#189449,#189450,#189451,#189452,#189453,#189454,#189455,
#189456,#189457,#189458,#189459,#189460,#189461,#189462,#189463,#189464,
#189465,#189466,#189467,#189468,#189469,#189470,#189471,#189472,#189473,
#189474,#189475),.UNSPECIFIED.,.F.,.F.,(4,3,3,3,3,3,3,3,3,3,3,3,3,3,3,3,
3,4),(0.,4.3070623786733E-5,8.47417087690687E-5,0.000124159989204553,0.000160467076288069,
0.000170998382116701,0.000182414994733781,0.000213747977645875,0.00024241595590332,
0.000256497573175049,0.000259169422895622,0.000261757777312428,0.000289965130403643,
0.000301877270772912,0.000321937017503154,0.000326951954185715,0.000334474359209555,
0.000341996764233396),.UNSPECIFIED.);
#4568=B_SPLINE_CURVE_WITH_KNOTS('',3,(#189476,#189477,#189478,#189479,#189480,
#189481,#189482,#189483,#189484,#189485,#189486,#189487,#189488,#189489,
#189490,#189491,#189492,#189493,#189494,#189495,#189496,#189497,#189498,
#189499,#189500,#189501,#189502,#189503,#189504,#189505,#189506,#189507,
#189508,#189509,#189510,#189511,#189512,#189513,#189514,#189515,#189516,
#189517,#189518,#189519,#189520,#189521,#189522,#189523,#189524,#189525,
#189526,#189527),.UNSPECIFIED.,.F.,.F.,(4,3,3,3,3,3,3,3,3,3,3,3,3,3,3,3,
3,4),(0.,2.5845745166866E-5,4.25394446195452E-5,6.46659869686944E-5,7.5729258143269E-5,
8.12608937305563E-5,8.26438026273781E-5,8.67925293178436E-5,0.000116015624427498,
0.000130188793976765,0.000151886926306226,0.000161963651211271,0.000162735992470957,
0.000173585058635687,0.000212487880461328,0.000255238173512605,0.000301397761148938,
0.00034717011727138),.UNSPECIFIED.);
#4569=B_SPLINE_CURVE_WITH_KNOTS('',3,(#189529,#189530,#189531,#189532,#189533,
#189534,#189535,#189536,#189537,#189538,#189539,#189540,#189541,#189542,
#189543,#189544,#189545,#189546,#189547,#189548,#189549,#189550,#189551,
#189552,#189553,#189554,#189555,#189556,#189557,#189558,#189559,#189560,
#189561,#189562,#189563,#189564,#189565,#189566,#189567,#189568,#189569,
#189570,#189571,#189572,#189573,#189574),.UNSPECIFIED.,.F.,.F.,(4,3,3,3,
3,3,3,3,3,3,3,3,3,3,3,4),(0.,2.57218161987294E-5,4.21568322567358E-5,6.45873314616753E-5,
7.5802581064145E-5,8.14102058653799E-5,8.28121120656886E-5,8.70178306666148E-5,
0.000116081955659026,0.000130526745999922,0.000162394111022043,0.00017403566133323,
0.000213138396960531,0.000256116935438422,0.000302406662863451,0.000348071322666455),
 .UNSPECIFIED.);
#4570=B_SPLINE_CURVE_WITH_KNOTS('',3,(#189575,#189576,#189577,#189578,#189579,
#189580,#189581,#189582,#189583,#189584,#189585,#189586,#189587,#189588,
#189589,#189590,#189591,#189592,#189593,#189594,#189595,#189596,#189597,
#189598,#189599,#189600,#189601,#189602,#189603,#189604,#189605,#189606,
#189607,#189608,#189609,#189610,#189611,#189612,#189613,#189614,#189615,
#189616,#189617,#189618,#189619,#189620,#189621,#189622,#189623,#189624,
#189625,#189626),.UNSPECIFIED.,.F.,.F.,(4,3,3,3,3,3,3,3,3,3,3,3,3,3,3,3,
3,4),(0.,4.29652152174181E-5,8.44519107551507E-5,0.00012366983086629,0.000159788877358252,
0.000170558847912638,0.000181218775907176,0.000181960046452432,0.000214460062643755,
0.000244755726198294,0.000255838271868943,0.000258503253867577,0.000261084955178754,
0.000289370476647915,0.000301101325502001,0.000321109510663624,0.000331113603244436,
0.000341117695825248),.UNSPECIFIED.);
#4571=B_SPLINE_CURVE_WITH_KNOTS('',3,(#189628,#189629,#189630,#189631,#189632,
#189633,#189634,#189635,#189636,#189637,#189638,#189639,#189640,#189641,
#189642,#189643,#189644,#189645,#189646,#189647,#189648,#189649,#189650,
#189651,#189652,#189653,#189654,#189655,#189656,#189657,#189658,#189659,
#189660,#189661,#189662,#189663,#189664,#189665,#189666,#189667,#189668,
#189669,#189670,#189671,#189672,#189673,#189674,#189675,#189676,#189677,
#189678,#189679),.UNSPECIFIED.,.F.,.F.,(4,3,3,3,3,3,3,3,3,3,3,3,3,3,3,3,
3,4),(0.,4.30706237872049E-5,8.47417087702058E-5,0.000124159989206704,0.000160467076291566,
0.000170998382116693,0.000182414994733776,0.000213747977645866,0.000242415955902374,
0.000256497573175039,0.000259169422895612,0.000261757777312417,0.000289965130404078,
0.000301877270772901,0.000321937017503142,0.000326951954185703,0.000334474359209543,
0.000341996764233384),.UNSPECIFIED.);
#4572=B_SPLINE_CURVE_WITH_KNOTS('',3,(#189680,#189681,#189682,#189683,#189684,
#189685,#189686,#189687,#189688,#189689,#189690,#189691,#189692,#189693,
#189694,#189695,#189696,#189697,#189698,#189699,#189700,#189701,#189702,
#189703,#189704,#189705,#189706,#189707,#189708,#189709,#189710,#189711,
#189712,#189713,#189714,#189715,#189716,#189717,#189718,#189719,#189720,
#189721,#189722,#189723,#189724,#189725,#189726,#189727,#189728,#189729,
#189730,#189731),.UNSPECIFIED.,.F.,.F.,(4,3,3,3,3,3,3,3,3,3,3,3,3,3,3,3,
3,4),(3.46944695195361E-18,2.58457451679455E-5,4.25394446195489E-5,6.46659869686949E-5,
7.57292581432678E-5,8.12608937305543E-5,8.2643802627376E-5,8.67925293178408E-5,
0.000116015624426877,0.000130188793976759,0.000151886926306219,0.000161963651211276,
0.000162735992470949,0.000173585058635678,0.000212487880458077,0.000255238173504525,
0.000301397761132519,0.000347170117271368),.UNSPECIFIED.);
#4573=B_SPLINE_CURVE_WITH_KNOTS('',3,(#189733,#189734,#189735,#189736,#189737,
#189738,#189739,#189740,#189741,#189742,#189743,#189744,#189745,#189746,
#189747,#189748,#189749,#189750,#189751,#189752,#189753,#189754,#189755,
#189756,#189757,#189758,#189759,#189760,#189761,#189762,#189763,#189764,
#189765,#189766,#189767,#189768,#189769,#189770,#189771,#189772,#189773,
#189774,#189775,#189776,#189777,#189778),.UNSPECIFIED.,.F.,.F.,(4,3,3,3,
3,3,3,3,3,3,3,3,3,3,3,4),(3.46944695195361E-18,2.57218162010662E-5,4.21568322569032E-5,
6.45873314617582E-5,7.58025810641856E-5,8.14102058653994E-5,8.28121120657028E-5,
8.70178306666131E-5,0.000116081955659514,0.000130526745999918,0.00016239411102203,
0.000174035661333223,0.000213138396958463,0.000256116935434209,0.000302406662856632,
0.000348071322666446),.UNSPECIFIED.);
#4574=B_SPLINE_CURVE_WITH_KNOTS('',3,(#189779,#189780,#189781,#189782,#189783,
#189784,#189785,#189786,#189787,#189788,#189789,#189790,#189791,#189792,
#189793,#189794,#189795,#189796,#189797,#189798,#189799,#189800,#189801,
#189802,#189803,#189804,#189805,#189806,#189807,#189808,#189809,#189810,
#189811,#189812,#189813,#189814,#189815,#189816,#189817,#189818,#189819,
#189820,#189821,#189822,#189823,#189824,#189825,#189826,#189827,#189828,
#189829,#189830),.UNSPECIFIED.,.F.,.F.,(4,3,3,3,3,3,3,3,3,3,3,3,3,3,3,3,
3,4),(0.,4.2965215219084E-5,8.44519107582157E-5,0.000123669830870834,0.000159788877364523,
0.000170558847912632,0.000181218775907171,0.000181960046452412,0.000214460062643453,
0.000244755726197965,0.000255838271868945,0.000258503253867579,0.000261084955178757,
0.000289370476647428,0.000301101325502007,0.000321109510663632,0.000331113603244445,
0.000341117695825257),.UNSPECIFIED.);
#4575=B_SPLINE_CURVE_WITH_KNOTS('',3,(#189832,#189833,#189834,#189835,#189836,
#189837,#189838,#189839,#189840,#189841,#189842,#189843,#189844,#189845,
#189846,#189847,#189848,#189849,#189850,#189851,#189852,#189853,#189854,
#189855,#189856,#189857,#189858,#189859,#189860,#189861,#189862,#189863,
#189864,#189865,#189866,#189867,#189868,#189869,#189870,#189871,#189872,
#189873,#189874,#189875,#189876,#189877,#189878,#189879,#189880,#189881,
#189882,#189883),.UNSPECIFIED.,.F.,.F.,(4,3,3,3,3,3,3,3,3,3,3,3,3,3,3,3,
3,4),(0.,4.30706237872751E-5,8.47417087704076E-5,0.000124159989207045,0.000160467076291976,
0.000170998382116688,0.000182414994733785,0.000213747977645864,0.000242415955904398,
0.000256497573175039,0.000259169422895612,0.000261757777312418,0.000289965130402912,
0.000301877270772903,0.000321937017503146,0.000326951954185707,0.000334474359209548,
0.000341996764233389),.UNSPECIFIED.);
#4576=B_SPLINE_CURVE_WITH_KNOTS('',3,(#189884,#189885,#189886,#189887,#189888,
#189889,#189890,#189891,#189892,#189893,#189894,#189895,#189896,#189897,
#189898,#189899,#189900,#189901,#189902,#189903,#189904,#189905,#189906,
#189907,#189908,#189909,#189910,#189911,#189912,#189913,#189914,#189915,
#189916,#189917,#189918,#189919,#189920,#189921,#189922,#189923,#189924,
#189925,#189926,#189927,#189928,#189929,#189930,#189931,#189932,#189933,
#189934,#189935),.UNSPECIFIED.,.F.,.F.,(4,3,3,3,3,3,3,3,3,3,3,3,3,3,3,3,
3,4),(0.,2.58457451679569E-5,4.25394446195776E-5,6.46659869687099E-5,7.5729258143276E-5,
8.12608937305591E-5,8.26438026273799E-5,8.67925293178422E-5,0.000116015624427706,
0.000130188793976763,0.000151886926306224,0.000161963651211281,0.000162735992470954,
0.000173585058635684,0.000212487880460481,0.000255238173510222,0.000301397761143518,
0.000347170117271362),.UNSPECIFIED.);
#4577=B_SPLINE_CURVE_WITH_KNOTS('',3,(#189937,#189938,#189939,#189940,#189941,
#189942,#189943,#189944,#189945,#189946,#189947,#189948,#189949,#189950,
#189951,#189952,#189953,#189954,#189955,#189956,#189957,#189958,#189959,
#189960,#189961,#189962,#189963,#189964,#189965,#189966,#189967,#189968,
#189969,#189970,#189971,#189972,#189973,#189974,#189975,#189976,#189977,
#189978,#189979,#189980,#189981,#189982),.UNSPECIFIED.,.F.,.F.,(4,3,3,3,
3,3,3,3,3,3,3,3,3,3,3,4),(0.,2.57218161989729E-5,4.21568322568806E-5,6.45873314617506E-5,
7.58025810641856E-5,8.14102058654031E-5,8.28121120657075E-5,8.70178306666206E-5,
0.000116081955658818,0.000130526745999931,0.000162394111022037,0.000174035661333241,
0.000213138396956396,0.000256116935430151,0.000302406662850685,0.000348071322666478),
 .UNSPECIFIED.);
#4578=B_SPLINE_CURVE_WITH_KNOTS('',3,(#189983,#189984,#189985,#189986,#189987,
#189988,#189989,#189990,#189991,#189992,#189993,#189994,#189995,#189996,
#189997,#189998,#189999,#190000,#190001,#190002,#190003,#190004,#190005,
#190006,#190007,#190008,#190009,#190010,#190011,#190012,#190013,#190014,
#190015,#190016,#190017,#190018,#190019,#190020,#190021,#190022,#190023,
#190024,#190025,#190026,#190027,#190028,#190029,#190030,#190031,#190032,
#190033,#190034),.UNSPECIFIED.,.F.,.F.,(4,3,3,3,3,3,3,3,3,3,3,3,3,3,3,3,
3,4),(0.,4.29652152136548E-5,8.44519107495283E-5,0.000123669830860329,0.000159788877352937,
0.000170558847912617,0.000181218775907158,0.000181960046452403,0.000214460062643498,
0.000244755726198013,0.00025583827186894,0.000258503253867575,0.000261084955178752,
0.000289370476647941,0.000301101325502007,0.000321109510663635,0.000331113603244448,
0.000341117695825262),.UNSPECIFIED.);
#4579=B_SPLINE_CURVE_WITH_KNOTS('',3,(#190036,#190037,#190038,#190039,#190040,
#190041,#190042,#190043,#190044,#190045,#190046,#190047,#190048,#190049,
#190050,#190051,#190052,#190053,#190054,#190055,#190056,#190057,#190058,
#190059,#190060,#190061,#190062,#190063,#190064,#190065,#190066,#190067,
#190068,#190069,#190070,#190071,#190072,#190073,#190074,#190075,#190076,
#190077,#190078,#190079,#190080,#190081,#190082,#190083,#190084,#190085,
#190086,#190087),.UNSPECIFIED.,.F.,.F.,(4,3,3,3,3,3,3,3,3,3,3,3,3,3,3,3,
3,4),(0.,4.30706237876541E-5,8.47417087708983E-5,0.000124159989207408,0.00016046707629211,
0.000170998382116697,0.000182414994733759,0.00021374797764587,0.000242415955902421,
0.000256497573175043,0.000259169422895616,0.000261757777312422,0.000289965130404187,
0.000301877270772906,0.000321937017503147,0.000326951954185708,0.000334474359209549,
0.000341996764233389),.UNSPECIFIED.);
#4580=B_SPLINE_CURVE_WITH_KNOTS('',3,(#190088,#190089,#190090,#190091,#190092,
#190093,#190094,#190095,#190096,#190097,#190098,#190099,#190100,#190101,
#190102,#190103,#190104,#190105,#190106,#190107,#190108,#190109,#190110,
#190111,#190112,#190113,#190114,#190115,#190116,#190117,#190118,#190119,
#190120,#190121,#190122,#190123,#190124,#190125,#190126,#190127,#190128,
#190129,#190130,#190131,#190132,#190133,#190134,#190135,#190136,#190137,
#190138,#190139),.UNSPECIFIED.,.F.,.F.,(4,3,3,3,3,3,3,3,3,3,3,3,3,3,3,3,
3,4),(0.,2.58457451677454E-5,4.25394446195769E-5,6.4665986968705E-5,7.5729258143269E-5,
8.1260893730551E-5,8.26438026273715E-5,8.6792529317833E-5,0.000116015624427558,
0.00013018879397675,0.000151886926306208,0.000161963651211251,0.000162735992470937,
0.000173585058635666,0.000212487880460707,0.00025523817351233,0.00030139776115075,
0.000347170117271366),.UNSPECIFIED.);
#4581=B_SPLINE_CURVE_WITH_KNOTS('',3,(#190141,#190142,#190143,#190144,#190145,
#190146,#190147,#190148,#190149,#190150,#190151,#190152,#190153,#190154,
#190155,#190156,#190157,#190158,#190159,#190160,#190161,#190162,#190163,
#190164,#190165,#190166,#190167,#190168,#190169,#190170,#190171,#190172,
#190173,#190174,#190175,#190176,#190177,#190178,#190179,#190180,#190181,
#190182,#190183,#190184,#190185,#190186),.UNSPECIFIED.,.F.,.F.,(4,3,3,3,
3,3,3,3,3,3,3,3,3,3,3,4),(0.,2.57218162002616E-5,4.21568322567789E-5,6.45873314616992E-5,
7.58025810641594E-5,8.14102058653895E-5,8.2812112065697E-5,8.70178306666196E-5,
0.000116081955657916,0.000130526745999929,0.000162394111022025,0.000174035661333239,
0.000213138396954118,0.000256116935425588,0.000302406662843531,0.000348071322666471),
 .UNSPECIFIED.);
#4582=B_SPLINE_CURVE_WITH_KNOTS('',3,(#190187,#190188,#190189,#190190,#190191,
#190192,#190193,#190194,#190195,#190196,#190197,#190198,#190199,#190200,
#190201,#190202,#190203,#190204,#190205,#190206,#190207,#190208,#190209,
#190210,#190211,#190212,#190213,#190214,#190215,#190216,#190217,#190218,
#190219,#190220,#190221,#190222,#190223,#190224,#190225,#190226,#190227,
#190228,#190229,#190230,#190231,#190232,#190233,#190234,#190235,#190236,
#190237,#190238),.UNSPECIFIED.,.F.,.F.,(4,3,3,3,3,3,3,3,3,3,3,3,3,3,3,3,
3,4),(0.,4.29652152132578E-5,8.44519107492023E-5,0.000123669830860594,0.000159788877354395,
0.000170558847912621,0.00018121877590716,0.000181960046452396,0.000214460062643361,
0.000244755726197735,0.000255838271868937,0.000258503253867572,0.00026108495517875,
0.00028937047664799,0.000301101325502002,0.000321109510663628,0.000331113603244441,
0.000341117695825254),.UNSPECIFIED.);
#4583=B_SPLINE_CURVE_WITH_KNOTS('',3,(#190240,#190241,#190242,#190243,#190244,
#190245,#190246,#190247,#190248,#190249,#190250,#190251,#190252,#190253,
#190254,#190255,#190256,#190257,#190258,#190259,#190260,#190261,#190262,
#190263,#190264,#190265,#190266,#190267,#190268,#190269,#190270,#190271,
#190272,#190273,#190274,#190275,#190276,#190277,#190278,#190279,#190280,
#190281,#190282,#190283,#190284,#190285,#190286,#190287,#190288,#190289,
#190290,#190291),.UNSPECIFIED.,.F.,.F.,(4,3,3,3,3,3,3,3,3,3,3,3,3,3,3,3,
3,4),(0.,4.30706237885874E-5,8.47417087727397E-5,0.000124159989210242,0.000160467076296224,
0.000170998382116709,0.000182414994733818,0.000213747977645879,0.000242415955903209,
0.000256497573175049,0.000259169422895622,0.000261757777312427,0.00028996513040331,
0.000301877270772908,0.000321937017503148,0.000326951954185708,0.000334474359209549,
0.000341996764233389),.UNSPECIFIED.);
#4584=B_SPLINE_CURVE_WITH_KNOTS('',3,(#190292,#190293,#190294,#190295,#190296,
#190297,#190298,#190299,#190300,#190301,#190302,#190303,#190304,#190305,
#190306,#190307,#190308,#190309,#190310,#190311,#190312,#190313,#190314,
#190315,#190316,#190317,#190318,#190319,#190320,#190321,#190322,#190323,
#190324,#190325,#190326,#190327,#190328,#190329,#190330,#190331,#190332,
#190333,#190334,#190335,#190336,#190337,#190338,#190339,#190340,#190341,
#190342,#190343),.UNSPECIFIED.,.F.,.F.,(4,3,3,3,3,3,3,3,3,3,3,3,3,3,3,3,
3,4),(0.,2.58457451690894E-5,4.25394446196487E-5,6.46659869687494E-5,7.57292581432998E-5,
8.1260893730575E-5,8.26438026273938E-5,8.67925293178501E-5,0.000116015624428787,
0.000130188793976775,0.000151886926306238,0.000161963651211307,0.000162735992470969,
0.0001735850586357,0.000212487880461016,0.000255238173513134,0.00030139776115256,
0.000347170117271371),.UNSPECIFIED.);
#4585=B_SPLINE_CURVE_WITH_KNOTS('',3,(#190345,#190346,#190347,#190348,#190349,
#190350,#190351,#190352,#190353,#190354,#190355,#190356,#190357,#190358,
#190359,#190360,#190361,#190362,#190363,#190364,#190365,#190366,#190367,
#190368,#190369,#190370,#190371,#190372,#190373,#190374,#190375,#190376,
#190377,#190378,#190379,#190380,#190381,#190382,#190383,#190384,#190385,
#190386,#190387,#190388,#190389,#190390),.UNSPECIFIED.,.F.,.F.,(4,3,3,3,
3,3,3,3,3,3,3,3,3,3,3,4),(0.,2.57218161979397E-5,4.21568322566978E-5,6.45873314616655E-5,
7.58025810641494E-5,8.14102058653913E-5,8.28121120657018E-5,8.70178306666332E-5,
0.000116081955659105,0.00013052674599995,0.000162394111022055,0.000174035661333266,
0.000213138396958747,0.000256116935434786,0.000302406662857728,0.0003480713226665),
 .UNSPECIFIED.);
#4586=B_SPLINE_CURVE_WITH_KNOTS('',3,(#190391,#190392,#190393,#190394,#190395,
#190396,#190397,#190398,#190399,#190400,#190401,#190402,#190403,#190404,
#190405,#190406,#190407,#190408,#190409,#190410,#190411,#190412,#190413,
#190414,#190415,#190416,#190417,#190418,#190419,#190420,#190421,#190422,
#190423,#190424,#190425,#190426,#190427,#190428,#190429,#190430,#190431,
#190432,#190433,#190434,#190435,#190436,#190437,#190438,#190439,#190440,
#190441,#190442),.UNSPECIFIED.,.F.,.F.,(4,3,3,3,3,3,3,3,3,3,3,3,3,3,3,3,
3,4),(0.,4.29652152110204E-5,8.44519107444466E-5,0.00012366983085245,0.000159788877341661,
0.000170558847912638,0.000181218775907178,0.000181960046452416,0.000214460062642894,
0.00024475572619666,0.000255838271868955,0.00025850325386759,0.000261084955178768,
0.000289370476650761,0.00030110132550202,0.000321109510663647,0.00033111360324446,
0.000341117695825273),.UNSPECIFIED.);
#4587=B_SPLINE_CURVE_WITH_KNOTS('',3,(#190444,#190445,#190446,#190447,#190448,
#190449,#190450,#190451,#190452,#190453,#190454,#190455,#190456,#190457,
#190458,#190459,#190460,#190461,#190462,#190463,#190464,#190465,#190466,
#190467,#190468,#190469,#190470,#190471,#190472,#190473,#190474,#190475,
#190476,#190477,#190478,#190479,#190480,#190481,#190482,#190483,#190484,
#190485,#190486,#190487,#190488,#190489,#190490,#190491,#190492,#190493,
#190494,#190495),.UNSPECIFIED.,.F.,.F.,(4,3,3,3,3,3,3,3,3,3,3,3,3,3,3,3,
3,4),(0.,4.30706237889129E-5,8.47417087731407E-5,0.000124159989210559,0.000160467076296243,
0.000170998382116688,0.00018241499473377,0.000213747977645864,0.000242415955903622,
0.000256497573175039,0.000259169422895612,0.000261757777312418,0.000289965130404044,
0.000301877270772903,0.000321937017503146,0.000326951954185707,0.000334474359209548,
0.000341996764233389),.UNSPECIFIED.);
#4588=B_SPLINE_CURVE_WITH_KNOTS('',3,(#190496,#190497,#190498,#190499,#190500,
#190501,#190502,#190503,#190504,#190505,#190506,#190507,#190508,#190509,
#190510,#190511,#190512,#190513,#190514,#190515,#190516,#190517,#190518,
#190519,#190520,#190521,#190522,#190523,#190524,#190525,#190526,#190527,
#190528,#190529,#190530,#190531,#190532,#190533,#190534,#190535,#190536,
#190537,#190538,#190539,#190540,#190541,#190542,#190543,#190544,#190545,
#190546,#190547),.UNSPECIFIED.,.F.,.F.,(4,3,3,3,3,3,3,3,3,3,3,3,3,3,3,3,
3,4),(0.,2.58457451665418E-5,4.25394446196923E-5,6.46659869687673E-5,7.57292581433048E-5,
8.12608937305736E-5,8.26438026273908E-5,8.67925293178423E-5,0.000116015624427747,
0.000130188793976764,0.000151886926306224,0.000161963651211288,0.000162735992470954,
0.000173585058635685,0.000212487880459422,0.000255238173507843,0.00030139776113927,
0.000347170117271382),.UNSPECIFIED.);
#4589=B_SPLINE_CURVE_WITH_KNOTS('',3,(#190549,#190550,#190551,#190552,#190553,
#190554,#190555,#190556,#190557,#190558,#190559,#190560,#190561,#190562,
#190563,#190564,#190565,#190566,#190567,#190568,#190569,#190570,#190571,
#190572,#190573,#190574,#190575,#190576,#190577,#190578,#190579,#190580,
#190581,#190582,#190583,#190584,#190585,#190586,#190587,#190588,#190589,
#190590,#190591,#190592,#190593,#190594),.UNSPECIFIED.,.F.,.F.,(4,3,3,3,
3,3,3,3,3,3,3,3,3,3,3,4),(0.,2.57218161992769E-5,4.21568322568503E-5,6.45873314617301E-5,
7.58025810641699E-5,8.14102058653899E-5,8.28121120656949E-5,8.70178306666098E-5,
0.000116081955658396,0.000130526745999915,0.00016239411102202,0.00017403566133322,
0.00021313839696102,0.000256116935439445,0.000302406662865238,0.000348071322666453),
 .UNSPECIFIED.);
#4590=B_SPLINE_CURVE_WITH_KNOTS('',3,(#190595,#190596,#190597,#190598,#190599,
#190600,#190601,#190602,#190603,#190604,#190605,#190606,#190607,#190608,
#190609,#190610,#190611,#190612,#190613,#190614,#190615,#190616,#190617,
#190618,#190619,#190620,#190621,#190622,#190623,#190624,#190625,#190626,
#190627,#190628,#190629,#190630,#190631,#190632,#190633,#190634,#190635,
#190636,#190637,#190638,#190639,#190640,#190641,#190642,#190643,#190644,
#190645,#190646),.UNSPECIFIED.,.F.,.F.,(4,3,3,3,3,3,3,3,3,3,3,3,3,3,3,3,
3,4),(0.,4.29652152249339E-5,8.44519107677232E-5,0.000123669830882601,0.000159788877377764,
0.000170558847912626,0.000181218775907166,0.000181960046452394,0.000214460062643825,
0.000244755726198773,0.000255838271868946,0.000258503253867581,0.000261084955178759,
0.000289370476647345,0.000301101325502013,0.000321109510663639,0.000331113603244453,
0.000341117695825266),.UNSPECIFIED.);
#4591=B_SPLINE_CURVE_WITH_KNOTS('',3,(#190648,#190649,#190650,#190651,#190652,
#190653,#190654,#190655,#190656,#190657,#190658,#190659,#190660,#190661,
#190662,#190663,#190664,#190665,#190666,#190667,#190668,#190669,#190670,
#190671,#190672,#190673,#190674,#190675,#190676,#190677,#190678,#190679,
#190680,#190681,#190682,#190683,#190684,#190685,#190686,#190687,#190688,
#190689,#190690,#190691,#190692,#190693,#190694,#190695,#190696,#190697,
#190698,#190699),.UNSPECIFIED.,.F.,.F.,(4,3,3,3,3,3,3,3,3,3,3,3,3,3,3,3,
3,4),(0.,4.30706237852771E-5,8.47417087665961E-5,0.000124159989201271,0.000160467076283982,
0.000170998382116692,0.000182414994733772,0.000213747977645867,0.000242415955903141,
0.000256497573175042,0.000259169422895616,0.000261757777312421,0.000289965130404113,
0.000301877270772907,0.000321937017503149,0.00032695195418571,0.000334474359209551,
0.000341996764233392),.UNSPECIFIED.);
#4592=B_SPLINE_CURVE_WITH_KNOTS('',3,(#190700,#190701,#190702,#190703,#190704,
#190705,#190706,#190707,#190708,#190709,#190710,#190711,#190712,#190713,
#190714,#190715,#190716,#190717,#190718,#190719,#190720,#190721,#190722,
#190723,#190724,#190725,#190726,#190727,#190728,#190729,#190730,#190731,
#190732,#190733,#190734,#190735,#190736,#190737,#190738,#190739,#190740,
#190741,#190742,#190743,#190744,#190745,#190746,#190747,#190748,#190749,
#190750,#190751),.UNSPECIFIED.,.F.,.F.,(4,3,3,3,3,3,3,3,3,3,3,3,3,3,3,3,
3,4),(0.,2.58457451676215E-5,4.25394446194861E-5,6.46659869686614E-5,7.5729258143249E-5,
8.12608937305428E-5,8.26438026273662E-5,8.67925293178366E-5,0.000116015624427751,
0.000130188793976755,0.000151886926306214,0.000161963651211277,0.000162735992470944,
0.000173585058635673,0.000212487880461416,0.00025523817351186,0.000301397761145538,
0.000347170117271364),.UNSPECIFIED.);
#4593=B_SPLINE_CURVE_WITH_KNOTS('',3,(#190753,#190754,#190755,#190756,#190757,
#190758,#190759,#190760,#190761,#190762,#190763,#190764,#190765,#190766,
#190767,#190768,#190769,#190770,#190771,#190772,#190773,#190774,#190775,
#190776,#190777,#190778,#190779,#190780,#190781,#190782,#190783,#190784,
#190785,#190786,#190787,#190788,#190789,#190790,#190791,#190792,#190793,
#190794,#190795,#190796,#190797,#190798),.UNSPECIFIED.,.F.,.F.,(4,3,3,3,
3,3,3,3,3,3,3,3,3,3,3,4),(0.,2.5721816201431E-5,4.2156832256571E-5,6.45873314615971E-5,
7.58025810641102E-5,8.14102058653667E-5,8.28121120656809E-5,8.70178306666232E-5,
0.000116081955658063,0.000130526745999935,0.000162394111022062,0.000174035661333246,
0.000213138396959622,0.000256116935436423,0.000302406662859842,0.00034807132266648),
 .UNSPECIFIED.);
#4594=B_SPLINE_CURVE_WITH_KNOTS('',3,(#190799,#190800,#190801,#190802,#190803,
#190804,#190805,#190806,#190807,#190808,#190809,#190810,#190811,#190812,
#190813,#190814,#190815,#190816,#190817,#190818,#190819,#190820,#190821,
#190822,#190823,#190824,#190825,#190826,#190827,#190828,#190829,#190830,
#190831,#190832,#190833,#190834,#190835,#190836,#190837,#190838,#190839,
#190840,#190841,#190842,#190843,#190844,#190845,#190846,#190847,#190848,
#190849,#190850),.UNSPECIFIED.,.F.,.F.,(4,3,3,3,3,3,3,3,3,3,3,3,3,3,3,3,
3,4),(0.,4.29652152174073E-5,8.44519107557636E-5,0.000123669830868272,0.000159788877362364,
0.000170558847912617,0.000181218775907158,0.000181960046452397,0.000214460062643918,
0.00024475572619964,0.00025583827186894,0.000258503253867575,0.000261084955178753,
0.000289370476646583,0.000301101325502008,0.000321109510663635,0.000331113603244449,
0.000341117695825263),.UNSPECIFIED.);
#4595=B_SPLINE_CURVE_WITH_KNOTS('',3,(#190852,#190853,#190854,#190855,#190856,
#190857,#190858,#190859,#190860,#190861,#190862,#190863,#190864,#190865,
#190866,#190867,#190868,#190869,#190870,#190871,#190872,#190873,#190874,
#190875,#190876,#190877,#190878,#190879,#190880,#190881,#190882,#190883,
#190884,#190885,#190886,#190887,#190888,#190889,#190890,#190891,#190892,
#190893,#190894,#190895,#190896,#190897,#190898,#190899,#190900,#190901,
#190902,#190903),.UNSPECIFIED.,.F.,.F.,(4,3,3,3,3,3,3,3,3,3,3,3,3,3,3,3,
3,4),(0.,4.30706237853522E-5,8.47417087667565E-5,0.000124159989201577,0.000160467076284533,
0.000170998382116685,0.000182414994733785,0.000213747977645861,0.000242415955903341,
0.000256497573175037,0.000259169422895611,0.000261757777312416,0.000289965130402767,
0.000301877270772903,0.000321937017503146,0.000326951954185707,0.000334474359209548,
0.00034199676423339),.UNSPECIFIED.);
#4596=B_SPLINE_CURVE_WITH_KNOTS('',3,(#190904,#190905,#190906,#190907,#190908,
#190909,#190910,#190911,#190912,#190913,#190914,#190915,#190916,#190917,
#190918,#190919,#190920,#190921,#190922,#190923,#190924,#190925,#190926,
#190927,#190928,#190929,#190930,#190931,#190932,#190933,#190934,#190935,
#190936,#190937,#190938,#190939,#190940,#190941,#190942,#190943,#190944,
#190945,#190946,#190947,#190948,#190949,#190950,#190951,#190952,#190953,
#190954,#190955),.UNSPECIFIED.,.F.,.F.,(4,3,3,3,3,3,3,3,3,3,3,3,3,3,3,3,
3,4),(0.,2.58457451685608E-5,4.25394446196307E-5,6.46659869687341E-5,7.57292581432858E-5,
8.12608937305616E-5,8.26438026273806E-5,8.67925293178375E-5,0.00011601562442651,
0.000130188793976756,0.000151886926306216,0.000161963651211271,0.000162735992470945,
0.000173585058635675,0.000212487880459305,0.00025523817350915,0.000301397761144963,
0.000347170117271364),.UNSPECIFIED.);
#4597=B_SPLINE_CURVE_WITH_KNOTS('',3,(#190957,#190958,#190959,#190960,#190961,
#190962,#190963,#190964,#190965,#190966,#190967,#190968,#190969,#190970,
#190971,#190972,#190973,#190974,#190975,#190976,#190977,#190978,#190979,
#190980,#190981,#190982,#190983,#190984,#190985,#190986,#190987,#190988,
#190989,#190990,#190991,#190992,#190993,#190994,#190995,#190996,#190997,
#190998,#190999,#191000,#191001,#191002),.UNSPECIFIED.,.F.,.F.,(4,3,3,3,
3,3,3,3,3,3,3,3,3,3,3,4),(0.,2.57218161988706E-5,4.21568322567235E-5,6.45873314616673E-5,
7.58025810641392E-5,8.14102058653752E-5,8.28121120656842E-5,8.70178306666111E-5,
0.00011608195565852,0.000130526745999917,0.000162394111022032,0.000174035661333222,
0.00021313839695844,0.000256116935434141,0.00030240666285643,0.000348071322666455),
 .UNSPECIFIED.);
#4598=B_SPLINE_CURVE_WITH_KNOTS('',3,(#191003,#191004,#191005,#191006,#191007,
#191008,#191009,#191010,#191011,#191012,#191013,#191014,#191015,#191016,
#191017,#191018,#191019,#191020,#191021,#191022,#191023,#191024,#191025,
#191026,#191027,#191028,#191029,#191030,#191031,#191032,#191033,#191034,
#191035,#191036,#191037,#191038,#191039,#191040,#191041,#191042,#191043,
#191044,#191045,#191046,#191047,#191048,#191049,#191050,#191051,#191052,
#191053,#191054),.UNSPECIFIED.,.F.,.F.,(4,3,3,3,3,3,3,3,3,3,3,3,3,3,3,3,
3,4),(0.,4.29652152136145E-5,8.44519107492294E-5,0.000123669830859522,0.000159788877351505,
0.000170558847912633,0.000181218775907172,0.000181960046452411,0.000214460062643391,
0.000244755726198025,0.000255838271868944,0.000258503253867578,0.000261084955178756,
0.000289370476648214,0.000301101325502005,0.000321109510663629,0.000331113603244442,
0.000341117695825254),.UNSPECIFIED.);
#4599=B_SPLINE_CURVE_WITH_KNOTS('',3,(#191056,#191057,#191058,#191059,#191060,
#191061,#191062,#191063,#191064,#191065,#191066,#191067,#191068,#191069,
#191070,#191071,#191072,#191073,#191074,#191075,#191076,#191077,#191078,
#191079,#191080,#191081,#191082,#191083,#191084,#191085,#191086,#191087,
#191088,#191089,#191090,#191091,#191092,#191093,#191094,#191095,#191096,
#191097,#191098,#191099,#191100,#191101,#191102,#191103,#191104,#191105,
#191106,#191107),.UNSPECIFIED.,.F.,.F.,(4,3,3,3,3,3,3,3,3,3,3,3,3,3,3,3,
3,4),(0.,4.3070623786896E-5,8.47417087695961E-5,0.000124159989205574,0.000160467076289785,
0.000170998382116694,0.00018241499473378,0.000213747977645867,0.000242415955902538,
0.000256497573175039,0.000259169422895613,0.000261757777312418,0.000289965130402436,
0.000301877270772901,0.000321937017503143,0.000326951954185703,0.000334474359209544,
0.000341996764233384),.UNSPECIFIED.);
#4600=B_SPLINE_CURVE_WITH_KNOTS('',3,(#191108,#191109,#191110,#191111,#191112,
#191113,#191114,#191115,#191116,#191117,#191118,#191119,#191120,#191121,
#191122,#191123,#191124,#191125,#191126,#191127,#191128,#191129,#191130,
#191131,#191132,#191133,#191134,#191135,#191136,#191137,#191138,#191139,
#191140,#191141,#191142,#191143,#191144,#191145,#191146,#191147,#191148,
#191149,#191150,#191151,#191152,#191153,#191154,#191155,#191156,#191157,
#191158,#191159),.UNSPECIFIED.,.F.,.F.,(4,3,3,3,3,3,3,3,3,3,3,3,3,3,3,3,
3,4),(0.,2.58457451667925E-5,4.25394446195448E-5,6.46659869686894E-5,7.57292581432617E-5,
8.12608937305479E-5,8.26438026273694E-5,8.6792529317834E-5,0.000116015624426846,
0.000130188793976751,0.00015188692630621,0.000161963651211258,0.000162735992470939,
0.000173585058635668,0.000212487880462275,0.000255238173515101,0.000301397761154326,
0.000347170117271365),.UNSPECIFIED.);
#4601=B_SPLINE_CURVE_WITH_KNOTS('',3,(#191161,#191162,#191163,#191164,#191165,
#191166,#191167,#191168,#191169,#191170,#191171,#191172,#191173,#191174,
#191175,#191176,#191177,#191178,#191179,#191180,#191181,#191182,#191183,
#191184,#191185,#191186,#191187,#191188,#191189,#191190,#191191,#191192,
#191193,#191194,#191195,#191196,#191197,#191198,#191199,#191200,#191201,
#191202,#191203,#191204,#191205,#191206),.UNSPECIFIED.,.F.,.F.,(4,3,3,3,
3,3,3,3,3,3,3,3,3,3,3,4),(0.,2.57218161986573E-5,4.21568322566464E-5,6.45873314616308E-5,
7.5802581064123E-5,8.14102058653691E-5,8.28121120656806E-5,8.70178306666152E-5,
0.00011608195565807,0.000130526745999923,0.000162394111022048,0.00017403566133323,
0.000213138396960761,0.000256116935438828,0.000302406662863967,0.000348071322666457),
 .UNSPECIFIED.);
#4602=B_SPLINE_CURVE_WITH_KNOTS('',3,(#191207,#191208,#191209,#191210,#191211,
#191212,#191213,#191214,#191215,#191216,#191217,#191218,#191219,#191220,
#191221,#191222,#191223,#191224,#191225,#191226,#191227,#191228,#191229,
#191230,#191231,#191232,#191233,#191234,#191235,#191236,#191237,#191238,
#191239,#191240,#191241,#191242,#191243,#191244,#191245,#191246,#191247,
#191248,#191249,#191250,#191251,#191252,#191253,#191254,#191255,#191256,
#191257,#191258),.UNSPECIFIED.,.F.,.F.,(4,3,3,3,3,3,3,3,3,3,3,3,3,3,3,3,
3,4),(0.,4.296521522581E-5,8.44519107689155E-5,0.000123669830883573,0.000159788877378198,
0.000170558847912618,0.000181218775907158,0.000181960046452403,0.000214460062644037,
0.000244755726199692,0.000255838271868937,0.000258503253867572,0.00026108495517875,
0.000289370476646679,0.000301101325502003,0.00032110951066363,0.000331113603244443,
0.000341117695825257),.UNSPECIFIED.);
#4603=B_SPLINE_CURVE_WITH_KNOTS('',3,(#191260,#191261,#191262,#191263,#191264,
#191265,#191266,#191267,#191268,#191269,#191270,#191271,#191272,#191273,
#191274,#191275,#191276,#191277,#191278,#191279,#191280,#191281,#191282,
#191283,#191284,#191285,#191286,#191287,#191288,#191289,#191290,#191291,
#191292,#191293,#191294,#191295,#191296,#191297,#191298,#191299,#191300,
#191301,#191302,#191303,#191304,#191305,#191306,#191307,#191308,#191309,
#191310,#191311),.UNSPECIFIED.,.F.,.F.,(4,3,3,3,3,3,3,3,3,3,3,3,3,3,3,3,
3,4),(2.23960286815172E-17,4.30706237876585E-5,8.47417087709534E-5,0.000124159989207585,
0.00016046707629245,0.000170998382116699,0.000182414994733791,0.000213747977645874,
0.000242415955903611,0.000256497573175049,0.000259169422895623,0.000261757777312428,
0.000289965130403366,0.000301877270772914,0.000321937017503157,0.000326951954185718,
0.000334474359209559,0.0003419967642334),.UNSPECIFIED.);
#4604=B_SPLINE_CURVE_WITH_KNOTS('',3,(#191312,#191313,#191314,#191315,#191316,
#191317,#191318,#191319,#191320,#191321,#191322,#191323,#191324,#191325,
#191326,#191327,#191328,#191329,#191330,#191331,#191332,#191333,#191334,
#191335,#191336,#191337,#191338,#191339,#191340,#191341,#191342,#191343,
#191344,#191345,#191346,#191347,#191348,#191349,#191350,#191351,#191352,
#191353,#191354,#191355,#191356,#191357,#191358,#191359,#191360,#191361,
#191362,#191363),.UNSPECIFIED.,.F.,.F.,(4,3,3,3,3,3,3,3,3,3,3,3,3,3,3,3,
3,4),(0.,2.58457451680856E-5,4.25394446195527E-5,6.46659869687014E-5,7.57292581432757E-5,
8.12608937305629E-5,8.26438026273847E-5,8.67925293178501E-5,0.000116015624427437,
0.000130188793976775,0.000151886926306238,0.000161963651211304,0.000162735992470969,
0.0001735850586357,0.000212487880459721,0.000255238173510426,0.000301397761147914,
0.000347170117271371),.UNSPECIFIED.);
#4605=B_SPLINE_CURVE_WITH_KNOTS('',3,(#191365,#191366,#191367,#191368,#191369,
#191370,#191371,#191372,#191373,#191374,#191375,#191376,#191377,#191378,
#191379,#191380,#191381,#191382,#191383,#191384,#191385,#191386,#191387,
#191388,#191389,#191390,#191391,#191392,#191393,#191394,#191395,#191396,
#191397,#191398,#191399,#191400,#191401,#191402,#191403,#191404,#191405,
#191406,#191407,#191408,#191409,#191410),.UNSPECIFIED.,.F.,.F.,(4,3,3,3,
3,3,3,3,3,3,3,3,3,3,3,4),(3.46944695195361E-18,2.57218162016344E-5,4.21568322567852E-5,
6.45873314617071E-5,7.58025810641681E-5,8.14102058653986E-5,8.28121120657062E-5,
8.70178306666291E-5,0.000116081955658797,0.000130526745999942,0.000162394111022068,
0.000174035661333255,0.000213138396959518,0.000256116935436304,0.000302406662860053,
0.000348071322666477),.UNSPECIFIED.);
#4606=B_SPLINE_CURVE_WITH_KNOTS('',3,(#191411,#191412,#191413,#191414,#191415,
#191416,#191417,#191418,#191419,#191420,#191421,#191422,#191423,#191424,
#191425,#191426,#191427,#191428,#191429,#191430,#191431,#191432,#191433,
#191434,#191435,#191436,#191437,#191438,#191439,#191440,#191441,#191442,
#191443,#191444,#191445,#191446,#191447,#191448,#191449,#191450,#191451,
#191452,#191453,#191454,#191455,#191456,#191457,#191458,#191459,#191460,
#191461,#191462),.UNSPECIFIED.,.F.,.F.,(4,3,3,3,3,3,3,3,3,3,3,3,3,3,3,3,
3,4),(0.,4.2965215215576E-5,8.44519107527791E-5,0.000123669830864603,0.00015978887735827,
0.000170558847912638,0.000181218775907178,0.000181960046452423,0.00021446006264388,
0.000244755726199131,0.000255838271868956,0.000258503253867591,0.000261084955178768,
0.000289370476647343,0.000301101325502021,0.000321109510663647,0.00033111360324446,
0.000341117695825273),.UNSPECIFIED.);
#4607=B_SPLINE_CURVE_WITH_KNOTS('',3,(#191464,#191465,#191466,#191467,#191468,
#191469,#191470,#191471,#191472,#191473,#191474,#191475,#191476,#191477,
#191478,#191479,#191480,#191481,#191482,#191483,#191484,#191485,#191486,
#191487,#191488,#191489,#191490,#191491,#191492,#191493,#191494,#191495,
#191496,#191497,#191498,#191499,#191500,#191501,#191502,#191503,#191504,
#191505,#191506,#191507,#191508,#191509,#191510,#191511,#191512,#191513,
#191514,#191515),.UNSPECIFIED.,.F.,.F.,(4,3,3,3,3,3,3,3,3,3,3,3,3,3,3,3,
3,4),(0.,4.30706237881386E-5,8.47417087717555E-5,0.000124159989208601,0.000160467076293699,
0.000170998382116686,0.000182414994733776,0.000213747977645861,0.000242415955903616,
0.000256497573175037,0.00025916942289561,0.000261757777312415,0.000289965130402526,
0.000301877270772901,0.000321937017503144,0.000326951954185705,0.000334474359209546,
0.000341996764233387),.UNSPECIFIED.);
#4608=B_SPLINE_CURVE_WITH_KNOTS('',3,(#191516,#191517,#191518,#191519,#191520,
#191521,#191522,#191523,#191524,#191525,#191526,#191527,#191528,#191529,
#191530,#191531,#191532,#191533,#191534,#191535,#191536,#191537,#191538,
#191539,#191540,#191541,#191542,#191543,#191544,#191545,#191546,#191547,
#191548,#191549,#191550,#191551,#191552,#191553,#191554,#191555,#191556,
#191557,#191558,#191559,#191560,#191561,#191562,#191563,#191564,#191565,
#191566,#191567),.UNSPECIFIED.,.F.,.F.,(4,3,3,3,3,3,3,3,3,3,3,3,3,3,3,3,
3,4),(0.,2.584574516724E-5,4.25394446196669E-5,6.46659869687501E-5,7.57292581432917E-5,
8.12608937305625E-5,8.26438026273802E-5,8.67925293178333E-5,0.000116015624427194,
0.00013018879397675,0.000151886926306208,0.000161963651211274,0.000162735992470937,
0.000173585058635667,0.000212487880460265,0.000255238173511465,0.000301397761149537,
0.00034717011727135),.UNSPECIFIED.);
#4609=B_SPLINE_CURVE_WITH_KNOTS('',3,(#191569,#191570,#191571,#191572,#191573,
#191574,#191575,#191576,#191577,#191578,#191579,#191580,#191581,#191582,
#191583,#191584,#191585,#191586,#191587,#191588,#191589,#191590,#191591,
#191592,#191593,#191594,#191595,#191596,#191597,#191598,#191599,#191600,
#191601,#191602,#191603,#191604,#191605,#191606,#191607,#191608,#191609,
#191610,#191611,#191612,#191613,#191614),.UNSPECIFIED.,.F.,.F.,(4,3,3,3,
3,3,3,3,3,3,3,3,3,3,3,4),(1.73472347597681E-18,2.57218162000535E-5,4.21568322566752E-5,
6.45873314616487E-5,7.58025810641355E-5,8.14102058653789E-5,8.28121120656897E-5,
8.70178306666222E-5,0.000116081955659069,0.000130526745999932,0.000162394111022052,
0.000174035661333243,0.000213138396958092,0.000256116935433535,0.000302406662855884,
0.000348071322666481),.UNSPECIFIED.);
#4610=B_SPLINE_CURVE_WITH_KNOTS('',3,(#191615,#191616,#191617,#191618,#191619,
#191620,#191621,#191622,#191623,#191624,#191625,#191626,#191627,#191628,
#191629,#191630,#191631,#191632,#191633,#191634,#191635,#191636,#191637,
#191638,#191639,#191640,#191641,#191642,#191643,#191644,#191645,#191646,
#191647,#191648,#191649,#191650,#191651,#191652,#191653,#191654,#191655,
#191656,#191657,#191658,#191659,#191660,#191661,#191662,#191663,#191664,
#191665,#191666),.UNSPECIFIED.,.F.,.F.,(4,3,3,3,3,3,3,3,3,3,3,3,3,3,3,3,
3,4),(0.,4.29652152124446E-5,8.44519107478593E-5,0.000123669830858857,0.000159788877352283,
0.000170558847912616,0.000181218775907156,0.000181960046452394,0.000214460062644285,
0.000244755726200151,0.000255838271868935,0.00025850325386757,0.000261084955178748,
0.000289370476646895,0.000301101325502001,0.000321109510663628,0.000331113603244441,
0.000341117695825255),.UNSPECIFIED.);
#4611=B_SPLINE_CURVE_WITH_KNOTS('',3,(#191668,#191669,#191670,#191671,#191672,
#191673,#191674,#191675,#191676,#191677,#191678,#191679,#191680,#191681,
#191682,#191683,#191684,#191685,#191686,#191687,#191688,#191689,#191690,
#191691,#191692,#191693,#191694,#191695,#191696,#191697,#191698,#191699,
#191700,#191701,#191702,#191703,#191704,#191705,#191706,#191707,#191708,
#191709,#191710,#191711,#191712,#191713,#191714,#191715,#191716,#191717,
#191718,#191719),.UNSPECIFIED.,.F.,.F.,(4,3,3,3,3,3,3,3,3,3,3,3,3,3,3,3,
3,4),(0.,4.3070623786735E-5,8.47417087692355E-5,0.000124159989205176,0.00016046707628918,
0.000170998382116699,0.000182414994733791,0.000213747977645873,0.000242415955904601,
0.000256497573175047,0.00025916942289562,0.000261757777312426,0.000289965130402128,
0.000301877270772907,0.000321937017503148,0.000326951954185708,0.000334474359209548,
0.000341996764233388),.UNSPECIFIED.);
#4612=B_SPLINE_CURVE_WITH_KNOTS('',3,(#191720,#191721,#191722,#191723,#191724,
#191725,#191726,#191727,#191728,#191729,#191730,#191731,#191732,#191733,
#191734,#191735,#191736,#191737,#191738,#191739,#191740,#191741,#191742,
#191743,#191744,#191745,#191746,#191747,#191748,#191749,#191750,#191751,
#191752,#191753,#191754,#191755,#191756,#191757,#191758,#191759,#191760,
#191761,#191762,#191763,#191764,#191765,#191766,#191767,#191768,#191769,
#191770,#191771),.UNSPECIFIED.,.F.,.F.,(4,3,3,3,3,3,3,3,3,3,3,3,3,3,3,3,
3,4),(0.,2.58457451678823E-5,4.25394446195921E-5,6.46659869687165E-5,7.57292581432787E-5,
8.12608937305598E-5,8.26438026273801E-5,8.67925293178409E-5,0.00011601562442684,
0.000130188793976761,0.000151886926306222,0.000161963651211289,0.000162735992470952,
0.000173585058635682,0.000212487880460706,0.00025523817351073,0.000301397761144501,
0.000347170117271364),.UNSPECIFIED.);
#4613=B_SPLINE_CURVE_WITH_KNOTS('',3,(#191773,#191774,#191775,#191776,#191777,
#191778,#191779,#191780,#191781,#191782,#191783,#191784,#191785,#191786,
#191787,#191788,#191789,#191790,#191791,#191792,#191793,#191794,#191795,
#191796,#191797,#191798,#191799,#191800,#191801,#191802,#191803,#191804,
#191805,#191806,#191807,#191808,#191809,#191810,#191811,#191812,#191813,
#191814,#191815,#191816,#191817,#191818),.UNSPECIFIED.,.F.,.F.,(4,3,3,3,
3,3,3,3,3,3,3,3,3,3,3,4),(1.73472347597681E-18,2.57218161989433E-5,4.21568322567811E-5,
6.45873314617046E-5,7.58025810641663E-5,8.14102058653971E-5,8.28121120657048E-5,
8.7017830666628E-5,0.000116081955658619,0.000130526745999941,0.000162394111022059,
0.000174035661333254,0.000213138396960531,0.00025611693543839,0.000302406662863409,
0.000348071322666518),.UNSPECIFIED.);
#4614=B_SPLINE_CURVE_WITH_KNOTS('',3,(#191819,#191820,#191821,#191822,#191823,
#191824,#191825,#191826,#191827,#191828,#191829,#191830,#191831,#191832,
#191833,#191834,#191835,#191836,#191837,#191838,#191839,#191840,#191841,
#191842,#191843,#191844,#191845,#191846,#191847,#191848,#191849,#191850,
#191851,#191852,#191853,#191854,#191855,#191856,#191857,#191858,#191859,
#191860,#191861,#191862,#191863,#191864,#191865,#191866,#191867,#191868,
#191869,#191870),.UNSPECIFIED.,.F.,.F.,(4,3,3,3,3,3,3,3,3,3,3,3,3,3,3,3,
3,4),(0.,4.29652152204607E-5,8.44519107603203E-5,0.000123669830873161,0.000159788877366737,
0.000170558847912626,0.000181218775907165,0.000181960046452412,0.000214460062644189,
0.000244755726200295,0.000255838271868945,0.00025850325386758,0.000261084955178758,
0.000289370476646845,0.000301101325502011,0.000321109510663638,0.000331113603244451,
0.000341117695825265),.UNSPECIFIED.);
#4615=B_SPLINE_CURVE_WITH_KNOTS('',3,(#191872,#191873,#191874,#191875,#191876,
#191877,#191878,#191879,#191880,#191881,#191882,#191883,#191884,#191885,
#191886,#191887,#191888,#191889,#191890,#191891,#191892,#191893,#191894,
#191895,#191896,#191897,#191898,#191899,#191900,#191901,#191902,#191903,
#191904,#191905,#191906,#191907,#191908,#191909,#191910,#191911,#191912,
#191913,#191914,#191915,#191916,#191917,#191918,#191919,#191920,#191921,
#191922,#191923),.UNSPECIFIED.,.F.,.F.,(4,3,3,3,3,3,3,3,3,3,3,3,3,3,3,3,
3,4),(0.,4.3070623786749E-5,8.4741708769304E-5,0.000124159989205248,0.000160467076289362,
0.000170998382116684,0.000182414994733762,0.000213747977645858,0.00024241595590281,
0.000256497573175033,0.000259169422895606,0.000261757777312412,0.000289965130403439,
0.000301877270772897,0.000321937017503139,0.0003269519541857,0.000334474359209541,
0.000341996764233382),.UNSPECIFIED.);
#4616=B_SPLINE_CURVE_WITH_KNOTS('',3,(#191924,#191925,#191926,#191927,#191928,
#191929,#191930,#191931,#191932,#191933,#191934,#191935,#191936,#191937,
#191938,#191939,#191940,#191941,#191942,#191943,#191944,#191945,#191946,
#191947,#191948,#191949,#191950,#191951,#191952,#191953,#191954,#191955,
#191956,#191957,#191958,#191959,#191960,#191961,#191962,#191963,#191964,
#191965,#191966,#191967,#191968,#191969,#191970,#191971,#191972,#191973,
#191974,#191975),.UNSPECIFIED.,.F.,.F.,(4,3,3,3,3,3,3,3,3,3,3,3,3,3,3,3,
3,4),(0.,2.58457451687104E-5,4.25394446195245E-5,6.46659869686809E-5,7.57292581432591E-5,
8.12608937305483E-5,8.26438026273705E-5,8.67925293178374E-5,0.000116015624427198,
0.000130188793976756,0.000151886926306215,0.000161963651211279,0.000162735992470945,
0.000173585058635675,0.000212487880460741,0.000255238173511971,0.000301397761149513,
0.00034717011727135),.UNSPECIFIED.);
#4617=B_SPLINE_CURVE_WITH_KNOTS('',3,(#191977,#191978,#191979,#191980,#191981,
#191982,#191983,#191984,#191985,#191986,#191987,#191988,#191989,#191990,
#191991,#191992,#191993,#191994,#191995,#191996,#191997,#191998,#191999,
#192000,#192001,#192002,#192003,#192004,#192005,#192006,#192007,#192008,
#192009,#192010,#192011,#192012,#192013,#192014,#192015,#192016,#192017,
#192018,#192019,#192020,#192021,#192022),.UNSPECIFIED.,.F.,.F.,(4,3,3,3,
3,3,3,3,3,3,3,3,3,3,3,4),(5.48877349820787E-19,2.57218161989097E-5,4.2156832256823E-5,
6.45873314617228E-5,7.58025810641727E-5,8.14102058653976E-5,8.28121120657039E-5,
8.70178306666226E-5,0.000116081955657846,0.000130526745999934,0.000162394111022054,
0.000174035661333245,0.000213138396957884,0.000256116935433115,0.000302406662855211,
0.000348071322666501),.UNSPECIFIED.);
#4618=B_SPLINE_CURVE_WITH_KNOTS('',3,(#192023,#192024,#192025,#192026,#192027,
#192028,#192029,#192030,#192031,#192032,#192033,#192034,#192035,#192036,
#192037,#192038,#192039,#192040,#192041,#192042,#192043,#192044,#192045,
#192046,#192047,#192048,#192049,#192050,#192051,#192052,#192053,#192054,
#192055,#192056,#192057,#192058,#192059,#192060,#192061,#192062,#192063,
#192064,#192065,#192066,#192067,#192068,#192069,#192070,#192071,#192072,
#192073,#192074),.UNSPECIFIED.,.F.,.F.,(4,3,3,3,3,3,3,3,3,3,3,3,3,3,3,3,
3,4),(0.,4.29652152190797E-5,8.44519107582085E-5,0.000123669830870829,0.000159788877364511,
0.000170558847912623,0.000181218775907163,0.000181960046452403,0.000214460062643601,
0.000244755726198573,0.000255838271868941,0.000258503253867576,0.000261084955178753,
0.000289370476648259,0.000301101325502006,0.000321109510663632,0.000331113603244445,
0.000341117695825259),.UNSPECIFIED.);
#4619=B_SPLINE_CURVE_WITH_KNOTS('',3,(#192076,#192077,#192078,#192079,#192080,
#192081,#192082,#192083,#192084,#192085,#192086,#192087,#192088,#192089,
#192090,#192091,#192092,#192093,#192094,#192095,#192096,#192097,#192098,
#192099,#192100,#192101,#192102,#192103,#192104,#192105,#192106,#192107,
#192108,#192109,#192110,#192111,#192112,#192113,#192114,#192115,#192116,
#192117,#192118,#192119,#192120,#192121,#192122,#192123,#192124,#192125,
#192126,#192127),.UNSPECIFIED.,.F.,.F.,(4,3,3,3,3,3,3,3,3,3,3,3,3,3,3,3,
3,4),(9.85133562538035E-18,4.30706237855933E-5,8.47417087672294E-5,0.000124159989202406,
0.000160467076285688,0.000170998382116695,0.000182414994733793,0.000213747977645867,
0.000242415955902541,0.000256497573175038,0.000259169422895611,0.000261757777312417,
0.00028996513040345,0.000301877270772899,0.00032193701750314,0.0003269519541857,
0.00033447435920954,0.000341996764233381),.UNSPECIFIED.);
#4620=B_SPLINE_CURVE_WITH_KNOTS('',3,(#192128,#192129,#192130,#192131,#192132,
#192133,#192134,#192135,#192136,#192137,#192138,#192139,#192140,#192141,
#192142,#192143,#192144,#192145,#192146,#192147,#192148,#192149,#192150,
#192151,#192152,#192153,#192154,#192155,#192156,#192157,#192158,#192159,
#192160,#192161,#192162,#192163,#192164,#192165,#192166,#192167,#192168,
#192169,#192170,#192171,#192172,#192173,#192174,#192175,#192176,#192177,
#192178,#192179),.UNSPECIFIED.,.F.,.F.,(4,3,3,3,3,3,3,3,3,3,3,3,3,3,3,3,
3,4),(0.,2.58457451673525E-5,4.25394446195986E-5,6.46659869687198E-5,7.57292581432803E-5,
8.12608937305606E-5,8.26438026273807E-5,8.67925293178409E-5,0.000116015624426975,
0.000130188793976761,0.000151886926306222,0.000161963651211268,0.000162735992470952,
0.000173585058635682,0.000212487880460807,0.00025523817351178,0.000301397761147946,
0.000347170117271376),.UNSPECIFIED.);
#4621=B_SPLINE_CURVE_WITH_KNOTS('',3,(#192181,#192182,#192183,#192184,#192185,
#192186,#192187,#192188,#192189,#192190,#192191,#192192,#192193,#192194,
#192195,#192196,#192197,#192198,#192199,#192200,#192201,#192202,#192203,
#192204,#192205,#192206,#192207,#192208,#192209,#192210,#192211,#192212,
#192213,#192214,#192215,#192216,#192217,#192218,#192219,#192220,#192221,
#192222,#192223,#192224,#192225,#192226),.UNSPECIFIED.,.F.,.F.,(4,3,3,3,
3,3,3,3,3,3,3,3,3,3,3,4),(8.67361737988403E-19,2.57218161984597E-5,4.21568322567013E-5,
6.45873314616616E-5,7.58025810641418E-5,8.14102058653818E-5,8.28121120656919E-5,
8.70178306666219E-5,0.000116081955658696,0.000130526745999929,0.000162394111022049,
0.000174035661333235,0.00021313839696006,0.000256116935437399,0.00030240666286165,
0.000348071322666489),.UNSPECIFIED.);
#4622=B_SPLINE_CURVE_WITH_KNOTS('',3,(#192227,#192228,#192229,#192230,#192231,
#192232,#192233,#192234,#192235,#192236,#192237,#192238,#192239,#192240,
#192241,#192242,#192243,#192244,#192245,#192246,#192247,#192248,#192249,
#192250,#192251,#192252,#192253,#192254,#192255,#192256,#192257,#192258,
#192259,#192260,#192261,#192262,#192263,#192264,#192265,#192266,#192267,
#192268,#192269,#192270,#192271,#192272,#192273,#192274,#192275,#192276,
#192277,#192278),.UNSPECIFIED.,.F.,.F.,(4,3,3,3,3,3,3,3,3,3,3,3,3,3,3,3,
3,4),(0.,4.29652152191222E-5,8.44519107581807E-5,0.000123669830870584,0.000159788877363929,
0.000170558847912617,0.000181218775907157,0.0001819600464524,0.000214460062643968,
0.000244755726199534,0.000255838271868939,0.000258503253867574,0.000261084955178751,
0.000289370476646808,0.000301101325502006,0.000321109510663633,0.000331113603244447,
0.00034111769582526),.UNSPECIFIED.);
#4623=B_SPLINE_CURVE_WITH_KNOTS('',3,(#192280,#192281,#192282,#192283,#192284,
#192285,#192286,#192287,#192288,#192289,#192290,#192291,#192292,#192293,
#192294,#192295,#192296,#192297,#192298,#192299,#192300,#192301,#192302,
#192303,#192304,#192305,#192306,#192307,#192308,#192309,#192310,#192311,
#192312,#192313,#192314,#192315,#192316,#192317,#192318,#192319,#192320,
#192321,#192322,#192323,#192324,#192325,#192326,#192327,#192328,#192329,
#192330,#192331),.UNSPECIFIED.,.F.,.F.,(4,3,3,3,3,3,3,3,3,3,3,3,3,3,3,3,
3,4),(0.,4.30706237878556E-5,8.47417087713877E-5,0.000124159989208393,0.000160467076293688,
0.000170998382116697,0.000182414994733767,0.000213747977645869,0.000242415955903676,
0.000256497573175041,0.000259169422895614,0.000261757777312419,0.000289965130402761,
0.000301877270772902,0.000321937017503143,0.000326951954185703,0.000334474359209544,
0.000341996764233384),.UNSPECIFIED.);
#4624=B_SPLINE_CURVE_WITH_KNOTS('',3,(#192332,#192333,#192334,#192335,#192336,
#192337,#192338,#192339,#192340,#192341,#192342,#192343,#192344,#192345,
#192346,#192347,#192348,#192349,#192350,#192351,#192352,#192353,#192354,
#192355,#192356,#192357,#192358,#192359,#192360,#192361,#192362,#192363,
#192364,#192365,#192366,#192367,#192368,#192369,#192370,#192371,#192372,
#192373,#192374,#192375,#192376,#192377,#192378,#192379,#192380,#192381,
#192382,#192383),.UNSPECIFIED.,.F.,.F.,(4,3,3,3,3,3,3,3,3,3,3,3,3,3,3,3,
3,4),(0.,2.5845745168666E-5,4.25394446195824E-5,6.46659869687127E-5,7.57292581432779E-5,
8.12608937305605E-5,8.26438026273811E-5,8.6792529317843E-5,0.000116015624428386,
0.000130188793976765,0.000151886926306225,0.000161963651211285,0.000162735992470956,
0.000173585058635686,0.000212487880463336,0.00025523817351687,0.000301397761156083,
0.000347170117271363),.UNSPECIFIED.);
#4625=B_SPLINE_CURVE_WITH_KNOTS('',3,(#192385,#192386,#192387,#192388,#192389,
#192390,#192391,#192392,#192393,#192394,#192395,#192396,#192397,#192398,
#192399,#192400,#192401,#192402,#192403,#192404,#192405,#192406,#192407,
#192408,#192409,#192410,#192411,#192412,#192413,#192414,#192415,#192416,
#192417,#192418,#192419,#192420,#192421,#192422,#192423,#192424,#192425,
#192426,#192427,#192428,#192429,#192430),.UNSPECIFIED.,.F.,.F.,(4,3,3,3,
3,3,3,3,3,3,3,3,3,3,3,4),(0.,2.57218161995338E-5,4.21568322567715E-5,6.45873314616955E-5,
7.58025810641576E-5,8.14102058653886E-5,8.28121120656963E-5,8.70178306666196E-5,
0.000116081955657908,0.000130526745999929,0.000162394111022051,0.000174035661333239,
0.000213138396960905,0.000256116935439096,0.0003024066628643,0.000348071322666476),
 .UNSPECIFIED.);
#4626=B_SPLINE_CURVE_WITH_KNOTS('',3,(#192431,#192432,#192433,#192434,#192435,
#192436,#192437,#192438,#192439,#192440,#192441,#192442,#192443,#192444,
#192445,#192446,#192447,#192448,#192449,#192450,#192451,#192452,#192453,
#192454,#192455,#192456,#192457,#192458,#192459,#192460,#192461,#192462,
#192463,#192464,#192465,#192466,#192467,#192468,#192469,#192470,#192471,
#192472,#192473,#192474,#192475,#192476,#192477,#192478,#192479,#192480,
#192481,#192482),.UNSPECIFIED.,.F.,.F.,(4,3,3,3,3,3,3,3,3,3,3,3,3,3,3,3,
3,4),(0.,4.29652152168045E-5,8.44519107545815E-5,0.000123669830866463,0.000159788877359758,
0.000170558847912623,0.000181218775907163,0.000181960046452399,0.000214460062643643,
0.000244755726198916,0.000255838271868941,0.000258503253867576,0.000261084955178754,
0.000289370476647759,0.000301101325502006,0.000321109510663633,0.000331113603244446,
0.000341117695825259),.UNSPECIFIED.);
#4627=B_SPLINE_CURVE_WITH_KNOTS('',3,(#192484,#192485,#192486,#192487,#192488,
#192489,#192490,#192491,#192492,#192493,#192494,#192495,#192496,#192497,
#192498,#192499,#192500,#192501,#192502,#192503,#192504,#192505,#192506,
#192507,#192508,#192509,#192510,#192511,#192512,#192513,#192514,#192515,
#192516,#192517,#192518,#192519,#192520,#192521,#192522,#192523,#192524,
#192525,#192526,#192527,#192528,#192529,#192530,#192531,#192532,#192533,
#192534,#192535),.UNSPECIFIED.,.F.,.F.,(4,3,3,3,3,3,3,3,3,3,3,3,3,3,3,3,
3,4),(0.,4.30706237843463E-5,8.47417087647801E-5,0.000124159989198604,0.000160467076280188,
0.000170998382116709,0.000182414994733815,0.00021374797764588,0.00024241595590353,
0.000256497573175051,0.000259169422895624,0.000261757777312429,0.000289965130403544,
0.000301877270772911,0.000321937017503151,0.000326951954185712,0.000334474359209552,
0.000341996764233392),.UNSPECIFIED.);
#4628=B_SPLINE_CURVE_WITH_KNOTS('',3,(#192536,#192537,#192538,#192539,#192540,
#192541,#192542,#192543,#192544,#192545,#192546,#192547,#192548,#192549,
#192550,#192551,#192552,#192553,#192554,#192555,#192556,#192557,#192558,
#192559,#192560,#192561,#192562,#192563,#192564,#192565,#192566,#192567,
#192568,#192569,#192570,#192571,#192572,#192573,#192574,#192575,#192576,
#192577,#192578,#192579,#192580,#192581,#192582,#192583,#192584,#192585,
#192586,#192587),.UNSPECIFIED.,.F.,.F.,(4,3,3,3,3,3,3,3,3,3,3,3,3,3,3,3,
3,4),(0.,2.58457451680454E-5,4.25394446195865E-5,6.46659869687126E-5,7.57292581432756E-5,
8.12608937305571E-5,8.26438026273775E-5,8.67925293178386E-5,0.000116015624427228,
0.000130188793976758,0.000151886926306218,0.000161963651211266,0.000162735992470947,
0.000173585058635677,0.00021248788045917,0.000255238173507915,0.000301397761140769,
0.000347170117271374),.UNSPECIFIED.);
#4629=B_SPLINE_CURVE_WITH_KNOTS('',3,(#192589,#192590,#192591,#192592,#192593,
#192594,#192595,#192596,#192597,#192598,#192599,#192600,#192601,#192602,
#192603,#192604,#192605,#192606,#192607,#192608,#192609,#192610,#192611,
#192612,#192613,#192614,#192615,#192616,#192617,#192618,#192619,#192620,
#192621,#192622,#192623,#192624,#192625,#192626,#192627,#192628,#192629,
#192630,#192631,#192632,#192633,#192634),.UNSPECIFIED.,.F.,.F.,(4,3,3,3,
3,3,3,3,3,3,3,3,3,3,3,4),(0.,2.57218162011368E-5,4.21568322568854E-5,6.45873314617514E-5,
7.58025810641844E-5,8.14102058654009E-5,8.2812112065705E-5,8.70178306666174E-5,
0.000116081955658846,0.000130526745999926,0.000162394111022064,0.000174035661333235,
0.000213138396958756,0.000256116935434756,0.000302406662857426,0.000348071322666454),
 .UNSPECIFIED.);
#4630=B_SPLINE_CURVE_WITH_KNOTS('',3,(#192635,#192636,#192637,#192638,#192639,
#192640,#192641,#192642,#192643,#192644,#192645,#192646,#192647,#192648,
#192649,#192650,#192651,#192652,#192653,#192654,#192655,#192656,#192657,
#192658,#192659,#192660,#192661,#192662,#192663,#192664,#192665,#192666,
#192667,#192668,#192669,#192670,#192671,#192672,#192673,#192674,#192675,
#192676,#192677,#192678,#192679,#192680,#192681,#192682,#192683,#192684,
#192685,#192686),.UNSPECIFIED.,.F.,.F.,(4,3,3,3,3,3,3,3,3,3,3,3,3,3,3,3,
3,4),(0.,4.29652152214354E-5,8.44519107622748E-5,0.000123669830876302,0.00015978887737137,
0.000170558847912627,0.000181218775907166,0.000181960046452393,0.000214460062643908,
0.000244755726199127,0.000255838271868937,0.000258503253867572,0.000261084955178749,
0.000289370476646983,0.000301101325501999,0.000321109510663623,0.000331113603244436,
0.000341117695825248),.UNSPECIFIED.);
#4631=B_SPLINE_CURVE_WITH_KNOTS('',3,(#192688,#192689,#192690,#192691,#192692,
#192693,#192694,#192695,#192696,#192697,#192698,#192699,#192700,#192701,
#192702,#192703,#192704,#192705,#192706,#192707,#192708,#192709,#192710,
#192711,#192712,#192713,#192714,#192715,#192716,#192717,#192718,#192719,
#192720,#192721,#192722,#192723,#192724,#192725,#192726,#192727,#192728,
#192729,#192730,#192731,#192732,#192733,#192734,#192735,#192736,#192737,
#192738,#192739),.UNSPECIFIED.,.F.,.F.,(4,3,3,3,3,3,3,3,3,3,3,3,3,3,3,3,
3,4),(0.,4.30706237879649E-5,8.47417087713518E-5,0.000124159989207974,0.000160467076292721,
0.000170998382116688,0.000182414994733775,0.000213747977645863,0.000242415955903171,
0.000256497573175039,0.000259169422895612,0.000261757777312418,0.000289965130403515,
0.000301877270772904,0.000321937017503147,0.000326951954185707,0.000334474359209549,
0.00034199676423339),.UNSPECIFIED.);
#4632=B_SPLINE_CURVE_WITH_KNOTS('',3,(#192740,#192741,#192742,#192743,#192744,
#192745,#192746,#192747,#192748,#192749,#192750,#192751,#192752,#192753,
#192754,#192755,#192756,#192757,#192758,#192759,#192760,#192761,#192762,
#192763,#192764,#192765,#192766,#192767,#192768,#192769,#192770,#192771,
#192772,#192773,#192774,#192775,#192776,#192777,#192778,#192779,#192780,
#192781,#192782,#192783,#192784,#192785,#192786,#192787,#192788,#192789,
#192790,#192791),.UNSPECIFIED.,.F.,.F.,(4,3,3,3,3,3,3,3,3,3,3,3,3,3,3,3,
3,4),(0.,2.58457451674872E-5,4.25394446196628E-5,6.46659869687521E-5,7.57292581432967E-5,
8.12608937305691E-5,8.26438026273871E-5,8.67925293178414E-5,0.000116015624427357,
0.000130188793976762,0.000151886926306222,0.000161963651211285,0.000162735992470953,
0.000173585058635683,0.000212487880460278,0.00025523817350991,0.000301397761143294,
0.000347170117271361),.UNSPECIFIED.);
#4633=B_SPLINE_CURVE_WITH_KNOTS('',3,(#192793,#192794,#192795,#192796,#192797,
#192798,#192799,#192800,#192801,#192802,#192803,#192804,#192805,#192806,
#192807,#192808,#192809,#192810,#192811,#192812,#192813,#192814,#192815,
#192816,#192817,#192818,#192819,#192820,#192821,#192822,#192823,#192824,
#192825,#192826,#192827,#192828,#192829,#192830,#192831,#192832,#192833,
#192834,#192835,#192836,#192837,#192838),.UNSPECIFIED.,.F.,.F.,(4,3,3,3,
3,3,3,3,3,3,3,3,3,3,3,4),(3.46944695195361E-18,2.57218162008425E-5,4.21568322567336E-5,
6.45873314616739E-5,7.58025810641441E-5,8.14102058653791E-5,8.28121120656879E-5,
8.70178306666142E-5,0.000116081955659379,0.00013052674599992,0.000162394111022033,
0.000174035661333225,0.000213138396959368,0.000256116935436057,0.000302406662859663,
0.00034807132266646),.UNSPECIFIED.);
#4634=B_SPLINE_CURVE_WITH_KNOTS('',3,(#192839,#192840,#192841,#192842,#192843,
#192844,#192845,#192846,#192847,#192848,#192849,#192850,#192851,#192852,
#192853,#192854,#192855,#192856,#192857,#192858,#192859,#192860,#192861,
#192862,#192863,#192864,#192865,#192866,#192867,#192868,#192869,#192870,
#192871,#192872,#192873,#192874,#192875,#192876,#192877,#192878,#192879,
#192880,#192881,#192882,#192883,#192884,#192885,#192886,#192887,#192888,
#192889,#192890),.UNSPECIFIED.,.F.,.F.,(4,3,3,3,3,3,3,3,3,3,3,3,3,3,3,3,
3,4),(0.,4.29652152146269E-5,8.44519107510616E-5,0.000123669830862063,0.000159788877354834,
0.000170558847912627,0.000181218775907166,0.000181960046452403,0.000214460062643365,
0.0002447557261976,0.000255838271868941,0.000258503253867576,0.000261084955178753,
0.000289370476647798,0.000301101325502004,0.00032110951066363,0.000331113603244442,
0.000341117695825255),.UNSPECIFIED.);
#4635=B_SPLINE_CURVE_WITH_KNOTS('',3,(#192892,#192893,#192894,#192895,#192896,
#192897,#192898,#192899,#192900,#192901,#192902,#192903,#192904,#192905,
#192906,#192907,#192908,#192909,#192910,#192911,#192912,#192913,#192914,
#192915,#192916,#192917,#192918,#192919,#192920,#192921,#192922,#192923,
#192924,#192925,#192926,#192927,#192928,#192929,#192930,#192931,#192932,
#192933,#192934,#192935,#192936,#192937,#192938,#192939,#192940,#192941,
#192942,#192943),.UNSPECIFIED.,.F.,.F.,(4,3,3,3,3,3,3,3,3,3,3,3,3,3,3,3,
3,4),(0.,4.30706237882749E-5,8.47417087721192E-5,0.000124159989209344,0.000160467076294915,
0.000170998382116705,0.000182414994733787,0.000213747977645879,0.00024241595590288,
0.000256497573175053,0.000259169422895626,0.000261757777312432,0.000289965130402957,
0.000301877270772916,0.000321937017503158,0.000326951954185719,0.00033447435920956,
0.0003419967642334),.UNSPECIFIED.);
#4636=B_SPLINE_CURVE_WITH_KNOTS('',3,(#192944,#192945,#192946,#192947,#192948,
#192949,#192950,#192951,#192952,#192953,#192954,#192955,#192956,#192957,
#192958,#192959,#192960,#192961,#192962,#192963,#192964,#192965,#192966,
#192967,#192968,#192969,#192970,#192971,#192972,#192973,#192974,#192975,
#192976,#192977,#192978,#192979,#192980,#192981,#192982,#192983,#192984,
#192985,#192986,#192987,#192988,#192989,#192990,#192991,#192992,#192993,
#192994,#192995),.UNSPECIFIED.,.F.,.F.,(4,3,3,3,3,3,3,3,3,3,3,3,3,3,3,3,
3,4),(0.,2.58457451677947E-5,4.25394446196165E-5,6.46659869687299E-5,7.57292581432866E-5,
8.12608937305649E-5,8.26438026273845E-5,8.67925293178432E-5,0.000116015624427386,
0.000130188793976765,0.000151886926306226,0.000161963651211264,0.000162735992470956,
0.000173585058635686,0.00021248788045667,0.000255238173502178,0.000301397761129961,
0.000347170117271371),.UNSPECIFIED.);
#4637=B_SPLINE_CURVE_WITH_KNOTS('',3,(#192997,#192998,#192999,#193000,#193001,
#193002,#193003,#193004,#193005,#193006,#193007,#193008,#193009,#193010,
#193011,#193012,#193013,#193014,#193015,#193016,#193017,#193018,#193019,
#193020,#193021,#193022,#193023,#193024,#193025,#193026,#193027,#193028,
#193029,#193030,#193031,#193032,#193033,#193034,#193035,#193036,#193037,
#193038,#193039,#193040,#193041,#193042),.UNSPECIFIED.,.F.,.F.,(4,3,3,3,
3,3,3,3,3,3,3,3,3,3,3,4),(0.,2.57218161985032E-5,4.21568322569506E-5,6.45873314617842E-5,
7.5802581064201E-5,8.14102058654094E-5,8.28121120657115E-5,8.70178306666178E-5,
0.00011608195565788,0.000130526745999927,0.000162394111022043,0.000174035661333236,
0.000213138396958693,0.000256116935434544,0.000302406662856772,0.000348071322666484),
 .UNSPECIFIED.);
#4638=B_SPLINE_CURVE_WITH_KNOTS('',3,(#193043,#193044,#193045,#193046,#193047,
#193048,#193049,#193050,#193051,#193052,#193053,#193054,#193055,#193056,
#193057,#193058,#193059,#193060,#193061,#193062,#193063,#193064,#193065,
#193066,#193067,#193068,#193069,#193070,#193071,#193072,#193073,#193074,
#193075,#193076,#193077,#193078,#193079,#193080,#193081,#193082,#193083,
#193084,#193085,#193086,#193087,#193088,#193089,#193090,#193091,#193092,
#193093,#193094),.UNSPECIFIED.,.F.,.F.,(4,3,3,3,3,3,3,3,3,3,3,3,3,3,3,3,
3,4),(0.,4.29652152129906E-5,8.44519107478209E-5,0.000123669830856864,0.000159788877347059,
0.000170558847912636,0.000181218775907175,0.000181960046452432,0.000214460062643819,
0.000244755726198886,0.000255838271868951,0.000258503253867586,0.000261084955178763,
0.000289370476647964,0.000301101325502015,0.00032110951066364,0.000331113603244453,
0.000341117695825266),.UNSPECIFIED.);
#4639=B_SPLINE_CURVE_WITH_KNOTS('',3,(#193096,#193097,#193098,#193099,#193100,
#193101,#193102,#193103,#193104,#193105,#193106,#193107,#193108,#193109,
#193110,#193111,#193112,#193113,#193114,#193115,#193116,#193117,#193118,
#193119,#193120,#193121,#193122,#193123,#193124,#193125,#193126,#193127,
#193128,#193129,#193130,#193131,#193132,#193133,#193134,#193135,#193136,
#193137,#193138,#193139,#193140,#193141,#193142,#193143,#193144,#193145,
#193146,#193147),.UNSPECIFIED.,.F.,.F.,(4,3,3,3,3,3,3,3,3,3,3,3,3,3,3,3,
3,4),(0.,4.3070623787665E-5,8.47417087708582E-5,0.000124159989207229,0.000160467076291828,
0.000170998382116699,0.000182414994733755,0.000213747977645872,0.000242415955902611,
0.000256497573175046,0.000259169422895619,0.000261757777312424,0.000289965130403524,
0.000301877270772909,0.000321937017503151,0.000326951954185711,0.000334474359209552,
0.000341996764233393),.UNSPECIFIED.);
#4640=B_SPLINE_CURVE_WITH_KNOTS('',3,(#193148,#193149,#193150,#193151,#193152,
#193153,#193154,#193155,#193156,#193157,#193158,#193159,#193160,#193161,
#193162,#193163,#193164,#193165,#193166,#193167,#193168,#193169,#193170,
#193171,#193172,#193173,#193174,#193175,#193176,#193177,#193178,#193179,
#193180,#193181,#193182,#193183,#193184,#193185,#193186,#193187,#193188,
#193189,#193190,#193191,#193192,#193193,#193194,#193195,#193196,#193197,
#193198,#193199),.UNSPECIFIED.,.F.,.F.,(4,3,3,3,3,3,3,3,3,3,3,3,3,3,3,3,
3,4),(0.,2.58457451692331E-5,4.25394446195874E-5,6.46659869687102E-5,7.57292581432715E-5,
8.12608937305522E-5,8.26438026273724E-5,8.67925293178329E-5,0.000116015624428751,
0.000130188793976749,0.000151886926306208,0.000161963651211278,0.000162735992470937,
0.000173585058635666,0.000212487880459203,0.000255238173507225,0.000301397761137999,
0.000347170117271348),.UNSPECIFIED.);
#4641=B_SPLINE_CURVE_WITH_KNOTS('',3,(#193201,#193202,#193203,#193204,#193205,
#193206,#193207,#193208,#193209,#193210,#193211,#193212,#193213,#193214,
#193215,#193216,#193217,#193218,#193219,#193220,#193221,#193222,#193223,
#193224,#193225,#193226,#193227,#193228,#193229,#193230,#193231,#193232,
#193233,#193234,#193235,#193236,#193237,#193238,#193239,#193240,#193241,
#193242,#193243,#193244,#193245,#193246),.UNSPECIFIED.,.F.,.F.,(4,3,3,3,
3,3,3,3,3,3,3,3,3,3,3,4),(6.93889390390723E-18,2.57218162003168E-5,4.2156832256597E-5,
6.45873314616125E-5,7.58025810641203E-5,8.14102058653742E-5,8.28121120656877E-5,
8.70178306666281E-5,0.000116081955659664,0.000130526745999939,0.000162394111022071,
0.000174035661333249,0.000213138396962072,0.000256116935441266,0.000302406662867136,
0.000348071322666479),.UNSPECIFIED.);
#4642=B_SPLINE_CURVE_WITH_KNOTS('',3,(#193247,#193248,#193249,#193250,#193251,
#193252,#193253,#193254,#193255,#193256,#193257,#193258,#193259,#193260,
#193261,#193262,#193263,#193264,#193265,#193266,#193267,#193268,#193269,
#193270,#193271,#193272,#193273,#193274,#193275,#193276,#193277,#193278,
#193279,#193280,#193281,#193282,#193283,#193284,#193285,#193286,#193287,
#193288,#193289,#193290,#193291,#193292,#193293,#193294,#193295,#193296,
#193297,#193298),.UNSPECIFIED.,.F.,.F.,(4,3,3,3,3,3,3,3,3,3,3,3,3,3,3,3,
3,4),(0.,4.29652152181114E-5,8.44519107563061E-5,0.000123669830867864,0.000159788877360231,
0.00017055884791263,0.000181218775907169,0.000181960046452423,0.000214460062643701,
0.000244755726198761,0.000255838271868939,0.000258503253867574,0.000261084955178751,
0.000289370476648725,0.000301101325502,0.000321109510663624,0.000331113603244436,
0.000341117695825248),.UNSPECIFIED.);
#4643=B_SPLINE_CURVE_WITH_KNOTS('',3,(#193300,#193301,#193302,#193303,#193304,
#193305,#193306,#193307,#193308,#193309,#193310,#193311,#193312,#193313,
#193314,#193315,#193316,#193317,#193318,#193319,#193320,#193321,#193322,
#193323,#193324,#193325,#193326,#193327,#193328,#193329,#193330,#193331,
#193332,#193333,#193334,#193335,#193336,#193337,#193338,#193339,#193340,
#193341,#193342,#193343,#193344,#193345,#193346,#193347,#193348,#193349,
#193350,#193351),.UNSPECIFIED.,.F.,.F.,(4,3,3,3,3,3,3,3,3,3,3,3,3,3,3,3,
3,4),(0.,4.30706237873436E-5,8.47417087703543E-5,0.000124159989206768,0.000160467076291368,
0.000170998382116691,0.000182414994733778,0.000213747977645865,0.000242415955903022,
0.000256497573175039,0.000259169422895612,0.000261757777312417,0.000289965130402893,
0.000301877270772902,0.000321937017503144,0.000326951954185705,0.000334474359209545,
0.000341996764233386),.UNSPECIFIED.);
#4644=B_SPLINE_CURVE_WITH_KNOTS('',3,(#193352,#193353,#193354,#193355,#193356,
#193357,#193358,#193359,#193360,#193361,#193362,#193363,#193364,#193365,
#193366,#193367,#193368,#193369,#193370,#193371,#193372,#193373,#193374,
#193375,#193376,#193377,#193378,#193379,#193380,#193381,#193382,#193383,
#193384,#193385,#193386,#193387,#193388,#193389,#193390,#193391,#193392,
#193393,#193394,#193395,#193396,#193397,#193398,#193399,#193400,#193401,
#193402,#193403),.UNSPECIFIED.,.F.,.F.,(4,3,3,3,3,3,3,3,3,3,3,3,3,3,3,3,
3,4),(0.,2.58457451679608E-5,4.25394446195563E-5,6.46659869686995E-5,7.57292581432711E-5,
8.12608937305569E-5,8.26438026273783E-5,8.67925293178427E-5,0.000116015624427097,
0.000130188793976764,0.000151886926306225,0.000161963651211274,0.000162735992470955,
0.000173585058635685,0.000212487880461448,0.000255238173513823,0.000301397761153107,
0.000347170117271366),.UNSPECIFIED.);
#4645=B_SPLINE_CURVE_WITH_KNOTS('',3,(#193405,#193406,#193407,#193408,#193409,
#193410,#193411,#193412,#193413,#193414,#193415,#193416,#193417,#193418,
#193419,#193420,#193421,#193422,#193423,#193424,#193425,#193426,#193427,
#193428,#193429,#193430,#193431,#193432,#193433,#193434,#193435,#193436,
#193437,#193438,#193439,#193440,#193441,#193442,#193443,#193444,#193445,
#193446,#193447,#193448,#193449,#193450),.UNSPECIFIED.,.F.,.F.,(4,3,3,3,
3,3,3,3,3,3,3,3,3,3,3,4),(0.,2.57218162026608E-5,4.21568322568483E-5,6.45873314617269E-5,
7.58025810641662E-5,8.14102058653858E-5,8.28121120656908E-5,8.70178306666055E-5,
0.00011608195565896,0.000130526745999908,0.000162394111022025,0.000174035661333211,
0.000213138396955903,0.000256116935429113,0.000302406662848748,0.000348071322666448),
 .UNSPECIFIED.);
#4646=B_SPLINE_CURVE_WITH_KNOTS('',3,(#193451,#193452,#193453,#193454,#193455,
#193456,#193457,#193458,#193459,#193460,#193461,#193462,#193463,#193464,
#193465,#193466,#193467,#193468,#193469,#193470,#193471,#193472,#193473,
#193474,#193475,#193476,#193477,#193478,#193479,#193480,#193481,#193482,
#193483,#193484,#193485,#193486,#193487,#193488,#193489,#193490,#193491,
#193492,#193493,#193494,#193495,#193496,#193497,#193498,#193499,#193500,
#193501,#193502),.UNSPECIFIED.,.F.,.F.,(4,3,3,3,3,3,3,3,3,3,3,3,3,3,3,3,
3,4),(0.,4.29652152145236E-5,8.44519107509453E-5,0.000123669830862064,0.00015978887735497,
0.000170558847912636,0.000181218775907175,0.00018196004645242,0.000214460062643987,
0.000244755726199668,0.000255838271868951,0.000258503253867586,0.000261084955178763,
0.000289370476647399,0.000301101325502015,0.000321109510663641,0.000331113603244453,
0.000341117695825266),.UNSPECIFIED.);
#4647=B_SPLINE_CURVE_WITH_KNOTS('',3,(#193504,#193505,#193506,#193507,#193508,
#193509,#193510,#193511,#193512,#193513,#193514,#193515,#193516,#193517,
#193518,#193519,#193520,#193521,#193522,#193523,#193524,#193525,#193526,
#193527,#193528,#193529,#193530,#193531,#193532,#193533,#193534,#193535,
#193536,#193537,#193538,#193539,#193540,#193541,#193542,#193543,#193544,
#193545,#193546,#193547,#193548,#193549,#193550,#193551,#193552,#193553,
#193554,#193555),.UNSPECIFIED.,.F.,.F.,(4,3,3,3,3,3,3,3,3,3,3,3,3,3,3,3,
3,4),(0.,4.30706237867132E-5,8.47417087692055E-5,0.000124159989205097,0.000160467076289105,
0.000170998382116699,0.00018241499473378,0.000213747977645872,0.000242415955902537,
0.000256497573175045,0.000259169422895618,0.000261757777312424,0.000289965130403846,
0.000301877270772907,0.000321937017503149,0.000326951954185709,0.00033447435920955,
0.000341996764233391),.UNSPECIFIED.);
#4648=B_SPLINE_CURVE_WITH_KNOTS('',3,(#193556,#193557,#193558,#193559,#193560,
#193561,#193562,#193563,#193564,#193565,#193566,#193567,#193568,#193569,
#193570,#193571,#193572,#193573,#193574,#193575,#193576,#193577,#193578,
#193579,#193580,#193581,#193582,#193583,#193584,#193585,#193586,#193587,
#193588,#193589,#193590,#193591,#193592,#193593,#193594,#193595,#193596,
#193597,#193598,#193599,#193600,#193601,#193602,#193603,#193604,#193605,
#193606,#193607),.UNSPECIFIED.,.F.,.F.,(4,3,3,3,3,3,3,3,3,3,3,3,3,3,3,3,
3,4),(0.,2.58457451670712E-5,4.25394446195834E-5,6.46659869687109E-5,7.57292581432746E-5,
8.12608937305565E-5,8.26438026273769E-5,8.67925293178383E-5,0.000116015624426661,
0.000130188793976757,0.000151886926306217,0.000161963651211276,0.000162735992470947,
0.000173585058635677,0.000212487880459323,0.000255238173507097,0.00030139776113686,
0.000347170117271366),.UNSPECIFIED.);
#4649=B_SPLINE_CURVE_WITH_KNOTS('',3,(#193609,#193610,#193611,#193612,#193613,
#193614,#193615,#193616,#193617,#193618,#193619,#193620,#193621,#193622,
#193623,#193624,#193625,#193626,#193627,#193628,#193629,#193630,#193631,
#193632,#193633,#193634,#193635,#193636,#193637,#193638,#193639,#193640,
#193641,#193642,#193643,#193644,#193645,#193646,#193647,#193648,#193649,
#193650,#193651,#193652,#193653,#193654),.UNSPECIFIED.,.F.,.F.,(4,3,3,3,
3,3,3,3,3,3,3,3,3,3,3,4),(0.,2.57218161984597E-5,4.21568322568931E-5,6.45873314617548E-5,
7.58025810641856E-5,8.1410205865401E-5,8.28121120657048E-5,8.70178306666164E-5,
0.000116081955658237,0.000130526745999925,0.000162394111022039,0.000174035661333233,
0.0002131383969588,0.000256116935434844,0.000302406662857505,0.000348071322666477),
 .UNSPECIFIED.);
#4650=B_SPLINE_CURVE_WITH_KNOTS('',3,(#193655,#193656,#193657,#193658,#193659,
#193660,#193661,#193662,#193663,#193664,#193665,#193666,#193667,#193668,
#193669,#193670,#193671,#193672,#193673,#193674,#193675,#193676,#193677,
#193678,#193679,#193680,#193681,#193682,#193683,#193684,#193685,#193686,
#193687,#193688,#193689,#193690,#193691,#193692,#193693,#193694,#193695,
#193696,#193697,#193698,#193699,#193700,#193701,#193702,#193703,#193704,
#193705,#193706),.UNSPECIFIED.,.F.,.F.,(4,3,3,3,3,3,3,3,3,3,3,3,3,3,3,3,
3,4),(0.,4.29652152191473E-5,8.44519107585247E-5,0.000123669830871658,0.000159788877366025,
0.000170558847912618,0.000181218775907159,0.0001819600464524,0.000214460062643458,
0.000244755726197822,0.000255838271868943,0.000258503253867578,0.000261084955178756,
0.000289370476647256,0.000301101325502011,0.000321109510663639,0.000331113603244453,
0.000341117695825267),.UNSPECIFIED.);
#4651=B_SPLINE_CURVE_WITH_KNOTS('',3,(#193708,#193709,#193710,#193711,#193712,
#193713,#193714,#193715,#193716,#193717,#193718,#193719,#193720,#193721,
#193722,#193723,#193724,#193725,#193726,#193727,#193728,#193729,#193730,
#193731,#193732,#193733,#193734,#193735,#193736,#193737,#193738,#193739,
#193740,#193741,#193742,#193743,#193744,#193745,#193746,#193747,#193748,
#193749,#193750,#193751,#193752,#193753,#193754,#193755,#193756,#193757,
#193758,#193759),.UNSPECIFIED.,.F.,.F.,(4,3,3,3,3,3,3,3,3,3,3,3,3,3,3,3,
3,4),(0.,4.30706237879909E-5,8.47417087713626E-5,0.000124159989208026,0.000160467076292825,
0.000170998382116693,0.000182414994733774,0.000213747977645869,0.000242415955903556,
0.000256497573175044,0.000259169422895617,0.000261757777312423,0.000289965130402278,
0.000301877270772909,0.000321937017503151,0.000326951954185712,0.000334474359209553,
0.000341996764233394),.UNSPECIFIED.);
#4652=B_SPLINE_CURVE_WITH_KNOTS('',3,(#193760,#193761,#193762,#193763,#193764,
#193765,#193766,#193767,#193768,#193769,#193770,#193771,#193772,#193773,
#193774,#193775,#193776,#193777,#193778,#193779,#193780,#193781,#193782,
#193783,#193784,#193785,#193786,#193787,#193788,#193789,#193790,#193791,
#193792,#193793,#193794,#193795,#193796,#193797,#193798,#193799,#193800,
#193801,#193802,#193803,#193804,#193805,#193806,#193807,#193808,#193809,
#193810,#193811),.UNSPECIFIED.,.F.,.F.,(4,3,3,3,3,3,3,3,3,3,3,3,3,3,3,3,
3,4),(0.,2.58457451684838E-5,4.25394446196393E-5,6.46659869687357E-5,7.5729258143284E-5,
8.12608937305581E-5,8.26438026273766E-5,8.67925293178322E-5,0.000116015624428102,
0.000130188793976748,0.000151886926306206,0.000161963651211262,0.000162735992470935,
0.000173585058635664,0.000212487880461562,0.000255238173513034,0.000301397761149555,
0.000347170117271345),.UNSPECIFIED.);
#4653=B_SPLINE_CURVE_WITH_KNOTS('',3,(#193813,#193814,#193815,#193816,#193817,
#193818,#193819,#193820,#193821,#193822,#193823,#193824,#193825,#193826,
#193827,#193828,#193829,#193830,#193831,#193832,#193833,#193834,#193835,
#193836,#193837,#193838,#193839,#193840,#193841,#193842,#193843,#193844,
#193845,#193846,#193847,#193848,#193849,#193850,#193851,#193852,#193853,
#193854,#193855,#193856,#193857,#193858),.UNSPECIFIED.,.F.,.F.,(4,3,3,3,
3,3,3,3,3,3,3,3,3,3,3,4),(0.,2.57218162004422E-5,4.21568322566571E-5,6.45873314616386E-5,
7.58025810641293E-5,8.14102058653747E-5,8.2812112065686E-5,8.701783066662E-5,
0.000116081955658433,0.00013052674599993,0.000162394111022039,0.00017403566133324,
0.000213138396960911,0.00025611693543884,0.00030240666286298,0.000348071322666468),
 .UNSPECIFIED.);
#4654=B_SPLINE_CURVE_WITH_KNOTS('',3,(#193859,#193860,#193861,#193862,#193863,
#193864,#193865,#193866,#193867,#193868,#193869,#193870,#193871,#193872,
#193873,#193874,#193875,#193876,#193877,#193878,#193879,#193880,#193881,
#193882,#193883,#193884,#193885,#193886,#193887,#193888,#193889,#193890,
#193891,#193892,#193893,#193894,#193895,#193896,#193897,#193898,#193899,
#193900,#193901,#193902,#193903,#193904,#193905,#193906,#193907,#193908,
#193909,#193910),.UNSPECIFIED.,.F.,.F.,(4,3,3,3,3,3,3,3,3,3,3,3,3,3,3,3,
3,4),(0.,4.2965215219619E-5,8.44519107588242E-5,0.000123669830871205,0.000159788877364292,
0.000170558847912618,0.000181218775907158,0.000181960046452387,0.000214460062643356,
0.000244755726198647,0.000255838271868941,0.000258503253867576,0.000261084955178754,
0.000289370476647944,0.000301101325502009,0.000321109510663637,0.00033111360324445,
0.000341117695825264),.UNSPECIFIED.);
#4655=B_SPLINE_CURVE_WITH_KNOTS('',3,(#193912,#193913,#193914,#193915,#193916,
#193917,#193918,#193919,#193920,#193921,#193922,#193923,#193924,#193925,
#193926,#193927,#193928,#193929,#193930,#193931,#193932,#193933,#193934,
#193935,#193936,#193937,#193938,#193939,#193940,#193941,#193942,#193943,
#193944,#193945,#193946,#193947,#193948,#193949,#193950,#193951,#193952,
#193953,#193954,#193955,#193956,#193957,#193958,#193959,#193960,#193961,
#193962,#193963),.UNSPECIFIED.,.F.,.F.,(4,3,3,3,3,3,3,3,3,3,3,3,3,3,3,3,
3,4),(0.,4.30706237860952E-5,8.47417087682543E-5,0.000124159989203998,0.000160467076288037,
0.000170998382116714,0.000182414994733819,0.000213747977645884,0.000242415955903088,
0.000256497573175054,0.000259169422895627,0.000261757777312432,0.00028996513040302,
0.000301877270772912,0.000321937017503153,0.000326951954185713,0.000334474359209553,
0.000341996764233393),.UNSPECIFIED.);
#4656=B_SPLINE_CURVE_WITH_KNOTS('',3,(#193964,#193965,#193966,#193967,#193968,
#193969,#193970,#193971,#193972,#193973,#193974,#193975,#193976,#193977,
#193978,#193979,#193980,#193981,#193982,#193983,#193984,#193985,#193986,
#193987,#193988,#193989,#193990,#193991,#193992,#193993,#193994,#193995,
#193996,#193997,#193998,#193999,#194000,#194001,#194002,#194003,#194004,
#194005,#194006,#194007,#194008,#194009,#194010,#194011,#194012,#194013,
#194014,#194015),.UNSPECIFIED.,.F.,.F.,(4,3,3,3,3,3,3,3,3,3,3,3,3,3,3,3,
3,4),(0.,2.58457451687623E-5,4.25394446196227E-5,6.46659869687286E-5,7.57292581432816E-5,
8.12608937305581E-5,8.26438026273772E-5,8.67925293178346E-5,0.000116015624427777,
0.000130188793976752,0.000151886926306211,0.000161963651211265,0.00016273599247094,
0.000173585058635669,0.000212487880462122,0.000255238173513666,0.000301397761149318,
0.000347170117271352),.UNSPECIFIED.);
#4657=B_SPLINE_CURVE_WITH_KNOTS('',3,(#194017,#194018,#194019,#194020,#194021,
#194022,#194023,#194024,#194025,#194026,#194027,#194028,#194029,#194030,
#194031,#194032,#194033,#194034,#194035,#194036,#194037,#194038,#194039,
#194040,#194041,#194042,#194043,#194044,#194045,#194046,#194047,#194048,
#194049,#194050,#194051,#194052,#194053,#194054,#194055,#194056,#194057,
#194058,#194059,#194060,#194061,#194062),.UNSPECIFIED.,.F.,.F.,(4,3,3,3,
3,3,3,3,3,3,3,3,3,3,3,4),(0.,2.57218161985908E-5,4.21568322566518E-5,6.45873314616328E-5,
7.58025810641234E-5,8.14102058653686E-5,8.28121120656799E-5,8.70178306666139E-5,
0.000116081955657255,0.000130526745999921,0.000162394111022039,0.000174035661333228,
0.000213138396959342,0.000256116935435933,0.000302406662859232,0.000348071322666485),
 .UNSPECIFIED.);
#4658=B_SPLINE_CURVE_WITH_KNOTS('',3,(#194063,#194064,#194065,#194066,#194067,
#194068,#194069,#194070,#194071,#194072,#194073,#194074,#194075,#194076,
#194077,#194078,#194079,#194080,#194081,#194082,#194083,#194084,#194085,
#194086,#194087,#194088,#194089,#194090,#194091,#194092,#194093,#194094,
#194095,#194096,#194097,#194098,#194099,#194100,#194101,#194102,#194103,
#194104,#194105,#194106,#194107,#194108,#194109,#194110,#194111,#194112,
#194113,#194114),.UNSPECIFIED.,.F.,.F.,(4,3,3,3,3,3,3,3,3,3,3,3,3,3,3,3,
3,4),(0.,4.29652152172666E-5,8.44519107551468E-5,0.000123669830866818,0.000159788877359668,
0.000170558847912628,0.000181218775907168,0.000181960046452396,0.000214460062643525,
0.000244755726198588,0.000255838271868947,0.000258503253867582,0.00026108495517876,
0.000289370476648551,0.000301101325502014,0.000321109510663641,0.000331113603244454,
0.000341117695825267),.UNSPECIFIED.);
#4659=B_SPLINE_CURVE_WITH_KNOTS('',3,(#194116,#194117,#194118,#194119,#194120,
#194121,#194122,#194123,#194124,#194125,#194126,#194127,#194128,#194129,
#194130,#194131,#194132,#194133,#194134,#194135,#194136,#194137,#194138,
#194139,#194140,#194141,#194142,#194143,#194144,#194145,#194146,#194147,
#194148,#194149,#194150,#194151,#194152,#194153,#194154,#194155,#194156,
#194157,#194158,#194159,#194160,#194161,#194162,#194163,#194164,#194165,
#194166,#194167),.UNSPECIFIED.,.F.,.F.,(4,3,3,3,3,3,3,3,3,3,3,3,3,3,3,3,
3,4),(3.46944695195361E-18,4.30706237857577E-5,8.4741708767591E-5,0.000124159989202823,
0.000160467076286219,0.000170998382116696,0.000182414994733758,0.00021374797764587,
0.000242415955904134,0.000256497573175044,0.000259169422895617,0.000261757777312423,
0.000289965130402185,0.000301877270772907,0.00032193701750315,0.00032695195418571,
0.000334474359209551,0.000341996764233392),.UNSPECIFIED.);
#4660=B_SPLINE_CURVE_WITH_KNOTS('',3,(#194168,#194169,#194170,#194171,#194172,
#194173,#194174,#194175,#194176,#194177,#194178,#194179,#194180,#194181,
#194182,#194183,#194184,#194185,#194186,#194187,#194188,#194189,#194190,
#194191,#194192,#194193,#194194,#194195,#194196,#194197,#194198,#194199,
#194200,#194201,#194202,#194203,#194204,#194205,#194206,#194207,#194208,
#194209,#194210,#194211,#194212,#194213,#194214,#194215,#194216,#194217,
#194218,#194219),.UNSPECIFIED.,.F.,.F.,(4,3,3,3,3,3,3,3,3,3,3,3,3,3,3,3,
3,4),(0.,2.58457451699863E-5,4.25394446196659E-5,6.46659869687493E-5,7.5729258143291E-5,
8.12608937305619E-5,8.26438026273796E-5,8.67925293178327E-5,0.000116015624429004,
0.000130188793976749,0.000151886926306207,0.000161963651211244,0.000162735992470936,
0.000173585058635665,0.000212487880462874,0.000255238173516106,0.000301397761155294,
0.00034717011727135),.UNSPECIFIED.);
#4661=B_SPLINE_CURVE_WITH_KNOTS('',3,(#194221,#194222,#194223,#194224,#194225,
#194226,#194227,#194228,#194229,#194230,#194231,#194232,#194233,#194234,
#194235,#194236,#194237,#194238,#194239,#194240,#194241,#194242,#194243,
#194244,#194245,#194246,#194247,#194248,#194249,#194250,#194251,#194252,
#194253,#194254,#194255,#194256,#194257,#194258,#194259,#194260,#194261,
#194262,#194263,#194264,#194265,#194266),.UNSPECIFIED.,.F.,.F.,(4,3,3,3,
3,3,3,3,3,3,3,3,3,3,3,4),(3.46944695195361E-18,2.57218161988661E-5,4.21568322568949E-5,
6.45873314617574E-5,7.58025810641886E-5,8.14102058654043E-5,8.28121120657082E-5,
8.70178306666199E-5,0.000116081955658138,0.000130526745999928,0.000162394111022053,
0.000174035661333236,0.000213138396955745,0.000256116935428962,0.000302406662849146,
0.000348071322666463),.UNSPECIFIED.);
#4662=B_SPLINE_CURVE_WITH_KNOTS('',3,(#194267,#194268,#194269,#194270,#194271,
#194272,#194273,#194274,#194275,#194276,#194277,#194278,#194279,#194280,
#194281,#194282,#194283,#194284,#194285,#194286,#194287,#194288,#194289,
#194290,#194291,#194292,#194293,#194294,#194295,#194296,#194297,#194298,
#194299,#194300,#194301,#194302,#194303,#194304,#194305,#194306,#194307,
#194308,#194309,#194310,#194311,#194312,#194313,#194314,#194315,#194316,
#194317,#194318),.UNSPECIFIED.,.F.,.F.,(4,3,3,3,3,3,3,3,3,3,3,3,3,3,3,3,
3,4),(0.,4.29652152205376E-5,8.44519107610295E-5,0.000123669830875294,0.000159788877370972,
0.000170558847912616,0.000181218775907156,0.000181960046452398,0.000214460062644455,
0.000244755726200831,0.000255838271868934,0.000258503253867569,0.000261084955178747,
0.000289370476647454,0.000301101325502,0.000321109510663626,0.000331113603244439,
0.000341117695825252),.UNSPECIFIED.);
#4663=B_SPLINE_CURVE_WITH_KNOTS('',3,(#194320,#194321,#194322,#194323,#194324,
#194325,#194326,#194327,#194328,#194329,#194330,#194331,#194332,#194333,
#194334,#194335,#194336,#194337,#194338,#194339,#194340,#194341,#194342,
#194343,#194344,#194345,#194346,#194347,#194348,#194349,#194350,#194351,
#194352,#194353,#194354,#194355,#194356,#194357,#194358,#194359,#194360,
#194361,#194362,#194363,#194364,#194365,#194366,#194367,#194368,#194369,
#194370,#194371),.UNSPECIFIED.,.F.,.F.,(4,3,3,3,3,3,3,3,3,3,3,3,3,3,3,3,
3,4),(0.,4.30706237863112E-5,8.47417087684205E-5,0.000124159989203888,0.000160467076287372,
0.000170998382116698,0.00018241499473378,0.000213747977645872,0.000242415955903452,
0.000256497573175046,0.000259169422895619,0.000261757777312424,0.000289965130402983,
0.000301877270772909,0.000321937017503151,0.000326951954185711,0.000334474359209552,
0.000341996764233393),.UNSPECIFIED.);
#4664=B_SPLINE_CURVE_WITH_KNOTS('',3,(#194372,#194373,#194374,#194375,#194376,
#194377,#194378,#194379,#194380,#194381,#194382,#194383,#194384,#194385,
#194386,#194387,#194388,#194389,#194390,#194391,#194392,#194393,#194394,
#194395,#194396,#194397,#194398,#194399,#194400,#194401,#194402,#194403,
#194404,#194405,#194406,#194407,#194408,#194409,#194410,#194411,#194412,
#194413,#194414,#194415,#194416,#194417,#194418,#194419,#194420,#194421,
#194422,#194423),.UNSPECIFIED.,.F.,.F.,(4,3,3,3,3,3,3,3,3,3,3,3,3,3,3,3,
3,4),(3.46944695195361E-18,2.5845745168372E-5,4.25394446194478E-5,6.46659869686474E-5,
7.57292581432472E-5,8.12608937305471E-5,8.26438026273721E-5,8.6792529317847E-5,
0.000116015624428185,0.000130188793976769,0.00015188692630623,0.000161963651211288,
0.00016273599247096,0.000173585058635691,0.000212487880457827,0.000255238173505098,
0.000301397761135908,0.000347170117271362),.UNSPECIFIED.);
#4665=B_SPLINE_CURVE_WITH_KNOTS('',3,(#194425,#194426,#194427,#194428,#194429,
#194430,#194431,#194432,#194433,#194434,#194435,#194436,#194437,#194438,
#194439,#194440,#194441,#194442,#194443,#194444,#194445,#194446,#194447,
#194448,#194449,#194450,#194451,#194452,#194453,#194454,#194455,#194456,
#194457,#194458,#194459,#194460,#194461,#194462,#194463,#194464,#194465,
#194466,#194467,#194468,#194469,#194470),.UNSPECIFIED.,.F.,.F.,(4,3,3,3,
3,3,3,3,3,3,3,3,3,3,3,4),(3.46944695195361E-18,2.57218161998776E-5,4.21568322567625E-5,
6.45873314616899E-5,7.58025810641537E-5,8.14102058653855E-5,8.28121120656935E-5,
8.70178306666174E-5,0.000116081955658038,0.000130526745999924,0.000162394111022039,
0.000174035661333231,0.000213138396958318,0.000256116935433942,0.00030240666285635,
0.000348071322666463),.UNSPECIFIED.);
#4666=B_SPLINE_CURVE_WITH_KNOTS('',3,(#194471,#194472,#194473,#194474,#194475,
#194476,#194477,#194478,#194479,#194480,#194481,#194482,#194483,#194484,
#194485,#194486,#194487,#194488,#194489,#194490,#194491,#194492,#194493,
#194494,#194495,#194496,#194497,#194498,#194499,#194500,#194501,#194502,
#194503,#194504,#194505,#194506,#194507,#194508,#194509,#194510,#194511,
#194512,#194513,#194514,#194515,#194516,#194517,#194518,#194519,#194520,
#194521,#194522),.UNSPECIFIED.,.F.,.F.,(4,3,3,3,3,3,3,3,3,3,3,3,3,3,3,3,
3,4),(0.,4.29652152155444E-5,8.44519107519921E-5,0.000123669830862218,0.000159788877353411,
0.000170558847912627,0.000181218775907166,0.0001819600464524,0.000214460062643083,
0.00024475572619671,0.000255838271868938,0.000258503253867573,0.00026108495517875,
0.000289370476649592,0.000301101325502,0.000321109510663625,0.000331113603244437,
0.00034111769582525),.UNSPECIFIED.);
#4667=B_SPLINE_CURVE_WITH_KNOTS('',3,(#194524,#194525,#194526,#194527,#194528,
#194529,#194530,#194531,#194532,#194533,#194534,#194535,#194536,#194537,
#194538,#194539,#194540,#194541,#194542,#194543,#194544,#194545,#194546,
#194547,#194548,#194549,#194550,#194551,#194552,#194553,#194554,#194555,
#194556,#194557,#194558,#194559,#194560,#194561,#194562,#194563,#194564,
#194565,#194566,#194567,#194568,#194569,#194570,#194571,#194572,#194573,
#194574,#194575),.UNSPECIFIED.,.F.,.F.,(4,3,3,3,3,3,3,3,3,3,3,3,3,3,3,3,
3,4),(1.04083408558608E-17,4.30706237864328E-5,8.47417087688249E-5,0.000124159989204731,
0.000160467076288871,0.000170998382116696,0.00018241499473378,0.00021374797764587,
0.000242415955903496,0.000256497573175044,0.000259169422895617,0.000261757777312422,
0.000289965130403092,0.000301877270772907,0.000321937017503149,0.000326951954185709,
0.00033447435920955,0.000341996764233391),.UNSPECIFIED.);
#4668=B_SPLINE_CURVE_WITH_KNOTS('',3,(#194576,#194577,#194578,#194579,#194580,
#194581,#194582,#194583,#194584,#194585,#194586,#194587,#194588,#194589,
#194590,#194591,#194592,#194593,#194594,#194595,#194596,#194597,#194598,
#194599,#194600,#194601,#194602,#194603,#194604,#194605,#194606,#194607,
#194608,#194609,#194610,#194611,#194612,#194613,#194614,#194615,#194616,
#194617,#194618,#194619,#194620,#194621,#194622,#194623,#194624,#194625,
#194626,#194627),.UNSPECIFIED.,.F.,.F.,(4,3,3,3,3,3,3,3,3,3,3,3,3,3,3,3,
3,4),(1.73472347597681E-18,2.58457451674207E-5,4.25394446196043E-5,6.46659869687212E-5,
7.57292581432797E-5,8.12608937305589E-5,8.26438026273787E-5,8.67925293178381E-5,
0.000116015624426875,0.000130188793976756,0.000151886926306215,0.000161963651211264,
0.000162735992470945,0.000173585058635675,0.000212487880460368,0.000255238173510853,
0.000301397761146635,0.000347170117271375),.UNSPECIFIED.);
#4669=B_SPLINE_CURVE_WITH_KNOTS('',3,(#194629,#194630,#194631,#194632,#194633,
#194634,#194635,#194636,#194637,#194638,#194639,#194640,#194641,#194642,
#194643,#194644,#194645,#194646,#194647,#194648,#194649,#194650,#194651,
#194652,#194653,#194654,#194655,#194656,#194657,#194658,#194659,#194660,
#194661,#194662,#194663,#194664,#194665,#194666,#194667,#194668,#194669,
#194670,#194671,#194672,#194673,#194674),.UNSPECIFIED.,.F.,.F.,(4,3,3,3,
3,3,3,3,3,3,3,3,3,3,3,4),(0.,2.57218161994108E-5,4.21568322568941E-5,6.45873314617598E-5,
7.58025810641926E-5,8.14102058654091E-5,8.28121120657132E-5,8.70178306666255E-5,
0.000116081955658529,0.000130526745999938,0.000162394111022068,0.000174035661333251,
0.000213138396959093,0.000256116935435327,0.000302406662857997,0.000348071322666476),
 .UNSPECIFIED.);
#4670=B_SPLINE_CURVE_WITH_KNOTS('',3,(#194675,#194676,#194677,#194678,#194679,
#194680,#194681,#194682,#194683,#194684,#194685,#194686,#194687,#194688,
#194689,#194690,#194691,#194692,#194693,#194694,#194695,#194696,#194697,
#194698,#194699,#194700,#194701,#194702,#194703,#194704,#194705,#194706,
#194707,#194708,#194709,#194710,#194711,#194712,#194713,#194714,#194715,
#194716,#194717,#194718,#194719,#194720,#194721,#194722,#194723,#194724,
#194725,#194726),.UNSPECIFIED.,.F.,.F.,(4,3,3,3,3,3,3,3,3,3,3,3,3,3,3,3,
3,4),(0.,4.296521521763E-5,8.44519107554871E-5,0.000123669830866643,0.000159788877358575,
0.000170558847912618,0.000181218775907158,0.000181960046452402,0.000214460062644093,
0.00024475572619934,0.00025583827186894,0.000258503253867575,0.000261084955178753,
0.000289370476647943,0.000301101325502008,0.000321109510663635,0.000331113603244448,
0.000341117695825262),.UNSPECIFIED.);
#4671=B_SPLINE_CURVE_WITH_KNOTS('',3,(#194728,#194729,#194730,#194731,#194732,
#194733,#194734,#194735,#194736,#194737,#194738,#194739,#194740,#194741,
#194742,#194743,#194744,#194745,#194746,#194747,#194748,#194749,#194750,
#194751,#194752,#194753,#194754,#194755,#194756,#194757,#194758,#194759,
#194760,#194761,#194762,#194763,#194764,#194765,#194766,#194767,#194768,
#194769,#194770,#194771,#194772,#194773,#194774,#194775,#194776,#194777,
#194778,#194779),.UNSPECIFIED.,.F.,.F.,(4,3,3,3,3,3,3,3,3,3,3,3,3,3,3,3,
3,4),(9.96522768216898E-18,4.30706237863075E-5,8.47417087683585E-5,0.000124159989203683,
0.000160467076287053,0.000170998382116712,0.000182414994733787,0.000213747977645881,
0.000242415955903098,0.000256497573175051,0.000259169422895624,0.000261757777312429,
0.000289965130403181,0.000301877270772909,0.00032193701750315,0.00032695195418571,
0.00033447435920955,0.00034199676423339),.UNSPECIFIED.);
#4672=B_SPLINE_CURVE_WITH_KNOTS('',3,(#194780,#194781,#194782,#194783,#194784,
#194785,#194786,#194787,#194788,#194789,#194790,#194791,#194792,#194793,
#194794,#194795,#194796,#194797,#194798,#194799,#194800,#194801,#194802,
#194803,#194804,#194805,#194806,#194807,#194808,#194809,#194810,#194811,
#194812,#194813,#194814,#194815,#194816,#194817,#194818,#194819,#194820,
#194821,#194822,#194823,#194824,#194825,#194826,#194827,#194828,#194829,
#194830,#194831),.UNSPECIFIED.,.F.,.F.,(4,3,3,3,3,3,3,3,3,3,3,3,3,3,3,3,
3,4),(0.,2.58457451687118E-5,4.25394446195713E-5,6.46659869687085E-5,7.57292581432772E-5,
8.12608937305615E-5,8.26438026273826E-5,8.67925293178458E-5,0.000116015624427385,
0.000130188793976769,0.00015188692630623,0.000161963651211277,0.000162735992470961,
0.000173585058635692,0.000212487880461626,0.00025523817351366,0.000301397761151513,
0.000347170117271372),.UNSPECIFIED.);
#4673=B_SPLINE_CURVE_WITH_KNOTS('',3,(#194833,#194834,#194835,#194836,#194837,
#194838,#194839,#194840,#194841,#194842,#194843,#194844,#194845,#194846,
#194847,#194848,#194849,#194850,#194851,#194852,#194853,#194854,#194855,
#194856,#194857,#194858,#194859,#194860,#194861,#194862,#194863,#194864,
#194865,#194866,#194867,#194868,#194869,#194870,#194871,#194872,#194873,
#194874,#194875,#194876,#194877,#194878),.UNSPECIFIED.,.F.,.F.,(4,3,3,3,
3,3,3,3,3,3,3,3,3,3,3,4),(8.67361737988404E-19,2.57218161993721E-5,4.21568322568887E-5,
6.45873314617549E-5,7.5802581064188E-5,8.14102058654046E-5,8.28121120657087E-5,
8.70178306666211E-5,0.000116081955659502,0.000130526745999931,0.000162394111022061,
0.000174035661333241,0.000213138396957143,0.000256116935431465,0.000302406662852055,
0.000348071322666494),.UNSPECIFIED.);
#4674=B_SPLINE_CURVE_WITH_KNOTS('',3,(#194879,#194880,#194881,#194882,#194883,
#194884,#194885,#194886,#194887,#194888,#194889,#194890,#194891,#194892,
#194893,#194894,#194895,#194896,#194897,#194898,#194899,#194900,#194901,
#194902,#194903,#194904,#194905,#194906,#194907,#194908,#194909,#194910,
#194911,#194912,#194913,#194914,#194915,#194916,#194917,#194918,#194919,
#194920,#194921,#194922,#194923,#194924,#194925,#194926,#194927,#194928,
#194929,#194930),.UNSPECIFIED.,.F.,.F.,(4,3,3,3,3,3,3,3,3,3,3,3,3,3,3,3,
3,4),(0.,4.2965215213771E-5,8.44519107494884E-5,0.000123669830859856,0.000159788877351868,
0.000170558847912631,0.00018121877590717,0.000181960046452402,0.000214460062643814,
0.000244755726199141,0.000255838271868941,0.000258503253867576,0.000261084955178753,
0.000289370476648063,0.000301101325502002,0.000321109510663626,0.000331113603244439,
0.000341117695825251),.UNSPECIFIED.);
#4675=B_SPLINE_CURVE_WITH_KNOTS('',3,(#194932,#194933,#194934,#194935,#194936,
#194937,#194938,#194939,#194940,#194941,#194942,#194943,#194944,#194945,
#194946,#194947,#194948,#194949,#194950,#194951,#194952,#194953,#194954,
#194955,#194956,#194957,#194958,#194959,#194960,#194961,#194962,#194963,
#194964,#194965,#194966,#194967,#194968,#194969,#194970,#194971,#194972,
#194973,#194974,#194975,#194976,#194977,#194978,#194979,#194980,#194981,
#194982,#194983),.UNSPECIFIED.,.F.,.F.,(4,3,3,3,3,3,3,3,3,3,3,3,3,3,3,3,
3,4),(5.96311194867027E-19,4.30706237866237E-5,8.47417087690704E-5,0.0001241599892049,
0.000160467076288867,0.000170998382116678,0.000182414994733734,0.000213747977645854,
0.000242415955902605,0.00025649757317503,0.000259169422895604,0.000261757777312409,
0.000289965130403055,0.000301877270772896,0.000321937017503139,0.0003269519541857,
0.000334474359209541,0.000341996764233382),.UNSPECIFIED.);
#4676=B_SPLINE_CURVE_WITH_KNOTS('',3,(#194984,#194985,#194986,#194987,#194988,
#194989,#194990,#194991,#194992,#194993,#194994,#194995,#194996,#194997,
#194998,#194999,#195000,#195001,#195002,#195003,#195004,#195005,#195006,
#195007,#195008,#195009,#195010,#195011,#195012,#195013,#195014,#195015,
#195016,#195017,#195018,#195019,#195020,#195021,#195022,#195023,#195024,
#195025,#195026,#195027,#195028,#195029,#195030,#195031,#195032,#195033,
#195034,#195035),.UNSPECIFIED.,.F.,.F.,(4,3,3,3,3,3,3,3,3,3,3,3,3,3,3,3,
3,4),(0.,2.58457451671235E-5,4.25394446195251E-5,6.46659869686816E-5,7.57292581432598E-5,
8.12608937305489E-5,8.26438026273711E-5,8.6792529317838E-5,0.000116015624427186,
0.000130188793976757,0.000151886926306216,0.000161963651211284,0.000162735992470946,
0.000173585058635676,0.000212487880462066,0.000255238173513635,0.000301397761149358,
0.000347170117271353),.UNSPECIFIED.);
#4677=B_SPLINE_CURVE_WITH_KNOTS('',3,(#195037,#195038,#195039,#195040,#195041,
#195042,#195043,#195044,#195045,#195046,#195047,#195048,#195049,#195050,
#195051,#195052,#195053,#195054,#195055,#195056,#195057,#195058,#195059,
#195060,#195061,#195062,#195063,#195064,#195065,#195066,#195067,#195068,
#195069,#195070,#195071,#195072,#195073,#195074,#195075,#195076,#195077,
#195078,#195079,#195080,#195081,#195082),.UNSPECIFIED.,.F.,.F.,(4,3,3,3,
3,3,3,3,3,3,3,3,3,3,3,4),(2.74438674910393E-19,2.57218161990037E-5,4.21568322568875E-5,
6.45873314617528E-5,7.58025810641855E-5,8.14102058654018E-5,8.28121120657059E-5,
8.70178306666182E-5,0.000116081955659215,0.000130526745999927,0.000162394111022046,
0.000174035661333236,0.000213138396958664,0.000256116935434767,0.000302406662858074,
0.000348071322666484),.UNSPECIFIED.);
#4678=B_SPLINE_CURVE_WITH_KNOTS('',3,(#195083,#195084,#195085,#195086,#195087,
#195088,#195089,#195090,#195091,#195092,#195093,#195094,#195095,#195096,
#195097,#195098,#195099,#195100,#195101,#195102,#195103,#195104,#195105,
#195106,#195107,#195108,#195109,#195110,#195111,#195112,#195113,#195114,
#195115,#195116,#195117,#195118,#195119,#195120,#195121,#195122,#195123,
#195124,#195125,#195126,#195127,#195128,#195129,#195130,#195131,#195132,
#195133,#195134),.UNSPECIFIED.,.F.,.F.,(4,3,3,3,3,3,3,3,3,3,3,3,3,3,3,3,
3,4),(0.,4.29652152166783E-5,8.44519107543665E-5,0.000123669830866176,0.000159788877359447,
0.000170558847912639,0.000181218775907178,0.000181960046452414,0.000214460062643347,
0.000244755726197935,0.000255838271868953,0.000258503253867587,0.000261084955178765,
0.000289370476648123,0.000301101325502015,0.000321109510663641,0.000331113603244453,
0.000341117695825266),.UNSPECIFIED.);
#4679=B_SPLINE_CURVE_WITH_KNOTS('',3,(#195136,#195137,#195138,#195139,#195140,
#195141,#195142,#195143,#195144,#195145,#195146,#195147,#195148,#195149,
#195150,#195151,#195152,#195153,#195154,#195155,#195156,#195157,#195158,
#195159,#195160,#195161,#195162,#195163,#195164,#195165,#195166,#195167,
#195168,#195169,#195170,#195171,#195172,#195173,#195174,#195175,#195176,
#195177,#195178,#195179,#195180,#195181,#195182,#195183,#195184,#195185,
#195186,#195187),.UNSPECIFIED.,.F.,.F.,(4,3,3,3,3,3,3,3,3,3,3,3,3,3,3,3,
3,4),(0.,4.30706237874845E-5,8.47417087706428E-5,0.00012415998920723,0.000160467076292075,
0.000170998382116687,0.000182414994733767,0.000213747977645861,0.000242415955902588,
0.000256497573175036,0.000259169422895609,0.000261757777312415,0.000289965130404048,
0.0003018772707729,0.000321937017503143,0.000326951954185703,0.000334474359209544,
0.000341996764233385),.UNSPECIFIED.);
#4680=B_SPLINE_CURVE_WITH_KNOTS('',3,(#195188,#195189,#195190,#195191,#195192,
#195193,#195194,#195195,#195196,#195197,#195198,#195199,#195200,#195201,
#195202,#195203,#195204,#195205,#195206,#195207,#195208,#195209,#195210,
#195211,#195212,#195213,#195214,#195215,#195216,#195217,#195218,#195219,
#195220,#195221,#195222,#195223,#195224,#195225,#195226,#195227,#195228,
#195229,#195230,#195231,#195232,#195233,#195234,#195235,#195236,#195237,
#195238,#195239),.UNSPECIFIED.,.F.,.F.,(4,3,3,3,3,3,3,3,3,3,3,3,3,3,3,3,
3,4),(0.,2.58457451673457E-5,4.2539444619484E-5,6.46659869686634E-5,7.57292581432531E-5,
8.1260893730548E-5,8.26438026273717E-5,8.67925293178428E-5,0.000116015624427219,
0.000130188793976764,0.000151886926306225,0.000161963651211282,0.000162735992470955,
0.000173585058635686,0.000212487880462819,0.000255238173516115,0.000301397761155885,
0.000347170117271382),.UNSPECIFIED.);
#4681=B_SPLINE_CURVE_WITH_KNOTS('',3,(#195241,#195242,#195243,#195244,#195245,
#195246,#195247,#195248,#195249,#195250,#195251,#195252,#195253,#195254,
#195255,#195256,#195257,#195258,#195259,#195260,#195261,#195262,#195263,
#195264,#195265,#195266,#195267,#195268,#195269,#195270,#195271,#195272,
#195273,#195274,#195275,#195276,#195277,#195278,#195279,#195280,#195281,
#195282,#195283,#195284,#195285,#195286),.UNSPECIFIED.,.F.,.F.,(4,3,3,3,
3,3,3,3,3,3,3,3,3,3,3,4),(8.67361737988404E-19,2.57218161990736E-5,4.21568322568542E-5,
6.45873314617417E-5,7.58025810641855E-5,8.14102058654074E-5,8.28121120657128E-5,
8.70178306666293E-5,0.00011608195565874,0.000130526745999943,0.00016239411102208,
0.000174035661333258,0.000213138396959731,0.000256116935436739,0.000302406662860658,
0.000348071322666488),.UNSPECIFIED.);
#4682=B_SPLINE_CURVE_WITH_KNOTS('',3,(#195287,#195288,#195289,#195290,#195291,
#195292,#195293,#195294,#195295,#195296,#195297,#195298,#195299,#195300,
#195301,#195302,#195303,#195304,#195305,#195306,#195307,#195308,#195309,
#195310,#195311,#195312,#195313,#195314,#195315,#195316,#195317,#195318,
#195319,#195320,#195321,#195322,#195323,#195324,#195325,#195326,#195327,
#195328,#195329,#195330,#195331,#195332,#195333,#195334,#195335,#195336,
#195337,#195338),.UNSPECIFIED.,.F.,.F.,(4,3,3,3,3,3,3,3,3,3,3,3,3,3,3,3,
3,4),(0.,4.29652152202833E-5,8.44519107603119E-5,0.000123669830873692,0.000159788877368183,
0.000170558847912632,0.000181218775907171,0.000181960046452397,0.000214460062643704,
0.00024475572619857,0.000255838271868947,0.000258503253867581,0.000261084955178759,
0.000289370476647362,0.00030110132550201,0.000321109510663636,0.000331113603244449,
0.000341117695825261),.UNSPECIFIED.);
#4683=B_SPLINE_CURVE_WITH_KNOTS('',3,(#195340,#195341,#195342,#195343,#195344,
#195345,#195346,#195347,#195348,#195349,#195350,#195351,#195352,#195353,
#195354,#195355,#195356,#195357,#195358,#195359,#195360,#195361,#195362,
#195363,#195364,#195365,#195366,#195367,#195368,#195369,#195370,#195371,
#195372,#195373,#195374,#195375,#195376,#195377,#195378,#195379,#195380,
#195381,#195382,#195383,#195384,#195385,#195386,#195387,#195388,#195389,
#195390,#195391),.UNSPECIFIED.,.F.,.F.,(4,3,3,3,3,3,3,3,3,3,3,3,3,3,3,3,
3,4),(0.,4.30706237877163E-5,8.47417087709679E-5,0.000124159989207455,0.000160467076292245,
0.000170998382116692,0.000182414994733783,0.000213747977645868,0.000242415955903003,
0.000256497573175044,0.000259169422895617,0.000261757777312423,0.00028996513040353,
0.000301877270772909,0.000321937017503152,0.000326951954185713,0.000334474359209554,
0.000341996764233395),.UNSPECIFIED.);
#4684=B_SPLINE_CURVE_WITH_KNOTS('',3,(#195392,#195393,#195394,#195395,#195396,
#195397,#195398,#195399,#195400,#195401,#195402,#195403,#195404,#195405,
#195406,#195407,#195408,#195409,#195410,#195411,#195412,#195413,#195414,
#195415,#195416,#195417,#195418,#195419,#195420,#195421,#195422,#195423,
#195424,#195425,#195426,#195427,#195428,#195429,#195430,#195431,#195432,
#195433,#195434,#195435,#195436,#195437,#195438,#195439,#195440,#195441,
#195442,#195443),.UNSPECIFIED.,.F.,.F.,(4,3,3,3,3,3,3,3,3,3,3,3,3,3,3,3,
3,4),(0.,2.58457451689302E-5,4.25394446195954E-5,6.46659869687191E-5,7.57292581432809E-5,
8.12608937305618E-5,8.26438026273821E-5,8.67925293178427E-5,0.000116015624427155,
0.000130188793976764,0.000151886926306225,0.000161963651211299,0.000162735992470955,
0.000173585058635685,0.000212487880459557,0.000255238173508823,0.000301397761142415,
0.000347170117271368),.UNSPECIFIED.);
#4685=B_SPLINE_CURVE_WITH_KNOTS('',3,(#195445,#195446,#195447,#195448,#195449,
#195450,#195451,#195452,#195453,#195454,#195455,#195456,#195457,#195458,
#195459,#195460,#195461,#195462,#195463,#195464,#195465,#195466,#195467,
#195468,#195469,#195470,#195471,#195472,#195473,#195474,#195475,#195476,
#195477,#195478,#195479,#195480,#195481,#195482,#195483,#195484,#195485,
#195486,#195487,#195488,#195489,#195490),.UNSPECIFIED.,.F.,.F.,(4,3,3,3,
3,3,3,3,3,3,3,3,3,3,3,4),(0.,2.57218161989687E-5,4.21568322569323E-5,6.45873314617774E-5,
7.58025810641999E-5,8.14102058654112E-5,8.2812112065714E-5,8.70178306666224E-5,
0.000116081955658865,0.000130526745999934,0.000162394111022051,0.000174035661333245,
0.000213138396958673,0.000256116935434495,0.000302406662856898,0.000348071322666492),
 .UNSPECIFIED.);
#4686=B_SPLINE_CURVE_WITH_KNOTS('',3,(#195491,#195492,#195493,#195494,#195495,
#195496,#195497,#195498,#195499,#195500,#195501,#195502,#195503,#195504,
#195505,#195506,#195507,#195508,#195509,#195510,#195511,#195512,#195513,
#195514,#195515,#195516,#195517,#195518,#195519,#195520,#195521,#195522,
#195523,#195524,#195525,#195526,#195527,#195528,#195529,#195530,#195531,
#195532,#195533,#195534,#195535,#195536,#195537,#195538,#195539,#195540,
#195541,#195542),.UNSPECIFIED.,.F.,.F.,(4,3,3,3,3,3,3,3,3,3,3,3,3,3,3,3,
3,4),(0.,4.29652152166048E-5,8.44519107542708E-5,0.000123669830866133,0.000159788877359471,
0.000170558847912629,0.000181218775907169,0.000181960046452409,0.00021446006264399,
0.000244755726199507,0.000255838271868949,0.000258503253867584,0.000261084955178761,
0.000289370476647456,0.000301101325502015,0.000321109510663642,0.000331113603244455,
0.000341117695825268),.UNSPECIFIED.);
#4687=B_SPLINE_CURVE_WITH_KNOTS('',3,(#195544,#195545,#195546,#195547,#195548,
#195549,#195550,#195551,#195552,#195553,#195554,#195555,#195556,#195557,
#195558,#195559,#195560,#195561,#195562,#195563,#195564,#195565,#195566,
#195567,#195568,#195569,#195570,#195571,#195572,#195573,#195574,#195575,
#195576,#195577,#195578,#195579,#195580,#195581,#195582,#195583,#195584,
#195585,#195586,#195587,#195588,#195589,#195590,#195591,#195592,#195593,
#195594,#195595),.UNSPECIFIED.,.F.,.F.,(4,3,3,3,3,3,3,3,3,3,3,3,3,3,3,3,
3,4),(0.,4.30706237842305E-5,8.47417087646157E-5,0.000124159989198291,0.000160467076279865,
0.000170998382116677,0.000182414994733764,0.000213747977645854,0.000242415955901984,
0.000256497573175031,0.000259169422895605,0.000261757777312411,0.000289965130404686,
0.000301877270772898,0.000321937017503142,0.000326951954185703,0.000334474359209544,
0.000341996764233385),.UNSPECIFIED.);
#4688=B_SPLINE_CURVE_WITH_KNOTS('',3,(#195596,#195597,#195598,#195599,#195600,
#195601,#195602,#195603,#195604,#195605,#195606,#195607,#195608,#195609,
#195610,#195611,#195612,#195613,#195614,#195615,#195616,#195617,#195618,
#195619,#195620,#195621,#195622,#195623,#195624,#195625,#195626,#195627,
#195628,#195629,#195630,#195631,#195632,#195633,#195634,#195635,#195636,
#195637,#195638,#195639,#195640,#195641,#195642,#195643,#195644,#195645,
#195646,#195647),.UNSPECIFIED.,.F.,.F.,(4,3,3,3,3,3,3,3,3,3,3,3,3,3,3,3,
3,4),(3.46944695195361E-18,2.58457451680897E-5,4.25394446195799E-5,6.46659869687106E-5,
7.5729258143276E-5,8.12608937305587E-5,8.26438026273794E-5,8.67925293178414E-5,
0.000116015624427486,0.00013018879397676,0.00015188692630622,0.000161963651211284,
0.00016273599247095,0.000173585058635679,0.000212487880461467,0.00025523817351237,
0.000301397761147355,0.000347170117271362),.UNSPECIFIED.);
#4689=B_SPLINE_CURVE_WITH_KNOTS('',3,(#195649,#195650,#195651,#195652,#195653,
#195654,#195655,#195656,#195657,#195658,#195659,#195660,#195661,#195662,
#195663,#195664,#195665,#195666,#195667,#195668,#195669,#195670,#195671,
#195672,#195673,#195674,#195675,#195676,#195677,#195678,#195679,#195680,
#195681,#195682,#195683,#195684,#195685,#195686,#195687,#195688,#195689,
#195690,#195691,#195692,#195693,#195694),.UNSPECIFIED.,.F.,.F.,(4,3,3,3,
3,3,3,3,3,3,3,3,3,3,3,4),(0.,2.57218161988461E-5,4.21568322568433E-5,6.45873314617288E-5,
7.58025810641716E-5,8.1410205865393E-5,8.28121120656983E-5,8.70178306666144E-5,
0.00011608195565829,0.000130526745999922,0.000162394111022053,0.000174035661333229,
0.000213138396959319,0.000256116935436003,0.000302406662859732,0.00034807132266647),
 .UNSPECIFIED.);
#4690=B_SPLINE_CURVE_WITH_KNOTS('',3,(#195695,#195696,#195697,#195698,#195699,
#195700,#195701,#195702,#195703,#195704,#195705,#195706,#195707,#195708,
#195709,#195710,#195711,#195712,#195713,#195714,#195715,#195716,#195717,
#195718,#195719,#195720,#195721,#195722,#195723,#195724,#195725,#195726,
#195727,#195728,#195729,#195730,#195731,#195732,#195733,#195734,#195735,
#195736,#195737,#195738,#195739,#195740,#195741,#195742,#195743,#195744,
#195745,#195746),.UNSPECIFIED.,.F.,.F.,(4,3,3,3,3,3,3,3,3,3,3,3,3,3,3,3,
3,4),(0.,4.29652152158802E-5,8.44519107530096E-5,0.000123669830864391,0.000159788877357164,
0.000170558847912637,0.000181218775907177,0.000181960046452427,0.000214460062643589,
0.000244755726198111,0.000255838271868954,0.000258503253867589,0.000261084955178767,
0.000289370476648303,0.000301101325502019,0.000321109510663645,0.000331113603244458,
0.000341117695825271),.UNSPECIFIED.);
#4691=B_SPLINE_CURVE_WITH_KNOTS('',3,(#195748,#195749,#195750,#195751,#195752,
#195753,#195754,#195755,#195756,#195757,#195758,#195759,#195760,#195761,
#195762,#195763,#195764,#195765,#195766,#195767,#195768,#195769,#195770,
#195771,#195772,#195773,#195774,#195775,#195776,#195777,#195778,#195779,
#195780,#195781,#195782,#195783,#195784,#195785,#195786,#195787,#195788,
#195789,#195790,#195791,#195792,#195793,#195794,#195795,#195796,#195797,
#195798,#195799),.UNSPECIFIED.,.F.,.F.,(4,3,3,3,3,3,3,3,3,3,3,3,3,3,3,3,
3,4),(0.,4.30706237886451E-5,8.4741708772696E-5,0.000124159989209975,0.0001604670762956,
0.000170998382116695,0.000182414994733774,0.000213747977645868,0.000242415955903289,
0.000256497573175042,0.000259169422895615,0.00026175777731242,0.000289965130403147,
0.000301877270772904,0.000321937017503146,0.000326951954185707,0.000334474359209547,
0.000341996764233388),.UNSPECIFIED.);
#4692=B_SPLINE_CURVE_WITH_KNOTS('',3,(#195800,#195801,#195802,#195803,#195804,
#195805,#195806,#195807,#195808,#195809,#195810,#195811,#195812,#195813,
#195814,#195815,#195816,#195817,#195818,#195819,#195820,#195821,#195822,
#195823,#195824,#195825,#195826,#195827,#195828,#195829,#195830,#195831,
#195832,#195833,#195834,#195835,#195836,#195837,#195838,#195839,#195840,
#195841,#195842,#195843,#195844,#195845,#195846,#195847,#195848,#195849,
#195850,#195851),.UNSPECIFIED.,.F.,.F.,(4,3,3,3,3,3,3,3,3,3,3,3,3,3,3,3,
3,4),(0.,2.58457451684994E-5,4.25394446194796E-5,6.466598696866E-5,7.57292581432503E-5,
8.12608937305454E-5,8.26438026273691E-5,8.67925293178405E-5,0.000116015624427484,
0.000130188793976761,0.000151886926306221,0.000161963651211264,0.000162735992470951,
0.000173585058635681,0.000212487880461759,0.000255238173513016,0.000301397761148625,
0.000347170117271374),.UNSPECIFIED.);
#4693=B_SPLINE_CURVE_WITH_KNOTS('',3,(#195853,#195854,#195855,#195856,#195857,
#195858,#195859,#195860,#195861,#195862,#195863,#195864,#195865,#195866,
#195867,#195868,#195869,#195870,#195871,#195872,#195873,#195874,#195875,
#195876,#195877,#195878,#195879,#195880,#195881,#195882,#195883,#195884,
#195885,#195886,#195887,#195888,#195889,#195890,#195891,#195892,#195893,
#195894,#195895,#195896,#195897,#195898),.UNSPECIFIED.,.F.,.F.,(4,3,3,3,
3,3,3,3,3,3,3,3,3,3,3,4),(0.,2.57218162002198E-5,4.21568322567467E-5,6.45873314616841E-5,
7.58025810641528E-5,8.14102058653871E-5,8.28121120656957E-5,8.70178306666214E-5,
0.000116081955658617,0.000130526745999932,0.000162394111022051,0.000174035661333243,
0.000213138396957433,0.000256116935432043,0.000302406662852999,0.000348071322666481),
 .UNSPECIFIED.);
#4694=B_SPLINE_CURVE_WITH_KNOTS('',3,(#195899,#195900,#195901,#195902,#195903,
#195904,#195905,#195906,#195907,#195908,#195909,#195910,#195911,#195912,
#195913,#195914,#195915,#195916,#195917,#195918,#195919,#195920,#195921,
#195922,#195923,#195924,#195925,#195926,#195927,#195928,#195929,#195930,
#195931,#195932,#195933,#195934,#195935,#195936,#195937,#195938,#195939,
#195940,#195941,#195942,#195943,#195944,#195945,#195946,#195947,#195948,
#195949,#195950),.UNSPECIFIED.,.F.,.F.,(4,3,3,3,3,3,3,3,3,3,3,3,3,3,3,3,
3,4),(0.,4.29652152173429E-5,8.44519107554398E-5,0.000123669830867436,0.00015978887736076,
0.000170558847912635,0.000181218775907174,0.000181960046452407,0.000214460062643482,
0.000244755726198295,0.000255838271868951,0.000258503253867586,0.000261084955178764,
0.000289370476647682,0.000301101325502016,0.000321109510663642,0.000331113603244455,
0.000341117695825268),.UNSPECIFIED.);
#4695=B_SPLINE_CURVE_WITH_KNOTS('',3,(#195952,#195953,#195954,#195955,#195956,
#195957,#195958,#195959,#195960,#195961,#195962,#195963,#195964,#195965,
#195966,#195967,#195968,#195969,#195970,#195971,#195972,#195973,#195974,
#195975,#195976,#195977,#195978,#195979,#195980,#195981,#195982,#195983,
#195984,#195985,#195986,#195987,#195988,#195989,#195990,#195991,#195992,
#195993,#195994,#195995,#195996,#195997,#195998,#195999,#196000,#196001,
#196002,#196003),.UNSPECIFIED.,.F.,.F.,(4,3,3,3,3,3,3,3,3,3,3,3,3,3,3,3,
3,4),(0.,4.30706237823169E-5,8.47417087612841E-5,0.000124159989193728,0.000160467076274024,
0.00017099838211669,0.000182414994733806,0.000213747977645865,0.000242415955902471,
0.000256497573175041,0.000259169422895614,0.00026175777731242,0.000289965130404446,
0.000301877270772906,0.000321937017503149,0.000326951954185709,0.00033447435920955,
0.000341996764233392),.UNSPECIFIED.);
#4696=B_SPLINE_CURVE_WITH_KNOTS('',3,(#196004,#196005,#196006,#196007,#196008,
#196009,#196010,#196011,#196012,#196013,#196014,#196015,#196016,#196017,
#196018,#196019,#196020,#196021,#196022,#196023,#196024,#196025,#196026,
#196027,#196028,#196029,#196030,#196031,#196032,#196033,#196034,#196035,
#196036,#196037,#196038,#196039,#196040,#196041,#196042,#196043,#196044,
#196045,#196046,#196047,#196048,#196049,#196050,#196051,#196052,#196053,
#196054,#196055),.UNSPECIFIED.,.F.,.F.,(4,3,3,3,3,3,3,3,3,3,3,3,3,3,3,3,
3,4),(0.,2.58457451671982E-5,4.25394446196549E-5,6.4665986968747E-5,7.5729258143293E-5,
8.12608937305661E-5,8.26438026273843E-5,8.67925293178391E-5,0.00011601562442746,
0.000130188793976759,0.000151886926306218,0.000161963651211268,0.000162735992470948,
0.000173585058635678,0.000212487880462689,0.000255238173515773,0.00030139776115473,
0.000347170117271358),.UNSPECIFIED.);
#4697=B_SPLINE_CURVE_WITH_KNOTS('',3,(#196057,#196058,#196059,#196060,#196061,
#196062,#196063,#196064,#196065,#196066,#196067,#196068,#196069,#196070,
#196071,#196072,#196073,#196074,#196075,#196076,#196077,#196078,#196079,
#196080,#196081,#196082,#196083,#196084,#196085,#196086,#196087,#196088,
#196089,#196090,#196091,#196092,#196093,#196094,#196095,#196096,#196097,
#196098,#196099,#196100,#196101,#196102),.UNSPECIFIED.,.F.,.F.,(4,3,3,3,
3,3,3,3,3,3,3,3,3,3,3,4),(0.,2.57218162004827E-5,4.21568322567461E-5,6.4587331461682E-5,
7.58025810641499E-5,8.14102058653839E-5,8.28121120656924E-5,8.70178306666178E-5,
0.000116081955659027,0.000130526745999927,0.000162394111022054,0.000174035661333236,
0.00021313839695725,0.000256116935432016,0.000302406662854051,0.000348071322666459),
 .UNSPECIFIED.);
#4698=B_SPLINE_CURVE_WITH_KNOTS('',3,(#196103,#196104,#196105,#196106,#196107,
#196108,#196109,#196110,#196111,#196112,#196113,#196114,#196115,#196116,
#196117,#196118,#196119,#196120,#196121,#196122,#196123,#196124,#196125,
#196126,#196127,#196128,#196129,#196130,#196131,#196132,#196133,#196134,
#196135,#196136,#196137,#196138,#196139,#196140,#196141,#196142,#196143,
#196144,#196145,#196146,#196147,#196148,#196149,#196150,#196151,#196152,
#196153,#196154),.UNSPECIFIED.,.F.,.F.,(4,3,3,3,3,3,3,3,3,3,3,3,3,3,3,3,
3,4),(0.,4.29652152210268E-5,8.44519107616881E-5,0.000123669830875786,0.000159788877371095,
0.000170558847912614,0.000181218775907154,0.0001819600464524,0.000214460062643448,
0.000244755726197702,0.000255838271868935,0.00025850325386757,0.000261084955178747,
0.000289370476647446,0.000301101325502001,0.000321109510663628,0.000331113603244442,
0.000341117695825255),.UNSPECIFIED.);
#4699=B_SPLINE_CURVE_WITH_KNOTS('',3,(#196156,#196157,#196158,#196159,#196160,
#196161,#196162,#196163,#196164,#196165,#196166,#196167,#196168,#196169,
#196170,#196171,#196172,#196173,#196174,#196175,#196176,#196177,#196178,
#196179,#196180,#196181,#196182,#196183,#196184,#196185,#196186,#196187,
#196188,#196189,#196190,#196191,#196192,#196193,#196194,#196195,#196196,
#196197,#196198,#196199,#196200,#196201,#196202,#196203,#196204,#196205,
#196206,#196207),.UNSPECIFIED.,.F.,.F.,(4,3,3,3,3,3,3,3,3,3,3,3,3,3,3,3,
3,4),(0.,4.30706237873732E-5,8.47417087705962E-5,0.000124159989207352,0.000160467076292369,
0.000170998382116696,0.000182414994733765,0.000213747977645869,0.000242415955903072,
0.000256497573175042,0.000259169422895615,0.000261757777312421,0.000289965130403374,
0.000301877270772904,0.000321937017503146,0.000326951954185707,0.000334474359209547,
0.000341996764233388),.UNSPECIFIED.);
#4700=B_SPLINE_CURVE_WITH_KNOTS('',3,(#196208,#196209,#196210,#196211,#196212,
#196213,#196214,#196215,#196216,#196217,#196218,#196219,#196220,#196221,
#196222,#196223,#196224,#196225,#196226,#196227,#196228,#196229,#196230,
#196231,#196232,#196233,#196234,#196235,#196236,#196237,#196238,#196239,
#196240,#196241,#196242,#196243,#196244,#196245,#196246,#196247,#196248,
#196249,#196250,#196251,#196252,#196253,#196254,#196255,#196256,#196257,
#196258,#196259),.UNSPECIFIED.,.F.,.F.,(4,3,3,3,3,3,3,3,3,3,3,3,3,3,3,3,
3,4),(0.,2.58457451703126E-5,4.25394446196281E-5,6.46659869687304E-5,7.57292581432815E-5,
8.12608937305571E-5,8.2643802627376E-5,8.67925293178326E-5,0.000116015624428797,
0.000130188793976749,0.000151886926306207,0.000161963651211271,0.000162735992470936,
0.000173585058635665,0.000212487880461566,0.000255238173512672,0.000301397761147969,
0.000347170117271347),.UNSPECIFIED.);
#4701=B_SPLINE_CURVE_WITH_KNOTS('',3,(#196261,#196262,#196263,#196264,#196265,
#196266,#196267,#196268,#196269,#196270,#196271,#196272,#196273,#196274,
#196275,#196276,#196277,#196278,#196279,#196280,#196281,#196282,#196283,
#196284,#196285,#196286,#196287,#196288,#196289,#196290,#196291,#196292,
#196293,#196294,#196295,#196296,#196297,#196298,#196299,#196300,#196301,
#196302,#196303,#196304,#196305,#196306),.UNSPECIFIED.,.F.,.F.,(4,3,3,3,
3,3,3,3,3,3,3,3,3,3,3,4),(0.,2.57218161992659E-5,4.21568322566835E-5,6.45873314616532E-5,
7.58025810641381E-5,8.14102058653805E-5,8.28121120656911E-5,8.70178306666229E-5,
0.00011608195565876,0.000130526745999934,0.000162394111022074,0.000174035661333246,
0.00021313839696108,0.000256116935439352,0.000302406662864497,0.000348071322666474),
 .UNSPECIFIED.);
#4702=B_SPLINE_CURVE_WITH_KNOTS('',3,(#196307,#196308,#196309,#196310,#196311,
#196312,#196313,#196314,#196315,#196316,#196317,#196318,#196319,#196320,
#196321,#196322,#196323,#196324,#196325,#196326,#196327,#196328,#196329,
#196330,#196331,#196332,#196333,#196334,#196335,#196336,#196337,#196338,
#196339,#196340,#196341,#196342,#196343,#196344,#196345,#196346,#196347,
#196348,#196349,#196350,#196351,#196352,#196353,#196354,#196355,#196356,
#196357,#196358),.UNSPECIFIED.,.F.,.F.,(4,3,3,3,3,3,3,3,3,3,3,3,3,3,3,3,
3,4),(0.,4.29652152199114E-5,8.44519107592339E-5,0.000123669830871405,0.000159788877364126,
0.000170558847912617,0.000181218775907156,0.000181960046452403,0.000214460062642956,
0.000244755726197005,0.000255838271868931,0.000258503253867566,0.000261084955178744,
0.000289370476649217,0.000301101325501995,0.00032110951066362,0.000331113603244433,
0.000341117695825246),.UNSPECIFIED.);
#4703=B_SPLINE_CURVE_WITH_KNOTS('',3,(#196360,#196361,#196362,#196363,#196364,
#196365,#196366,#196367,#196368,#196369,#196370,#196371,#196372,#196373,
#196374,#196375,#196376,#196377,#196378,#196379,#196380,#196381,#196382,
#196383,#196384,#196385,#196386,#196387,#196388,#196389,#196390,#196391,
#196392,#196393,#196394,#196395,#196396,#196397,#196398,#196399,#196400,
#196401,#196402,#196403,#196404,#196405,#196406,#196407,#196408,#196409,
#196410,#196411),.UNSPECIFIED.,.F.,.F.,(4,3,3,3,3,3,3,3,3,3,3,3,3,3,3,3,
3,4),(0.,4.30706237903638E-5,8.47417087757578E-5,0.000124159989214328,0.000160467076301428,
0.000170998382116691,0.000182414994733775,0.000213747977645864,0.000242415955904961,
0.000256497573175038,0.000259169422895611,0.000261757777312417,0.00028996513040181,
0.000301877270772901,0.000321937017503143,0.000326951954185704,0.000334474359209545,
0.000341996764233386),.UNSPECIFIED.);
#4704=B_SPLINE_CURVE_WITH_KNOTS('',3,(#196412,#196413,#196414,#196415,#196416,
#196417,#196418,#196419,#196420,#196421,#196422,#196423,#196424,#196425,
#196426,#196427,#196428,#196429,#196430,#196431,#196432,#196433,#196434,
#196435,#196436,#196437,#196438,#196439,#196440,#196441,#196442,#196443,
#196444,#196445,#196446,#196447,#196448,#196449,#196450,#196451,#196452,
#196453,#196454,#196455,#196456,#196457,#196458,#196459,#196460,#196461,
#196462,#196463),.UNSPECIFIED.,.F.,.F.,(4,3,3,3,3,3,3,3,3,3,3,3,3,3,3,3,
3,4),(0.,2.58457451685466E-5,4.25394446196209E-5,6.46659869687306E-5,7.57292581432855E-5,
8.12608937305629E-5,8.26438026273823E-5,8.67925293178403E-5,0.000116015624427434,
0.00013018879397676,0.000151886926306221,0.000161963651211266,0.000162735992470951,
0.000173585058635681,0.000212487880459847,0.000255238173510006,0.000301397761145795,
0.000347170117271344),.UNSPECIFIED.);
#4705=B_SPLINE_CURVE_WITH_KNOTS('',3,(#196465,#196466,#196467,#196468,#196469,
#196470,#196471,#196472,#196473,#196474,#196475,#196476,#196477,#196478,
#196479,#196480,#196481,#196482,#196483,#196484,#196485,#196486,#196487,
#196488,#196489,#196490,#196491,#196492,#196493,#196494,#196495,#196496,
#196497,#196498,#196499,#196500,#196501,#196502,#196503,#196504,#196505,
#196506,#196507,#196508,#196509,#196510),.UNSPECIFIED.,.F.,.F.,(4,3,3,3,
3,3,3,3,3,3,3,3,3,3,3,4),(0.,2.57218162017772E-5,4.21568322567134E-5,6.4587331461665E-5,
7.58025810641408E-5,8.14102058653787E-5,8.28121120656881E-5,8.70178306666165E-5,
0.000116081955658973,0.000130526745999925,0.000162394111022045,0.000174035661333233,
0.000213138396960719,0.000256116935438802,0.00030240666286413,0.000348071322666467),
 .UNSPECIFIED.);
#4706=B_SPLINE_CURVE_WITH_KNOTS('',3,(#196511,#196512,#196513,#196514,#196515,
#196516,#196517,#196518,#196519,#196520,#196521,#196522,#196523,#196524,
#196525,#196526,#196527,#196528,#196529,#196530,#196531,#196532,#196533,
#196534,#196535,#196536,#196537,#196538,#196539,#196540,#196541,#196542,
#196543,#196544,#196545,#196546,#196547,#196548,#196549,#196550,#196551,
#196552,#196553,#196554,#196555,#196556,#196557,#196558,#196559,#196560,
#196561,#196562),.UNSPECIFIED.,.F.,.F.,(4,3,3,3,3,3,3,3,3,3,3,3,3,3,3,3,
3,4),(0.,4.29652152161511E-5,8.4451910753523E-5,0.000123669830865121,0.000159788877358086,
0.000170558847912621,0.000181218775907161,0.000181960046452392,0.000214460062644014,
0.000244755726199354,0.000255838271868946,0.000258503253867581,0.000261084955178759,
0.000289370476646352,0.000301101325502015,0.000321109510663643,0.000331113603244457,
0.000341117695825271),.UNSPECIFIED.);
#4707=B_SPLINE_CURVE_WITH_KNOTS('',3,(#196564,#196565,#196566,#196567,#196568,
#196569,#196570,#196571,#196572,#196573,#196574,#196575,#196576,#196577,
#196578,#196579,#196580,#196581,#196582,#196583,#196584,#196585,#196586,
#196587,#196588,#196589,#196590,#196591,#196592,#196593,#196594,#196595,
#196596,#196597,#196598,#196599,#196600,#196601,#196602,#196603,#196604,
#196605,#196606,#196607,#196608,#196609,#196610,#196611,#196612,#196613,
#196614,#196615),.UNSPECIFIED.,.F.,.F.,(4,3,3,3,3,3,3,3,3,3,3,3,3,3,3,3,
3,4),(0.,4.30706237866705E-5,8.47417087691936E-5,0.000124159989205159,0.000160467076289346,
0.000170998382116694,0.000182414994733781,0.000213747977645868,0.000242415955904174,
0.000256497573175041,0.000259169422895614,0.00026175777731242,0.000289965130405258,
0.000301877270772903,0.000321937017503145,0.000326951954185706,0.000334474359209547,
0.000341996764233387),.UNSPECIFIED.);
#4708=B_SPLINE_CURVE_WITH_KNOTS('',3,(#196616,#196617,#196618,#196619,#196620,
#196621,#196622,#196623,#196624,#196625,#196626,#196627,#196628,#196629,
#196630,#196631,#196632,#196633,#196634,#196635,#196636,#196637,#196638,
#196639,#196640,#196641,#196642,#196643,#196644,#196645,#196646,#196647,
#196648,#196649,#196650,#196651,#196652,#196653,#196654,#196655,#196656,
#196657,#196658,#196659,#196660,#196661,#196662,#196663,#196664,#196665,
#196666,#196667),.UNSPECIFIED.,.F.,.F.,(4,3,3,3,3,3,3,3,3,3,3,3,3,3,3,3,
3,4),(0.,2.58457451669911E-5,4.25394446195997E-5,6.46659869687207E-5,7.57292581432812E-5,
8.12608937305615E-5,8.26438026273815E-5,8.67925293178417E-5,0.000116015624426113,
0.000130188793976763,0.000151886926306223,0.000161963651211266,0.000162735992470953,
0.000173585058635683,0.000212487880456845,0.000255238173501831,0.000301397761127879,
0.00034717011727138),.UNSPECIFIED.);
#4709=B_SPLINE_CURVE_WITH_KNOTS('',3,(#196669,#196670,#196671,#196672,#196673,
#196674,#196675,#196676,#196677,#196678,#196679,#196680,#196681,#196682,
#196683,#196684,#196685,#196686,#196687,#196688,#196689,#196690,#196691,
#196692,#196693,#196694,#196695,#196696,#196697,#196698,#196699,#196700,
#196701,#196702,#196703,#196704,#196705,#196706,#196707,#196708,#196709,
#196710,#196711,#196712,#196713,#196714),.UNSPECIFIED.,.F.,.F.,(4,3,3,3,
3,3,3,3,3,3,3,3,3,3,3,4),(0.,2.57218161991998E-5,4.21568322567933E-5,6.45873314617068E-5,
7.58025810641636E-5,8.14102058653919E-5,8.2812112065699E-5,8.70178306666203E-5,
0.000116081955658395,0.00013052674599993,0.000162394111022055,0.000174035661333241,
0.000213138396959329,0.000256116935435947,0.000302406662859352,0.00034807132266647),
 .UNSPECIFIED.);
#4710=B_SPLINE_CURVE_WITH_KNOTS('',3,(#196715,#196716,#196717,#196718,#196719,
#196720,#196721,#196722,#196723,#196724,#196725,#196726,#196727,#196728,
#196729,#196730,#196731,#196732,#196733,#196734,#196735,#196736,#196737,
#196738,#196739,#196740,#196741,#196742,#196743,#196744,#196745,#196746,
#196747,#196748,#196749,#196750,#196751,#196752,#196753,#196754,#196755,
#196756,#196757,#196758,#196759,#196760,#196761,#196762,#196763,#196764,
#196765,#196766),.UNSPECIFIED.,.F.,.F.,(4,3,3,3,3,3,3,3,3,3,3,3,3,3,3,3,
3,4),(0.,4.29652152145126E-5,8.44519107508585E-5,0.000123669830861906,0.0001597888773547,
0.000170558847912636,0.000181218775907175,0.000181960046452407,0.000214460062643629,
0.000244755726198551,0.000255838271868953,0.000258503253867588,0.000261084955178766,
0.000289370476648523,0.000301101325502018,0.000321109510663644,0.000331113603244457,
0.00034111769582527),.UNSPECIFIED.);
#4711=B_SPLINE_CURVE_WITH_KNOTS('',3,(#196768,#196769,#196770,#196771,#196772,
#196773,#196774,#196775,#196776,#196777,#196778,#196779,#196780,#196781,
#196782,#196783,#196784,#196785,#196786,#196787,#196788,#196789,#196790,
#196791,#196792,#196793,#196794,#196795,#196796,#196797,#196798,#196799,
#196800,#196801,#196802,#196803,#196804,#196805,#196806,#196807,#196808,
#196809,#196810,#196811,#196812,#196813,#196814,#196815,#196816,#196817,
#196818,#196819),.UNSPECIFIED.,.F.,.F.,(4,3,3,3,3,3,3,3,3,3,3,3,3,3,3,3,
3,4),(0.,4.30706237893538E-5,8.47417087739242E-5,0.000124159989211692,0.000160467076297654,
0.0001709983821167,0.000182414994733784,0.000213747977645873,0.000242415955902547,
0.000256497573175046,0.000259169422895619,0.000261757777312425,0.000289965130402395,
0.000301877270772908,0.00032193701750315,0.000326951954185711,0.000334474359209551,
0.000341996764233392),.UNSPECIFIED.);
#4712=B_SPLINE_CURVE_WITH_KNOTS('',3,(#196820,#196821,#196822,#196823,#196824,
#196825,#196826,#196827,#196828,#196829,#196830,#196831,#196832,#196833,
#196834,#196835,#196836,#196837,#196838,#196839,#196840,#196841,#196842,
#196843,#196844,#196845,#196846,#196847,#196848,#196849,#196850,#196851,
#196852,#196853,#196854,#196855,#196856,#196857,#196858,#196859,#196860,
#196861,#196862,#196863,#196864,#196865,#196866,#196867,#196868,#196869,
#196870,#196871),.UNSPECIFIED.,.F.,.F.,(4,3,3,3,3,3,3,3,3,3,3,3,3,3,3,3,
3,4),(0.,2.58457451681646E-5,4.25394446194625E-5,6.46659869686492E-5,7.57292581432425E-5,
8.12608937305392E-5,8.26438026273634E-5,8.67925293178359E-5,0.000116015624428639,
0.000130188793976754,0.000151886926306213,0.000161963651211277,0.000162735992470942,
0.000173585058635672,0.000212487880460382,0.00025523817351074,0.000301397761146053,
0.00034717011727136),.UNSPECIFIED.);
#4713=B_SPLINE_CURVE_WITH_KNOTS('',3,(#196873,#196874,#196875,#196876,#196877,
#196878,#196879,#196880,#196881,#196882,#196883,#196884,#196885,#196886,
#196887,#196888,#196889,#196890,#196891,#196892,#196893,#196894,#196895,
#196896,#196897,#196898,#196899,#196900,#196901,#196902,#196903,#196904,
#196905,#196906,#196907,#196908,#196909,#196910,#196911,#196912,#196913,
#196914,#196915,#196916,#196917,#196918),.UNSPECIFIED.,.F.,.F.,(4,3,3,3,
3,3,3,3,3,3,3,3,3,3,3,4),(6.93889390390723E-18,2.57218162012745E-5,4.21568322568842E-5,
6.45873314617536E-5,7.58025810641882E-5,8.14102058654056E-5,8.28121120657099E-5,
8.70178306666229E-5,0.000116081955657485,0.000130526745999931,0.000162394111022046,
0.000174035661333239,0.000213138396958867,0.000256116935434972,0.000302406662857771,
0.000348071322666458),.UNSPECIFIED.);
#4714=B_SPLINE_CURVE_WITH_KNOTS('',3,(#196919,#196920,#196921,#196922,#196923,
#196924,#196925,#196926,#196927,#196928,#196929,#196930,#196931,#196932,
#196933,#196934,#196935,#196936,#196937,#196938,#196939,#196940,#196941,
#196942,#196943,#196944,#196945,#196946,#196947,#196948,#196949,#196950,
#196951,#196952,#196953,#196954,#196955,#196956,#196957,#196958,#196959,
#196960,#196961,#196962,#196963,#196964,#196965,#196966,#196967,#196968,
#196969,#196970),.UNSPECIFIED.,.F.,.F.,(4,3,3,3,3,3,3,3,3,3,3,3,3,3,3,3,
3,4),(0.,4.29652152149597E-5,8.4451910751605E-5,0.000123669830862903,0.000159788877355898,
0.000170558847912635,0.000181218775907175,0.000181960046452407,0.000214460062643025,
0.00024475572619701,0.000255838271868953,0.000258503253867588,0.000261084955178765,
0.000289370476648861,0.000301101325502018,0.000321109510663644,0.000331113603244457,
0.00034111769582527),.UNSPECIFIED.);
#4715=B_SPLINE_CURVE_WITH_KNOTS('',3,(#196972,#196973,#196974,#196975,#196976,
#196977,#196978,#196979,#196980,#196981,#196982,#196983,#196984,#196985,
#196986,#196987,#196988,#196989,#196990,#196991,#196992,#196993,#196994,
#196995,#196996,#196997,#196998,#196999,#197000,#197001,#197002,#197003,
#197004,#197005,#197006,#197007,#197008,#197009,#197010,#197011,#197012,
#197013,#197014,#197015,#197016,#197017,#197018,#197019,#197020,#197021,
#197022,#197023),.UNSPECIFIED.,.F.,.F.,(4,3,3,3,3,3,3,3,3,3,3,3,3,3,3,3,
3,4),(0.,4.30706237845979E-5,8.4741708765375E-5,0.00012415998919943,0.00016046707628152,
0.00017099838211669,0.000182414994733782,0.000213747977645867,0.000242415955903715,
0.000256497573175044,0.000259169422895618,0.000261757777312424,0.000289965130403571,
0.000301877270772911,0.000321937017503155,0.000326951954185716,0.000334474359209558,
0.000341996764233399),.UNSPECIFIED.);
#4716=B_SPLINE_CURVE_WITH_KNOTS('',3,(#197024,#197025,#197026,#197027,#197028,
#197029,#197030,#197031,#197032,#197033,#197034,#197035,#197036,#197037,
#197038,#197039,#197040,#197041,#197042,#197043,#197044,#197045,#197046,
#197047,#197048,#197049,#197050,#197051,#197052,#197053,#197054,#197055,
#197056,#197057,#197058,#197059,#197060,#197061,#197062,#197063,#197064,
#197065,#197066,#197067,#197068,#197069,#197070,#197071,#197072,#197073,
#197074,#197075),.UNSPECIFIED.,.F.,.F.,(4,3,3,3,3,3,3,3,3,3,3,3,3,3,3,3,
3,4),(3.46944695195361E-18,2.58457451685079E-5,4.25394446195536E-5,6.46659869686988E-5,
7.57292581432714E-5,8.12608937305577E-5,8.26438026273792E-5,8.6792529317844E-5,
0.000116015624427737,0.000130188793976764,0.000151886926306224,0.000161963651211275,
0.000162735992470954,0.000173585058635684,0.000212487880460469,0.000255238173510927,
0.00030139776114628,0.000347170117271379),.UNSPECIFIED.);
#4717=B_SPLINE_CURVE_WITH_KNOTS('',3,(#197077,#197078,#197079,#197080,#197081,
#197082,#197083,#197084,#197085,#197086,#197087,#197088,#197089,#197090,
#197091,#197092,#197093,#197094,#197095,#197096,#197097,#197098,#197099,
#197100,#197101,#197102,#197103,#197104,#197105,#197106,#197107,#197108,
#197109,#197110,#197111,#197112,#197113,#197114,#197115,#197116,#197117,
#197118,#197119,#197120,#197121,#197122),.UNSPECIFIED.,.F.,.F.,(4,3,3,3,
3,3,3,3,3,3,3,3,3,3,3,4),(0.,2.57218161989107E-5,4.21568322568349E-5,6.45873314617258E-5,
7.58025810641712E-5,8.1410205865394E-5,8.28121120656996E-5,8.70178306666167E-5,
0.000116081955658387,0.000130526745999925,0.00016239411102205,0.000174035661333233,
0.000213138396959998,0.000256116935437306,0.0003024066628616,0.000348071322666454),
 .UNSPECIFIED.);
#4718=B_SPLINE_CURVE_WITH_KNOTS('',3,(#197123,#197124,#197125,#197126,#197127,
#197128,#197129,#197130,#197131,#197132,#197133,#197134,#197135,#197136,
#197137,#197138,#197139,#197140,#197141,#197142,#197143,#197144,#197145,
#197146,#197147,#197148,#197149,#197150,#197151,#197152,#197153,#197154,
#197155,#197156,#197157,#197158,#197159,#197160,#197161,#197162,#197163,
#197164,#197165,#197166,#197167,#197168,#197169,#197170,#197171,#197172,
#197173,#197174),.UNSPECIFIED.,.F.,.F.,(4,3,3,3,3,3,3,3,3,3,3,3,3,3,3,3,
3,4),(0.,4.29652152148382E-5,8.44519107513973E-5,0.000123669830862666,0.000159788877355585,
0.000170558847912623,0.000181218775907163,0.000181960046452376,0.000214460062643276,
0.000244755726198279,0.000255838271868941,0.000258503253867575,0.000261084955178753,
0.000289370476647672,0.000301101325502006,0.000321109510663632,0.000331113603244445,
0.000341117695825258),.UNSPECIFIED.);
#4719=B_SPLINE_CURVE_WITH_KNOTS('',3,(#197176,#197177,#197178,#197179,#197180,
#197181,#197182,#197183,#197184,#197185,#197186,#197187,#197188,#197189,
#197190,#197191,#197192,#197193,#197194,#197195,#197196,#197197,#197198,
#197199,#197200,#197201,#197202,#197203,#197204,#197205,#197206,#197207,
#197208,#197209,#197210,#197211,#197212,#197213,#197214,#197215,#197216,
#197217,#197218,#197219,#197220,#197221,#197222,#197223,#197224,#197225,
#197226,#197227),.UNSPECIFIED.,.F.,.F.,(4,3,3,3,3,3,3,3,3,3,3,3,3,3,3,3,
3,4),(0.,4.30706237889783E-5,8.47417087733069E-5,0.000124159989210858,0.000160467076296833,
0.000170998382116681,0.000182414994733743,0.000213747977645858,0.000242415955903097,
0.000256497573175036,0.000259169422895609,0.000261757777312415,0.000289965130403247,
0.000301877270772902,0.000321937017503146,0.000326951954185707,0.000334474359209549,
0.00034199676423339),.UNSPECIFIED.);
#4720=B_SPLINE_CURVE_WITH_KNOTS('',3,(#197228,#197229,#197230,#197231,#197232,
#197233,#197234,#197235,#197236,#197237,#197238,#197239,#197240,#197241,
#197242,#197243,#197244,#197245,#197246,#197247,#197248,#197249,#197250,
#197251,#197252,#197253,#197254,#197255,#197256,#197257,#197258,#197259,
#197260,#197261,#197262,#197263,#197264,#197265,#197266,#197267,#197268,
#197269,#197270,#197271,#197272,#197273,#197274,#197275,#197276,#197277,
#197278,#197279),.UNSPECIFIED.,.F.,.F.,(4,3,3,3,3,3,3,3,3,3,3,3,3,3,3,3,
3,4),(3.46944695195361E-18,2.58457451679395E-5,4.25394446196648E-5,6.46659869687534E-5,
7.57292581432977E-5,8.12608937305698E-5,8.26438026273878E-5,8.67925293178419E-5,
0.000116015624428513,0.000130188793976761,0.000151886926306221,0.00016196365121127,
0.000162735992470951,0.00017358505863568,0.000212487880461813,0.000255238173513001,
0.000301397761148148,0.000347170117271353),.UNSPECIFIED.);
#4721=B_SPLINE_CURVE_WITH_KNOTS('',3,(#197281,#197282,#197283,#197284,#197285,
#197286,#197287,#197288,#197289,#197290,#197291,#197292,#197293,#197294,
#197295,#197296,#197297,#197298,#197299,#197300,#197301,#197302,#197303,
#197304,#197305,#197306,#197307,#197308,#197309,#197310,#197311,#197312,
#197313,#197314,#197315,#197316,#197317,#197318,#197319,#197320,#197321,
#197322,#197323,#197324,#197325,#197326),.UNSPECIFIED.,.F.,.F.,(4,3,3,3,
3,3,3,3,3,3,3,3,3,3,3,4),(0.,2.57218161995894E-5,4.21568322567858E-5,6.4587331461702E-5,
7.58025810641601E-5,8.14102058653892E-5,8.28121120656964E-5,8.70178306666182E-5,
0.000116081955658822,0.000130526745999927,0.000162394111022044,0.000174035661333236,
0.000213138396956959,0.000256116935431279,0.000302406662852392,0.000348071322666469),
 .UNSPECIFIED.);
#4722=B_SPLINE_CURVE_WITH_KNOTS('',3,(#197327,#197328,#197329,#197330,#197331,
#197332,#197333,#197334,#197335,#197336,#197337,#197338,#197339,#197340,
#197341,#197342,#197343,#197344,#197345,#197346,#197347,#197348,#197349,
#197350,#197351,#197352,#197353,#197354,#197355,#197356,#197357,#197358,
#197359,#197360,#197361,#197362,#197363,#197364,#197365,#197366,#197367,
#197368,#197369,#197370,#197371,#197372,#197373,#197374,#197375,#197376,
#197377,#197378),.UNSPECIFIED.,.F.,.F.,(4,3,3,3,3,3,3,3,3,3,3,3,3,3,3,3,
3,4),(0.,4.29652152094933E-5,8.44519107431452E-5,0.000123669830853246,0.000159788877346178,
0.000170558847912626,0.000181218775907166,0.000181960046452406,0.000214460062643372,
0.000244755726197706,0.000255838271868949,0.000258503253867584,0.000261084955178762,
0.000289370476648327,0.000301101325502017,0.000321109510663644,0.000331113603244458,
0.000341117695825272),.UNSPECIFIED.);
#4723=B_SPLINE_CURVE_WITH_KNOTS('',3,(#197380,#197381,#197382,#197383,#197384,
#197385,#197386,#197387,#197388,#197389,#197390,#197391,#197392,#197393,
#197394,#197395,#197396,#197397,#197398,#197399,#197400,#197401,#197402,
#197403,#197404,#197405,#197406,#197407,#197408,#197409,#197410,#197411,
#197412,#197413,#197414,#197415,#197416,#197417,#197418,#197419,#197420,
#197421,#197422,#197423,#197424,#197425,#197426,#197427,#197428,#197429,
#197430,#197431),.UNSPECIFIED.,.F.,.F.,(4,3,3,3,3,3,3,3,3,3,3,3,3,3,3,3,
3,4),(0.,4.30706237876313E-5,8.47417087707628E-5,0.000124159989207121,0.000160467076291592,
0.000170998382116703,0.00018241499473379,0.000213747977645873,0.000242415955903416,
0.000256497573175044,0.000259169422895617,0.000261757777312422,0.00028996513040352,
0.000301877270772903,0.000321937017503144,0.000326951954185704,0.000334474359209544,
0.000341996764233385),.UNSPECIFIED.);
#4724=B_SPLINE_CURVE_WITH_KNOTS('',3,(#197432,#197433,#197434,#197435,#197436,
#197437,#197438,#197439,#197440,#197441,#197442,#197443,#197444,#197445,
#197446,#197447,#197448,#197449,#197450,#197451,#197452,#197453,#197454,
#197455,#197456,#197457,#197458,#197459,#197460,#197461,#197462,#197463,
#197464,#197465,#197466,#197467,#197468,#197469,#197470,#197471,#197472,
#197473,#197474,#197475,#197476,#197477,#197478,#197479,#197480,#197481,
#197482,#197483),.UNSPECIFIED.,.F.,.F.,(4,3,3,3,3,3,3,3,3,3,3,3,3,3,3,3,
3,4),(0.,2.58457451665638E-5,4.25394446195485E-5,6.4665986968694E-5,7.57292581432668E-5,
8.12608937305532E-5,8.26438026273748E-5,8.67925293178396E-5,0.000116015624426654,
0.000130188793976759,0.000151886926306219,0.00016196365121128,0.000162735992470949,
0.000173585058635679,0.000212487880458713,0.00025523817350687,0.000301397761138754,
0.000347170117271368),.UNSPECIFIED.);
#4725=B_SPLINE_CURVE_WITH_KNOTS('',3,(#197485,#197486,#197487,#197488,#197489,
#197490,#197491,#197492,#197493,#197494,#197495,#197496,#197497,#197498,
#197499,#197500,#197501,#197502,#197503,#197504,#197505,#197506,#197507,
#197508,#197509,#197510,#197511,#197512,#197513,#197514,#197515,#197516,
#197517,#197518,#197519,#197520,#197521,#197522,#197523,#197524,#197525,
#197526,#197527,#197528,#197529,#197530),.UNSPECIFIED.,.F.,.F.,(4,3,3,3,
3,3,3,3,3,3,3,3,3,3,3,4),(0.,2.57218162017605E-5,4.21568322567747E-5,6.45873314616954E-5,
7.58025810641557E-5,8.14102058653859E-5,8.28121120656934E-5,8.7017830666616E-5,
0.000116081955659622,0.000130526745999924,0.000162394111022032,0.000174035661333232,
0.000213138396958048,0.000256116935433517,0.00030240666285608,0.000348071322666468),
 .UNSPECIFIED.);
#4726=B_SPLINE_CURVE_WITH_KNOTS('',3,(#197531,#197532,#197533,#197534,#197535,
#197536,#197537,#197538,#197539,#197540,#197541,#197542,#197543,#197544,
#197545,#197546,#197547,#197548,#197549,#197550,#197551,#197552,#197553,
#197554,#197555,#197556,#197557,#197558,#197559,#197560,#197561,#197562,
#197563,#197564,#197565,#197566,#197567,#197568,#197569,#197570,#197571,
#197572,#197573,#197574,#197575,#197576,#197577,#197578,#197579,#197580,
#197581,#197582),.UNSPECIFIED.,.F.,.F.,(4,3,3,3,3,3,3,3,3,3,3,3,3,3,3,3,
3,4),(0.,4.29652152129689E-5,8.44519107480275E-5,0.000123669830857744,0.000159788877348903,
0.000170558847912613,0.000181218775907154,0.000181960046452395,0.000214460062643831,
0.000244755726199015,0.000255838271868934,0.000258503253867569,0.000261084955178747,
0.000289370476647275,0.000301101325502001,0.000321109510663628,0.000331113603244442,
0.000341117695825255),.UNSPECIFIED.);
#4727=B_SPLINE_CURVE_WITH_KNOTS('',3,(#197584,#197585,#197586,#197587,#197588,
#197589,#197590,#197591,#197592,#197593,#197594,#197595,#197596,#197597,
#197598,#197599,#197600,#197601,#197602,#197603,#197604,#197605,#197606,
#197607,#197608,#197609,#197610,#197611,#197612,#197613,#197614,#197615,
#197616,#197617,#197618,#197619,#197620,#197621,#197622,#197623,#197624,
#197625,#197626,#197627,#197628,#197629,#197630,#197631,#197632,#197633,
#197634,#197635),.UNSPECIFIED.,.F.,.F.,(4,3,3,3,3,3,3,3,3,3,3,3,3,3,3,3,
3,4),(1.04083408558608E-17,4.307062378596E-5,8.47417087679539E-5,0.000124159989203457,
0.000160467076287138,0.000170998382116702,0.000182414994733776,0.000213747977645871,
0.000242415955902389,0.000256497573175041,0.000259169422895614,0.000261757777312419,
0.000289965130404368,0.000301877270772899,0.000321937017503139,0.000326951954185699,
0.00033447435920954,0.00034199676423338),.UNSPECIFIED.);
#4728=B_SPLINE_CURVE_WITH_KNOTS('',3,(#197636,#197637,#197638,#197639,#197640,
#197641,#197642,#197643,#197644,#197645,#197646,#197647,#197648,#197649,
#197650,#197651,#197652,#197653,#197654,#197655,#197656,#197657,#197658,
#197659,#197660,#197661,#197662,#197663,#197664,#197665,#197666,#197667,
#197668,#197669,#197670,#197671,#197672,#197673,#197674,#197675,#197676,
#197677,#197678,#197679,#197680,#197681,#197682,#197683,#197684,#197685,
#197686,#197687),.UNSPECIFIED.,.F.,.F.,(4,3,3,3,3,3,3,3,3,3,3,3,3,3,3,3,
3,4),(0.,2.58457451687787E-5,4.25394446196238E-5,6.46659869687319E-5,7.57292581432859E-5,
8.12608937305629E-5,8.26438026273822E-5,8.679252931784E-5,0.000116015624426979,
0.00013018879397676,0.00015188692630622,0.000161963651211278,0.00016273599247095,
0.00017358505863568,0.000212487880458027,0.000255238173505867,0.00030139776113807,
0.000347170117271346),.UNSPECIFIED.);
#4729=B_SPLINE_CURVE_WITH_KNOTS('',3,(#197689,#197690,#197691,#197692,#197693,
#197694,#197695,#197696,#197697,#197698,#197699,#197700,#197701,#197702,
#197703,#197704,#197705,#197706,#197707,#197708,#197709,#197710,#197711,
#197712,#197713,#197714,#197715,#197716,#197717,#197718,#197719,#197720,
#197721,#197722,#197723,#197724,#197725,#197726,#197727,#197728,#197729,
#197730,#197731,#197732,#197733,#197734),.UNSPECIFIED.,.F.,.F.,(4,3,3,3,
3,3,3,3,3,3,3,3,3,3,3,4),(0.,2.57218162007852E-5,4.21568322569827E-5,6.45873314618037E-5,
7.58025810642142E-5,8.14102058654194E-5,8.28121120657208E-5,8.70178306666247E-5,
0.000116081955658545,0.000130526745999937,0.000162394111022054,0.000174035661333249,
0.000213138396956967,0.00025611693543107,0.000302406662851331,0.000348071322666473),
 .UNSPECIFIED.);
#4730=B_SPLINE_CURVE_WITH_KNOTS('',3,(#197735,#197736,#197737,#197738,#197739,
#197740,#197741,#197742,#197743,#197744,#197745,#197746,#197747,#197748,
#197749,#197750,#197751,#197752,#197753,#197754,#197755,#197756,#197757,
#197758,#197759,#197760,#197761,#197762,#197763,#197764,#197765,#197766,
#197767,#197768,#197769,#197770,#197771,#197772,#197773,#197774,#197775,
#197776,#197777,#197778,#197779,#197780,#197781,#197782,#197783,#197784,
#197785,#197786),.UNSPECIFIED.,.F.,.F.,(4,3,3,3,3,3,3,3,3,3,3,3,3,3,3,3,
3,4),(0.,4.2965215213286E-5,8.44519107492582E-5,0.000123669830860511,0.000159788877354162,
0.000170558847912629,0.000181218775907169,0.000181960046452393,0.000214460062644021,
0.000244755726199397,0.00025583827186895,0.000258503253867585,0.000261084955178762,
0.000289370476647532,0.000301101325502016,0.000321109510663643,0.000331113603244457,
0.00034111769582527),.UNSPECIFIED.);
#4731=B_SPLINE_CURVE_WITH_KNOTS('',3,(#197788,#197789,#197790,#197791,#197792,
#197793,#197794,#197795,#197796,#197797,#197798,#197799,#197800,#197801,
#197802,#197803,#197804,#197805,#197806,#197807,#197808,#197809,#197810,
#197811,#197812,#197813,#197814,#197815,#197816,#197817,#197818,#197819,
#197820,#197821,#197822,#197823,#197824,#197825,#197826,#197827,#197828,
#197829,#197830,#197831,#197832,#197833,#197834,#197835,#197836,#197837,
#197838,#197839),.UNSPECIFIED.,.F.,.F.,(4,3,3,3,3,3,3,3,3,3,3,3,3,3,3,3,
3,4),(0.,4.30706237867224E-5,8.4741708769075E-5,0.000124159989204539,0.000160467076288079,
0.000170998382116707,0.000182414994733804,0.000213747977645877,0.000242415955904902,
0.000256497573175047,0.00025916942289562,0.000261757777312425,0.00028996513040259,
0.000301877270772906,0.000321937017503147,0.000326951954185707,0.000334474359209547,
0.000341996764233387),.UNSPECIFIED.);
#4732=B_SPLINE_CURVE_WITH_KNOTS('',3,(#197840,#197841,#197842,#197843,#197844,
#197845,#197846,#197847,#197848,#197849,#197850,#197851,#197852,#197853,
#197854,#197855,#197856,#197857,#197858,#197859,#197860,#197861,#197862,
#197863,#197864,#197865,#197866,#197867,#197868,#197869,#197870,#197871,
#197872,#197873,#197874,#197875,#197876,#197877,#197878,#197879,#197880,
#197881,#197882,#197883,#197884,#197885,#197886,#197887,#197888,#197889,
#197890,#197891),.UNSPECIFIED.,.F.,.F.,(4,3,3,3,3,3,3,3,3,3,3,3,3,3,3,3,
3,4),(0.,2.58457451687167E-5,4.25394446195716E-5,6.4665986968707E-5,7.57292581432747E-5,
8.12608937305585E-5,8.26438026273795E-5,8.67925293178424E-5,0.000116015624428119,
0.000130188793976764,0.000151886926306224,0.00016196365121127,0.000162735992470954,
0.000173585058635685,0.000212487880460168,0.000255238173509542,0.000301397761142473,
0.000347170117271368),.UNSPECIFIED.);
#4733=B_SPLINE_CURVE_WITH_KNOTS('',3,(#197893,#197894,#197895,#197896,#197897,
#197898,#197899,#197900,#197901,#197902,#197903,#197904,#197905,#197906,
#197907,#197908,#197909,#197910,#197911,#197912,#197913,#197914,#197915,
#197916,#197917,#197918,#197919,#197920,#197921,#197922,#197923,#197924,
#197925,#197926,#197927,#197928,#197929,#197930,#197931,#197932,#197933,
#197934,#197935,#197936,#197937,#197938),.UNSPECIFIED.,.F.,.F.,(4,3,3,3,
3,3,3,3,3,3,3,3,3,3,3,4),(0.,2.57218161993116E-5,4.21568322567207E-5,6.458733146167E-5,
7.58025810641446E-5,8.14102058653819E-5,8.28121120656913E-5,8.70178306666193E-5,
0.000116081955658386,0.000130526745999929,0.000162394111022047,0.000174035661333239,
0.000213138396957292,0.000256116935431947,0.00030240666285341,0.000348071322666464),
 .UNSPECIFIED.);
#4734=B_SPLINE_CURVE_WITH_KNOTS('',3,(#197939,#197940,#197941,#197942,#197943,
#197944,#197945,#197946,#197947,#197948,#197949,#197950,#197951,#197952,
#197953,#197954,#197955,#197956,#197957,#197958,#197959,#197960,#197961,
#197962,#197963,#197964,#197965,#197966,#197967,#197968,#197969,#197970,
#197971,#197972,#197973,#197974,#197975,#197976,#197977,#197978,#197979,
#197980,#197981,#197982,#197983,#197984,#197985,#197986,#197987,#197988,
#197989,#197990),.UNSPECIFIED.,.F.,.F.,(4,3,3,3,3,3,3,3,3,3,3,3,3,3,3,3,
3,4),(0.,4.29652152170491E-5,8.44519107548311E-5,0.000123669830866424,0.000159788877359245,
0.000170558847912628,0.000181218775907168,0.000181960046452396,0.000214460062643474,
0.000244755726198156,0.000255838271868947,0.000258503253867582,0.00026108495517876,
0.000289370476647647,0.000301101325502013,0.00032110951066364,0.000331113603244453,
0.000341117695825266),.UNSPECIFIED.);
#4735=B_SPLINE_CURVE_WITH_KNOTS('',3,(#210566,#210567,#210568,#210569,#210570,
#210571,#210572,#210573,#210574,#210575,#210576,#210577,#210578,#210579,
#210580,#210581,#210582,#210583,#210584,#210585,#210586,#210587,#210588,
#210589,#210590,#210591,#210592,#210593,#210594,#210595,#210596,#210597,
#210598,#210599,#210600,#210601,#210602,#210603,#210604,#210605,#210606,
#210607,#210608),.UNSPECIFIED.,.F.,.F.,(4,3,3,3,3,3,3,3,3,3,3,3,3,3,4),
(1.00966327312713E-18,1.12890698065814E-5,7.65259667132928E-5,0.000102837507928491,
0.000112544869199234,0.000130746171581876,0.000194450729921123,0.000226303009090746,
0.000242229148675558,0.00025815528826037,0.000258291104876521,0.000327654633610499,
0.000399363990827472,0.000469709285179123,0.000516310576520739),
 .UNSPECIFIED.);
#4736=B_SPLINE_CURVE_WITH_KNOTS('',3,(#210616,#210617,#210618,#210619,#210620,
#210621,#210622,#210623,#210624,#210625,#210626,#210627,#210628,#210629,
#210630,#210631,#210632,#210633,#210634,#210635,#210636,#210637,#210638,
#210639,#210640,#210641,#210642,#210643,#210644,#210645,#210646,#210647,
#210648,#210649,#210650,#210651,#210652,#210653,#210654,#210655),
 .UNSPECIFIED.,.F.,.F.,(4,3,3,3,3,3,3,3,3,3,3,3,3,4),(4.33680868994202E-19,
6.84564250796869E-5,0.000138288406590208,0.000205407478923098,0.000256966021225852,
0.000257101146970264,0.000271589374668167,0.000352213067611634,0.000388398097499792,
0.000404123622054884,0.000459162957997706,0.000486682625969117,0.000500442459954822,
0.000514202293940528),.UNSPECIFIED.);
#4737=B_SPLINE_CURVE_WITH_KNOTS('',3,(#210659,#210660,#210661,#210662,#210663,
#210664,#210665,#210666,#210667,#210668,#210669,#210670,#210671,#210672,
#210673,#210674,#210675,#210676,#210677,#210678,#210679,#210680,#210681,
#210682,#210683,#210684,#210685,#210686,#210687,#210688,#210689,#210690,
#210691,#210692,#210693,#210694,#210695,#210696,#210697,#210698,#210699,
#210700,#210701),.UNSPECIFIED.,.F.,.F.,(4,3,3,3,3,3,3,3,3,3,3,3,3,3,4),
(8.67361737988403E-19,1.12890698065815E-5,7.65259667117838E-5,0.000102837507928496,
0.000112544869199238,0.00013074617158188,0.000194450729921126,0.000226303009090749,
0.000242229148675561,0.000258155288260372,0.000258291104876519,0.000327654633617137,
0.000399363990840869,0.000469709285198284,0.000516310576520743),
 .UNSPECIFIED.);
#4738=B_SPLINE_CURVE_WITH_KNOTS('',3,(#210709,#210710,#210711,#210712,#210713,
#210714,#210715,#210716,#210717,#210718,#210719,#210720,#210721,#210722,
#210723,#210724,#210725,#210726,#210727,#210728,#210729,#210730,#210731,
#210732,#210733,#210734,#210735,#210736,#210737,#210738,#210739,#210740,
#210741,#210742,#210743,#210744,#210745,#210746,#210747,#210748),
 .UNSPECIFIED.,.F.,.F.,(4,3,3,3,3,3,3,3,3,3,3,3,3,4),(4.33680868994202E-19,
6.84564250822044E-5,0.000138288406595129,0.000205407478930009,0.000256966021225841,
0.000257101146970262,0.000271589374668164,0.000352213067605997,0.000388398097499794,
0.000404123622054885,0.000459162957997704,0.000486682625969113,0.000500442459954818,
0.000514202293940523),.UNSPECIFIED.);
#4739=B_SPLINE_CURVE_WITH_KNOTS('',3,(#210752,#210753,#210754,#210755,#210756,
#210757,#210758,#210759,#210760,#210761,#210762,#210763,#210764,#210765,
#210766,#210767,#210768,#210769,#210770,#210771,#210772,#210773,#210774,
#210775,#210776,#210777,#210778,#210779,#210780,#210781,#210782,#210783,
#210784,#210785,#210786,#210787,#210788,#210789,#210790,#210791,#210792,
#210793,#210794),.UNSPECIFIED.,.F.,.F.,(4,3,3,3,3,3,3,3,3,3,3,3,3,3,4),
(1.73472347597681E-18,1.12890698065814E-5,7.65259667015125E-5,0.000102837507928481,
0.000112544869199225,0.000130746171581868,0.000194450729921122,0.000226303009090748,
0.000242229148675561,0.000258155288260375,0.000258291104876516,0.000327654633617638,
0.000399363990841712,0.000469709285199623,0.000516310576520747),
 .UNSPECIFIED.);
#4740=B_SPLINE_CURVE_WITH_KNOTS('',3,(#210802,#210803,#210804,#210805,#210806,
#210807,#210808,#210809,#210810,#210811,#210812,#210813,#210814,#210815,
#210816,#210817,#210818,#210819,#210820,#210821,#210822,#210823,#210824,
#210825,#210826,#210827,#210828,#210829,#210830,#210831,#210832,#210833,
#210834,#210835,#210836,#210837,#210838,#210839,#210840,#210841),
 .UNSPECIFIED.,.F.,.F.,(4,3,3,3,3,3,3,3,3,3,3,3,3,4),(8.67361737988404E-19,
6.84564250848222E-5,0.000138288406600658,0.000205407478938653,0.000256966021225847,
0.00025710114697026,0.000271589374668165,0.00035221306760003,0.000388398097499774,
0.000404123622054867,0.000459162957997694,0.000486682625969107,0.000500442459954813,
0.00051420229394052),.UNSPECIFIED.);
#4741=B_SPLINE_CURVE_WITH_KNOTS('',3,(#210845,#210846,#210847,#210848,#210849,
#210850,#210851,#210852,#210853,#210854,#210855,#210856,#210857,#210858,
#210859,#210860,#210861,#210862,#210863,#210864,#210865,#210866,#210867,
#210868,#210869,#210870,#210871,#210872,#210873,#210874,#210875,#210876,
#210877,#210878,#210879,#210880,#210881,#210882,#210883,#210884,#210885,
#210886,#210887),.UNSPECIFIED.,.F.,.F.,(4,3,3,3,3,3,3,3,3,3,3,3,3,3,4),
(0.,1.12890698065831E-5,7.65259667075185E-5,0.000102837507928526,0.000112544869199266,
0.000130746171581904,0.000194450729921138,0.000226303009090756,0.000242229148675564,
0.000258155288260373,0.0002582911048765,0.000327654633616213,0.000399363990838748,
0.000469709285194883,0.000516310576520745),.UNSPECIFIED.);
#4742=B_SPLINE_CURVE_WITH_KNOTS('',3,(#210895,#210896,#210897,#210898,#210899,
#210900,#210901,#210902,#210903,#210904,#210905,#210906,#210907,#210908,
#210909,#210910,#210911,#210912,#210913,#210914,#210915,#210916,#210917,
#210918,#210919,#210920,#210921,#210922,#210923,#210924,#210925,#210926,
#210927,#210928,#210929,#210930,#210931,#210932,#210933,#210934),
 .UNSPECIFIED.,.F.,.F.,(4,3,3,3,3,3,3,3,3,3,3,3,3,4),(1.30104260698261E-18,
6.84564250769938E-5,0.000138288406585387,0.000205407478917741,0.000256966021225848,
0.000257101146970264,0.000271589374668167,0.000352213067597738,0.000388398097499812,
0.000404123622054901,0.000459162957997714,0.000486682625969121,0.000500442459954824,
0.000514202293940527),.UNSPECIFIED.);
#4743=B_SPLINE_CURVE_WITH_KNOTS('',3,(#210938,#210939,#210940,#210941,#210942,
#210943,#210944,#210945,#210946,#210947,#210948,#210949,#210950,#210951,
#210952,#210953,#210954,#210955,#210956,#210957,#210958,#210959,#210960,
#210961,#210962,#210963,#210964,#210965,#210966,#210967,#210968,#210969,
#210970,#210971,#210972,#210973,#210974,#210975,#210976,#210977,#210978,
#210979,#210980),.UNSPECIFIED.,.F.,.F.,(4,3,3,3,3,3,3,3,3,3,3,3,3,3,4),
(3.49644694633735E-18,1.12890698065849E-5,7.65259667044717E-5,0.000102837507928498,
0.00011254486919924,0.000130746171581882,0.00019445072992113,0.000226303009090754,
0.000242229148675566,0.000258155288260378,0.000258291104876529,0.000327654633621337,
0.000399363990849304,0.000469709285210601,0.000516310576520752),
 .UNSPECIFIED.);
#4744=B_SPLINE_CURVE_WITH_KNOTS('',3,(#210988,#210989,#210990,#210991,#210992,
#210993,#210994,#210995,#210996,#210997,#210998,#210999,#211000,#211001,
#211002,#211003,#211004,#211005,#211006,#211007,#211008,#211009,#211010,
#211011,#211012,#211013,#211014,#211015,#211016,#211017,#211018,#211019,
#211020,#211021,#211022,#211023,#211024,#211025,#211026,#211027),
 .UNSPECIFIED.,.F.,.F.,(4,3,3,3,3,3,3,3,3,3,3,3,3,4),(1.30104260698261E-18,
6.84564250824312E-5,0.000138288406595942,0.000205407478931792,0.000256966021225845,
0.000257101146970262,0.00027158937466816,0.000352213067614797,0.000388398097499752,
0.000404123622054848,0.000459162957997682,0.000486682625969099,0.000500442459954807,
0.000514202293940516),.UNSPECIFIED.);
#4745=B_SPLINE_CURVE_WITH_KNOTS('',3,(#211031,#211032,#211033,#211034,#211035,
#211036,#211037,#211038,#211039,#211040,#211041,#211042,#211043,#211044,
#211045,#211046,#211047,#211048,#211049,#211050,#211051,#211052,#211053,
#211054,#211055,#211056,#211057,#211058,#211059,#211060,#211061,#211062,
#211063,#211064,#211065,#211066,#211067,#211068,#211069,#211070,#211071,
#211072,#211073),.UNSPECIFIED.,.F.,.F.,(4,3,3,3,3,3,3,3,3,3,3,3,3,3,4),
(0.,1.12890698065827E-5,7.65259667060974E-5,0.00010283750792849,0.000112544869199233,
0.000130746171581877,0.000194450729921129,0.000226303009090755,0.000242229148675568,
0.000258155288260381,0.000258291104876531,0.000327654633612254,0.000399363990830589,
0.000469709285182946,0.000516310576520763),.UNSPECIFIED.);
#4746=B_SPLINE_CURVE_WITH_KNOTS('',3,(#211081,#211082,#211083,#211084,#211085,
#211086,#211087,#211088,#211089,#211090,#211091,#211092,#211093,#211094,
#211095,#211096,#211097,#211098,#211099,#211100,#211101,#211102,#211103,
#211104,#211105,#211106,#211107,#211108,#211109,#211110,#211111,#211112,
#211113,#211114,#211115,#211116,#211117,#211118,#211119,#211120),
 .UNSPECIFIED.,.F.,.F.,(4,3,3,3,3,3,3,3,3,3,3,3,3,4),(2.60208521396521E-18,
6.84564250839596E-5,0.000138288406599065,0.00020540747893661,0.000256966021225842,
0.000257101146970262,0.000271589374668167,0.000352213067605811,0.000388398097499827,
0.000404123622054914,0.000459162957997718,0.00048668262596912,0.000500442459954821,
0.000514202293940522),.UNSPECIFIED.);
#4747=B_SPLINE_CURVE_WITH_KNOTS('',3,(#211124,#211125,#211126,#211127,#211128,
#211129,#211130,#211131,#211132,#211133,#211134,#211135,#211136,#211137,
#211138,#211139,#211140,#211141,#211142,#211143,#211144,#211145,#211146,
#211147,#211148,#211149,#211150,#211151,#211152,#211153,#211154,#211155,
#211156,#211157,#211158,#211159,#211160,#211161,#211162,#211163,#211164,
#211165,#211166),.UNSPECIFIED.,.F.,.F.,(4,3,3,3,3,3,3,3,3,3,3,3,3,3,4),
(0.,1.12890698065808E-5,7.65259667096804E-5,0.00010283750792849,0.000112544869199233,
0.000130746171581876,0.000194450729921126,0.000226303009090751,0.000242229148675564,
0.000258155288260376,0.000258291104876522,0.00032765463361035,0.000399363990827097,
0.000469709285178512,0.000516310576520752),.UNSPECIFIED.);
#4748=B_SPLINE_CURVE_WITH_KNOTS('',3,(#211174,#211175,#211176,#211177,#211178,
#211179,#211180,#211181,#211182,#211183,#211184,#211185,#211186,#211187,
#211188,#211189,#211190,#211191,#211192,#211193,#211194,#211195,#211196,
#211197,#211198,#211199,#211200,#211201,#211202,#211203,#211204,#211205,
#211206,#211207,#211208,#211209,#211210,#211211,#211212,#211213),
 .UNSPECIFIED.,.F.,.F.,(4,3,3,3,3,3,3,3,3,3,3,3,3,4),(0.,6.84564250845964E-5,
0.00013828840659994,0.000205407478937272,0.000256966021225841,0.000257101146970266,
0.000271589374668168,0.000352213067593158,0.000388398097499835,0.000404123622054922,
0.000459162957997727,0.00048668262596913,0.000500442459954831,0.000514202293940532),
 .UNSPECIFIED.);
#4749=B_SPLINE_CURVE_WITH_KNOTS('',3,(#211217,#211218,#211219,#211220,#211221,
#211222,#211223,#211224,#211225,#211226,#211227,#211228,#211229,#211230,
#211231,#211232,#211233,#211234,#211235,#211236,#211237,#211238,#211239,
#211240,#211241,#211242,#211243,#211244,#211245,#211246,#211247,#211248,
#211249,#211250,#211251,#211252,#211253,#211254,#211255,#211256,#211257,
#211258,#211259),.UNSPECIFIED.,.F.,.F.,(4,3,3,3,3,3,3,3,3,3,3,3,3,3,4),
(0.,1.12890698065865E-5,7.65259667038362E-5,0.000102837507928542,0.000112544869199282,
0.00013074617158192,0.00019445072992115,0.000226303009090765,0.000242229148675573,
0.000258155288260381,0.00025829110487653,0.000327654633624173,0.000399363990855843,
0.000469709285221651,0.000516310576520761),.UNSPECIFIED.);
#4750=B_SPLINE_CURVE_WITH_KNOTS('',3,(#211267,#211268,#211269,#211270,#211271,
#211272,#211273,#211274,#211275,#211276,#211277,#211278,#211279,#211280,
#211281,#211282,#211283,#211284,#211285,#211286,#211287,#211288,#211289,
#211290,#211291,#211292,#211293,#211294,#211295,#211296,#211297,#211298,
#211299,#211300,#211301,#211302,#211303,#211304,#211305,#211306),
 .UNSPECIFIED.,.F.,.F.,(4,3,3,3,3,3,3,3,3,3,3,3,3,4),(0.,6.84564250818784E-5,
0.000138288406593889,0.000205407478926654,0.000256966021225852,0.000257101146970261,
0.000271589374668155,0.000352213067609107,0.000388398097499764,0.000404123622054859,
0.000459162957997691,0.000486682625969106,0.000500442459954814,0.000514202293940522),
 .UNSPECIFIED.);
#4751=B_SPLINE_CURVE_WITH_KNOTS('',3,(#211310,#211311,#211312,#211313,#211314,
#211315,#211316,#211317,#211318,#211319,#211320,#211321,#211322,#211323,
#211324,#211325,#211326,#211327,#211328,#211329,#211330,#211331,#211332,
#211333,#211334,#211335,#211336,#211337,#211338,#211339,#211340,#211341,
#211342,#211343,#211344,#211345,#211346,#211347,#211348,#211349,#211350,
#211351,#211352),.UNSPECIFIED.,.F.,.F.,(4,3,3,3,3,3,3,3,3,3,3,3,3,3,4),
(0.,1.12890698065827E-5,7.65259666926421E-5,0.00010283750792851,0.000112544869199251,
0.000130746171581891,0.00019445072992113,0.00022630300909075,0.00024222914867556,
0.00025815528826037,0.000258291104876511,0.000327654633619911,0.000399363990845548,
0.000469709285203805,0.00051631057652074),.UNSPECIFIED.);
#4752=B_SPLINE_CURVE_WITH_KNOTS('',3,(#211360,#211361,#211362,#211363,#211364,
#211365,#211366,#211367,#211368,#211369,#211370,#211371,#211372,#211373,
#211374,#211375,#211376,#211377,#211378,#211379,#211380,#211381,#211382,
#211383,#211384,#211385,#211386,#211387,#211388,#211389,#211390,#211391,
#211392,#211393,#211394,#211395,#211396,#211397,#211398,#211399),
 .UNSPECIFIED.,.F.,.F.,(4,3,3,3,3,3,3,3,3,3,3,3,3,4),(0.,6.84564250825335E-5,
0.000138288406596393,0.000205407478932587,0.000256966021225845,0.000257101146970255,
0.000271589374668162,0.00035221306762113,0.00038839809749983,0.000404123622054915,
0.000459162957997712,0.000486682625969111,0.00050044245995481,0.000514202293940509),
 .UNSPECIFIED.);
#4753=B_SPLINE_CURVE_WITH_KNOTS('',3,(#211403,#211404,#211405,#211406,#211407,
#211408,#211409,#211410,#211411,#211412,#211413,#211414,#211415,#211416,
#211417,#211418,#211419,#211420,#211421,#211422,#211423,#211424,#211425,
#211426,#211427,#211428,#211429,#211430,#211431,#211432,#211433,#211434,
#211435,#211436,#211437,#211438,#211439,#211440,#211441,#211442,#211443,
#211444,#211445),.UNSPECIFIED.,.F.,.F.,(4,3,3,3,3,3,3,3,3,3,3,3,3,3,4),
(0.,1.12890698065864E-5,7.65259667099654E-5,0.000102837507928553,0.000112544869199291,
0.000130746171581926,0.000194450729921147,0.000226303009090758,0.000242229148675563,
0.000258155288260369,0.000258291104876501,0.000327654633610913,0.000399363990828535,
0.000469709285181062,0.000516310576520738),.UNSPECIFIED.);
#4754=B_SPLINE_CURVE_WITH_KNOTS('',3,(#211453,#211454,#211455,#211456,#211457,
#211458,#211459,#211460,#211461,#211462,#211463,#211464,#211465,#211466,
#211467,#211468,#211469,#211470,#211471,#211472,#211473,#211474,#211475,
#211476,#211477,#211478,#211479,#211480,#211481,#211482,#211483,#211484,
#211485,#211486,#211487,#211488,#211489,#211490,#211491,#211492),
 .UNSPECIFIED.,.F.,.F.,(4,3,3,3,3,3,3,3,3,3,3,3,3,4),(4.33680868994202E-19,
6.84564250886368E-5,0.000138288406607453,0.000205407478945846,0.000256966021225854,
0.000257101146970262,0.00027158937466817,0.000352213067613361,0.000388398097499844,
0.000404123622054929,0.000459162957997726,0.000486682625969125,0.000500442459954824,
0.000514202293940523),.UNSPECIFIED.);
#4755=B_SPLINE_CURVE_WITH_KNOTS('',3,(#211496,#211497,#211498,#211499,#211500,
#211501,#211502,#211503,#211504,#211505,#211506,#211507,#211508,#211509,
#211510,#211511,#211512,#211513,#211514,#211515,#211516,#211517,#211518,
#211519,#211520,#211521,#211522,#211523,#211524,#211525,#211526,#211527,
#211528,#211529,#211530,#211531,#211532,#211533,#211534,#211535,#211536,
#211537,#211538),.UNSPECIFIED.,.F.,.F.,(4,3,3,3,3,3,3,3,3,3,3,3,3,3,4),
(0.,1.12890698065847E-5,7.65259667058506E-5,0.000102837507928533,0.000112544869199273,
0.00013074617158191,0.000194450729921141,0.000226303009090757,0.000242229148675565,
0.000258155288260372,0.000258291104876516,0.000327654633608951,0.000399363990824417,
0.000469709285175076,0.000516310576520745),.UNSPECIFIED.);
#4756=B_SPLINE_CURVE_WITH_KNOTS('',3,(#211546,#211547,#211548,#211549,#211550,
#211551,#211552,#211553,#211554,#211555,#211556,#211557,#211558,#211559,
#211560,#211561,#211562,#211563,#211564,#211565,#211566,#211567,#211568,
#211569,#211570,#211571,#211572,#211573,#211574,#211575,#211576,#211577,
#211578,#211579,#211580,#211581,#211582,#211583,#211584,#211585),
 .UNSPECIFIED.,.F.,.F.,(4,3,3,3,3,3,3,3,3,3,3,3,3,4),(0.,6.84564250865644E-5,
0.000138288406603816,0.000205407478941927,0.000256966021225846,0.00025710114697026,
0.000271589374668163,0.000352213067623985,0.000388398097499785,0.000404123622054877,
0.000459162957997698,0.000486682625969109,0.000500442459954814,0.000514202293940519),
 .UNSPECIFIED.);
#4757=B_SPLINE_CURVE_WITH_KNOTS('',3,(#211589,#211590,#211591,#211592,#211593,
#211594,#211595,#211596,#211597,#211598,#211599,#211600,#211601,#211602,
#211603,#211604,#211605,#211606,#211607,#211608,#211609,#211610,#211611,
#211612,#211613,#211614,#211615,#211616,#211617,#211618,#211619,#211620,
#211621,#211622,#211623,#211624,#211625,#211626,#211627,#211628,#211629,
#211630,#211631),.UNSPECIFIED.,.F.,.F.,(4,3,3,3,3,3,3,3,3,3,3,3,3,3,4),
(0.,1.12890698065774E-5,7.65259667018237E-5,0.000102837507928468,0.000112544869199212,
0.000130746171581857,0.000194450729921116,0.000226303009090745,0.000242229148675559,
0.000258155288260374,0.000258291104876517,0.000327654633618882,0.000399363990844482,
0.000469709285204073,0.000516310576520747),.UNSPECIFIED.);
#4758=B_SPLINE_CURVE_WITH_KNOTS('',3,(#211639,#211640,#211641,#211642,#211643,
#211644,#211645,#211646,#211647,#211648,#211649,#211650,#211651,#211652,
#211653,#211654,#211655,#211656,#211657,#211658,#211659,#211660,#211661,
#211662,#211663,#211664,#211665,#211666,#211667,#211668,#211669,#211670,
#211671,#211672,#211673,#211674,#211675,#211676,#211677,#211678),
 .UNSPECIFIED.,.F.,.F.,(4,3,3,3,3,3,3,3,3,3,3,3,3,4),(0.,6.84564250816909E-5,
0.000138288406594364,0.000205407478929581,0.000256966021225844,0.000257101146970261,
0.000271589374668163,0.000352213067604973,0.000388398097499789,0.000404123622054881,
0.000459162957997701,0.000486682625969112,0.000500442459954817,0.000514202293940522),
 .UNSPECIFIED.);
#4759=B_SPLINE_CURVE_WITH_KNOTS('',3,(#211682,#211683,#211684,#211685,#211686,
#211687,#211688,#211689,#211690,#211691,#211692,#211693,#211694,#211695,
#211696,#211697,#211698,#211699,#211700,#211701,#211702,#211703,#211704,
#211705,#211706,#211707,#211708,#211709,#211710,#211711,#211712,#211713,
#211714,#211715,#211716,#211717,#211718,#211719,#211720,#211721,#211722,
#211723,#211724),.UNSPECIFIED.,.F.,.F.,(4,3,3,3,3,3,3,3,3,3,3,3,3,3,4),
(3.49644694633735E-18,1.12890698065813E-5,7.65259667019077E-5,0.000102837507928475,
0.000112544869199218,0.000130746171581863,0.000194450729921118,0.000226303009090746,
0.00024222914867556,0.000258155288260374,0.000258291104876514,0.00032765463360937,
0.000399363990824599,0.000469709285174166,0.000516310576520744),
 .UNSPECIFIED.);
#4760=B_SPLINE_CURVE_WITH_KNOTS('',3,(#211732,#211733,#211734,#211735,#211736,
#211737,#211738,#211739,#211740,#211741,#211742,#211743,#211744,#211745,
#211746,#211747,#211748,#211749,#211750,#211751,#211752,#211753,#211754,
#211755,#211756,#211757,#211758,#211759,#211760,#211761,#211762,#211763,
#211764,#211765,#211766,#211767,#211768,#211769,#211770,#211771),
 .UNSPECIFIED.,.F.,.F.,(4,3,3,3,3,3,3,3,3,3,3,3,3,4),(0.,6.84564250813522E-5,
0.00013828840659376,0.000205407478929029,0.000256966021225855,0.000257101146970262,
0.000271589374668161,0.000352213067597481,0.000388398097499751,0.000404123622054848,
0.000459162957997686,0.000486682625969105,0.000500442459954814,0.000514202293940524),
 .UNSPECIFIED.);
#4761=B_SPLINE_CURVE_WITH_KNOTS('',3,(#211775,#211776,#211777,#211778,#211779,
#211780,#211781,#211782,#211783,#211784,#211785,#211786,#211787,#211788,
#211789,#211790,#211791,#211792,#211793,#211794,#211795,#211796,#211797,
#211798,#211799,#211800,#211801,#211802,#211803,#211804,#211805,#211806,
#211807,#211808,#211809,#211810,#211811,#211812,#211813,#211814,#211815,
#211816,#211817),.UNSPECIFIED.,.F.,.F.,(4,3,3,3,3,3,3,3,3,3,3,3,3,3,4),
(1.73472347597681E-18,1.12890698065837E-5,7.65259667051301E-5,0.000102837507928518,
0.000112544869199259,0.000130746171581897,0.000194450729921133,0.000226303009090751,
0.00024222914867556,0.000258155288260369,0.000258291104876513,0.000327654633617816,
0.000399363990842313,0.000469709285200686,0.000516310576520726),
 .UNSPECIFIED.);
#4762=B_SPLINE_CURVE_WITH_KNOTS('',3,(#211825,#211826,#211827,#211828,#211829,
#211830,#211831,#211832,#211833,#211834,#211835,#211836,#211837,#211838,
#211839,#211840,#211841,#211842,#211843,#211844,#211845,#211846,#211847,
#211848,#211849,#211850,#211851,#211852,#211853,#211854,#211855,#211856,
#211857,#211858,#211859,#211860,#211861,#211862,#211863,#211864),
 .UNSPECIFIED.,.F.,.F.,(4,3,3,3,3,3,3,3,3,3,3,3,3,4),(0.,6.84564250894095E-5,
0.000138288406610231,0.000205407478953372,0.000256966021225845,0.000257101146970263,
0.000271589374668162,0.000352213067603236,0.000388398097499751,0.000404123622054848,
0.000459162957997687,0.000486682625969107,0.000500442459954817,0.000514202293940527),
 .UNSPECIFIED.);
#4763=B_SPLINE_CURVE_WITH_KNOTS('',3,(#211868,#211869,#211870,#211871,#211872,
#211873,#211874,#211875,#211876,#211877,#211878,#211879,#211880,#211881,
#211882,#211883,#211884,#211885,#211886,#211887,#211888,#211889,#211890,
#211891,#211892,#211893,#211894,#211895,#211896,#211897,#211898,#211899,
#211900,#211901,#211902,#211903,#211904,#211905,#211906,#211907,#211908,
#211909,#211910),.UNSPECIFIED.,.F.,.F.,(4,3,3,3,3,3,3,3,3,3,3,3,3,3,4),
(0.,1.12890698065877E-5,7.65259667073395E-5,0.000102837507928553,0.000112544869199292,
0.000130746171581928,0.000194450729921153,0.000226303009090765,0.000242229148675571,
0.000258155288260377,0.000258291104876526,0.000327654633615,0.00039936399083635,
0.000469709285191737,0.000516310576520754),.UNSPECIFIED.);
#4764=B_SPLINE_CURVE_WITH_KNOTS('',3,(#211918,#211919,#211920,#211921,#211922,
#211923,#211924,#211925,#211926,#211927,#211928,#211929,#211930,#211931,
#211932,#211933,#211934,#211935,#211936,#211937,#211938,#211939,#211940,
#211941,#211942,#211943,#211944,#211945,#211946,#211947,#211948,#211949,
#211950,#211951,#211952,#211953,#211954,#211955,#211956,#211957),
 .UNSPECIFIED.,.F.,.F.,(4,3,3,3,3,3,3,3,3,3,3,3,3,4),(0.,6.84564250787773E-5,
0.000138288406588452,0.000205407478920936,0.000256966021225854,0.000257101146970262,
0.000271589374668165,0.000352213067598457,0.000388398097499807,0.000404123622054896,
0.00045916295799771,0.000486682625969117,0.00050044245995482,0.000514202293940524),
 .UNSPECIFIED.);
#4765=B_SPLINE_CURVE_WITH_KNOTS('',3,(#211961,#211962,#211963,#211964,#211965,
#211966,#211967,#211968,#211969,#211970,#211971,#211972,#211973,#211974,
#211975,#211976,#211977,#211978,#211979,#211980,#211981,#211982,#211983,
#211984,#211985,#211986,#211987,#211988,#211989,#211990,#211991,#211992,
#211993,#211994,#211995,#211996,#211997,#211998,#211999,#212000,#212001,
#212002,#212003),.UNSPECIFIED.,.F.,.F.,(4,3,3,3,3,3,3,3,3,3,3,3,3,3,4),
(0.,1.12890698065883E-5,7.65259667085461E-5,0.00010283750792858,0.000112544869199317,
0.000130746171581948,0.000194450729921159,0.000226303009090765,0.000242229148675568,
0.00025815528826037,0.000258291104876529,0.000327654633609379,0.000399363990825211,
0.000469709285175903,0.000516310576520741),.UNSPECIFIED.);
#4766=B_SPLINE_CURVE_WITH_KNOTS('',3,(#212011,#212012,#212013,#212014,#212015,
#212016,#212017,#212018,#212019,#212020,#212021,#212022,#212023,#212024,
#212025,#212026,#212027,#212028,#212029,#212030,#212031,#212032,#212033,
#212034,#212035,#212036,#212037,#212038,#212039,#212040,#212041,#212042,
#212043,#212044,#212045,#212046,#212047,#212048,#212049,#212050),
 .UNSPECIFIED.,.F.,.F.,(4,3,3,3,3,3,3,3,3,3,3,3,3,4),(0.,6.84564250867182E-5,
0.000138288406604464,0.000205407478943975,0.000256966021225847,0.000257101146970263,
0.000271589374668164,0.000352213067606211,0.000388398097499806,0.000404123622054896,
0.000459162957997711,0.000486682625969118,0.000500442459954822,0.000514202293940525),
 .UNSPECIFIED.);
#4767=B_SPLINE_CURVE_WITH_KNOTS('',3,(#212054,#212055,#212056,#212057,#212058,
#212059,#212060,#212061,#212062,#212063,#212064,#212065,#212066,#212067,
#212068,#212069,#212070,#212071,#212072,#212073,#212074,#212075,#212076,
#212077,#212078,#212079,#212080,#212081,#212082,#212083,#212084,#212085,
#212086,#212087,#212088,#212089,#212090,#212091,#212092,#212093,#212094,
#212095,#212096),.UNSPECIFIED.,.F.,.F.,(4,3,3,3,3,3,3,3,3,3,3,3,3,3,4),
(8.67361737988404E-19,1.12890698065864E-5,7.65259667038092E-5,0.000102837507928523,
0.000112544869199264,0.000130746171581903,0.000194450729921138,0.000226303009090756,
0.000242229148675565,0.000258155288260374,0.000258291104876511,0.000327654633611257,
0.000399363990828871,0.000469709285181089,0.000516310576520747),
 .UNSPECIFIED.);
#4768=B_SPLINE_CURVE_WITH_KNOTS('',3,(#212104,#212105,#212106,#212107,#212108,
#212109,#212110,#212111,#212112,#212113,#212114,#212115,#212116,#212117,
#212118,#212119,#212120,#212121,#212122,#212123,#212124,#212125,#212126,
#212127,#212128,#212129,#212130,#212131,#212132,#212133,#212134,#212135,
#212136,#212137,#212138,#212139,#212140,#212141,#212142,#212143),
 .UNSPECIFIED.,.F.,.F.,(4,3,3,3,3,3,3,3,3,3,3,3,3,4),(4.33680868994202E-19,
6.84564250888431E-5,0.000138288406609379,0.000205407478952497,0.000256966021225853,
0.000257101146970263,0.000271589374668164,0.000352213067610745,0.000388398097499789,
0.000404123622054881,0.000459162957997703,0.000486682625969114,0.00050044245995482,
0.000514202293940525),.UNSPECIFIED.);
#4769=B_SPLINE_CURVE_WITH_KNOTS('',3,(#212147,#212148,#212149,#212150,#212151,
#212152,#212153,#212154,#212155,#212156,#212157,#212158,#212159,#212160,
#212161,#212162,#212163,#212164,#212165,#212166,#212167,#212168,#212169,
#212170,#212171,#212172,#212173,#212174,#212175,#212176,#212177,#212178,
#212179,#212180,#212181,#212182,#212183,#212184,#212185,#212186,#212187,
#212188,#212189),.UNSPECIFIED.,.F.,.F.,(4,3,3,3,3,3,3,3,3,3,3,3,3,3,4),
(1.73472347597681E-18,1.12890698065875E-5,7.65259667031789E-5,0.000102837507928535,
0.000112544869199274,0.000130746171581911,0.000194450729921138,0.000226303009090752,
0.000242229148675558,0.000258155288260365,0.000258291104876515,0.000327654633613017,
0.000399363990832523,0.000469709285186505,0.000516310576520729),
 .UNSPECIFIED.);
#4770=B_SPLINE_CURVE_WITH_KNOTS('',3,(#212197,#212198,#212199,#212200,#212201,
#212202,#212203,#212204,#212205,#212206,#212207,#212208,#212209,#212210,
#212211,#212212,#212213,#212214,#212215,#212216,#212217,#212218,#212219,
#212220,#212221,#212222,#212223,#212224,#212225,#212226,#212227,#212228,
#212229,#212230,#212231,#212232,#212233,#212234,#212235,#212236),
 .UNSPECIFIED.,.F.,.F.,(4,3,3,3,3,3,3,3,3,3,3,3,3,4),(0.,6.845642507945E-5,
0.00013828840658994,0.000205407478922911,0.000256966021225852,0.000257101146970265,
0.000271589374668169,0.000352213067613375,0.000388398097499794,0.000404123622054886,
0.000459162957997708,0.000486682625969119,0.000500442459954824,0.00051420229394053),
 .UNSPECIFIED.);
#4771=B_SPLINE_CURVE_WITH_KNOTS('',3,(#212240,#212241,#212242,#212243,#212244,
#212245,#212246,#212247,#212248,#212249,#212250,#212251,#212252,#212253,
#212254,#212255,#212256,#212257,#212258,#212259,#212260,#212261,#212262,
#212263,#212264,#212265,#212266,#212267,#212268,#212269,#212270,#212271,
#212272,#212273,#212274,#212275,#212276,#212277,#212278,#212279,#212280,
#212281,#212282),.UNSPECIFIED.,.F.,.F.,(4,3,3,3,3,3,3,3,3,3,3,3,3,3,4),
(0.,1.12890698065816E-5,7.65259667026669E-5,0.000102837507928515,0.000112544869199256,
0.000130746171581896,0.000194450729921135,0.000226303009090754,0.000242229148675564,
0.000258155288260373,0.000258291104876517,0.000327654633613867,0.000399363990833934,
0.0004697092851882,0.000516310576520747),.UNSPECIFIED.);
#4772=B_SPLINE_CURVE_WITH_KNOTS('',3,(#212290,#212291,#212292,#212293,#212294,
#212295,#212296,#212297,#212298,#212299,#212300,#212301,#212302,#212303,
#212304,#212305,#212306,#212307,#212308,#212309,#212310,#212311,#212312,
#212313,#212314,#212315,#212316,#212317,#212318,#212319,#212320,#212321,
#212322,#212323,#212324,#212325,#212326,#212327,#212328,#212329),
 .UNSPECIFIED.,.F.,.F.,(4,3,3,3,3,3,3,3,3,3,3,3,3,4),(0.,6.84564250866856E-5,
0.000138288406604513,0.000205407478944171,0.00025696602122585,0.00025710114697026,
0.000271589374668166,0.000352213067614554,0.00038839809749983,0.000404123622054916,
0.000459162957997718,0.000486682625969119,0.00050044245995482,0.00051420229394052),
 .UNSPECIFIED.);
#4773=B_SPLINE_CURVE_WITH_KNOTS('',3,(#212333,#212334,#212335,#212336,#212337,
#212338,#212339,#212340,#212341,#212342,#212343,#212344,#212345,#212346,
#212347,#212348,#212349,#212350,#212351,#212352,#212353,#212354,#212355,
#212356,#212357,#212358,#212359,#212360,#212361,#212362,#212363,#212364,
#212365,#212366,#212367,#212368,#212369,#212370,#212371,#212372,#212373,
#212374,#212375),.UNSPECIFIED.,.F.,.F.,(4,3,3,3,3,3,3,3,3,3,3,3,3,3,4),
(0.,1.12890698065806E-5,7.65259667141636E-5,0.000102837507928481,0.000112544869199224,
0.000130746171581867,0.000194450729921119,0.000226303009090746,0.000242229148675559,
0.000258155288260372,0.000258291104876518,0.000327654633616041,0.000399363990838671,
0.000469709285194909,0.000516310576520743),.UNSPECIFIED.);
#4774=B_SPLINE_CURVE_WITH_KNOTS('',3,(#212383,#212384,#212385,#212386,#212387,
#212388,#212389,#212390,#212391,#212392,#212393,#212394,#212395,#212396,
#212397,#212398,#212399,#212400,#212401,#212402,#212403,#212404,#212405,
#212406,#212407,#212408,#212409,#212410,#212411,#212412,#212413,#212414,
#212415,#212416,#212417,#212418,#212419,#212420,#212421,#212422),
 .UNSPECIFIED.,.F.,.F.,(4,3,3,3,3,3,3,3,3,3,3,3,3,4),(0.,6.84564250774396E-5,
0.000138288406586533,0.000205407478919854,0.000256966021225855,0.00025710114697026,
0.000271589374668168,0.000352213067602211,0.000388398097499803,0.000404123622054893,
0.000459162957997706,0.000486682625969113,0.000500442459954816,0.000514202293940519),
 .UNSPECIFIED.);
#4775=B_SPLINE_CURVE_WITH_KNOTS('',3,(#212426,#212427,#212428,#212429,#212430,
#212431,#212432,#212433,#212434,#212435,#212436,#212437,#212438,#212439,
#212440,#212441,#212442,#212443,#212444,#212445,#212446,#212447,#212448,
#212449,#212450,#212451,#212452,#212453,#212454,#212455,#212456,#212457,
#212458,#212459,#212460,#212461,#212462,#212463,#212464,#212465,#212466,
#212467,#212468),.UNSPECIFIED.,.F.,.F.,(4,3,3,3,3,3,3,3,3,3,3,3,3,3,4),
(0.,1.12890698065791E-5,7.65259667026007E-5,0.000102837507928491,0.000112544869199234,
0.000130746171581876,0.000194450729921125,0.00022630300909075,0.000242229148675562,
0.000258155288260374,0.000258291104876513,0.000327654633618617,0.000399363990843893,
0.000469709285202695,0.000516310576520748),.UNSPECIFIED.);
#4776=B_SPLINE_CURVE_WITH_KNOTS('',3,(#212476,#212477,#212478,#212479,#212480,
#212481,#212482,#212483,#212484,#212485,#212486,#212487,#212488,#212489,
#212490,#212491,#212492,#212493,#212494,#212495,#212496,#212497,#212498,
#212499,#212500,#212501,#212502,#212503,#212504,#212505,#212506,#212507,
#212508,#212509,#212510,#212511,#212512,#212513,#212514,#212515),
 .UNSPECIFIED.,.F.,.F.,(4,3,3,3,3,3,3,3,3,3,3,3,3,4),(0.,6.84564250846693E-5,
0.000138288406600395,0.000205407478938273,0.000256966021225847,0.000257101146970259,
0.000271589374668162,0.000352213067606228,0.000388398097499803,0.000404123622054892,
0.000459162957997705,0.000486682625969112,0.000500442459954815,0.000514202293940518),
 .UNSPECIFIED.);
#4777=B_SPLINE_CURVE_WITH_KNOTS('',3,(#212519,#212520,#212521,#212522,#212523,
#212524,#212525,#212526,#212527,#212528,#212529,#212530,#212531,#212532,
#212533,#212534,#212535,#212536,#212537,#212538,#212539,#212540,#212541,
#212542,#212543,#212544,#212545,#212546,#212547,#212548,#212549,#212550,
#212551,#212552,#212553,#212554,#212555,#212556,#212557,#212558,#212559,
#212560,#212561),.UNSPECIFIED.,.F.,.F.,(4,3,3,3,3,3,3,3,3,3,3,3,3,3,4),
(0.,1.12890698065812E-5,7.65259667018894E-5,0.000102837507928503,0.000112544869199245,
0.000130746171581885,0.000194450729921128,0.000226303009090749,0.00024222914867556,
0.00025815528826037,0.000258291104876506,0.000327654633607904,0.000399363990821826,
0.000469709285170662,0.000516310576520741),.UNSPECIFIED.);
#4778=B_SPLINE_CURVE_WITH_KNOTS('',3,(#212569,#212570,#212571,#212572,#212573,
#212574,#212575,#212576,#212577,#212578,#212579,#212580,#212581,#212582,
#212583,#212584,#212585,#212586,#212587,#212588,#212589,#212590,#212591,
#212592,#212593,#212594,#212595,#212596,#212597,#212598,#212599,#212600,
#212601,#212602,#212603,#212604,#212605,#212606,#212607,#212608),
 .UNSPECIFIED.,.F.,.F.,(4,3,3,3,3,3,3,3,3,3,3,3,3,4),(1.30104260698261E-18,
6.84564250830632E-5,0.000138288406597626,0.000205407478935301,0.000256966021225847,
0.000257101146970268,0.000271589374668169,0.00035221306760621,0.00038839809749974,
0.000404123622054839,0.000459162957997687,0.000486682625969111,0.000500442459954823,
0.000514202293940535),.UNSPECIFIED.);
#4779=B_SPLINE_CURVE_WITH_KNOTS('',3,(#212612,#212613,#212614,#212615,#212616,
#212617,#212618,#212619,#212620,#212621,#212622,#212623,#212624,#212625,
#212626,#212627,#212628,#212629,#212630,#212631,#212632,#212633,#212634,
#212635,#212636,#212637,#212638,#212639,#212640,#212641,#212642,#212643,
#212644,#212645,#212646,#212647,#212648,#212649,#212650,#212651,#212652,
#212653,#212654),.UNSPECIFIED.,.F.,.F.,(4,3,3,3,3,3,3,3,3,3,3,3,3,3,4),
(0.,1.12890698065819E-5,7.65259666993655E-5,0.000102837507928517,0.000112544869199258,
0.000130746171581898,0.000194450729921138,0.000226303009090758,0.000242229148675569,
0.000258155288260379,0.000258291104876534,0.000327654633615767,0.000399363990838623,
0.00046970928519652,0.000516310576520757),.UNSPECIFIED.);
#4780=B_SPLINE_CURVE_WITH_KNOTS('',3,(#212662,#212663,#212664,#212665,#212666,
#212667,#212668,#212669,#212670,#212671,#212672,#212673,#212674,#212675,
#212676,#212677,#212678,#212679,#212680,#212681,#212682,#212683,#212684,
#212685,#212686,#212687,#212688,#212689,#212690,#212691,#212692,#212693,
#212694,#212695,#212696,#212697,#212698,#212699,#212700,#212701),
 .UNSPECIFIED.,.F.,.F.,(4,3,3,3,3,3,3,3,3,3,3,3,3,4),(1.73472347597681E-18,
6.84564250816081E-5,0.000138288406594168,0.000205407478929045,0.000256966021225858,
0.000257101146970264,0.000271589374668166,0.000352213067603754,0.000388398097499799,
0.000404123622054889,0.000459162957997708,0.000486682625969117,0.000500442459954821,
0.000514202293940526),.UNSPECIFIED.);
#4781=B_SPLINE_CURVE_WITH_KNOTS('',3,(#212705,#212706,#212707,#212708,#212709,
#212710,#212711,#212712,#212713,#212714,#212715,#212716,#212717,#212718,
#212719,#212720,#212721,#212722,#212723,#212724,#212725,#212726,#212727,
#212728,#212729,#212730,#212731,#212732,#212733,#212734,#212735,#212736,
#212737,#212738,#212739,#212740,#212741,#212742,#212743,#212744,#212745,
#212746,#212747),.UNSPECIFIED.,.F.,.F.,(4,3,3,3,3,3,3,3,3,3,3,3,3,3,4),
(0.,1.12890698065796E-5,7.65259667013587E-5,0.000102837507928479,0.000112544869199222,
0.000130746171581866,0.00019445072992112,0.000226303009090747,0.00024222914867556,
0.000258155288260373,0.000258291104876525,0.000327654633618632,0.000399363990844032,
0.000469709285203426,0.000516310576520747),.UNSPECIFIED.);
#4782=B_SPLINE_CURVE_WITH_KNOTS('',3,(#212755,#212756,#212757,#212758,#212759,
#212760,#212761,#212762,#212763,#212764,#212765,#212766,#212767,#212768,
#212769,#212770,#212771,#212772,#212773,#212774,#212775,#212776,#212777,
#212778,#212779,#212780,#212781,#212782,#212783,#212784,#212785,#212786,
#212787,#212788,#212789,#212790,#212791,#212792,#212793,#212794),
 .UNSPECIFIED.,.F.,.F.,(4,3,3,3,3,3,3,3,3,3,3,3,3,4),(3.03576608295941E-18,
6.84564250824445E-5,0.000138288406596601,0.000205407478934739,0.000256966021225856,
0.000257101146970265,0.000271589374668165,0.000352213067598913,0.000388398097499742,
0.00040412362205484,0.000459162957997684,0.000486682625969106,0.000500442459954816,
0.000514202293940527),.UNSPECIFIED.);
#4783=B_SPLINE_CURVE_WITH_KNOTS('',3,(#212798,#212799,#212800,#212801,#212802,
#212803,#212804,#212805,#212806,#212807,#212808,#212809,#212810,#212811,
#212812,#212813,#212814,#212815,#212816,#212817,#212818,#212819,#212820,
#212821,#212822,#212823,#212824,#212825,#212826,#212827,#212828,#212829,
#212830,#212831,#212832,#212833,#212834,#212835,#212836,#212837,#212838,
#212839,#212840),.UNSPECIFIED.,.F.,.F.,(4,3,3,3,3,3,3,3,3,3,3,3,3,3,4),
(0.,1.12890698065835E-5,7.65259667091678E-5,0.000102837507928531,0.000112544869199271,
0.000130746171581909,0.000194450729921141,0.000226303009090757,0.000242229148675566,
0.000258155288260374,0.000258291104876515,0.000327654633617367,0.000399363990841117,
0.000469709285198328,0.000516310576520747),.UNSPECIFIED.);
#4784=B_SPLINE_CURVE_WITH_KNOTS('',3,(#212848,#212849,#212850,#212851,#212852,
#212853,#212854,#212855,#212856,#212857,#212858,#212859,#212860,#212861,
#212862,#212863,#212864,#212865,#212866,#212867,#212868,#212869,#212870,
#212871,#212872,#212873,#212874,#212875,#212876,#212877,#212878,#212879,
#212880,#212881,#212882,#212883,#212884,#212885,#212886,#212887),
 .UNSPECIFIED.,.F.,.F.,(4,3,3,3,3,3,3,3,3,3,3,3,3,4),(0.,6.84564250852912E-5,
0.000138288406602005,0.000205407478941458,0.000256966021225849,0.000257101146970268,
0.000271589374668176,0.000352213067603525,0.000388398097499865,0.000404123622054949,
0.000459162957997742,0.000486682625969139,0.000500442459954838,0.000514202293940536),
 .UNSPECIFIED.);
#4785=B_SPLINE_CURVE_WITH_KNOTS('',3,(#212891,#212892,#212893,#212894,#212895,
#212896,#212897,#212898,#212899,#212900,#212901,#212902,#212903,#212904,
#212905,#212906,#212907,#212908,#212909,#212910,#212911,#212912,#212913,
#212914,#212915,#212916,#212917,#212918,#212919,#212920,#212921,#212922,
#212923,#212924,#212925,#212926,#212927,#212928,#212929,#212930,#212931,
#212932,#212933),.UNSPECIFIED.,.F.,.F.,(4,3,3,3,3,3,3,3,3,3,3,3,3,3,4),
(0.,1.12890698065827E-5,7.65259667068948E-5,0.00010283750792852,0.00011254486919926,
0.000130746171581899,0.000194450729921134,0.000226303009090752,0.000242229148675561,
0.000258155288260369,0.000258291104876524,0.000327654633614918,0.000399363990836254,
0.000469709285191718,0.000516310576520739),.UNSPECIFIED.);
#4786=B_SPLINE_CURVE_WITH_KNOTS('',3,(#212941,#212942,#212943,#212944,#212945,
#212946,#212947,#212948,#212949,#212950,#212951,#212952,#212953,#212954,
#212955,#212956,#212957,#212958,#212959,#212960,#212961,#212962,#212963,
#212964,#212965,#212966,#212967,#212968,#212969,#212970,#212971,#212972,
#212973,#212974,#212975,#212976,#212977,#212978,#212979,#212980),
 .UNSPECIFIED.,.F.,.F.,(4,3,3,3,3,3,3,3,3,3,3,3,3,4),(0.,6.84564250828912E-5,
0.000138288406596643,0.000205407478932016,0.000256966021225854,0.000257101146970266,
0.000271589374668171,0.000352213067611571,0.000388398097499799,0.000404123622054891,
0.000459162957997711,0.000486682625969122,0.000500442459954827,0.000514202293940532),
 .UNSPECIFIED.);
#4787=B_SPLINE_CURVE_WITH_KNOTS('',3,(#212984,#212985,#212986,#212987,#212988,
#212989,#212990,#212991,#212992,#212993,#212994,#212995,#212996,#212997,
#212998,#212999,#213000,#213001,#213002,#213003,#213004,#213005,#213006,
#213007,#213008,#213009,#213010,#213011,#213012,#213013,#213014,#213015,
#213016,#213017,#213018,#213019,#213020,#213021,#213022,#213023,#213024,
#213025,#213026),.UNSPECIFIED.,.F.,.F.,(4,3,3,3,3,3,3,3,3,3,3,3,3,3,4),
(0.,1.12890698065862E-5,7.6525966702336E-5,0.000102837507928534,0.000112544869199274,
0.000130746171581911,0.000194450729921141,0.000226303009090756,0.000242229148675563,
0.00025815528826037,0.000258291104876527,0.000327654633615046,0.000399363990836708,
0.000469709285192809,0.000516310576520741),.UNSPECIFIED.);
#4788=B_SPLINE_CURVE_WITH_KNOTS('',3,(#213034,#213035,#213036,#213037,#213038,
#213039,#213040,#213041,#213042,#213043,#213044,#213045,#213046,#213047,
#213048,#213049,#213050,#213051,#213052,#213053,#213054,#213055,#213056,
#213057,#213058,#213059,#213060,#213061,#213062,#213063,#213064,#213065,
#213066,#213067,#213068,#213069,#213070,#213071,#213072,#213073),
 .UNSPECIFIED.,.F.,.F.,(4,3,3,3,3,3,3,3,3,3,3,3,3,4),(0.,6.84564250856532E-5,
0.000138288406601763,0.000205407478938914,0.000256966021225856,0.000257101146970268,
0.000271589374668171,0.00035221306760409,0.000388398097499817,0.000404123622054907,
0.000459162957997721,0.000486682625969128,0.000500442459954832,0.000514202293940535),
 .UNSPECIFIED.);
#4789=B_SPLINE_CURVE_WITH_KNOTS('',3,(#213077,#213078,#213079,#213080,#213081,
#213082,#213083,#213084,#213085,#213086,#213087,#213088,#213089,#213090,
#213091,#213092,#213093,#213094,#213095,#213096,#213097,#213098,#213099,
#213100,#213101,#213102,#213103,#213104,#213105,#213106,#213107,#213108,
#213109,#213110,#213111,#213112,#213113,#213114,#213115,#213116,#213117,
#213118,#213119),.UNSPECIFIED.,.F.,.F.,(4,3,3,3,3,3,3,3,3,3,3,3,3,3,4),
(0.,1.12890698065867E-5,7.65259667130106E-5,0.000102837507928551,0.00011254486919929,
0.000130746171581926,0.000194450729921151,0.000226303009090763,0.00024222914867557,
0.000258155288260376,0.000258291104876518,0.000327654633617211,0.000399363990841065,
0.000469709285198404,0.000516310576520752),.UNSPECIFIED.);
#4790=B_SPLINE_CURVE_WITH_KNOTS('',3,(#213127,#213128,#213129,#213130,#213131,
#213132,#213133,#213134,#213135,#213136,#213137,#213138,#213139,#213140,
#213141,#213142,#213143,#213144,#213145,#213146,#213147,#213148,#213149,
#213150,#213151,#213152,#213153,#213154,#213155,#213156,#213157,#213158,
#213159,#213160,#213161,#213162,#213163,#213164,#213165,#213166),
 .UNSPECIFIED.,.F.,.F.,(4,3,3,3,3,3,3,3,3,3,3,3,3,4),(0.,6.84564250819788E-5,
0.000138288406594927,0.000205407478930393,0.000256966021225853,0.000257101146970261,
0.000271589374668166,0.000352213067606589,0.000388398097499793,0.000404123622054884,
0.000459162957997703,0.000486682625969113,0.000500442459954818,0.000514202293940523),
 .UNSPECIFIED.);
#4791=B_SPLINE_CURVE_WITH_KNOTS('',3,(#213170,#213171,#213172,#213173,#213174,
#213175,#213176,#213177,#213178,#213179,#213180,#213181,#213182,#213183,
#213184,#213185,#213186,#213187,#213188,#213189,#213190,#213191,#213192,
#213193,#213194,#213195,#213196,#213197,#213198,#213199,#213200,#213201,
#213202,#213203,#213204,#213205,#213206,#213207,#213208,#213209,#213210,
#213211,#213212),.UNSPECIFIED.,.F.,.F.,(4,3,3,3,3,3,3,3,3,3,3,3,3,3,4),
(0.,1.12890698065856E-5,7.65259667056268E-5,0.000102837507928536,0.000112544869199275,
0.000130746171581911,0.000194450729921138,0.000226303009090751,0.000242229148675558,
0.000258155288260364,0.000258291104876502,0.000327654633618074,0.000399363990842774,
0.00046970928520123,0.000516310576520728),.UNSPECIFIED.);
#4792=B_SPLINE_CURVE_WITH_KNOTS('',3,(#213220,#213221,#213222,#213223,#213224,
#213225,#213226,#213227,#213228,#213229,#213230,#213231,#213232,#213233,
#213234,#213235,#213236,#213237,#213238,#213239,#213240,#213241,#213242,
#213243,#213244,#213245,#213246,#213247,#213248,#213249,#213250,#213251,
#213252,#213253,#213254,#213255,#213256,#213257,#213258,#213259),
 .UNSPECIFIED.,.F.,.F.,(4,3,3,3,3,3,3,3,3,3,3,3,3,4),(0.,6.84564250843941E-5,
0.000138288406600047,0.000205407478938544,0.000256966021225849,0.000257101146970261,
0.000271589374668161,0.000352213067598837,0.000388398097499768,0.000404123622054862,
0.000459162957997692,0.000486682625969107,0.000500442459954815,0.000514202293940522),
 .UNSPECIFIED.);
#4793=B_SPLINE_CURVE_WITH_KNOTS('',3,(#213263,#213264,#213265,#213266,#213267,
#213268,#213269,#213270,#213271,#213272,#213273,#213274,#213275,#213276,
#213277,#213278,#213279,#213280,#213281,#213282,#213283,#213284,#213285,
#213286,#213287,#213288,#213289,#213290,#213291,#213292,#213293,#213294,
#213295,#213296,#213297,#213298,#213299,#213300,#213301,#213302,#213303,
#213304,#213305),.UNSPECIFIED.,.F.,.F.,(4,3,3,3,3,3,3,3,3,3,3,3,3,3,4),
(0.,1.12890698065839E-5,7.65259667039472E-5,0.000102837507928521,0.000112544869199262,
0.000130746171581902,0.00019445072992114,0.000226303009090759,0.000242229148675569,
0.000258155288260379,0.000258291104876519,0.00032765463361463,0.000399363990835635,
0.000469709285190714,0.000516310576520757),.UNSPECIFIED.);
#4794=B_SPLINE_CURVE_WITH_KNOTS('',3,(#213312,#213313,#213314,#213315,#213316,
#213317,#213318,#213319,#213320,#213321,#213322,#213323,#213324,#213325,
#213326,#213327,#213328,#213329,#213330,#213331,#213332,#213333,#213334,
#213335,#213336,#213337,#213338,#213339,#213340,#213341,#213342,#213343,
#213344,#213345,#213346,#213347,#213348,#213349,#213350,#213351),
 .UNSPECIFIED.,.F.,.F.,(4,3,3,3,3,3,3,3,3,3,3,3,3,4),(0.,6.84564250787631E-5,
0.000138288406588445,0.000205407478920956,0.000256966021225842,0.000257101146970262,
0.000271589374668168,0.00035221306760281,0.000388398097499837,0.000404123622054923,
0.000459162957997723,0.000486682625969124,0.000500442459954824,0.000514202293940524),
 .UNSPECIFIED.);
#4795=B_SPLINE_CURVE_WITH_KNOTS('',3,(#213354,#213355,#213356,#213357,#213358,
#213359,#213360,#213361,#213362,#213363,#213364,#213365,#213366,#213367,
#213368,#213369,#213370,#213371,#213372,#213373,#213374,#213375,#213376,
#213377,#213378,#213379,#213380,#213381,#213382,#213383,#213384,#213385,
#213386,#213387,#213388,#213389,#213390,#213391,#213392,#213393,#213394,
#213395,#213396),.UNSPECIFIED.,.F.,.F.,(4,3,3,3,3,3,3,3,3,3,3,3,3,3,4),
(0.,1.1289069806579E-5,7.65259666957119E-5,0.000102837507928486,0.000112544869199229,
0.000130746171581871,0.00019445072992112,0.000226303009090744,0.000242229148675556,
0.000258155288260368,0.000258291104876506,0.000327654633618157,0.000399363990842572,
0.000469709285200546,0.000516310576520737),.UNSPECIFIED.);
#4796=B_SPLINE_CURVE_WITH_KNOTS('',3,(#213404,#213405,#213406,#213407,#213408,
#213409,#213410,#213411,#213412,#213413,#213414,#213415,#213416,#213417,
#213418,#213419,#213420,#213421,#213422,#213423,#213424,#213425,#213426,
#213427,#213428,#213429,#213430,#213431,#213432,#213433,#213434,#213435,
#213436,#213437,#213438,#213439,#213440,#213441,#213442,#213443),
 .UNSPECIFIED.,.F.,.F.,(4,3,3,3,3,3,3,3,3,3,3,3,3,4),(4.33680868994202E-19,
6.8456425087802E-5,0.000138288406606736,0.000205407478947457,0.00025696602122585,
0.00025710114697026,0.000271589374668168,0.000352213067608876,0.000388398097499855,
0.000404123622054938,0.000459162957997729,0.000486682625969124,0.000500442459954822,
0.00051420229394052),.UNSPECIFIED.);
#4797=B_SPLINE_CURVE_WITH_KNOTS('',3,(#213447,#213448,#213449,#213450,#213451,
#213452,#213453,#213454,#213455,#213456,#213457,#213458,#213459,#213460,
#213461,#213462,#213463,#213464,#213465,#213466,#213467,#213468,#213469,
#213470,#213471,#213472,#213473,#213474,#213475,#213476,#213477,#213478,
#213479,#213480,#213481,#213482,#213483,#213484,#213485,#213486,#213487,
#213488,#213489),.UNSPECIFIED.,.F.,.F.,(4,3,3,3,3,3,3,3,3,3,3,3,3,3,4),
(0.,1.12890698065821E-5,7.65259666989574E-5,0.000102837507928512,0.000112544869199253,
0.000130746171581893,0.000194450729921131,0.00022630300909075,0.000242229148675559,
0.000258155288260368,0.000258291104876505,0.000327654633622185,0.000399363990850742,
0.000469709285212212,0.000516310576520737),.UNSPECIFIED.);
#4798=B_SPLINE_CURVE_WITH_KNOTS('',3,(#213497,#213498,#213499,#213500,#213501,
#213502,#213503,#213504,#213505,#213506,#213507,#213508,#213509,#213510,
#213511,#213512,#213513,#213514,#213515,#213516,#213517,#213518,#213519,
#213520,#213521,#213522,#213523,#213524,#213525,#213526,#213527,#213528,
#213529,#213530,#213531,#213532,#213533,#213534,#213535,#213536),
 .UNSPECIFIED.,.F.,.F.,(4,3,3,3,3,3,3,3,3,3,3,3,3,4),(0.,6.84564250781753E-5,
0.000138288406587289,0.000205407478919208,0.00025696602122585,0.000257101146970262,
0.000271589374668164,0.000352213067607333,0.00038839809749979,0.000404123622054882,
0.000459162957997703,0.000486682625969114,0.000500442459954819,0.000514202293940525),
 .UNSPECIFIED.);
#4799=B_SPLINE_CURVE_WITH_KNOTS('',3,(#213540,#213541,#213542,#213543,#213544,
#213545,#213546,#213547,#213548,#213549,#213550,#213551,#213552,#213553,
#213554,#213555,#213556,#213557,#213558,#213559,#213560,#213561,#213562,
#213563,#213564,#213565,#213566,#213567,#213568,#213569,#213570,#213571,
#213572,#213573,#213574,#213575,#213576,#213577,#213578,#213579,#213580,
#213581,#213582),.UNSPECIFIED.,.F.,.F.,(4,3,3,3,3,3,3,3,3,3,3,3,3,3,4),
(0.,1.12890698065806E-5,7.65259667054612E-5,0.000102837507928489,0.000112544869199231,
0.000130746171581873,0.000194450729921119,0.000226303009090741,0.000242229148675553,
0.000258155288260364,0.000258291104876508,0.000327654633618402,0.000399363990843321,
0.000469709285201685,0.000516310576520728),.UNSPECIFIED.);
#4800=B_SPLINE_CURVE_WITH_KNOTS('',3,(#213590,#213591,#213592,#213593,#213594,
#213595,#213596,#213597,#213598,#213599,#213600,#213601,#213602,#213603,
#213604,#213605,#213606,#213607,#213608,#213609,#213610,#213611,#213612,
#213613,#213614,#213615,#213616,#213617,#213618,#213619,#213620,#213621,
#213622,#213623,#213624,#213625,#213626,#213627,#213628,#213629),
 .UNSPECIFIED.,.F.,.F.,(4,3,3,3,3,3,3,3,3,3,3,3,3,4),(4.33680868994202E-19,
6.84564250831933E-5,0.000138288406597582,0.000205407478934626,0.000256966021225843,
0.000257101146970263,0.000271589374668168,0.000352213067601041,0.00038839809749985,
0.000404123622054935,0.00045916295799773,0.000486682625969128,0.000500442459954826,
0.000514202293940525),.UNSPECIFIED.);
#4801=B_SPLINE_CURVE_WITH_KNOTS('',3,(#213633,#213634,#213635,#213636,#213637,
#213638,#213639,#213640,#213641,#213642,#213643,#213644,#213645,#213646,
#213647,#213648,#213649,#213650,#213651,#213652,#213653,#213654,#213655,
#213656,#213657,#213658,#213659,#213660,#213661,#213662,#213663,#213664,
#213665,#213666,#213667,#213668,#213669,#213670,#213671,#213672,#213673,
#213674,#213675),.UNSPECIFIED.,.F.,.F.,(4,3,3,3,3,3,3,3,3,3,3,3,3,3,4),
(0.,1.12890698065816E-5,7.6525966705804E-5,0.000102837507928503,0.000112544869199245,
0.000130746171581886,0.000194450729921129,0.000226303009090751,0.000242229148675562,
0.000258155288260373,0.000258291104876505,0.000327654633620337,0.000399363990847408,
0.000469709285207948,0.000516310576520746),.UNSPECIFIED.);
#4802=B_SPLINE_CURVE_WITH_KNOTS('',3,(#213683,#213684,#213685,#213686,#213687,
#213688,#213689,#213690,#213691,#213692,#213693,#213694,#213695,#213696,
#213697,#213698,#213699,#213700,#213701,#213702,#213703,#213704,#213705,
#213706,#213707,#213708,#213709,#213710,#213711,#213712,#213713,#213714,
#213715,#213716,#213717,#213718,#213719,#213720,#213721,#213722),
 .UNSPECIFIED.,.F.,.F.,(4,3,3,3,3,3,3,3,3,3,3,3,3,4),(1.30104260698261E-18,
6.8456425086901E-5,0.000138288406605303,0.000205407478945984,0.00025696602122585,
0.000257101146970262,0.000271589374668163,0.000352213067612747,0.000388398097499783,
0.000404123622054875,0.000459162957997699,0.000486682625969111,0.000500442459954817,
0.000514202293940523),.UNSPECIFIED.);
#4803=B_SPLINE_CURVE_WITH_KNOTS('',3,(#213726,#213727,#213728,#213729,#213730,
#213731,#213732,#213733,#213734,#213735,#213736,#213737,#213738,#213739,
#213740,#213741,#213742,#213743,#213744,#213745,#213746,#213747,#213748,
#213749,#213750,#213751,#213752,#213753,#213754,#213755,#213756,#213757,
#213758,#213759,#213760,#213761,#213762,#213763,#213764,#213765,#213766,
#213767,#213768),.UNSPECIFIED.,.F.,.F.,(4,3,3,3,3,3,3,3,3,3,3,3,3,3,4),
(0.,1.12890698065817E-5,7.65259667124228E-5,0.000102837507928514,0.000112544869199255,
0.000130746171581895,0.000194450729921135,0.000226303009090755,0.000242229148675565,
0.000258155288260375,0.000258291104876506,0.000327654633614057,0.000399363990834877,
0.00046970928519008,0.000516310576520749),.UNSPECIFIED.);
#4804=B_SPLINE_CURVE_WITH_KNOTS('',3,(#213776,#213777,#213778,#213779,#213780,
#213781,#213782,#213783,#213784,#213785,#213786,#213787,#213788,#213789,
#213790,#213791,#213792,#213793,#213794,#213795,#213796,#213797,#213798,
#213799,#213800,#213801,#213802,#213803,#213804,#213805,#213806,#213807,
#213808,#213809,#213810,#213811,#213812,#213813,#213814,#213815),
 .UNSPECIFIED.,.F.,.F.,(4,3,3,3,3,3,3,3,3,3,3,3,3,4),(0.,6.8456425084337E-5,
0.000138288406599689,0.000205407478937187,0.000256966021225854,0.000257101146970268,
0.00027158937466817,0.000352213067599072,0.000388398097499823,0.000404123622054912,
0.000459162957997724,0.00048668262596913,0.000500442459954833,0.000514202293940536),
 .UNSPECIFIED.);
#4805=B_SPLINE_CURVE_WITH_KNOTS('',3,(#213819,#213820,#213821,#213822,#213823,
#213824,#213825,#213826,#213827,#213828,#213829,#213830,#213831,#213832,
#213833,#213834,#213835,#213836,#213837,#213838,#213839,#213840,#213841,
#213842,#213843,#213844,#213845,#213846,#213847,#213848,#213849,#213850,
#213851,#213852,#213853,#213854,#213855,#213856,#213857,#213858,#213859,
#213860,#213861),.UNSPECIFIED.,.F.,.F.,(4,3,3,3,3,3,3,3,3,3,3,3,3,3,4),
(0.,1.12890698065782E-5,7.65259667090296E-5,0.0001028375079285,0.000112544869199242,
0.000130746171581883,0.000194450729921127,0.00022630300909075,0.000242229148675561,
0.000258155288260372,0.000258291104876505,0.000327654633625998,0.00039936399085858,
0.000469709285223216,0.000516310576520744),.UNSPECIFIED.);
#4806=B_SPLINE_CURVE_WITH_KNOTS('',3,(#213869,#213870,#213871,#213872,#213873,
#213874,#213875,#213876,#213877,#213878,#213879,#213880,#213881,#213882,
#213883,#213884,#213885,#213886,#213887,#213888,#213889,#213890,#213891,
#213892,#213893,#213894,#213895,#213896,#213897,#213898,#213899,#213900,
#213901,#213902,#213903,#213904,#213905,#213906,#213907,#213908),
 .UNSPECIFIED.,.F.,.F.,(4,3,3,3,3,3,3,3,3,3,3,3,3,4),(8.67361737988404E-19,
6.84564250816429E-5,0.000138288406594391,0.000205407478929637,0.000256966021225841,
0.000257101146970264,0.000271589374668172,0.000352213067612495,0.000388398097499806,
0.000404123622054896,0.000459162957997711,0.000486682625969119,0.000500442459954823,
0.000514202293940526),.UNSPECIFIED.);
#4807=B_SPLINE_CURVE_WITH_KNOTS('',3,(#213912,#213913,#213914,#213915,#213916,
#213917,#213918,#213919,#213920,#213921,#213922,#213923,#213924,#213925,
#213926,#213927,#213928,#213929,#213930,#213931,#213932,#213933,#213934,
#213935,#213936,#213937,#213938,#213939,#213940,#213941,#213942,#213943,
#213944,#213945,#213946,#213947,#213948,#213949,#213950,#213951,#213952,
#213953,#213954),.UNSPECIFIED.,.F.,.F.,(4,3,3,3,3,3,3,3,3,3,3,3,3,3,4),
(0.,1.12890698065835E-5,7.6525966723323E-5,0.000102837507928538,0.000112544869199278,
0.000130746171581915,0.000194450729921145,0.00022630300909076,0.000242229148675568,
0.000258155288260375,0.000258291104876509,0.000327654633610471,0.000399363990827954,
0.000469709285180224,0.000516310576520751),.UNSPECIFIED.);
#4808=B_SPLINE_CURVE_WITH_KNOTS('',3,(#213962,#213963,#213964,#213965,#213966,
#213967,#213968,#213969,#213970,#213971,#213972,#213973,#213974,#213975,
#213976,#213977,#213978,#213979,#213980,#213981,#213982,#213983,#213984,
#213985,#213986,#213987,#213988,#213989,#213990,#213991,#213992,#213993,
#213994,#213995,#213996,#213997,#213998,#213999,#214000,#214001),
 .UNSPECIFIED.,.F.,.F.,(4,3,3,3,3,3,3,3,3,3,3,3,3,4),(0.,6.8456425088049E-5,
0.00013828840660642,0.000205407478945175,0.00025696602122584,0.000257101146970266,
0.000271589374668167,0.000352213067609995,0.000388398097499859,0.000404123622054943,
0.000459162957997738,0.000486682625969135,0.000500442459954834,0.000514202293940532),
 .UNSPECIFIED.);
#4809=B_SPLINE_CURVE_WITH_KNOTS('',3,(#214005,#214006,#214007,#214008,#214009,
#214010,#214011,#214012,#214013,#214014,#214015,#214016,#214017,#214018,
#214019,#214020,#214021,#214022,#214023,#214024,#214025,#214026,#214027,
#214028,#214029,#214030,#214031,#214032,#214033,#214034,#214035,#214036,
#214037,#214038,#214039,#214040,#214041,#214042,#214043,#214044,#214045,
#214046,#214047),.UNSPECIFIED.,.F.,.F.,(4,3,3,3,3,3,3,3,3,3,3,3,3,3,4),
(0.,1.12890698065781E-5,7.65259667000974E-5,0.000102837507928479,0.000112544869199222,
0.000130746171581865,0.000194450729921117,0.000226303009090743,0.000242229148675556,
0.000258155288260369,0.000258291104876513,0.000327654633621327,0.000399363990848474,
0.000469709285207863,0.000516310576520738),.UNSPECIFIED.);
#4810=B_SPLINE_CURVE_WITH_KNOTS('',3,(#214055,#214056,#214057,#214058,#214059,
#214060,#214061,#214062,#214063,#214064,#214065,#214066,#214067,#214068,
#214069,#214070,#214071,#214072,#214073,#214074,#214075,#214076,#214077,
#214078,#214079,#214080,#214081,#214082,#214083,#214084,#214085,#214086,
#214087,#214088,#214089,#214090,#214091,#214092,#214093,#214094),
 .UNSPECIFIED.,.F.,.F.,(4,3,3,3,3,3,3,3,3,3,3,3,3,4),(0.,6.84564250764968E-5,
0.000138288406584722,0.000205407478917204,0.000256966021225873,0.000257101146970265,
0.000271589374668165,0.000352213067601251,0.000388398097499829,0.000404123622054916,
0.000459162957997723,0.000486682625969127,0.000500442459954828,0.00051420229394053),
 .UNSPECIFIED.);
#4811=B_SPLINE_CURVE_WITH_KNOTS('',3,(#214098,#214099,#214100,#214101,#214102,
#214103,#214104,#214105,#214106,#214107,#214108,#214109,#214110,#214111,
#214112,#214113,#214114,#214115,#214116,#214117,#214118,#214119,#214120,
#214121,#214122,#214123,#214124,#214125,#214126,#214127,#214128,#214129,
#214130,#214131,#214132,#214133,#214134,#214135,#214136,#214137,#214138,
#214139,#214140),.UNSPECIFIED.,.F.,.F.,(4,3,3,3,3,3,3,3,3,3,3,3,3,3,4),
(0.,1.12890698065823E-5,7.6525966699459E-5,0.000102837507928546,0.000112544869199285,
0.000130746171581921,0.000194450729921148,0.000226303009090761,0.000242229148675567,
0.000258155288260374,0.000258291104876522,0.000327654633612774,0.000399363990831956,
0.000469709285185906,0.000516310576520748),.UNSPECIFIED.);
#4812=B_SPLINE_CURVE_WITH_KNOTS('',3,(#214148,#214149,#214150,#214151,#214152,
#214153,#214154,#214155,#214156,#214157,#214158,#214159,#214160,#214161,
#214162,#214163,#214164,#214165,#214166,#214167,#214168,#214169,#214170,
#214171,#214172,#214173,#214174,#214175,#214176,#214177,#214178,#214179,
#214180,#214181,#214182,#214183,#214184,#214185,#214186,#214187),
 .UNSPECIFIED.,.F.,.F.,(4,3,3,3,3,3,3,3,3,3,3,3,3,4),(2.16840434497101E-18,
6.84564250792317E-5,0.000138288406589936,0.000205407478924871,0.000256966021225843,
0.000257101146970267,0.000271589374668169,0.000352213067585113,0.00038839809749978,
0.000404123622054874,0.000459162957997703,0.000486682625969117,0.000500442459954824,
0.000514202293940531),.UNSPECIFIED.);
#4813=B_SPLINE_CURVE_WITH_KNOTS('',3,(#214191,#214192,#214193,#214194,#214195,
#214196,#214197,#214198,#214199,#214200,#214201,#214202,#214203,#214204,
#214205,#214206,#214207,#214208,#214209,#214210,#214211,#214212,#214213,
#214214,#214215,#214216,#214217,#214218,#214219,#214220,#214221,#214222,
#214223,#214224,#214225,#214226,#214227,#214228,#214229,#214230,#214231,
#214232,#214233),.UNSPECIFIED.,.F.,.F.,(4,3,3,3,3,3,3,3,3,3,3,3,3,3,4),
(0.,1.12890698065786E-5,7.65259667078253E-5,0.000102837507928478,0.000112544869199221,
0.000130746171581865,0.00019445072992112,0.000226303009090747,0.000242229148675561,
0.000258155288260374,0.000258291104876519,0.000327654633616867,0.000399363990839437,
0.000469709285194635,0.000516310576520749),.UNSPECIFIED.);
#4814=B_SPLINE_CURVE_WITH_KNOTS('',3,(#214241,#214242,#214243,#214244,#214245,
#214246,#214247,#214248,#214249,#214250,#214251,#214252,#214253,#214254,
#214255,#214256,#214257,#214258,#214259,#214260,#214261,#214262,#214263,
#214264,#214265,#214266,#214267,#214268,#214269,#214270,#214271,#214272,
#214273,#214274,#214275,#214276,#214277,#214278,#214279,#214280),
 .UNSPECIFIED.,.F.,.F.,(4,3,3,3,3,3,3,3,3,3,3,3,3,4),(0.,6.84564250887403E-5,
0.000138288406608633,0.000205407478950316,0.000256966021225859,0.000257101146970265,
0.000271589374668167,0.000352213067601687,0.000388398097499787,0.00040412362205488,
0.000459162957997705,0.000486682625969117,0.000500442459954824,0.00051420229394053),
 .UNSPECIFIED.);
#4815=B_SPLINE_CURVE_WITH_KNOTS('',3,(#214284,#214285,#214286,#214287,#214288,
#214289,#214290,#214291,#214292,#214293,#214294,#214295,#214296,#214297,
#214298,#214299,#214300,#214301,#214302,#214303,#214304,#214305,#214306,
#214307,#214308,#214309,#214310,#214311,#214312,#214313,#214314,#214315,
#214316,#214317,#214318,#214319,#214320,#214321,#214322,#214323,#214324,
#214325,#214326),.UNSPECIFIED.,.F.,.F.,(4,3,3,3,3,3,3,3,3,3,3,3,3,3,4),
(0.,1.12890698065784E-5,7.65259667061265E-5,0.000102837507928456,0.000112544869199201,
0.000130746171581848,0.000194450729921111,0.000226303009090743,0.000242229148675559,
0.000258155288260375,0.000258291104876522,0.000327654633623582,0.000399363990853684,
0.00046970928521631,0.00051631057652075),.UNSPECIFIED.);
#4816=B_SPLINE_CURVE_WITH_KNOTS('',3,(#214334,#214335,#214336,#214337,#214338,
#214339,#214340,#214341,#214342,#214343,#214344,#214345,#214346,#214347,
#214348,#214349,#214350,#214351,#214352,#214353,#214354,#214355,#214356,
#214357,#214358,#214359,#214360,#214361,#214362,#214363,#214364,#214365,
#214366,#214367,#214368,#214369,#214370,#214371,#214372,#214373),
 .UNSPECIFIED.,.F.,.F.,(4,3,3,3,3,3,3,3,3,3,3,3,3,4),(0.,6.84564250746384E-5,
0.000138288406580315,0.000205407478909537,0.000256966021225844,0.000257101146970262,
0.000271589374668164,0.000352213067601251,0.000388398097499803,0.000404123622054893,
0.000459162957997708,0.000486682625969115,0.000500442459954819,0.000514202293940523),
 .UNSPECIFIED.);
#4817=B_SPLINE_CURVE_WITH_KNOTS('',3,(#214377,#214378,#214379,#214380,#214381,
#214382,#214383,#214384,#214385,#214386,#214387,#214388,#214389,#214390,
#214391,#214392,#214393,#214394,#214395,#214396,#214397,#214398,#214399,
#214400,#214401,#214402,#214403,#214404,#214405,#214406,#214407,#214408,
#214409,#214410,#214411,#214412,#214413,#214414,#214415,#214416,#214417,
#214418,#214419),.UNSPECIFIED.,.F.,.F.,(4,3,3,3,3,3,3,3,3,3,3,3,3,3,4),
(0.,1.1289069806584E-5,7.65259667114897E-5,0.000102837507928548,0.000112544869199287,
0.000130746171581922,0.000194450729921144,0.000226303009090756,0.000242229148675561,
0.000258155288260367,0.000258291104876515,0.000327654633614386,0.000399363990835393,
0.00046970928519037,0.000516310576520734),.UNSPECIFIED.);
#4818=B_SPLINE_CURVE_WITH_KNOTS('',3,(#214427,#214428,#214429,#214430,#214431,
#214432,#214433,#214434,#214435,#214436,#214437,#214438,#214439,#214440,
#214441,#214442,#214443,#214444,#214445,#214446,#214447,#214448,#214449,
#214450,#214451,#214452,#214453,#214454,#214455,#214456,#214457,#214458,
#214459,#214460,#214461,#214462,#214463,#214464,#214465,#214466),
 .UNSPECIFIED.,.F.,.F.,(4,3,3,3,3,3,3,3,3,3,3,3,3,4),(0.,6.84564250820019E-5,
0.000138288406594776,0.000205407478930105,0.000256966021225842,0.000257101146970264,
0.000271589374668166,0.000352213067593631,0.000388398097499784,0.000404123622054877,
0.000459162957997702,0.000486682625969115,0.000500442459954821,0.000514202293940528),
 .UNSPECIFIED.);
#4819=B_SPLINE_CURVE_WITH_KNOTS('',3,(#214470,#214471,#214472,#214473,#214474,
#214475,#214476,#214477,#214478,#214479,#214480,#214481,#214482,#214483,
#214484,#214485,#214486,#214487,#214488,#214489,#214490,#214491,#214492,
#214493,#214494,#214495,#214496,#214497,#214498,#214499,#214500,#214501,
#214502,#214503,#214504,#214505,#214506,#214507,#214508,#214509,#214510,
#214511,#214512),.UNSPECIFIED.,.F.,.F.,(4,3,3,3,3,3,3,3,3,3,3,3,3,3,4),
(0.,1.12890698065801E-5,7.65259667059785E-5,0.000102837507928484,0.000112544869199227,
0.000130746171581871,0.000194450729921124,0.000226303009090751,0.000242229148675564,
0.000258155288260378,0.000258291104876511,0.000327654633620538,0.000399363990847956,
0.000469709285209015,0.000516310576520756),.UNSPECIFIED.);
#4820=B_SPLINE_CURVE_WITH_KNOTS('',3,(#214520,#214521,#214522,#214523,#214524,
#214525,#214526,#214527,#214528,#214529,#214530,#214531,#214532,#214533,
#214534,#214535,#214536,#214537,#214538,#214539,#214540,#214541,#214542,
#214543,#214544,#214545,#214546,#214547,#214548,#214549,#214550,#214551,
#214552,#214553,#214554,#214555,#214556,#214557,#214558,#214559),
 .UNSPECIFIED.,.F.,.F.,(4,3,3,3,3,3,3,3,3,3,3,3,3,4),(0.,6.84564250772788E-5,
0.00013828840658568,0.00020540747891715,0.000256966021225849,0.000257101146970263,
0.000271589374668166,0.000352213067611876,0.000388398097499787,0.000404123622054879,
0.000459162957997702,0.000486682625969114,0.00050044245995482,0.000514202293940525),
 .UNSPECIFIED.);
#4821=B_SPLINE_CURVE_WITH_KNOTS('',3,(#214563,#214564,#214565,#214566,#214567,
#214568,#214569,#214570,#214571,#214572,#214573,#214574,#214575,#214576,
#214577,#214578,#214579,#214580,#214581,#214582,#214583,#214584,#214585,
#214586,#214587,#214588,#214589,#214590,#214591,#214592,#214593,#214594,
#214595,#214596,#214597,#214598,#214599,#214600,#214601,#214602,#214603,
#214604,#214605),.UNSPECIFIED.,.F.,.F.,(4,3,3,3,3,3,3,3,3,3,3,3,3,3,4),
(1.73472347597681E-18,1.1289069806587E-5,7.65259666978257E-5,0.000102837507928504,
0.000112544869199246,0.000130746171581887,0.00019445072992113,0.000226303009090752,
0.000242229148675562,0.000258155288260373,0.000258291104876518,0.00032765463361364,
0.000399363990833812,0.000469709285188545,0.000516310576520745),
 .UNSPECIFIED.);
#4822=B_SPLINE_CURVE_WITH_KNOTS('',3,(#214613,#214614,#214615,#214616,#214617,
#214618,#214619,#214620,#214621,#214622,#214623,#214624,#214625,#214626,
#214627,#214628,#214629,#214630,#214631,#214632,#214633,#214634,#214635,
#214636,#214637,#214638,#214639,#214640,#214641,#214642,#214643,#214644,
#214645,#214646,#214647,#214648,#214649,#214650,#214651,#214652),
 .UNSPECIFIED.,.F.,.F.,(4,3,3,3,3,3,3,3,3,3,3,3,3,4),(0.,6.845642508068E-5,
0.000138288406592413,0.000205407478926651,0.000256966021225851,0.000257101146970266,
0.000271589374668168,0.000352213067602528,0.000388398097499775,0.000404123622054869,
0.0004591629579977,0.000486682625969116,0.000500442459954824,0.000514202293940531),
 .UNSPECIFIED.);
#4823=B_SPLINE_CURVE_WITH_KNOTS('',3,(#214656,#214657,#214658,#214659,#214660,
#214661,#214662,#214663,#214664,#214665,#214666,#214667,#214668,#214669,
#214670,#214671,#214672,#214673,#214674,#214675,#214676,#214677,#214678,
#214679,#214680,#214681,#214682,#214683,#214684,#214685,#214686,#214687,
#214688,#214689,#214690,#214691,#214692,#214693,#214694,#214695,#214696,
#214697,#214698),.UNSPECIFIED.,.F.,.F.,(4,3,3,3,3,3,3,3,3,3,3,3,3,3,4),
(0.,1.12890698065804E-5,7.65259667068095E-5,0.000102837507928478,0.000112544869199221,
0.000130746171581864,0.000194450729921116,0.000226303009090741,0.000242229148675554,
0.000258155288260367,0.000258291104876496,0.000327654633604266,0.00039936399081459,
0.000469709285160263,0.000516310576520733),.UNSPECIFIED.);
#4824=B_SPLINE_CURVE_WITH_KNOTS('',3,(#214705,#214706,#214707,#214708,#214709,
#214710,#214711,#214712,#214713,#214714,#214715,#214716,#214717,#214718,
#214719,#214720,#214721,#214722,#214723,#214724,#214725,#214726,#214727,
#214728,#214729,#214730,#214731,#214732,#214733,#214734,#214735,#214736,
#214737,#214738,#214739,#214740,#214741,#214742,#214743,#214744),
 .UNSPECIFIED.,.F.,.F.,(4,3,3,3,3,3,3,3,3,3,3,3,3,4),(0.,6.84564250814195E-5,
0.000138288406593869,0.000205407478929251,0.000256966021225844,0.000257101146970262,
0.000271589374668161,0.000352213067594447,0.000388398097499754,0.00040412362205485,
0.000459162957997688,0.000486682625969106,0.000500442459954816,0.000514202293940525),
 .UNSPECIFIED.);
#4825=B_SPLINE_CURVE_WITH_KNOTS('',3,(#214746,#214747,#214748,#214749,#214750,
#214751,#214752,#214753,#214754,#214755,#214756,#214757,#214758,#214759,
#214760,#214761,#214762,#214763,#214764,#214765,#214766,#214767,#214768,
#214769,#214770,#214771,#214772,#214773,#214774,#214775,#214776,#214777,
#214778,#214779,#214780,#214781,#214782,#214783,#214784,#214785,#214786,
#214787,#214788),.UNSPECIFIED.,.F.,.F.,(4,3,3,3,3,3,3,3,3,3,3,3,3,3,4),
(0.,1.12890698065878E-5,7.65259667079882E-5,0.000102837507928575,0.000112544869199312,
0.000130746171581944,0.000194450729921155,0.000226303009090761,0.000242229148675564,
0.000258155288260367,0.000258291104876521,0.00032765463362058,0.000399363990847816,
0.000469709285208397,0.000516310576520733),.UNSPECIFIED.);
#4826=B_SPLINE_CURVE_WITH_KNOTS('',3,(#214796,#214797,#214798,#214799,#214800,
#214801,#214802,#214803,#214804,#214805,#214806,#214807,#214808,#214809,
#214810,#214811,#214812,#214813,#214814,#214815,#214816,#214817,#214818,
#214819,#214820,#214821,#214822,#214823,#214824,#214825,#214826,#214827,
#214828,#214829,#214830,#214831,#214832,#214833,#214834,#214835),
 .UNSPECIFIED.,.F.,.F.,(4,3,3,3,3,3,3,3,3,3,3,3,3,4),(0.,6.84564250828593E-5,
0.000138288406596549,0.000205407478932344,0.000256966021225844,0.000257101146970264,
0.00027158937466816,0.000352213067602491,0.000388398097499745,0.000404123622054843,
0.000459162957997685,0.000486682625969106,0.000500442459954816,0.000514202293940527),
 .UNSPECIFIED.);
#4827=B_SPLINE_CURVE_WITH_KNOTS('',3,(#214839,#214840,#214841,#214842,#214843,
#214844,#214845,#214846,#214847,#214848,#214849,#214850,#214851,#214852,
#214853,#214854,#214855,#214856,#214857,#214858,#214859,#214860,#214861,
#214862,#214863,#214864,#214865,#214866,#214867,#214868,#214869,#214870,
#214871,#214872,#214873,#214874,#214875,#214876,#214877,#214878,#214879,
#214880,#214881),.UNSPECIFIED.,.F.,.F.,(4,3,3,3,3,3,3,3,3,3,3,3,3,3,4),
(0.,1.12890698065845E-5,7.65259667089463E-5,0.000102837507928522,0.000112544869199262,
0.0001307461715819,0.000194450729921135,0.000226303009090752,0.000242229148675561,
0.000258155288260369,0.000258291104876517,0.000327654633616968,0.000399363990840608,
0.00046970928519815,0.000516310576520738),.UNSPECIFIED.);
#4828=B_SPLINE_CURVE_WITH_KNOTS('',3,(#214889,#214890,#214891,#214892,#214893,
#214894,#214895,#214896,#214897,#214898,#214899,#214900,#214901,#214902,
#214903,#214904,#214905,#214906,#214907,#214908,#214909,#214910,#214911,
#214912,#214913,#214914,#214915,#214916,#214917,#214918,#214919,#214920,
#214921,#214922,#214923,#214924,#214925,#214926,#214927,#214928),
 .UNSPECIFIED.,.F.,.F.,(4,3,3,3,3,3,3,3,3,3,3,3,3,4),(4.33680868994202E-19,
6.8456425081903E-5,0.000138288406594929,0.000205407478930537,0.000256966021225847,
0.000257101146970261,0.000271589374668165,0.000352213067606131,0.000388398097499846,
0.00040412362205493,0.000459162957997726,0.000486682625969123,0.000500442459954822,
0.000514202293940521),.UNSPECIFIED.);
#4829=B_SPLINE_CURVE_WITH_KNOTS('',3,(#214932,#214933,#214934,#214935,#214936,
#214937,#214938,#214939,#214940,#214941,#214942,#214943,#214944,#214945,
#214946,#214947,#214948,#214949,#214950,#214951,#214952,#214953,#214954,
#214955,#214956,#214957,#214958,#214959,#214960,#214961,#214962,#214963,
#214964,#214965,#214966,#214967,#214968,#214969,#214970,#214971,#214972,
#214973,#214974),.UNSPECIFIED.,.F.,.F.,(4,3,3,3,3,3,3,3,3,3,3,3,3,3,4),
(0.,1.12890698065809E-5,7.65259667023175E-5,0.000102837507928505,0.000112544869199247,
0.000130746171581888,0.000194450729921132,0.000226303009090755,0.000242229148675566,
0.000258155288260377,0.000258291104876515,0.000327654633619138,0.000399363990844944,
0.000469709285204301,0.000516310576520754),.UNSPECIFIED.);
#4830=B_SPLINE_CURVE_WITH_KNOTS('',3,(#214982,#214983,#214984,#214985,#214986,
#214987,#214988,#214989,#214990,#214991,#214992,#214993,#214994,#214995,
#214996,#214997,#214998,#214999,#215000,#215001,#215002,#215003,#215004,
#215005,#215006,#215007,#215008,#215009,#215010,#215011,#215012,#215013,
#215014,#215015,#215016,#215017,#215018,#215019,#215020,#215021),
 .UNSPECIFIED.,.F.,.F.,(4,3,3,3,3,3,3,3,3,3,3,3,3,4),(0.,6.84564250785299E-5,
0.00013828840658849,0.000205407478922068,0.000256966021225852,0.00025710114697026,
0.000271589374668164,0.000352213067604385,0.000388398097499773,0.000404123622054867,
0.000459162957997693,0.000486682625969106,0.000500442459954813,0.000514202293940519),
 .UNSPECIFIED.);
#4831=B_SPLINE_CURVE_WITH_KNOTS('',3,(#215025,#215026,#215027,#215028,#215029,
#215030,#215031,#215032,#215033,#215034,#215035,#215036,#215037,#215038,
#215039,#215040,#215041,#215042,#215043,#215044,#215045,#215046,#215047,
#215048,#215049,#215050,#215051,#215052,#215053,#215054,#215055,#215056,
#215057,#215058,#215059,#215060,#215061,#215062,#215063,#215064,#215065,
#215066,#215067),.UNSPECIFIED.,.F.,.F.,(4,3,3,3,3,3,3,3,3,3,3,3,3,3,4),
(0.,1.12890698065803E-5,7.65259667084363E-5,0.00010283750792847,0.000112544869199214,
0.000130746171581859,0.000194450729921117,0.000226303009090746,0.000242229148675561,
0.000258155288260375,0.000258291104876523,0.000327654633608061,0.000399363990822207,
0.000469709285171161,0.00051631057652075),.UNSPECIFIED.);
#4832=B_SPLINE_CURVE_WITH_KNOTS('',3,(#215075,#215076,#215077,#215078,#215079,
#215080,#215081,#215082,#215083,#215084,#215085,#215086,#215087,#215088,
#215089,#215090,#215091,#215092,#215093,#215094,#215095,#215096,#215097,
#215098,#215099,#215100,#215101,#215102,#215103,#215104,#215105,#215106,
#215107,#215108,#215109,#215110,#215111,#215112,#215113,#215114),
 .UNSPECIFIED.,.F.,.F.,(4,3,3,3,3,3,3,3,3,3,3,3,3,4),(2.16840434497101E-18,
6.84564250825956E-5,0.000138288406596379,0.000205407478932536,0.000256966021225845,
0.000257101146970259,0.000271589374668164,0.000352213067616007,0.000388398097499831,
0.000404123622054917,0.000459162957997717,0.000486682625969117,0.000500442459954816,
0.000514202293940516),.UNSPECIFIED.);
#4833=B_SPLINE_CURVE_WITH_KNOTS('',3,(#215118,#215119,#215120,#215121,#215122,
#215123,#215124,#215125,#215126,#215127,#215128,#215129,#215130,#215131,
#215132,#215133,#215134,#215135,#215136,#215137,#215138,#215139,#215140,
#215141,#215142,#215143,#215144,#215145,#215146,#215147,#215148,#215149,
#215150,#215151,#215152,#215153,#215154,#215155,#215156,#215157,#215158,
#215159,#215160),.UNSPECIFIED.,.F.,.F.,(4,3,3,3,3,3,3,3,3,3,3,3,3,3,4),
(0.,1.12890698065779E-5,7.6525966700619E-5,0.000102837507928493,0.000112544869199235,
0.000130746171581877,0.000194450729921122,0.000226303009090745,0.000242229148675556,
0.000258155288260368,0.000258291104876509,0.000327654633624863,0.000399363990856454,
0.000469709285220816,0.000516310576520735),.UNSPECIFIED.);
#4834=B_SPLINE_CURVE_WITH_KNOTS('',3,(#215168,#215169,#215170,#215171,#215172,
#215173,#215174,#215175,#215176,#215177,#215178,#215179,#215180,#215181,
#215182,#215183,#215184,#215185,#215186,#215187,#215188,#215189,#215190,
#215191,#215192,#215193,#215194,#215195,#215196,#215197,#215198,#215199,
#215200,#215201,#215202,#215203,#215204,#215205,#215206,#215207),
 .UNSPECIFIED.,.F.,.F.,(4,3,3,3,3,3,3,3,3,3,3,3,3,4),(0.,6.84564250783218E-5,
0.000138288406587982,0.000205407478921425,0.000256966021225847,0.000257101146970263,
0.000271589374668172,0.000352213067602529,0.000388398097499895,0.000404123622054973,
0.000459162957997745,0.000486682625969131,0.000500442459954824,0.000514202293940517),
 .UNSPECIFIED.);
#4835=B_SPLINE_CURVE_WITH_KNOTS('',3,(#215211,#215212,#215213,#215214,#215215,
#215216,#215217,#215218,#215219,#215220,#215221,#215222,#215223,#215224,
#215225,#215226,#215227,#215228,#215229,#215230,#215231,#215232,#215233,
#215234,#215235,#215236,#215237,#215238,#215239,#215240,#215241,#215242,
#215243,#215244,#215245,#215246,#215247,#215248,#215249,#215250,#215251,
#215252,#215253),.UNSPECIFIED.,.F.,.F.,(4,3,3,3,3,3,3,3,3,3,3,3,3,3,4),
(0.,1.12890698065829E-5,7.6525966723226E-5,0.000102837507928496,0.000112544869199238,
0.00013074617158188,0.000194450729921127,0.000226303009090751,0.000242229148675563,
0.000258155288260374,0.000258291104876528,0.000327654633609462,0.000399363990825717,
0.000469709285176748,0.000516310576520749),.UNSPECIFIED.);
#4836=B_SPLINE_CURVE_WITH_KNOTS('',3,(#215261,#215262,#215263,#215264,#215265,
#215266,#215267,#215268,#215269,#215270,#215271,#215272,#215273,#215274,
#215275,#215276,#215277,#215278,#215279,#215280,#215281,#215282,#215283,
#215284,#215285,#215286,#215287,#215288,#215289,#215290,#215291,#215292,
#215293,#215294,#215295,#215296,#215297,#215298,#215299,#215300),
 .UNSPECIFIED.,.F.,.F.,(4,3,3,3,3,3,3,3,3,3,3,3,3,4),(2.60208521396521E-18,
6.84564250868235E-5,0.000138288406605512,0.00020540747894714,0.000256966021225843,
0.00025710114697026,0.000271589374668176,0.000352213067624583,0.000388398097499925,
0.000404123622054999,0.000459162957997759,0.000486682625969138,0.000500442459954828,
0.000514202293940518),.UNSPECIFIED.);
#4837=B_SPLINE_CURVE_WITH_KNOTS('',3,(#215304,#215305,#215306,#215307,#215308,
#215309,#215310,#215311,#215312,#215313,#215314,#215315,#215316,#215317,
#215318,#215319,#215320,#215321,#215322,#215323,#215324,#215325,#215326,
#215327,#215328,#215329,#215330,#215331,#215332,#215333,#215334,#215335,
#215336,#215337,#215338,#215339,#215340,#215341,#215342,#215343,#215344,
#215345,#215346),.UNSPECIFIED.,.F.,.F.,(4,3,3,3,3,3,3,3,3,3,3,3,3,3,4),
(0.,1.12890698065793E-5,7.65259667123674E-5,0.000102837507928489,0.000112544869199231,
0.000130746171581874,0.000194450729921124,0.000226303009090748,0.000242229148675561,
0.000258155288260373,0.000258291104876523,0.000327654633615003,0.000399363990836477,
0.000469709285191897,0.000516310576520746),.UNSPECIFIED.);
#4838=B_SPLINE_CURVE_WITH_KNOTS('',3,(#215354,#215355,#215356,#215357,#215358,
#215359,#215360,#215361,#215362,#215363,#215364,#215365,#215366,#215367,
#215368,#215369,#215370,#215371,#215372,#215373,#215374,#215375,#215376,
#215377,#215378,#215379,#215380,#215381,#215382,#215383,#215384,#215385,
#215386,#215387,#215388,#215389,#215390,#215391,#215392,#215393),
 .UNSPECIFIED.,.F.,.F.,(4,3,3,3,3,3,3,3,3,3,3,3,3,4),(1.73472347597681E-18,
6.845642508305E-5,0.000138288406596686,0.000205407478931409,0.000256966021225855,
0.000257101146970272,0.000271589374668164,0.000352213067614368,0.000388398097499747,
0.000404123622054847,0.000459162957997695,0.000486682625969118,0.00050044245995483,
0.000514202293940542),.UNSPECIFIED.);
#4839=B_SPLINE_CURVE_WITH_KNOTS('',3,(#215397,#215398,#215399,#215400,#215401,
#215402,#215403,#215404,#215405,#215406,#215407,#215408,#215409,#215410,
#215411,#215412,#215413,#215414,#215415,#215416,#215417,#215418,#215419,
#215420,#215421,#215422,#215423,#215424,#215425,#215426,#215427,#215428,
#215429,#215430,#215431,#215432,#215433,#215434,#215435,#215436,#215437,
#215438,#215439),.UNSPECIFIED.,.F.,.F.,(4,3,3,3,3,3,3,3,3,3,3,3,3,3,4),
(0.,1.12890698065779E-5,7.65259666775026E-5,0.00010283750792847,0.000112544869199214,
0.000130746171581858,0.000194450729921113,0.000226303009090741,0.000242229148675555,
0.000258155288260369,0.00025829110487651,0.000327654633629564,0.000399363990865801,
0.000469709285235127,0.000516310576520737),.UNSPECIFIED.);
#4840=B_SPLINE_CURVE_WITH_KNOTS('',3,(#215447,#215448,#215449,#215450,#215451,
#215452,#215453,#215454,#215455,#215456,#215457,#215458,#215459,#215460,
#215461,#215462,#215463,#215464,#215465,#215466,#215467,#215468,#215469,
#215470,#215471,#215472,#215473,#215474,#215475,#215476,#215477,#215478,
#215479,#215480,#215481,#215482,#215483,#215484,#215485,#215486),
 .UNSPECIFIED.,.F.,.F.,(4,3,3,3,3,3,3,3,3,3,3,3,3,4),(0.,6.84564250806006E-5,
0.000138288406591434,0.000205407478922972,0.000256966021225842,0.000257101146970266,
0.000271589374668167,0.000352213067618348,0.000388398097499851,0.000404123622054936,
0.000459162957997734,0.000486682625969134,0.000500442459954833,0.000514202293940533),
 .UNSPECIFIED.);
#4841=B_SPLINE_CURVE_WITH_KNOTS('',3,(#215490,#215491,#215492,#215493,#215494,
#215495,#215496,#215497,#215498,#215499,#215500,#215501,#215502,#215503,
#215504,#215505,#215506,#215507,#215508,#215509,#215510,#215511,#215512,
#215513,#215514,#215515,#215516,#215517,#215518,#215519,#215520,#215521,
#215522,#215523,#215524,#215525,#215526,#215527,#215528,#215529,#215530,
#215531,#215532),.UNSPECIFIED.,.F.,.F.,(4,3,3,3,3,3,3,3,3,3,3,3,3,3,4),
(0.,1.12890698065802E-5,7.6525966703759E-5,0.000102837507928505,0.000112544869199247,
0.000130746171581888,0.000194450729921132,0.000226303009090754,0.000242229148675565,
0.000258155288260376,0.000258291104876512,0.000327654633617546,0.000399363990841935,
0.00046970928520053,0.000516310576520752),.UNSPECIFIED.);
#4842=B_SPLINE_CURVE_WITH_KNOTS('',3,(#215540,#215541,#215542,#215543,#215544,
#215545,#215546,#215547,#215548,#215549,#215550,#215551,#215552,#215553,
#215554,#215555,#215556,#215557,#215558,#215559,#215560,#215561,#215562,
#215563,#215564,#215565,#215566,#215567,#215568,#215569,#215570,#215571,
#215572,#215573,#215574,#215575,#215576,#215577,#215578,#215579),
 .UNSPECIFIED.,.F.,.F.,(4,3,3,3,3,3,3,3,3,3,3,3,3,4),(0.,6.84564250876636E-5,
0.000138288406606712,0.000205407478948682,0.000256966021225854,0.000257101146970261,
0.00027158937466816,0.000352213067590487,0.000388398097499747,0.000404123622054844,
0.000459162957997683,0.000486682625969103,0.000500442459954813,0.000514202293940522),
 .UNSPECIFIED.);
#4843=B_SPLINE_CURVE_WITH_KNOTS('',3,(#215583,#215584,#215585,#215586,#215587,
#215588,#215589,#215590,#215591,#215592,#215593,#215594,#215595,#215596,
#215597,#215598,#215599,#215600,#215601,#215602,#215603,#215604,#215605,
#215606,#215607,#215608,#215609,#215610,#215611,#215612,#215613,#215614,
#215615,#215616,#215617,#215618,#215619,#215620,#215621,#215622,#215623,
#215624,#215625),.UNSPECIFIED.,.F.,.F.,(4,3,3,3,3,3,3,3,3,3,3,3,3,3,4),
(0.,1.12890698065826E-5,7.65259666897135E-5,0.000102837507928503,0.000112544869199245,
0.000130746171581886,0.00019445072992113,0.000226303009090752,0.000242229148675564,
0.000258155288260375,0.00025829110487651,0.000327654633619508,0.000399363990844196,
0.000469709285200996,0.000516310576520749),.UNSPECIFIED.);
#4844=B_SPLINE_CURVE_WITH_KNOTS('',3,(#215633,#215634,#215635,#215636,#215637,
#215638,#215639,#215640,#215641,#215642,#215643,#215644,#215645,#215646,
#215647,#215648,#215649,#215650,#215651,#215652,#215653,#215654,#215655,
#215656,#215657,#215658,#215659,#215660,#215661,#215662,#215663,#215664,
#215665,#215666,#215667,#215668,#215669,#215670,#215671,#215672),
 .UNSPECIFIED.,.F.,.F.,(4,3,3,3,3,3,3,3,3,3,3,3,3,4),(2.60208521396521E-18,
6.84564250877193E-5,0.000138288406606367,0.000205407478946553,0.000256966021225849,
0.000257101146970267,0.000271589374668177,0.000352213067599024,0.000388398097499851,
0.000404123622054936,0.000459162957997734,0.000486682625969133,0.000500442459954832,
0.000514202293940532),.UNSPECIFIED.);
#4845=B_SPLINE_CURVE_WITH_KNOTS('',3,(#215676,#215677,#215678,#215679,#215680,
#215681,#215682,#215683,#215684,#215685,#215686,#215687,#215688,#215689,
#215690,#215691,#215692,#215693,#215694,#215695,#215696,#215697,#215698,
#215699,#215700,#215701,#215702,#215703,#215704,#215705,#215706,#215707,
#215708,#215709,#215710,#215711,#215712,#215713,#215714,#215715,#215716,
#215717,#215718),.UNSPECIFIED.,.F.,.F.,(4,3,3,3,3,3,3,3,3,3,3,3,3,3,4),
(0.,1.12890698065771E-5,7.65259667020667E-5,0.000102837507928448,0.000112544869199193,
0.00013074617158184,0.000194450729921102,0.000226303009090734,0.000242229148675549,
0.000258155288260365,0.000258291104876513,0.000327654633616971,0.000399363990840478,
0.000469709285197867,0.000516310576520737),.UNSPECIFIED.);
#4846=B_SPLINE_CURVE_WITH_KNOTS('',3,(#215726,#215727,#215728,#215729,#215730,
#215731,#215732,#215733,#215734,#215735,#215736,#215737,#215738,#215739,
#215740,#215741,#215742,#215743,#215744,#215745,#215746,#215747,#215748,
#215749,#215750,#215751,#215752,#215753,#215754,#215755,#215756,#215757,
#215758,#215759,#215760,#215761,#215762,#215763,#215764,#215765),
 .UNSPECIFIED.,.F.,.F.,(4,3,3,3,3,3,3,3,3,3,3,3,3,4),(0.,6.84564250802978E-5,
0.000138288406591518,0.000205407478925098,0.000256966021225857,0.000257101146970261,
0.000271589374668162,0.000352213067612065,0.000388398097499789,0.000404123622054881,
0.000459162957997701,0.000486682625969112,0.000500442459954817,0.000514202293940522),
 .UNSPECIFIED.);
#4847=B_SPLINE_CURVE_WITH_KNOTS('',3,(#215769,#215770,#215771,#215772,#215773,
#215774,#215775,#215776,#215777,#215778,#215779,#215780,#215781,#215782,
#215783,#215784,#215785,#215786,#215787,#215788,#215789,#215790,#215791,
#215792,#215793,#215794,#215795,#215796,#215797,#215798,#215799,#215800,
#215801,#215802,#215803,#215804,#215805,#215806,#215807,#215808,#215809,
#215810,#215811),.UNSPECIFIED.,.F.,.F.,(4,3,3,3,3,3,3,3,3,3,3,3,3,3,4),
(0.,1.12890698065831E-5,7.65259667143359E-5,0.000102837507928517,0.000112544869199258,
0.000130746171581897,0.000194450729921133,0.000226303009090751,0.00024222914867556,
0.000258155288260369,0.000258291104876512,0.000327654633615957,0.000399363990839121,
0.000469709285196728,0.000516310576520738),.UNSPECIFIED.);
#4848=B_SPLINE_CURVE_WITH_KNOTS('',3,(#215819,#215820,#215821,#215822,#215823,
#215824,#215825,#215826,#215827,#215828,#215829,#215830,#215831,#215832,
#215833,#215834,#215835,#215836,#215837,#215838,#215839,#215840,#215841,
#215842,#215843,#215844,#215845,#215846,#215847,#215848,#215849,#215850,
#215851,#215852,#215853,#215854,#215855,#215856,#215857,#215858),
 .UNSPECIFIED.,.F.,.F.,(4,3,3,3,3,3,3,3,3,3,3,3,3,4),(0.,6.8456425084354E-5,
0.000138288406599791,0.000205407478937876,0.000256966021225842,0.000257101146970262,
0.000271589374668162,0.000352213067600001,0.00038839809749976,0.000404123622054856,
0.00045916295799769,0.000486682625969107,0.000500442459954816,0.000514202293940525),
 .UNSPECIFIED.);
#4849=B_SPLINE_CURVE_WITH_KNOTS('',3,(#215862,#215863,#215864,#215865,#215866,
#215867,#215868,#215869,#215870,#215871,#215872,#215873,#215874,#215875,
#215876,#215877,#215878,#215879,#215880,#215881,#215882,#215883,#215884,
#215885,#215886,#215887,#215888,#215889,#215890,#215891,#215892,#215893,
#215894,#215895,#215896,#215897,#215898,#215899,#215900,#215901,#215902,
#215903,#215904),.UNSPECIFIED.,.F.,.F.,(4,3,3,3,3,3,3,3,3,3,3,3,3,3,4),
(0.,1.12890698065845E-5,7.65259667118142E-5,0.000102837507928515,0.000112544869199256,
0.000130746171581896,0.000194450729921136,0.000226303009090755,0.000242229148675565,
0.000258155288260375,0.000258291104876512,0.000327654633609095,0.000399363990824695,
0.000469709285175208,0.00051631057652075),.UNSPECIFIED.);
#4850=B_SPLINE_CURVE_WITH_KNOTS('',3,(#215912,#215913,#215914,#215915,#215916,
#215917,#215918,#215919,#215920,#215921,#215922,#215923,#215924,#215925,
#215926,#215927,#215928,#215929,#215930,#215931,#215932,#215933,#215934,
#215935,#215936,#215937,#215938,#215939,#215940,#215941,#215942,#215943,
#215944,#215945,#215946,#215947,#215948,#215949,#215950,#215951),
 .UNSPECIFIED.,.F.,.F.,(4,3,3,3,3,3,3,3,3,3,3,3,3,4),(0.,6.84564250776835E-5,
0.000138288406586343,0.000205407478917895,0.000256966021225848,0.000257101146970261,
0.000271589374668164,0.000352213067606,0.000388398097499787,0.000404123622054879,
0.0004591629579977,0.000486682625969111,0.000500442459954816,0.000514202293940522),
 .UNSPECIFIED.);
#4851=B_SPLINE_CURVE_WITH_KNOTS('',3,(#215955,#215956,#215957,#215958,#215959,
#215960,#215961,#215962,#215963,#215964,#215965,#215966,#215967,#215968,
#215969,#215970,#215971,#215972,#215973,#215974,#215975,#215976,#215977,
#215978,#215979,#215980,#215981,#215982,#215983,#215984,#215985,#215986,
#215987,#215988,#215989,#215990,#215991,#215992,#215993,#215994,#215995,
#215996,#215997),.UNSPECIFIED.,.F.,.F.,(4,3,3,3,3,3,3,3,3,3,3,3,3,3,4),
(1.73472347597681E-18,1.12890698065845E-5,7.65259667057065E-5,0.000102837507928531,
0.000112544869199271,0.000130746171581908,0.000194450729921137,0.000226303009090752,
0.00024222914867556,0.000258155288260367,0.000258291104876518,0.000327654633610688,
0.000399363990827742,0.000469709285179423,0.000516310576520732),
 .UNSPECIFIED.);
#4852=B_SPLINE_CURVE_WITH_KNOTS('',3,(#216005,#216006,#216007,#216008,#216009,
#216010,#216011,#216012,#216013,#216014,#216015,#216016,#216017,#216018,
#216019,#216020,#216021,#216022,#216023,#216024,#216025,#216026,#216027,
#216028,#216029,#216030,#216031,#216032,#216033,#216034,#216035,#216036,
#216037,#216038,#216039,#216040,#216041,#216042,#216043,#216044),
 .UNSPECIFIED.,.F.,.F.,(4,3,3,3,3,3,3,3,3,3,3,3,3,4),(0.,6.84564250845372E-5,
0.000138288406600476,0.000205407478939388,0.000256966021225852,0.000257101146970261,
0.000271589374668165,0.000352213067598438,0.000388398097499816,0.000404123622054904,
0.000459162957997713,0.000486682625969117,0.000500442459954819,0.000514202293940521),
 .UNSPECIFIED.);
#4853=B_SPLINE_CURVE_WITH_KNOTS('',3,(#216048,#216049,#216050,#216051,#216052,
#216053,#216054,#216055,#216056,#216057,#216058,#216059,#216060,#216061,
#216062,#216063,#216064,#216065,#216066,#216067,#216068,#216069,#216070,
#216071,#216072,#216073,#216074,#216075,#216076,#216077,#216078,#216079,
#216080,#216081,#216082,#216083,#216084,#216085,#216086,#216087,#216088,
#216089,#216090),.UNSPECIFIED.,.F.,.F.,(4,3,3,3,3,3,3,3,3,3,3,3,3,3,4),
(8.67361737988403E-19,1.12890698065789E-5,7.65259667078676E-5,0.000102837507928473,
0.000112544869199216,0.00013074617158186,0.000194450729921113,0.000226303009090739,
0.000242229148675552,0.000258155288260366,0.000258291104876509,0.000327654633616604,
0.000399363990839486,0.000469709285196016,0.00051631057652073),
 .UNSPECIFIED.);
#4854=B_SPLINE_CURVE_WITH_KNOTS('',3,(#216097,#216098,#216099,#216100,#216101,
#216102,#216103,#216104,#216105,#216106,#216107,#216108,#216109,#216110,
#216111,#216112,#216113,#216114,#216115,#216116,#216117,#216118,#216119,
#216120,#216121,#216122,#216123,#216124,#216125,#216126,#216127,#216128,
#216129,#216130,#216131,#216132,#216133,#216134,#216135,#216136),
 .UNSPECIFIED.,.F.,.F.,(4,3,3,3,3,3,3,3,3,3,3,3,3,4),(0.,6.8456425078443E-5,
0.000138288406587804,0.000205407478920017,0.000256966021225852,0.000257101146970261,
0.000271589374668165,0.000352213067601245,0.000388398097499795,0.000404123622054885,
0.000459162957997703,0.000486682625969112,0.000500442459954817,0.000514202293940521),
 .UNSPECIFIED.);
#4855=B_SPLINE_CURVE_WITH_KNOTS('',3,(#216139,#216140,#216141,#216142,#216143,
#216144,#216145,#216146,#216147,#216148,#216149,#216150,#216151,#216152,
#216153,#216154,#216155,#216156,#216157,#216158,#216159,#216160,#216161,
#216162,#216163,#216164,#216165,#216166,#216167,#216168,#216169,#216170,
#216171,#216172,#216173,#216174,#216175),.UNSPECIFIED.,.F.,.F.,(4,3,3,3,
3,3,3,3,3,3,3,3,4),(0.,1.12535551670991E-5,7.76936938516679E-5,0.000102513517961096,
0.000121879189824247,0.000189659041345274,0.000223548967105788,0.000257294099096098,
0.000257438892866301,0.00032572085175526,0.000396486773955018,0.00046624270766206,
0.000514877785732602),.UNSPECIFIED.);
#4856=B_SPLINE_CURVE_WITH_KNOTS('',3,(#216183,#216184,#216185,#216186,#216187,
#216188,#216189,#216190,#216191,#216192,#216193,#216194,#216195,#216196,
#216197,#216198,#216199,#216200,#216201,#216202,#216203,#216204,#216205,
#216206,#216207,#216208,#216209,#216210,#216211,#216212,#216213,#216214,
#216215,#216216,#216217,#216218,#216219,#216220,#216221,#216222),
 .UNSPECIFIED.,.F.,.F.,(4,3,3,3,3,3,3,3,3,3,3,3,3,4),(0.,6.80370855387726E-5,
0.00013730316930294,0.000203636706669859,0.000256396220959708,0.000256540237295739,
0.000285209320207746,0.000342105100635664,0.000384776935956602,0.000400778874201954,
0.000456785658060685,0.000484789049990051,0.000498790745954733,0.000512792441919416),
 .UNSPECIFIED.);
#4857=B_SPLINE_CURVE_WITH_KNOTS('',3,(#216226,#216227,#216228,#216229,#216230,
#216231,#216232,#216233,#216234,#216235,#216236,#216237,#216238,#216239,
#216240,#216241,#216242,#216243,#216244,#216245,#216246,#216247,#216248,
#216249,#216250,#216251,#216252,#216253,#216254,#216255,#216256,#216257,
#216258,#216259,#216260,#216261,#216262),.UNSPECIFIED.,.F.,.F.,(4,3,3,3,
3,3,3,3,3,3,3,3,4),(0.,1.12535551670995E-5,7.76936938481029E-5,0.000102513517961135,
0.00012187918982428,0.000189659041345289,0.000223548967105794,0.000257294099096101,
0.000257438892866298,0.000325720851760917,0.000396486773966304,0.000466242707678062,
0.000514877785732596),.UNSPECIFIED.);
#4858=B_SPLINE_CURVE_WITH_KNOTS('',3,(#216270,#216271,#216272,#216273,#216274,
#216275,#216276,#216277,#216278,#216279,#216280,#216281,#216282,#216283,
#216284,#216285,#216286,#216287,#216288,#216289,#216290,#216291,#216292,
#216293,#216294,#216295,#216296,#216297,#216298,#216299,#216300,#216301,
#216302,#216303,#216304,#216305,#216306,#216307,#216308,#216309),
 .UNSPECIFIED.,.F.,.F.,(4,3,3,3,3,3,3,3,3,3,3,3,3,4),(0.,6.80370855360972E-5,
0.000137303169297683,0.000203636706662521,0.000256396220959706,0.000256540237295735,
0.00028520932020774,0.000342105100635658,0.000384776935956597,0.000400778874201949,
0.00045678565806068,0.000484789049990046,0.000498790745954729,0.000512792441919412),
 .UNSPECIFIED.);
#4859=B_SPLINE_CURVE_WITH_KNOTS('',3,(#216313,#216314,#216315,#216316,#216317,
#216318,#216319,#216320,#216321,#216322,#216323,#216324,#216325,#216326,
#216327,#216328,#216329,#216330,#216331,#216332,#216333,#216334,#216335,
#216336,#216337,#216338,#216339,#216340,#216341,#216342,#216343,#216344,
#216345,#216346,#216347,#216348,#216349),.UNSPECIFIED.,.F.,.F.,(4,3,3,3,
3,3,3,3,3,3,3,3,4),(0.,1.12535551671024E-5,7.76936938462203E-5,0.000102513517961152,
0.000121879189824295,0.000189659041345298,0.000223548967105799,0.000257294099096102,
0.000257438892866301,0.00032572085176373,0.00039648677397213,0.000466242707686686,
0.000514877785732602),.UNSPECIFIED.);
#4860=B_SPLINE_CURVE_WITH_KNOTS('',3,(#216357,#216358,#216359,#216360,#216361,
#216362,#216363,#216364,#216365,#216366,#216367,#216368,#216369,#216370,
#216371,#216372,#216373,#216374,#216375,#216376,#216377,#216378,#216379,
#216380,#216381,#216382,#216383,#216384,#216385,#216386,#216387,#216388,
#216389,#216390,#216391,#216392,#216393,#216394,#216395,#216396),
 .UNSPECIFIED.,.F.,.F.,(4,3,3,3,3,3,3,3,3,3,3,3,3,4),(0.,6.80370855362733E-5,
0.00013730316929717,0.000203636706659883,0.000256396220959707,0.000256540237295737,
0.000285209320207728,0.000342105100635649,0.000384776935956591,0.000400778874201944,
0.000456785658060679,0.000484789049990047,0.00049879074595473,0.000512792441919414),
 .UNSPECIFIED.);
#4861=B_SPLINE_CURVE_WITH_KNOTS('',3,(#216400,#216401,#216402,#216403,#216404,
#216405,#216406,#216407,#216408,#216409,#216410,#216411,#216412,#216413,
#216414,#216415,#216416,#216417,#216418,#216419,#216420,#216421,#216422,
#216423,#216424,#216425,#216426,#216427,#216428,#216429,#216430,#216431,
#216432,#216433,#216434,#216435,#216436),.UNSPECIFIED.,.F.,.F.,(4,3,3,3,
3,3,3,3,3,3,3,3,4),(0.,1.12535551670993E-5,7.7693693845788E-5,0.000102513517961118,
0.000121879189824266,0.000189659041345283,0.000223548967105792,0.000257294099096107,
0.000257438892866301,0.000325720851757369,0.000396486773959682,0.000466242707669865,
0.000514877785732601),.UNSPECIFIED.);
#4862=B_SPLINE_CURVE_WITH_KNOTS('',3,(#216444,#216445,#216446,#216447,#216448,
#216449,#216450,#216451,#216452,#216453,#216454,#216455,#216456,#216457,
#216458,#216459,#216460,#216461,#216462,#216463,#216464,#216465,#216466,
#216467,#216468,#216469,#216470,#216471,#216472,#216473,#216474,#216475,
#216476,#216477,#216478,#216479,#216480,#216481,#216482,#216483),
 .UNSPECIFIED.,.F.,.F.,(4,3,3,3,3,3,3,3,3,3,3,3,3,4),(0.,6.80370855408422E-5,
0.000137303169306678,0.000203636706674689,0.000256396220959706,0.000256540237295731,
0.000285209320207737,0.000342105100635656,0.000384776935956595,0.000400778874201947,
0.000456785658060679,0.000484789049990045,0.000498790745954728,0.000512792441919411),
 .UNSPECIFIED.);
#4863=B_SPLINE_CURVE_WITH_KNOTS('',3,(#216487,#216488,#216489,#216490,#216491,
#216492,#216493,#216494,#216495,#216496,#216497,#216498,#216499,#216500,
#216501,#216502,#216503,#216504,#216505,#216506,#216507,#216508,#216509,
#216510,#216511,#216512,#216513,#216514,#216515,#216516,#216517,#216518,
#216519,#216520,#216521,#216522,#216523),.UNSPECIFIED.,.F.,.F.,(4,3,3,3,
3,3,3,3,3,3,3,3,4),(0.,1.1253555167101E-5,7.76936938405201E-5,0.00010251351796113,
0.000121879189824277,0.000189659041345291,0.000223548967105797,0.000257294099096104,
0.000257438892866304,0.000325720851758851,0.000396486773962169,0.000466242707672447,
0.000514877785732608),.UNSPECIFIED.);
#4864=B_SPLINE_CURVE_WITH_KNOTS('',3,(#216531,#216532,#216533,#216534,#216535,
#216536,#216537,#216538,#216539,#216540,#216541,#216542,#216543,#216544,
#216545,#216546,#216547,#216548,#216549,#216550,#216551,#216552,#216553,
#216554,#216555,#216556,#216557,#216558,#216559,#216560,#216561,#216562,
#216563,#216564,#216565,#216566,#216567,#216568,#216569,#216570),
 .UNSPECIFIED.,.F.,.F.,(4,3,3,3,3,3,3,3,3,3,3,3,3,4),(0.,6.80370855415949E-5,
0.000137303169308611,0.000203636706678468,0.00025639622095971,0.000256540237295739,
0.000285209320207752,0.000342105100635669,0.000384776935956607,0.000400778874201959,
0.000456785658060689,0.000484789049990055,0.000498790745954737,0.00051279244191942),
 .UNSPECIFIED.);
#4865=B_SPLINE_CURVE_WITH_KNOTS('',3,(#216574,#216575,#216576,#216577,#216578,
#216579,#216580,#216581,#216582,#216583,#216584,#216585,#216586,#216587,
#216588,#216589,#216590,#216591,#216592,#216593,#216594,#216595,#216596,
#216597,#216598,#216599,#216600,#216601,#216602,#216603,#216604,#216605,
#216606,#216607,#216608,#216609,#216610),.UNSPECIFIED.,.F.,.F.,(4,3,3,3,
3,3,3,3,3,3,3,3,4),(0.,1.12535551671007E-5,7.76936938506112E-5,0.000102513517961138,
0.000121879189824284,0.000189659041345297,0.000223548967105804,0.000257294099096102,
0.000257438892866311,0.000325720851751308,0.000396486773947479,0.000466242707652249,
0.000514877785732621),.UNSPECIFIED.);
#4866=B_SPLINE_CURVE_WITH_KNOTS('',3,(#216618,#216619,#216620,#216621,#216622,
#216623,#216624,#216625,#216626,#216627,#216628,#216629,#216630,#216631,
#216632,#216633,#216634,#216635,#216636,#216637,#216638,#216639,#216640,
#216641,#216642,#216643,#216644,#216645,#216646,#216647,#216648,#216649,
#216650,#216651,#216652,#216653,#216654,#216655,#216656,#216657),
 .UNSPECIFIED.,.F.,.F.,(4,3,3,3,3,3,3,3,3,3,3,3,3,4),(0.,6.80370855331494E-5,
0.000137303169291901,0.000203636706654186,0.000256396220959702,0.000256540237295728,
0.000285209320207747,0.000342105100635661,0.000384776935956597,0.000400778874201948,
0.000456785658060676,0.00048478904999004,0.000498790745954722,0.000512792441919404),
 .UNSPECIFIED.);
#4867=B_SPLINE_CURVE_WITH_KNOTS('',3,(#216661,#216662,#216663,#216664,#216665,
#216666,#216667,#216668,#216669,#216670,#216671,#216672,#216673,#216674,
#216675,#216676,#216677,#216678,#216679,#216680,#216681,#216682,#216683,
#216684,#216685,#216686,#216687,#216688,#216689,#216690,#216691,#216692,
#216693,#216694,#216695,#216696,#216697),.UNSPECIFIED.,.F.,.F.,(4,3,3,3,
3,3,3,3,3,3,3,3,4),(0.,1.12535551670965E-5,7.76936938411505E-5,0.000102513517961098,
0.00012187918982425,0.00018965904134528,0.000223548967105795,0.000257294099096113,
0.00025743889286631,0.000325720851756961,0.00039648677395731,0.00046624270766338,
0.00051487778573262),.UNSPECIFIED.);
#4868=B_SPLINE_CURVE_WITH_KNOTS('',3,(#216705,#216706,#216707,#216708,#216709,
#216710,#216711,#216712,#216713,#216714,#216715,#216716,#216717,#216718,
#216719,#216720,#216721,#216722,#216723,#216724,#216725,#216726,#216727,
#216728,#216729,#216730,#216731,#216732,#216733,#216734,#216735,#216736,
#216737,#216738,#216739,#216740,#216741,#216742,#216743,#216744),
 .UNSPECIFIED.,.F.,.F.,(4,3,3,3,3,3,3,3,3,3,3,3,3,4),(0.,6.8037085541185E-5,
0.000137303169307903,0.000203636706677904,0.000256396220959706,0.000256540237295741,
0.00028520932020772,0.000342105100635643,0.000384776935956585,0.000400778874201939,
0.000456785658060676,0.000484789049990044,0.000498790745954728,0.000512792441919413),
 .UNSPECIFIED.);
#4869=B_SPLINE_CURVE_WITH_KNOTS('',3,(#216748,#216749,#216750,#216751,#216752,
#216753,#216754,#216755,#216756,#216757,#216758,#216759,#216760,#216761,
#216762,#216763,#216764,#216765,#216766,#216767,#216768,#216769,#216770,
#216771,#216772,#216773,#216774,#216775,#216776,#216777,#216778,#216779,
#216780,#216781,#216782,#216783,#216784),.UNSPECIFIED.,.F.,.F.,(4,3,3,3,
3,3,3,3,3,3,3,3,4),(0.,1.12535551670995E-5,7.76936938413587E-5,0.000102513517961138,
0.000121879189824285,0.0001896590413453,0.000223548967105808,0.00025729409909611,
0.000257438892866315,0.000325720851766884,0.000396486773977355,0.000466242707691934,
0.00051487778573263),.UNSPECIFIED.);
#4870=B_SPLINE_CURVE_WITH_KNOTS('',3,(#216792,#216793,#216794,#216795,#216796,
#216797,#216798,#216799,#216800,#216801,#216802,#216803,#216804,#216805,
#216806,#216807,#216808,#216809,#216810,#216811,#216812,#216813,#216814,
#216815,#216816,#216817,#216818,#216819,#216820,#216821,#216822,#216823,
#216824,#216825,#216826,#216827,#216828,#216829,#216830,#216831),
 .UNSPECIFIED.,.F.,.F.,(4,3,3,3,3,3,3,3,3,3,3,3,3,4),(0.,6.80370855392613E-5,
0.000137303169304968,0.000203636706675208,0.000256396220959704,0.000256540237295727,
0.000285209320207745,0.000342105100635661,0.000384776935956598,0.000400778874201949,
0.000456785658060679,0.000484789049990044,0.000498790745954726,0.000512792441919408),
 .UNSPECIFIED.);
#4871=B_SPLINE_CURVE_WITH_KNOTS('',3,(#216835,#216836,#216837,#216838,#216839,
#216840,#216841,#216842,#216843,#216844,#216845,#216846,#216847,#216848,
#216849,#216850,#216851,#216852,#216853,#216854,#216855,#216856,#216857,
#216858,#216859,#216860,#216861,#216862,#216863,#216864,#216865,#216866,
#216867,#216868,#216869,#216870,#216871),.UNSPECIFIED.,.F.,.F.,(4,3,3,3,
3,3,3,3,3,3,3,3,4),(0.,1.1253555167103E-5,7.76936938409016E-5,0.000102513517961149,
0.000121879189824294,0.000189659041345302,0.000223548967105806,0.000257294099096109,
0.00025743889286631,0.00032572085175361,0.000396486773951826,0.000466242707658243,
0.000514877785732621),.UNSPECIFIED.);
#4872=B_SPLINE_CURVE_WITH_KNOTS('',3,(#216879,#216880,#216881,#216882,#216883,
#216884,#216885,#216886,#216887,#216888,#216889,#216890,#216891,#216892,
#216893,#216894,#216895,#216896,#216897,#216898,#216899,#216900,#216901,
#216902,#216903,#216904,#216905,#216906,#216907,#216908,#216909,#216910,
#216911,#216912,#216913,#216914,#216915,#216916,#216917,#216918),
 .UNSPECIFIED.,.F.,.F.,(4,3,3,3,3,3,3,3,3,3,3,3,3,4),(0.,6.80370855404509E-5,
0.000137303169306047,0.000203636706674211,0.000256396220959703,0.000256540237295742,
0.000285209320207733,0.000342105100635652,0.00038477693595659,0.000400778874201942,
0.000456785658060675,0.000484789049990041,0.000498790745954724,0.000512792441919407),
 .UNSPECIFIED.);
#4873=B_SPLINE_CURVE_WITH_KNOTS('',3,(#216922,#216923,#216924,#216925,#216926,
#216927,#216928,#216929,#216930,#216931,#216932,#216933,#216934,#216935,
#216936,#216937,#216938,#216939,#216940,#216941,#216942,#216943,#216944,
#216945,#216946,#216947,#216948,#216949,#216950,#216951,#216952,#216953,
#216954,#216955,#216956,#216957,#216958),.UNSPECIFIED.,.F.,.F.,(4,3,3,3,
3,3,3,3,3,3,3,3,4),(0.,1.12535551670926E-5,7.76936938578812E-5,0.000102513517961074,
0.000121879189824228,0.00018965904134527,0.00022354896710579,0.000257294099096107,
0.000257438892866311,0.000325720851755129,0.000396486773954983,0.000466242707662315,
0.000514877785732621),.UNSPECIFIED.);
#4874=B_SPLINE_CURVE_WITH_KNOTS('',3,(#216966,#216967,#216968,#216969,#216970,
#216971,#216972,#216973,#216974,#216975,#216976,#216977,#216978,#216979,
#216980,#216981,#216982,#216983,#216984,#216985,#216986,#216987,#216988,
#216989,#216990,#216991,#216992,#216993,#216994,#216995,#216996,#216997,
#216998,#216999,#217000,#217001,#217002,#217003,#217004,#217005),
 .UNSPECIFIED.,.F.,.F.,(4,3,3,3,3,3,3,3,3,3,3,3,3,4),(0.,6.80370855390923E-5,
0.000137303169303434,0.000203636706670414,0.000256396220959702,0.000256540237295738,
0.000285209320207726,0.000342105100635646,0.000384776935956586,0.000400778874201938,
0.000456785658060671,0.000484789049990038,0.000498790745954721,0.000512792441919405),
 .UNSPECIFIED.);
#4875=B_SPLINE_CURVE_WITH_KNOTS('',3,(#217009,#217010,#217011,#217012,#217013,
#217014,#217015,#217016,#217017,#217018,#217019,#217020,#217021,#217022,
#217023,#217024,#217025,#217026,#217027,#217028,#217029,#217030,#217031,
#217032,#217033,#217034,#217035,#217036,#217037,#217038,#217039,#217040,
#217041,#217042,#217043,#217044,#217045),.UNSPECIFIED.,.F.,.F.,(4,3,3,3,
3,3,3,3,3,3,3,3,4),(0.,1.12535551670967E-5,7.76936938457851E-5,0.000102513517961083,
0.000121879189824237,0.000189659041345273,0.000223548967105791,0.000257294099096112,
0.000257438892866309,0.000325720851758272,0.000396486773960363,0.000466242707668341,
0.000514877785732617),.UNSPECIFIED.);
#4876=B_SPLINE_CURVE_WITH_KNOTS('',3,(#217053,#217054,#217055,#217056,#217057,
#217058,#217059,#217060,#217061,#217062,#217063,#217064,#217065,#217066,
#217067,#217068,#217069,#217070,#217071,#217072,#217073,#217074,#217075,
#217076,#217077,#217078,#217079,#217080,#217081,#217082,#217083,#217084,
#217085,#217086,#217087,#217088,#217089,#217090,#217091,#217092),
 .UNSPECIFIED.,.F.,.F.,(4,3,3,3,3,3,3,3,3,3,3,3,3,4),(0.,6.80370855408783E-5,
0.000137303169307437,0.000203636706676985,0.000256396220959703,0.000256540237295734,
0.000285209320207724,0.000342105100635644,0.000384776935956585,0.000400778874201937,
0.000456785658060672,0.000484789049990039,0.000498790745954723,0.000512792441919406),
 .UNSPECIFIED.);
#4877=B_SPLINE_CURVE_WITH_KNOTS('',3,(#217096,#217097,#217098,#217099,#217100,
#217101,#217102,#217103,#217104,#217105,#217106,#217107,#217108,#217109,
#217110,#217111,#217112,#217113,#217114,#217115,#217116,#217117,#217118,
#217119,#217120,#217121,#217122,#217123,#217124,#217125,#217126,#217127,
#217128,#217129,#217130,#217131,#217132),.UNSPECIFIED.,.F.,.F.,(4,3,3,3,
3,3,3,3,3,3,3,3,4),(0.,1.12535551670943E-5,7.76936938418916E-5,0.000102513517961078,
0.000121879189824232,0.000189659041345268,0.000223548967105787,0.000257294099096112,
0.000257438892866305,0.000325720851760699,0.000396486773966138,0.000466242707678695,
0.00051487778573261),.UNSPECIFIED.);
#4878=B_SPLINE_CURVE_WITH_KNOTS('',3,(#217140,#217141,#217142,#217143,#217144,
#217145,#217146,#217147,#217148,#217149,#217150,#217151,#217152,#217153,
#217154,#217155,#217156,#217157,#217158,#217159,#217160,#217161,#217162,
#217163,#217164,#217165,#217166,#217167,#217168,#217169,#217170,#217171,
#217172,#217173,#217174,#217175,#217176,#217177,#217178,#217179),
 .UNSPECIFIED.,.F.,.F.,(4,3,3,3,3,3,3,3,3,3,3,3,3,4),(0.,6.80370855409884E-5,
0.000137303169307076,0.000203636706675499,0.000256396220959705,0.00025654023729574,
0.000285209320207724,0.000342105100635646,0.000384776935956587,0.00040077887420194,
0.000456785658060675,0.000484789049990042,0.000498790745954726,0.00051279244191941),
 .UNSPECIFIED.);
#4879=B_SPLINE_CURVE_WITH_KNOTS('',3,(#217183,#217184,#217185,#217186,#217187,
#217188,#217189,#217190,#217191,#217192,#217193,#217194,#217195,#217196,
#217197,#217198,#217199,#217200,#217201,#217202,#217203,#217204,#217205,
#217206,#217207,#217208,#217209,#217210,#217211,#217212,#217213,#217214,
#217215,#217216,#217217,#217218,#217219),.UNSPECIFIED.,.F.,.F.,(4,3,3,3,
3,3,3,3,3,3,3,3,4),(0.,1.12535551670965E-5,7.76936938395602E-5,0.000102513517961085,
0.000121879189824238,0.000189659041345273,0.000223548967105791,0.000257294099096104,
0.000257438892866308,0.000325720851759098,0.000396486773962644,0.000466242707673163,
0.000514877785732617),.UNSPECIFIED.);
#4880=B_SPLINE_CURVE_WITH_KNOTS('',3,(#217227,#217228,#217229,#217230,#217231,
#217232,#217233,#217234,#217235,#217236,#217237,#217238,#217239,#217240,
#217241,#217242,#217243,#217244,#217245,#217246,#217247,#217248,#217249,
#217250,#217251,#217252,#217253,#217254,#217255,#217256,#217257,#217258,
#217259,#217260,#217261,#217262,#217263,#217264,#217265,#217266),
 .UNSPECIFIED.,.F.,.F.,(4,3,3,3,3,3,3,3,3,3,3,3,3,4),(0.,6.80370855374658E-5,
0.000137303169300085,0.000203636706665282,0.000256396220959703,0.00025654023729573,
0.000285209320207737,0.000342105100635654,0.000384776935956592,0.000400778874201944,
0.000456785658060675,0.00048478904999004,0.000498790745954723,0.000512792441919406),
 .UNSPECIFIED.);
#4881=B_SPLINE_CURVE_WITH_KNOTS('',3,(#217270,#217271,#217272,#217273,#217274,
#217275,#217276,#217277,#217278,#217279,#217280,#217281,#217282,#217283,
#217284,#217285,#217286,#217287,#217288,#217289,#217290,#217291,#217292,
#217293,#217294,#217295,#217296,#217297,#217298,#217299,#217300,#217301,
#217302,#217303,#217304,#217305,#217306),.UNSPECIFIED.,.F.,.F.,(4,3,3,3,
3,3,3,3,3,3,3,3,4),(0.,1.12535551670993E-5,7.76936938487074E-5,0.000102513517961113,
0.000121879189824263,0.000189659041345285,0.000223548967105796,0.000257294099096103,
0.000257438892866307,0.000325720851757075,0.000396486773958827,0.000466242707667839,
0.000514877785732613),.UNSPECIFIED.);
#4882=B_SPLINE_CURVE_WITH_KNOTS('',3,(#217314,#217315,#217316,#217317,#217318,
#217319,#217320,#217321,#217322,#217323,#217324,#217325,#217326,#217327,
#217328,#217329,#217330,#217331,#217332,#217333,#217334,#217335,#217336,
#217337,#217338,#217339,#217340,#217341,#217342,#217343,#217344,#217345,
#217346,#217347,#217348,#217349,#217350,#217351,#217352,#217353),
 .UNSPECIFIED.,.F.,.F.,(4,3,3,3,3,3,3,3,3,3,3,3,3,4),(0.,6.80370855423606E-5,
0.00013730316931023,0.000203636706680789,0.000256396220959703,0.000256540237295728,
0.000285209320207732,0.00034210510063565,0.000384776935956589,0.000400778874201941,
0.000456785658060673,0.000484789049990039,0.000498790745954722,0.000512792441919405),
 .UNSPECIFIED.);
#4883=B_SPLINE_CURVE_WITH_KNOTS('',3,(#217357,#217358,#217359,#217360,#217361,
#217362,#217363,#217364,#217365,#217366,#217367,#217368,#217369,#217370,
#217371,#217372,#217373,#217374,#217375,#217376,#217377,#217378,#217379,
#217380,#217381,#217382,#217383,#217384,#217385,#217386,#217387,#217388,
#217389,#217390,#217391,#217392,#217393),.UNSPECIFIED.,.F.,.F.,(4,3,3,3,
3,3,3,3,3,3,3,3,4),(0.,1.1253555167105E-5,7.76936938446724E-5,0.000102513517961175,
0.000121879189824317,0.000189659041345312,0.00022354896710581,0.000257294099096104,
0.000257438892866308,0.000325720851757317,0.000396486773958935,0.000466242707667538,
0.000514877785732616),.UNSPECIFIED.);
#4884=B_SPLINE_CURVE_WITH_KNOTS('',3,(#217401,#217402,#217403,#217404,#217405,
#217406,#217407,#217408,#217409,#217410,#217411,#217412,#217413,#217414,
#217415,#217416,#217417,#217418,#217419,#217420,#217421,#217422,#217423,
#217424,#217425,#217426,#217427,#217428,#217429,#217430,#217431,#217432,
#217433,#217434,#217435,#217436,#217437,#217438,#217439,#217440),
 .UNSPECIFIED.,.F.,.F.,(4,3,3,3,3,3,3,3,3,3,3,3,3,4),(0.,6.80370855342187E-5,
0.000137303169293596,0.00020363670665595,0.000256396220959707,0.000256540237295735,
0.000285209320207739,0.000342105100635658,0.000384776935956597,0.000400778874201949,
0.000456785658060681,0.000484789049990047,0.000498790745954731,0.000512792441919414),
 .UNSPECIFIED.);
#4885=B_SPLINE_CURVE_WITH_KNOTS('',3,(#217444,#217445,#217446,#217447,#217448,
#217449,#217450,#217451,#217452,#217453,#217454,#217455,#217456,#217457,
#217458,#217459,#217460,#217461,#217462,#217463,#217464,#217465,#217466,
#217467,#217468,#217469,#217470,#217471,#217472,#217473,#217474,#217475,
#217476,#217477,#217478,#217479,#217480),.UNSPECIFIED.,.F.,.F.,(4,3,3,3,
3,3,3,3,3,3,3,3,4),(0.,1.12535551671E-5,7.76936938449809E-5,0.000102513517961145,
0.000121879189824289,0.000189659041345296,0.0002235489671058,0.000257294099096096,
0.000257438892866303,0.000325720851758823,0.000396486773962096,0.000466242707672159,
0.000514877785732606),.UNSPECIFIED.);
#4886=B_SPLINE_CURVE_WITH_KNOTS('',3,(#217488,#217489,#217490,#217491,#217492,
#217493,#217494,#217495,#217496,#217497,#217498,#217499,#217500,#217501,
#217502,#217503,#217504,#217505,#217506,#217507,#217508,#217509,#217510,
#217511,#217512,#217513,#217514,#217515,#217516,#217517,#217518,#217519,
#217520,#217521,#217522,#217523,#217524,#217525,#217526,#217527),
 .UNSPECIFIED.,.F.,.F.,(4,3,3,3,3,3,3,3,3,3,3,3,3,4),(0.,6.80370855354539E-5,
0.000137303169295957,0.000203636706659032,0.000256396220959704,0.000256540237295736,
0.000285209320207732,0.000342105100635651,0.00038477693595659,0.000400778874201942,
0.000456785658060675,0.000484789049990042,0.000498790745954725,0.000512792441919408),
 .UNSPECIFIED.);
#4887=B_SPLINE_CURVE_WITH_KNOTS('',3,(#217531,#217532,#217533,#217534,#217535,
#217536,#217537,#217538,#217539,#217540,#217541,#217542,#217543,#217544,
#217545,#217546,#217547,#217548,#217549,#217550,#217551,#217552,#217553,
#217554,#217555,#217556,#217557,#217558,#217559,#217560,#217561,#217562,
#217563,#217564,#217565,#217566,#217567),.UNSPECIFIED.,.F.,.F.,(4,3,3,3,
3,3,3,3,3,3,3,3,4),(0.,1.1253555167102E-5,7.76936938454641E-5,0.00010251351796113,
0.000121879189824277,0.00018965904134529,0.000223548967105796,0.000257294099096106,
0.000257438892866303,0.000325720851760651,0.000396486773965936,0.000466242707677974,
0.000514877785732606),.UNSPECIFIED.);
#4888=B_SPLINE_CURVE_WITH_KNOTS('',3,(#217575,#217576,#217577,#217578,#217579,
#217580,#217581,#217582,#217583,#217584,#217585,#217586,#217587,#217588,
#217589,#217590,#217591,#217592,#217593,#217594,#217595,#217596,#217597,
#217598,#217599,#217600,#217601,#217602,#217603,#217604,#217605,#217606,
#217607,#217608,#217609,#217610,#217611,#217612,#217613,#217614),
 .UNSPECIFIED.,.F.,.F.,(4,3,3,3,3,3,3,3,3,3,3,3,3,4),(0.,6.803708553663E-5,
0.000137303169298813,0.000203636706664354,0.000256396220959703,0.00025654023729573,
0.000285209320207739,0.000342105100635656,0.000384776935956593,0.000400778874201945,
0.000456785658060676,0.000484789049990041,0.000498790745954724,0.000512792441919407),
 .UNSPECIFIED.);
#4889=B_SPLINE_CURVE_WITH_KNOTS('',3,(#217618,#217619,#217620,#217621,#217622,
#217623,#217624,#217625,#217626,#217627,#217628,#217629,#217630,#217631,
#217632,#217633,#217634,#217635,#217636,#217637,#217638,#217639,#217640,
#217641,#217642,#217643,#217644,#217645,#217646,#217647,#217648,#217649,
#217650,#217651,#217652,#217653,#217654),.UNSPECIFIED.,.F.,.F.,(4,3,3,3,
3,3,3,3,3,3,3,3,4),(0.,1.12535551671007E-5,7.76936938461026E-5,0.000102513517961134,
0.000121879189824281,0.000189659041345296,0.000223548967105803,0.000257294099096114,
0.00025743889286631,0.000325720851760575,0.000396486773965635,0.00046624270767721,
0.00051487778573262),.UNSPECIFIED.);
#4890=B_SPLINE_CURVE_WITH_KNOTS('',3,(#217662,#217663,#217664,#217665,#217666,
#217667,#217668,#217669,#217670,#217671,#217672,#217673,#217674,#217675,
#217676,#217677,#217678,#217679,#217680,#217681,#217682,#217683,#217684,
#217685,#217686,#217687,#217688,#217689,#217690,#217691,#217692,#217693,
#217694,#217695,#217696,#217697,#217698,#217699,#217700,#217701),
 .UNSPECIFIED.,.F.,.F.,(4,3,3,3,3,3,3,3,3,3,3,3,3,4),(0.,6.80370855347069E-5,
0.000137303169294128,0.000203636706655648,0.000256396220959708,0.000256540237295743,
0.000285209320207736,0.000342105100635656,0.000384776935956596,0.000400778874201949,
0.000456785658060683,0.000484789049990049,0.000498790745954733,0.000512792441919416),
 .UNSPECIFIED.);
#4891=B_SPLINE_CURVE_WITH_KNOTS('',3,(#217705,#217706,#217707,#217708,#217709,
#217710,#217711,#217712,#217713,#217714,#217715,#217716,#217717,#217718,
#217719,#217720,#217721,#217722,#217723,#217724,#217725,#217726,#217727,
#217728,#217729,#217730,#217731,#217732,#217733,#217734,#217735,#217736,
#217737,#217738,#217739,#217740,#217741),.UNSPECIFIED.,.F.,.F.,(4,3,3,3,
3,3,3,3,3,3,3,3,4),(0.,1.12535551670983E-5,7.76936938492197E-5,0.000102513517961119,
0.000121879189824267,0.000189659041345288,0.000223548967105798,0.000257294099096109,
0.000257438892866308,0.000325720851756761,0.000396486773957922,0.000466242707665982,
0.000514877785732616),.UNSPECIFIED.);
#4892=B_SPLINE_CURVE_WITH_KNOTS('',3,(#217749,#217750,#217751,#217752,#217753,
#217754,#217755,#217756,#217757,#217758,#217759,#217760,#217761,#217762,
#217763,#217764,#217765,#217766,#217767,#217768,#217769,#217770,#217771,
#217772,#217773,#217774,#217775,#217776,#217777,#217778,#217779,#217780,
#217781,#217782,#217783,#217784,#217785,#217786,#217787,#217788),
 .UNSPECIFIED.,.F.,.F.,(4,3,3,3,3,3,3,3,3,3,3,3,3,4),(0.,6.80370855408555E-5,
0.000137303169306811,0.000203636706674952,0.000256396220959707,0.000256540237295744,
0.000285209320207731,0.000342105100635651,0.000384776935956592,0.000400778874201945,
0.000456785658060679,0.000484789049990046,0.00049879074595473,0.000512792441919414),
 .UNSPECIFIED.);
#4893=B_SPLINE_CURVE_WITH_KNOTS('',3,(#217792,#217793,#217794,#217795,#217796,
#217797,#217798,#217799,#217800,#217801,#217802,#217803,#217804,#217805,
#217806,#217807,#217808,#217809,#217810,#217811,#217812,#217813,#217814,
#217815,#217816,#217817,#217818,#217819,#217820,#217821,#217822,#217823,
#217824,#217825,#217826,#217827,#217828),.UNSPECIFIED.,.F.,.F.,(4,3,3,3,
3,3,3,3,3,3,3,3,4),(0.,1.12535551670949E-5,7.76936938407407E-5,0.000102513517961092,
0.000121879189824244,0.000189659041345276,0.000223548967105792,0.00025729409909611,
0.000257438892866308,0.000325720851755195,0.000396486773954161,0.000466242707659613,
0.000514877785732615),.UNSPECIFIED.);
#4894=B_SPLINE_CURVE_WITH_KNOTS('',3,(#217836,#217837,#217838,#217839,#217840,
#217841,#217842,#217843,#217844,#217845,#217846,#217847,#217848,#217849,
#217850,#217851,#217852,#217853,#217854,#217855,#217856,#217857,#217858,
#217859,#217860,#217861,#217862,#217863,#217864,#217865,#217866,#217867,
#217868,#217869,#217870,#217871,#217872,#217873,#217874,#217875),
 .UNSPECIFIED.,.F.,.F.,(4,3,3,3,3,3,3,3,3,3,3,3,3,4),(0.,6.80370855333573E-5,
0.000137303169291925,0.000203636706653624,0.000256396220959706,0.000256540237295727,
0.000285209320207726,0.000342105100635648,0.000384776935956589,0.000400778874201942,
0.000456785658060677,0.000484789049990045,0.000498790745954729,0.000512792441919413),
 .UNSPECIFIED.);
#4895=B_SPLINE_CURVE_WITH_KNOTS('',3,(#217879,#217880,#217881,#217882,#217883,
#217884,#217885,#217886,#217887,#217888,#217889,#217890,#217891,#217892,
#217893,#217894,#217895,#217896,#217897,#217898,#217899,#217900,#217901,
#217902,#217903,#217904,#217905,#217906,#217907,#217908,#217909,#217910,
#217911,#217912,#217913,#217914,#217915),.UNSPECIFIED.,.F.,.F.,(4,3,3,3,
3,3,3,3,3,3,3,3,4),(0.,1.1253555167097E-5,7.76936938509154E-5,0.000102513517961086,
0.000121879189824237,0.000189659041345268,0.000223548967105783,0.000257294099096094,
0.000257438892866298,0.000325720851754246,0.000396486773952907,0.000466242707658961,
0.000514877785732597),.UNSPECIFIED.);
#4896=B_SPLINE_CURVE_WITH_KNOTS('',3,(#217923,#217924,#217925,#217926,#217927,
#217928,#217929,#217930,#217931,#217932,#217933,#217934,#217935,#217936,
#217937,#217938,#217939,#217940,#217941,#217942,#217943,#217944,#217945,
#217946,#217947,#217948,#217949,#217950,#217951,#217952,#217953,#217954,
#217955,#217956,#217957,#217958,#217959,#217960,#217961,#217962),
 .UNSPECIFIED.,.F.,.F.,(4,3,3,3,3,3,3,3,3,3,3,3,3,4),(0.,6.80370855338805E-5,
0.000137303169293391,0.000203636706656483,0.000256396220959711,0.000256540237295738,
0.000285209320207759,0.000342105100635674,0.000384776935956611,0.000400778874201962,
0.000456785658060692,0.000484789049990056,0.000498790745954739,0.000512792441919421),
 .UNSPECIFIED.);
#4897=B_SPLINE_CURVE_WITH_KNOTS('',3,(#217966,#217967,#217968,#217969,#217970,
#217971,#217972,#217973,#217974,#217975,#217976,#217977,#217978,#217979,
#217980,#217981,#217982,#217983,#217984,#217985,#217986,#217987,#217988,
#217989,#217990,#217991,#217992,#217993,#217994,#217995,#217996,#217997,
#217998,#217999,#218000,#218001,#218002),.UNSPECIFIED.,.F.,.F.,(4,3,3,3,
3,3,3,3,3,3,3,3,4),(0.,1.12535551670982E-5,7.769369384278E-5,0.000102513517961137,
0.000121879189824283,0.00018965904134529,0.000223548967105794,0.000257294099096092,
0.000257438892866298,0.000325720851758372,0.000396486773960825,0.000466242707669822,
0.000514877785732597),.UNSPECIFIED.);
#4898=B_SPLINE_CURVE_WITH_KNOTS('',3,(#218010,#218011,#218012,#218013,#218014,
#218015,#218016,#218017,#218018,#218019,#218020,#218021,#218022,#218023,
#218024,#218025,#218026,#218027,#218028,#218029,#218030,#218031,#218032,
#218033,#218034,#218035,#218036,#218037,#218038,#218039,#218040,#218041,
#218042,#218043,#218044,#218045,#218046,#218047,#218048,#218049),
 .UNSPECIFIED.,.F.,.F.,(4,3,3,3,3,3,3,3,3,3,3,3,3,4),(0.,6.80370855393617E-5,
0.000137303169304187,0.000203636706671761,0.000256396220959703,0.000256540237295725,
0.000285209320207727,0.000342105100635646,0.000384776935956586,0.000400778874201938,
0.000456785658060672,0.000484789049990039,0.000498790745954722,0.000512792441919405),
 .UNSPECIFIED.);
#4899=B_SPLINE_CURVE_WITH_KNOTS('',3,(#218053,#218054,#218055,#218056,#218057,
#218058,#218059,#218060,#218061,#218062,#218063,#218064,#218065,#218066,
#218067,#218068,#218069,#218070,#218071,#218072,#218073,#218074,#218075,
#218076,#218077,#218078,#218079,#218080,#218081,#218082,#218083,#218084,
#218085,#218086,#218087,#218088,#218089),.UNSPECIFIED.,.F.,.F.,(4,3,3,3,
3,3,3,3,3,3,3,3,4),(0.,1.12535551670974E-5,7.76936938354461E-5,0.000102513517961112,
0.000121879189824261,0.000189659041345284,0.000223548967105795,0.000257294099096103,
0.000257438892866306,0.000325720851764097,0.000396486773972469,0.000466242707686801,
0.000514877785732612),.UNSPECIFIED.);
#4900=B_SPLINE_CURVE_WITH_KNOTS('',3,(#218097,#218098,#218099,#218100,#218101,
#218102,#218103,#218104,#218105,#218106,#218107,#218108,#218109,#218110,
#218111,#218112,#218113,#218114,#218115,#218116,#218117,#218118,#218119,
#218120,#218121,#218122,#218123,#218124,#218125,#218126,#218127,#218128,
#218129,#218130,#218131,#218132,#218133,#218134,#218135,#218136),
 .UNSPECIFIED.,.F.,.F.,(4,3,3,3,3,3,3,3,3,3,3,3,3,4),(0.,6.8037085540861E-5,
0.000137303169307164,0.000203636706676043,0.000256396220959705,0.000256540237295742,
0.000285209320207739,0.000342105100635657,0.000384776935956595,0.000400778874201947,
0.000456785658060679,0.000484789049990045,0.000498790745954728,0.000512792441919411),
 .UNSPECIFIED.);
#4901=B_SPLINE_CURVE_WITH_KNOTS('',3,(#218140,#218141,#218142,#218143,#218144,
#218145,#218146,#218147,#218148,#218149,#218150,#218151,#218152,#218153,
#218154,#218155,#218156,#218157,#218158,#218159,#218160,#218161,#218162,
#218163,#218164,#218165,#218166,#218167,#218168,#218169,#218170,#218171,
#218172,#218173,#218174,#218175,#218176),.UNSPECIFIED.,.F.,.F.,(4,3,3,3,
3,3,3,3,3,3,3,3,4),(0.,1.12535551670985E-5,7.76936938454086E-5,0.000102513517961139,
0.000121879189824285,0.000189659041345297,0.000223548967105803,0.000257294099096096,
0.000257438892866308,0.000325720851768916,0.000396486773983027,0.000466242707703339,
0.000514877785732617),.UNSPECIFIED.);
#4902=B_SPLINE_CURVE_WITH_KNOTS('',3,(#218184,#218185,#218186,#218187,#218188,
#218189,#218190,#218191,#218192,#218193,#218194,#218195,#218196,#218197,
#218198,#218199,#218200,#218201,#218202,#218203,#218204,#218205,#218206,
#218207,#218208,#218209,#218210,#218211,#218212,#218213,#218214,#218215,
#218216,#218217,#218218,#218219,#218220,#218221,#218222,#218223),
 .UNSPECIFIED.,.F.,.F.,(4,3,3,3,3,3,3,3,3,3,3,3,3,4),(0.,6.80370855365877E-5,
0.000137303169299356,0.000203636706666889,0.000256396220959707,0.000256540237295743,
0.000285209320207725,0.000342105100635648,0.000384776935956589,0.000400778874201942,
0.000456785658060678,0.000484789049990046,0.00049879074595473,0.000512792441919414),
 .UNSPECIFIED.);
#4903=B_SPLINE_CURVE_WITH_KNOTS('',3,(#218227,#218228,#218229,#218230,#218231,
#218232,#218233,#218234,#218235,#218236,#218237,#218238,#218239,#218240,
#218241,#218242,#218243,#218244,#218245,#218246,#218247,#218248,#218249,
#218250,#218251,#218252,#218253,#218254,#218255,#218256,#218257,#218258,
#218259,#218260,#218261,#218262,#218263),.UNSPECIFIED.,.F.,.F.,(4,3,3,3,
3,3,3,3,3,3,3,3,4),(0.,1.12535551670997E-5,7.76936938459687E-5,0.000102513517961119,
0.000121879189824267,0.000189659041345284,0.000223548967105793,0.000257294099096094,
0.000257438892866301,0.000325720851764935,0.000396486773975291,0.000466242707692906,
0.000514877785732603),.UNSPECIFIED.);
#4904=B_SPLINE_CURVE_WITH_KNOTS('',3,(#218271,#218272,#218273,#218274,#218275,
#218276,#218277,#218278,#218279,#218280,#218281,#218282,#218283,#218284,
#218285,#218286,#218287,#218288,#218289,#218290,#218291,#218292,#218293,
#218294,#218295,#218296,#218297,#218298,#218299,#218300,#218301,#218302,
#218303,#218304,#218305,#218306,#218307,#218308,#218309,#218310),
 .UNSPECIFIED.,.F.,.F.,(4,3,3,3,3,3,3,3,3,3,3,3,3,4),(0.,6.80370855413805E-5,
0.000137303169307998,0.00020363670667671,0.000256396220959706,0.000256540237295745,
0.000285209320207745,0.000342105100635662,0.0003847769359566,0.000400778874201951,
0.000456785658060682,0.000484789049990047,0.00049879074595473,0.000512792441919413),
 .UNSPECIFIED.);
#4905=B_SPLINE_CURVE_WITH_KNOTS('',3,(#218314,#218315,#218316,#218317,#218318,
#218319,#218320,#218321,#218322,#218323,#218324,#218325,#218326,#218327,
#218328,#218329,#218330,#218331,#218332,#218333,#218334,#218335,#218336,
#218337,#218338,#218339,#218340,#218341,#218342,#218343,#218344,#218345,
#218346,#218347,#218348,#218349,#218350),.UNSPECIFIED.,.F.,.F.,(4,3,3,3,
3,3,3,3,3,3,3,3,4),(0.,1.12535551671018E-5,7.76936938515147E-5,0.000102513517961147,
0.000121879189824292,0.0001896590413453,0.000223548967105803,0.000257294099096102,
0.000257438892866307,0.000325720851754139,0.000396486773952012,0.000466242707656176,
0.000514877785732614),.UNSPECIFIED.);
#4906=B_SPLINE_CURVE_WITH_KNOTS('',3,(#218358,#218359,#218360,#218361,#218362,
#218363,#218364,#218365,#218366,#218367,#218368,#218369,#218370,#218371,
#218372,#218373,#218374,#218375,#218376,#218377,#218378,#218379,#218380,
#218381,#218382,#218383,#218384,#218385,#218386,#218387,#218388,#218389,
#218390,#218391,#218392,#218393,#218394,#218395,#218396,#218397),
 .UNSPECIFIED.,.F.,.F.,(4,3,3,3,3,3,3,3,3,3,3,3,3,4),(0.,6.80370855389298E-5,
0.000137303169302839,0.000203636706669121,0.000256396220959704,0.000256540237295741,
0.000285209320207746,0.000342105100635661,0.000384776935956598,0.000400778874201949,
0.000456785658060678,0.000484789049990043,0.000498790745954725,0.000512792441919407),
 .UNSPECIFIED.);
#4907=B_SPLINE_CURVE_WITH_KNOTS('',3,(#218401,#218402,#218403,#218404,#218405,
#218406,#218407,#218408,#218409,#218410,#218411,#218412,#218413,#218414,
#218415,#218416,#218417,#218418,#218419,#218420,#218421,#218422,#218423,
#218424,#218425,#218426,#218427,#218428,#218429,#218430,#218431,#218432,
#218433,#218434,#218435,#218436,#218437),.UNSPECIFIED.,.F.,.F.,(4,3,3,3,
3,3,3,3,3,3,3,3,4),(0.,1.12535551670959E-5,7.76936938459669E-5,0.0001025135179611,
0.00012187918982425,0.000189659041345275,0.000223548967105788,0.000257294099096094,
0.000257438892866301,0.000325720851752298,0.000396486773948228,0.000466242707650774,
0.000514877785732601),.UNSPECIFIED.);
#4908=B_SPLINE_CURVE_WITH_KNOTS('',3,(#218445,#218446,#218447,#218448,#218449,
#218450,#218451,#218452,#218453,#218454,#218455,#218456,#218457,#218458,
#218459,#218460,#218461,#218462,#218463,#218464,#218465,#218466,#218467,
#218468,#218469,#218470,#218471,#218472,#218473,#218474,#218475,#218476,
#218477,#218478,#218479,#218480,#218481,#218482,#218483,#218484),
 .UNSPECIFIED.,.F.,.F.,(4,3,3,3,3,3,3,3,3,3,3,3,3,4),(0.,6.80370855424441E-5,
0.000137303169309744,0.000203636706678789,0.000256396220959707,0.000256540237295729,
0.000285209320207743,0.000342105100635661,0.000384776935956599,0.000400778874201951,
0.000456785658060683,0.000484789049990049,0.000498790745954732,0.000512792441919415),
 .UNSPECIFIED.);
#4909=B_SPLINE_CURVE_WITH_KNOTS('',3,(#218488,#218489,#218490,#218491,#218492,
#218493,#218494,#218495,#218496,#218497,#218498,#218499,#218500,#218501,
#218502,#218503,#218504,#218505,#218506,#218507,#218508,#218509,#218510,
#218511,#218512,#218513,#218514,#218515,#218516,#218517,#218518,#218519,
#218520,#218521,#218522,#218523,#218524),.UNSPECIFIED.,.F.,.F.,(4,3,3,3,
3,3,3,3,3,3,3,3,4),(0.,1.12535551670972E-5,7.76936938431592E-5,0.00010251351796109,
0.000121879189824242,0.000189659041345273,0.000223548967105789,0.000257294099096099,
0.000257438892866304,0.000325720851758791,0.000396486773961801,0.000466242707671268,
0.000514877785732608),.UNSPECIFIED.);
#4910=B_SPLINE_CURVE_WITH_KNOTS('',3,(#218532,#218533,#218534,#218535,#218536,
#218537,#218538,#218539,#218540,#218541,#218542,#218543,#218544,#218545,
#218546,#218547,#218548,#218549,#218550,#218551,#218552,#218553,#218554,
#218555,#218556,#218557,#218558,#218559,#218560,#218561,#218562,#218563,
#218564,#218565,#218566,#218567,#218568,#218569,#218570,#218571),
 .UNSPECIFIED.,.F.,.F.,(4,3,3,3,3,3,3,3,3,3,3,3,3,4),(0.,6.8037085534851E-5,
0.000137303169294966,0.000203636706658237,0.000256396220959703,0.000256540237295729,
0.000285209320207737,0.000342105100635654,0.000384776935956592,0.000400778874201944,
0.000456785658060675,0.00048478904999004,0.000498790745954723,0.000512792441919405),
 .UNSPECIFIED.);
#4911=B_SPLINE_CURVE_WITH_KNOTS('',3,(#218575,#218576,#218577,#218578,#218579,
#218580,#218581,#218582,#218583,#218584,#218585,#218586,#218587,#218588,
#218589,#218590,#218591,#218592,#218593,#218594,#218595,#218596,#218597,
#218598,#218599,#218600,#218601,#218602,#218603,#218604,#218605,#218606,
#218607,#218608,#218609,#218610,#218611),.UNSPECIFIED.,.F.,.F.,(4,3,3,3,
3,3,3,3,3,3,3,3,4),(0.,1.12535551670989E-5,7.76936938479744E-5,0.000102513517961094,
0.000121879189824246,0.000189659041345275,0.00022354896710579,0.000257294099096105,
0.000257438892866304,0.00032572085175291,0.000396486773950194,0.000466242707655154,
0.000514877785732609),.UNSPECIFIED.);
#4912=B_SPLINE_CURVE_WITH_KNOTS('',3,(#218619,#218620,#218621,#218622,#218623,
#218624,#218625,#218626,#218627,#218628,#218629,#218630,#218631,#218632,
#218633,#218634,#218635,#218636,#218637,#218638,#218639,#218640,#218641,
#218642,#218643,#218644,#218645,#218646,#218647,#218648,#218649,#218650,
#218651,#218652,#218653,#218654,#218655,#218656,#218657,#218658),
 .UNSPECIFIED.,.F.,.F.,(4,3,3,3,3,3,3,3,3,3,3,3,3,4),(0.,6.80370855361618E-5,
0.000137303169297681,0.000203636706662249,0.000256396220959705,0.000256540237295736,
0.000285209320207737,0.000342105100635655,0.000384776935956594,0.000400778874201946,
0.000456785658060677,0.000484789049990043,0.000498790745954726,0.000512792441919409),
 .UNSPECIFIED.);
#4913=B_SPLINE_CURVE_WITH_KNOTS('',3,(#218662,#218663,#218664,#218665,#218666,
#218667,#218668,#218669,#218670,#218671,#218672,#218673,#218674,#218675,
#218676,#218677,#218678,#218679,#218680,#218681,#218682,#218683,#218684,
#218685,#218686,#218687,#218688,#218689,#218690,#218691,#218692,#218693,
#218694,#218695,#218696,#218697,#218698),.UNSPECIFIED.,.F.,.F.,(4,3,3,3,
3,3,3,3,3,3,3,3,4),(0.,1.12535551671016E-5,7.76936938480596E-5,0.000102513517961156,
0.0001218791898243,0.000189659041345303,0.000223548967105804,0.000257294099096105,
0.000257438892866306,0.000325720851759106,0.000396486773962859,0.00046624270767365,
0.000514877785732612),.UNSPECIFIED.);
#4914=B_SPLINE_CURVE_WITH_KNOTS('',3,(#218706,#218707,#218708,#218709,#218710,
#218711,#218712,#218713,#218714,#218715,#218716,#218717,#218718,#218719,
#218720,#218721,#218722,#218723,#218724,#218725,#218726,#218727,#218728,
#218729,#218730,#218731,#218732,#218733,#218734,#218735,#218736,#218737,
#218738,#218739,#218740,#218741,#218742,#218743,#218744,#218745),
 .UNSPECIFIED.,.F.,.F.,(4,3,3,3,3,3,3,3,3,3,3,3,3,4),(0.,6.8037085534625E-5,
0.00013730316929443,0.000203636706657177,0.000256396220959704,0.000256540237295729,
0.000285209320207743,0.00034210510063566,0.000384776935956597,0.000400778874201948,
0.000456785658060678,0.000484789049990043,0.000498790745954726,0.000512792441919408),
 .UNSPECIFIED.);
#4915=B_SPLINE_CURVE_WITH_KNOTS('',3,(#218752,#218753,#218754,#218755,#218756,
#218757,#218758,#218759,#218760,#218761,#218762,#218763,#218764,#218765,
#218766,#218767,#218768,#218769,#218770,#218771,#218772,#218773,#218774,
#218775,#218776,#218777,#218778,#218779,#218780,#218781,#218782,#218783,
#218784,#218785,#218786,#218787,#218788),.UNSPECIFIED.,.F.,.F.,(4,3,3,3,
3,3,3,3,3,3,3,3,4),(0.,1.12535551670991E-5,7.76936938497371E-5,0.000102513517961127,
0.000121879189824275,0.00018965904134529,0.000223548967105798,0.000257294099096094,
0.000257438892866306,0.000325720851756744,0.000396486773957958,0.000466242707666199,
0.000514877785732612),.UNSPECIFIED.);
#4916=B_SPLINE_CURVE_WITH_KNOTS('',3,(#218796,#218797,#218798,#218799,#218800,
#218801,#218802,#218803,#218804,#218805,#218806,#218807,#218808,#218809,
#218810,#218811,#218812,#218813,#218814,#218815,#218816,#218817,#218818,
#218819,#218820,#218821,#218822,#218823,#218824,#218825,#218826,#218827,
#218828,#218829,#218830,#218831,#218832,#218833,#218834,#218835),
 .UNSPECIFIED.,.F.,.F.,(4,3,3,3,3,3,3,3,3,3,3,3,3,4),(0.,6.8037085536429E-5,
0.00013730316929818,0.000203636706662896,0.000256396220959701,0.000256540237295736,
0.000285209320207738,0.000342105100635654,0.000384776935956591,0.000400778874201942,
0.000456785658060672,0.000484789049990037,0.000498790745954719,0.000512792441919401),
 .UNSPECIFIED.);
#4917=B_SPLINE_CURVE_WITH_KNOTS('',3,(#218839,#218840,#218841,#218842,#218843,
#218844,#218845,#218846,#218847,#218848,#218849,#218850,#218851,#218852,
#218853,#218854,#218855,#218856,#218857,#218858,#218859,#218860,#218861,
#218862,#218863,#218864,#218865,#218866,#218867,#218868,#218869,#218870,
#218871,#218872,#218873,#218874,#218875),.UNSPECIFIED.,.F.,.F.,(4,3,3,3,
3,3,3,3,3,3,3,3,4),(0.,1.12535551670982E-5,7.76936938451034E-5,0.000102513517961114,
0.000121879189824263,0.000189659041345285,0.000223548967105796,0.000257294099096108,
0.000257438892866307,0.000325720851759771,0.000396486773963886,0.000466242707674355,
0.000514877785732613),.UNSPECIFIED.);
#4918=B_SPLINE_CURVE_WITH_KNOTS('',3,(#218883,#218884,#218885,#218886,#218887,
#218888,#218889,#218890,#218891,#218892,#218893,#218894,#218895,#218896,
#218897,#218898,#218899,#218900,#218901,#218902,#218903,#218904,#218905,
#218906,#218907,#218908,#218909,#218910,#218911,#218912,#218913,#218914,
#218915,#218916,#218917,#218918,#218919,#218920,#218921,#218922),
 .UNSPECIFIED.,.F.,.F.,(4,3,3,3,3,3,3,3,3,3,3,3,3,4),(0.,6.80370855360243E-5,
0.000137303169297593,0.000203636706662558,0.000256396220959703,0.000256540237295725,
0.000285209320207735,0.000342105100635653,0.000384776935956591,0.000400778874201943,
0.000456785658060674,0.00048478904999004,0.000498790745954723,0.000512792441919406),
 .UNSPECIFIED.);
#4919=B_SPLINE_CURVE_WITH_KNOTS('',3,(#218926,#218927,#218928,#218929,#218930,
#218931,#218932,#218933,#218934,#218935,#218936,#218937,#218938,#218939,
#218940,#218941,#218942,#218943,#218944,#218945,#218946,#218947,#218948,
#218949,#218950,#218951,#218952,#218953,#218954,#218955,#218956,#218957,
#218958,#218959,#218960,#218961,#218962),.UNSPECIFIED.,.F.,.F.,(4,3,3,3,
3,3,3,3,3,3,3,3,4),(0.,1.12535551670984E-5,7.76936938487798E-5,0.000102513517961109,
0.000121879189824259,0.000189659041345282,0.000223548967105794,0.000257294099096103,
0.000257438892866306,0.000325720851760856,0.000396486773966341,0.000466242707678374,
0.000514877785732612),.UNSPECIFIED.);
#4920=B_SPLINE_CURVE_WITH_KNOTS('',3,(#218970,#218971,#218972,#218973,#218974,
#218975,#218976,#218977,#218978,#218979,#218980,#218981,#218982,#218983,
#218984,#218985,#218986,#218987,#218988,#218989,#218990,#218991,#218992,
#218993,#218994,#218995,#218996,#218997,#218998,#218999,#219000,#219001,
#219002,#219003,#219004,#219005,#219006,#219007,#219008,#219009),
 .UNSPECIFIED.,.F.,.F.,(4,3,3,3,3,3,3,3,3,3,3,3,3,4),(0.,6.80370855341084E-5,
0.000137303169293612,0.000203636706656273,0.000256396220959707,0.000256540237295736,
0.000285209320207752,0.000342105100635667,0.000384776935956604,0.000400778874201955,
0.000456785658060684,0.000484789049990049,0.000498790745954731,0.000512792441919413),
 .UNSPECIFIED.);
#4921=B_SPLINE_CURVE_WITH_KNOTS('',3,(#219013,#219014,#219015,#219016,#219017,
#219018,#219019,#219020,#219021,#219022,#219023,#219024,#219025,#219026,
#219027,#219028,#219029,#219030,#219031,#219032,#219033,#219034,#219035,
#219036,#219037,#219038,#219039,#219040,#219041,#219042,#219043,#219044,
#219045,#219046,#219047,#219048,#219049),.UNSPECIFIED.,.F.,.F.,(4,3,3,3,
3,3,3,3,3,3,3,3,4),(0.,1.1253555167101E-5,7.76936938410561E-5,0.000102513517961155,
0.000121879189824298,0.000189659041345302,0.000223548967105803,0.000257294099096109,
0.000257438892866305,0.000325720851758758,0.000396486773962038,0.000466242707672476,
0.000514877785732609),.UNSPECIFIED.);
#4922=B_SPLINE_CURVE_WITH_KNOTS('',3,(#219057,#219058,#219059,#219060,#219061,
#219062,#219063,#219064,#219065,#219066,#219067,#219068,#219069,#219070,
#219071,#219072,#219073,#219074,#219075,#219076,#219077,#219078,#219079,
#219080,#219081,#219082,#219083,#219084,#219085,#219086,#219087,#219088,
#219089,#219090,#219091,#219092,#219093,#219094,#219095,#219096),
 .UNSPECIFIED.,.F.,.F.,(4,3,3,3,3,3,3,3,3,3,3,3,3,4),(0.,6.80370855362772E-5,
0.0001373031692974,0.000203636706660765,0.000256396220959705,0.00025654023729573,
0.000285209320207733,0.000342105100635652,0.000384776935956592,0.000400778874201944,
0.000456785658060677,0.000484789049990043,0.000498790745954727,0.00051279244191941),
 .UNSPECIFIED.);
#4923=B_SPLINE_CURVE_WITH_KNOTS('',3,(#219100,#219101,#219102,#219103,#219104,
#219105,#219106,#219107,#219108,#219109,#219110,#219111,#219112,#219113,
#219114,#219115,#219116,#219117,#219118,#219119,#219120,#219121,#219122,
#219123,#219124,#219125,#219126,#219127,#219128,#219129,#219130,#219131,
#219132,#219133,#219134,#219135,#219136),.UNSPECIFIED.,.F.,.F.,(4,3,3,3,
3,3,3,3,3,3,3,3,4),(0.,1.12535551670954E-5,7.7693693843438E-5,0.000102513517961085,
0.000121879189824238,0.000189659041345273,0.000223548967105791,0.000257294099096106,
0.000257438892866309,0.0003257208517587,0.000396486773961633,0.000466242707671069,
0.000514877785732617),.UNSPECIFIED.);
#4924=B_SPLINE_CURVE_WITH_KNOTS('',3,(#219144,#219145,#219146,#219147,#219148,
#219149,#219150,#219151,#219152,#219153,#219154,#219155,#219156,#219157,
#219158,#219159,#219160,#219161,#219162,#219163,#219164,#219165,#219166,
#219167,#219168,#219169,#219170,#219171,#219172,#219173,#219174,#219175,
#219176,#219177,#219178,#219179,#219180,#219181,#219182,#219183),
 .UNSPECIFIED.,.F.,.F.,(4,3,3,3,3,3,3,3,3,3,3,3,3,4),(0.,6.80370855369493E-5,
0.00013730316929952,0.000203636706665799,0.000256396220959709,0.000256540237295725,
0.000285209320207727,0.00034210510063565,0.000384776935956592,0.000400778874201945,
0.000456785658060681,0.000484789049990049,0.000498790745954733,0.000512792441919417),
 .UNSPECIFIED.);
#4925=B_SPLINE_CURVE_WITH_KNOTS('',3,(#219187,#219188,#219189,#219190,#219191,
#219192,#219193,#219194,#219195,#219196,#219197,#219198,#219199,#219200,
#219201,#219202,#219203,#219204,#219205,#219206,#219207,#219208,#219209,
#219210,#219211,#219212,#219213,#219214,#219215,#219216,#219217,#219218,
#219219,#219220,#219221,#219222,#219223),.UNSPECIFIED.,.F.,.F.,(4,3,3,3,
3,3,3,3,3,3,3,3,4),(0.,1.12535551670973E-5,7.76936938503403E-5,0.000102513517961109,
0.000121879189824258,0.000189659041345281,0.000223548967105792,0.000257294099096104,
0.000257438892866303,0.000325720851751885,0.000396486773948232,0.000466242707652404,
0.000514877785732606),.UNSPECIFIED.);
#4926=B_SPLINE_CURVE_WITH_KNOTS('',3,(#219231,#219232,#219233,#219234,#219235,
#219236,#219237,#219238,#219239,#219240,#219241,#219242,#219243,#219244,
#219245,#219246,#219247,#219248,#219249,#219250,#219251,#219252,#219253,
#219254,#219255,#219256,#219257,#219258,#219259,#219260,#219261,#219262,
#219263,#219264,#219265,#219266,#219267,#219268,#219269,#219270),
 .UNSPECIFIED.,.F.,.F.,(4,3,3,3,3,3,3,3,3,3,3,3,3,4),(0.,6.80370855305542E-5,
0.000137303169286892,0.000203636706647725,0.000256396220959703,0.000256540237295726,
0.00028520932020773,0.000342105100635649,0.000384776935956589,0.000400778874201941,
0.000456785658060674,0.00048478904999004,0.000498790745954723,0.000512792441919407),
 .UNSPECIFIED.);
#4927=B_SPLINE_CURVE_WITH_KNOTS('',3,(#219274,#219275,#219276,#219277,#219278,
#219279,#219280,#219281,#219282,#219283,#219284,#219285,#219286,#219287,
#219288,#219289,#219290,#219291,#219292,#219293,#219294,#219295,#219296,
#219297,#219298,#219299,#219300,#219301,#219302,#219303,#219304,#219305,
#219306,#219307,#219308,#219309,#219310),.UNSPECIFIED.,.F.,.F.,(4,3,3,3,
3,3,3,3,3,3,3,3,4),(0.,1.12535551670967E-5,7.7693693841938E-5,0.000102513517961121,
0.000121879189824269,0.000189659041345287,0.000223548967105796,0.000257294099096099,
0.000257438892866305,0.000325720851753896,0.000396486773952486,0.000466242707659185,
0.000514877785732609),.UNSPECIFIED.);
#4928=B_SPLINE_CURVE_WITH_KNOTS('',3,(#219318,#219319,#219320,#219321,#219322,
#219323,#219324,#219325,#219326,#219327,#219328,#219329,#219330,#219331,
#219332,#219333,#219334,#219335,#219336,#219337,#219338,#219339,#219340,
#219341,#219342,#219343,#219344,#219345,#219346,#219347,#219348,#219349,
#219350,#219351,#219352,#219353,#219354,#219355,#219356,#219357),
 .UNSPECIFIED.,.F.,.F.,(4,3,3,3,3,3,3,3,3,3,3,3,3,4),(0.,6.80370855360398E-5,
0.000137303169296802,0.000203636706659669,0.000256396220959709,0.000256540237295733,
0.00028520932020774,0.000342105100635659,0.000384776935956599,0.000400778874201952,
0.000456785658060685,0.000484789049990052,0.000498790745954735,0.000512792441919418),
 .UNSPECIFIED.);
#4929=B_SPLINE_CURVE_WITH_KNOTS('',3,(#219361,#219362,#219363,#219364,#219365,
#219366,#219367,#219368,#219369,#219370,#219371,#219372,#219373,#219374,
#219375,#219376,#219377,#219378,#219379,#219380,#219381,#219382,#219383,
#219384,#219385,#219386,#219387,#219388,#219389,#219390,#219391,#219392,
#219393,#219394,#219395,#219396,#219397),.UNSPECIFIED.,.F.,.F.,(4,3,3,3,
3,3,3,3,3,3,3,3,4),(0.,1.12535551671021E-5,7.76936938520304E-5,0.00010251351796116,
0.000121879189824304,0.000189659041345306,0.000223548967105807,0.00025729409909611,
0.000257438892866308,0.00032572085175869,0.000396486773962042,0.000466242707672318,
0.000514877785732615),.UNSPECIFIED.);
#4930=B_SPLINE_CURVE_WITH_KNOTS('',3,(#219405,#219406,#219407,#219408,#219409,
#219410,#219411,#219412,#219413,#219414,#219415,#219416,#219417,#219418,
#219419,#219420,#219421,#219422,#219423,#219424,#219425,#219426,#219427,
#219428,#219429,#219430,#219431,#219432,#219433,#219434,#219435,#219436,
#219437,#219438,#219439,#219440,#219441,#219442,#219443,#219444),
 .UNSPECIFIED.,.F.,.F.,(4,3,3,3,3,3,3,3,3,3,3,3,3,4),(0.,6.80370855343923E-5,
0.000137303169294156,0.000203636706657648,0.000256396220959702,0.00025654023729573,
0.000285209320207731,0.000342105100635649,0.000384776935956587,0.000400778874201939,
0.000456785658060671,0.000484789049990037,0.00049879074595472,0.000512792441919403),
 .UNSPECIFIED.);
#4931=B_SPLINE_CURVE_WITH_KNOTS('',3,(#219448,#219449,#219450,#219451,#219452,
#219453,#219454,#219455,#219456,#219457,#219458,#219459,#219460,#219461,
#219462,#219463,#219464,#219465,#219466,#219467,#219468,#219469,#219470,
#219471,#219472,#219473,#219474,#219475,#219476,#219477,#219478,#219479,
#219480,#219481,#219482,#219483,#219484),.UNSPECIFIED.,.F.,.F.,(4,3,3,3,
3,3,3,3,3,3,3,3,4),(0.,1.12535551671044E-5,7.76936938363717E-5,0.000102513517961159,
0.000121879189824302,0.000189659041345305,0.000223548967105807,0.000257294099096106,
0.000257438892866309,0.00032572085175684,0.000396486773958732,0.000466242707668953,
0.000514877785732617),.UNSPECIFIED.);
#4932=B_SPLINE_CURVE_WITH_KNOTS('',3,(#219492,#219493,#219494,#219495,#219496,
#219497,#219498,#219499,#219500,#219501,#219502,#219503,#219504,#219505,
#219506,#219507,#219508,#219509,#219510,#219511,#219512,#219513,#219514,
#219515,#219516,#219517,#219518,#219519,#219520,#219521,#219522,#219523,
#219524,#219525,#219526,#219527,#219528,#219529,#219530,#219531),
 .UNSPECIFIED.,.F.,.F.,(4,3,3,3,3,3,3,3,3,3,3,3,3,4),(0.,6.80370855361023E-5,
0.000137303169297632,0.00020363670666265,0.000256396220959704,0.000256540237295734,
0.000285209320207739,0.000342105100635657,0.000384776935956595,0.000400778874201946,
0.000456785658060677,0.000484789049990043,0.000498790745954726,0.000512792441919408),
 .UNSPECIFIED.);
#4933=B_SPLINE_CURVE_WITH_KNOTS('',3,(#219535,#219536,#219537,#219538,#219539,
#219540,#219541,#219542,#219543,#219544,#219545,#219546,#219547,#219548,
#219549,#219550,#219551,#219552,#219553,#219554,#219555,#219556,#219557,
#219558,#219559,#219560,#219561,#219562,#219563,#219564,#219565,#219566,
#219567,#219568,#219569,#219570,#219571),.UNSPECIFIED.,.F.,.F.,(4,3,3,3,
3,3,3,3,3,3,3,3,4),(0.,1.12535551671001E-5,7.76936938493738E-5,0.000102513517961137,
0.000121879189824282,0.000189659041345291,0.000223548967105795,0.000257294099096098,
0.000257438892866299,0.00032572085174627,0.000396486773936295,0.000466242707634075,
0.000514877785732599),.UNSPECIFIED.);
#4934=B_SPLINE_CURVE_WITH_KNOTS('',3,(#219579,#219580,#219581,#219582,#219583,
#219584,#219585,#219586,#219587,#219588,#219589,#219590,#219591,#219592,
#219593,#219594,#219595,#219596,#219597,#219598,#219599,#219600,#219601,
#219602,#219603,#219604,#219605,#219606,#219607,#219608,#219609,#219610,
#219611,#219612,#219613,#219614,#219615,#219616,#219617,#219618),
 .UNSPECIFIED.,.F.,.F.,(4,3,3,3,3,3,3,3,3,3,3,3,3,4),(0.,6.80370855373009E-5,
0.000137303169299663,0.000203636706664318,0.000256396220959702,0.000256540237295726,
0.000285209320207732,0.00034210510063565,0.000384776935956588,0.00040077887420194,
0.000456785658060672,0.000484789049990038,0.000498790745954721,0.000512792441919404),
 .UNSPECIFIED.);
#4935=B_SPLINE_CURVE_WITH_KNOTS('',3,(#219622,#219623,#219624,#219625,#219626,
#219627,#219628,#219629,#219630,#219631,#219632,#219633,#219634,#219635,
#219636,#219637,#219638,#219639,#219640,#219641,#219642,#219643,#219644,
#219645,#219646,#219647,#219648,#219649,#219650,#219651,#219652,#219653,
#219654,#219655,#219656,#219657,#219658),.UNSPECIFIED.,.F.,.F.,(4,3,3,3,
3,3,3,3,3,3,3,3,4),(0.,1.12535551670992E-5,7.76936938444347E-5,0.000102513517961116,
0.000121879189824265,0.000189659041345288,0.000223548967105799,0.000257294099096112,
0.00025743889286631,0.00032572085175845,0.000396486773961124,0.000466242707670346,
0.000514877785732621),.UNSPECIFIED.);
#4936=B_SPLINE_CURVE_WITH_KNOTS('',3,(#219666,#219667,#219668,#219669,#219670,
#219671,#219672,#219673,#219674,#219675,#219676,#219677,#219678,#219679,
#219680,#219681,#219682,#219683,#219684,#219685,#219686,#219687,#219688,
#219689,#219690,#219691,#219692,#219693,#219694,#219695,#219696,#219697,
#219698,#219699,#219700,#219701,#219702,#219703,#219704,#219705),
 .UNSPECIFIED.,.F.,.F.,(4,3,3,3,3,3,3,3,3,3,3,3,3,4),(0.,6.80370855375739E-5,
0.000137303169299986,0.000203636706664461,0.000256396220959699,0.000256540237295735,
0.000285209320207733,0.00034210510063565,0.000384776935956587,0.000400778874201938,
0.000456785658060669,0.000484789049990034,0.000498790745954716,0.000512792441919399),
 .UNSPECIFIED.);
#4937=B_SPLINE_CURVE_WITH_KNOTS('',3,(#219709,#219710,#219711,#219712,#219713,
#219714,#219715,#219716,#219717,#219718,#219719,#219720,#219721,#219722,
#219723,#219724,#219725,#219726,#219727,#219728,#219729,#219730,#219731,
#219732,#219733,#219734,#219735,#219736,#219737,#219738,#219739,#219740,
#219741,#219742,#219743,#219744,#219745),.UNSPECIFIED.,.F.,.F.,(4,3,3,3,
3,3,3,3,3,3,3,3,4),(0.,1.12535551671018E-5,7.76936938560993E-5,0.000102513517961127,
0.000121879189824273,0.000189659041345284,0.00022354896710579,0.000257294099096101,
0.000257438892866296,0.00032572085175287,0.000396486773949805,0.000466242707653759,
0.000514877785732592),.UNSPECIFIED.);
#4938=B_SPLINE_CURVE_WITH_KNOTS('',3,(#219753,#219754,#219755,#219756,#219757,
#219758,#219759,#219760,#219761,#219762,#219763,#219764,#219765,#219766,
#219767,#219768,#219769,#219770,#219771,#219772,#219773,#219774,#219775,
#219776,#219777,#219778,#219779,#219780,#219781,#219782,#219783,#219784,
#219785,#219786,#219787,#219788,#219789,#219790,#219791,#219792),
 .UNSPECIFIED.,.F.,.F.,(4,3,3,3,3,3,3,3,3,3,3,3,3,4),(0.,6.80370855373682E-5,
0.00013730316930006,0.000203636706665804,0.000256396220959704,0.000256540237295727,
0.000285209320207723,0.000342105100635644,0.000384776935956585,0.000400778874201938,
0.000456785658060672,0.00048478904999004,0.000498790745954723,0.000512792441919407),
 .UNSPECIFIED.);
#4939=B_SPLINE_CURVE_WITH_KNOTS('',3,(#219796,#219797,#219798,#219799,#219800,
#219801,#219802,#219803,#219804,#219805,#219806,#219807,#219808,#219809,
#219810,#219811,#219812,#219813,#219814,#219815,#219816,#219817,#219818,
#219819,#219820,#219821,#219822,#219823,#219824,#219825,#219826,#219827,
#219828,#219829,#219830,#219831,#219832),.UNSPECIFIED.,.F.,.F.,(4,3,3,3,
3,3,3,3,3,3,3,3,4),(0.,1.12535551670959E-5,7.7693693848883E-5,0.000102513517961114,
0.000121879189824263,0.000189659041345284,0.000223548967105795,0.000257294099096117,
0.000257438892866305,0.000325720851755243,0.000396486773954683,0.000466242707661072,
0.00051487778573261),.UNSPECIFIED.);
#4940=B_SPLINE_CURVE_WITH_KNOTS('',3,(#219840,#219841,#219842,#219843,#219844,
#219845,#219846,#219847,#219848,#219849,#219850,#219851,#219852,#219853,
#219854,#219855,#219856,#219857,#219858,#219859,#219860,#219861,#219862,
#219863,#219864,#219865,#219866,#219867,#219868,#219869,#219870,#219871,
#219872,#219873,#219874,#219875,#219876,#219877,#219878,#219879),
 .UNSPECIFIED.,.F.,.F.,(4,3,3,3,3,3,3,3,3,3,3,3,3,4),(0.,6.80370855356864E-5,
0.000137303169296884,0.000203636706661411,0.000256396220959704,0.00025654023729573,
0.00028520932020772,0.000342105100635642,0.000384776935956584,0.000400778874201937,
0.000456785658060672,0.00048478904999004,0.000498790745954724,0.000512792441919408),
 .UNSPECIFIED.);
#4941=B_SPLINE_CURVE_WITH_KNOTS('',3,(#219883,#219884,#219885,#219886,#219887,
#219888,#219889,#219890,#219891,#219892,#219893,#219894,#219895,#219896,
#219897,#219898,#219899,#219900,#219901,#219902,#219903,#219904,#219905,
#219906,#219907,#219908,#219909,#219910,#219911,#219912,#219913,#219914,
#219915,#219916,#219917,#219918,#219919),.UNSPECIFIED.,.F.,.F.,(4,3,3,3,
3,3,3,3,3,3,3,3,4),(0.,1.12535551670985E-5,7.76936938457793E-5,0.000102513517961143,
0.000121879189824288,0.000189659041345298,0.000223548967105802,0.0002572940990961,
0.000257438892866307,0.000325720851758952,0.000396486773962268,0.00046624270767231,
0.000514877785732614),.UNSPECIFIED.);
#4942=B_SPLINE_CURVE_WITH_KNOTS('',3,(#219927,#219928,#219929,#219930,#219931,
#219932,#219933,#219934,#219935,#219936,#219937,#219938,#219939,#219940,
#219941,#219942,#219943,#219944,#219945,#219946,#219947,#219948,#219949,
#219950,#219951,#219952,#219953,#219954,#219955,#219956,#219957,#219958,
#219959,#219960,#219961,#219962,#219963,#219964,#219965,#219966),
 .UNSPECIFIED.,.F.,.F.,(4,3,3,3,3,3,3,3,3,3,3,3,3,4),(0.,6.80370855404787E-5,
0.000137303169306344,0.000203636706674795,0.000256396220959704,0.000256540237295735,
0.000285209320207736,0.000342105100635654,0.000384776935956593,0.000400778874201945,
0.000456785658060677,0.000484789049990043,0.000498790745954726,0.000512792441919409),
 .UNSPECIFIED.);
#4943=B_SPLINE_CURVE_WITH_KNOTS('',3,(#219970,#219971,#219972,#219973,#219974,
#219975,#219976,#219977,#219978,#219979,#219980,#219981,#219982,#219983,
#219984,#219985,#219986,#219987,#219988,#219989,#219990,#219991,#219992,
#219993,#219994,#219995,#219996,#219997,#219998,#219999,#220000,#220001,
#220002,#220003,#220004,#220005,#220006),.UNSPECIFIED.,.F.,.F.,(4,3,3,3,
3,3,3,3,3,3,3,3,4),(0.,1.12535551670986E-5,7.76936938445697E-5,0.000102513517961116,
0.000121879189824264,0.000189659041345283,0.000223548967105793,0.00025729409909611,
0.000257438892866302,0.000325720851758691,0.000396486773961759,0.000466242707671471,
0.000514877785732605),.UNSPECIFIED.);
#4944=B_SPLINE_CURVE_WITH_KNOTS('',3,(#220013,#220014,#220015,#220016,#220017,
#220018,#220019,#220020,#220021,#220022,#220023,#220024,#220025,#220026,
#220027,#220028,#220029,#220030,#220031,#220032,#220033,#220034,#220035,
#220036,#220037,#220038,#220039,#220040,#220041,#220042,#220043,#220044,
#220045,#220046,#220047,#220048,#220049,#220050,#220051,#220052),
 .UNSPECIFIED.,.F.,.F.,(4,3,3,3,3,3,3,3,3,3,3,3,3,4),(0.,6.80370855342381E-5,
0.000137303169293626,0.000203636706655953,0.000256396220959707,0.00025654023729573,
0.000285209320207736,0.000342105100635655,0.000384776935956595,0.000400778874201947,
0.00045678565806068,0.000484789049990047,0.00049879074595473,0.000512792441919414),
 .UNSPECIFIED.);
#4945=B_SPLINE_CURVE_WITH_KNOTS('',3,(#220054,#220055,#220056,#220057,#220058,
#220059,#220060,#220061,#220062,#220063,#220064,#220065,#220066,#220067,
#220068,#220069,#220070,#220071,#220072,#220073,#220074,#220075,#220076,
#220077,#220078,#220079,#220080,#220081,#220082,#220083,#220084,#220085,
#220086,#220087,#220088,#220089,#220090),.UNSPECIFIED.,.F.,.F.,(4,3,3,3,
3,3,3,3,3,3,3,3,4),(0.,1.12535551671018E-5,7.76936938435877E-5,0.000102513517961135,
0.000121879189824281,0.000189659041345292,0.000223548967105798,0.000257294099096097,
0.000257438892866303,0.000325720851759153,0.000396486773962767,0.000466242707673162,
0.000514877785732606),.UNSPECIFIED.);
#4946=B_SPLINE_CURVE_WITH_KNOTS('',3,(#220098,#220099,#220100,#220101,#220102,
#220103,#220104,#220105,#220106,#220107,#220108,#220109,#220110,#220111,
#220112,#220113,#220114,#220115,#220116,#220117,#220118,#220119,#220120,
#220121,#220122,#220123,#220124,#220125,#220126,#220127,#220128,#220129,
#220130,#220131,#220132,#220133,#220134,#220135,#220136,#220137),
 .UNSPECIFIED.,.F.,.F.,(4,3,3,3,3,3,3,3,3,3,3,3,3,4),(0.,6.80370855408103E-5,
0.000137303169307113,0.000203636706676278,0.000256396220959706,0.000256540237295737,
0.00028520932020774,0.000342105100635658,0.000384776935956596,0.000400778874201948,
0.00045678565806068,0.000484789049990046,0.000498790745954729,0.000512792441919412),
 .UNSPECIFIED.);
#4947=B_SPLINE_CURVE_WITH_KNOTS('',3,(#220141,#220142,#220143,#220144,#220145,
#220146,#220147,#220148,#220149,#220150,#220151,#220152,#220153,#220154,
#220155,#220156,#220157,#220158,#220159,#220160,#220161,#220162,#220163,
#220164,#220165,#220166,#220167,#220168,#220169,#220170,#220171,#220172,
#220173,#220174,#220175,#220176,#220177),.UNSPECIFIED.,.F.,.F.,(4,3,3,3,
3,3,3,3,3,3,3,3,4),(0.,1.12535551670972E-5,7.76936938468974E-5,0.000102513517961115,
0.000121879189824263,0.000189659041345284,0.000223548967105794,0.000257294099096101,
0.000257438892866304,0.000325720851754898,0.000396486773954035,0.000466242707660405,
0.000514877785732608),.UNSPECIFIED.);
#4948=B_SPLINE_CURVE_WITH_KNOTS('',3,(#220185,#220186,#220187,#220188,#220189,
#220190,#220191,#220192,#220193,#220194,#220195,#220196,#220197,#220198,
#220199,#220200,#220201,#220202,#220203,#220204,#220205,#220206,#220207,
#220208,#220209,#220210,#220211,#220212,#220213,#220214,#220215,#220216,
#220217,#220218,#220219,#220220,#220221,#220222,#220223,#220224),
 .UNSPECIFIED.,.F.,.F.,(4,3,3,3,3,3,3,3,3,3,3,3,3,4),(0.,6.80370855378567E-5,
0.000137303169300862,0.000203636706666544,0.000256396220959703,0.000256540237295736,
0.000285209320207733,0.000342105100635651,0.00038477693595659,0.000400778874201942,
0.000456785658060673,0.000484789049990039,0.000498790745954722,0.000512792441919405),
 .UNSPECIFIED.);
#4949=B_SPLINE_CURVE_WITH_KNOTS('',3,(#220228,#220229,#220230,#220231,#220232,
#220233,#220234,#220235,#220236,#220237,#220238,#220239,#220240,#220241,
#220242,#220243,#220244,#220245,#220246,#220247,#220248,#220249,#220250,
#220251,#220252,#220253,#220254,#220255,#220256,#220257,#220258,#220259,
#220260,#220261,#220262,#220263,#220264),.UNSPECIFIED.,.F.,.F.,(4,3,3,3,
3,3,3,3,3,3,3,3,4),(0.,1.12535551670993E-5,7.76936938400127E-5,0.00010251351796113,
0.000121879189824277,0.000189659041345292,0.000223548967105799,0.000257294099096103,
0.000257438892866306,0.000325720851756268,0.000396486773956665,0.000466242707663886,
0.000514877785732613),.UNSPECIFIED.);
#4950=B_SPLINE_CURVE_WITH_KNOTS('',3,(#220272,#220273,#220274,#220275,#220276,
#220277,#220278,#220279,#220280,#220281,#220282,#220283,#220284,#220285,
#220286,#220287,#220288,#220289,#220290,#220291,#220292,#220293,#220294,
#220295,#220296,#220297,#220298,#220299,#220300,#220301,#220302,#220303,
#220304,#220305,#220306,#220307,#220308,#220309,#220310,#220311),
 .UNSPECIFIED.,.F.,.F.,(4,3,3,3,3,3,3,3,3,3,3,3,3,4),(0.,6.80370855365677E-5,
0.000137303169297886,0.000203636706661229,0.000256396220959701,0.000256540237295728,
0.00028520932020773,0.000342105100635649,0.000384776935956587,0.000400778874201939,
0.000456785658060671,0.000484789049990037,0.00049879074595472,0.000512792441919403),
 .UNSPECIFIED.);
#4951=B_SPLINE_CURVE_WITH_KNOTS('',3,(#220315,#220316,#220317,#220318,#220319,
#220320,#220321,#220322,#220323,#220324,#220325,#220326,#220327,#220328,
#220329,#220330,#220331,#220332,#220333,#220334,#220335,#220336,#220337,
#220338,#220339,#220340,#220341,#220342,#220343,#220344,#220345,#220346,
#220347,#220348,#220349,#220350,#220351),.UNSPECIFIED.,.F.,.F.,(4,3,3,3,
3,3,3,3,3,3,3,3,4),(0.,1.12535551670979E-5,7.76936938450434E-5,0.000102513517961105,
0.000121879189824256,0.000189659041345283,0.000223548967105797,0.00025729409909611,
0.000257438892866311,0.000325720851755806,0.000396486773955716,0.000466242707662355,
0.000514877785732622),.UNSPECIFIED.);
#4952=B_SPLINE_CURVE_WITH_KNOTS('',3,(#220359,#220360,#220361,#220362,#220363,
#220364,#220365,#220366,#220367,#220368,#220369,#220370,#220371,#220372,
#220373,#220374,#220375,#220376,#220377,#220378,#220379,#220380,#220381,
#220382,#220383,#220384,#220385,#220386,#220387,#220388,#220389,#220390,
#220391,#220392,#220393,#220394,#220395,#220396,#220397,#220398),
 .UNSPECIFIED.,.F.,.F.,(4,3,3,3,3,3,3,3,3,3,3,3,3,4),(0.,6.80370855353079E-5,
0.000137303169296173,0.000203636706660593,0.0002563962209597,0.000256540237295731,
0.000285209320207733,0.000342105100635649,0.000384776935956587,0.000400778874201939,
0.000456785658060669,0.000484789049990034,0.000498790745954717,0.0005127924419194),
 .UNSPECIFIED.);
#4953=B_SPLINE_CURVE_WITH_KNOTS('',3,(#220402,#220403,#220404,#220405,#220406,
#220407,#220408,#220409,#220410,#220411,#220412,#220413,#220414,#220415,
#220416,#220417,#220418,#220419,#220420,#220421,#220422,#220423,#220424,
#220425,#220426,#220427,#220428,#220429,#220430,#220431,#220432,#220433,
#220434,#220435,#220436,#220437,#220438),.UNSPECIFIED.,.F.,.F.,(4,3,3,3,
3,3,3,3,3,3,3,3,4),(0.,1.12535551670958E-5,7.76936938484934E-5,0.0001025135179611,
0.000121879189824251,0.000189659041345279,0.000223548967105793,0.000257294099096104,
0.000257438892866307,0.00032572085176472,0.000396486773974065,0.000466242707689337,
0.000514877785732614),.UNSPECIFIED.);
#4954=B_SPLINE_CURVE_WITH_KNOTS('',3,(#220446,#220447,#220448,#220449,#220450,
#220451,#220452,#220453,#220454,#220455,#220456,#220457,#220458,#220459,
#220460,#220461,#220462,#220463,#220464,#220465,#220466,#220467,#220468,
#220469,#220470,#220471,#220472,#220473,#220474,#220475,#220476,#220477,
#220478,#220479,#220480,#220481,#220482,#220483,#220484,#220485),
 .UNSPECIFIED.,.F.,.F.,(4,3,3,3,3,3,3,3,3,3,3,3,3,4),(0.,6.80370855370149E-5,
0.000137303169299152,0.00020363670666395,0.000256396220959702,0.000256540237295726,
0.000285209320207733,0.000342105100635651,0.000384776935956589,0.000400778874201941,
0.000456785658060673,0.000484789049990039,0.000498790745954722,0.000512792441919404),
 .UNSPECIFIED.);
#4955=B_SPLINE_CURVE_WITH_KNOTS('',3,(#220489,#220490,#220491,#220492,#220493,
#220494,#220495,#220496,#220497,#220498,#220499,#220500,#220501,#220502,
#220503,#220504,#220505,#220506,#220507,#220508,#220509,#220510,#220511,
#220512,#220513,#220514,#220515,#220516,#220517,#220518,#220519,#220520,
#220521,#220522,#220523,#220524,#220525),.UNSPECIFIED.,.F.,.F.,(4,3,3,3,
3,3,3,3,3,3,3,3,4),(0.,1.12535551670976E-5,7.76936938539417E-5,0.000102513517961119,
0.000121879189824268,0.000189659041345289,0.0002235489671058,0.000257294099096114,
0.00025743889286631,0.000325720851758913,0.000396486773961676,0.000466242707670145,
0.000514877785732621),.UNSPECIFIED.);
#4956=B_SPLINE_CURVE_WITH_KNOTS('',3,(#220533,#220534,#220535,#220536,#220537,
#220538,#220539,#220540,#220541,#220542,#220543,#220544,#220545,#220546,
#220547,#220548,#220549,#220550,#220551,#220552,#220553,#220554,#220555,
#220556,#220557,#220558,#220559,#220560,#220561,#220562,#220563,#220564,
#220565,#220566,#220567,#220568,#220569,#220570,#220571,#220572),
 .UNSPECIFIED.,.F.,.F.,(4,3,3,3,3,3,3,3,3,3,3,3,3,4),(0.,6.80370855405262E-5,
0.000137303169306291,0.000203636706674482,0.000256396220959699,0.000256540237295709,
0.000285209320207743,0.000342105100635657,0.000384776935956592,0.000400778874201943,
0.00045678565806067,0.000484789049990034,0.000498790745954716,0.000512792441919397),
 .UNSPECIFIED.);
#4957=B_SPLINE_CURVE_WITH_KNOTS('',3,(#220576,#220577,#220578,#220579,#220580,
#220581,#220582,#220583,#220584,#220585,#220586,#220587,#220588,#220589,
#220590,#220591,#220592,#220593,#220594,#220595,#220596,#220597,#220598,
#220599,#220600,#220601,#220602,#220603,#220604,#220605,#220606,#220607,
#220608,#220609,#220610,#220611,#220612),.UNSPECIFIED.,.F.,.F.,(4,3,3,3,
3,3,3,3,3,3,3,3,4),(0.,1.12535551670982E-5,7.7693693851138E-5,0.000102513517961117,
0.000121879189824266,0.000189659041345289,0.0002235489671058,0.000257294099096116,
0.000257438892866312,0.000325720851754073,0.000396486773952516,0.000466242707658386,
0.000514877785732623),.UNSPECIFIED.);
#4958=B_SPLINE_CURVE_WITH_KNOTS('',3,(#220620,#220621,#220622,#220623,#220624,
#220625,#220626,#220627,#220628,#220629,#220630,#220631,#220632,#220633,
#220634,#220635,#220636,#220637,#220638,#220639,#220640,#220641,#220642,
#220643,#220644,#220645,#220646,#220647,#220648,#220649,#220650,#220651,
#220652,#220653,#220654,#220655,#220656,#220657,#220658,#220659),
 .UNSPECIFIED.,.F.,.F.,(4,3,3,3,3,3,3,3,3,3,3,3,3,4),(0.,6.80370855406125E-5,
0.000137303169307245,0.000203636706678069,0.000256396220959702,0.000256540237295741,
0.000285209320207742,0.000342105100635658,0.000384776935956594,0.000400778874201945,
0.000456785658060675,0.000484789049990039,0.000498790745954721,0.000512792441919404),
 .UNSPECIFIED.);
#4959=B_SPLINE_CURVE_WITH_KNOTS('',3,(#220663,#220664,#220665,#220666,#220667,
#220668,#220669,#220670,#220671,#220672,#220673,#220674,#220675,#220676,
#220677,#220678,#220679,#220680,#220681,#220682,#220683,#220684,#220685,
#220686,#220687,#220688,#220689,#220690,#220691,#220692,#220693,#220694,
#220695,#220696,#220697,#220698,#220699),.UNSPECIFIED.,.F.,.F.,(4,3,3,3,
3,3,3,3,3,3,3,3,4),(0.,1.12535551670976E-5,7.76936938533714E-5,0.000102513517961116,
0.000121879189824266,0.000189659041345289,0.000223548967105801,0.000257294099096104,
0.000257438892866313,0.000325720851754926,0.000396486773953946,0.000466242707659578,
0.000514877785732626),.UNSPECIFIED.);
#4960=B_SPLINE_CURVE_WITH_KNOTS('',3,(#220707,#220708,#220709,#220710,#220711,
#220712,#220713,#220714,#220715,#220716,#220717,#220718,#220719,#220720,
#220721,#220722,#220723,#220724,#220725,#220726,#220727,#220728,#220729,
#220730,#220731,#220732,#220733,#220734,#220735,#220736,#220737,#220738,
#220739,#220740,#220741,#220742,#220743,#220744,#220745,#220746),
 .UNSPECIFIED.,.F.,.F.,(4,3,3,3,3,3,3,3,3,3,3,3,3,4),(0.,6.80370855376524E-5,
0.000137303169300624,0.000203636706666611,0.000256396220959709,0.000256540237295741,
0.000285209320207731,0.000342105100635653,0.000384776935956595,0.000400778874201948,
0.000456785658060683,0.000484789049990051,0.000498790745954735,0.000512792441919419),
 .UNSPECIFIED.);
#4961=B_SPLINE_CURVE_WITH_KNOTS('',3,(#220750,#220751,#220752,#220753,#220754,
#220755,#220756,#220757,#220758,#220759,#220760,#220761,#220762,#220763,
#220764,#220765,#220766,#220767,#220768,#220769,#220770,#220771,#220772,
#220773,#220774,#220775,#220776,#220777,#220778,#220779,#220780,#220781,
#220782,#220783,#220784,#220785,#220786),.UNSPECIFIED.,.F.,.F.,(4,3,3,3,
3,3,3,3,3,3,3,3,4),(0.,1.12535551671015E-5,7.76936938364543E-5,0.000102513517961143,
0.000121879189824288,0.000189659041345293,0.000223548967105796,0.000257294099096091,
0.000257438892866299,0.000325720851761098,0.000396486773965608,0.000466242707675163,
0.000514877785732598),.UNSPECIFIED.);
#4962=B_SPLINE_CURVE_WITH_KNOTS('',3,(#220794,#220795,#220796,#220797,#220798,
#220799,#220800,#220801,#220802,#220803,#220804,#220805,#220806,#220807,
#220808,#220809,#220810,#220811,#220812,#220813,#220814,#220815,#220816,
#220817,#220818,#220819,#220820,#220821,#220822,#220823,#220824,#220825,
#220826,#220827,#220828,#220829,#220830,#220831,#220832,#220833),
 .UNSPECIFIED.,.F.,.F.,(4,3,3,3,3,3,3,3,3,3,3,3,3,4),(0.,6.80370855383874E-5,
0.000137303169301691,0.000203636706667116,0.000256396220959699,0.000256540237295735,
0.000285209320207737,0.000342105100635652,0.000384776935956589,0.00040077887420194,
0.000456785658060669,0.000484789049990033,0.000498790745954715,0.000512792441919398),
 .UNSPECIFIED.);
#4963=B_SPLINE_CURVE_WITH_KNOTS('',3,(#220837,#220838,#220839,#220840,#220841,
#220842,#220843,#220844,#220845,#220846,#220847,#220848,#220849,#220850,
#220851,#220852,#220853,#220854,#220855,#220856,#220857,#220858,#220859,
#220860,#220861,#220862,#220863,#220864,#220865,#220866,#220867,#220868,
#220869,#220870,#220871,#220872,#220873),.UNSPECIFIED.,.F.,.F.,(4,3,3,3,
3,3,3,3,3,3,3,3,4),(0.,1.1253555167099E-5,7.76936938505077E-5,0.000102513517961127,
0.000121879189824275,0.000189659041345293,0.000223548967105801,0.000257294099096114,
0.00025743889286631,0.000325720851755436,0.000396486773954861,0.00046624270766092,
0.000514877785732621),.UNSPECIFIED.);
#4964=B_SPLINE_CURVE_WITH_KNOTS('',3,(#220881,#220882,#220883,#220884,#220885,
#220886,#220887,#220888,#220889,#220890,#220891,#220892,#220893,#220894,
#220895,#220896,#220897,#220898,#220899,#220900,#220901,#220902,#220903,
#220904,#220905,#220906,#220907,#220908,#220909,#220910,#220911,#220912,
#220913,#220914,#220915,#220916,#220917,#220918,#220919,#220920),
 .UNSPECIFIED.,.F.,.F.,(4,3,3,3,3,3,3,3,3,3,3,3,3,4),(0.,6.80370855367628E-5,
0.000137303169298667,0.000203636706663435,0.000256396220959711,0.000256540237295747,
0.000285209320207732,0.000342105100635654,0.000384776935956596,0.000400778874201949,
0.000456785658060685,0.000484789049990053,0.000498790745954737,0.000512792441919421),
 .UNSPECIFIED.);
#4965=B_SPLINE_CURVE_WITH_KNOTS('',3,(#220924,#220925,#220926,#220927,#220928,
#220929,#220930,#220931,#220932,#220933,#220934,#220935,#220936,#220937,
#220938,#220939,#220940,#220941,#220942,#220943,#220944,#220945,#220946,
#220947,#220948,#220949,#220950,#220951,#220952,#220953,#220954,#220955,
#220956,#220957,#220958,#220959,#220960),.UNSPECIFIED.,.F.,.F.,(4,3,3,3,
3,3,3,3,3,3,3,3,4),(0.,1.12535551671004E-5,7.76936938370177E-5,0.000102513517961122,
0.00012187918982427,0.000189659041345288,0.000223548967105797,0.000257294099096105,
0.000257438892866306,0.000325720851761926,0.000396486773968017,0.000466242707679974,
0.000514877785732611),.UNSPECIFIED.);
#4966=B_SPLINE_CURVE_WITH_KNOTS('',3,(#220968,#220969,#220970,#220971,#220972,
#220973,#220974,#220975,#220976,#220977,#220978,#220979,#220980,#220981,
#220982,#220983,#220984,#220985,#220986,#220987,#220988,#220989,#220990,
#220991,#220992,#220993,#220994,#220995,#220996,#220997,#220998,#220999,
#221000,#221001,#221002,#221003,#221004,#221005,#221006,#221007),
 .UNSPECIFIED.,.F.,.F.,(4,3,3,3,3,3,3,3,3,3,3,3,3,4),(0.,6.80370855368759E-5,
0.000137303169298515,0.000203636706662323,0.000256396220959706,0.000256540237295727,
0.000285209320207712,0.000342105100635637,0.000384776935956581,0.000400778874201935,
0.000456785658060674,0.000484789049990043,0.000498790745954728,0.000512792441919413),
 .UNSPECIFIED.);
#4967=B_SPLINE_CURVE_WITH_KNOTS('',3,(#221011,#221012,#221013,#221014,#221015,
#221016,#221017,#221018,#221019,#221020,#221021,#221022,#221023,#221024,
#221025,#221026,#221027,#221028,#221029,#221030,#221031,#221032,#221033,
#221034,#221035,#221036,#221037,#221038,#221039,#221040,#221041,#221042,
#221043,#221044,#221045,#221046,#221047),.UNSPECIFIED.,.F.,.F.,(4,3,3,3,
3,3,3,3,3,3,3,3,4),(0.,1.12535551670969E-5,7.76936938444744E-5,0.000102513517961099,
0.000121879189824249,0.000189659041345277,0.00022354896710579,0.000257294099096095,
0.000257438892866304,0.000325720851753951,0.000396486773952143,0.000466242707657648,
0.000514877785732608),.UNSPECIFIED.);
#4968=B_SPLINE_CURVE_WITH_KNOTS('',3,(#221055,#221056,#221057,#221058,#221059,
#221060,#221061,#221062,#221063,#221064,#221065,#221066,#221067,#221068,
#221069,#221070,#221071,#221072,#221073,#221074,#221075,#221076,#221077,
#221078,#221079,#221080,#221081,#221082,#221083,#221084,#221085,#221086,
#221087,#221088,#221089,#221090,#221091,#221092,#221093,#221094),
 .UNSPECIFIED.,.F.,.F.,(4,3,3,3,3,3,3,3,3,3,3,3,3,4),(0.,6.80370855430361E-5,
0.000137303169311202,0.000203636706681394,0.000256396220959711,0.000256540237295744,
0.000285209320207742,0.000342105100635662,0.000384776935956602,0.000400778874201954,
0.000456785658060688,0.000484789049990054,0.000498790745954738,0.000512792441919421),
 .UNSPECIFIED.);
#4969=B_SPLINE_CURVE_WITH_KNOTS('',3,(#221098,#221099,#221100,#221101,#221102,
#221103,#221104,#221105,#221106,#221107,#221108,#221109,#221110,#221111,
#221112,#221113,#221114,#221115,#221116,#221117,#221118,#221119,#221120,
#221121,#221122,#221123,#221124,#221125,#221126,#221127,#221128,#221129,
#221130,#221131,#221132,#221133,#221134),.UNSPECIFIED.,.F.,.F.,(4,3,3,3,
3,3,3,3,3,3,3,3,4),(0.,1.12535551670993E-5,7.76936938391851E-5,0.000102513517961135,
0.000121879189824282,0.000189659041345295,0.000223548967105801,0.000257294099096109,
0.000257438892866308,0.000325720851757329,0.000396486773959131,0.000466242707668275,
0.000514877785732615),.UNSPECIFIED.);
#4970=B_SPLINE_CURVE_WITH_KNOTS('',3,(#221142,#221143,#221144,#221145,#221146,
#221147,#221148,#221149,#221150,#221151,#221152,#221153,#221154,#221155,
#221156,#221157,#221158,#221159,#221160,#221161,#221162,#221163,#221164,
#221165,#221166,#221167,#221168,#221169,#221170,#221171,#221172,#221173,
#221174,#221175,#221176,#221177,#221178,#221179,#221180,#221181),
 .UNSPECIFIED.,.F.,.F.,(4,3,3,3,3,3,3,3,3,3,3,3,3,4),(0.,6.80370855362148E-5,
0.000137303169297774,0.000203636706662515,0.000256396220959708,0.000256540237295738,
0.000285209320207736,0.000342105100635656,0.000384776935956596,0.000400778874201949,
0.000456785658060683,0.00048478904999005,0.000498790745954733,0.000512792441919417),
 .UNSPECIFIED.);
#4971=B_SPLINE_CURVE_WITH_KNOTS('',3,(#221185,#221186,#221187,#221188,#221189,
#221190,#221191,#221192,#221193,#221194,#221195,#221196,#221197,#221198,
#221199,#221200,#221201,#221202,#221203,#221204,#221205,#221206,#221207,
#221208,#221209,#221210,#221211,#221212,#221213,#221214,#221215,#221216,
#221217,#221218,#221219,#221220,#221221),.UNSPECIFIED.,.F.,.F.,(4,3,3,3,
3,3,3,3,3,3,3,3,4),(0.,1.12535551670964E-5,7.76936938562025E-5,0.0001025135179611,
0.00012187918982425,0.000189659041345276,0.000223548967105789,0.000257294099096091,
0.000257438892866302,0.00032572085175626,0.000396486773956917,0.000466242707664596,
0.000514877785732604),.UNSPECIFIED.);
#4972=B_SPLINE_CURVE_WITH_KNOTS('',3,(#221229,#221230,#221231,#221232,#221233,
#221234,#221235,#221236,#221237,#221238,#221239,#221240,#221241,#221242,
#221243,#221244,#221245,#221246,#221247,#221248,#221249,#221250,#221251,
#221252,#221253,#221254,#221255,#221256,#221257,#221258,#221259,#221260,
#221261,#221262,#221263,#221264,#221265,#221266,#221267,#221268),
 .UNSPECIFIED.,.F.,.F.,(4,3,3,3,3,3,3,3,3,3,3,3,3,4),(0.,6.80370855342904E-5,
0.000137303169293723,0.000203636706656155,0.000256396220959708,0.000256540237295735,
0.000285209320207743,0.000342105100635661,0.0003847769359566,0.000400778874201952,
0.000456785658060683,0.000484789049990049,0.000498790745954732,0.000512792441919415),
 .UNSPECIFIED.);
#4973=B_SPLINE_CURVE_WITH_KNOTS('',3,(#221272,#221273,#221274,#221275,#221276,
#221277,#221278,#221279,#221280,#221281,#221282,#221283,#221284,#221285,
#221286,#221287,#221288,#221289,#221290,#221291,#221292,#221293,#221294,
#221295,#221296,#221297,#221298,#221299,#221300,#221301,#221302,#221303,
#221304,#221305,#221306,#221307,#221308),.UNSPECIFIED.,.F.,.F.,(4,3,3,3,
3,3,3,3,3,3,3,3,4),(0.,1.12535551670994E-5,7.76936938473578E-5,0.000102513517961135,
0.000121879189824281,0.000189659041345291,0.000223548967105796,0.000257294099096098,
0.000257438892866302,0.000325720851756026,0.000396486773956574,0.000466242707664513,
0.000514877785732603),.UNSPECIFIED.);
#4974=B_SPLINE_CURVE_WITH_KNOTS('',3,(#221315,#221316,#221317,#221318,#221319,
#221320,#221321,#221322,#221323,#221324,#221325,#221326,#221327,#221328,
#221329,#221330,#221331,#221332,#221333,#221334,#221335,#221336,#221337,
#221338,#221339,#221340,#221341,#221342,#221343,#221344,#221345,#221346,
#221347,#221348,#221349,#221350,#221351,#221352,#221353,#221354),
 .UNSPECIFIED.,.F.,.F.,(4,3,3,3,3,3,3,3,3,3,3,3,3,4),(0.,6.80370855359559E-5,
0.000137303169297146,0.000203636706661351,0.000256396220959708,0.000256540237295741,
0.000285209320207738,0.000342105100635657,0.000384776935956596,0.000400778874201949,
0.000456785658060682,0.000484789049990049,0.000498790745954732,0.000512792441919415),
 .UNSPECIFIED.);
#4975=B_SPLINE_CURVE_WITH_KNOTS('',3,(#224968,#224969,#224970,#224971,#224972,
#224973,#224974,#224975,#224976,#224977,#224978,#224979,#224980,#224981,
#224982,#224983,#224984,#224985,#224986,#224987,#224988,#224989,#224990,
#224991,#224992,#224993,#224994,#224995,#224996,#224997,#224998,#224999,
#225000,#225001,#225002,#225003,#225004,#225005,#225006,#225007,#225008,
#225009,#225010,#225011,#225012,#225013,#225014,#225015,#225016,#225017,
#225018,#225019),.UNSPECIFIED.,.F.,.F.,(4,3,3,3,3,3,3,3,3,3,3,3,3,3,3,3,
3,4),(0.,4.30706237870626E-5,8.47417087698098E-5,0.000124159989205863,0.000160467076290102,
0.000170998382116694,0.000182414994733773,0.000213747977645868,0.000242415955903168,
0.000256497573175041,0.000259169422895615,0.00026175777731242,0.00028996513040335,
0.000301877270772904,0.000321937017503146,0.000326951954185707,0.000334474359209548,
0.000341996764233388),.UNSPECIFIED.);
#4976=B_SPLINE_CURVE_WITH_KNOTS('',3,(#225020,#225021,#225022,#225023,#225024,
#225025,#225026,#225027,#225028,#225029,#225030,#225031,#225032,#225033,
#225034,#225035,#225036,#225037,#225038,#225039,#225040,#225041,#225042,
#225043,#225044,#225045,#225046,#225047,#225048,#225049,#225050,#225051,
#225052,#225053,#225054,#225055,#225056,#225057,#225058,#225059,#225060,
#225061,#225062,#225063,#225064,#225065,#225066,#225067,#225068,#225069,
#225070,#225071),.UNSPECIFIED.,.F.,.F.,(4,3,3,3,3,3,3,3,3,3,3,3,3,3,3,3,
3,4),(0.,2.58457451675679E-5,4.2539444619485E-5,6.46659869686642E-5,7.57292581432538E-5,
8.12608937305486E-5,8.26438026273723E-5,8.67925293178434E-5,0.000116015624426966,
0.000130188793976765,0.000151886926306226,0.00016196365121128,0.000162735992470956,
0.000173585058635687,0.000212487880461617,0.000255238173514508,0.000301397761155089,
0.000347170117271359),.UNSPECIFIED.);
#4977=B_SPLINE_CURVE_WITH_KNOTS('',3,(#225073,#225074,#225075,#225076,#225077,
#225078,#225079,#225080,#225081,#225082,#225083,#225084,#225085,#225086,
#225087,#225088,#225089,#225090,#225091,#225092,#225093,#225094,#225095,
#225096,#225097,#225098,#225099,#225100,#225101,#225102,#225103,#225104,
#225105,#225106,#225107,#225108,#225109,#225110,#225111,#225112,#225113,
#225114,#225115,#225116,#225117,#225118),.UNSPECIFIED.,.F.,.F.,(4,3,3,3,
3,3,3,3,3,3,3,3,3,3,3,4),(3.3881317890172E-21,2.57218161987639E-5,4.21568322569294E-5,
6.4587331461773E-5,7.58025810641948E-5,8.14102058654057E-5,8.28121120657085E-5,
8.70178306666167E-5,0.000116081955658157,0.000130526745999925,0.000162394111022045,
0.000174035661333233,0.000213138396957335,0.000256116935431967,0.000302406662853213,
0.000348071322666466),.UNSPECIFIED.);
#4978=B_SPLINE_CURVE_WITH_KNOTS('',3,(#225119,#225120,#225121,#225122,#225123,
#225124,#225125,#225126,#225127,#225128,#225129,#225130,#225131,#225132,
#225133,#225134,#225135,#225136,#225137,#225138,#225139,#225140,#225141,
#225142,#225143,#225144,#225145,#225146,#225147,#225148,#225149,#225150,
#225151,#225152,#225153,#225154,#225155,#225156,#225157,#225158,#225159,
#225160,#225161,#225162,#225163,#225164,#225165,#225166,#225167,#225168,
#225169,#225170),.UNSPECIFIED.,.F.,.F.,(4,3,3,3,3,3,3,3,3,3,3,3,3,3,3,3,
3,4),(0.,4.29652152146413E-5,8.44519107510641E-5,0.000123669830862078,0.000159788877354881,
0.000170558847912631,0.000181218775907171,0.000181960046452396,0.000214460062643458,
0.000244755726198141,0.000255838271868947,0.000258503253867582,0.000261084955178759,
0.000289370476647919,0.000301101325502011,0.000321109510663637,0.00033111360324445,
0.000341117695825263),.UNSPECIFIED.);
#4979=B_SPLINE_CURVE_WITH_KNOTS('',3,(#228853,#228854,#228855,#228856,#228857,
#228858,#228859,#228860,#228861,#228862,#228863,#228864,#228865,#228866,
#228867,#228868,#228869,#228870,#228871,#228872,#228873,#228874,#228875,
#228876,#228877,#228878,#228879,#228880,#228881,#228882,#228883,#228884,
#228885,#228886,#228887,#228888,#228889,#228890,#228891,#228892,#228893,
#228894,#228895,#228896,#228897,#228898,#228899,#228900,#228901,#228902,
#228903,#228904),.UNSPECIFIED.,.F.,.F.,(4,3,3,3,3,3,3,3,3,3,3,3,3,3,3,3,
3,4),(0.,4.30706237887532E-5,8.4741708772828E-5,0.000124159989210102,0.000160467076295626,
0.000170998382116695,0.000182414994733766,0.000213747977645869,0.000242415955903966,
0.000256497573175043,0.000259169422895616,0.000261757777312422,0.000289965130402892,
0.000301877270772906,0.000321937017503149,0.000326951954185709,0.00033447435920955,
0.000341996764233391),.UNSPECIFIED.);
#4980=B_SPLINE_CURVE_WITH_KNOTS('',3,(#228905,#228906,#228907,#228908,#228909,
#228910,#228911,#228912,#228913,#228914,#228915,#228916,#228917,#228918,
#228919,#228920,#228921,#228922,#228923,#228924,#228925,#228926,#228927,
#228928,#228929,#228930,#228931,#228932,#228933,#228934,#228935,#228936,
#228937,#228938,#228939,#228940,#228941,#228942,#228943,#228944,#228945,
#228946,#228947,#228948,#228949,#228950,#228951,#228952,#228953,#228954,
#228955,#228956),.UNSPECIFIED.,.F.,.F.,(4,3,3,3,3,3,3,3,3,3,3,3,3,3,3,3,
3,4),(8.67361737988404E-19,2.58457451673786E-5,4.25394446195963E-5,6.4665986968718E-5,
7.57292581432788E-5,8.12608937305592E-5,8.26438026273793E-5,8.67925293178396E-5,
0.000116015624426922,0.000130188793976759,0.000151886926306219,0.000161963651211269,
0.000162735992470948,0.000173585058635678,0.000212487880462208,0.000255238173514594,
0.000301397761152511,0.000347170117271357),.UNSPECIFIED.);
#4981=B_SPLINE_CURVE_WITH_KNOTS('',3,(#228958,#228959,#228960,#228961,#228962,
#228963,#228964,#228965,#228966,#228967,#228968,#228969,#228970,#228971,
#228972,#228973,#228974,#228975,#228976,#228977,#228978,#228979,#228980,
#228981,#228982,#228983,#228984,#228985,#228986,#228987,#228988,#228989,
#228990,#228991,#228992,#228993,#228994,#228995,#228996,#228997,#228998,
#228999,#229000,#229001,#229002,#229003),.UNSPECIFIED.,.F.,.F.,(4,3,3,3,
3,3,3,3,3,3,3,3,3,3,3,4),(0.,2.57218162000954E-5,4.21568322569208E-5,6.45873314617704E-5,
7.58025810641952E-5,8.14102058654076E-5,8.28121120657107E-5,8.701783066662E-5,
0.000116081955658867,0.000130526745999926,0.000162394111022053,0.000174035661333232,
0.000213138396959432,0.000256116935436117,0.000302406662859553,0.00034807132266647),
 .UNSPECIFIED.);
#4982=B_SPLINE_CURVE_WITH_KNOTS('',3,(#229004,#229005,#229006,#229007,#229008,
#229009,#229010,#229011,#229012,#229013,#229014,#229015,#229016,#229017,
#229018,#229019,#229020,#229021,#229022,#229023,#229024,#229025,#229026,
#229027,#229028,#229029,#229030,#229031,#229032,#229033,#229034,#229035,
#229036,#229037,#229038,#229039,#229040,#229041,#229042,#229043,#229044,
#229045,#229046,#229047,#229048,#229049,#229050,#229051,#229052,#229053,
#229054,#229055),.UNSPECIFIED.,.F.,.F.,(4,3,3,3,3,3,3,3,3,3,3,3,3,3,3,3,
3,4),(0.,4.29652152129061E-5,8.44519107484223E-5,0.000123669830859236,0.000159788877352066,
0.000170558847912624,0.000181218775907164,0.000181960046452401,0.000214460062644132,
0.000244755726200044,0.000255838271868943,0.000258503253867578,0.000261084955178755,
0.000289370476646873,0.000301101325502008,0.000321109510663635,0.000331113603244448,
0.000341117695825261),.UNSPECIFIED.);
#4983=B_SPLINE_CURVE_WITH_KNOTS('',3,(#229057,#229058,#229059,#229060,#229061,
#229062,#229063,#229064,#229065,#229066,#229067,#229068,#229069,#229070,
#229071,#229072,#229073,#229074,#229075,#229076,#229077,#229078,#229079,
#229080,#229081,#229082,#229083,#229084,#229085,#229086,#229087,#229088,
#229089,#229090,#229091,#229092,#229093,#229094,#229095,#229096,#229097,
#229098,#229099,#229100,#229101,#229102,#229103,#229104,#229105,#229106,
#229107,#229108),.UNSPECIFIED.,.F.,.F.,(4,3,3,3,3,3,3,3,3,3,3,3,3,3,3,3,
3,4),(0.,4.30706237867375E-5,8.47417087691522E-5,0.000124159989204823,0.00016046707628857,
0.000170998382116696,0.000182414994733785,0.000213747977645869,0.000242415955903806,
0.000256497573175043,0.000259169422895616,0.000261757777312422,0.000289965130402222,
0.000301877270772906,0.000321937017503148,0.000326951954185709,0.00033447435920955,
0.00034199676423339),.UNSPECIFIED.);
#4984=B_SPLINE_CURVE_WITH_KNOTS('',3,(#229109,#229110,#229111,#229112,#229113,
#229114,#229115,#229116,#229117,#229118,#229119,#229120,#229121,#229122,
#229123,#229124,#229125,#229126,#229127,#229128,#229129,#229130,#229131,
#229132,#229133,#229134,#229135,#229136,#229137,#229138,#229139,#229140,
#229141,#229142,#229143,#229144,#229145,#229146,#229147,#229148,#229149,
#229150,#229151,#229152,#229153,#229154,#229155,#229156,#229157,#229158,
#229159,#229160),.UNSPECIFIED.,.F.,.F.,(4,3,3,3,3,3,3,3,3,3,3,3,3,3,3,3,
3,4),(0.,2.58457451687563E-5,4.25394446196343E-5,6.46659869687391E-5,7.57292581432915E-5,
8.12608937305677E-5,8.26438026273867E-5,8.67925293178438E-5,0.000116015624427484,
0.000130188793976766,0.000151886926306227,0.000161963651211279,0.000162735992470957,
0.000173585058635688,0.000212487880458173,0.000255238173505986,0.000301397761137943,
0.000347170117271372),.UNSPECIFIED.);
#4985=B_SPLINE_CURVE_WITH_KNOTS('',3,(#229162,#229163,#229164,#229165,#229166,
#229167,#229168,#229169,#229170,#229171,#229172,#229173,#229174,#229175,
#229176,#229177,#229178,#229179,#229180,#229181,#229182,#229183,#229184,
#229185,#229186,#229187,#229188,#229189,#229190,#229191,#229192,#229193,
#229194,#229195,#229196,#229197,#229198,#229199,#229200,#229201,#229202,
#229203,#229204,#229205,#229206,#229207),.UNSPECIFIED.,.F.,.F.,(4,3,3,3,
3,3,3,3,3,3,3,3,3,3,3,4),(1.73472347597681E-18,2.57218161994071E-5,4.21568322567322E-5,
6.45873314616717E-5,7.58025810641414E-5,8.14102058653763E-5,8.2812112065685E-5,
8.70178306666112E-5,0.000116081955658581,0.000130526745999916,0.000162394111022036,
0.000174035661333221,0.000213138396957988,0.00025611693543334,0.000302406662855556,
0.000348071322666432),.UNSPECIFIED.);
#4986=B_SPLINE_CURVE_WITH_KNOTS('',3,(#229208,#229209,#229210,#229211,#229212,
#229213,#229214,#229215,#229216,#229217,#229218,#229219,#229220,#229221,
#229222,#229223,#229224,#229225,#229226,#229227,#229228,#229229,#229230,
#229231,#229232,#229233,#229234,#229235,#229236,#229237,#229238,#229239,
#229240,#229241,#229242,#229243,#229244,#229245,#229246,#229247,#229248,
#229249,#229250,#229251,#229252,#229253,#229254,#229255,#229256,#229257,
#229258,#229259),.UNSPECIFIED.,.F.,.F.,(4,3,3,3,3,3,3,3,3,3,3,3,3,3,3,3,
3,4),(0.,4.2965215217082E-5,8.44519107547709E-5,0.000123669830866139,0.00015978887735852,
0.000170558847912625,0.000181218775907164,0.00018196004645241,0.000214460062644103,
0.000244755726200267,0.000255838271868937,0.000258503253867572,0.000261084955178749,
0.000289370476647232,0.000301101325501999,0.000321109510663624,0.000331113603244437,
0.000341117695825249),.UNSPECIFIED.);
#4987=B_SPLINE_CURVE_WITH_KNOTS('',3,(#229261,#229262,#229263,#229264,#229265,
#229266,#229267,#229268,#229269,#229270,#229271,#229272,#229273,#229274,
#229275,#229276,#229277,#229278,#229279,#229280,#229281,#229282,#229283,
#229284,#229285,#229286,#229287,#229288,#229289,#229290,#229291,#229292,
#229293,#229294,#229295,#229296,#229297,#229298,#229299,#229300,#229301,
#229302,#229303,#229304,#229305,#229306,#229307,#229308,#229309,#229310,
#229311,#229312),.UNSPECIFIED.,.F.,.F.,(4,3,3,3,3,3,3,3,3,3,3,3,3,3,3,3,
3,4),(9.81307786677359E-18,4.30706237882728E-5,8.4741708772019E-5,0.000124159989209085,
0.000160467076294421,0.000170998382116706,0.000182414994733799,0.000213747977645876,
0.000242415955904087,0.000256497573175047,0.00025916942289562,0.000261757777312426,
0.000289965130402721,0.000301877270772907,0.000321937017503148,0.000326951954185708,
0.000334474359209548,0.000341996764233389),.UNSPECIFIED.);
#4988=B_SPLINE_CURVE_WITH_KNOTS('',3,(#229313,#229314,#229315,#229316,#229317,
#229318,#229319,#229320,#229321,#229322,#229323,#229324,#229325,#229326,
#229327,#229328,#229329,#229330,#229331,#229332,#229333,#229334,#229335,
#229336,#229337,#229338,#229339,#229340,#229341,#229342,#229343,#229344,
#229345,#229346,#229347,#229348,#229349,#229350,#229351,#229352,#229353,
#229354,#229355,#229356,#229357,#229358,#229359,#229360,#229361,#229362,
#229363,#229364),.UNSPECIFIED.,.F.,.F.,(4,3,3,3,3,3,3,3,3,3,3,3,3,3,3,3,
3,4),(0.,2.58457451680732E-5,4.25394446195484E-5,6.46659869686971E-5,7.57292581432714E-5,
8.12608937305585E-5,8.26438026273803E-5,8.67925293178457E-5,0.000116015624427878,
0.000130188793976769,0.00015188692630623,0.000161963651211275,0.000162735992470961,
0.000173585058635691,0.000212487880461201,0.000255238173511369,0.000301397761144767,
0.000347170117271375),.UNSPECIFIED.);
#4989=B_SPLINE_CURVE_WITH_KNOTS('',3,(#229366,#229367,#229368,#229369,#229370,
#229371,#229372,#229373,#229374,#229375,#229376,#229377,#229378,#229379,
#229380,#229381,#229382,#229383,#229384,#229385,#229386,#229387,#229388,
#229389,#229390,#229391,#229392,#229393,#229394,#229395,#229396,#229397,
#229398,#229399,#229400,#229401,#229402,#229403,#229404,#229405,#229406,
#229407,#229408,#229409,#229410,#229411),.UNSPECIFIED.,.F.,.F.,(4,3,3,3,
3,3,3,3,3,3,3,3,3,3,3,4),(0.,2.57218161998569E-5,4.21568322567428E-5,6.45873314616809E-5,
7.580258106415E-5,8.14102058653845E-5,8.28121120656931E-5,8.7017830666619E-5,
0.000116081955658763,0.000130526745999929,0.000162394111022056,0.000174035661333238,
0.000213138396959539,0.000256116935436271,0.000302406662859608,0.000348071322666466),
 .UNSPECIFIED.);
#4990=B_SPLINE_CURVE_WITH_KNOTS('',3,(#229412,#229413,#229414,#229415,#229416,
#229417,#229418,#229419,#229420,#229421,#229422,#229423,#229424,#229425,
#229426,#229427,#229428,#229429,#229430,#229431,#229432,#229433,#229434,
#229435,#229436,#229437,#229438,#229439,#229440,#229441,#229442,#229443,
#229444,#229445,#229446,#229447,#229448,#229449,#229450,#229451,#229452,
#229453,#229454,#229455,#229456,#229457,#229458,#229459,#229460,#229461,
#229462,#229463),.UNSPECIFIED.,.F.,.F.,(4,3,3,3,3,3,3,3,3,3,3,3,3,3,3,3,
3,4),(4.33680868994202E-19,4.29652152167429E-5,8.44519107544172E-5,0.00012366983086611,
0.000159788877359186,0.000170558847912624,0.000181218775907164,0.000181960046452399,
0.000214460062644025,0.000244755726199709,0.000255838271868944,0.000258503253867579,
0.000261084955178756,0.000289370476647272,0.00030110132550201,0.000321109510663636,
0.00033111360324445,0.000341117695825263),.UNSPECIFIED.);
#4991=B_SPLINE_CURVE_WITH_KNOTS('',3,(#229465,#229466,#229467,#229468,#229469,
#229470,#229471,#229472,#229473,#229474,#229475,#229476,#229477,#229478,
#229479,#229480,#229481,#229482,#229483,#229484,#229485,#229486,#229487,
#229488,#229489,#229490,#229491,#229492,#229493,#229494,#229495,#229496,
#229497,#229498,#229499,#229500,#229501,#229502,#229503,#229504,#229505,
#229506,#229507,#229508,#229509,#229510,#229511,#229512,#229513,#229514,
#229515,#229516),.UNSPECIFIED.,.F.,.F.,(4,3,3,3,3,3,3,3,3,3,3,3,3,3,3,3,
3,4),(0.,4.30706237880298E-5,8.47417087716239E-5,0.000124159989208614,0.000160467076293979,
0.000170998382116694,0.00018241499473377,0.000213747977645868,0.000242415955903985,
0.000256497573175042,0.000259169422895615,0.00026175777731242,0.00028996513040211,
0.000301877270772905,0.000321937017503147,0.000326951954185707,0.000334474359209548,
0.000341996764233389),.UNSPECIFIED.);
#4992=B_SPLINE_CURVE_WITH_KNOTS('',3,(#229517,#229518,#229519,#229520,#229521,
#229522,#229523,#229524,#229525,#229526,#229527,#229528,#229529,#229530,
#229531,#229532,#229533,#229534,#229535,#229536,#229537,#229538,#229539,
#229540,#229541,#229542,#229543,#229544,#229545,#229546,#229547,#229548,
#229549,#229550,#229551,#229552,#229553,#229554,#229555,#229556,#229557,
#229558,#229559,#229560,#229561,#229562,#229563,#229564,#229565,#229566,
#229567,#229568),.UNSPECIFIED.,.F.,.F.,(4,3,3,3,3,3,3,3,3,3,3,3,3,3,3,3,
3,4),(0.,2.58457451667647E-5,4.25394446195672E-5,6.46659869687037E-5,7.57292581432719E-5,
8.1260893730556E-5,8.2643802627377E-5,8.67925293178401E-5,0.000116015624426914,
0.00013018879397676,0.00015188692630622,0.000161963651211274,0.00016273599247095,
0.00017358505863568,0.000212487880460383,0.000255238173510125,0.000301397761143776,
0.000347170117271361),.UNSPECIFIED.);
#4993=B_SPLINE_CURVE_WITH_KNOTS('',3,(#229570,#229571,#229572,#229573,#229574,
#229575,#229576,#229577,#229578,#229579,#229580,#229581,#229582,#229583,
#229584,#229585,#229586,#229587,#229588,#229589,#229590,#229591,#229592,
#229593,#229594,#229595,#229596,#229597,#229598,#229599,#229600,#229601,
#229602,#229603,#229604,#229605,#229606,#229607,#229608,#229609,#229610,
#229611,#229612,#229613,#229614,#229615),.UNSPECIFIED.,.F.,.F.,(4,3,3,3,
3,3,3,3,3,3,3,3,3,3,3,4),(3.46944695195361E-18,2.57218161985872E-5,4.21568322569015E-5,
6.458733146176E-5,7.58025810641893E-5,8.14102058654039E-5,8.28121120657076E-5,
8.70178306666186E-5,0.000116081955658227,0.000130526745999926,0.000162394111022037,
0.000174035661333234,0.000213138396958737,0.000256116935434941,0.000302406662858469,
0.000348071322666472),.UNSPECIFIED.);
#4994=B_SPLINE_CURVE_WITH_KNOTS('',3,(#229616,#229617,#229618,#229619,#229620,
#229621,#229622,#229623,#229624,#229625,#229626,#229627,#229628,#229629,
#229630,#229631,#229632,#229633,#229634,#229635,#229636,#229637,#229638,
#229639,#229640,#229641,#229642,#229643,#229644,#229645,#229646,#229647,
#229648,#229649,#229650,#229651,#229652,#229653,#229654,#229655,#229656,
#229657,#229658,#229659,#229660,#229661,#229662,#229663,#229664,#229665,
#229666,#229667),.UNSPECIFIED.,.F.,.F.,(4,3,3,3,3,3,3,3,3,3,3,3,3,3,3,3,
3,4),(0.,4.29652152154219E-5,8.44519107522863E-5,0.000123669830863478,0.000159788877356216,
0.000170558847912624,0.000181218775907164,0.000181960046452393,0.000214460062643201,
0.000244755726197205,0.000255838271868943,0.000258503253867578,0.000261084955178756,
0.000289370476648893,0.00030110132550201,0.000321109510663636,0.00033111360324445,
0.000341117695825263),.UNSPECIFIED.);
#4995=B_SPLINE_CURVE_WITH_KNOTS('',3,(#229669,#229670,#229671,#229672,#229673,
#229674,#229675,#229676,#229677,#229678,#229679,#229680,#229681,#229682,
#229683,#229684,#229685,#229686,#229687,#229688,#229689,#229690,#229691,
#229692,#229693,#229694,#229695,#229696,#229697,#229698,#229699,#229700,
#229701,#229702,#229703,#229704,#229705,#229706,#229707,#229708,#229709,
#229710,#229711,#229712,#229713,#229714,#229715,#229716,#229717,#229718,
#229719,#229720),.UNSPECIFIED.,.F.,.F.,(4,3,3,3,3,3,3,3,3,3,3,3,3,3,3,3,
3,4),(0.,4.30706237873536E-5,8.47417087703233E-5,0.000124159989206582,0.000160467076290998,
0.000170998382116696,0.00018241499473377,0.000213747977645869,0.000242415955903727,
0.000256497573175043,0.000259169422895616,0.000261757777312422,0.000289965130402594,
0.000301877270772906,0.000321937017503148,0.000326951954185709,0.00033447435920955,
0.000341996764233391),.UNSPECIFIED.);
#4996=B_SPLINE_CURVE_WITH_KNOTS('',3,(#229721,#229722,#229723,#229724,#229725,
#229726,#229727,#229728,#229729,#229730,#229731,#229732,#229733,#229734,
#229735,#229736,#229737,#229738,#229739,#229740,#229741,#229742,#229743,
#229744,#229745,#229746,#229747,#229748,#229749,#229750,#229751,#229752,
#229753,#229754,#229755,#229756,#229757,#229758,#229759,#229760,#229761,
#229762,#229763,#229764,#229765,#229766,#229767,#229768,#229769,#229770,
#229771,#229772),.UNSPECIFIED.,.F.,.F.,(4,3,3,3,3,3,3,3,3,3,3,3,3,3,3,3,
3,4),(3.46944695195361E-18,2.58457451679116E-5,4.25394446195865E-5,6.46659869687166E-5,
7.57292581432817E-5,8.12608937305642E-5,8.26438026273848E-5,8.67925293178467E-5,
0.000116015624426944,0.000130188793976768,0.000151886926306229,0.00016196365121128,
0.00016273599247096,0.00017358505863569,0.000212487880461716,0.000255238173512545,
0.000301397761146856,0.000347170117271378),.UNSPECIFIED.);
#4997=B_SPLINE_CURVE_WITH_KNOTS('',3,(#229774,#229775,#229776,#229777,#229778,
#229779,#229780,#229781,#229782,#229783,#229784,#229785,#229786,#229787,
#229788,#229789,#229790,#229791,#229792,#229793,#229794,#229795,#229796,
#229797,#229798,#229799,#229800,#229801,#229802,#229803,#229804,#229805,
#229806,#229807,#229808,#229809,#229810,#229811,#229812,#229813,#229814,
#229815,#229816,#229817,#229818,#229819),.UNSPECIFIED.,.F.,.F.,(4,3,3,3,
3,3,3,3,3,3,3,3,3,3,3,4),(0.,2.5721816201399E-5,4.21568322568262E-5,6.45873314617204E-5,
7.58025810641675E-5,8.14102058653911E-5,8.28121120656969E-5,8.70178306666146E-5,
0.000116081955658794,0.000130526745999922,0.00016239411102205,0.000174035661333229,
0.000213138396959652,0.000256116935436567,0.000302406662860262,0.000348071322666458),
 .UNSPECIFIED.);
#4998=B_SPLINE_CURVE_WITH_KNOTS('',3,(#229820,#229821,#229822,#229823,#229824,
#229825,#229826,#229827,#229828,#229829,#229830,#229831,#229832,#229833,
#229834,#229835,#229836,#229837,#229838,#229839,#229840,#229841,#229842,
#229843,#229844,#229845,#229846,#229847,#229848,#229849,#229850,#229851,
#229852,#229853,#229854,#229855,#229856,#229857,#229858,#229859,#229860,
#229861,#229862,#229863,#229864,#229865,#229866,#229867,#229868,#229869,
#229870,#229871),.UNSPECIFIED.,.F.,.F.,(4,3,3,3,3,3,3,3,3,3,3,3,3,3,3,3,
3,4),(1.30104260698261E-18,4.29652152181542E-5,8.44519107567955E-5,0.000123669830869214,
0.000159788877362927,0.000170558847912638,0.000181218775907177,0.000181960046452419,
0.000214460062643728,0.000244755726198606,0.000255838271868948,0.000258503253867583,
0.00026108495517876,0.000289370476648016,0.000301101325502009,0.000321109510663634,
0.000331113603244446,0.000341117695825258),.UNSPECIFIED.);
#4999=B_SPLINE_CURVE_WITH_KNOTS('',3,(#229873,#229874,#229875,#229876,#229877,
#229878,#229879,#229880,#229881,#229882,#229883,#229884,#229885,#229886,
#229887,#229888,#229889,#229890,#229891,#229892,#229893,#229894,#229895,
#229896,#229897,#229898,#229899,#229900,#229901,#229902,#229903,#229904,
#229905,#229906,#229907,#229908,#229909,#229910,#229911,#229912,#229913,
#229914,#229915,#229916,#229917,#229918,#229919,#229920,#229921,#229922,
#229923,#229924),.UNSPECIFIED.,.F.,.F.,(4,3,3,3,3,3,3,3,3,3,3,3,3,3,3,3,
3,4),(1.25393031850254E-17,4.30706237863908E-5,8.47417087685059E-5,0.000124159989203962,
0.000160467076287454,0.000170998382116688,0.000182414994733768,0.000213747977645861,
0.000242415955902704,0.000256497573175034,0.000259169422895607,0.000261757777312413,
0.000289965130403529,0.000301877270772897,0.000321937017503139,0.000326951954185699,
0.00033447435920954,0.000341996764233381),.UNSPECIFIED.);
#5000=B_SPLINE_CURVE_WITH_KNOTS('',3,(#229925,#229926,#229927,#229928,#229929,
#229930,#229931,#229932,#229933,#229934,#229935,#229936,#229937,#229938,
#229939,#229940,#229941,#229942,#229943,#229944,#229945,#229946,#229947,
#229948,#229949,#229950,#229951,#229952,#229953,#229954,#229955,#229956,
#229957,#229958,#229959,#229960,#229961,#229962,#229963,#229964,#229965,
#229966,#229967,#229968,#229969,#229970,#229971,#229972,#229973,#229974,
#229975,#229976),.UNSPECIFIED.,.F.,.F.,(4,3,3,3,3,3,3,3,3,3,3,3,3,3,3,3,
3,4),(0.,2.58457451685014E-5,4.2539444619537E-5,6.4665986968689E-5,7.57292581432651E-5,
8.12608937305531E-5,8.26438026273751E-5,8.67925293178411E-5,0.000116015624427711,
0.000130188793976762,0.000151886926306222,0.000161963651211274,0.000162735992470952,
0.000173585058635682,0.000212487880459268,0.000255238173508192,0.000301397761141237,
0.000347170117271364),.UNSPECIFIED.);
#5001=B_SPLINE_CURVE_WITH_KNOTS('',3,(#229978,#229979,#229980,#229981,#229982,
#229983,#229984,#229985,#229986,#229987,#229988,#229989,#229990,#229991,
#229992,#229993,#229994,#229995,#229996,#229997,#229998,#229999,#230000,
#230001,#230002,#230003,#230004,#230005,#230006,#230007,#230008,#230009,
#230010,#230011,#230012,#230013,#230014,#230015,#230016,#230017,#230018,
#230019,#230020,#230021,#230022,#230023),.UNSPECIFIED.,.F.,.F.,(4,3,3,3,
3,3,3,3,3,3,3,3,3,3,3,4),(0.,2.5721816199478E-5,4.21568322567195E-5,6.45873314616702E-5,
7.58025810641455E-5,8.14102058653832E-5,8.28121120656926E-5,8.70178306666208E-5,
0.000116081955658429,0.000130526745999931,0.000162394111022058,0.000174035661333242,
0.000213138396959934,0.000256116935437069,0.000302406662860884,0.000348071322666478),
 .UNSPECIFIED.);
#5002=B_SPLINE_CURVE_WITH_KNOTS('',3,(#230024,#230025,#230026,#230027,#230028,
#230029,#230030,#230031,#230032,#230033,#230034,#230035,#230036,#230037,
#230038,#230039,#230040,#230041,#230042,#230043,#230044,#230045,#230046,
#230047,#230048,#230049,#230050,#230051,#230052,#230053,#230054,#230055,
#230056,#230057,#230058,#230059,#230060,#230061,#230062,#230063,#230064,
#230065,#230066,#230067,#230068,#230069,#230070,#230071,#230072,#230073,
#230074,#230075),.UNSPECIFIED.,.F.,.F.,(4,3,3,3,3,3,3,3,3,3,3,3,3,3,3,3,
3,4),(1.73472347597681E-18,4.29652152148517E-5,8.44519107515775E-5,0.000123669830863035,
0.000159788877356324,0.000170558847912634,0.000181218775907174,0.000181960046452412,
0.000214460062643518,0.000244755726197894,0.000255838271868951,0.000258503253867585,
0.000261084955178763,0.000289370476647261,0.000301101325502015,0.000321109510663641,
0.000331113603244454,0.000341117695825267),.UNSPECIFIED.);
#5003=B_SPLINE_CURVE_WITH_KNOTS('',3,(#230077,#230078,#230079,#230080,#230081,
#230082,#230083,#230084,#230085,#230086,#230087,#230088,#230089,#230090,
#230091,#230092,#230093,#230094,#230095,#230096,#230097,#230098,#230099,
#230100,#230101,#230102,#230103,#230104,#230105,#230106,#230107,#230108,
#230109,#230110,#230111,#230112,#230113,#230114,#230115,#230116,#230117,
#230118,#230119,#230120,#230121,#230122,#230123,#230124,#230125,#230126,
#230127,#230128),.UNSPECIFIED.,.F.,.F.,(4,3,3,3,3,3,3,3,3,3,3,3,3,3,3,3,
3,4),(0.,4.30706237876963E-5,8.47417087710402E-5,0.000124159989207774,0.000160467076292755,
0.000170998382116703,0.000182414994733789,0.000213747977645875,0.000242415955903658,
0.000256497573175047,0.00025916942289562,0.000261757777312425,0.0002899651304043,
0.000301877270772908,0.000321937017503149,0.000326951954185709,0.00033447435920955,
0.00034199676423339),.UNSPECIFIED.);
#5004=B_SPLINE_CURVE_WITH_KNOTS('',3,(#230129,#230130,#230131,#230132,#230133,
#230134,#230135,#230136,#230137,#230138,#230139,#230140,#230141,#230142,
#230143,#230144,#230145,#230146,#230147,#230148,#230149,#230150,#230151,
#230152,#230153,#230154,#230155,#230156,#230157,#230158,#230159,#230160,
#230161,#230162,#230163,#230164,#230165,#230166,#230167,#230168,#230169,
#230170,#230171,#230172,#230173,#230174,#230175,#230176,#230177,#230178,
#230179,#230180),.UNSPECIFIED.,.F.,.F.,(4,3,3,3,3,3,3,3,3,3,3,3,3,3,3,3,
3,4),(0.,2.58457451675268E-5,4.2539444619566E-5,6.46659869687072E-5,7.57292581432777E-5,
8.1260893730563E-5,8.26438026273844E-5,8.67925293178483E-5,0.000116015624427071,
0.000130188793976773,0.000151886926306235,0.000161963651211294,0.000162735992470966,
0.000173585058635697,0.000212487880460834,0.000255238173511205,0.000301397761145922,
0.000347170117271376),.UNSPECIFIED.);
#5005=B_SPLINE_CURVE_WITH_KNOTS('',3,(#230182,#230183,#230184,#230185,#230186,
#230187,#230188,#230189,#230190,#230191,#230192,#230193,#230194,#230195,
#230196,#230197,#230198,#230199,#230200,#230201,#230202,#230203,#230204,
#230205,#230206,#230207,#230208,#230209,#230210,#230211,#230212,#230213,
#230214,#230215,#230216,#230217,#230218,#230219,#230220,#230221,#230222,
#230223,#230224,#230225,#230226,#230227),.UNSPECIFIED.,.F.,.F.,(4,3,3,3,
3,3,3,3,3,3,3,3,3,3,3,4),(0.,2.57218161991606E-5,4.21568322569619E-5,6.45873314617843E-5,
7.58025810641956E-5,8.14102058654012E-5,8.28121120657026E-5,8.70178306666068E-5,
0.000116081955658637,0.00013052674599991,0.000162394111022018,0.000174035661333214,
0.000213138396962703,0.00025611693544274,0.000302406662870117,0.000348071322666447),
 .UNSPECIFIED.);
#5006=B_SPLINE_CURVE_WITH_KNOTS('',3,(#230228,#230229,#230230,#230231,#230232,
#230233,#230234,#230235,#230236,#230237,#230238,#230239,#230240,#230241,
#230242,#230243,#230244,#230245,#230246,#230247,#230248,#230249,#230250,
#230251,#230252,#230253,#230254,#230255,#230256,#230257,#230258,#230259,
#230260,#230261,#230262,#230263,#230264,#230265,#230266,#230267,#230268,
#230269,#230270,#230271,#230272,#230273,#230274,#230275,#230276,#230277,
#230278,#230279),.UNSPECIFIED.,.F.,.F.,(4,3,3,3,3,3,3,3,3,3,3,3,3,3,3,3,
3,4),(1.30104260698261E-18,4.2965215217907E-5,8.44519107568489E-5,0.000123669830870173,
0.000159788877365401,0.000170558847912636,0.000181218775907176,0.000181960046452404,
0.000214460062644115,0.000244755726199935,0.000255838271868953,0.000258503253867588,
0.000261084955178766,0.000289370476646324,0.000301101325502018,0.000321109510663644,
0.000331113603244457,0.00034111769582527),.UNSPECIFIED.);
#5007=B_SPLINE_CURVE_WITH_KNOTS('',3,(#230281,#230282,#230283,#230284,#230285,
#230286,#230287,#230288,#230289,#230290,#230291,#230292,#230293,#230294,
#230295,#230296,#230297,#230298,#230299,#230300,#230301,#230302,#230303,
#230304,#230305,#230306,#230307,#230308,#230309,#230310,#230311,#230312,
#230313,#230314,#230315,#230316,#230317,#230318,#230319,#230320,#230321,
#230322,#230323,#230324,#230325,#230326,#230327,#230328,#230329,#230330,
#230331,#230332),.UNSPECIFIED.,.F.,.F.,(4,3,3,3,3,3,3,3,3,3,3,3,3,3,3,3,
3,4),(0.,4.30706237876165E-5,8.47417087707063E-5,0.000124159989206986,0.000160467076291406,
0.000170998382116689,0.000182414994733778,0.000213747977645862,0.000242415955902294,
0.000256497573175035,0.000259169422895608,0.000261757777312413,0.000289965130403309,
0.000301877270772897,0.000321937017503139,0.000326951954185699,0.00033447435920954,
0.000341996764233381),.UNSPECIFIED.);
#5008=B_SPLINE_CURVE_WITH_KNOTS('',3,(#230333,#230334,#230335,#230336,#230337,
#230338,#230339,#230340,#230341,#230342,#230343,#230344,#230345,#230346,
#230347,#230348,#230349,#230350,#230351,#230352,#230353,#230354,#230355,
#230356,#230357,#230358,#230359,#230360,#230361,#230362,#230363,#230364,
#230365,#230366,#230367,#230368,#230369,#230370,#230371,#230372,#230373,
#230374,#230375,#230376,#230377,#230378,#230379,#230380,#230381,#230382,
#230383,#230384),.UNSPECIFIED.,.F.,.F.,(4,3,3,3,3,3,3,3,3,3,3,3,3,3,3,3,
3,4),(0.,2.58457451683339E-5,4.25394446195427E-5,6.46659869686937E-5,7.57292581432692E-5,
8.12608937305569E-5,8.26438026273789E-5,8.67925293178447E-5,0.000116015624427496,
0.000130188793976767,0.000151886926306228,0.000161963651211283,0.000162735992470959,
0.000173585058635689,0.000212487880461562,0.000255238173512928,0.000301397761149189,
0.000347170117271379),.UNSPECIFIED.);
#5009=B_SPLINE_CURVE_WITH_KNOTS('',3,(#230386,#230387,#230388,#230389,#230390,
#230391,#230392,#230393,#230394,#230395,#230396,#230397,#230398,#230399,
#230400,#230401,#230402,#230403,#230404,#230405,#230406,#230407,#230408,
#230409,#230410,#230411,#230412,#230413,#230414,#230415,#230416,#230417,
#230418,#230419,#230420,#230421,#230422,#230423,#230424,#230425,#230426,
#230427,#230428,#230429,#230430,#230431),.UNSPECIFIED.,.F.,.F.,(4,3,3,3,
3,3,3,3,3,3,3,3,3,3,3,4),(0.,2.57218161995344E-5,4.21568322568466E-5,6.45873314617301E-5,
7.58025810641718E-5,8.14102058653927E-5,8.28121120656979E-5,8.70178306666136E-5,
0.000116081955657677,0.00013052674599992,0.000162394111022036,0.000174035661333227,
0.000213138396957751,0.000256116935432942,0.000302406662855227,0.000348071322666453),
 .UNSPECIFIED.);
#5010=B_SPLINE_CURVE_WITH_KNOTS('',3,(#230432,#230433,#230434,#230435,#230436,
#230437,#230438,#230439,#230440,#230441,#230442,#230443,#230444,#230445,
#230446,#230447,#230448,#230449,#230450,#230451,#230452,#230453,#230454,
#230455,#230456,#230457,#230458,#230459,#230460,#230461,#230462,#230463,
#230464,#230465,#230466,#230467,#230468,#230469,#230470,#230471,#230472,
#230473,#230474,#230475,#230476,#230477,#230478,#230479,#230480,#230481,
#230482,#230483),.UNSPECIFIED.,.F.,.F.,(4,3,3,3,3,3,3,3,3,3,3,3,3,3,3,3,
3,4),(0.,4.29652152186797E-5,8.44519107576635E-5,0.000123669830870363,0.000159788877364213,
0.000170558847912623,0.000181218775907163,0.000181960046452394,0.00021446006264392,
0.000244755726199048,0.000255838271868943,0.000258503253867578,0.000261084955178756,
0.000289370476647024,0.00030110132550201,0.000321109510663637,0.00033111360324445,
0.000341117695825264),.UNSPECIFIED.);
#5011=B_SPLINE_CURVE_WITH_KNOTS('',3,(#230485,#230486,#230487,#230488,#230489,
#230490,#230491,#230492,#230493,#230494,#230495,#230496,#230497,#230498,
#230499,#230500,#230501,#230502,#230503,#230504,#230505,#230506,#230507,
#230508,#230509,#230510,#230511,#230512,#230513,#230514,#230515,#230516,
#230517,#230518,#230519,#230520,#230521,#230522,#230523,#230524,#230525,
#230526,#230527,#230528,#230529,#230530,#230531,#230532,#230533,#230534,
#230535,#230536),.UNSPECIFIED.,.F.,.F.,(4,3,3,3,3,3,3,3,3,3,3,3,3,3,3,3,
3,4),(8.67361737988404E-19,4.30706237860763E-5,8.47417087680201E-5,0.000124159989203277,
0.000160467076286602,0.00017099838211669,0.000182414994733777,0.000213747977645865,
0.00024241595590321,0.00025649757317504,0.000259169422895614,0.000261757777312419,
0.000289965130402967,0.000301877270772905,0.000321937017503148,0.000326951954185708,
0.000334474359209549,0.00034199676423339),.UNSPECIFIED.);
#5012=B_SPLINE_CURVE_WITH_KNOTS('',3,(#230537,#230538,#230539,#230540,#230541,
#230542,#230543,#230544,#230545,#230546,#230547,#230548,#230549,#230550,
#230551,#230552,#230553,#230554,#230555,#230556,#230557,#230558,#230559,
#230560,#230561,#230562,#230563,#230564,#230565,#230566,#230567,#230568,
#230569,#230570,#230571,#230572,#230573,#230574,#230575,#230576,#230577,
#230578,#230579,#230580,#230581,#230582,#230583,#230584,#230585,#230586,
#230587,#230588),.UNSPECIFIED.,.F.,.F.,(4,3,3,3,3,3,3,3,3,3,3,3,3,3,3,3,
3,4),(6.93889390390723E-18,2.58457451701831E-5,4.25394446195401E-5,6.46659869686908E-5,
7.57292581432661E-5,8.12608937305538E-5,8.26438026273757E-5,8.67925293178415E-5,
0.000116015624427578,0.000130188793976759,0.000151886926306217,0.000161963651211268,
0.000162735992470947,0.000173585058635676,0.000212487880458399,0.000255238173505916,
0.000301397761136468,0.000347170117271362),.UNSPECIFIED.);
#5013=B_SPLINE_CURVE_WITH_KNOTS('',3,(#230590,#230591,#230592,#230593,#230594,
#230595,#230596,#230597,#230598,#230599,#230600,#230601,#230602,#230603,
#230604,#230605,#230606,#230607,#230608,#230609,#230610,#230611,#230612,
#230613,#230614,#230615,#230616,#230617,#230618,#230619,#230620,#230621,
#230622,#230623,#230624,#230625,#230626,#230627,#230628,#230629,#230630,
#230631,#230632,#230633,#230634,#230635),.UNSPECIFIED.,.F.,.F.,(4,3,3,3,
3,3,3,3,3,3,3,3,3,3,3,4),(6.93889390390723E-18,2.57218161998122E-5,4.21568322568062E-5,
6.45873314617115E-5,7.58025810641641E-5,8.14102058653904E-5,8.2812112065697E-5,
8.70178306666167E-5,0.000116081955658388,0.000130526745999922,0.000162394111022033,
0.000174035661333226,0.000213138396956944,0.000256116935431236,0.000302406662852219,
0.000348071322666445),.UNSPECIFIED.);
#5014=B_SPLINE_CURVE_WITH_KNOTS('',3,(#230636,#230637,#230638,#230639,#230640,
#230641,#230642,#230643,#230644,#230645,#230646,#230647,#230648,#230649,
#230650,#230651,#230652,#230653,#230654,#230655,#230656,#230657,#230658,
#230659,#230660,#230661,#230662,#230663,#230664,#230665,#230666,#230667,
#230668,#230669,#230670,#230671,#230672,#230673,#230674,#230675,#230676,
#230677,#230678,#230679,#230680,#230681,#230682,#230683,#230684,#230685,
#230686,#230687),.UNSPECIFIED.,.F.,.F.,(4,3,3,3,3,3,3,3,3,3,3,3,3,3,3,3,
3,4),(0.,4.29652152192065E-5,8.44519107585664E-5,0.000123669830871595,0.000159788877365913,
0.000170558847912624,0.000181218775907164,0.000181960046452394,0.000214460062644216,
0.000244755726200167,0.000255838271868943,0.000258503253867578,0.000261084955178756,
0.000289370476646725,0.000301101325502009,0.000321109510663636,0.000331113603244449,
0.000341117695825263),.UNSPECIFIED.);
#5015=B_SPLINE_CURVE_WITH_KNOTS('',3,(#230689,#230690,#230691,#230692,#230693,
#230694,#230695,#230696,#230697,#230698,#230699,#230700,#230701,#230702,
#230703,#230704,#230705,#230706,#230707,#230708,#230709,#230710,#230711,
#230712,#230713,#230714,#230715,#230716,#230717,#230718,#230719,#230720,
#230721,#230722,#230723,#230724,#230725,#230726,#230727,#230728,#230729,
#230730,#230731,#230732,#230733,#230734,#230735,#230736,#230737,#230738,
#230739,#230740),.UNSPECIFIED.,.F.,.F.,(4,3,3,3,3,3,3,3,3,3,3,3,3,3,3,3,
3,4),(0.,4.30706237839992E-5,8.47417087643213E-5,0.000124159989198158,0.000160467076279949,
0.000170998382116701,0.00018241499473378,0.000213747977645876,0.000242415955902872,
0.000256497573175051,0.000259169422895625,0.00026175777731243,0.000289965130403972,
0.000301877270772916,0.000321937017503159,0.00032695195418572,0.000334474359209561,
0.000341996764233402),.UNSPECIFIED.);
#5016=B_SPLINE_CURVE_WITH_KNOTS('',3,(#230741,#230742,#230743,#230744,#230745,
#230746,#230747,#230748,#230749,#230750,#230751,#230752,#230753,#230754,
#230755,#230756,#230757,#230758,#230759,#230760,#230761,#230762,#230763,
#230764,#230765,#230766,#230767,#230768,#230769,#230770,#230771,#230772,
#230773,#230774,#230775,#230776,#230777,#230778,#230779,#230780,#230781,
#230782,#230783,#230784,#230785,#230786,#230787,#230788,#230789,#230790,
#230791,#230792),.UNSPECIFIED.,.F.,.F.,(4,3,3,3,3,3,3,3,3,3,3,3,3,3,3,3,
3,4),(3.46944695195361E-18,2.58457451697252E-5,4.25394446195546E-5,6.46659869687025E-5,
7.57292581432765E-5,8.12608937305634E-5,8.26438026273852E-5,8.67925293178504E-5,
0.000116015624427319,0.000130188793976774,0.000151886926306236,0.000161963651211266,
0.000162735992470966,0.000173585058635697,0.000212487880459449,0.0002552381735094,
0.000301397761145159,0.000347170117271374),.UNSPECIFIED.);
#5017=B_SPLINE_CURVE_WITH_KNOTS('',3,(#230794,#230795,#230796,#230797,#230798,
#230799,#230800,#230801,#230802,#230803,#230804,#230805,#230806,#230807,
#230808,#230809,#230810,#230811,#230812,#230813,#230814,#230815,#230816,
#230817,#230818,#230819,#230820,#230821,#230822,#230823,#230824,#230825,
#230826,#230827,#230828,#230829,#230830,#230831,#230832,#230833,#230834,
#230835,#230836,#230837,#230838,#230839),.UNSPECIFIED.,.F.,.F.,(4,3,3,3,
3,3,3,3,3,3,3,3,3,3,3,4),(0.,2.57218161988346E-5,4.21568322566952E-5,6.45873314616517E-5,
7.580258106413E-5,8.14102058653691E-5,8.28121120656789E-5,8.70178306666082E-5,
0.000116081955657482,0.000130526745999912,0.000162394111022032,0.000174035661333216,
0.000213138396961443,0.000256116935440209,0.000302406662866123,0.000348071322666431),
 .UNSPECIFIED.);
#5018=B_SPLINE_CURVE_WITH_KNOTS('',3,(#230840,#230841,#230842,#230843,#230844,
#230845,#230846,#230847,#230848,#230849,#230850,#230851,#230852,#230853,
#230854,#230855,#230856,#230857,#230858,#230859,#230860,#230861,#230862,
#230863,#230864,#230865,#230866,#230867,#230868,#230869,#230870,#230871,
#230872,#230873,#230874,#230875,#230876,#230877,#230878,#230879,#230880,
#230881,#230882,#230883,#230884,#230885,#230886,#230887,#230888,#230889,
#230890,#230891),.UNSPECIFIED.,.F.,.F.,(4,3,3,3,3,3,3,3,3,3,3,3,3,3,3,3,
3,4),(1.30104260698261E-18,4.29652152148209E-5,8.44519107512452E-5,0.000123669830862091,
0.000159788877354504,0.000170558847912628,0.000181218775907167,0.000181960046452412,
0.000214460062643743,0.000244755726199073,0.00025583827186894,0.000258503253867575,
0.000261084955178753,0.000289370476647586,0.000301101325502003,0.000321109510663628,
0.00033111360324444,0.000341117695825253),.UNSPECIFIED.);
#5019=B_SPLINE_CURVE_WITH_KNOTS('',3,(#230893,#230894,#230895,#230896,#230897,
#230898,#230899,#230900,#230901,#230902,#230903,#230904,#230905,#230906,
#230907,#230908,#230909,#230910,#230911,#230912,#230913,#230914,#230915,
#230916,#230917,#230918,#230919,#230920,#230921,#230922,#230923,#230924,
#230925,#230926,#230927,#230928,#230929,#230930,#230931,#230932,#230933,
#230934,#230935,#230936,#230937,#230938,#230939,#230940,#230941,#230942,
#230943,#230944),.UNSPECIFIED.,.F.,.F.,(4,3,3,3,3,3,3,3,3,3,3,3,3,3,3,3,
3,4),(0.,4.30706237882036E-5,8.47417087719642E-5,0.000124159989209034,0.000160467076294394,
0.000170998382116691,0.00018241499473377,0.000213747977645865,0.000242415955902961,
0.00025649757317504,0.000259169422895613,0.000261757777312419,0.00028996513040394,
0.000301877270772904,0.000321937017503146,0.000326951954185707,0.000334474359209548,
0.000341996764233389),.UNSPECIFIED.);
#5020=B_SPLINE_CURVE_WITH_KNOTS('',3,(#230945,#230946,#230947,#230948,#230949,
#230950,#230951,#230952,#230953,#230954,#230955,#230956,#230957,#230958,
#230959,#230960,#230961,#230962,#230963,#230964,#230965,#230966,#230967,
#230968,#230969,#230970,#230971,#230972,#230973,#230974,#230975,#230976,
#230977,#230978,#230979,#230980,#230981,#230982,#230983,#230984,#230985,
#230986,#230987,#230988,#230989,#230990,#230991,#230992,#230993,#230994,
#230995,#230996),.UNSPECIFIED.,.F.,.F.,(4,3,3,3,3,3,3,3,3,3,3,3,3,3,3,3,
3,4),(3.46944695195361E-18,2.58457451678337E-5,4.25394446195919E-5,6.46659869687144E-5,
7.57292581432757E-5,8.12608937305563E-5,8.26438026273765E-5,8.67925293178369E-5,
0.000116015624427211,0.000130188793976754,0.000151886926306212,0.000161963651211262,
0.000162735992470941,0.00017358505863567,0.00021248788046187,0.000255238173513225,
0.000301397761148772,0.000347170117271356),.UNSPECIFIED.);
#5021=B_SPLINE_CURVE_WITH_KNOTS('',3,(#230998,#230999,#231000,#231001,#231002,
#231003,#231004,#231005,#231006,#231007,#231008,#231009,#231010,#231011,
#231012,#231013,#231014,#231015,#231016,#231017,#231018,#231019,#231020,
#231021,#231022,#231023,#231024,#231025,#231026,#231027,#231028,#231029,
#231030,#231031,#231032,#231033,#231034,#231035,#231036,#231037,#231038,
#231039,#231040,#231041,#231042,#231043),.UNSPECIFIED.,.F.,.F.,(4,3,3,3,
3,3,3,3,3,3,3,3,3,3,3,4),(0.,2.57218162018153E-5,4.21568322567147E-5,6.45873314616719E-5,
7.58025810641505E-5,8.14102058653898E-5,8.28121120656996E-5,8.70178306666291E-5,
0.000116081955659704,0.000130526745999944,0.000162394111022071,0.000174035661333258,
0.000213138396959943,0.0002561169354372,0.000302406662861553,0.000348071322666499),
 .UNSPECIFIED.);
#5022=B_SPLINE_CURVE_WITH_KNOTS('',3,(#231044,#231045,#231046,#231047,#231048,
#231049,#231050,#231051,#231052,#231053,#231054,#231055,#231056,#231057,
#231058,#231059,#231060,#231061,#231062,#231063,#231064,#231065,#231066,
#231067,#231068,#231069,#231070,#231071,#231072,#231073,#231074,#231075,
#231076,#231077,#231078,#231079,#231080,#231081,#231082,#231083,#231084,
#231085,#231086,#231087,#231088,#231089,#231090,#231091,#231092,#231093,
#231094,#231095),.UNSPECIFIED.,.F.,.F.,(4,3,3,3,3,3,3,3,3,3,3,3,3,3,3,3,
3,4),(8.67361737988404E-19,4.2965215210266E-5,8.44519107438952E-5,0.000123669830853,
0.000159788877344359,0.000170558847912642,0.000181218775907182,0.000181960046452411,
0.000214460062643778,0.000244755726198623,0.000255838271868959,0.000258503253867594,
0.000261084955178771,0.000289370476647211,0.000301101325502024,0.00032110951066365,
0.000331113603244463,0.000341117695825276),.UNSPECIFIED.);
#5023=B_SPLINE_CURVE_WITH_KNOTS('',3,(#231097,#231098,#231099,#231100,#231101,
#231102,#231103,#231104,#231105,#231106,#231107,#231108,#231109,#231110,
#231111,#231112,#231113,#231114,#231115,#231116,#231117,#231118,#231119,
#231120,#231121,#231122,#231123,#231124,#231125,#231126,#231127,#231128,
#231129,#231130,#231131,#231132,#231133,#231134,#231135,#231136,#231137,
#231138,#231139,#231140,#231141,#231142,#231143,#231144,#231145,#231146,
#231147,#231148),.UNSPECIFIED.,.F.,.F.,(4,3,3,3,3,3,3,3,3,3,3,3,3,3,3,3,
3,4),(0.,4.30706237851929E-5,8.47417087663985E-5,0.000124159989200908,0.000160467076283494,
0.000170998382116701,0.000182414994733797,0.000213747977645873,0.000242415955903371,
0.000256497573175046,0.00025916942289562,0.000261757777312425,0.000289965130403631,
0.000301877270772908,0.00032193701750315,0.000326951954185711,0.000334474359209551,
0.000341996764233392),.UNSPECIFIED.);
#5024=B_SPLINE_CURVE_WITH_KNOTS('',3,(#231149,#231150,#231151,#231152,#231153,
#231154,#231155,#231156,#231157,#231158,#231159,#231160,#231161,#231162,
#231163,#231164,#231165,#231166,#231167,#231168,#231169,#231170,#231171,
#231172,#231173,#231174,#231175,#231176,#231177,#231178,#231179,#231180,
#231181,#231182,#231183,#231184,#231185,#231186,#231187,#231188,#231189,
#231190,#231191,#231192,#231193,#231194,#231195,#231196,#231197,#231198,
#231199,#231200),.UNSPECIFIED.,.F.,.F.,(4,3,3,3,3,3,3,3,3,3,3,3,3,3,3,3,
3,4),(3.46944695195361E-18,2.58457451697524E-5,4.25394446195375E-5,6.46659869686935E-5,
7.57292581432715E-5,8.12608937305605E-5,8.26438026273827E-5,8.67925293178494E-5,
0.000116015624427668,0.000130188793976772,0.000151886926306234,0.000161963651211282,
0.000162735992470965,0.000173585058635695,0.000212487880458633,0.000255238173507009,
0.000301397761139473,0.000347170117271371),.UNSPECIFIED.);
#5025=B_SPLINE_CURVE_WITH_KNOTS('',3,(#231202,#231203,#231204,#231205,#231206,
#231207,#231208,#231209,#231210,#231211,#231212,#231213,#231214,#231215,
#231216,#231217,#231218,#231219,#231220,#231221,#231222,#231223,#231224,
#231225,#231226,#231227,#231228,#231229,#231230,#231231,#231232,#231233,
#231234,#231235,#231236,#231237,#231238,#231239,#231240,#231241,#231242,
#231243,#231244,#231245,#231246,#231247),.UNSPECIFIED.,.F.,.F.,(4,3,3,3,
3,3,3,3,3,3,3,3,3,3,3,4),(0.,2.57218161998829E-5,4.21568322568464E-5,6.45873314617307E-5,
7.58025810641729E-5,8.14102058653939E-5,8.28121120656992E-5,8.7017830666615E-5,
0.000116081955659212,0.000130526745999922,0.000162394111022053,0.00017403566133323,
0.000213138396958018,0.000256116935433331,0.000302406662855306,0.000348071322666447),
 .UNSPECIFIED.);
#5026=B_SPLINE_CURVE_WITH_KNOTS('',3,(#231248,#231249,#231250,#231251,#231252,
#231253,#231254,#231255,#231256,#231257,#231258,#231259,#231260,#231261,
#231262,#231263,#231264,#231265,#231266,#231267,#231268,#231269,#231270,
#231271,#231272,#231273,#231274,#231275,#231276,#231277,#231278,#231279,
#231280,#231281,#231282,#231283,#231284,#231285,#231286,#231287,#231288,
#231289,#231290,#231291,#231292,#231293,#231294,#231295,#231296,#231297,
#231298,#231299),.UNSPECIFIED.,.F.,.F.,(4,3,3,3,3,3,3,3,3,3,3,3,3,3,3,3,
3,4),(0.,4.29652152128983E-5,8.44519107483271E-5,0.000123669830858996,0.000159788877351773,
0.000170558847912631,0.00018121877590717,0.000181960046452391,0.000214460062644109,
0.000244755726200095,0.000255838271868941,0.000258503253867576,0.000261084955178753,
0.000289370476647502,0.000301101325502003,0.000321109510663627,0.000331113603244439,
0.000341117695825252),.UNSPECIFIED.);
#5027=B_SPLINE_CURVE_WITH_KNOTS('',3,(#231301,#231302,#231303,#231304,#231305,
#231306,#231307,#231308,#231309,#231310,#231311,#231312,#231313,#231314,
#231315,#231316,#231317,#231318,#231319,#231320,#231321,#231322,#231323,
#231324,#231325,#231326,#231327,#231328,#231329,#231330,#231331,#231332,
#231333,#231334,#231335,#231336,#231337,#231338,#231339,#231340,#231341,
#231342,#231343,#231344,#231345,#231346,#231347,#231348,#231349,#231350,
#231351,#231352),.UNSPECIFIED.,.F.,.F.,(4,3,3,3,3,3,3,3,3,3,3,3,3,3,3,3,
3,4),(0.,4.30706237880135E-5,8.4741708771494E-5,0.000124159989208263,0.000160467076293188,
0.000170998382116689,0.000182414994733767,0.000213747977645861,0.000242415955903085,
0.000256497573175034,0.000259169422895607,0.000261757777312412,0.000289965130403409,
0.000301877270772895,0.000321937017503137,0.000326951954185697,0.000334474359209537,
0.000341996764233378),.UNSPECIFIED.);
#5028=B_SPLINE_CURVE_WITH_KNOTS('',3,(#231353,#231354,#231355,#231356,#231357,
#231358,#231359,#231360,#231361,#231362,#231363,#231364,#231365,#231366,
#231367,#231368,#231369,#231370,#231371,#231372,#231373,#231374,#231375,
#231376,#231377,#231378,#231379,#231380,#231381,#231382,#231383,#231384,
#231385,#231386,#231387,#231388,#231389,#231390,#231391,#231392,#231393,
#231394,#231395,#231396,#231397,#231398,#231399,#231400,#231401,#231402,
#231403,#231404),.UNSPECIFIED.,.F.,.F.,(4,3,3,3,3,3,3,3,3,3,3,3,3,3,3,3,
3,4),(0.,2.5845745169089E-5,4.25394446195701E-5,6.46659869687081E-5,7.57292581432771E-5,
8.12608937305616E-5,8.26438026273827E-5,8.6792529317846E-5,0.000116015624427623,
0.000130188793976769,0.000151886926306231,0.00016196365121128,0.000162735992470961,
0.000173585058635692,0.000212487880461807,0.000255238173513942,0.000301397761151968,
0.000347170117271371),.UNSPECIFIED.);
#5029=B_SPLINE_CURVE_WITH_KNOTS('',3,(#231406,#231407,#231408,#231409,#231410,
#231411,#231412,#231413,#231414,#231415,#231416,#231417,#231418,#231419,
#231420,#231421,#231422,#231423,#231424,#231425,#231426,#231427,#231428,
#231429,#231430,#231431,#231432,#231433,#231434,#231435,#231436,#231437,
#231438,#231439,#231440,#231441,#231442,#231443,#231444,#231445,#231446,
#231447,#231448,#231449,#231450,#231451),.UNSPECIFIED.,.F.,.F.,(4,3,3,3,
3,3,3,3,3,3,3,3,3,3,3,4),(0.,2.5721816199856E-5,4.21568322568771E-5,6.45873314617458E-5,
7.58025810641801E-5,8.14102058653973E-5,8.28121120657016E-5,8.70178306666145E-5,
0.000116081955658527,0.000130526745999922,0.000162394111022043,0.000174035661333229,
0.00021313839695968,0.000256116935436711,0.000302406662860802,0.000348071322666442),
 .UNSPECIFIED.);
#5030=B_SPLINE_CURVE_WITH_KNOTS('',3,(#231452,#231453,#231454,#231455,#231456,
#231457,#231458,#231459,#231460,#231461,#231462,#231463,#231464,#231465,
#231466,#231467,#231468,#231469,#231470,#231471,#231472,#231473,#231474,
#231475,#231476,#231477,#231478,#231479,#231480,#231481,#231482,#231483,
#231484,#231485,#231486,#231487,#231488,#231489,#231490,#231491,#231492,
#231493,#231494,#231495,#231496,#231497,#231498,#231499,#231500,#231501,
#231502,#231503),.UNSPECIFIED.,.F.,.F.,(4,3,3,3,3,3,3,3,3,3,3,3,3,3,3,3,
3,4),(4.33680868994202E-19,4.29652152140341E-5,8.44519107501717E-5,0.000123669830861157,
0.000159788877354104,0.000170558847912632,0.000181218775907171,0.000181960046452407,
0.000214460062644171,0.000244755726200186,0.000255838271868944,0.000258503253867579,
0.000261084955178757,0.000289370476646964,0.000301101325502007,0.000321109510663632,
0.000331113603244444,0.000341117695825257),.UNSPECIFIED.);
#5031=B_SPLINE_CURVE_WITH_KNOTS('',3,(#231505,#231506,#231507,#231508,#231509,
#231510,#231511,#231512,#231513,#231514,#231515,#231516,#231517,#231518,
#231519,#231520,#231521,#231522,#231523,#231524,#231525,#231526,#231527,
#231528,#231529,#231530,#231531,#231532,#231533,#231534,#231535,#231536,
#231537,#231538,#231539,#231540,#231541,#231542,#231543,#231544,#231545,
#231546,#231547,#231548,#231549,#231550,#231551,#231552,#231553,#231554,
#231555,#231556),.UNSPECIFIED.,.F.,.F.,(4,3,3,3,3,3,3,3,3,3,3,3,3,3,3,3,
3,4),(0.,4.30706237871702E-5,8.47417087699776E-5,0.000124159989206078,0.000160467076290317,
0.000170998382116687,0.000182414994733769,0.000213747977645862,0.000242415955904907,
0.000256497573175036,0.00025916942289561,0.000261757777312415,0.000289965130402048,
0.000301877270772901,0.000321937017503143,0.000326951954185704,0.000334474359209545,
0.000341996764233386),.UNSPECIFIED.);
#5032=B_SPLINE_CURVE_WITH_KNOTS('',3,(#231557,#231558,#231559,#231560,#231561,
#231562,#231563,#231564,#231565,#231566,#231567,#231568,#231569,#231570,
#231571,#231572,#231573,#231574,#231575,#231576,#231577,#231578,#231579,
#231580,#231581,#231582,#231583,#231584,#231585,#231586,#231587,#231588,
#231589,#231590,#231591,#231592,#231593,#231594,#231595,#231596,#231597,
#231598,#231599,#231600,#231601,#231602,#231603,#231604,#231605,#231606,
#231607,#231608),.UNSPECIFIED.,.F.,.F.,(4,3,3,3,3,3,3,3,3,3,3,3,3,3,3,3,
3,4),(0.,2.58457451693448E-5,4.25394446196001E-5,6.46659869687223E-5,7.57292581432835E-5,
8.1260893730564E-5,8.26438026273842E-5,8.67925293178446E-5,0.000116015624427668,
0.000130188793976767,0.000151886926306228,0.000161963651211283,0.000162735992470959,
0.000173585058635689,0.00021248788045699,0.00025523817350245,0.000301397761129275,
0.000347170117271378),.UNSPECIFIED.);
#5033=B_SPLINE_CURVE_WITH_KNOTS('',3,(#231610,#231611,#231612,#231613,#231614,
#231615,#231616,#231617,#231618,#231619,#231620,#231621,#231622,#231623,
#231624,#231625,#231626,#231627,#231628,#231629,#231630,#231631,#231632,
#231633,#231634,#231635,#231636,#231637,#231638,#231639,#231640,#231641,
#231642,#231643,#231644,#231645,#231646,#231647,#231648,#231649,#231650,
#231651,#231652,#231653,#231654,#231655),.UNSPECIFIED.,.F.,.F.,(4,3,3,3,
3,3,3,3,3,3,3,3,3,3,3,4),(8.67361737988404E-19,2.57218162006469E-5,4.21568322567888E-5,
6.45873314617057E-5,7.58025810641642E-5,8.14102058653934E-5,8.28121120657007E-5,
8.70178306666226E-5,0.000116081955659052,0.000130526745999934,0.000162394111022055,
0.000174035661333244,0.000213138396957381,0.000256116935431866,0.000302406662852459,
0.000348071322666488),.UNSPECIFIED.);
#5034=B_SPLINE_CURVE_WITH_KNOTS('',3,(#231656,#231657,#231658,#231659,#231660,
#231661,#231662,#231663,#231664,#231665,#231666,#231667,#231668,#231669,
#231670,#231671,#231672,#231673,#231674,#231675,#231676,#231677,#231678,
#231679,#231680,#231681,#231682,#231683,#231684,#231685,#231686,#231687,
#231688,#231689,#231690,#231691,#231692,#231693,#231694,#231695,#231696,
#231697,#231698,#231699,#231700,#231701,#231702,#231703,#231704,#231705,
#231706,#231707),.UNSPECIFIED.,.F.,.F.,(4,3,3,3,3,3,3,3,3,3,3,3,3,3,3,3,
3,4),(0.,4.2965215222015E-5,8.44519107628343E-5,0.000123669830876255,0.000159788877370164,
0.000170558847912636,0.000181218775907176,0.000181960046452415,0.000214460062643924,
0.00024475572619964,0.000255838271868954,0.000258503253867589,0.000261084955178766,
0.000289370476647491,0.000301101325502019,0.000321109510663645,0.000331113603244458,
0.000341117695825272),.UNSPECIFIED.);
#5035=B_SPLINE_CURVE_WITH_KNOTS('',3,(#231709,#231710,#231711,#231712,#231713,
#231714,#231715,#231716,#231717,#231718,#231719,#231720,#231721,#231722,
#231723,#231724,#231725,#231726,#231727,#231728,#231729,#231730,#231731,
#231732,#231733,#231734,#231735,#231736,#231737,#231738,#231739,#231740,
#231741,#231742,#231743,#231744,#231745,#231746,#231747,#231748,#231749,
#231750,#231751,#231752,#231753,#231754,#231755,#231756,#231757,#231758,
#231759,#231760),.UNSPECIFIED.,.F.,.F.,(4,3,3,3,3,3,3,3,3,3,3,3,3,3,3,3,
3,4),(3.09377807083354E-18,4.30706237851843E-5,8.47417087666321E-5,0.000124159989201714,
0.00016046707628494,0.00017099838211668,0.000182414994733754,0.000213747977645856,
0.000242415955903085,0.000256497573175032,0.000259169422895605,0.000261757777312411,
0.000289965130403707,0.000301877270772897,0.000321937017503141,0.000326951954185701,
0.000334474359209543,0.000341996764233384),.UNSPECIFIED.);
#5036=B_SPLINE_CURVE_WITH_KNOTS('',3,(#231761,#231762,#231763,#231764,#231765,
#231766,#231767,#231768,#231769,#231770,#231771,#231772,#231773,#231774,
#231775,#231776,#231777,#231778,#231779,#231780,#231781,#231782,#231783,
#231784,#231785,#231786,#231787,#231788,#231789,#231790,#231791,#231792,
#231793,#231794,#231795,#231796,#231797,#231798,#231799,#231800,#231801,
#231802,#231803,#231804,#231805,#231806,#231807,#231808,#231809,#231810,
#231811,#231812),.UNSPECIFIED.,.F.,.F.,(4,3,3,3,3,3,3,3,3,3,3,3,3,3,3,3,
3,4),(2.76132740804902E-19,2.58457451684212E-5,4.25394446196281E-5,6.4665986968732E-5,
7.5729258143284E-5,8.126089373056E-5,8.2643802627379E-5,8.6792529317836E-5,
0.000116015624427268,0.000130188793976754,0.000151886926306213,0.000161963651211274,
0.000162735992470942,0.000173585058635672,0.000212487880460351,0.00025523817351116,
0.000301397761147902,0.000347170117271357),.UNSPECIFIED.);
#5037=B_SPLINE_CURVE_WITH_KNOTS('',3,(#231814,#231815,#231816,#231817,#231818,
#231819,#231820,#231821,#231822,#231823,#231824,#231825,#231826,#231827,
#231828,#231829,#231830,#231831,#231832,#231833,#231834,#231835,#231836,
#231837,#231838,#231839,#231840,#231841,#231842,#231843,#231844,#231845,
#231846,#231847,#231848,#231849,#231850,#231851,#231852,#231853,#231854,
#231855,#231856,#231857,#231858,#231859),.UNSPECIFIED.,.F.,.F.,(4,3,3,3,
3,3,3,3,3,3,3,3,3,3,3,4),(2.74438674910393E-19,2.57218161985759E-5,4.215683225698E-5,
6.45873314618026E-5,7.58025810642139E-5,8.14102058654196E-5,8.2812112065721E-5,
8.70178306666252E-5,0.000116081955658136,0.000130526745999938,0.000162394111022044,
0.00017403566133325,0.000213138396957668,0.000256116935432663,0.000302406662854469,
0.000348071322666499),.UNSPECIFIED.);
#5038=B_SPLINE_CURVE_WITH_KNOTS('',3,(#231860,#231861,#231862,#231863,#231864,
#231865,#231866,#231867,#231868,#231869,#231870,#231871,#231872,#231873,
#231874,#231875,#231876,#231877,#231878,#231879,#231880,#231881,#231882,
#231883,#231884,#231885,#231886,#231887,#231888,#231889,#231890,#231891,
#231892,#231893,#231894,#231895,#231896,#231897,#231898,#231899,#231900,
#231901,#231902,#231903,#231904,#231905,#231906,#231907,#231908,#231909,
#231910,#231911),.UNSPECIFIED.,.F.,.F.,(4,3,3,3,3,3,3,3,3,3,3,3,3,3,3,3,
3,4),(0.,4.29652152154259E-5,8.44519107524018E-5,0.000123669830863876,0.000159788877357041,
0.000170558847912633,0.000181218775907173,0.000181960046452409,0.000214460062643776,
0.000244755726199061,0.00025583827186895,0.000258503253867585,0.000261084955178762,
0.000289370476647126,0.000301101325502014,0.00032110951066364,0.000331113603244453,
0.000341117695825266),.UNSPECIFIED.);
#5039=B_SPLINE_CURVE_WITH_KNOTS('',3,(#231913,#231914,#231915,#231916,#231917,
#231918,#231919,#231920,#231921,#231922,#231923,#231924,#231925,#231926,
#231927,#231928,#231929,#231930,#231931,#231932,#231933,#231934,#231935,
#231936,#231937,#231938,#231939,#231940,#231941,#231942,#231943,#231944,
#231945,#231946,#231947,#231948,#231949,#231950,#231951,#231952,#231953,
#231954,#231955,#231956,#231957,#231958,#231959,#231960,#231961,#231962,
#231963,#231964),.UNSPECIFIED.,.F.,.F.,(4,3,3,3,3,3,3,3,3,3,3,3,3,3,3,3,
3,4),(4.33680868994202E-19,4.30706237868497E-5,8.47417087694449E-5,0.000124159989205399,
0.000160467076289471,0.000170998382116693,0.000182414994733784,0.000213747977645867,
0.000242415955901955,0.00025649757317504,0.000259169422895613,0.000261757777312419,
0.000289965130404522,0.000301877270772902,0.000321937017503144,0.000326951954185705,
0.000334474359209546,0.000341996764233386),.UNSPECIFIED.);
#5040=B_SPLINE_CURVE_WITH_KNOTS('',3,(#231965,#231966,#231967,#231968,#231969,
#231970,#231971,#231972,#231973,#231974,#231975,#231976,#231977,#231978,
#231979,#231980,#231981,#231982,#231983,#231984,#231985,#231986,#231987,
#231988,#231989,#231990,#231991,#231992,#231993,#231994,#231995,#231996,
#231997,#231998,#231999,#232000,#232001,#232002,#232003,#232004,#232005,
#232006,#232007,#232008,#232009,#232010,#232011,#232012,#232013,#232014,
#232015,#232016),.UNSPECIFIED.,.F.,.F.,(4,3,3,3,3,3,3,3,3,3,3,3,3,3,3,3,
3,4),(0.,2.58457451692491E-5,4.25394446195899E-5,6.46659869687183E-5,7.57292581432825E-5,
8.12608937305646E-5,8.26438026273851E-5,8.67925293178467E-5,0.000116015624427845,
0.00013018879397677,0.000151886926306232,0.000161963651211282,0.000162735992470962,
0.000173585058635693,0.000212487880462679,0.000255238173514224,0.000301397761148888,
0.000347170117271385),.UNSPECIFIED.);
#5041=B_SPLINE_CURVE_WITH_KNOTS('',3,(#232018,#232019,#232020,#232021,#232022,
#232023,#232024,#232025,#232026,#232027,#232028,#232029,#232030,#232031,
#232032,#232033,#232034,#232035,#232036,#232037,#232038,#232039,#232040,
#232041,#232042,#232043,#232044,#232045,#232046,#232047,#232048,#232049,
#232050,#232051,#232052,#232053,#232054,#232055,#232056,#232057,#232058,
#232059,#232060,#232061,#232062,#232063),.UNSPECIFIED.,.F.,.F.,(4,3,3,3,
3,3,3,3,3,3,3,3,3,3,3,4),(0.,2.57218161988135E-5,4.21568322567256E-5,6.45873314616746E-5,
7.58025810641491E-5,8.14102058653863E-5,8.28121120656956E-5,8.70178306666236E-5,
0.000116081955657963,0.000130526745999932,0.000162394111022053,0.00017403566133324,
0.000213138396959429,0.00025611693543614,0.000302406662859657,0.000348071322666484),
 .UNSPECIFIED.);
#5042=B_SPLINE_CURVE_WITH_KNOTS('',3,(#232064,#232065,#232066,#232067,#232068,
#232069,#232070,#232071,#232072,#232073,#232074,#232075,#232076,#232077,
#232078,#232079,#232080,#232081,#232082,#232083,#232084,#232085,#232086,
#232087,#232088,#232089,#232090,#232091,#232092,#232093,#232094,#232095,
#232096,#232097,#232098,#232099,#232100,#232101,#232102,#232103,#232104,
#232105,#232106,#232107,#232108,#232109,#232110,#232111,#232112,#232113,
#232114,#232115),.UNSPECIFIED.,.F.,.F.,(4,3,3,3,3,3,3,3,3,3,3,3,3,3,3,3,
3,4),(0.,4.29652152159573E-5,8.44519107531576E-5,0.000123669830864513,0.000159788877357335,
0.000170558847912642,0.000181218775907181,0.000181960046452405,0.000214460062643898,
0.000244755726199067,0.000255838271868955,0.00025850325386759,0.000261084955178767,
0.000289370476647809,0.000301101325502018,0.000321109510663643,0.000331113603244455,
0.000341117695825268),.UNSPECIFIED.);
#5043=B_SPLINE_CURVE_WITH_KNOTS('',3,(#232117,#232118,#232119,#232120,#232121,
#232122,#232123,#232124,#232125,#232126,#232127,#232128,#232129,#232130,
#232131,#232132,#232133,#232134,#232135,#232136,#232137,#232138,#232139,
#232140,#232141,#232142,#232143,#232144,#232145,#232146,#232147,#232148,
#232149,#232150,#232151,#232152,#232153,#232154,#232155,#232156,#232157,
#232158,#232159,#232160,#232161,#232162,#232163,#232164,#232165,#232166,
#232167,#232168),.UNSPECIFIED.,.F.,.F.,(4,3,3,3,3,3,3,3,3,3,3,3,3,3,3,3,
3,4),(0.,4.30706237860396E-5,8.47417087679563E-5,0.0001241599892032,0.000160467076286543,
0.000170998382116691,0.000182414994733795,0.000213747977645864,0.000242415955901919,
0.000256497573175036,0.00025916942289561,0.000261757777312415,0.000289965130403713,
0.000301877270772899,0.00032193701750314,0.000326951954185701,0.000334474359209541,
0.000341996764233382),.UNSPECIFIED.);
#5044=B_SPLINE_CURVE_WITH_KNOTS('',3,(#232169,#232170,#232171,#232172,#232173,
#232174,#232175,#232176,#232177,#232178,#232179,#232180,#232181,#232182,
#232183,#232184,#232185,#232186,#232187,#232188,#232189,#232190,#232191,
#232192,#232193,#232194,#232195,#232196,#232197,#232198,#232199,#232200,
#232201,#232202,#232203,#232204,#232205,#232206,#232207,#232208,#232209,
#232210,#232211,#232212,#232213,#232214,#232215,#232216,#232217,#232218,
#232219,#232220),.UNSPECIFIED.,.F.,.F.,(4,3,3,3,3,3,3,3,3,3,3,3,3,3,3,3,
3,4),(0.,2.58457451683671E-5,4.25394446195126E-5,6.46659869686776E-5,7.57292581432601E-5,
8.12608937305513E-5,8.26438026273742E-5,8.67925293178426E-5,0.000116015624427412,
0.000130188793976764,0.000151886926306224,0.000161963651211278,0.000162735992470955,
0.000173585058635685,0.000212487880460796,0.000255238173511836,0.000301397761148485,
0.000347170117271367),.UNSPECIFIED.);
#5045=B_SPLINE_CURVE_WITH_KNOTS('',3,(#232222,#232223,#232224,#232225,#232226,
#232227,#232228,#232229,#232230,#232231,#232232,#232233,#232234,#232235,
#232236,#232237,#232238,#232239,#232240,#232241,#232242,#232243,#232244,
#232245,#232246,#232247,#232248,#232249,#232250,#232251,#232252,#232253,
#232254,#232255,#232256,#232257,#232258,#232259,#232260,#232261,#232262,
#232263,#232264,#232265,#232266,#232267),.UNSPECIFIED.,.F.,.F.,(4,3,3,3,
3,3,3,3,3,3,3,3,3,3,3,4),(0.,2.57218162000375E-5,4.21568322568943E-5,6.45873314617579E-5,
7.58025810641896E-5,8.14102058654055E-5,8.28121120657095E-5,8.70178306666214E-5,
0.000116081955658435,0.000130526745999932,0.00016239411102205,0.000174035661333243,
0.000213138396958206,0.000256116935433626,0.000302406662855561,0.000348071322666497),
 .UNSPECIFIED.);
#5046=B_SPLINE_CURVE_WITH_KNOTS('',3,(#232268,#232269,#232270,#232271,#232272,
#232273,#232274,#232275,#232276,#232277,#232278,#232279,#232280,#232281,
#232282,#232283,#232284,#232285,#232286,#232287,#232288,#232289,#232290,
#232291,#232292,#232293,#232294,#232295,#232296,#232297,#232298,#232299,
#232300,#232301,#232302,#232303,#232304,#232305,#232306,#232307,#232308,
#232309,#232310,#232311,#232312,#232313,#232314,#232315,#232316,#232317,
#232318,#232319),.UNSPECIFIED.,.F.,.F.,(4,3,3,3,3,3,3,3,3,3,3,3,3,3,3,3,
3,4),(0.,4.29652152202979E-5,8.44519107602457E-5,0.000123669830873534,0.000159788877367743,
0.000170558847912636,0.000181218775907176,0.000181960046452409,0.000214460062644036,
0.000244755726199992,0.000255838271868954,0.000258503253867589,0.000261084955178767,
0.000289370476647365,0.000301101325502019,0.000321109510663646,0.000331113603244459,
0.000341117695825272),.UNSPECIFIED.);
#5047=B_SPLINE_CURVE_WITH_KNOTS('',3,(#232321,#232322,#232323,#232324,#232325,
#232326,#232327,#232328,#232329,#232330,#232331,#232332,#232333,#232334,
#232335,#232336,#232337,#232338,#232339,#232340,#232341,#232342,#232343,
#232344,#232345,#232346,#232347,#232348,#232349,#232350,#232351,#232352,
#232353,#232354,#232355,#232356,#232357,#232358,#232359,#232360,#232361,
#232362,#232363,#232364,#232365,#232366,#232367,#232368,#232369,#232370,
#232371,#232372),.UNSPECIFIED.,.F.,.F.,(4,3,3,3,3,3,3,3,3,3,3,3,3,3,3,3,
3,4),(3.03576608295941E-18,4.30706237861208E-5,8.47417087680312E-5,0.000124159989203224,
0.000160467076286393,0.000170998382116691,0.000182414994733784,0.000213747977645867,
0.000242415955902087,0.000256497573175044,0.000259169422895617,0.000261757777312423,
0.000289965130404165,0.00030187727077291,0.000321937017503154,0.000326951954185715,
0.000334474359209556,0.000341996764233397),.UNSPECIFIED.);
#5048=B_SPLINE_CURVE_WITH_KNOTS('',3,(#232373,#232374,#232375,#232376,#232377,
#232378,#232379,#232380,#232381,#232382,#232383,#232384,#232385,#232386,
#232387,#232388,#232389,#232390,#232391,#232392,#232393,#232394,#232395,
#232396,#232397,#232398,#232399,#232400,#232401,#232402,#232403,#232404,
#232405,#232406,#232407,#232408,#232409,#232410,#232411,#232412,#232413,
#232414,#232415,#232416,#232417,#232418,#232419,#232420,#232421,#232422,
#232423,#232424),.UNSPECIFIED.,.F.,.F.,(4,3,3,3,3,3,3,3,3,3,3,3,3,3,3,3,
3,4),(0.,2.58457451680044E-5,4.25394446195641E-5,6.46659869687053E-5,7.5729258143276E-5,
8.12608937305613E-5,8.26438026273826E-5,8.67925293178466E-5,0.000116015624427261,
0.00013018879397677,0.000151886926306231,0.000161963651211282,0.000162735992470962,
0.000173585058635693,0.000212487880461109,0.000255238173510755,0.000301397761142687,
0.000347170117271378),.UNSPECIFIED.);
#5049=B_SPLINE_CURVE_WITH_KNOTS('',3,(#232426,#232427,#232428,#232429,#232430,
#232431,#232432,#232433,#232434,#232435,#232436,#232437,#232438,#232439,
#232440,#232441,#232442,#232443,#232444,#232445,#232446,#232447,#232448,
#232449,#232450,#232451,#232452,#232453,#232454,#232455,#232456,#232457,
#232458,#232459,#232460,#232461,#232462,#232463,#232464,#232465,#232466,
#232467,#232468,#232469,#232470,#232471),.UNSPECIFIED.,.F.,.F.,(4,3,3,3,
3,3,3,3,3,3,3,3,3,3,3,4),(0.,2.57218161993042E-5,4.21568322568458E-5,6.45873314617294E-5,
7.58025810641711E-5,8.1410205865392E-5,8.28121120656972E-5,8.70178306666129E-5,
0.000116081955657926,0.000130526745999919,0.000162394111022046,0.000174035661333226,
0.000213138396960043,0.000256116935437413,0.000302406662861798,0.000348071322666454),
 .UNSPECIFIED.);
#5050=B_SPLINE_CURVE_WITH_KNOTS('',3,(#232472,#232473,#232474,#232475,#232476,
#232477,#232478,#232479,#232480,#232481,#232482,#232483,#232484,#232485,
#232486,#232487,#232488,#232489,#232490,#232491,#232492,#232493,#232494,
#232495,#232496,#232497,#232498,#232499,#232500,#232501,#232502,#232503,
#232504,#232505,#232506,#232507,#232508,#232509,#232510,#232511,#232512,
#232513,#232514,#232515,#232516,#232517,#232518,#232519,#232520,#232521,
#232522,#232523),.UNSPECIFIED.,.F.,.F.,(4,3,3,3,3,3,3,3,3,3,3,3,3,3,3,3,
3,4),(4.33680868994202E-19,4.29652152180482E-5,8.44519107565262E-5,0.000123669830868743,
0.000159788877362074,0.000170558847912614,0.000181218775907154,0.000181960046452388,
0.00021446006264368,0.000244755726198699,0.000255838271868931,0.000258503253867566,
0.000261084955178743,0.000289370476647433,0.000301101325501995,0.000321109510663621,
0.000331113603244434,0.000341117695825247),.UNSPECIFIED.);
#5051=B_SPLINE_CURVE_WITH_KNOTS('',3,(#232525,#232526,#232527,#232528,#232529,
#232530,#232531,#232532,#232533,#232534,#232535,#232536,#232537,#232538,
#232539,#232540,#232541,#232542,#232543,#232544,#232545,#232546,#232547,
#232548,#232549,#232550,#232551,#232552,#232553,#232554,#232555,#232556,
#232557,#232558,#232559,#232560,#232561,#232562,#232563,#232564,#232565,
#232566,#232567,#232568,#232569,#232570,#232571,#232572,#232573,#232574,
#232575,#232576),.UNSPECIFIED.,.F.,.F.,(4,3,3,3,3,3,3,3,3,3,3,3,3,3,3,3,
3,4),(0.,4.30706237873825E-5,8.47417087705214E-5,0.000124159989207137,0.000160467076292,
0.000170998382116685,0.000182414994733762,0.000213747977645859,0.000242415955902243,
0.000256497573175034,0.000259169422895608,0.000261757777312413,0.000289965130403732,
0.000301877270772898,0.000321937017503141,0.000326951954185702,0.000334474359209543,
0.000341996764233384),.UNSPECIFIED.);
#5052=B_SPLINE_CURVE_WITH_KNOTS('',3,(#232577,#232578,#232579,#232580,#232581,
#232582,#232583,#232584,#232585,#232586,#232587,#232588,#232589,#232590,
#232591,#232592,#232593,#232594,#232595,#232596,#232597,#232598,#232599,
#232600,#232601,#232602,#232603,#232604,#232605,#232606,#232607,#232608,
#232609,#232610,#232611,#232612,#232613,#232614,#232615,#232616,#232617,
#232618,#232619,#232620,#232621,#232622,#232623,#232624,#232625,#232626,
#232627,#232628),.UNSPECIFIED.,.F.,.F.,(4,3,3,3,3,3,3,3,3,3,3,3,3,3,3,3,
3,4),(3.46944695195361E-18,2.5845745168417E-5,4.25394446196045E-5,6.46659869687246E-5,
7.57292581432846E-5,8.12608937305647E-5,8.26438026273847E-5,8.67925293178447E-5,
0.000116015624427804,0.000130188793976765,0.000151886926306226,0.000161963651211278,
0.000162735992470956,0.000173585058635686,0.0002124878804612,0.000255238173511817,
0.000301397761146479,0.000347170117271368),.UNSPECIFIED.);
#5053=B_SPLINE_CURVE_WITH_KNOTS('',3,(#232630,#232631,#232632,#232633,#232634,
#232635,#232636,#232637,#232638,#232639,#232640,#232641,#232642,#232643,
#232644,#232645,#232646,#232647,#232648,#232649,#232650,#232651,#232652,
#232653,#232654,#232655,#232656,#232657,#232658,#232659,#232660,#232661,
#232662,#232663,#232664,#232665,#232666,#232667,#232668,#232669,#232670,
#232671,#232672,#232673,#232674,#232675),.UNSPECIFIED.,.F.,.F.,(4,3,3,3,
3,3,3,3,3,3,3,3,3,3,3,4),(3.46944695195361E-18,2.57218162005469E-5,4.21568322568319E-5,
6.45873314617224E-5,7.58025810641676E-5,8.14102058653903E-5,8.28121120656959E-5,
8.70178306666129E-5,0.000116081955659199,0.000130526745999918,0.000162394111022043,
0.000174035661333222,0.000213138396958457,0.000256116935434178,0.000302406662856551,
0.000348071322666449),.UNSPECIFIED.);
#5054=B_SPLINE_CURVE_WITH_KNOTS('',3,(#232676,#232677,#232678,#232679,#232680,
#232681,#232682,#232683,#232684,#232685,#232686,#232687,#232688,#232689,
#232690,#232691,#232692,#232693,#232694,#232695,#232696,#232697,#232698,
#232699,#232700,#232701,#232702,#232703,#232704,#232705,#232706,#232707,
#232708,#232709,#232710,#232711,#232712,#232713,#232714,#232715,#232716,
#232717,#232718,#232719,#232720,#232721,#232722,#232723,#232724,#232725,
#232726,#232727),.UNSPECIFIED.,.F.,.F.,(4,3,3,3,3,3,3,3,3,3,3,3,3,3,3,3,
3,4),(4.33680868994202E-19,4.29652152162623E-5,8.44519107536651E-5,0.000123669830865264,
0.000159788877358329,0.000170558847912636,0.000181218775907175,0.000181960046452412,
0.000214460062643658,0.000244755726198798,0.000255838271868947,0.000258503253867581,
0.000261084955178759,0.000289370476647833,0.000301101325502008,0.000321109510663633,
0.000331113603244445,0.000341117695825257),.UNSPECIFIED.);
#5055=B_SPLINE_CURVE_WITH_KNOTS('',3,(#232729,#232730,#232731,#232732,#232733,
#232734,#232735,#232736,#232737,#232738,#232739,#232740,#232741,#232742,
#232743,#232744,#232745,#232746,#232747,#232748,#232749,#232750,#232751,
#232752,#232753,#232754,#232755,#232756,#232757,#232758,#232759,#232760,
#232761,#232762,#232763,#232764,#232765,#232766,#232767,#232768,#232769,
#232770,#232771,#232772,#232773,#232774,#232775,#232776,#232777,#232778,
#232779,#232780),.UNSPECIFIED.,.F.,.F.,(4,3,3,3,3,3,3,3,3,3,3,3,3,3,3,3,
3,4),(3.03576608295941E-18,4.30706237878269E-5,8.47417087712909E-5,0.000124159989208148,
0.000160467076293277,0.000170998382116696,0.000182414994733774,0.00021374797764587,
0.000242415955903288,0.000256497573175043,0.000259169422895616,0.000261757777312422,
0.000289965130403097,0.000301877270772906,0.000321937017503147,0.000326951954185708,
0.000334474359209549,0.000341996764233389),.UNSPECIFIED.);
#5056=B_SPLINE_CURVE_WITH_KNOTS('',3,(#232781,#232782,#232783,#232784,#232785,
#232786,#232787,#232788,#232789,#232790,#232791,#232792,#232793,#232794,
#232795,#232796,#232797,#232798,#232799,#232800,#232801,#232802,#232803,
#232804,#232805,#232806,#232807,#232808,#232809,#232810,#232811,#232812,
#232813,#232814,#232815,#232816,#232817,#232818,#232819,#232820,#232821,
#232822,#232823,#232824,#232825,#232826,#232827,#232828,#232829,#232830,
#232831,#232832),.UNSPECIFIED.,.F.,.F.,(4,3,3,3,3,3,3,3,3,3,3,3,3,3,3,3,
3,4),(0.,2.58457451702089E-5,4.25394446196088E-5,6.46659869687252E-5,7.57292581432834E-5,
8.12608937305625E-5,8.26438026273823E-5,8.67925293178416E-5,0.000116015624427369,
0.000130188793976762,0.000151886926306223,0.000161963651211283,0.000162735992470953,
0.000173585058635683,0.000212487880460468,0.000255238173510466,0.000301397761144727,
0.000347170117271358),.UNSPECIFIED.);
#5057=B_SPLINE_CURVE_WITH_KNOTS('',3,(#232834,#232835,#232836,#232837,#232838,
#232839,#232840,#232841,#232842,#232843,#232844,#232845,#232846,#232847,
#232848,#232849,#232850,#232851,#232852,#232853,#232854,#232855,#232856,
#232857,#232858,#232859,#232860,#232861,#232862,#232863,#232864,#232865,
#232866,#232867,#232868,#232869,#232870,#232871,#232872,#232873,#232874,
#232875,#232876,#232877,#232878,#232879),.UNSPECIFIED.,.F.,.F.,(4,3,3,3,
3,3,3,3,3,3,3,3,3,3,3,4),(0.,2.57218161987217E-5,4.21568322567636E-5,6.45873314616907E-5,
7.58025810641543E-5,8.14102058653861E-5,8.28121120656941E-5,8.70178306666179E-5,
0.000116081955658106,0.000130526745999927,0.000162394111022036,0.000174035661333236,
0.000213138396955684,0.000256116935428608,0.000302406662847822,0.000348071322666479),
 .UNSPECIFIED.);
#5058=B_SPLINE_CURVE_WITH_KNOTS('',3,(#232880,#232881,#232882,#232883,#232884,
#232885,#232886,#232887,#232888,#232889,#232890,#232891,#232892,#232893,
#232894,#232895,#232896,#232897,#232898,#232899,#232900,#232901,#232902,
#232903,#232904,#232905,#232906,#232907,#232908,#232909,#232910,#232911,
#232912,#232913,#232914,#232915,#232916,#232917,#232918,#232919,#232920,
#232921,#232922,#232923,#232924,#232925,#232926,#232927,#232928,#232929,
#232930,#232931),.UNSPECIFIED.,.F.,.F.,(4,3,3,3,3,3,3,3,3,3,3,3,3,3,3,3,
3,4),(0.,4.29652152151169E-5,8.4451910752229E-5,0.000123669830864283,0.000159788877358467,
0.000170558847912639,0.000181218775907178,0.000181960046452411,0.00021446006264415,
0.000244755726200223,0.00025583827186895,0.000258503253867585,0.000261084955178762,
0.000289370476646099,0.000301101325502012,0.000321109510663636,0.000331113603244449,
0.000341117695825261),.UNSPECIFIED.);
#5059=B_SPLINE_CURVE_WITH_KNOTS('',3,(#232933,#232934,#232935,#232936,#232937,
#232938,#232939,#232940,#232941,#232942,#232943,#232944,#232945,#232946,
#232947,#232948,#232949,#232950,#232951,#232952,#232953,#232954,#232955,
#232956,#232957,#232958,#232959,#232960,#232961,#232962,#232963,#232964,
#232965,#232966,#232967,#232968,#232969,#232970,#232971,#232972,#232973,
#232974,#232975,#232976,#232977,#232978,#232979,#232980,#232981,#232982,
#232983,#232984),.UNSPECIFIED.,.F.,.F.,(4,3,3,3,3,3,3,3,3,3,3,3,3,3,3,3,
3,4),(0.,4.30706237873135E-5,8.47417087702485E-5,0.000124159989206487,0.000160467076290862,
0.000170998382116686,0.000182414994733771,0.000213747977645862,0.000242415955902801,
0.000256497573175037,0.000259169422895611,0.000261757777312416,0.000289965130403939,
0.000301877270772903,0.000321937017503146,0.000326951954185706,0.000334474359209548,
0.000341996764233389),.UNSPECIFIED.);
#5060=B_SPLINE_CURVE_WITH_KNOTS('',3,(#232985,#232986,#232987,#232988,#232989,
#232990,#232991,#232992,#232993,#232994,#232995,#232996,#232997,#232998,
#232999,#233000,#233001,#233002,#233003,#233004,#233005,#233006,#233007,
#233008,#233009,#233010,#233011,#233012,#233013,#233014,#233015,#233016,
#233017,#233018,#233019,#233020,#233021,#233022,#233023,#233024,#233025,
#233026,#233027,#233028,#233029,#233030,#233031,#233032,#233033,#233034,
#233035,#233036),.UNSPECIFIED.,.F.,.F.,(4,3,3,3,3,3,3,3,3,3,3,3,3,3,3,3,
3,4),(0.,2.58457451693913E-5,4.2539444619546E-5,6.46659869686941E-5,7.57292581432681E-5,
8.12608937305551E-5,8.26438026273769E-5,8.67925293178422E-5,0.000116015624427399,
0.000130188793976763,0.000151886926306224,0.000161963651211272,0.000162735992470954,
0.000173585058635684,0.000212487880460446,0.000255238173511253,0.000301397761147859,
0.000347170117271368),.UNSPECIFIED.);
#5061=B_SPLINE_CURVE_WITH_KNOTS('',3,(#233038,#233039,#233040,#233041,#233042,
#233043,#233044,#233045,#233046,#233047,#233048,#233049,#233050,#233051,
#233052,#233053,#233054,#233055,#233056,#233057,#233058,#233059,#233060,
#233061,#233062,#233063,#233064,#233065,#233066,#233067,#233068,#233069,
#233070,#233071,#233072,#233073,#233074,#233075,#233076,#233077,#233078,
#233079,#233080,#233081,#233082,#233083),.UNSPECIFIED.,.F.,.F.,(4,3,3,3,
3,3,3,3,3,3,3,3,3,3,3,4),(0.,2.57218161993301E-5,4.21568322567844E-5,6.45873314617024E-5,
7.58025810641613E-5,8.14102058653908E-5,8.28121120656982E-5,8.70178306666203E-5,
0.000116081955658652,0.00013052674599993,0.000162394111022054,0.000174035661333241,
0.00021313839696057,0.000256116935438433,0.000302406662863314,0.000348071322666482),
 .UNSPECIFIED.);
#5062=B_SPLINE_CURVE_WITH_KNOTS('',3,(#233084,#233085,#233086,#233087,#233088,
#233089,#233090,#233091,#233092,#233093,#233094,#233095,#233096,#233097,
#233098,#233099,#233100,#233101,#233102,#233103,#233104,#233105,#233106,
#233107,#233108,#233109,#233110,#233111,#233112,#233113,#233114,#233115,
#233116,#233117,#233118,#233119,#233120,#233121,#233122,#233123,#233124,
#233125,#233126,#233127,#233128,#233129,#233130,#233131,#233132,#233133,
#233134,#233135),.UNSPECIFIED.,.F.,.F.,(4,3,3,3,3,3,3,3,3,3,3,3,3,3,3,3,
3,4),(0.,4.29652152133293E-5,8.44519107489887E-5,0.000123669830859642,0.000159788877352289,
0.000170558847912625,0.000181218775907164,0.000181960046452431,0.000214460062644072,
0.000244755726200207,0.000255838271868938,0.000258503253867573,0.00026108495517875,
0.000289370476647827,0.000301101325502001,0.000321109510663626,0.000331113603244438,
0.000341117695825251),.UNSPECIFIED.);
#5063=B_SPLINE_CURVE_WITH_KNOTS('',3,(#233137,#233138,#233139,#233140,#233141,
#233142,#233143,#233144,#233145,#233146,#233147,#233148,#233149,#233150,
#233151,#233152,#233153,#233154,#233155,#233156,#233157,#233158,#233159,
#233160,#233161,#233162,#233163,#233164,#233165,#233166,#233167,#233168,
#233169,#233170,#233171,#233172,#233173,#233174,#233175,#233176,#233177,
#233178,#233179,#233180,#233181,#233182,#233183,#233184,#233185,#233186,
#233187,#233188),.UNSPECIFIED.,.F.,.F.,(4,3,3,3,3,3,3,3,3,3,3,3,3,3,3,3,
3,4),(0.,4.30706237846825E-5,8.47417087656643E-5,0.000124159989200225,0.000160467076282839,
0.000170998382116685,0.000182414994733771,0.00021374797764586,0.000242415955903785,
0.000256497573175036,0.000259169422895609,0.000261757777312415,0.000289965130404008,
0.000301877270772901,0.000321937017503144,0.000326951954185705,0.000334474359209546,
0.000341996764233387),.UNSPECIFIED.);
#5064=B_SPLINE_CURVE_WITH_KNOTS('',3,(#233189,#233190,#233191,#233192,#233193,
#233194,#233195,#233196,#233197,#233198,#233199,#233200,#233201,#233202,
#233203,#233204,#233205,#233206,#233207,#233208,#233209,#233210,#233211,
#233212,#233213,#233214,#233215,#233216,#233217,#233218,#233219,#233220,
#233221,#233222,#233223,#233224,#233225,#233226,#233227,#233228,#233229,
#233230,#233231,#233232,#233233,#233234,#233235,#233236,#233237,#233238,
#233239,#233240),.UNSPECIFIED.,.F.,.F.,(4,3,3,3,3,3,3,3,3,3,3,3,3,3,3,3,
3,4),(0.,2.58457451681982E-5,4.25394446197375E-5,6.46659869687881E-5,7.57292581433134E-5,
8.1260893730576E-5,8.26438026273917E-5,8.67925293178387E-5,0.000116015624428111,
0.000130188793976758,0.000151886926306218,0.000161963651211279,0.000162735992470948,
0.000173585058635677,0.000212487880463093,0.000255238173516002,0.000301397761153951,
0.000347170117271371),.UNSPECIFIED.);
#5065=B_SPLINE_CURVE_WITH_KNOTS('',3,(#233242,#233243,#233244,#233245,#233246,
#233247,#233248,#233249,#233250,#233251,#233252,#233253,#233254,#233255,
#233256,#233257,#233258,#233259,#233260,#233261,#233262,#233263,#233264,
#233265,#233266,#233267,#233268,#233269,#233270,#233271,#233272,#233273,
#233274,#233275,#233276,#233277,#233278,#233279,#233280,#233281,#233282,
#233283,#233284,#233285,#233286,#233287),.UNSPECIFIED.,.F.,.F.,(4,3,3,3,
3,3,3,3,3,3,3,3,3,3,3,4),(0.,2.57218161997734E-5,4.21568322567237E-5,6.45873314616717E-5,
7.58025810641458E-5,8.14102058653828E-5,8.2812112065692E-5,8.70178306666198E-5,
0.00011608195565779,0.00013052674599993,0.000162394111022048,0.00017403566133324,
0.000213138396958063,0.00025611693543337,0.000302406662855231,0.000348071322666498),
 .UNSPECIFIED.);
#5066=B_SPLINE_CURVE_WITH_KNOTS('',3,(#233288,#233289,#233290,#233291,#233292,
#233293,#233294,#233295,#233296,#233297,#233298,#233299,#233300,#233301,
#233302,#233303,#233304,#233305,#233306,#233307,#233308,#233309,#233310,
#233311,#233312,#233313,#233314,#233315,#233316,#233317,#233318,#233319,
#233320,#233321,#233322,#233323,#233324,#233325,#233326,#233327,#233328,
#233329,#233330,#233331,#233332,#233333,#233334,#233335,#233336,#233337,
#233338,#233339),.UNSPECIFIED.,.F.,.F.,(4,3,3,3,3,3,3,3,3,3,3,3,3,3,3,3,
3,4),(0.,4.29652152152899E-5,8.44519107520695E-5,0.000123669830863396,0.000159788877356221,
0.000170558847912629,0.000181218775907169,0.00018196004645238,0.000214460062643359,
0.000244755726197827,0.000255838271868951,0.000258503253867586,0.000261084955178764,
0.000289370476648966,0.000301101325502019,0.000321109510663646,0.00033111360324446,
0.000341117695825274),.UNSPECIFIED.);
#5067=B_SPLINE_CURVE_WITH_KNOTS('',3,(#233341,#233342,#233343,#233344,#233345,
#233346,#233347,#233348,#233349,#233350,#233351,#233352,#233353,#233354,
#233355,#233356,#233357,#233358,#233359,#233360,#233361,#233362,#233363,
#233364,#233365,#233366,#233367,#233368,#233369,#233370,#233371,#233372,
#233373,#233374,#233375,#233376,#233377,#233378,#233379,#233380,#233381,
#233382,#233383,#233384,#233385,#233386,#233387,#233388,#233389,#233390,
#233391,#233392),.UNSPECIFIED.,.F.,.F.,(4,3,3,3,3,3,3,3,3,3,3,3,3,3,3,3,
3,4),(4.33680868994202E-19,4.30706237891753E-5,8.47417087736514E-5,0.000124159989211244,
0.00016046707629719,0.000170998382116694,0.000182414994733769,0.000213747977645867,
0.000242415955902945,0.00025649757317504,0.000259169422895614,0.000261757777312419,
0.000289965130403412,0.000301877270772903,0.000321937017503145,0.000326951954185705,
0.000334474359209546,0.000341996764233387),.UNSPECIFIED.);
#5068=B_SPLINE_CURVE_WITH_KNOTS('',3,(#233393,#233394,#233395,#233396,#233397,
#233398,#233399,#233400,#233401,#233402,#233403,#233404,#233405,#233406,
#233407,#233408,#233409,#233410,#233411,#233412,#233413,#233414,#233415,
#233416,#233417,#233418,#233419,#233420,#233421,#233422,#233423,#233424,
#233425,#233426,#233427,#233428,#233429,#233430,#233431,#233432,#233433,
#233434,#233435,#233436,#233437,#233438,#233439,#233440,#233441,#233442,
#233443,#233444),.UNSPECIFIED.,.F.,.F.,(4,3,3,3,3,3,3,3,3,3,3,3,3,3,3,3,
3,4),(0.,2.58457451678341E-5,4.25394446195883E-5,6.46659869687171E-5,7.57292581432815E-5,
8.12608937305636E-5,8.26438026273842E-5,8.67925293178458E-5,0.000116015624426969,
0.000130188793976769,0.00015188692630623,0.000161963651211286,0.000162735992470961,
0.000173585058635692,0.000212487880461625,0.000255238173512158,0.00030139776114569,
0.000347170117271384),.UNSPECIFIED.);
#5069=B_SPLINE_CURVE_WITH_KNOTS('',3,(#233446,#233447,#233448,#233449,#233450,
#233451,#233452,#233453,#233454,#233455,#233456,#233457,#233458,#233459,
#233460,#233461,#233462,#233463,#233464,#233465,#233466,#233467,#233468,
#233469,#233470,#233471,#233472,#233473,#233474,#233475,#233476,#233477,
#233478,#233479,#233480,#233481,#233482,#233483,#233484,#233485,#233486,
#233487,#233488,#233489,#233490,#233491),.UNSPECIFIED.,.F.,.F.,(4,3,3,3,
3,3,3,3,3,3,3,3,3,3,3,4),(0.,2.57218161985664E-5,4.21568322568204E-5,6.45873314617178E-5,
7.58025810641665E-5,8.14102058653908E-5,8.28121120656969E-5,8.70178306666152E-5,
0.000116081955657799,0.000130526745999923,0.000162394111022031,0.00017403566133323,
0.00021313839695763,0.000256116935432652,0.000302406662854616,0.00034807132266646),
 .UNSPECIFIED.);
#5070=B_SPLINE_CURVE_WITH_KNOTS('',3,(#233492,#233493,#233494,#233495,#233496,
#233497,#233498,#233499,#233500,#233501,#233502,#233503,#233504,#233505,
#233506,#233507,#233508,#233509,#233510,#233511,#233512,#233513,#233514,
#233515,#233516,#233517,#233518,#233519,#233520,#233521,#233522,#233523,
#233524,#233525,#233526,#233527,#233528,#233529,#233530,#233531,#233532,
#233533,#233534,#233535,#233536,#233537,#233538,#233539,#233540,#233541,
#233542,#233543),.UNSPECIFIED.,.F.,.F.,(4,3,3,3,3,3,3,3,3,3,3,3,3,3,3,3,
3,4),(4.33680868994202E-19,4.2965215218658E-5,8.44519107577739E-5,0.000123669830870734,
0.000159788877365064,0.000170558847912629,0.000181218775907169,0.000181960046452411,
0.000214460062643825,0.000244755726198647,0.000255838271868945,0.00025850325386758,
0.000261084955178758,0.000289370476647757,0.00030110132550201,0.000321109510663636,
0.000331113603244449,0.000341117695825262),.UNSPECIFIED.);
#5071=B_SPLINE_CURVE_WITH_KNOTS('',3,(#233545,#233546,#233547,#233548,#233549,
#233550,#233551,#233552,#233553,#233554,#233555,#233556,#233557,#233558,
#233559,#233560,#233561,#233562,#233563,#233564,#233565,#233566,#233567,
#233568,#233569,#233570,#233571,#233572,#233573,#233574,#233575,#233576,
#233577,#233578,#233579,#233580,#233581,#233582,#233583,#233584,#233585,
#233586,#233587,#233588,#233589,#233590,#233591,#233592,#233593,#233594,
#233595,#233596),.UNSPECIFIED.,.F.,.F.,(4,3,3,3,3,3,3,3,3,3,3,3,3,3,3,3,
3,4),(0.,4.30706237853674E-5,8.47417087668512E-5,0.000124159989201798,0.000160467076284875,
0.000170998382116698,0.00018241499473378,0.000213747977645872,0.00024241595590339,
0.000256497573175045,0.000259169422895618,0.000261757777312424,0.000289965130402989,
0.000301877270772908,0.00032193701750315,0.00032695195418571,0.000334474359209551,
0.000341996764233392),.UNSPECIFIED.);
#5072=B_SPLINE_CURVE_WITH_KNOTS('',3,(#233597,#233598,#233599,#233600,#233601,
#233602,#233603,#233604,#233605,#233606,#233607,#233608,#233609,#233610,
#233611,#233612,#233613,#233614,#233615,#233616,#233617,#233618,#233619,
#233620,#233621,#233622,#233623,#233624,#233625,#233626,#233627,#233628,
#233629,#233630,#233631,#233632,#233633,#233634,#233635,#233636,#233637,
#233638,#233639,#233640,#233641,#233642,#233643,#233644,#233645,#233646,
#233647,#233648),.UNSPECIFIED.,.F.,.F.,(4,3,3,3,3,3,3,3,3,3,3,3,3,3,3,3,
3,4),(0.,2.5845745169787E-5,4.25394446194455E-5,6.46659869686411E-5,7.57292581432389E-5,
8.12608937305378E-5,8.26438026273625E-5,8.67925293178367E-5,0.000116015624427309,
0.000130188793976755,0.000151886926306214,0.000161963651211279,0.000162735992470944,
0.000173585058635673,0.000212487880458767,0.000255238173506756,0.000301397761138237,
0.000347170117271364),.UNSPECIFIED.);
#5073=B_SPLINE_CURVE_WITH_KNOTS('',3,(#233650,#233651,#233652,#233653,#233654,
#233655,#233656,#233657,#233658,#233659,#233660,#233661,#233662,#233663,
#233664,#233665,#233666,#233667,#233668,#233669,#233670,#233671,#233672,
#233673,#233674,#233675,#233676,#233677,#233678,#233679,#233680,#233681,
#233682,#233683,#233684,#233685,#233686,#233687,#233688,#233689,#233690,
#233691,#233692,#233693,#233694,#233695),.UNSPECIFIED.,.F.,.F.,(4,3,3,3,
3,3,3,3,3,3,3,3,3,3,3,4),(0.,2.57218161994861E-5,4.21568322567979E-5,6.45873314617086E-5,
7.5802581064164E-5,8.14102058653917E-5,8.28121120656986E-5,8.70178306666193E-5,
0.000116081955658953,0.000130526745999929,0.000162394111022036,0.000174035661333239,
0.000213138396959787,0.000256116935436981,0.000302406662861451,0.000348071322666494),
 .UNSPECIFIED.);
#5074=B_SPLINE_CURVE_WITH_KNOTS('',3,(#233696,#233697,#233698,#233699,#233700,
#233701,#233702,#233703,#233704,#233705,#233706,#233707,#233708,#233709,
#233710,#233711,#233712,#233713,#233714,#233715,#233716,#233717,#233718,
#233719,#233720,#233721,#233722,#233723,#233724,#233725,#233726,#233727,
#233728,#233729,#233730,#233731,#233732,#233733,#233734,#233735,#233736,
#233737,#233738,#233739,#233740,#233741,#233742,#233743,#233744,#233745,
#233746,#233747),.UNSPECIFIED.,.F.,.F.,(4,3,3,3,3,3,3,3,3,3,3,3,3,3,3,3,
3,4),(0.,4.29652152170427E-5,8.44519107551245E-5,0.000123669830867409,0.000159788877361216,
0.000170558847912622,0.000181218775907161,0.000181960046452394,0.000214460062643908,
0.000244755726199335,0.00025583827186894,0.000258503253867575,0.000261084955178753,
0.000289370476646841,0.000301101325502006,0.000321109510663632,0.000331113603244446,
0.000341117695825259),.UNSPECIFIED.);
#5075=B_SPLINE_CURVE_WITH_KNOTS('',3,(#233749,#233750,#233751,#233752,#233753,
#233754,#233755,#233756,#233757,#233758,#233759,#233760,#233761,#233762,
#233763,#233764,#233765,#233766,#233767,#233768,#233769,#233770,#233771,
#233772,#233773,#233774,#233775,#233776,#233777,#233778,#233779,#233780,
#233781,#233782,#233783,#233784,#233785,#233786,#233787,#233788,#233789,
#233790,#233791,#233792,#233793,#233794,#233795,#233796,#233797,#233798,
#233799,#233800),.UNSPECIFIED.,.F.,.F.,(4,3,3,3,3,3,3,3,3,3,3,3,3,3,3,3,
3,4),(1.73472347597681E-18,4.30706237846257E-5,8.47417087654249E-5,0.000124159989199596,
0.000160467076281756,0.000170998382116706,0.000182414994733789,0.000213747977645876,
0.000242415955904062,0.000256497573175046,0.000259169422895619,0.000261757777312425,
0.000289965130401927,0.000301877270772905,0.000321937017503146,0.000326951954185706,
0.000334474359209546,0.000341996764233386),.UNSPECIFIED.);
#5076=B_SPLINE_CURVE_WITH_KNOTS('',3,(#233801,#233802,#233803,#233804,#233805,
#233806,#233807,#233808,#233809,#233810,#233811,#233812,#233813,#233814,
#233815,#233816,#233817,#233818,#233819,#233820,#233821,#233822,#233823,
#233824,#233825,#233826,#233827,#233828,#233829,#233830,#233831,#233832,
#233833,#233834,#233835,#233836,#233837,#233838,#233839,#233840,#233841,
#233842,#233843,#233844,#233845,#233846,#233847,#233848,#233849,#233850,
#233851,#233852),.UNSPECIFIED.,.F.,.F.,(4,3,3,3,3,3,3,3,3,3,3,3,3,3,3,3,
3,4),(0.,2.58457451679675E-5,4.25394446195623E-5,6.46659869687017E-5,7.57292581432714E-5,
8.12608937305563E-5,8.26438026273775E-5,8.67925293178412E-5,0.000116015624427185,
0.000130188793976762,0.000151886926306222,0.000161963651211282,0.000162735992470952,
0.000173585058635682,0.000212487880461526,0.000255238173513458,0.000301397761151195,
0.000347170117271365),.UNSPECIFIED.);
#5077=B_SPLINE_CURVE_WITH_KNOTS('',3,(#233854,#233855,#233856,#233857,#233858,
#233859,#233860,#233861,#233862,#233863,#233864,#233865,#233866,#233867,
#233868,#233869,#233870,#233871,#233872,#233873,#233874,#233875,#233876,
#233877,#233878,#233879,#233880,#233881,#233882,#233883,#233884,#233885,
#233886,#233887,#233888,#233889,#233890,#233891,#233892,#233893,#233894,
#233895,#233896,#233897,#233898,#233899),.UNSPECIFIED.,.F.,.F.,(4,3,3,3,
3,3,3,3,3,3,3,3,3,3,3,4),(0.,2.57218162002627E-5,4.21568322568371E-5,6.45873314617265E-5,
7.58025810641712E-5,8.14102058653936E-5,8.28121120656992E-5,8.70178306666159E-5,
0.000116081955658511,0.000130526745999924,0.000162394111022038,0.000174035661333232,
0.000213138396959335,0.00025611693543601,0.000302406662859656,0.000348071322666466),
 .UNSPECIFIED.);
#5078=B_SPLINE_CURVE_WITH_KNOTS('',3,(#233900,#233901,#233902,#233903,#233904,
#233905,#233906,#233907,#233908,#233909,#233910,#233911,#233912,#233913,
#233914,#233915,#233916,#233917,#233918,#233919,#233920,#233921,#233922,
#233923,#233924,#233925,#233926,#233927,#233928,#233929,#233930,#233931,
#233932,#233933,#233934,#233935,#233936,#233937,#233938,#233939,#233940,
#233941,#233942,#233943,#233944,#233945,#233946,#233947,#233948,#233949,
#233950,#233951),.UNSPECIFIED.,.F.,.F.,(4,3,3,3,3,3,3,3,3,3,3,3,3,3,3,3,
3,4),(0.,4.29652152182024E-5,8.44519107564933E-5,0.00012366983086809,0.000159788877360639,
0.000170558847912628,0.000181218775907167,0.000181960046452403,0.000214460062643301,
0.000244755726197727,0.000255838271868942,0.000258503253867577,0.000261084955178754,
0.00028937047664789,0.000301101325502005,0.000321109510663631,0.000331113603244444,
0.000341117695825256),.UNSPECIFIED.);
#5079=B_SPLINE_CURVE_WITH_KNOTS('',3,(#233953,#233954,#233955,#233956,#233957,
#233958,#233959,#233960,#233961,#233962,#233963,#233964,#233965,#233966,
#233967,#233968,#233969,#233970,#233971,#233972,#233973,#233974,#233975,
#233976,#233977,#233978,#233979,#233980,#233981,#233982,#233983,#233984,
#233985,#233986,#233987,#233988,#233989,#233990,#233991,#233992,#233993,
#233994,#233995,#233996,#233997,#233998,#233999,#234000,#234001,#234002,
#234003,#234004),.UNSPECIFIED.,.F.,.F.,(4,3,3,3,3,3,3,3,3,3,3,3,3,3,3,3,
3,4),(1.30104260698261E-18,4.30706237875003E-5,8.47417087704618E-5,0.000124159989206612,
0.00016046707629077,0.000170998382116696,0.00018241499473378,0.000213747977645868,
0.000242415955902669,0.00025649757317504,0.000259169422895613,0.000261757777312418,
0.00028996513040356,0.000301877270772901,0.000321937017503142,0.000326951954185702,
0.000334474359209543,0.000341996764233383),.UNSPECIFIED.);
#5080=B_SPLINE_CURVE_WITH_KNOTS('',3,(#234005,#234006,#234007,#234008,#234009,
#234010,#234011,#234012,#234013,#234014,#234015,#234016,#234017,#234018,
#234019,#234020,#234021,#234022,#234023,#234024,#234025,#234026,#234027,
#234028,#234029,#234030,#234031,#234032,#234033,#234034,#234035,#234036,
#234037,#234038,#234039,#234040,#234041,#234042,#234043,#234044,#234045,
#234046,#234047,#234048,#234049,#234050,#234051,#234052,#234053,#234054,
#234055,#234056),.UNSPECIFIED.,.F.,.F.,(4,3,3,3,3,3,3,3,3,3,3,3,3,3,3,3,
3,4),(0.,2.58457451671873E-5,4.25394446196736E-5,6.46659869687558E-5,7.5729258143297E-5,
8.12608937305675E-5,8.26438026273852E-5,8.67925293178381E-5,0.000116015624426789,
0.000130188793976757,0.000151886926306217,0.000161963651211268,0.000162735992470946,
0.000173585058635676,0.000212487880462401,0.000255238173514613,0.000301397761151736,
0.000347170117271366),.UNSPECIFIED.);
#5081=B_SPLINE_CURVE_WITH_KNOTS('',3,(#234058,#234059,#234060,#234061,#234062,
#234063,#234064,#234065,#234066,#234067,#234068,#234069,#234070,#234071,
#234072,#234073,#234074,#234075,#234076,#234077,#234078,#234079,#234080,
#234081,#234082,#234083,#234084,#234085,#234086,#234087,#234088,#234089,
#234090,#234091,#234092,#234093,#234094,#234095,#234096,#234097,#234098,
#234099,#234100,#234101,#234102,#234103),.UNSPECIFIED.,.F.,.F.,(4,3,3,3,
3,3,3,3,3,3,3,3,3,3,3,4),(0.,2.57218161987729E-5,4.21568322568131E-5,6.45873314617148E-5,
7.58025810641656E-5,8.1410205865391E-5,8.28121120656974E-5,8.70178306666164E-5,
0.000116081955658176,0.000130526745999925,0.000162394111022042,0.000174035661333233,
0.000213138396957878,0.00025611693543317,0.000302406662855509,0.000348071322666435),
 .UNSPECIFIED.);
#5082=B_SPLINE_CURVE_WITH_KNOTS('',3,(#234104,#234105,#234106,#234107,#234108,
#234109,#234110,#234111,#234112,#234113,#234114,#234115,#234116,#234117,
#234118,#234119,#234120,#234121,#234122,#234123,#234124,#234125,#234126,
#234127,#234128,#234129,#234130,#234131,#234132,#234133,#234134,#234135,
#234136,#234137,#234138,#234139,#234140,#234141,#234142,#234143,#234144,
#234145,#234146,#234147,#234148,#234149,#234150,#234151,#234152,#234153,
#234154,#234155),.UNSPECIFIED.,.F.,.F.,(4,3,3,3,3,3,3,3,3,3,3,3,3,3,3,3,
3,4),(0.,4.29652152218646E-5,8.44519107628296E-5,0.000123669830876734,0.000159788877371542,
0.000170558847912634,0.000181218775907173,0.000181960046452415,0.00021446006264388,
0.000244755726199356,0.000255838271868947,0.000258503253867581,0.000261084955178759,
0.000289370476646635,0.000301101325502009,0.000321109510663634,0.000331113603244447,
0.000341117695825259),.UNSPECIFIED.);
#5083=B_SPLINE_CURVE_WITH_KNOTS('',3,(#234157,#234158,#234159,#234160,#234161,
#234162,#234163,#234164,#234165,#234166,#234167,#234168,#234169,#234170,
#234171,#234172,#234173,#234174,#234175,#234176,#234177,#234178,#234179,
#234180,#234181,#234182,#234183,#234184,#234185,#234186,#234187,#234188,
#234189,#234190,#234191,#234192,#234193,#234194,#234195,#234196,#234197,
#234198,#234199,#234200,#234201,#234202,#234203,#234204,#234205,#234206,
#234207,#234208),.UNSPECIFIED.,.F.,.F.,(4,3,3,3,3,3,3,3,3,3,3,3,3,3,3,3,
3,4),(8.68445263380243E-18,4.30706237867881E-5,8.47417087695995E-5,0.000124159989206084,
0.000160467076290811,0.000170998382116702,0.000182414994733779,0.000213747977645876,
0.000242415955903851,0.000256497573175051,0.000259169422895625,0.00026175777731243,
0.00028996513040331,0.000301877270772915,0.000321937017503158,0.000326951954185719,
0.00033447435920956,0.000341996764233401),.UNSPECIFIED.);
#5084=B_SPLINE_CURVE_WITH_KNOTS('',3,(#234209,#234210,#234211,#234212,#234213,
#234214,#234215,#234216,#234217,#234218,#234219,#234220,#234221,#234222,
#234223,#234224,#234225,#234226,#234227,#234228,#234229,#234230,#234231,
#234232,#234233,#234234,#234235,#234236,#234237,#234238,#234239,#234240,
#234241,#234242,#234243,#234244,#234245,#234246,#234247,#234248,#234249,
#234250,#234251,#234252,#234253,#234254,#234255,#234256,#234257,#234258,
#234259,#234260),.UNSPECIFIED.,.F.,.F.,(4,3,3,3,3,3,3,3,3,3,3,3,3,3,3,3,
3,4),(0.,2.58457451680534E-5,4.25394446195252E-5,6.46659869686818E-5,7.57292581432601E-5,
8.12608937305493E-5,8.26438026273716E-5,8.67925293178384E-5,0.000116015624427207,
0.000130188793976758,0.000151886926306217,0.000161963651211286,0.000162735992470947,
0.000173585058635677,0.00021248788045977,0.000255238173509542,0.000301397761144293,
0.000347170117271369),.UNSPECIFIED.);
#5085=B_SPLINE_CURVE_WITH_KNOTS('',3,(#234262,#234263,#234264,#234265,#234266,
#234267,#234268,#234269,#234270,#234271,#234272,#234273,#234274,#234275,
#234276,#234277,#234278,#234279,#234280,#234281,#234282,#234283,#234284,
#234285,#234286,#234287,#234288,#234289,#234290,#234291,#234292,#234293,
#234294,#234295,#234296,#234297,#234298,#234299,#234300,#234301,#234302,
#234303,#234304,#234305,#234306,#234307),.UNSPECIFIED.,.F.,.F.,(4,3,3,3,
3,3,3,3,3,3,3,3,3,3,3,4),(3.46944695195361E-18,2.57218162013466E-5,4.21568322567922E-5,
6.45873314617082E-5,7.58025810641662E-5,8.14102058653952E-5,8.28121120657025E-5,
8.70178306666242E-5,0.0001160819556593,0.000130526745999935,0.000162394111022058,
0.000174035661333245,0.00021313839695979,0.000256116935436838,0.000302406662860849,
0.000348071322666457),.UNSPECIFIED.);
#5086=B_SPLINE_CURVE_WITH_KNOTS('',3,(#234308,#234309,#234310,#234311,#234312,
#234313,#234314,#234315,#234316,#234317,#234318,#234319,#234320,#234321,
#234322,#234323,#234324,#234325,#234326,#234327,#234328,#234329,#234330,
#234331,#234332,#234333,#234334,#234335,#234336,#234337,#234338,#234339,
#234340,#234341,#234342,#234343,#234344,#234345,#234346,#234347,#234348,
#234349,#234350,#234351,#234352,#234353,#234354,#234355,#234356,#234357,
#234358,#234359),.UNSPECIFIED.,.F.,.F.,(4,3,3,3,3,3,3,3,3,3,3,3,3,3,3,3,
3,4),(0.,4.29652152143574E-5,8.44519107509678E-5,0.000123669830862744,0.000159788877356808,
0.000170558847912645,0.000181218775907184,0.000181960046452413,0.00021446006264388,
0.000244755726199279,0.000255838271868959,0.000258503253867594,0.000261084955178771,
0.000289370476647778,0.000301101325502022,0.000321109510663648,0.00033111360324446,
0.000341117695825273),.UNSPECIFIED.);
#5087=B_SPLINE_CURVE_WITH_KNOTS('',3,(#234361,#234362,#234363,#234364,#234365,
#234366,#234367,#234368,#234369,#234370,#234371,#234372,#234373,#234374,
#234375,#234376,#234377,#234378,#234379,#234380,#234381,#234382,#234383,
#234384,#234385,#234386,#234387,#234388,#234389,#234390,#234391,#234392,
#234393,#234394,#234395,#234396,#234397,#234398,#234399,#234400,#234401,
#234402,#234403,#234404,#234405,#234406,#234407,#234408,#234409,#234410,
#234411,#234412),.UNSPECIFIED.,.F.,.F.,(4,3,3,3,3,3,3,3,3,3,3,3,3,3,3,3,
3,4),(0.,4.30706237877896E-5,8.47417087711211E-5,0.000124159989207682,0.000160467076292507,
0.000170998382116696,0.000182414994733788,0.000213747977645869,0.000242415955903998,
0.000256497573175042,0.000259169422895615,0.000261757777312421,0.000289965130402697,
0.000301877270772904,0.000321937017503146,0.000326951954185707,0.000334474359209547,
0.000341996764233388),.UNSPECIFIED.);
#5088=B_SPLINE_CURVE_WITH_KNOTS('',3,(#234413,#234414,#234415,#234416,#234417,
#234418,#234419,#234420,#234421,#234422,#234423,#234424,#234425,#234426,
#234427,#234428,#234429,#234430,#234431,#234432,#234433,#234434,#234435,
#234436,#234437,#234438,#234439,#234440,#234441,#234442,#234443,#234444,
#234445,#234446,#234447,#234448,#234449,#234450,#234451,#234452,#234453,
#234454,#234455,#234456,#234457,#234458,#234459,#234460,#234461,#234462,
#234463,#234464),.UNSPECIFIED.,.F.,.F.,(4,3,3,3,3,3,3,3,3,3,3,3,3,3,3,3,
3,4),(0.,2.58457451671327E-5,4.25394446196085E-5,6.46659869687207E-5,7.57292581432768E-5,
8.12608937305548E-5,8.26438026273743E-5,8.67925293178329E-5,0.000116015624427058,
0.000130188793976749,0.000151886926306208,0.000161963651211277,0.000162735992470937,
0.000173585058635666,0.000212487880460147,0.000255238173510913,0.000301397761147941,
0.000347170117271348),.UNSPECIFIED.);
#5089=B_SPLINE_CURVE_WITH_KNOTS('',3,(#234466,#234467,#234468,#234469,#234470,
#234471,#234472,#234473,#234474,#234475,#234476,#234477,#234478,#234479,
#234480,#234481,#234482,#234483,#234484,#234485,#234486,#234487,#234488,
#234489,#234490,#234491,#234492,#234493,#234494,#234495,#234496,#234497,
#234498,#234499,#234500,#234501,#234502,#234503,#234504,#234505,#234506,
#234507,#234508,#234509,#234510,#234511),.UNSPECIFIED.,.F.,.F.,(4,3,3,3,
3,3,3,3,3,3,3,3,3,3,3,4),(1.73472347597681E-18,2.57218162001682E-5,4.21568322567692E-5,
6.45873314616974E-5,7.58025810641615E-5,8.14102058653936E-5,8.28121120657016E-5,
8.70178306666256E-5,0.000116081955658883,0.000130526745999938,0.000162394111022063,
0.00017403566133325,0.000213138396957746,0.000256116935432846,0.000302406662854858,
0.000348071322666484),.UNSPECIFIED.);
#5090=B_SPLINE_CURVE_WITH_KNOTS('',3,(#234512,#234513,#234514,#234515,#234516,
#234517,#234518,#234519,#234520,#234521,#234522,#234523,#234524,#234525,
#234526,#234527,#234528,#234529,#234530,#234531,#234532,#234533,#234534,
#234535,#234536,#234537,#234538,#234539,#234540,#234541,#234542,#234543,
#234544,#234545,#234546,#234547,#234548,#234549,#234550,#234551,#234552,
#234553,#234554,#234555,#234556,#234557,#234558,#234559,#234560,#234561,
#234562,#234563),.UNSPECIFIED.,.F.,.F.,(4,3,3,3,3,3,3,3,3,3,3,3,3,3,3,3,
3,4),(4.33680868994202E-19,4.29652152122471E-5,8.44519107475262E-5,0.000123669830858404,
0.000159788877351739,0.000170558847912622,0.000181218775907162,0.000181960046452396,
0.000214460062643998,0.00024475572619965,0.000255838271868939,0.000258503253867574,
0.000261084955178751,0.000289370476647007,0.000301101325502003,0.000321109510663629,
0.000331113603244442,0.000341117695825255),.UNSPECIFIED.);
#5091=B_SPLINE_CURVE_WITH_KNOTS('',3,(#234565,#234566,#234567,#234568,#234569,
#234570,#234571,#234572,#234573,#234574,#234575,#234576,#234577,#234578,
#234579,#234580,#234581,#234582,#234583,#234584,#234585,#234586,#234587,
#234588,#234589,#234590,#234591,#234592,#234593,#234594,#234595,#234596,
#234597,#234598,#234599,#234600,#234601,#234602,#234603,#234604,#234605,
#234606,#234607,#234608,#234609,#234610,#234611,#234612,#234613,#234614,
#234615,#234616),.UNSPECIFIED.,.F.,.F.,(4,3,3,3,3,3,3,3,3,3,3,3,3,3,3,3,
3,4),(4.33680868994202E-19,4.30706237874098E-5,8.47417087703705E-5,0.000124159989206565,
0.000160467076290862,0.000170998382116692,0.000182414994733768,0.000213747977645868,
0.000242415955904643,0.000256497573175044,0.000259169422895618,0.000261757777312423,
0.000289965130402133,0.000301877270772906,0.000321937017503148,0.000326951954185708,
0.000334474359209549,0.000341996764233389),.UNSPECIFIED.);
#5092=B_SPLINE_CURVE_WITH_KNOTS('',3,(#234617,#234618,#234619,#234620,#234621,
#234622,#234623,#234624,#234625,#234626,#234627,#234628,#234629,#234630,
#234631,#234632,#234633,#234634,#234635,#234636,#234637,#234638,#234639,
#234640,#234641,#234642,#234643,#234644,#234645,#234646,#234647,#234648,
#234649,#234650,#234651,#234652,#234653,#234654,#234655,#234656,#234657,
#234658,#234659,#234660,#234661,#234662,#234663,#234664,#234665,#234666,
#234667,#234668),.UNSPECIFIED.,.F.,.F.,(4,3,3,3,3,3,3,3,3,3,3,3,3,3,3,3,
3,4),(0.,2.58457451681173E-5,4.25394446196654E-5,6.46659869687525E-5,7.5729258143296E-5,
8.12608937305678E-5,8.26438026273857E-5,8.67925293178395E-5,0.00011601562442695,
0.000130188793976759,0.000151886926306219,0.000161963651211275,0.000162735992470949,
0.000173585058635679,0.00021248788045979,0.00025523817350832,0.000301397761139514,
0.000347170117271359),.UNSPECIFIED.);
#5093=B_SPLINE_CURVE_WITH_KNOTS('',3,(#234670,#234671,#234672,#234673,#234674,
#234675,#234676,#234677,#234678,#234679,#234680,#234681,#234682,#234683,
#234684,#234685,#234686,#234687,#234688,#234689,#234690,#234691,#234692,
#234693,#234694,#234695,#234696,#234697,#234698,#234699,#234700,#234701,
#234702,#234703,#234704,#234705,#234706,#234707,#234708,#234709,#234710,
#234711,#234712,#234713,#234714,#234715),.UNSPECIFIED.,.F.,.F.,(4,3,3,3,
3,3,3,3,3,3,3,3,3,3,3,4),(1.73472347597681E-18,2.57218161991517E-5,4.21568322568403E-5,
6.45873314617371E-5,7.58025810641855E-5,8.14102058654097E-5,8.28121120657157E-5,
8.70178306666339E-5,0.000116081955658399,0.00013052674599995,0.000162394111022071,
0.000174035661333266,0.000213138396959586,0.000256116935436441,0.000302406662860196,
0.000348071322666516),.UNSPECIFIED.);
#5094=B_SPLINE_CURVE_WITH_KNOTS('',3,(#234716,#234717,#234718,#234719,#234720,
#234721,#234722,#234723,#234724,#234725,#234726,#234727,#234728,#234729,
#234730,#234731,#234732,#234733,#234734,#234735,#234736,#234737,#234738,
#234739,#234740,#234741,#234742,#234743,#234744,#234745,#234746,#234747,
#234748,#234749,#234750,#234751,#234752,#234753,#234754,#234755,#234756,
#234757,#234758,#234759,#234760,#234761,#234762,#234763,#234764,#234765,
#234766,#234767),.UNSPECIFIED.,.F.,.F.,(4,3,3,3,3,3,3,3,3,3,3,3,3,3,3,3,
3,4),(4.33680868994202E-19,4.29652152179851E-5,8.44519107563622E-5,0.000123669830868358,
0.000159788877361452,0.000170558847912632,0.000181218775907171,0.00018196004645241,
0.000214460062643803,0.00024475572619926,0.000255838271868948,0.000258503253867583,
0.000261084955178761,0.000289370476647563,0.000301101325502013,0.000321109510663639,
0.000331113603244452,0.000341117695825265),.UNSPECIFIED.);
#5095=B_SPLINE_CURVE_WITH_KNOTS('',3,(#234769,#234770,#234771,#234772,#234773,
#234774,#234775,#234776,#234777,#234778,#234779,#234780,#234781,#234782,
#234783,#234784,#234785,#234786,#234787,#234788,#234789,#234790,#234791,
#234792,#234793,#234794,#234795,#234796,#234797,#234798,#234799,#234800,
#234801,#234802,#234803,#234804,#234805,#234806,#234807,#234808,#234809,
#234810,#234811,#234812,#234813,#234814,#234815,#234816,#234817,#234818,
#234819,#234820),.UNSPECIFIED.,.F.,.F.,(4,3,3,3,3,3,3,3,3,3,3,3,3,3,3,3,
3,4),(0.,4.30706237861595E-5,8.4741708768375E-5,0.000124159989204126,0.000160467076288123,
0.000170998382116677,0.000182414994733771,0.000213747977645853,0.000242415955903301,
0.000256497573175029,0.000259169422895603,0.000261757777312408,0.000289965130402838,
0.000301877270772894,0.000321937017503137,0.000326951954185698,0.000334474359209539,
0.000341996764233381),.UNSPECIFIED.);
#5096=B_SPLINE_CURVE_WITH_KNOTS('',3,(#234821,#234822,#234823,#234824,#234825,
#234826,#234827,#234828,#234829,#234830,#234831,#234832,#234833,#234834,
#234835,#234836,#234837,#234838,#234839,#234840,#234841,#234842,#234843,
#234844,#234845,#234846,#234847,#234848,#234849,#234850,#234851,#234852,
#234853,#234854,#234855,#234856,#234857,#234858,#234859,#234860,#234861,
#234862,#234863,#234864,#234865,#234866,#234867,#234868,#234869,#234870,
#234871,#234872),.UNSPECIFIED.,.F.,.F.,(4,3,3,3,3,3,3,3,3,3,3,3,3,3,3,3,
3,4),(0.,2.58457451685323E-5,4.25394446196102E-5,6.46659869687251E-5,7.57292581432825E-5,
8.12608937305612E-5,8.26438026273809E-5,8.679252931784E-5,0.000116015624427535,
0.00013018879397676,0.00015188692630622,0.000161963651211282,0.00016273599247095,
0.00017358505863568,0.000212487880460561,0.000255238173511503,0.000301397761148276,
0.000347170117271346),.UNSPECIFIED.);
#5097=B_SPLINE_CURVE_WITH_KNOTS('',3,(#234874,#234875,#234876,#234877,#234878,
#234879,#234880,#234881,#234882,#234883,#234884,#234885,#234886,#234887,
#234888,#234889,#234890,#234891,#234892,#234893,#234894,#234895,#234896,
#234897,#234898,#234899,#234900,#234901,#234902,#234903,#234904,#234905,
#234906,#234907,#234908,#234909,#234910,#234911,#234912,#234913,#234914,
#234915,#234916,#234917,#234918,#234919),.UNSPECIFIED.,.F.,.F.,(4,3,3,3,
3,3,3,3,3,3,3,3,3,3,3,4),(5.48877349820787E-19,2.57218161988899E-5,4.21568322568674E-5,
6.45873314617467E-5,7.58025810641863E-5,8.14102058654061E-5,8.28121120657111E-5,
8.70178306666259E-5,0.000116081955658109,0.000130526745999939,0.000162394111022064,
0.000174035661333251,0.000213138396957216,0.000256116935431698,0.000302406662852769,
0.000348071322666503),.UNSPECIFIED.);
#5098=B_SPLINE_CURVE_WITH_KNOTS('',3,(#234920,#234921,#234922,#234923,#234924,
#234925,#234926,#234927,#234928,#234929,#234930,#234931,#234932,#234933,
#234934,#234935,#234936,#234937,#234938,#234939,#234940,#234941,#234942,
#234943,#234944,#234945,#234946,#234947,#234948,#234949,#234950,#234951,
#234952,#234953,#234954,#234955,#234956,#234957,#234958,#234959,#234960,
#234961,#234962,#234963,#234964,#234965,#234966,#234967,#234968,#234969,
#234970,#234971),.UNSPECIFIED.,.F.,.F.,(4,3,3,3,3,3,3,3,3,3,3,3,3,3,3,3,
3,4),(0.,4.29652152139708E-5,8.44519107499793E-5,0.000123669830860699,0.000159788877353224,
0.00017055884791263,0.000181218775907169,0.000181960046452404,0.000214460062643146,
0.000244755726197271,0.000255838271868945,0.00025850325386758,0.000261084955178757,
0.000289370476648699,0.000301101325502009,0.000321109510663634,0.000331113603244447,
0.00034111769582526),.UNSPECIFIED.);
#5099=B_SPLINE_CURVE_WITH_KNOTS('',3,(#234973,#234974,#234975,#234976,#234977,
#234978,#234979,#234980,#234981,#234982,#234983,#234984,#234985,#234986,
#234987,#234988,#234989,#234990,#234991,#234992,#234993,#234994,#234995,
#234996,#234997,#234998,#234999,#235000,#235001,#235002,#235003,#235004,
#235005,#235006,#235007,#235008,#235009,#235010,#235011,#235012,#235013,
#235014,#235015,#235016,#235017,#235018,#235019,#235020,#235021,#235022,
#235023,#235024),.UNSPECIFIED.,.F.,.F.,(4,3,3,3,3,3,3,3,3,3,3,3,3,3,3,3,
3,4),(9.85133562538035E-18,4.30706237881605E-5,8.47417087718283E-5,0.000124159989208858,
0.0001604670762942,0.000170998382116695,0.000182414994733785,0.000213747977645867,
0.000242415955903381,0.000256497573175038,0.000259169422895612,0.000261757777312417,
0.00028996513040321,0.000301877270772899,0.00032193701750314,0.000326951954185701,
0.000334474359209541,0.000341996764233381),.UNSPECIFIED.);
#5100=B_SPLINE_CURVE_WITH_KNOTS('',3,(#235025,#235026,#235027,#235028,#235029,
#235030,#235031,#235032,#235033,#235034,#235035,#235036,#235037,#235038,
#235039,#235040,#235041,#235042,#235043,#235044,#235045,#235046,#235047,
#235048,#235049,#235050,#235051,#235052,#235053,#235054,#235055,#235056,
#235057,#235058,#235059,#235060,#235061,#235062,#235063,#235064,#235065,
#235066,#235067,#235068,#235069,#235070,#235071,#235072,#235073,#235074,
#235075,#235076),.UNSPECIFIED.,.F.,.F.,(4,3,3,3,3,3,3,3,3,3,3,3,3,3,3,3,
3,4),(0.,2.58457451672615E-5,4.25394446195262E-5,6.46659869686852E-5,7.57292581432647E-5,
8.12608937305545E-5,8.26438026273769E-5,8.67925293178442E-5,0.0001160156244269,
0.000130188793976766,0.000151886926306227,0.000161963651211279,0.000162735992470958,
0.000173585058635688,0.000212487880460214,0.000255238173510026,0.000301397761144323,
0.000347170117271377),.UNSPECIFIED.);
#5101=B_SPLINE_CURVE_WITH_KNOTS('',3,(#235078,#235079,#235080,#235081,#235082,
#235083,#235084,#235085,#235086,#235087,#235088,#235089,#235090,#235091,
#235092,#235093,#235094,#235095,#235096,#235097,#235098,#235099,#235100,
#235101,#235102,#235103,#235104,#235105,#235106,#235107,#235108,#235109,
#235110,#235111,#235112,#235113,#235114,#235115,#235116,#235117,#235118,
#235119,#235120,#235121,#235122,#235123),.UNSPECIFIED.,.F.,.F.,(4,3,3,3,
3,3,3,3,3,3,3,3,3,3,3,4),(8.67361737988403E-19,2.57218161987776E-5,4.21568322567847E-5,
6.45873314617043E-5,7.58025810641641E-5,8.1410205865394E-5,8.28121120657015E-5,
8.7017830666624E-5,0.000116081955658135,0.000130526745999932,0.000162394111022062,
0.000174035661333239,0.000213138396959045,0.000256116935435313,0.000302406662858188,
0.000348071322666484),.UNSPECIFIED.);
#5102=B_SPLINE_CURVE_WITH_KNOTS('',3,(#235124,#235125,#235126,#235127,#235128,
#235129,#235130,#235131,#235132,#235133,#235134,#235135,#235136,#235137,
#235138,#235139,#235140,#235141,#235142,#235143,#235144,#235145,#235146,
#235147,#235148,#235149,#235150,#235151,#235152,#235153,#235154,#235155,
#235156,#235157,#235158,#235159,#235160,#235161,#235162,#235163,#235164,
#235165,#235166,#235167,#235168,#235169,#235170,#235171,#235172,#235173,
#235174,#235175),.UNSPECIFIED.,.F.,.F.,(4,3,3,3,3,3,3,3,3,3,3,3,3,3,3,3,
3,4),(0.,4.29652152157613E-5,8.44519107527578E-5,0.000123669830863927,0.000159788877356499,
0.000170558847912623,0.000181218775907163,0.000181960046452398,0.000214460062643952,
0.00024475572619948,0.000255838271868942,0.000258503253867577,0.000261084955178755,
0.000289370476647228,0.000301101325502008,0.000321109510663634,0.000331113603244447,
0.000341117695825261),.UNSPECIFIED.);
#5103=B_SPLINE_CURVE_WITH_KNOTS('',3,(#235177,#235178,#235179,#235180,#235181,
#235182,#235183,#235184,#235185,#235186,#235187,#235188,#235189,#235190,
#235191,#235192,#235193,#235194,#235195,#235196,#235197,#235198,#235199,
#235200,#235201,#235202,#235203,#235204,#235205,#235206,#235207,#235208,
#235209,#235210,#235211,#235212,#235213,#235214,#235215,#235216,#235217,
#235218,#235219,#235220,#235221,#235222,#235223,#235224,#235225,#235226,
#235227,#235228),.UNSPECIFIED.,.F.,.F.,(4,3,3,3,3,3,3,3,3,3,3,3,3,3,3,3,
3,4),(3.03576608295941E-18,4.30706237875898E-5,8.47417087709076E-5,0.000124159989207655,
0.000160467076292736,0.000170998382116693,0.000182414994733774,0.000213747977645865,
0.000242415955903445,0.000256497573175038,0.000259169422895611,0.000261757777312417,
0.000289965130403454,0.0003018772707729,0.000321937017503142,0.000326951954185703,
0.000334474359209543,0.000341996764233384),.UNSPECIFIED.);
#5104=B_SPLINE_CURVE_WITH_KNOTS('',3,(#235229,#235230,#235231,#235232,#235233,
#235234,#235235,#235236,#235237,#235238,#235239,#235240,#235241,#235242,
#235243,#235244,#235245,#235246,#235247,#235248,#235249,#235250,#235251,
#235252,#235253,#235254,#235255,#235256,#235257,#235258,#235259,#235260,
#235261,#235262,#235263,#235264,#235265,#235266,#235267,#235268,#235269,
#235270,#235271,#235272,#235273,#235274,#235275,#235276,#235277,#235278,
#235279,#235280),.UNSPECIFIED.,.F.,.F.,(4,3,3,3,3,3,3,3,3,3,3,3,3,3,3,3,
3,4),(0.,2.58457451669222E-5,4.25394446196541E-5,6.46659869687471E-5,7.57292581432935E-5,
8.12608937305668E-5,8.26438026273851E-5,8.679252931784E-5,0.000116015624426832,
0.00013018879397676,0.00015188692630622,0.000161963651211278,0.00016273599247095,
0.00017358505863568,0.00021248788046056,0.000255238173511179,0.000301397761147054,
0.000347170117271364),.UNSPECIFIED.);
#5105=B_SPLINE_CURVE_WITH_KNOTS('',3,(#235282,#235283,#235284,#235285,#235286,
#235287,#235288,#235289,#235290,#235291,#235292,#235293,#235294,#235295,
#235296,#235297,#235298,#235299,#235300,#235301,#235302,#235303,#235304,
#235305,#235306,#235307,#235308,#235309,#235310,#235311,#235312,#235313,
#235314,#235315,#235316,#235317,#235318,#235319,#235320,#235321,#235322,
#235323,#235324,#235325,#235326,#235327),.UNSPECIFIED.,.F.,.F.,(4,3,3,3,
3,3,3,3,3,3,3,3,3,3,3,4),(0.,2.57218162009012E-5,4.21568322567646E-5,6.45873314616925E-5,
7.58025810641564E-5,8.14102058653884E-5,8.28121120656964E-5,8.70178306666204E-5,
0.000116081955658897,0.000130526745999931,0.000162394111022045,0.000174035661333241,
0.000213138396957201,0.000256116935431684,0.000302406662852778,0.000348071322666473),
 .UNSPECIFIED.);
#5106=B_SPLINE_CURVE_WITH_KNOTS('',3,(#235328,#235329,#235330,#235331,#235332,
#235333,#235334,#235335,#235336,#235337,#235338,#235339,#235340,#235341,
#235342,#235343,#235344,#235345,#235346,#235347,#235348,#235349,#235350,
#235351,#235352,#235353,#235354,#235355,#235356,#235357,#235358,#235359,
#235360,#235361,#235362,#235363,#235364,#235365,#235366,#235367,#235368,
#235369,#235370,#235371,#235372,#235373,#235374,#235375,#235376,#235377,
#235378,#235379),.UNSPECIFIED.,.F.,.F.,(4,3,3,3,3,3,3,3,3,3,3,3,3,3,3,3,
3,4),(0.,4.29652152152673E-5,8.44519107521068E-5,0.000123669830863404,0.000159788877356394,
0.000170558847912628,0.000181218775907168,0.000181960046452405,0.000214460062643706,
0.000244755726199078,0.000255838271868944,0.000258503253867578,0.000261084955178756,
0.000289370476647239,0.000301101325502007,0.000321109510663633,0.000331113603244446,
0.000341117695825259),.UNSPECIFIED.);
#5107=B_SPLINE_CURVE_WITH_KNOTS('',3,(#235381,#235382,#235383,#235384,#235385,
#235386,#235387,#235388,#235389,#235390,#235391,#235392,#235393,#235394,
#235395,#235396,#235397,#235398,#235399,#235400,#235401,#235402,#235403,
#235404,#235405,#235406,#235407,#235408,#235409,#235410,#235411,#235412,
#235413,#235414,#235415,#235416,#235417,#235418,#235419,#235420,#235421,
#235422,#235423,#235424,#235425,#235426,#235427,#235428,#235429,#235430,
#235431,#235432),.UNSPECIFIED.,.F.,.F.,(4,3,3,3,3,3,3,3,3,3,3,3,3,3,3,3,
3,4),(3.03576608295941E-18,4.30706237872071E-5,8.474170877004E-5,0.00012415998920614,
0.000160467076290401,0.000170998382116706,0.000182414994733797,0.000213747977645878,
0.000242415955903907,0.000256497573175049,0.000259169422895622,0.000261757777312428,
0.000289965130403662,0.00030187727077291,0.000321937017503151,0.000326951954185711,
0.000334474359209552,0.000341996764233392),.UNSPECIFIED.);
#5108=B_SPLINE_CURVE_WITH_KNOTS('',3,(#235433,#235434,#235435,#235436,#235437,
#235438,#235439,#235440,#235441,#235442,#235443,#235444,#235445,#235446,
#235447,#235448,#235449,#235450,#235451,#235452,#235453,#235454,#235455,
#235456,#235457,#235458,#235459,#235460,#235461,#235462,#235463,#235464,
#235465,#235466,#235467,#235468,#235469,#235470,#235471,#235472,#235473,
#235474,#235475,#235476,#235477,#235478,#235479,#235480,#235481,#235482,
#235483,#235484),.UNSPECIFIED.,.F.,.F.,(4,3,3,3,3,3,3,3,3,3,3,3,3,3,3,3,
3,4),(0.,2.58457451681574E-5,4.2539444619624E-5,6.46659869687327E-5,7.5729258143287E-5,
8.12608937305642E-5,8.26438026273834E-5,8.67925293178413E-5,0.000116015624427458,
0.000130188793976762,0.000151886926306222,0.000161963651211265,0.000162735992470952,
0.000173585058635683,0.000212487880461666,0.000255238173513071,0.000301397761149064,
0.000347170117271372),.UNSPECIFIED.);
#5109=B_SPLINE_CURVE_WITH_KNOTS('',3,(#235486,#235487,#235488,#235489,#235490,
#235491,#235492,#235493,#235494,#235495,#235496,#235497,#235498,#235499,
#235500,#235501,#235502,#235503,#235504,#235505,#235506,#235507,#235508,
#235509,#235510,#235511,#235512,#235513,#235514,#235515,#235516,#235517,
#235518,#235519,#235520,#235521,#235522,#235523,#235524,#235525,#235526,
#235527,#235528,#235529,#235530,#235531),.UNSPECIFIED.,.F.,.F.,(4,3,3,3,
3,3,3,3,3,3,3,3,3,3,3,4),(0.,2.57218161989481E-5,4.21568322568538E-5,6.45873314617329E-5,
7.58025810641724E-5,8.14102058653922E-5,8.28121120656971E-5,8.7017830666612E-5,
0.000116081955658189,0.000130526745999918,0.000162394111022038,0.000174035661333224,
0.000213138396958885,0.000256116935435022,0.000302406662857814,0.00034807132266645),
 .UNSPECIFIED.);
#5110=B_SPLINE_CURVE_WITH_KNOTS('',3,(#235532,#235533,#235534,#235535,#235536,
#235537,#235538,#235539,#235540,#235541,#235542,#235543,#235544,#235545,
#235546,#235547,#235548,#235549,#235550,#235551,#235552,#235553,#235554,
#235555,#235556,#235557,#235558,#235559,#235560,#235561,#235562,#235563,
#235564,#235565,#235566,#235567,#235568,#235569,#235570,#235571,#235572,
#235573,#235574,#235575,#235576,#235577,#235578,#235579,#235580,#235581,
#235582,#235583),.UNSPECIFIED.,.F.,.F.,(4,3,3,3,3,3,3,3,3,3,3,3,3,3,3,3,
3,4),(4.33680868994202E-19,4.2965215221666E-5,8.44519107623575E-5,0.000123669830875747,
0.000159788877369812,0.000170558847912634,0.000181218775907173,0.000181960046452406,
0.00021446006264371,0.00024475572619867,0.000255838271868942,0.000258503253867577,
0.000261084955178754,0.000289370476647226,0.000301101325502002,0.000321109510663626,
0.000331113603244438,0.00034111769582525),.UNSPECIFIED.);
#5111=B_SPLINE_CURVE_WITH_KNOTS('',3,(#235585,#235586,#235587,#235588,#235589,
#235590,#235591,#235592,#235593,#235594,#235595,#235596,#235597,#235598,
#235599,#235600,#235601,#235602,#235603,#235604,#235605,#235606,#235607,
#235608,#235609,#235610,#235611,#235612,#235613,#235614,#235615,#235616,
#235617,#235618,#235619,#235620,#235621,#235622,#235623,#235624,#235625,
#235626,#235627,#235628,#235629,#235630,#235631,#235632,#235633,#235634,
#235635,#235636),.UNSPECIFIED.,.F.,.F.,(4,3,3,3,3,3,3,3,3,3,3,3,3,3,3,3,
3,4),(0.,4.30706237877873E-5,8.47417087710622E-5,0.000124159989207586,0.000160467076292239,
0.000170998382116696,0.000182414994733785,0.000213747977645869,0.000242415955902956,
0.000256497573175042,0.000259169422895616,0.000261757777312421,0.000289965130403431,
0.000301877270772905,0.000321937017503147,0.000326951954185708,0.000334474359209548,
0.000341996764233389),.UNSPECIFIED.);
#5112=B_SPLINE_CURVE_WITH_KNOTS('',3,(#235637,#235638,#235639,#235640,#235641,
#235642,#235643,#235644,#235645,#235646,#235647,#235648,#235649,#235650,
#235651,#235652,#235653,#235654,#235655,#235656,#235657,#235658,#235659,
#235660,#235661,#235662,#235663,#235664,#235665,#235666,#235667,#235668,
#235669,#235670,#235671,#235672,#235673,#235674,#235675,#235676,#235677,
#235678,#235679,#235680,#235681,#235682,#235683,#235684,#235685,#235686,
#235687,#235688),.UNSPECIFIED.,.F.,.F.,(4,3,3,3,3,3,3,3,3,3,3,3,3,3,3,3,
3,4),(0.,2.58457451676357E-5,4.25394446196733E-5,6.46659869687554E-5,7.57292581432964E-5,
8.1260893730567E-5,8.26438026273846E-5,8.67925293178375E-5,0.000116015624426936,
0.000130188793976756,0.000151886926306216,0.000161963651211277,0.000162735992470945,
0.000173585058635675,0.000212487880461714,0.000255238173514346,0.00030139776115405,
0.000347170117271358),.UNSPECIFIED.);
#5113=B_SPLINE_CURVE_WITH_KNOTS('',3,(#235690,#235691,#235692,#235693,#235694,
#235695,#235696,#235697,#235698,#235699,#235700,#235701,#235702,#235703,
#235704,#235705,#235706,#235707,#235708,#235709,#235710,#235711,#235712,
#235713,#235714,#235715,#235716,#235717,#235718,#235719,#235720,#235721,
#235722,#235723,#235724,#235725,#235726,#235727,#235728,#235729,#235730,
#235731,#235732,#235733,#235734,#235735),.UNSPECIFIED.,.F.,.F.,(4,3,3,3,
3,3,3,3,3,3,3,3,3,3,3,4),(3.46944695195361E-18,2.57218162006677E-5,4.2156832256807E-5,
6.45873314617123E-5,7.5802581064165E-5,8.14102058653913E-5,8.28121120656978E-5,
8.70178306666176E-5,0.000116081955659339,0.000130526745999925,0.000162394111022045,
0.000174035661333232,0.000213138396960436,0.000256116935438212,0.000302406662863133,
0.00034807132266646),.UNSPECIFIED.);
#5114=B_SPLINE_CURVE_WITH_KNOTS('',3,(#235736,#235737,#235738,#235739,#235740,
#235741,#235742,#235743,#235744,#235745,#235746,#235747,#235748,#235749,
#235750,#235751,#235752,#235753,#235754,#235755,#235756,#235757,#235758,
#235759,#235760,#235761,#235762,#235763,#235764,#235765,#235766,#235767,
#235768,#235769,#235770,#235771,#235772,#235773,#235774,#235775,#235776,
#235777,#235778,#235779,#235780,#235781,#235782,#235783,#235784,#235785,
#235786,#235787),.UNSPECIFIED.,.F.,.F.,(4,3,3,3,3,3,3,3,3,3,3,3,3,3,3,3,
3,4),(0.,4.29652152160775E-5,8.44519107533754E-5,0.000123669830864951,0.00015978887735793,
0.000170558847912619,0.000181218775907159,0.000181960046452398,0.000214460062643413,
0.000244755726197593,0.000255838271868937,0.000258503253867572,0.00026108495517875,
0.000289370476648662,0.000301101325502003,0.000321109510663629,0.000331113603244443,
0.000341117695825256),.UNSPECIFIED.);
#5115=B_SPLINE_CURVE_WITH_KNOTS('',3,(#235789,#235790,#235791,#235792,#235793,
#235794,#235795,#235796,#235797,#235798,#235799,#235800,#235801,#235802,
#235803,#235804,#235805,#235806,#235807,#235808,#235809,#235810,#235811,
#235812,#235813,#235814,#235815,#235816,#235817,#235818,#235819,#235820,
#235821,#235822,#235823,#235824,#235825,#235826,#235827,#235828,#235829,
#235830,#235831,#235832,#235833,#235834,#235835,#235836,#235837,#235838,
#235839,#235840),.UNSPECIFIED.,.F.,.F.,(4,3,3,3,3,3,3,3,3,3,3,3,3,3,3,3,
3,4),(0.,4.30706237882173E-5,8.47417087719784E-5,0.000124159989209114,0.000160467076294534,
0.000170998382116702,0.000182414994733779,0.000213747977645877,0.0002424159559042,
0.000256497573175052,0.000259169422895626,0.000261757777312431,0.000289965130403038,
0.000301877270772917,0.00032193701750316,0.000326951954185721,0.000334474359209562,
0.000341996764233403),.UNSPECIFIED.);
#5116=B_SPLINE_CURVE_WITH_KNOTS('',3,(#235841,#235842,#235843,#235844,#235845,
#235846,#235847,#235848,#235849,#235850,#235851,#235852,#235853,#235854,
#235855,#235856,#235857,#235858,#235859,#235860,#235861,#235862,#235863,
#235864,#235865,#235866,#235867,#235868,#235869,#235870,#235871,#235872,
#235873,#235874,#235875,#235876,#235877,#235878,#235879,#235880,#235881,
#235882,#235883,#235884,#235885,#235886,#235887,#235888,#235889,#235890,
#235891,#235892),.UNSPECIFIED.,.F.,.F.,(4,3,3,3,3,3,3,3,3,3,3,3,3,3,3,3,
3,4),(0.,2.58457451679575E-5,4.25394446196678E-5,6.46659869687542E-5,7.57292581432974E-5,
8.1260893730569E-5,8.26438026273869E-5,8.67925293178406E-5,0.000116015624427285,
0.000130188793976761,0.000151886926306221,0.000161963651211261,0.000162735992470951,
0.000173585058635681,0.000212487880457631,0.000255238173503925,0.000301397761132213,
0.000347170117271364),.UNSPECIFIED.);
#5117=B_SPLINE_CURVE_WITH_KNOTS('',3,(#235894,#235895,#235896,#235897,#235898,
#235899,#235900,#235901,#235902,#235903,#235904,#235905,#235906,#235907,
#235908,#235909,#235910,#235911,#235912,#235913,#235914,#235915,#235916,
#235917,#235918,#235919,#235920,#235921,#235922,#235923,#235924,#235925,
#235926,#235927,#235928,#235929,#235930,#235931,#235932,#235933,#235934,
#235935,#235936,#235937,#235938,#235939),.UNSPECIFIED.,.F.,.F.,(4,3,3,3,
3,3,3,3,3,3,3,3,3,3,3,4),(0.,2.57218161982287E-5,4.21568322568021E-5,6.45873314617112E-5,
7.58025810641658E-5,8.1410205865393E-5,8.28121120656999E-5,8.70178306666203E-5,
0.000116081955657987,0.00013052674599993,0.000162394111022054,0.000174035661333241,
0.000213138396958526,0.000256116935434306,0.00030240666285673,0.000348071322666488),
 .UNSPECIFIED.);
#5118=B_SPLINE_CURVE_WITH_KNOTS('',3,(#235940,#235941,#235942,#235943,#235944,
#235945,#235946,#235947,#235948,#235949,#235950,#235951,#235952,#235953,
#235954,#235955,#235956,#235957,#235958,#235959,#235960,#235961,#235962,
#235963,#235964,#235965,#235966,#235967,#235968,#235969,#235970,#235971,
#235972,#235973,#235974,#235975,#235976,#235977,#235978,#235979,#235980,
#235981,#235982,#235983,#235984,#235985,#235986,#235987,#235988,#235989,
#235990,#235991),.UNSPECIFIED.,.F.,.F.,(4,3,3,3,3,3,3,3,3,3,3,3,3,3,3,3,
3,4),(2.16840434497101E-18,4.29652152152268E-5,8.44519107520661E-5,0.00012366983086337,
0.000159788877356357,0.000170558847912644,0.000181218775907183,0.000181960046452433,
0.000214460062643565,0.000244755726198341,0.000255838271868955,0.00025850325386759,
0.000261084955178768,0.000289370476647945,0.000301101325502017,0.000321109510663642,
0.000331113603244455,0.000341117695825267),.UNSPECIFIED.);
#5119=B_SPLINE_CURVE_WITH_KNOTS('',3,(#235993,#235994,#235995,#235996,#235997,
#235998,#235999,#236000,#236001,#236002,#236003,#236004,#236005,#236006,
#236007,#236008,#236009,#236010,#236011,#236012,#236013,#236014,#236015,
#236016,#236017,#236018,#236019,#236020,#236021,#236022,#236023,#236024,
#236025,#236026,#236027,#236028,#236029,#236030,#236031,#236032,#236033,
#236034,#236035,#236036,#236037,#236038,#236039,#236040,#236041,#236042,
#236043,#236044),.UNSPECIFIED.,.F.,.F.,(4,3,3,3,3,3,3,3,3,3,3,3,3,3,3,3,
3,4),(0.,4.30706237861587E-5,8.47417087681614E-5,0.000124159989203496,0.000160467076286933,
0.000170998382116704,0.000182414994733766,0.000213747977645876,0.000242415955903066,
0.000256497573175048,0.000259169422895621,0.000261757777312426,0.00028996513040416,
0.000301877270772909,0.00032193701750315,0.000326951954185711,0.000334474359209551,
0.000341996764233392),.UNSPECIFIED.);
#5120=B_SPLINE_CURVE_WITH_KNOTS('',3,(#236045,#236046,#236047,#236048,#236049,
#236050,#236051,#236052,#236053,#236054,#236055,#236056,#236057,#236058,
#236059,#236060,#236061,#236062,#236063,#236064,#236065,#236066,#236067,
#236068,#236069,#236070,#236071,#236072,#236073,#236074,#236075,#236076,
#236077,#236078,#236079,#236080,#236081,#236082,#236083,#236084,#236085,
#236086,#236087,#236088,#236089,#236090,#236091,#236092,#236093,#236094,
#236095,#236096),.UNSPECIFIED.,.F.,.F.,(4,3,3,3,3,3,3,3,3,3,3,3,3,3,3,3,
3,4),(0.,2.58457451684377E-5,4.25394446196284E-5,6.46659869687342E-5,7.57292581432872E-5,
8.12608937305636E-5,8.26438026273828E-5,8.67925293178401E-5,0.000116015624426965,
0.00013018879397676,0.00015188692630622,0.000161963651211263,0.00016273599247095,
0.00017358505863568,0.000212487880458883,0.000255238173506548,0.000301397761136831,
0.00034717011727135),.UNSPECIFIED.);
#5121=B_SPLINE_CURVE_WITH_KNOTS('',3,(#236098,#236099,#236100,#236101,#236102,
#236103,#236104,#236105,#236106,#236107,#236108,#236109,#236110,#236111,
#236112,#236113,#236114,#236115,#236116,#236117,#236118,#236119,#236120,
#236121,#236122,#236123,#236124,#236125,#236126,#236127,#236128,#236129,
#236130,#236131,#236132,#236133,#236134,#236135,#236136,#236137,#236138,
#236139,#236140,#236141,#236142,#236143),.UNSPECIFIED.,.F.,.F.,(4,3,3,3,
3,3,3,3,3,3,3,3,3,3,3,4),(6.95243322195995E-18,2.57218161990052E-5,4.21568322569008E-5,
6.4587331461763E-5,7.58025810641941E-5,8.14102058654096E-5,8.28121120657135E-5,
8.70178306666252E-5,0.000116081955658842,0.000130526745999934,0.000162394111022056,
0.000174035661333243,0.000213138396957983,0.000256116935433331,0.000302406662855623,
0.00034807132266648),.UNSPECIFIED.);
#5122=B_SPLINE_CURVE_WITH_KNOTS('',3,(#236144,#236145,#236146,#236147,#236148,
#236149,#236150,#236151,#236152,#236153,#236154,#236155,#236156,#236157,
#236158,#236159,#236160,#236161,#236162,#236163,#236164,#236165,#236166,
#236167,#236168,#236169,#236170,#236171,#236172,#236173,#236174,#236175,
#236176,#236177,#236178,#236179,#236180,#236181,#236182,#236183,#236184,
#236185,#236186,#236187,#236188,#236189,#236190,#236191,#236192,#236193,
#236194,#236195),.UNSPECIFIED.,.F.,.F.,(4,3,3,3,3,3,3,3,3,3,3,3,3,3,3,3,
3,4),(0.,4.29652152188777E-5,8.44519107579093E-5,0.000123669830870508,0.000159788877364258,
0.000170558847912623,0.000181218775907162,0.000181960046452384,0.00021446006264357,
0.000244755726198643,0.000255838271868934,0.000258503253867569,0.000261084955178746,
0.000289370476649059,0.000301101325501996,0.00032110951066362,0.000331113603244433,
0.000341117695825245),.UNSPECIFIED.);
#5123=B_SPLINE_CURVE_WITH_KNOTS('',3,(#236197,#236198,#236199,#236200,#236201,
#236202,#236203,#236204,#236205,#236206,#236207,#236208,#236209,#236210,
#236211,#236212,#236213,#236214,#236215,#236216,#236217,#236218,#236219,
#236220,#236221,#236222,#236223,#236224,#236225,#236226,#236227,#236228,
#236229,#236230,#236231,#236232,#236233,#236234,#236235,#236236,#236237,
#236238,#236239,#236240,#236241,#236242,#236243,#236244,#236245,#236246,
#236247,#236248),.UNSPECIFIED.,.F.,.F.,(4,3,3,3,3,3,3,3,3,3,3,3,3,3,3,3,
3,4),(0.,4.30706237872035E-5,8.47417087699752E-5,0.000124159989205975,0.00016046707629009,
0.000170998382116686,0.000182414994733785,0.000213747977645861,0.000242415955903207,
0.000256497573175036,0.00025916942289561,0.000261757777312415,0.000289965130403885,
0.000301877270772901,0.000321937017503144,0.000326951954185705,0.000334474359209546,
0.000341996764233387),.UNSPECIFIED.);
#5124=B_SPLINE_CURVE_WITH_KNOTS('',3,(#236249,#236250,#236251,#236252,#236253,
#236254,#236255,#236256,#236257,#236258,#236259,#236260,#236261,#236262,
#236263,#236264,#236265,#236266,#236267,#236268,#236269,#236270,#236271,
#236272,#236273,#236274,#236275,#236276,#236277,#236278,#236279,#236280,
#236281,#236282,#236283,#236284,#236285,#236286,#236287,#236288,#236289,
#236290,#236291,#236292,#236293,#236294,#236295,#236296,#236297,#236298,
#236299,#236300),.UNSPECIFIED.,.F.,.F.,(4,3,3,3,3,3,3,3,3,3,3,3,3,3,3,3,
3,4),(0.,2.58457451676233E-5,4.25394446195383E-5,6.46659869686869E-5,7.57292581432612E-5,
8.12608937305484E-5,8.26438026273701E-5,8.67925293178355E-5,0.000116015624427426,
0.000130188793976753,0.000151886926306212,0.000161963651211271,0.000162735992470942,
0.000173585058635671,0.000212487880461207,0.000255238173513124,0.000301397761151479,
0.00034717011727136),.UNSPECIFIED.);
#5125=B_SPLINE_CURVE_WITH_KNOTS('',3,(#236302,#236303,#236304,#236305,#236306,
#236307,#236308,#236309,#236310,#236311,#236312,#236313,#236314,#236315,
#236316,#236317,#236318,#236319,#236320,#236321,#236322,#236323,#236324,
#236325,#236326,#236327,#236328,#236329,#236330,#236331,#236332,#236333,
#236334,#236335,#236336,#236337,#236338,#236339,#236340,#236341,#236342,
#236343,#236344,#236345,#236346,#236347),.UNSPECIFIED.,.F.,.F.,(4,3,3,3,
3,3,3,3,3,3,3,3,3,3,3,4),(0.,2.57218162000743E-5,4.21568322568328E-5,6.45873314617215E-5,
7.58025810641659E-5,8.14102058653881E-5,8.28121120656936E-5,8.70178306666103E-5,
0.000116081955658848,0.000130526745999915,0.000162394111022043,0.000174035661333221,
0.000213138396961521,0.000256116935440342,0.00030240666286625,0.000348071322666455),
 .UNSPECIFIED.);
#5126=B_SPLINE_CURVE_WITH_KNOTS('',3,(#236348,#236349,#236350,#236351,#236352,
#236353,#236354,#236355,#236356,#236357,#236358,#236359,#236360,#236361,
#236362,#236363,#236364,#236365,#236366,#236367,#236368,#236369,#236370,
#236371,#236372,#236373,#236374,#236375,#236376,#236377,#236378,#236379,
#236380,#236381,#236382,#236383,#236384,#236385,#236386,#236387,#236388,
#236389,#236390,#236391,#236392,#236393,#236394,#236395,#236396,#236397,
#236398,#236399),.UNSPECIFIED.,.F.,.F.,(4,3,3,3,3,3,3,3,3,3,3,3,3,3,3,3,
3,4),(1.30104260698261E-18,4.29652152171682E-5,8.4451910755208E-5,0.000123669830867249,
0.000159788877360641,0.000170558847912643,0.000181218775907182,0.000181960046452421,
0.000214460062643499,0.000244755726198127,0.000255838271868955,0.00025850325386759,
0.000261084955178767,0.000289370476646182,0.000301101325502018,0.000321109510663643,
0.000331113603244455,0.000341117695825268),.UNSPECIFIED.);
#5127=B_SPLINE_CURVE_WITH_KNOTS('',3,(#236401,#236402,#236403,#236404,#236405,
#236406,#236407,#236408,#236409,#236410,#236411,#236412,#236413,#236414,
#236415,#236416,#236417,#236418,#236419,#236420,#236421,#236422,#236423,
#236424,#236425,#236426,#236427,#236428,#236429,#236430,#236431,#236432,
#236433,#236434,#236435,#236436,#236437,#236438,#236439,#236440,#236441,
#236442,#236443,#236444,#236445,#236446,#236447,#236448,#236449,#236450,
#236451,#236452),.UNSPECIFIED.,.F.,.F.,(4,3,3,3,3,3,3,3,3,3,3,3,3,3,3,3,
3,4),(2.60208521396521E-18,4.30706237873492E-5,8.4741708770217E-5,0.000124159989206236,
0.000160467076290362,0.000170998382116704,0.000182414994733796,0.000213747977645875,
0.000242415955902185,0.000256497573175047,0.00025916942289562,0.000261757777312426,
0.000289965130404871,0.000301877270772908,0.000321937017503149,0.00032695195418571,
0.00033447435920955,0.000341996764233391),.UNSPECIFIED.);
#5128=B_SPLINE_CURVE_WITH_KNOTS('',3,(#236453,#236454,#236455,#236456,#236457,
#236458,#236459,#236460,#236461,#236462,#236463,#236464,#236465,#236466,
#236467,#236468,#236469,#236470,#236471,#236472,#236473,#236474,#236475,
#236476,#236477,#236478,#236479,#236480,#236481,#236482,#236483,#236484,
#236485,#236486,#236487,#236488,#236489,#236490,#236491,#236492,#236493,
#236494,#236495,#236496,#236497,#236498,#236499,#236500,#236501,#236502,
#236503,#236504),.UNSPECIFIED.,.F.,.F.,(4,3,3,3,3,3,3,3,3,3,3,3,3,3,3,3,
3,4),(0.,2.58457451673697E-5,4.25394446196103E-5,6.46659869687253E-5,7.57292581432827E-5,
8.12608937305615E-5,8.26438026273812E-5,8.67925293178402E-5,0.000116015624426797,
0.00013018879397676,0.00015188692630622,0.000161963651211268,0.00016273599247095,
0.00017358505863568,0.000212487880460138,0.000255238173509389,0.000301397761142022,
0.000347170117271361),.UNSPECIFIED.);
#5129=B_SPLINE_CURVE_WITH_KNOTS('',3,(#236506,#236507,#236508,#236509,#236510,
#236511,#236512,#236513,#236514,#236515,#236516,#236517,#236518,#236519,
#236520,#236521,#236522,#236523,#236524,#236525,#236526,#236527,#236528,
#236529,#236530,#236531,#236532,#236533,#236534,#236535,#236536,#236537,
#236538,#236539,#236540,#236541,#236542,#236543,#236544,#236545,#236546,
#236547,#236548,#236549,#236550,#236551),.UNSPECIFIED.,.F.,.F.,(4,3,3,3,
3,3,3,3,3,3,3,3,3,3,3,4),(0.,2.57218162001389E-5,4.21568322567862E-5,6.45873314617047E-5,
7.58025810641639E-5,8.14102058653935E-5,8.28121120657009E-5,8.70178306666231E-5,
0.00011608195565799,0.000130526745999935,0.000162394111022053,0.000174035661333246,
0.000213138396956027,0.000256116935429245,0.000302406662848675,0.000348071322666491),
 .UNSPECIFIED.);
#5130=B_SPLINE_CURVE_WITH_KNOTS('',3,(#236552,#236553,#236554,#236555,#236556,
#236557,#236558,#236559,#236560,#236561,#236562,#236563,#236564,#236565,
#236566,#236567,#236568,#236569,#236570,#236571,#236572,#236573,#236574,
#236575,#236576,#236577,#236578,#236579,#236580,#236581,#236582,#236583,
#236584,#236585,#236586,#236587,#236588,#236589,#236590,#236591,#236592,
#236593,#236594,#236595,#236596,#236597,#236598,#236599,#236600,#236601,
#236602,#236603),.UNSPECIFIED.,.F.,.F.,(4,3,3,3,3,3,3,3,3,3,3,3,3,3,3,3,
3,4),(0.,4.2965215217983E-5,8.44519107565792E-5,0.000123669830869106,0.000159788877362988,
0.000170558847912624,0.000181218775907164,0.000181960046452389,0.000214460062643136,
0.000244755726196858,0.000255838271868946,0.000258503253867581,0.000261084955178759,
0.000289370476648369,0.000301101325502013,0.00032110951066364,0.000331113603244454,
0.000341117695825268),.UNSPECIFIED.);
#5131=B_SPLINE_CURVE_WITH_KNOTS('',3,(#236605,#236606,#236607,#236608,#236609,
#236610,#236611,#236612,#236613,#236614,#236615,#236616,#236617,#236618,
#236619,#236620,#236621,#236622,#236623,#236624,#236625,#236626,#236627,
#236628,#236629,#236630,#236631,#236632,#236633,#236634,#236635,#236636,
#236637,#236638,#236639,#236640,#236641,#236642,#236643,#236644,#236645,
#236646,#236647,#236648,#236649,#236650,#236651,#236652,#236653,#236654,
#236655,#236656),.UNSPECIFIED.,.F.,.F.,(4,3,3,3,3,3,3,3,3,3,3,3,3,3,3,3,
3,4),(2.60208521396521E-18,4.30706237866639E-5,8.47417087690563E-5,0.000124159989204738,
0.000160467076288479,0.000170998382116689,0.000182414994733784,0.000213747977645866,
0.000242415955903435,0.000256497573175042,0.000259169422895616,0.000261757777312422,
0.000289965130402706,0.000301877270772909,0.000321937017503152,0.000326951954185713,
0.000334474359209554,0.000341996764233396),.UNSPECIFIED.);
#5132=B_SPLINE_CURVE_WITH_KNOTS('',3,(#236657,#236658,#236659,#236660,#236661,
#236662,#236663,#236664,#236665,#236666,#236667,#236668,#236669,#236670,
#236671,#236672,#236673,#236674,#236675,#236676,#236677,#236678,#236679,
#236680,#236681,#236682,#236683,#236684,#236685,#236686,#236687,#236688,
#236689,#236690,#236691,#236692,#236693,#236694,#236695,#236696,#236697,
#236698,#236699,#236700,#236701,#236702,#236703,#236704,#236705,#236706,
#236707,#236708),.UNSPECIFIED.,.F.,.F.,(4,3,3,3,3,3,3,3,3,3,3,3,3,3,3,3,
3,4),(0.,2.58457451681371E-5,4.25394446196679E-5,6.46659869687498E-5,7.57292581432907E-5,
8.12608937305612E-5,8.26438026273788E-5,8.67925293178317E-5,0.000116015624426802,
0.000130188793976748,0.000151886926306205,0.000161963651211261,0.000162735992470934,
0.000173585058635663,0.000212487880461001,0.000255238173511442,0.000301397761145844,
0.000347170117271343),.UNSPECIFIED.);
#5133=B_SPLINE_CURVE_WITH_KNOTS('',3,(#236710,#236711,#236712,#236713,#236714,
#236715,#236716,#236717,#236718,#236719,#236720,#236721,#236722,#236723,
#236724,#236725,#236726,#236727,#236728,#236729,#236730,#236731,#236732,
#236733,#236734,#236735,#236736,#236737,#236738,#236739,#236740,#236741,
#236742,#236743,#236744,#236745,#236746,#236747,#236748,#236749,#236750,
#236751,#236752,#236753,#236754,#236755),.UNSPECIFIED.,.F.,.F.,(4,3,3,3,
3,3,3,3,3,3,3,3,3,3,3,4),(0.,2.57218161995437E-5,4.21568322568779E-5,6.45873314617477E-5,
7.58025810641826E-5,8.14102058654001E-5,8.28121120657045E-5,8.70178306666175E-5,
0.000116081955658804,0.000130526745999926,0.000162394111022033,0.000174035661333235,
0.000213138396959203,0.000256116935435482,0.00030240666285809,0.00034807132266647),
 .UNSPECIFIED.);
#5134=B_SPLINE_CURVE_WITH_KNOTS('',3,(#236756,#236757,#236758,#236759,#236760,
#236761,#236762,#236763,#236764,#236765,#236766,#236767,#236768,#236769,
#236770,#236771,#236772,#236773,#236774,#236775,#236776,#236777,#236778,
#236779,#236780,#236781,#236782,#236783,#236784,#236785,#236786,#236787,
#236788,#236789,#236790,#236791,#236792,#236793,#236794,#236795,#236796,
#236797,#236798,#236799,#236800,#236801,#236802,#236803,#236804,#236805,
#236806,#236807),.UNSPECIFIED.,.F.,.F.,(4,3,3,3,3,3,3,3,3,3,3,3,3,3,3,3,
3,4),(0.,4.29652152188126E-5,8.44519107580872E-5,0.000123669830871332,0.000159788877365956,
0.000170558847912625,0.000181218775907165,0.000181960046452407,0.000214460062643281,
0.000244755726197407,0.000255838271868945,0.00025850325386758,0.000261084955178758,
0.000289370476647596,0.000301101325502011,0.000321109510663638,0.000331113603244452,
0.000341117695825265),.UNSPECIFIED.);
#5135=B_SPLINE_CURVE_WITH_KNOTS('',3,(#236809,#236810,#236811,#236812,#236813,
#236814,#236815,#236816,#236817,#236818,#236819,#236820,#236821,#236822,
#236823,#236824,#236825,#236826,#236827,#236828,#236829,#236830,#236831,
#236832,#236833,#236834,#236835,#236836,#236837,#236838,#236839,#236840,
#236841,#236842,#236843,#236844,#236845,#236846,#236847,#236848,#236849,
#236850,#236851,#236852,#236853,#236854,#236855,#236856,#236857,#236858,
#236859,#236860),.UNSPECIFIED.,.F.,.F.,(4,3,3,3,3,3,3,3,3,3,3,3,3,3,3,3,
3,4),(2.16840434497101E-18,4.30706237861116E-5,8.47417087683157E-5,0.000124159989204117,
0.000160467076288115,0.000170998382116709,0.000182414994733807,0.00021374797764588,
0.000242415955902621,0.000256497573175051,0.000259169422895624,0.00026175777731243,
0.000289965130403717,0.000301877270772911,0.000321937017503152,0.000326951954185712,
0.000334474359209553,0.000341996764233393),.UNSPECIFIED.);
#5136=B_SPLINE_CURVE_WITH_KNOTS('',3,(#236861,#236862,#236863,#236864,#236865,
#236866,#236867,#236868,#236869,#236870,#236871,#236872,#236873,#236874,
#236875,#236876,#236877,#236878,#236879,#236880,#236881,#236882,#236883,
#236884,#236885,#236886,#236887,#236888,#236889,#236890,#236891,#236892,
#236893,#236894,#236895,#236896,#236897,#236898,#236899,#236900,#236901,
#236902,#236903,#236904,#236905,#236906,#236907,#236908,#236909,#236910,
#236911,#236912),.UNSPECIFIED.,.F.,.F.,(4,3,3,3,3,3,3,3,3,3,3,3,3,3,3,3,
3,4),(0.,2.58457451676982E-5,4.2539444619647E-5,6.46659869687423E-5,7.57292581432899E-5,
8.12608937305638E-5,8.26438026273822E-5,8.67925293178376E-5,0.000116015624426779,
0.000130188793976756,0.000151886926306216,0.000161963651211259,0.000162735992470945,
0.000173585058635675,0.000212487880458101,0.000255238173504257,0.000301397761131382,
0.000347170117271351),.UNSPECIFIED.);
#5137=B_SPLINE_CURVE_WITH_KNOTS('',3,(#236914,#236915,#236916,#236917,#236918,
#236919,#236920,#236921,#236922,#236923,#236924,#236925,#236926,#236927,
#236928,#236929,#236930,#236931,#236932,#236933,#236934,#236935,#236936,
#236937,#236938,#236939,#236940,#236941,#236942,#236943,#236944,#236945,
#236946,#236947,#236948,#236949,#236950,#236951,#236952,#236953,#236954,
#236955,#236956,#236957,#236958,#236959),.UNSPECIFIED.,.F.,.F.,(4,3,3,3,
3,3,3,3,3,3,3,3,3,3,3,4),(0.,2.57218161988846E-5,4.21568322567072E-5,6.45873314616639E-5,
7.58025810641423E-5,8.14102058653814E-5,8.28121120656912E-5,8.70178306666206E-5,
0.000116081955658271,0.000130526745999931,0.000162394111022053,0.000174035661333241,
0.000213138396958831,0.000256116935434894,0.000302406662857592,0.000348071322666483),
 .UNSPECIFIED.);
#5138=B_SPLINE_CURVE_WITH_KNOTS('',3,(#236960,#236961,#236962,#236963,#236964,
#236965,#236966,#236967,#236968,#236969,#236970,#236971,#236972,#236973,
#236974,#236975,#236976,#236977,#236978,#236979,#236980,#236981,#236982,
#236983,#236984,#236985,#236986,#236987,#236988,#236989,#236990,#236991,
#236992,#236993,#236994,#236995,#236996,#236997,#236998,#236999,#237000,
#237001,#237002,#237003,#237004,#237005,#237006,#237007,#237008,#237009,
#237010,#237011),.UNSPECIFIED.,.F.,.F.,(4,3,3,3,3,3,3,3,3,3,3,3,3,3,3,3,
3,4),(1.30104260698261E-18,4.29652152160316E-5,8.44519107531626E-5,0.000123669830864362,
0.000159788877356911,0.000170558847912634,0.000181218775907174,0.000181960046452401,
0.000214460062643762,0.000244755726199148,0.000255838271868951,0.000258503253867586,
0.000261084955178764,0.00028937047664804,0.000301101325502016,0.000321109510663642,
0.000331113603244455,0.000341117695825268),.UNSPECIFIED.);
#5139=B_SPLINE_CURVE_WITH_KNOTS('',3,(#237013,#237014,#237015,#237016,#237017,
#237018,#237019,#237020,#237021,#237022,#237023,#237024,#237025,#237026,
#237027,#237028,#237029,#237030,#237031,#237032,#237033,#237034,#237035,
#237036,#237037,#237038,#237039,#237040,#237041,#237042,#237043,#237044,
#237045,#237046,#237047,#237048,#237049,#237050,#237051,#237052,#237053,
#237054,#237055,#237056,#237057,#237058,#237059,#237060,#237061,#237062,
#237063,#237064),.UNSPECIFIED.,.F.,.F.,(4,3,3,3,3,3,3,3,3,3,3,3,3,3,3,3,
3,4),(4.61009087360184E-18,4.3070623786273E-5,8.47417087683938E-5,0.000124159989203818,
0.000160467076287337,0.000170998382116699,0.000182414994733776,0.000213747977645872,
0.000242415955903083,0.000256497573175046,0.000259169422895619,0.000261757777312424,
0.000289965130403635,0.000301877270772909,0.000321937017503151,0.000326951954185711,
0.000334474359209552,0.000341996764233393),.UNSPECIFIED.);
#5140=B_SPLINE_CURVE_WITH_KNOTS('',3,(#237065,#237066,#237067,#237068,#237069,
#237070,#237071,#237072,#237073,#237074,#237075,#237076,#237077,#237078,
#237079,#237080,#237081,#237082,#237083,#237084,#237085,#237086,#237087,
#237088,#237089,#237090,#237091,#237092,#237093,#237094,#237095,#237096,
#237097,#237098,#237099,#237100,#237101,#237102,#237103,#237104,#237105,
#237106,#237107,#237108,#237109,#237110,#237111,#237112,#237113,#237114,
#237115,#237116),.UNSPECIFIED.,.F.,.F.,(4,3,3,3,3,3,3,3,3,3,3,3,3,3,3,3,
3,4),(0.,2.5845745168412E-5,4.25394446195606E-5,6.46659869687013E-5,7.57292581432716E-5,
8.12608937305567E-5,8.2643802627378E-5,8.67925293178419E-5,0.000116015624427532,
0.000130188793976763,0.000151886926306223,0.000161963651211281,0.000162735992470954,
0.000173585058635684,0.00021248788046143,0.000255238173513324,0.000301397761151222,
0.000347170117271353),.UNSPECIFIED.);
#5141=B_SPLINE_CURVE_WITH_KNOTS('',3,(#237118,#237119,#237120,#237121,#237122,
#237123,#237124,#237125,#237126,#237127,#237128,#237129,#237130,#237131,
#237132,#237133,#237134,#237135,#237136,#237137,#237138,#237139,#237140,
#237141,#237142,#237143,#237144,#237145,#237146,#237147,#237148,#237149,
#237150,#237151,#237152,#237153,#237154,#237155,#237156,#237157,#237158,
#237159,#237160,#237161,#237162,#237163),.UNSPECIFIED.,.F.,.F.,(4,3,3,3,
3,3,3,3,3,3,3,3,3,3,3,4),(3.46944695195361E-18,2.57218161985864E-5,4.21568322567459E-5,
6.45873314616802E-5,7.58025810641474E-5,8.14102058653809E-5,8.28121120656893E-5,
8.70178306666145E-5,0.000116081955657513,0.00013052674599992,0.000162394111022048,
0.000174035661333226,0.000213138396957984,0.000256116935433399,0.000302406662855914,
0.000348071322666466),.UNSPECIFIED.);
#5142=B_SPLINE_CURVE_WITH_KNOTS('',3,(#237164,#237165,#237166,#237167,#237168,
#237169,#237170,#237171,#237172,#237173,#237174,#237175,#237176,#237177,
#237178,#237179,#237180,#237181,#237182,#237183,#237184,#237185,#237186,
#237187,#237188,#237189,#237190,#237191,#237192,#237193,#237194,#237195,
#237196,#237197,#237198,#237199,#237200,#237201,#237202,#237203,#237204,
#237205,#237206,#237207,#237208,#237209,#237210,#237211,#237212,#237213,
#237214,#237215),.UNSPECIFIED.,.F.,.F.,(4,3,3,3,3,3,3,3,3,3,3,3,3,3,3,3,
3,4),(8.67361737988404E-19,4.29652152182944E-5,8.44519107569389E-5,0.000123669830869201,
0.000159788877362635,0.000170558847912625,0.000181218775907165,0.0001819600464524,
0.000214460062643611,0.000244755726198789,0.000255838271868938,0.000258503253867573,
0.00026108495517875,0.000289370476648206,0.000301101325502001,0.000321109510663626,
0.000331113603244438,0.000341117695825251),.UNSPECIFIED.);
#5143=B_SPLINE_CURVE_WITH_KNOTS('',3,(#237217,#237218,#237219,#237220,#237221,
#237222,#237223,#237224,#237225,#237226,#237227,#237228,#237229,#237230,
#237231,#237232,#237233,#237234,#237235,#237236,#237237,#237238,#237239,
#237240,#237241,#237242,#237243,#237244,#237245,#237246,#237247,#237248,
#237249,#237250,#237251,#237252,#237253,#237254,#237255,#237256,#237257,
#237258,#237259,#237260,#237261,#237262,#237263,#237264,#237265,#237266,
#237267,#237268),.UNSPECIFIED.,.F.,.F.,(4,3,3,3,3,3,3,3,3,3,3,3,3,3,3,3,
3,4),(2.16840434497101E-18,4.30706237872889E-5,8.47417087702185E-5,0.000124159989206578,
0.000160467076291047,0.000170998382116701,0.00018241499473378,0.000213747977645874,
0.000242415955903897,0.000256497573175046,0.00025916942289562,0.000261757777312425,
0.00028996513040244,0.000301877270772909,0.00032193701750315,0.000326951954185711,
0.000334474359209551,0.000341996764233392),.UNSPECIFIED.);
#5144=B_SPLINE_CURVE_WITH_KNOTS('',3,(#237269,#237270,#237271,#237272,#237273,
#237274,#237275,#237276,#237277,#237278,#237279,#237280,#237281,#237282,
#237283,#237284,#237285,#237286,#237287,#237288,#237289,#237290,#237291,
#237292,#237293,#237294,#237295,#237296,#237297,#237298,#237299,#237300,
#237301,#237302,#237303,#237304,#237305,#237306,#237307,#237308,#237309,
#237310,#237311,#237312,#237313,#237314,#237315,#237316,#237317,#237318,
#237319,#237320),.UNSPECIFIED.,.F.,.F.,(4,3,3,3,3,3,3,3,3,3,3,3,3,3,3,3,
3,4),(3.46944695195361E-18,2.58457451676127E-5,4.25394446194762E-5,6.46659869686576E-5,
7.57292581432484E-5,8.12608937305437E-5,8.26438026273676E-5,8.67925293178391E-5,
0.000116015624427052,0.000130188793976757,0.000151886926306216,0.000161963651211258,
0.000162735992470945,0.000173585058635675,0.000212487880458538,0.000255238173506317,
0.000301397761137294,0.000347170117271365),.UNSPECIFIED.);
#5145=B_SPLINE_CURVE_WITH_KNOTS('',3,(#237322,#237323,#237324,#237325,#237326,
#237327,#237328,#237329,#237330,#237331,#237332,#237333,#237334,#237335,
#237336,#237337,#237338,#237339,#237340,#237341,#237342,#237343,#237344,
#237345,#237346,#237347,#237348,#237349,#237350,#237351,#237352,#237353,
#237354,#237355,#237356,#237357,#237358,#237359,#237360,#237361,#237362,
#237363,#237364,#237365,#237366,#237367),.UNSPECIFIED.,.F.,.F.,(4,3,3,3,
3,3,3,3,3,3,3,3,3,3,3,4),(3.46944695195361E-18,2.5721816201202E-5,4.21568322569165E-5,
6.45873314617695E-5,7.5802581064196E-5,8.14102058654092E-5,8.28121120657125E-5,
8.70178306666225E-5,0.000116081955659048,0.000130526745999932,0.000162394111022063,
0.000174035661333241,0.000213138396958407,0.000256116935434203,0.000302406662857052,
0.000348071322666463),.UNSPECIFIED.);
#5146=B_SPLINE_CURVE_WITH_KNOTS('',3,(#237368,#237369,#237370,#237371,#237372,
#237373,#237374,#237375,#237376,#237377,#237378,#237379,#237380,#237381,
#237382,#237383,#237384,#237385,#237386,#237387,#237388,#237389,#237390,
#237391,#237392,#237393,#237394,#237395,#237396,#237397,#237398,#237399,
#237400,#237401,#237402,#237403,#237404,#237405,#237406,#237407,#237408,
#237409,#237410,#237411,#237412,#237413,#237414,#237415,#237416,#237417,
#237418,#237419),.UNSPECIFIED.,.F.,.F.,(4,3,3,3,3,3,3,3,3,3,3,3,3,3,3,3,
3,4),(0.,4.29652152166832E-5,8.44519107542356E-5,0.000123669830865694,0.000159788877358465,
0.000170558847912624,0.000181218775907163,0.0001819600464524,0.000214460062643199,
0.000244755726197238,0.000255838271868937,0.000258503253867572,0.00026108495517875,
0.000289370476648487,0.000301101325502,0.000321109510663625,0.000331113603244438,
0.00034111769582525),.UNSPECIFIED.);
#5147=B_SPLINE_CURVE_WITH_KNOTS('',3,(#237421,#237422,#237423,#237424,#237425,
#237426,#237427,#237428,#237429,#237430,#237431,#237432,#237433,#237434,
#237435,#237436,#237437,#237438,#237439,#237440,#237441,#237442,#237443,
#237444,#237445,#237446,#237447,#237448,#237449,#237450,#237451,#237452,
#237453,#237454,#237455,#237456,#237457,#237458,#237459,#237460,#237461,
#237462,#237463,#237464,#237465,#237466,#237467,#237468,#237469,#237470,
#237471,#237472),.UNSPECIFIED.,.F.,.F.,(4,3,3,3,3,3,3,3,3,3,3,3,3,3,3,3,
3,4),(1.0702344114451E-17,4.30706237862214E-5,8.47417087682975E-5,0.000124159989203744,
0.000160467076287253,0.000170998382116703,0.000182414994733785,0.000213747977645876,
0.000242415955902651,0.000256497573175048,0.000259169422895622,0.000261757777312427,
0.000289965130403741,0.00030187727077291,0.000321937017503152,0.000326951954185712,
0.000334474359209553,0.000341996764233393),.UNSPECIFIED.);
#5148=B_SPLINE_CURVE_WITH_KNOTS('',3,(#237473,#237474,#237475,#237476,#237477,
#237478,#237479,#237480,#237481,#237482,#237483,#237484,#237485,#237486,
#237487,#237488,#237489,#237490,#237491,#237492,#237493,#237494,#237495,
#237496,#237497,#237498,#237499,#237500,#237501,#237502,#237503,#237504,
#237505,#237506,#237507,#237508,#237509,#237510,#237511,#237512,#237513,
#237514,#237515,#237516,#237517,#237518,#237519,#237520,#237521,#237522,
#237523,#237524),.UNSPECIFIED.,.F.,.F.,(4,3,3,3,3,3,3,3,3,3,3,3,3,3,3,3,
3,4),(1.73472347597681E-18,2.58457451676447E-5,4.25394446196667E-5,6.46659869687532E-5,
7.57292581432965E-5,8.12608937305681E-5,8.2643802627386E-5,8.67925293178398E-5,
0.000116015624427285,0.000130188793976759,0.000151886926306218,0.00016196365121126,
0.000162735992470948,0.000173585058635678,0.000212487880458775,0.000255238173506902,
0.000301397761138638,0.000347170117271369),.UNSPECIFIED.);
#5149=B_SPLINE_CURVE_WITH_KNOTS('',3,(#237526,#237527,#237528,#237529,#237530,
#237531,#237532,#237533,#237534,#237535,#237536,#237537,#237538,#237539,
#237540,#237541,#237542,#237543,#237544,#237545,#237546,#237547,#237548,
#237549,#237550,#237551,#237552,#237553,#237554,#237555,#237556,#237557,
#237558,#237559,#237560,#237561,#237562,#237563,#237564,#237565,#237566,
#237567,#237568,#237569,#237570,#237571),.UNSPECIFIED.,.F.,.F.,(4,3,3,3,
3,3,3,3,3,3,3,3,3,3,3,4),(0.,2.57218161997054E-5,4.2156832256664E-5,6.45873314616409E-5,
7.58025810641293E-5,8.14102058653735E-5,8.28121120656845E-5,8.70178306666177E-5,
0.00011608195565801,0.000130526745999927,0.000162394111022051,0.000174035661333235,
0.000213138396956663,0.000256116935430629,0.000302406662851181,0.000348071322666486),
 .UNSPECIFIED.);
#5150=B_SPLINE_CURVE_WITH_KNOTS('',3,(#237572,#237573,#237574,#237575,#237576,
#237577,#237578,#237579,#237580,#237581,#237582,#237583,#237584,#237585,
#237586,#237587,#237588,#237589,#237590,#237591,#237592,#237593,#237594,
#237595,#237596,#237597,#237598,#237599,#237600,#237601,#237602,#237603,
#237604,#237605,#237606,#237607,#237608,#237609,#237610,#237611,#237612,
#237613,#237614,#237615,#237616,#237617,#237618,#237619,#237620,#237621,
#237622,#237623),.UNSPECIFIED.,.F.,.F.,(4,3,3,3,3,3,3,3,3,3,3,3,3,3,3,3,
3,4),(4.33680868994202E-19,4.29652152129658E-5,8.44519107482501E-5,0.000123669830858316,
0.000159788877350148,0.000170558847912625,0.000181218775907164,0.000181960046452394,
0.000214460062643421,0.000244755726197445,0.000255838271868942,0.000258503253867577,
0.000261084955178755,0.000289370476647996,0.000301101325502007,0.000321109510663633,
0.000331113603244447,0.00034111769582526),.UNSPECIFIED.);
#5151=B_SPLINE_CURVE_WITH_KNOTS('',3,(#237625,#237626,#237627,#237628,#237629,
#237630,#237631,#237632,#237633,#237634,#237635,#237636,#237637,#237638,
#237639,#237640,#237641,#237642,#237643,#237644,#237645,#237646,#237647,
#237648,#237649,#237650,#237651,#237652,#237653,#237654,#237655,#237656,
#237657,#237658,#237659,#237660,#237661,#237662,#237663,#237664,#237665,
#237666,#237667,#237668,#237669,#237670,#237671,#237672,#237673,#237674,
#237675,#237676),.UNSPECIFIED.,.F.,.F.,(4,3,3,3,3,3,3,3,3,3,3,3,3,3,3,3,
3,4),(9.66826306931024E-18,4.30706237866843E-5,8.4741708768988E-5,0.000124159989204507,
0.000160467076288014,0.000170998382116706,0.000182414994733798,0.000213747977645878,
0.000242415955902607,0.000256497573175049,0.000259169422895622,0.000261757777312428,
0.000289965130403992,0.00030187727077291,0.000321937017503151,0.000326951954185711,
0.000334474359209552,0.000341996764233392),.UNSPECIFIED.);
#5152=B_SPLINE_CURVE_WITH_KNOTS('',3,(#237677,#237678,#237679,#237680,#237681,
#237682,#237683,#237684,#237685,#237686,#237687,#237688,#237689,#237690,
#237691,#237692,#237693,#237694,#237695,#237696,#237697,#237698,#237699,
#237700,#237701,#237702,#237703,#237704,#237705,#237706,#237707,#237708,
#237709,#237710,#237711,#237712,#237713,#237714,#237715,#237716,#237717,
#237718,#237719,#237720,#237721,#237722,#237723,#237724,#237725,#237726,
#237727,#237728),.UNSPECIFIED.,.F.,.F.,(4,3,3,3,3,3,3,3,3,3,3,3,3,3,3,3,
3,4),(0.,2.58457451676031E-5,4.25394446196135E-5,6.46659869687281E-5,7.57292581432855E-5,
8.12608937305641E-5,8.26438026273838E-5,8.67925293178428E-5,0.000116015624427197,
0.000130188793976764,0.000151886926306225,0.000161963651211278,0.000162735992470955,
0.000173585058635686,0.000212487880462397,0.000255238173513979,0.000301397761149119,
0.00034717011727137),.UNSPECIFIED.);
#5153=B_SPLINE_CURVE_WITH_KNOTS('',3,(#237730,#237731,#237732,#237733,#237734,
#237735,#237736,#237737,#237738,#237739,#237740,#237741,#237742,#237743,
#237744,#237745,#237746,#237747,#237748,#237749,#237750,#237751,#237752,
#237753,#237754,#237755,#237756,#237757,#237758,#237759,#237760,#237761,
#237762,#237763,#237764,#237765,#237766,#237767,#237768,#237769,#237770,
#237771,#237772,#237773,#237774,#237775),.UNSPECIFIED.,.F.,.F.,(4,3,3,3,
3,3,3,3,3,3,3,3,3,3,3,4),(8.67361737988404E-19,2.57218161993305E-5,4.21568322567911E-5,
6.45873314617076E-5,7.58025810641659E-5,8.1410205865395E-5,8.28121120657023E-5,
8.70178306666241E-5,0.000116081955658071,0.000130526745999936,0.00016239411102206,
0.000174035661333247,0.000213138396957183,0.000256116935431462,0.000302406662851793,
0.000348071322666493),.UNSPECIFIED.);
#5154=B_SPLINE_CURVE_WITH_KNOTS('',3,(#237776,#237777,#237778,#237779,#237780,
#237781,#237782,#237783,#237784,#237785,#237786,#237787,#237788,#237789,
#237790,#237791,#237792,#237793,#237794,#237795,#237796,#237797,#237798,
#237799,#237800,#237801,#237802,#237803,#237804,#237805,#237806,#237807,
#237808,#237809,#237810,#237811,#237812,#237813,#237814,#237815,#237816,
#237817,#237818,#237819,#237820,#237821,#237822,#237823,#237824,#237825,
#237826,#237827),.UNSPECIFIED.,.F.,.F.,(4,3,3,3,3,3,3,3,3,3,3,3,3,3,3,3,
3,4),(0.,4.29652152133897E-5,8.44519107489504E-5,0.00012366983085924,0.000159788877351311,
0.000170558847912625,0.000181218775907164,0.000181960046452397,0.000214460062643666,
0.000244755726198589,0.000255838271868937,0.000258503253867572,0.000261084955178749,
0.000289370476647751,0.000301101325502,0.000321109510663625,0.000331113603244437,
0.00034111769582525),.UNSPECIFIED.);
#5155=B_SPLINE_CURVE_WITH_KNOTS('',3,(#237829,#237830,#237831,#237832,#237833,
#237834,#237835,#237836,#237837,#237838,#237839,#237840,#237841,#237842,
#237843,#237844,#237845,#237846,#237847,#237848,#237849,#237850,#237851,
#237852,#237853,#237854,#237855,#237856,#237857,#237858,#237859,#237860,
#237861,#237862,#237863,#237864,#237865,#237866,#237867,#237868,#237869,
#237870,#237871,#237872,#237873,#237874,#237875,#237876,#237877,#237878,
#237879,#237880),.UNSPECIFIED.,.F.,.F.,(4,3,3,3,3,3,3,3,3,3,3,3,3,3,3,3,
3,4),(3.09377807083354E-18,4.30706237871686E-5,8.47417087700116E-5,0.000124159989206186,
0.000160467076290512,0.000170998382116679,0.000182414994733741,0.000213747977645855,
0.000242415955903015,0.00025649757317503,0.000259169422895604,0.000261757777312409,
0.000289965130403648,0.000301877270772895,0.000321937017503138,0.000326951954185699,
0.00033447435920954,0.000341996764233381),.UNSPECIFIED.);
#5156=B_SPLINE_CURVE_WITH_KNOTS('',3,(#237881,#237882,#237883,#237884,#237885,
#237886,#237887,#237888,#237889,#237890,#237891,#237892,#237893,#237894,
#237895,#237896,#237897,#237898,#237899,#237900,#237901,#237902,#237903,
#237904,#237905,#237906,#237907,#237908,#237909,#237910,#237911,#237912,
#237913,#237914,#237915,#237916,#237917,#237918,#237919,#237920,#237921,
#237922,#237923,#237924,#237925,#237926,#237927,#237928,#237929,#237930,
#237931,#237932),.UNSPECIFIED.,.F.,.F.,(4,3,3,3,3,3,3,3,3,3,3,3,3,3,3,3,
3,4),(0.,2.58457451678914E-5,4.2539444619683E-5,6.46659869687625E-5,7.57292581433022E-5,
8.12608937305721E-5,8.26438026273895E-5,8.67925293178419E-5,0.000116015624427083,
0.000130188793976763,0.000151886926306223,0.000161963651211268,0.000162735992470954,
0.000173585058635684,0.000212487880460161,0.000255238173510438,0.000301397761145908,
0.000347170117271354),.UNSPECIFIED.);
#5157=B_SPLINE_CURVE_WITH_KNOTS('',3,(#237934,#237935,#237936,#237937,#237938,
#237939,#237940,#237941,#237942,#237943,#237944,#237945,#237946,#237947,
#237948,#237949,#237950,#237951,#237952,#237953,#237954,#237955,#237956,
#237957,#237958,#237959,#237960,#237961,#237962,#237963,#237964,#237965,
#237966,#237967,#237968,#237969,#237970,#237971,#237972,#237973,#237974,
#237975,#237976,#237977,#237978,#237979),.UNSPECIFIED.,.F.,.F.,(4,3,3,3,
3,3,3,3,3,3,3,3,3,3,3,4),(2.74438674910393E-19,2.5721816198343E-5,4.21568322569397E-5,
6.45873314617789E-5,7.58025810641984E-5,8.14102058654082E-5,8.28121120657107E-5,
8.7017830666618E-5,0.000116081955658225,0.000130526745999927,0.00016239411102205,
0.000174035661333236,0.000213138396959223,0.000256116935435911,0.000302406662859976,
0.000348071322666472),.UNSPECIFIED.);
#5158=B_SPLINE_CURVE_WITH_KNOTS('',3,(#237980,#237981,#237982,#237983,#237984,
#237985,#237986,#237987,#237988,#237989,#237990,#237991,#237992,#237993,
#237994,#237995,#237996,#237997,#237998,#237999,#238000,#238001,#238002,
#238003,#238004,#238005,#238006,#238007,#238008,#238009,#238010,#238011,
#238012,#238013,#238014,#238015,#238016,#238017,#238018,#238019,#238020,
#238021,#238022,#238023,#238024,#238025,#238026,#238027,#238028,#238029,
#238030,#238031),.UNSPECIFIED.,.F.,.F.,(4,3,3,3,3,3,3,3,3,3,3,3,3,3,3,3,
3,4),(0.,4.29652152174176E-5,8.445191075561E-5,0.000123669830867732,0.000159788877361313,
0.000170558847912633,0.000181218775907173,0.000181960046452402,0.000214460062643273,
0.000244755726197394,0.00025583827186895,0.000258503253867585,0.000261084955178762,
0.000289370476648092,0.000301101325502014,0.00032110951066364,0.000331113603244453,
0.000341117695825266),.UNSPECIFIED.);
#5159=B_SPLINE_CURVE_WITH_KNOTS('',3,(#238033,#238034,#238035,#238036,#238037,
#238038,#238039,#238040,#238041,#238042,#238043,#238044,#238045,#238046,
#238047,#238048,#238049,#238050,#238051,#238052,#238053,#238054,#238055,
#238056,#238057,#238058,#238059,#238060,#238061,#238062,#238063,#238064,
#238065,#238066,#238067,#238068,#238069,#238070,#238071,#238072,#238073,
#238074,#238075,#238076,#238077,#238078,#238079,#238080,#238081,#238082,
#238083,#238084),.UNSPECIFIED.,.F.,.F.,(4,3,3,3,3,3,3,3,3,3,3,3,3,3,3,3,
3,4),(4.33680868994202E-19,4.30706237870913E-5,8.47417087699565E-5,0.000124159989206289,
0.000160467076290841,0.000170998382116694,0.000182414994733777,0.000213747977645867,
0.000242415955902843,0.00025649757317504,0.000259169422895614,0.000261757777312419,
0.000289965130403804,0.000301877270772903,0.000321937017503145,0.000326951954185706,
0.000334474359209546,0.000341996764233387),.UNSPECIFIED.);
#5160=B_SPLINE_CURVE_WITH_KNOTS('',3,(#238085,#238086,#238087,#238088,#238089,
#238090,#238091,#238092,#238093,#238094,#238095,#238096,#238097,#238098,
#238099,#238100,#238101,#238102,#238103,#238104,#238105,#238106,#238107,
#238108,#238109,#238110,#238111,#238112,#238113,#238114,#238115,#238116,
#238117,#238118,#238119,#238120,#238121,#238122,#238123,#238124,#238125,
#238126,#238127,#238128,#238129,#238130,#238131,#238132,#238133,#238134,
#238135,#238136),.UNSPECIFIED.,.F.,.F.,(4,3,3,3,3,3,3,3,3,3,3,3,3,3,3,3,
3,4),(0.,2.58457451666468E-5,4.25394446196103E-5,6.46659869687272E-5,7.57292581432856E-5,
8.12608937305648E-5,8.26438026273846E-5,8.6792529317844E-5,0.000116015624426662,
0.000130188793976766,0.000151886926306227,0.000161963651211283,0.000162735992470958,
0.000173585058635688,0.000212487880463352,0.000255238173516254,0.000301397761153875,
0.000347170117271378),.UNSPECIFIED.);
#5161=B_SPLINE_CURVE_WITH_KNOTS('',3,(#238138,#238139,#238140,#238141,#238142,
#238143,#238144,#238145,#238146,#238147,#238148,#238149,#238150,#238151,
#238152,#238153,#238154,#238155,#238156,#238157,#238158,#238159,#238160,
#238161,#238162,#238163,#238164,#238165,#238166,#238167,#238168,#238169,
#238170,#238171,#238172,#238173,#238174,#238175,#238176,#238177,#238178,
#238179,#238180,#238181,#238182,#238183),.UNSPECIFIED.,.F.,.F.,(4,3,3,3,
3,3,3,3,3,3,3,3,3,3,3,4),(8.67361737988404E-19,2.57218161983997E-5,4.21568322567976E-5,
6.45873314617104E-5,7.58025810641669E-5,8.14102058653951E-5,8.28121120657021E-5,
8.70178306666233E-5,0.000116081955658178,0.000130526745999931,0.000162394111022045,
0.000174035661333238,0.0002131383969601,0.000256116935437471,0.000302406662861761,
0.000348071322666481),.UNSPECIFIED.);
#5162=B_SPLINE_CURVE_WITH_KNOTS('',3,(#238184,#238185,#238186,#238187,#238188,
#238189,#238190,#238191,#238192,#238193,#238194,#238195,#238196,#238197,
#238198,#238199,#238200,#238201,#238202,#238203,#238204,#238205,#238206,
#238207,#238208,#238209,#238210,#238211,#238212,#238213,#238214,#238215,
#238216,#238217,#238218,#238219,#238220,#238221,#238222,#238223,#238224,
#238225,#238226,#238227,#238228,#238229,#238230,#238231,#238232,#238233,
#238234,#238235),.UNSPECIFIED.,.F.,.F.,(4,3,3,3,3,3,3,3,3,3,3,3,3,3,3,3,
3,4),(0.,4.29652152176474E-5,8.44519107560601E-5,0.00012366983086853,0.000159788877362454,
0.000170558847912624,0.000181218775907163,0.000181960046452395,0.000214460062643399,
0.000244755726197756,0.000255838271868942,0.000258503253867577,0.000261084955178754,
0.000289370476647851,0.000301101325502007,0.000321109510663634,0.000331113603244447,
0.00034111769582526),.UNSPECIFIED.);
#5163=B_SPLINE_CURVE_WITH_KNOTS('',3,(#238237,#238238,#238239,#238240,#238241,
#238242,#238243,#238244,#238245,#238246,#238247,#238248,#238249,#238250,
#238251,#238252,#238253,#238254,#238255,#238256,#238257,#238258,#238259,
#238260,#238261,#238262,#238263,#238264,#238265,#238266,#238267,#238268,
#238269,#238270,#238271,#238272,#238273,#238274,#238275,#238276,#238277,
#238278,#238279,#238280,#238281,#238282,#238283,#238284,#238285,#238286,
#238287,#238288),.UNSPECIFIED.,.F.,.F.,(4,3,3,3,3,3,3,3,3,3,3,3,3,3,3,3,
3,4),(3.03576608295941E-18,4.30706237872062E-5,8.47417087700904E-5,0.000124159989206327,
0.000160467076290739,0.000170998382116701,0.000182414994733785,0.000213747977645875,
0.000242415955903026,0.000256497573175049,0.000259169422895622,0.000261757777312428,
0.000289965130403995,0.000301877270772912,0.000321937017503155,0.000326951954185715,
0.000334474359209556,0.000341996764233397),.UNSPECIFIED.);
#5164=B_SPLINE_CURVE_WITH_KNOTS('',3,(#238289,#238290,#238291,#238292,#238293,
#238294,#238295,#238296,#238297,#238298,#238299,#238300,#238301,#238302,
#238303,#238304,#238305,#238306,#238307,#238308,#238309,#238310,#238311,
#238312,#238313,#238314,#238315,#238316,#238317,#238318,#238319,#238320,
#238321,#238322,#238323,#238324,#238325,#238326,#238327,#238328,#238329,
#238330,#238331,#238332,#238333,#238334,#238335,#238336,#238337,#238338,
#238339,#238340),.UNSPECIFIED.,.F.,.F.,(4,3,3,3,3,3,3,3,3,3,3,3,3,3,3,3,
3,4),(0.,2.58457451677985E-5,4.25394446195654E-5,6.46659869687035E-5,7.57292581432725E-5,
8.1260893730557E-5,8.26438026273782E-5,8.67925293178416E-5,0.000116015624427485,
0.000130188793976762,0.000151886926306223,0.000161963651211287,0.000162735992470953,
0.000173585058635683,0.000212487880460691,0.00025523817351173,0.000301397761148335,
0.000347170117271366),.UNSPECIFIED.);
#5165=B_SPLINE_CURVE_WITH_KNOTS('',3,(#238342,#238343,#238344,#238345,#238346,
#238347,#238348,#238349,#238350,#238351,#238352,#238353,#238354,#238355,
#238356,#238357,#238358,#238359,#238360,#238361,#238362,#238363,#238364,
#238365,#238366,#238367,#238368,#238369,#238370,#238371,#238372,#238373,
#238374,#238375,#238376,#238377,#238378,#238379,#238380,#238381,#238382,
#238383,#238384,#238385,#238386,#238387),.UNSPECIFIED.,.F.,.F.,(4,3,3,3,
3,3,3,3,3,3,3,3,3,3,3,4),(0.,2.57218161992493E-5,4.215683225679E-5,6.45873314617063E-5,
7.58025810641645E-5,8.14102058653936E-5,8.28121120657009E-5,8.70178306666227E-5,
0.000116081955658092,0.000130526745999934,0.000162394111022042,0.000174035661333245,
0.000213138396956871,0.000256116935430989,0.000302406662851721,0.000348071322666493),
 .UNSPECIFIED.);
#5166=B_SPLINE_CURVE_WITH_KNOTS('',3,(#238388,#238389,#238390,#238391,#238392,
#238393,#238394,#238395,#238396,#238397,#238398,#238399,#238400,#238401,
#238402,#238403,#238404,#238405,#238406,#238407,#238408,#238409,#238410,
#238411,#238412,#238413,#238414,#238415,#238416,#238417,#238418,#238419,
#238420,#238421,#238422,#238423,#238424,#238425,#238426,#238427,#238428,
#238429,#238430,#238431,#238432,#238433,#238434,#238435,#238436,#238437,
#238438,#238439),.UNSPECIFIED.,.F.,.F.,(4,3,3,3,3,3,3,3,3,3,3,3,3,3,3,3,
3,4),(3.03576608295941E-18,4.29652152151958E-5,8.44519107520227E-5,0.000123669830863345,
0.000159788877356407,0.000170558847912634,0.000181218775907174,0.000181960046452411,
0.000214460062643647,0.000244755726198505,0.000255838271868951,0.000258503253867586,
0.000261084955178763,0.000289370476647687,0.000301101325502015,0.000321109510663641,
0.000331113603244454,0.000341117695825267),.UNSPECIFIED.);
#5167=B_SPLINE_CURVE_WITH_KNOTS('',3,(#238441,#238442,#238443,#238444,#238445,
#238446,#238447,#238448,#238449,#238450,#238451,#238452,#238453,#238454,
#238455,#238456,#238457,#238458,#238459,#238460,#238461,#238462,#238463,
#238464,#238465,#238466,#238467,#238468,#238469,#238470,#238471,#238472,
#238473,#238474,#238475,#238476,#238477,#238478,#238479,#238480,#238481,
#238482,#238483,#238484,#238485,#238486,#238487,#238488,#238489,#238490,
#238491,#238492),.UNSPECIFIED.,.F.,.F.,(4,3,3,3,3,3,3,3,3,3,3,3,3,3,3,3,
3,4),(4.33680868994202E-19,4.3070623784098E-5,8.4741708764398E-5,0.000124159989198101,
0.000160467076279639,0.000170998382116699,0.000182414994733788,0.00021374797764587,
0.000242415955902635,0.000256497573175042,0.000259169422895615,0.00026175777731242,
0.000289965130405031,0.000301877270772902,0.000321937017503143,0.000326951954185704,
0.000334474359209544,0.000341996764233385),.UNSPECIFIED.);
#5168=B_SPLINE_CURVE_WITH_KNOTS('',3,(#238493,#238494,#238495,#238496,#238497,
#238498,#238499,#238500,#238501,#238502,#238503,#238504,#238505,#238506,
#238507,#238508,#238509,#238510,#238511,#238512,#238513,#238514,#238515,
#238516,#238517,#238518,#238519,#238520,#238521,#238522,#238523,#238524,
#238525,#238526,#238527,#238528,#238529,#238530,#238531,#238532,#238533,
#238534,#238535,#238536,#238537,#238538,#238539,#238540,#238541,#238542,
#238543,#238544),.UNSPECIFIED.,.F.,.F.,(4,3,3,3,3,3,3,3,3,3,3,3,3,3,3,3,
3,4),(3.46944695195361E-18,2.5845745167508E-5,4.25394446194645E-5,6.46659869686533E-5,
7.57292581432477E-5,8.12608937305449E-5,8.26438026273692E-5,8.67925293178421E-5,
0.00011601562442678,0.000130188793976761,0.000151886926306221,0.000161963651211275,
0.000162735992470951,0.000173585058635681,0.000212487880460457,0.000255238173511178,
0.000301397761147439,0.000347170117271366),.UNSPECIFIED.);
#5169=B_SPLINE_CURVE_WITH_KNOTS('',3,(#238546,#238547,#238548,#238549,#238550,
#238551,#238552,#238553,#238554,#238555,#238556,#238557,#238558,#238559,
#238560,#238561,#238562,#238563,#238564,#238565,#238566,#238567,#238568,
#238569,#238570,#238571,#238572,#238573,#238574,#238575,#238576,#238577,
#238578,#238579,#238580,#238581,#238582,#238583,#238584,#238585,#238586,
#238587,#238588,#238589,#238590,#238591),.UNSPECIFIED.,.F.,.F.,(4,3,3,3,
3,3,3,3,3,3,3,3,3,3,3,4),(0.,2.57218161987356E-5,4.21568322568225E-5,6.45873314617223E-5,
7.58025810641722E-5,8.14102058653971E-5,8.28121120657033E-5,8.7017830666622E-5,
0.000116081955657996,0.000130526745999933,0.000162394111022048,0.000174035661333244,
0.000213138396959427,0.000256116935436209,0.000302406662860123,0.000348071322666472),
 .UNSPECIFIED.);
#5170=B_SPLINE_CURVE_WITH_KNOTS('',3,(#238592,#238593,#238594,#238595,#238596,
#238597,#238598,#238599,#238600,#238601,#238602,#238603,#238604,#238605,
#238606,#238607,#238608,#238609,#238610,#238611,#238612,#238613,#238614,
#238615,#238616,#238617,#238618,#238619,#238620,#238621,#238622,#238623,
#238624,#238625,#238626,#238627,#238628,#238629,#238630,#238631,#238632,
#238633,#238634,#238635,#238636,#238637,#238638,#238639,#238640,#238641,
#238642,#238643),.UNSPECIFIED.,.F.,.F.,(4,3,3,3,3,3,3,3,3,3,3,3,3,3,3,3,
3,4),(4.33680868994202E-19,4.29652152166818E-5,8.44519107542978E-5,0.000123669830865928,
0.000159788877358893,0.000170558847912628,0.000181218775907169,0.000181960046452395,
0.000214460062643088,0.000244755726196831,0.00025583827186895,0.000258503253867585,
0.000261084955178763,0.000289370476648246,0.000301101325502018,0.000321109510663645,
0.000331113603244458,0.000341117695825272),.UNSPECIFIED.);
#5171=B_SPLINE_CURVE_WITH_KNOTS('',3,(#238645,#238646,#238647,#238648,#238649,
#238650,#238651,#238652,#238653,#238654,#238655,#238656,#238657,#238658,
#238659,#238660,#238661,#238662,#238663,#238664,#238665,#238666,#238667,
#238668,#238669,#238670,#238671,#238672,#238673,#238674,#238675,#238676,
#238677,#238678,#238679,#238680,#238681,#238682,#238683,#238684,#238685,
#238686,#238687,#238688,#238689,#238690,#238691,#238692,#238693,#238694,
#238695,#238696),.UNSPECIFIED.,.F.,.F.,(4,3,3,3,3,3,3,3,3,3,3,3,3,3,3,3,
3,4),(0.,4.30706237880981E-5,8.47417087717393E-5,0.000124159989208782,0.000160467076294121,
0.000170998382116685,0.000182414994733763,0.000213747977645861,0.000242415955903088,
0.000256497573175037,0.00025916942289561,0.000261757777312416,0.000289965130403175,
0.000301877270772902,0.000321937017503145,0.000326951954185706,0.000334474359209547,
0.000341996764233388),.UNSPECIFIED.);
#5172=B_SPLINE_CURVE_WITH_KNOTS('',3,(#238697,#238698,#238699,#238700,#238701,
#238702,#238703,#238704,#238705,#238706,#238707,#238708,#238709,#238710,
#238711,#238712,#238713,#238714,#238715,#238716,#238717,#238718,#238719,
#238720,#238721,#238722,#238723,#238724,#238725,#238726,#238727,#238728,
#238729,#238730,#238731,#238732,#238733,#238734,#238735,#238736,#238737,
#238738,#238739,#238740,#238741,#238742,#238743,#238744,#238745,#238746,
#238747,#238748),.UNSPECIFIED.,.F.,.F.,(4,3,3,3,3,3,3,3,3,3,3,3,3,3,3,3,
3,4),(0.,2.5845745168441E-5,4.25394446196211E-5,6.46659869687328E-5,7.57292581432887E-5,
8.12608937305666E-5,8.26438026273861E-5,8.67925293178446E-5,0.000116015624426974,
0.000130188793976767,0.000151886926306228,0.000161963651211272,0.000162735992470959,
0.000173585058635689,0.000212487880461697,0.000255238173513341,0.000301397761150061,
0.000347170117271378),.UNSPECIFIED.);
#5173=B_SPLINE_CURVE_WITH_KNOTS('',3,(#238750,#238751,#238752,#238753,#238754,
#238755,#238756,#238757,#238758,#238759,#238760,#238761,#238762,#238763,
#238764,#238765,#238766,#238767,#238768,#238769,#238770,#238771,#238772,
#238773,#238774,#238775,#238776,#238777,#238778,#238779,#238780,#238781,
#238782,#238783,#238784,#238785,#238786,#238787,#238788,#238789,#238790,
#238791,#238792,#238793,#238794,#238795),.UNSPECIFIED.,.F.,.F.,(4,3,3,3,
3,3,3,3,3,3,3,3,3,3,3,4),(0.,2.57218162001823E-5,4.21568322568501E-5,6.45873314617339E-5,
7.58025810641758E-5,8.14102058653967E-5,8.2812112065702E-5,8.70178306666177E-5,
0.000116081955658371,0.000130526745999927,0.000162394111022044,0.000174035661333235,
0.000213138396959927,0.000256116935437149,0.000302406662861384,0.000348071322666479),
 .UNSPECIFIED.);
#5174=B_SPLINE_CURVE_WITH_KNOTS('',3,(#238796,#238797,#238798,#238799,#238800,
#238801,#238802,#238803,#238804,#238805,#238806,#238807,#238808,#238809,
#238810,#238811,#238812,#238813,#238814,#238815,#238816,#238817,#238818,
#238819,#238820,#238821,#238822,#238823,#238824,#238825,#238826,#238827,
#238828,#238829,#238830,#238831,#238832,#238833,#238834,#238835,#238836,
#238837,#238838,#238839,#238840,#238841,#238842,#238843,#238844,#238845,
#238846,#238847),.UNSPECIFIED.,.F.,.F.,(4,3,3,3,3,3,3,3,3,3,3,3,3,3,3,3,
3,4),(8.67361737988404E-19,4.29652152182224E-5,8.44519107567866E-5,0.000123669830869072,
0.000159788877362546,0.000170558847912642,0.000181218775907181,0.000181960046452415,
0.000214460062643632,0.000244755726198693,0.000255838271868955,0.000258503253867589,
0.000261084955178767,0.000289370476647603,0.000301101325502017,0.000321109510663642,
0.000331113603244455,0.000341117695825267),.UNSPECIFIED.);
#5175=B_SPLINE_CURVE_WITH_KNOTS('',3,(#238849,#238850,#238851,#238852,#238853,
#238854,#238855,#238856,#238857,#238858,#238859,#238860,#238861,#238862,
#238863,#238864,#238865,#238866,#238867,#238868,#238869,#238870,#238871,
#238872,#238873,#238874,#238875,#238876,#238877,#238878,#238879,#238880,
#238881,#238882,#238883,#238884,#238885,#238886,#238887,#238888,#238889,
#238890,#238891,#238892,#238893,#238894,#238895,#238896,#238897,#238898,
#238899,#238900),.UNSPECIFIED.,.F.,.F.,(4,3,3,3,3,3,3,3,3,3,3,3,3,3,3,3,
3,4),(0.,4.3070623782646E-5,8.47417087619512E-5,0.000124159989194811,0.00016046707627559,
0.000170998382116695,0.00018241499473379,0.000213747977645869,0.00024241595590369,
0.000256497573175043,0.000259169422895617,0.000261757777312422,0.000289965130404861,
0.000301877270772907,0.000321937017503149,0.000326951954185709,0.00033447435920955,
0.000341996764233391),.UNSPECIFIED.);
#5176=B_SPLINE_CURVE_WITH_KNOTS('',3,(#238901,#238902,#238903,#238904,#238905,
#238906,#238907,#238908,#238909,#238910,#238911,#238912,#238913,#238914,
#238915,#238916,#238917,#238918,#238919,#238920,#238921,#238922,#238923,
#238924,#238925,#238926,#238927,#238928,#238929,#238930,#238931,#238932,
#238933,#238934,#238935,#238936,#238937,#238938,#238939,#238940,#238941,
#238942,#238943,#238944,#238945,#238946,#238947,#238948,#238949,#238950,
#238951,#238952),.UNSPECIFIED.,.F.,.F.,(4,3,3,3,3,3,3,3,3,3,3,3,3,3,3,3,
3,4),(0.,2.58457451662736E-5,4.25394446196895E-5,6.46659869687634E-5,7.57292581433003E-5,
8.12608937305688E-5,8.26438026273859E-5,8.67925293178372E-5,0.000116015624426251,
0.000130188793976756,0.000151886926306215,0.000161963651211272,0.000162735992470945,
0.000173585058635674,0.000212487880462082,0.00025523817351434,0.000301397761152266,
0.000347170117271362),.UNSPECIFIED.);
#5177=B_SPLINE_CURVE_WITH_KNOTS('',3,(#238954,#238955,#238956,#238957,#238958,
#238959,#238960,#238961,#238962,#238963,#238964,#238965,#238966,#238967,
#238968,#238969,#238970,#238971,#238972,#238973,#238974,#238975,#238976,
#238977,#238978,#238979,#238980,#238981,#238982,#238983,#238984,#238985,
#238986,#238987,#238988,#238989,#238990,#238991,#238992,#238993,#238994,
#238995,#238996,#238997,#238998,#238999),.UNSPECIFIED.,.F.,.F.,(4,3,3,3,
3,3,3,3,3,3,3,3,3,3,3,4),(0.,2.57218162006404E-5,4.2156832256781E-5,6.45873314616977E-5,
7.58025810641561E-5,8.14102058653853E-5,8.28121120656925E-5,8.70178306666144E-5,
0.000116081955658562,0.000130526745999922,0.000162394111022053,0.000174035661333229,
0.000213138396956554,0.000256116935430458,0.000302406662851075,0.000348071322666458),
 .UNSPECIFIED.);
#5178=B_SPLINE_CURVE_WITH_KNOTS('',3,(#239000,#239001,#239002,#239003,#239004,
#239005,#239006,#239007,#239008,#239009,#239010,#239011,#239012,#239013,
#239014,#239015,#239016,#239017,#239018,#239019,#239020,#239021,#239022,
#239023,#239024,#239025,#239026,#239027,#239028,#239029,#239030,#239031,
#239032,#239033,#239034,#239035,#239036,#239037,#239038,#239039,#239040,
#239041,#239042,#239043,#239044,#239045,#239046,#239047,#239048,#239049,
#239050,#239051),.UNSPECIFIED.,.F.,.F.,(4,3,3,3,3,3,3,3,3,3,3,3,3,3,3,3,
3,4),(4.33680868994202E-19,4.29652152217032E-5,8.44519107624915E-5,0.000123669830876186,
0.000159788877370628,0.000170558847912619,0.000181218775907159,0.000181960046452394,
0.000214460062643333,0.000244755726197477,0.000255838271868938,0.000258503253867573,
0.00026108495517875,0.000289370476647778,0.000301101325502003,0.00032110951066363,
0.000331113603244443,0.000341117695825256),.UNSPECIFIED.);
#5179=B_SPLINE_CURVE_WITH_KNOTS('',3,(#239053,#239054,#239055,#239056,#239057,
#239058,#239059,#239060,#239061,#239062,#239063,#239064,#239065,#239066,
#239067,#239068,#239069,#239070,#239071,#239072,#239073,#239074,#239075,
#239076,#239077,#239078,#239079,#239080,#239081,#239082,#239083,#239084,
#239085,#239086,#239087,#239088,#239089,#239090,#239091,#239092,#239093,
#239094,#239095,#239096,#239097,#239098,#239099,#239100,#239101,#239102,
#239103,#239104),.UNSPECIFIED.,.F.,.F.,(4,3,3,3,3,3,3,3,3,3,3,3,3,3,3,3,
3,4),(1.73472347597681E-18,4.30706237865187E-5,8.47417087690789E-5,0.000124159989205212,
0.000160467076289721,0.000170998382116687,0.000182414994733761,0.000213747977645862,
0.000242415955903363,0.000256497573175038,0.000259169422895611,0.000261757777312417,
0.00028996513040298,0.000301877270772903,0.000321937017503145,0.000326951954185706,
0.000334474359209547,0.000341996764233388),.UNSPECIFIED.);
#5180=B_SPLINE_CURVE_WITH_KNOTS('',3,(#239105,#239106,#239107,#239108,#239109,
#239110,#239111,#239112,#239113,#239114,#239115,#239116,#239117,#239118,
#239119,#239120,#239121,#239122,#239123,#239124,#239125,#239126,#239127,
#239128,#239129,#239130,#239131,#239132,#239133,#239134,#239135,#239136,
#239137,#239138,#239139,#239140,#239141,#239142,#239143,#239144,#239145,
#239146,#239147,#239148,#239149,#239150,#239151,#239152,#239153,#239154,
#239155,#239156),.UNSPECIFIED.,.F.,.F.,(4,3,3,3,3,3,3,3,3,3,3,3,3,3,3,3,
3,4),(0.,2.5845745167758E-5,4.25394446195707E-5,6.46659869687025E-5,7.57292581432684E-5,
8.12608937305514E-5,8.26438026273721E-5,8.67925293178343E-5,0.000116015624427299,
0.000130188793976752,0.00015188692630621,0.000161963651211261,0.000162735992470939,
0.000173585058635669,0.000212487880461096,0.000255238173511359,0.000301397761144902,
0.000347170117271349),.UNSPECIFIED.);
#5181=B_SPLINE_CURVE_WITH_KNOTS('',3,(#239158,#239159,#239160,#239161,#239162,
#239163,#239164,#239165,#239166,#239167,#239168,#239169,#239170,#239171,
#239172,#239173,#239174,#239175,#239176,#239177,#239178,#239179,#239180,
#239181,#239182,#239183,#239184,#239185,#239186,#239187,#239188,#239189,
#239190,#239191,#239192,#239193,#239194,#239195,#239196,#239197,#239198,
#239199,#239200,#239201,#239202,#239203),.UNSPECIFIED.,.F.,.F.,(4,3,3,3,
3,3,3,3,3,3,3,3,3,3,3,4),(0.,2.57218162006442E-5,4.21568322567569E-5,6.45873314616859E-5,
7.58025810641504E-5,8.14102058653826E-5,8.28121120656907E-5,8.70178306666148E-5,
0.000116081955659045,0.000130526745999922,0.000162394111022048,0.00017403566133323,
0.000213138396959227,0.00025611693543571,0.000302406662858846,0.000348071322666472),
 .UNSPECIFIED.);
#5182=B_SPLINE_CURVE_WITH_KNOTS('',3,(#239204,#239205,#239206,#239207,#239208,
#239209,#239210,#239211,#239212,#239213,#239214,#239215,#239216,#239217,
#239218,#239219,#239220,#239221,#239222,#239223,#239224,#239225,#239226,
#239227,#239228,#239229,#239230,#239231,#239232,#239233,#239234,#239235,
#239236,#239237,#239238,#239239,#239240,#239241,#239242,#239243,#239244,
#239245,#239246,#239247,#239248,#239249,#239250,#239251,#239252,#239253,
#239254,#239255),.UNSPECIFIED.,.F.,.F.,(4,3,3,3,3,3,3,3,3,3,3,3,3,3,3,3,
3,4),(0.,4.29652152172934E-5,8.445191075492E-5,0.000123669830866065,0.000159788877357958,
0.000170558847912622,0.000181218775907161,0.000181960046452391,0.000214460062643236,
0.000244755726197423,0.000255838271868933,0.000258503253867568,0.000261084955178745,
0.000289370476648821,0.000301101325501995,0.00032110951066362,0.000331113603244432,
0.000341117695825244),.UNSPECIFIED.);
#5183=B_SPLINE_CURVE_WITH_KNOTS('',3,(#239257,#239258,#239259,#239260,#239261,
#239262,#239263,#239264,#239265,#239266,#239267,#239268,#239269,#239270,
#239271,#239272,#239273,#239274,#239275,#239276,#239277,#239278,#239279,
#239280,#239281,#239282,#239283,#239284,#239285,#239286,#239287,#239288,
#239289,#239290,#239291,#239292,#239293,#239294,#239295,#239296,#239297,
#239298,#239299,#239300,#239301,#239302,#239303,#239304,#239305,#239306,
#239307,#239308),.UNSPECIFIED.,.F.,.F.,(4,3,3,3,3,3,3,3,3,3,3,3,3,3,3,3,
3,4),(1.73472347597681E-18,4.30706237903578E-5,8.47417087758089E-5,0.000124159989214496,
0.000160467076301624,0.000170998382116703,0.000182414994733777,0.000213747977645874,
0.000242415955905344,0.000256497573175045,0.000259169422895618,0.000261757777312424,
0.000289965130400276,0.000301877270772905,0.000321937017503146,0.000326951954185706,
0.000334474359209547,0.000341996764233387),.UNSPECIFIED.);
#5184=B_SPLINE_CURVE_WITH_KNOTS('',3,(#239309,#239310,#239311,#239312,#239313,
#239314,#239315,#239316,#239317,#239318,#239319,#239320,#239321,#239322,
#239323,#239324,#239325,#239326,#239327,#239328,#239329,#239330,#239331,
#239332,#239333,#239334,#239335,#239336,#239337,#239338,#239339,#239340,
#239341,#239342,#239343,#239344,#239345,#239346,#239347,#239348,#239349,
#239350,#239351,#239352,#239353,#239354,#239355,#239356,#239357,#239358,
#239359,#239360),.UNSPECIFIED.,.F.,.F.,(4,3,3,3,3,3,3,3,3,3,3,3,3,3,3,3,
3,4),(0.,2.58457451683151E-5,4.25394446196292E-5,6.46659869687347E-5,7.57292581432875E-5,
8.12608937305638E-5,8.26438026273829E-5,8.67925293178402E-5,0.000116015624427729,
0.00013018879397676,0.00015188692630622,0.000161963651211276,0.00016273599247095,
0.00017358505863568,0.000212487880461049,0.000255238173512498,0.000301397761149868,
0.000347170117271345),.UNSPECIFIED.);
#5185=B_SPLINE_CURVE_WITH_KNOTS('',3,(#239362,#239363,#239364,#239365,#239366,
#239367,#239368,#239369,#239370,#239371,#239372,#239373,#239374,#239375,
#239376,#239377,#239378,#239379,#239380,#239381,#239382,#239383,#239384,
#239385,#239386,#239387,#239388,#239389,#239390,#239391,#239392,#239393,
#239394,#239395,#239396,#239397,#239398,#239399,#239400,#239401,#239402,
#239403,#239404,#239405,#239406,#239407),.UNSPECIFIED.,.F.,.F.,(4,3,3,3,
3,3,3,3,3,3,3,3,3,3,3,4),(0.,2.57218161996909E-5,4.21568322568114E-5,6.45873314617117E-5,
7.58025810641618E-5,8.14102058653869E-5,8.28121120656932E-5,8.7017830666612E-5,
0.000116081955658437,0.000130526745999918,0.000162394111022029,0.000174035661333224,
0.000213138396959559,0.000256116935436461,0.000302406662860391,0.000348071322666469),
 .UNSPECIFIED.);
#5186=B_SPLINE_CURVE_WITH_KNOTS('',3,(#239408,#239409,#239410,#239411,#239412,
#239413,#239414,#239415,#239416,#239417,#239418,#239419,#239420,#239421,
#239422,#239423,#239424,#239425,#239426,#239427,#239428,#239429,#239430,
#239431,#239432,#239433,#239434,#239435,#239436,#239437,#239438,#239439,
#239440,#239441,#239442,#239443,#239444,#239445,#239446,#239447,#239448,
#239449,#239450,#239451,#239452,#239453,#239454,#239455,#239456,#239457,
#239458,#239459),.UNSPECIFIED.,.F.,.F.,(4,3,3,3,3,3,3,3,3,3,3,3,3,3,3,3,
3,4),(0.,4.29652152190705E-5,8.44519107582359E-5,0.000123669830870871,0.000159788877364706,
0.000170558847912644,0.000181218775907184,0.000181960046452415,0.000214460062643127,
0.000244755726196831,0.000255838271868958,0.000258503253867592,0.00026108495517877,
0.000289370476648193,0.00030110132550202,0.000321109510663645,0.000331113603244458,
0.00034111769582527),.UNSPECIFIED.);
#5187=B_SPLINE_CURVE_WITH_KNOTS('',3,(#239461,#239462,#239463,#239464,#239465,
#239466,#239467,#239468,#239469,#239470,#239471,#239472,#239473,#239474,
#239475,#239476,#239477,#239478,#239479,#239480,#239481,#239482,#239483,
#239484,#239485,#239486,#239487,#239488,#239489,#239490,#239491,#239492,
#239493,#239494,#239495,#239496,#239497,#239498,#239499,#239500,#239501,
#239502,#239503,#239504,#239505,#239506,#239507,#239508,#239509,#239510,
#239511,#239512),.UNSPECIFIED.,.F.,.F.,(4,3,3,3,3,3,3,3,3,3,3,3,3,3,3,3,
3,4),(0.,4.30706237873028E-5,8.47417087702334E-5,0.00012415998920642,0.000160467076290766,
0.000170998382116705,0.000182414994733777,0.000213747977645876,0.000242415955903002,
0.000256497573175047,0.00025916942289562,0.000261757777312426,0.000289965130403416,
0.000301877270772908,0.000321937017503149,0.000326951954185709,0.000334474359209549,
0.00034199676423339),.UNSPECIFIED.);
#5188=B_SPLINE_CURVE_WITH_KNOTS('',3,(#239513,#239514,#239515,#239516,#239517,
#239518,#239519,#239520,#239521,#239522,#239523,#239524,#239525,#239526,
#239527,#239528,#239529,#239530,#239531,#239532,#239533,#239534,#239535,
#239536,#239537,#239538,#239539,#239540,#239541,#239542,#239543,#239544,
#239545,#239546,#239547,#239548,#239549,#239550,#239551,#239552,#239553,
#239554,#239555,#239556,#239557,#239558,#239559,#239560,#239561,#239562,
#239563,#239564),.UNSPECIFIED.,.F.,.F.,(4,3,3,3,3,3,3,3,3,3,3,3,3,3,3,3,
3,4),(0.,2.58457451661623E-5,4.25394446195541E-5,6.46659869686995E-5,7.57292581432722E-5,
8.12608937305585E-5,8.26438026273801E-5,8.67925293178448E-5,0.000116015624426535,
0.000130188793976767,0.000151886926306228,0.000161963651211281,0.000162735992470959,
0.00017358505863569,0.000212487880458905,0.000255238173506665,0.000301397761136841,
0.000347170117271379),.UNSPECIFIED.);
#5189=B_SPLINE_CURVE_WITH_KNOTS('',3,(#239566,#239567,#239568,#239569,#239570,
#239571,#239572,#239573,#239574,#239575,#239576,#239577,#239578,#239579,
#239580,#239581,#239582,#239583,#239584,#239585,#239586,#239587,#239588,
#239589,#239590,#239591,#239592,#239593,#239594,#239595,#239596,#239597,
#239598,#239599,#239600,#239601,#239602,#239603,#239604,#239605,#239606,
#239607,#239608,#239609,#239610,#239611),.UNSPECIFIED.,.F.,.F.,(4,3,3,3,
3,3,3,3,3,3,3,3,3,3,3,4),(0.,2.57218161991911E-5,4.21568322568509E-5,6.45873314617345E-5,
7.58025810641763E-5,8.14102058653972E-5,8.28121120657024E-5,8.70178306666181E-5,
0.000116081955657687,0.000130526745999927,0.000162394111022044,0.000174035661333236,
0.000213138396959808,0.000256116935436941,0.000302406662861117,0.000348071322666471),
 .UNSPECIFIED.);
#5190=B_SPLINE_CURVE_WITH_KNOTS('',3,(#239612,#239613,#239614,#239615,#239616,
#239617,#239618,#239619,#239620,#239621,#239622,#239623,#239624,#239625,
#239626,#239627,#239628,#239629,#239630,#239631,#239632,#239633,#239634,
#239635,#239636,#239637,#239638,#239639,#239640,#239641,#239642,#239643,
#239644,#239645,#239646,#239647,#239648,#239649,#239650,#239651,#239652,
#239653,#239654,#239655,#239656,#239657,#239658,#239659,#239660,#239661,
#239662,#239663),.UNSPECIFIED.,.F.,.F.,(4,3,3,3,3,3,3,3,3,3,3,3,3,3,3,3,
3,4),(4.33680868994202E-19,4.29652152163512E-5,8.44519107537964E-5,0.000123669830865421,
0.000159788877358528,0.000170558847912628,0.000181218775907168,0.000181960046452404,
0.000214460062643096,0.000244755726197257,0.000255838271868949,0.000258503253867584,
0.000261084955178762,0.000289370476649044,0.000301101325502016,0.000321109510663643,
0.000331113603244456,0.00034111769582527),.UNSPECIFIED.);
#5191=B_SPLINE_CURVE_WITH_KNOTS('',3,(#239665,#239666,#239667,#239668,#239669,
#239670,#239671,#239672,#239673,#239674,#239675,#239676,#239677,#239678,
#239679,#239680,#239681,#239682,#239683,#239684,#239685,#239686,#239687,
#239688,#239689,#239690,#239691,#239692,#239693,#239694,#239695,#239696,
#239697,#239698,#239699,#239700,#239701,#239702,#239703,#239704,#239705,
#239706,#239707,#239708,#239709,#239710,#239711,#239712,#239713,#239714,
#239715,#239716),.UNSPECIFIED.,.F.,.F.,(4,3,3,3,3,3,3,3,3,3,3,3,3,3,3,3,
3,4),(0.,4.30706237882266E-5,8.47417087718488E-5,0.000124159989208699,0.000160467076293763,
0.000170998382116694,0.00018241499473379,0.000213747977645869,0.000242415955902749,
0.000256497573175043,0.000259169422895617,0.000261757777312422,0.00028996513040296,
0.000301877270772907,0.00032193701750315,0.000326951954185711,0.000334474359209552,
0.000341996764233392),.UNSPECIFIED.);
#5192=B_SPLINE_CURVE_WITH_KNOTS('',3,(#239717,#239718,#239719,#239720,#239721,
#239722,#239723,#239724,#239725,#239726,#239727,#239728,#239729,#239730,
#239731,#239732,#239733,#239734,#239735,#239736,#239737,#239738,#239739,
#239740,#239741,#239742,#239743,#239744,#239745,#239746,#239747,#239748,
#239749,#239750,#239751,#239752,#239753,#239754,#239755,#239756,#239757,
#239758,#239759,#239760,#239761,#239762,#239763,#239764,#239765,#239766,
#239767,#239768),.UNSPECIFIED.,.F.,.F.,(4,3,3,3,3,3,3,3,3,3,3,3,3,3,3,3,
3,4),(0.,2.58457451676442E-5,4.25394446196521E-5,6.46659869687445E-5,7.57292581432907E-5,
8.12608937305638E-5,8.26438026273821E-5,8.67925293178369E-5,0.000116015624426859,
0.000130188793976755,0.000151886926306215,0.000161963651211276,0.000162735992470944,
0.000173585058635674,0.000212487880459347,0.000255238173508912,0.000301397761143805,
0.000347170117271363),.UNSPECIFIED.);
#5193=B_SPLINE_CURVE_WITH_KNOTS('',3,(#239770,#239771,#239772,#239773,#239774,
#239775,#239776,#239777,#239778,#239779,#239780,#239781,#239782,#239783,
#239784,#239785,#239786,#239787,#239788,#239789,#239790,#239791,#239792,
#239793,#239794,#239795,#239796,#239797,#239798,#239799,#239800,#239801,
#239802,#239803,#239804,#239805,#239806,#239807,#239808,#239809,#239810,
#239811,#239812,#239813,#239814,#239815),.UNSPECIFIED.,.F.,.F.,(4,3,3,3,
3,3,3,3,3,3,3,3,3,3,3,4),(6.95243322195995E-18,2.57218161995218E-5,4.21568322569579E-5,
6.45873314617886E-5,7.58025810642039E-5,8.14102058654115E-5,8.28121120657135E-5,
8.70178306666192E-5,0.000116081955659034,0.000130526745999925,0.000162394111022051,
0.000174035661333231,0.000213138396961045,0.000256116935439446,0.00030240666286506,
0.000348071322666456),.UNSPECIFIED.);
#5194=B_SPLINE_CURVE_WITH_KNOTS('',3,(#239816,#239817,#239818,#239819,#239820,
#239821,#239822,#239823,#239824,#239825,#239826,#239827,#239828,#239829,
#239830,#239831,#239832,#239833,#239834,#239835,#239836,#239837,#239838,
#239839,#239840,#239841,#239842,#239843,#239844,#239845,#239846,#239847,
#239848,#239849,#239850,#239851,#239852,#239853,#239854,#239855,#239856,
#239857,#239858,#239859,#239860,#239861,#239862,#239863,#239864,#239865,
#239866,#239867),.UNSPECIFIED.,.F.,.F.,(4,3,3,3,3,3,3,3,3,3,3,3,3,3,3,3,
3,4),(0.,4.29652152161983E-5,8.44519107532164E-5,0.00012366983086397,0.000159788877355752,
0.000170558847912625,0.000181218775907166,0.000181960046452406,0.000214460062642528,
0.000244755726195342,0.000255838271868948,0.000258503253867583,0.000261084955178761,
0.000289370476648543,0.000301101325502016,0.000321109510663643,0.000331113603244457,
0.000341117695825271),.UNSPECIFIED.);
#5195=B_SPLINE_CURVE_WITH_KNOTS('',3,(#239869,#239870,#239871,#239872,#239873,
#239874,#239875,#239876,#239877,#239878,#239879,#239880,#239881,#239882,
#239883,#239884,#239885,#239886,#239887,#239888,#239889,#239890,#239891,
#239892,#239893,#239894,#239895,#239896,#239897,#239898,#239899,#239900,
#239901,#239902,#239903,#239904,#239905,#239906,#239907,#239908,#239909,
#239910,#239911,#239912,#239913,#239914,#239915,#239916,#239917,#239918,
#239919,#239920),.UNSPECIFIED.,.F.,.F.,(4,3,3,3,3,3,3,3,3,3,3,3,3,3,3,3,
3,4),(0.,4.30706237856902E-5,8.47417087673733E-5,0.00012415998920248,0.000160467076285652,
0.000170998382116697,0.000182414994733777,0.000213747977645874,0.000242415955903854,
0.00025649757317505,0.000259169422895623,0.000261757777312429,0.000289965130402078,
0.000301877270772916,0.000321937017503159,0.00032695195418572,0.000334474359209561,
0.000341996764233403),.UNSPECIFIED.);
#5196=B_SPLINE_CURVE_WITH_KNOTS('',3,(#239921,#239922,#239923,#239924,#239925,
#239926,#239927,#239928,#239929,#239930,#239931,#239932,#239933,#239934,
#239935,#239936,#239937,#239938,#239939,#239940,#239941,#239942,#239943,
#239944,#239945,#239946,#239947,#239948,#239949,#239950,#239951,#239952,
#239953,#239954,#239955,#239956,#239957,#239958,#239959,#239960,#239961,
#239962,#239963,#239964,#239965,#239966,#239967,#239968,#239969,#239970,
#239971,#239972),.UNSPECIFIED.,.F.,.F.,(4,3,3,3,3,3,3,3,3,3,3,3,3,3,3,3,
3,4),(3.46944695195361E-18,2.58457451684559E-5,4.25394446196587E-5,6.46659869687525E-5,
7.57292581432994E-5,8.12608937305728E-5,8.26438026273912E-5,8.67925293178463E-5,
0.000116015624427615,0.000130188793976768,0.000151886926306228,0.000161963651211276,
0.000162735992470959,0.000173585058635689,0.000212487880459735,0.000255238173508576,
0.000301397761140788,0.000347170117271376),.UNSPECIFIED.);
#5197=B_SPLINE_CURVE_WITH_KNOTS('',3,(#239974,#239975,#239976,#239977,#239978,
#239979,#239980,#239981,#239982,#239983,#239984,#239985,#239986,#239987,
#239988,#239989,#239990,#239991,#239992,#239993,#239994,#239995,#239996,
#239997,#239998,#239999,#240000,#240001,#240002,#240003,#240004,#240005,
#240006,#240007,#240008,#240009,#240010,#240011,#240012,#240013,#240014,
#240015,#240016,#240017,#240018,#240019),.UNSPECIFIED.,.F.,.F.,(4,3,3,3,
3,3,3,3,3,3,3,3,3,3,3,4),(0.,2.5721816198903E-5,4.21568322569722E-5,6.45873314617926E-5,
7.58025810642029E-5,8.1410205865408E-5,8.28121120657092E-5,8.70178306666131E-5,
0.000116081955658234,0.00013052674599992,0.000162394111022023,0.000174035661333226,
0.000213138396959779,0.000256116935436934,0.000302406662861205,0.000348071322666452),
 .UNSPECIFIED.);
#5198=B_SPLINE_CURVE_WITH_KNOTS('',3,(#240020,#240021,#240022,#240023,#240024,
#240025,#240026,#240027,#240028,#240029,#240030,#240031,#240032,#240033,
#240034,#240035,#240036,#240037,#240038,#240039,#240040,#240041,#240042,
#240043,#240044,#240045,#240046,#240047,#240048,#240049,#240050,#240051,
#240052,#240053,#240054,#240055,#240056,#240057,#240058,#240059,#240060,
#240061,#240062,#240063,#240064,#240065,#240066,#240067,#240068,#240069,
#240070,#240071),.UNSPECIFIED.,.F.,.F.,(4,3,3,3,3,3,3,3,3,3,3,3,3,3,3,3,
3,4),(4.33680868994202E-19,4.29652152147306E-5,8.4451910751015E-5,0.000123669830861697,
0.00015978887735388,0.000170558847912629,0.000181218775907168,0.000181960046452407,
0.000214460062643719,0.000244755726198878,0.000255838271868943,0.000258503253867578,
0.000261084955178756,0.000289370476647109,0.000301101325502007,0.000321109510663632,
0.000331113603244445,0.000341117695825258),.UNSPECIFIED.);
#5199=B_SPLINE_CURVE_WITH_KNOTS('',3,(#240073,#240074,#240075,#240076,#240077,
#240078,#240079,#240080,#240081,#240082,#240083,#240084,#240085,#240086,
#240087,#240088,#240089,#240090,#240091,#240092,#240093,#240094,#240095,
#240096,#240097,#240098,#240099,#240100,#240101,#240102,#240103,#240104,
#240105,#240106,#240107,#240108,#240109,#240110,#240111,#240112,#240113,
#240114,#240115,#240116,#240117,#240118,#240119,#240120,#240121,#240122,
#240123,#240124),.UNSPECIFIED.,.F.,.F.,(4,3,3,3,3,3,3,3,3,3,3,3,3,3,3,3,
3,4),(0.,4.30706237868881E-5,8.4741708769574E-5,0.000124159989205557,0.000160467076289722,
0.000170998382116688,0.000182414994733766,0.000213747977645864,0.000242415955901617,
0.000256497573175039,0.000259169422895613,0.000261757777312418,0.000289965130404738,
0.000301877270772905,0.000321937017503148,0.000326951954185709,0.00033447435920955,
0.000341996764233391),.UNSPECIFIED.);
#5200=B_SPLINE_CURVE_WITH_KNOTS('',3,(#240125,#240126,#240127,#240128,#240129,
#240130,#240131,#240132,#240133,#240134,#240135,#240136,#240137,#240138,
#240139,#240140,#240141,#240142,#240143,#240144,#240145,#240146,#240147,
#240148,#240149,#240150,#240151,#240152,#240153,#240154,#240155,#240156,
#240157,#240158,#240159,#240160,#240161,#240162,#240163,#240164,#240165,
#240166,#240167,#240168,#240169,#240170,#240171,#240172,#240173,#240174,
#240175,#240176),.UNSPECIFIED.,.F.,.F.,(4,3,3,3,3,3,3,3,3,3,3,3,3,3,3,3,
3,4),(3.46944695195361E-18,2.58457451686505E-5,4.25394446196537E-5,6.46659869687495E-5,
7.57292581432974E-5,8.12608937305713E-5,8.26438026273898E-5,8.67925293178453E-5,
0.000116015624427858,0.000130188793976766,0.000151886926306227,0.000161963651211277,
0.000162735992470957,0.000173585058635687,0.000212487880459702,0.000255238173508743,
0.000301397761141439,0.000347170117271355),.UNSPECIFIED.);
#5201=B_SPLINE_CURVE_WITH_KNOTS('',3,(#240178,#240179,#240180,#240181,#240182,
#240183,#240184,#240185,#240186,#240187,#240188,#240189,#240190,#240191,
#240192,#240193,#240194,#240195,#240196,#240197,#240198,#240199,#240200,
#240201,#240202,#240203,#240204,#240205,#240206,#240207,#240208,#240209,
#240210,#240211,#240212,#240213,#240214,#240215,#240216,#240217,#240218,
#240219,#240220,#240221,#240222,#240223),.UNSPECIFIED.,.F.,.F.,(4,3,3,3,
3,3,3,3,3,3,3,3,3,3,3,4),(0.,2.57218162003092E-5,4.21568322568195E-5,6.45873314617163E-5,
7.58025810641646E-5,8.14102058653888E-5,8.28121120656949E-5,8.7017830666613E-5,
0.000116081955658734,0.00013052674599992,0.000162394111022031,0.000174035661333226,
0.000213138396957737,0.000256116935432863,0.000302406662854935,0.000348071322666467),
 .UNSPECIFIED.);
#5202=B_SPLINE_CURVE_WITH_KNOTS('',3,(#240224,#240225,#240226,#240227,#240228,
#240229,#240230,#240231,#240232,#240233,#240234,#240235,#240236,#240237,
#240238,#240239,#240240,#240241,#240242,#240243,#240244,#240245,#240246,
#240247,#240248,#240249,#240250,#240251,#240252,#240253,#240254,#240255,
#240256,#240257,#240258,#240259,#240260,#240261,#240262,#240263,#240264,
#240265,#240266,#240267,#240268,#240269,#240270,#240271,#240272,#240273,
#240274,#240275),.UNSPECIFIED.,.F.,.F.,(4,3,3,3,3,3,3,3,3,3,3,3,3,3,3,3,
3,4),(0.,4.29652152126629E-5,8.44519107479425E-5,0.000123669830858356,0.000159788877350821,
0.000170558847912639,0.000181218775907178,0.000181960046452419,0.000214460062643348,
0.000244755726197514,0.000255838271868955,0.00025850325386759,0.000261084955178767,
0.000289370476647847,0.000301101325502019,0.000321109510663645,0.000331113603244458,
0.000341117695825271),.UNSPECIFIED.);
#5203=B_SPLINE_CURVE_WITH_KNOTS('',3,(#240277,#240278,#240279,#240280,#240281,
#240282,#240283,#240284,#240285,#240286,#240287,#240288,#240289,#240290,
#240291,#240292,#240293,#240294,#240295,#240296,#240297,#240298,#240299,
#240300,#240301,#240302,#240303,#240304,#240305,#240306,#240307,#240308,
#240309,#240310,#240311,#240312,#240313,#240314,#240315,#240316,#240317,
#240318,#240319,#240320,#240321,#240322,#240323,#240324,#240325,#240326,
#240327,#240328),.UNSPECIFIED.,.F.,.F.,(4,3,3,3,3,3,3,3,3,3,3,3,3,3,3,3,
3,4),(8.67361737988403E-19,4.30706237870993E-5,8.47417087698459E-5,0.000124159989205834,
0.000160467076289949,0.000170998382116697,0.000182414994733785,0.000213747977645869,
0.0002424159559032,0.00025649757317504,0.000259169422895614,0.000261757777312419,
0.000289965130403263,0.000301877270772901,0.000321937017503143,0.000326951954185703,
0.000334474359209543,0.000341996764233384),.UNSPECIFIED.);
#5204=B_SPLINE_CURVE_WITH_KNOTS('',3,(#240329,#240330,#240331,#240332,#240333,
#240334,#240335,#240336,#240337,#240338,#240339,#240340,#240341,#240342,
#240343,#240344,#240345,#240346,#240347,#240348,#240349,#240350,#240351,
#240352,#240353,#240354,#240355,#240356,#240357,#240358,#240359,#240360,
#240361,#240362,#240363,#240364,#240365,#240366,#240367,#240368,#240369,
#240370,#240371,#240372,#240373,#240374,#240375,#240376,#240377,#240378,
#240379,#240380),.UNSPECIFIED.,.F.,.F.,(4,3,3,3,3,3,3,3,3,3,3,3,3,3,3,3,
3,4),(0.,2.58457451673367E-5,4.25394446196646E-5,6.46659869687537E-5,7.57292581432982E-5,
8.12608937305705E-5,8.26438026273886E-5,8.67925293178428E-5,0.000116015624426733,
0.000130188793976764,0.000151886926306225,0.000161963651211275,0.000162735992470955,
0.000173585058635686,0.000212487880457774,0.000255238173504083,0.0003013977611323,
0.00034717011727137),.UNSPECIFIED.);
#5205=B_SPLINE_CURVE_WITH_KNOTS('',3,(#240382,#240383,#240384,#240385,#240386,
#240387,#240388,#240389,#240390,#240391,#240392,#240393,#240394,#240395,
#240396,#240397,#240398,#240399,#240400,#240401,#240402,#240403,#240404,
#240405,#240406,#240407,#240408,#240409,#240410,#240411,#240412,#240413,
#240414,#240415,#240416,#240417,#240418,#240419,#240420,#240421,#240422,
#240423,#240424,#240425,#240426,#240427),.UNSPECIFIED.,.F.,.F.,(4,3,3,3,
3,3,3,3,3,3,3,3,3,3,3,4),(0.,2.57218162008265E-5,4.21568322568929E-5,6.45873314617525E-5,
7.58025810641823E-5,8.14102058653972E-5,8.28121120657009E-5,8.70178306666121E-5,
0.000116081955659349,0.000130526745999918,0.000162394111022029,0.000174035661333224,
0.000213138396959796,0.00025611693543712,0.000302406662862035,0.000348071322666464),
 .UNSPECIFIED.);
#5206=B_SPLINE_CURVE_WITH_KNOTS('',3,(#240428,#240429,#240430,#240431,#240432,
#240433,#240434,#240435,#240436,#240437,#240438,#240439,#240440,#240441,
#240442,#240443,#240444,#240445,#240446,#240447,#240448,#240449,#240450,
#240451,#240452,#240453,#240454,#240455,#240456,#240457,#240458,#240459,
#240460,#240461,#240462,#240463,#240464,#240465,#240466,#240467,#240468,
#240469,#240470,#240471,#240472,#240473,#240474,#240475,#240476,#240477,
#240478,#240479),.UNSPECIFIED.,.F.,.F.,(4,3,3,3,3,3,3,3,3,3,3,3,3,3,3,3,
3,4),(0.,4.29652152136727E-5,8.44519107495488E-5,0.000123669830860388,0.000159788877352989,
0.000170558847912636,0.000181218775907175,0.000181960046452406,0.000214460062643941,
0.000244755726199492,0.000255838271868946,0.00025850325386758,0.000261084955178758,
0.000289370476647275,0.000301101325502007,0.000321109510663631,0.000331113603244443,
0.000341117695825255),.UNSPECIFIED.);
#5207=B_SPLINE_CURVE_WITH_KNOTS('',3,(#240481,#240482,#240483,#240484,#240485,
#240486,#240487,#240488,#240489,#240490,#240491,#240492,#240493,#240494,
#240495,#240496,#240497,#240498,#240499,#240500,#240501,#240502,#240503,
#240504,#240505,#240506,#240507,#240508,#240509,#240510,#240511,#240512,
#240513,#240514,#240515,#240516,#240517,#240518,#240519,#240520,#240521,
#240522,#240523,#240524,#240525,#240526,#240527,#240528,#240529,#240530,
#240531,#240532),.UNSPECIFIED.,.F.,.F.,(4,3,3,3,3,3,3,3,3,3,3,3,3,3,3,3,
3,4),(1.22969749649977E-17,4.30706237866378E-5,8.47417087689707E-5,0.000124159989204571,
0.000160467076288245,0.000170998382116699,0.000182414994733777,0.000213747977645869,
0.000242415955902751,0.000256497573175039,0.000259169422895612,0.000261757777312417,
0.000289965130403974,0.000301877270772898,0.000321937017503138,0.000326951954185699,
0.000334474359209539,0.000341996764233379),.UNSPECIFIED.);
#5208=B_SPLINE_CURVE_WITH_KNOTS('',3,(#240533,#240534,#240535,#240536,#240537,
#240538,#240539,#240540,#240541,#240542,#240543,#240544,#240545,#240546,
#240547,#240548,#240549,#240550,#240551,#240552,#240553,#240554,#240555,
#240556,#240557,#240558,#240559,#240560,#240561,#240562,#240563,#240564,
#240565,#240566,#240567,#240568,#240569,#240570,#240571,#240572,#240573,
#240574,#240575,#240576,#240577,#240578,#240579,#240580,#240581,#240582,
#240583,#240584),.UNSPECIFIED.,.F.,.F.,(4,3,3,3,3,3,3,3,3,3,3,3,3,3,3,3,
3,4),(0.,2.58457451669027E-5,4.25394446195448E-5,6.46659869686927E-5,7.57292581432667E-5,
8.12608937305537E-5,8.26438026273754E-5,8.67925293178407E-5,0.000116015624426837,
0.000130188793976761,0.000151886926306221,0.000161963651211277,0.000162735992470951,
0.000173585058635681,0.000212487880459692,0.0002552381735098,0.000301397761145626,
0.000347170117271346),.UNSPECIFIED.);
#5209=B_SPLINE_CURVE_WITH_KNOTS('',3,(#240586,#240587,#240588,#240589,#240590,
#240591,#240592,#240593,#240594,#240595,#240596,#240597,#240598,#240599,
#240600,#240601,#240602,#240603,#240604,#240605,#240606,#240607,#240608,
#240609,#240610,#240611,#240612,#240613,#240614,#240615,#240616,#240617,
#240618,#240619,#240620,#240621,#240622,#240623,#240624,#240625,#240626,
#240627,#240628,#240629,#240630,#240631),.UNSPECIFIED.,.F.,.F.,(4,3,3,3,
3,3,3,3,3,3,3,3,3,3,3,4),(0.,2.5721816200257E-5,4.21568322568039E-5,6.45873314617086E-5,
7.5802581064161E-5,8.14102058653872E-5,8.28121120656937E-5,8.70178306666133E-5,
0.000116081955658472,0.00013052674599992,0.000162394111022039,0.000174035661333227,
0.000213138396957767,0.000256116935432745,0.000302406662854146,0.00034807132266647),
 .UNSPECIFIED.);
#5210=B_SPLINE_CURVE_WITH_KNOTS('',3,(#240632,#240633,#240634,#240635,#240636,
#240637,#240638,#240639,#240640,#240641,#240642,#240643,#240644,#240645,
#240646,#240647,#240648,#240649,#240650,#240651,#240652,#240653,#240654,
#240655,#240656,#240657,#240658,#240659,#240660,#240661,#240662,#240663,
#240664,#240665,#240666,#240667,#240668,#240669,#240670,#240671,#240672,
#240673,#240674,#240675,#240676,#240677,#240678,#240679,#240680,#240681,
#240682,#240683),.UNSPECIFIED.,.F.,.F.,(4,3,3,3,3,3,3,3,3,3,3,3,3,3,3,3,
3,4),(4.33680868994202E-19,4.2965215214098E-5,8.44519107505796E-5,0.000123669830862313,
0.000159788877356241,0.000170558847912639,0.000181218775907178,0.000181960046452412,
0.000214460062644004,0.000244755726199407,0.000255838271868955,0.000258503253867589,
0.000261084955178767,0.000289370476646998,0.000301101325502019,0.000321109510663644,
0.000331113603244457,0.00034111769582527),.UNSPECIFIED.);
#5211=B_SPLINE_CURVE_WITH_KNOTS('',3,(#240685,#240686,#240687,#240688,#240689,
#240690,#240691,#240692,#240693,#240694,#240695,#240696,#240697,#240698,
#240699,#240700,#240701,#240702,#240703,#240704,#240705,#240706,#240707,
#240708,#240709,#240710,#240711,#240712,#240713,#240714,#240715,#240716,
#240717,#240718,#240719,#240720,#240721,#240722,#240723,#240724,#240725,
#240726,#240727,#240728,#240729,#240730,#240731,#240732,#240733,#240734,
#240735,#240736),.UNSPECIFIED.,.F.,.F.,(4,3,3,3,3,3,3,3,3,3,3,3,3,3,3,3,
3,4),(0.,4.30706237867457E-5,8.47417087691177E-5,0.00012415998920471,0.000160467076288282,
0.000170998382116703,0.000182414994733785,0.000213747977645875,0.00024241595590493,
0.000256497573175048,0.000259169422895621,0.000261757777312427,0.000289965130402185,
0.000301877270772907,0.000321937017503147,0.000326951954185707,0.000334474359209547,
0.000341996764233387),.UNSPECIFIED.);
#5212=B_SPLINE_CURVE_WITH_KNOTS('',3,(#240737,#240738,#240739,#240740,#240741,
#240742,#240743,#240744,#240745,#240746,#240747,#240748,#240749,#240750,
#240751,#240752,#240753,#240754,#240755,#240756,#240757,#240758,#240759,
#240760,#240761,#240762,#240763,#240764,#240765,#240766,#240767,#240768,
#240769,#240770,#240771,#240772,#240773,#240774,#240775,#240776,#240777,
#240778,#240779,#240780,#240781,#240782,#240783,#240784,#240785,#240786,
#240787,#240788),.UNSPECIFIED.,.F.,.F.,(4,3,3,3,3,3,3,3,3,3,3,3,3,3,3,3,
3,4),(0.,2.58457451683501E-5,4.25394446195563E-5,6.46659869686992E-5,7.57292581432707E-5,
8.12608937305565E-5,8.26438026273779E-5,8.67925293178422E-5,0.000116015624427275,
0.000130188793976763,0.000151886926306224,0.000161963651211262,0.000162735992470954,
0.000173585058635684,0.000212487880461338,0.000255238173512569,0.000301397761148645,
0.000347170117271369),.UNSPECIFIED.);
#5213=B_SPLINE_CURVE_WITH_KNOTS('',3,(#240790,#240791,#240792,#240793,#240794,
#240795,#240796,#240797,#240798,#240799,#240800,#240801,#240802,#240803,
#240804,#240805,#240806,#240807,#240808,#240809,#240810,#240811,#240812,
#240813,#240814,#240815,#240816,#240817,#240818,#240819,#240820,#240821,
#240822,#240823,#240824,#240825,#240826,#240827,#240828,#240829,#240830,
#240831,#240832,#240833,#240834,#240835),.UNSPECIFIED.,.F.,.F.,(4,3,3,3,
3,3,3,3,3,3,3,3,3,3,3,4),(0.,2.57218161991932E-5,4.21568322567385E-5,6.45873314616776E-5,
7.58025810641472E-5,8.1410205865382E-5,8.28121120656907E-5,8.70178306666167E-5,
0.00011608195565819,0.000130526745999925,0.00016239411102205,0.000174035661333233,
0.000213138396959465,0.00025611693543621,0.00030240666285981,0.000348071322666468),
 .UNSPECIFIED.);
#5214=B_SPLINE_CURVE_WITH_KNOTS('',3,(#240836,#240837,#240838,#240839,#240840,
#240841,#240842,#240843,#240844,#240845,#240846,#240847,#240848,#240849,
#240850,#240851,#240852,#240853,#240854,#240855,#240856,#240857,#240858,
#240859,#240860,#240861,#240862,#240863,#240864,#240865,#240866,#240867,
#240868,#240869,#240870,#240871,#240872,#240873,#240874,#240875,#240876,
#240877,#240878,#240879,#240880,#240881,#240882,#240883,#240884,#240885,
#240886,#240887),.UNSPECIFIED.,.F.,.F.,(4,3,3,3,3,3,3,3,3,3,3,3,3,3,3,3,
3,4),(0.,4.29652152176409E-5,8.44519107557594E-5,0.000123669830867554,0.000159788877360428,
0.000170558847912633,0.000181218775907172,0.000181960046452405,0.000214460062643479,
0.000244755726198168,0.000255838271868949,0.000258503253867584,0.000261084955178762,
0.000289370476647912,0.000301101325502014,0.00032110951066364,0.000331113603244453,
0.000341117695825266),.UNSPECIFIED.);
#5215=B_SPLINE_CURVE_WITH_KNOTS('',3,(#253551,#253552,#253553,#253554),
 .UNSPECIFIED.,.F.,.F.,(4,4),(1.73472347597681E-17,0.000497709506657957),
 .UNSPECIFIED.);
#5216=B_SPLINE_CURVE_WITH_KNOTS('',3,(#253556,#253557,#253558,#253559,#253560,
#253561,#253562,#253563,#253564,#253565,#253566,#253567,#253568,#253569,
#253570,#253571,#253572,#253573,#253574,#253575,#253576,#253577),
 .UNSPECIFIED.,.F.,.F.,(4,2,2,2,2,2,2,2,2,2,4),(0.000497709506657957,0.000958469059060371,
0.00141922861146278,0.0018799881638652,0.0021103679400664,0.0021679628841167,
0.00219676035614186,0.00222555782816702,0.00225435530019218,0.00228315277221733,
0.00234074771626765),.UNSPECIFIED.);
#5217=B_SPLINE_CURVE_WITH_KNOTS('',3,(#253583,#253584,#253585,#253586,#253587,
#253588,#253589,#253590,#253591,#253592,#253593,#253594,#253595,#253596,
#253597,#253598,#253599,#253600,#253601,#253602,#253603,#253604),
 .UNSPECIFIED.,.F.,.F.,(4,2,2,2,2,2,2,2,2,2,4),(1.9871740492849E-9,5.85234868205088E-5,
8.77842366437273E-5,0.000117044986466946,0.000146305736290164,0.000175566486113383,
0.000234087985759818,0.000468173984345514,0.000936345981516908,0.0014045179786883,
0.00187268997585969),.UNSPECIFIED.);
#5218=B_SPLINE_CURVE_WITH_KNOTS('',3,(#253606,#253607,#253608,#253609,#253610,
#253611,#253612,#253613,#253614,#253615,#253616,#253617,#253618,#253619,
#253620,#253621,#253622,#253623,#253624,#253625,#253626,#253627),
 .UNSPECIFIED.,.F.,.F.,(4,3,3,3,3,3,3,4),(0.00187268997585969,0.00199834274779399,
0.00204546253726935,0.00208669235306029,0.00220550294837832,0.00223099670832857,
0.00230314888596272,0.00237530106359686),.UNSPECIFIED.);
#5219=B_SPLINE_CURVE_WITH_KNOTS('',3,(#253635,#253636,#253637,#253638),
 .UNSPECIFIED.,.F.,.F.,(4,4),(3.46944695195361E-18,0.000776824705292371),
 .UNSPECIFIED.);
#5220=B_SPLINE_CURVE_WITH_KNOTS('',3,(#253640,#253641,#253642,#253643),
 .UNSPECIFIED.,.F.,.F.,(4,4),(0.,0.000776824705292379),.UNSPECIFIED.);
#5221=B_SPLINE_CURVE_WITH_KNOTS('',3,(#253682,#253683,#253684,#253685,#253686,
#253687,#253688,#253689,#253690,#253691),.UNSPECIFIED.,.F.,.F.,(4,3,3,4),
(0.00224752972328446,0.00254000000002921,0.0127000000034794,0.0252059134417286),
 .UNSPECIFIED.);
#5222=B_SPLINE_CURVE_WITH_KNOTS('',3,(#253695,#253696,#253697,#253698),
 .UNSPECIFIED.,.F.,.F.,(4,4),(-1.43540833573195E-5,0.000600070195786084),
 .UNSPECIFIED.);
#5223=B_SPLINE_CURVE_WITH_KNOTS('',3,(#253700,#253701,#253702,#253703,#253704,
#253705,#253706,#253707,#253708,#253709,#253710,#253711,#253712,#253713,
#253714,#253715,#253716,#253717,#253718,#253719,#253720,#253721,#253722,
#253723,#253724,#253725,#253726,#253727,#253728,#253729,#253730,#253731,
#253732,#253733,#253734,#253735,#253736,#253737,#253738,#253739,#253740,
#253741,#253742,#253743,#253744,#253745,#253746,#253747,#253748,#253749,
#253750,#253751,#253752,#253753,#253754),.UNSPECIFIED.,.F.,.F.,(4,3,3,3,
3,3,3,3,3,3,3,3,3,3,3,3,3,3,4),(0.000110053346854241,0.000527311723102858,
0.000718200211016914,0.000854122275949536,0.00126501374481543,0.00132634707517959,
0.00168651061235045,0.00193449393934226,0.00222985612775647,0.00251426340799128,
0.00254264080350493,0.00300412786917268,0.00333765384253305,0.00375893453183028,
0.00409210357716868,0.00415888746486257,0.00449321052526377,0.00480933253535804,
0.00497522826015563),.UNSPECIFIED.);
#5224=B_SPLINE_CURVE_WITH_KNOTS('',3,(#253758,#253759,#253760,#253761,#253762,
#253763,#253764,#253765,#253766,#253767,#253768,#253769,#253770,#253771,
#253772,#253773,#253774,#253775,#253776,#253777,#253778,#253779,#253780,
#253781,#253782,#253783,#253784,#253785,#253786,#253787,#253788,#253789,
#253790,#253791,#253792,#253793,#253794,#253795,#253796,#253797,#253798,
#253799,#253800,#253801,#253802,#253803,#253804,#253805,#253806),
 .UNSPECIFIED.,.F.,.F.,(4,3,3,3,3,3,3,3,3,3,3,3,3,3,3,3,4),(0.,0.000552804620400313,
0.000807500349755513,0.0012059666217394,0.00162007673419067,0.0021864702767717,
0.00241193324347881,0.00243219312565017,0.00283904062399015,0.00315006133501463,
0.0032484770180594,0.00361789986521821,0.00391885772791828,0.00407541417390928,
0.00422088317608792,0.00461166893086815,0.00482386648695763),
 .UNSPECIFIED.);
#5225=B_SPLINE_CURVE_WITH_KNOTS('',3,(#253807,#253808,#253809,#253810),
 .UNSPECIFIED.,.F.,.F.,(4,4),(6.04918746141641E-17,0.000614424279130608),
 .UNSPECIFIED.);
#5226=B_SPLINE_CURVE_WITH_KNOTS('',3,(#253812,#253813,#253814,#253815),
 .UNSPECIFIED.,.F.,.F.,(4,4),(-1.43540833568566E-5,0.000600070195786399),
 .UNSPECIFIED.);
#5227=B_SPLINE_CURVE_WITH_KNOTS('',3,(#253817,#253818,#253819,#253820,#253821,
#253822,#253823,#253824,#253825,#253826,#253827,#253828,#253829,#253830,
#253831,#253832,#253833,#253834,#253835,#253836,#253837,#253838,#253839,
#253840,#253841,#253842,#253843,#253844,#253845,#253846,#253847,#253848,
#253849,#253850,#253851,#253852,#253853,#253854,#253855,#253856,#253857,
#253858,#253859,#253860,#253861,#253862,#253863,#253864,#253865,#253866,
#253867,#253868,#253869,#253870,#253871),.UNSPECIFIED.,.F.,.F.,(4,3,3,3,
3,3,3,3,3,3,3,3,3,3,3,3,3,3,4),(0.000110053346854265,0.000527311723250969,
0.000718200211016931,0.000854122275951405,0.00126501374442658,0.0013263470751796,
0.00168651061235195,0.00193449393934226,0.00222985612779087,0.0025142634079924,
0.00254264080350493,0.00300412786893507,0.00333765384253336,0.00375893453183026,
0.00409210357719457,0.00415888746486208,0.00449321052529187,0.0048093325354323,
0.00497522826015559),.UNSPECIFIED.);
#5228=B_SPLINE_CURVE_WITH_KNOTS('',3,(#253875,#253876,#253877,#253878,#253879,
#253880,#253881,#253882,#253883,#253884,#253885,#253886,#253887,#253888,
#253889,#253890,#253891,#253892,#253893,#253894,#253895,#253896,#253897,
#253898,#253899,#253900,#253901,#253902,#253903,#253904,#253905,#253906,
#253907,#253908,#253909,#253910,#253911,#253912,#253913,#253914,#253915,
#253916,#253917,#253918,#253919,#253920,#253921,#253922,#253923),
 .UNSPECIFIED.,.F.,.F.,(4,3,3,3,3,3,3,3,3,3,3,3,3,3,3,3,4),(0.,0.000552804620158884,
0.000807500349754644,0.00120596662173943,0.00162007673419057,0.00218647027534087,
0.00241193324347885,0.00243219312565013,0.00283904062398887,0.00315006133493916,
0.00324847701805844,0.00361789986521828,0.00391885772791061,0.00407541417390921,
0.00422088317608798,0.00461166893084222,0.00482386648695769),
 .UNSPECIFIED.);
#5229=B_SPLINE_CURVE_WITH_KNOTS('',3,(#253925,#253926,#253927,#253928),
 .UNSPECIFIED.,.F.,.F.,(4,4),(1.47196168001604E-17,0.000614424279130721),
 .UNSPECIFIED.);
#5230=B_SPLINE_CURVE_WITH_KNOTS('',3,(#253932,#253933,#253934,#253935),
 .UNSPECIFIED.,.F.,.F.,(4,4),(-1.43540833566919E-5,0.000600070195786593),
 .UNSPECIFIED.);
#5231=B_SPLINE_CURVE_WITH_KNOTS('',3,(#253937,#253938,#253939,#253940,#253941,
#253942,#253943,#253944,#253945,#253946,#253947,#253948,#253949,#253950,
#253951,#253952,#253953,#253954,#253955,#253956,#253957,#253958,#253959,
#253960,#253961,#253962,#253963,#253964,#253965,#253966,#253967,#253968,
#253969,#253970,#253971,#253972,#253973,#253974,#253975,#253976,#253977,
#253978,#253979,#253980,#253981,#253982,#253983,#253984,#253985,#253986,
#253987,#253988,#253989,#253990,#253991),.UNSPECIFIED.,.F.,.F.,(4,3,3,3,
3,3,3,3,3,3,3,3,3,3,3,3,3,3,4),(0.000110053346854152,0.000527311722902683,
0.000718200211016838,0.000854122275951347,0.00126501374420219,0.00132634707517952,
0.0016865106123519,0.00193449393934221,0.00222985612782565,0.00251426340799237,
0.0025426408035049,0.00300412786903708,0.00333765384253382,0.00375893453183027,
0.00409210357719504,0.00415888746486192,0.00449321052529251,0.00480933253544403,
0.00497522826015564),.UNSPECIFIED.);
#5232=B_SPLINE_CURVE_WITH_KNOTS('',3,(#253995,#253996,#253997,#253998,#253999,
#254000,#254001,#254002,#254003,#254004,#254005,#254006,#254007,#254008,
#254009,#254010,#254011,#254012,#254013,#254014,#254015,#254016,#254017,
#254018,#254019,#254020,#254021,#254022,#254023,#254024,#254025,#254026,
#254027,#254028,#254029,#254030,#254031,#254032,#254033,#254034,#254035,
#254036,#254037,#254038,#254039,#254040,#254041,#254042,#254043),
 .UNSPECIFIED.,.F.,.F.,(4,3,3,3,3,3,3,3,3,3,3,3,3,3,3,3,4),(0.,0.000552804620541596,
0.000807500349756771,0.00120596662173938,0.00162007673419107,0.00218647027691998,
0.00241193324347875,0.0024321931256513,0.00283904062399194,0.00315006133501802,
0.0032484770180609,0.00361789986521813,0.00391885772790124,0.00407541417391128,
0.00422088317608781,0.00461166893077222,0.00482386648695749),
 .UNSPECIFIED.);
#5233=B_SPLINE_CURVE_WITH_KNOTS('',3,(#254045,#254046,#254047,#254048),
 .UNSPECIFIED.,.F.,.F.,(4,4),(9.81307786677359E-18,0.000614424279130633),
 .UNSPECIFIED.);
#5234=B_SPLINE_CURVE_WITH_KNOTS('',3,(#254052,#254053,#254054,#254055),
 .UNSPECIFIED.,.F.,.F.,(4,4),(-1.43540833570327E-5,0.000600070195786076),
 .UNSPECIFIED.);
#5235=B_SPLINE_CURVE_WITH_KNOTS('',3,(#254057,#254058,#254059,#254060,#254061,
#254062,#254063,#254064,#254065,#254066,#254067,#254068,#254069,#254070,
#254071,#254072,#254073,#254074,#254075,#254076,#254077,#254078,#254079,
#254080,#254081,#254082,#254083,#254084,#254085,#254086,#254087,#254088,
#254089,#254090,#254091,#254092,#254093,#254094,#254095,#254096,#254097,
#254098,#254099,#254100,#254101,#254102,#254103,#254104,#254105),
 .UNSPECIFIED.,.F.,.F.,(4,3,3,3,3,3,3,3,3,3,3,3,3,3,3,3,4),(0.000110053346854173,
0.000473524686504124,0.000718200211016846,0.000901529016375351,0.00127176706121883,
0.00132634707517952,0.00172429792281351,0.00193449393934219,0.00223976927323974,
0.00254238596260925,0.00254264080350487,0.00299415722452071,0.00335632568019801,
0.00375893453183022,0.00415022436231754,0.00456272631123656,0.00497522826015557),
 .UNSPECIFIED.);
#5236=B_SPLINE_CURVE_WITH_KNOTS('',3,(#254109,#254110,#254111,#254112,#254113,
#254114,#254115,#254116,#254117,#254118,#254119,#254120,#254121,#254122,
#254123,#254124,#254125,#254126,#254127,#254128,#254129,#254130,#254131,
#254132,#254133,#254134,#254135,#254136,#254137,#254138,#254139,#254140,
#254141,#254142,#254143,#254144,#254145,#254146,#254147,#254148,#254149,
#254150,#254151,#254152,#254153,#254154,#254155,#254156,#254157),
 .UNSPECIFIED.,.F.,.F.,(4,3,3,3,3,3,3,3,3,3,3,3,3,3,3,3,4),(0.,0.000552804620209682,
0.000807500349754742,0.00120596662173942,0.00162007673419038,0.00218647027609432,
0.00241193324347884,0.00243219312565006,0.00283904062398959,0.00315006133491644,
0.00324847701805861,0.00361789986521826,0.00391885772790331,0.00407541417390897,
0.00422088317608797,0.00461166893048689,0.00482386648695767),
 .UNSPECIFIED.);
#5237=B_SPLINE_CURVE_WITH_KNOTS('',3,(#254159,#254160,#254161,#254162),
 .UNSPECIFIED.,.F.,.F.,(4,4),(4.9065389333868E-18,0.000614424279130669),
 .UNSPECIFIED.);
#5238=B_SPLINE_CURVE_WITH_KNOTS('',3,(#254165,#254166,#254167,#254168,#254169,
#254170,#254171,#254172,#254173,#254174),.UNSPECIFIED.,.F.,.F.,(4,3,3,4),
(0.,0.00254000000002352,0.0127000000030823,0.0229583837181861),
 .UNSPECIFIED.);
#5239=B_SPLINE_CURVE_WITH_KNOTS('',3,(#254184,#254185,#254186,#254187,#254188,
#254189),.UNSPECIFIED.,.F.,.F.,(4,2,4),(-0.951075535059639,-0.475537767529819,
0.),.UNSPECIFIED.);
#5240=B_SPLINE_CURVE_WITH_KNOTS('',3,(#254197,#254198,#254199,#254200,#254201,
#254202,#254203,#254204,#254205,#254206,#254207,#254208,#254209,#254210,
#254211,#254212,#254213,#254214,#254215,#254216,#254217,#254218,#254219,
#254220,#254221,#254222,#254223,#254224,#254225,#254226,#254227,#254228,
#254229,#254230,#254231,#254232,#254233,#254234,#254235,#254236,#254237,
#254238,#254239,#254240,#254241,#254242,#254243,#254244,#254245,#254246,
#254247,#254248),.UNSPECIFIED.,.F.,.F.,(4,3,3,3,3,3,3,3,3,3,3,3,3,3,3,3,
3,4),(-3.16252941868488E-5,0.00137437432052449,0.00276766024128256,0.00349864849718784,
0.00351135631713655,0.00538023332270873,0.00702892228856252,0.00704872624461305,
0.00857771963899053,0.00879405918424988,0.00881347799615429,0.0105591960799372,
0.0105751229197932,0.0120513358719185,0.0123243329756246,0.0123340950401616,
0.0133922117480619,0.014089469871312),.UNSPECIFIED.);
#5241=B_SPLINE_CURVE_WITH_KNOTS('',3,(#254261,#254262,#254263,#254264,#254265,
#254266,#254267,#254268,#254269,#254270,#254271,#254272,#254273,#254274,
#254275,#254276,#254277,#254278,#254279,#254280,#254281,#254282,#254283,
#254284,#254285,#254286,#254287,#254288,#254289,#254290,#254291,#254292,
#254293,#254294,#254295,#254296,#254297,#254298,#254299,#254300,#254301,
#254302,#254303,#254304,#254305,#254306,#254307,#254308,#254309,#254310,
#254311,#254312,#254313,#254314,#254315,#254316,#254317,#254318),
 .UNSPECIFIED.,.F.,.F.,(4,3,3,3,3,3,3,3,3,3,3,3,3,3,3,3,3,3,3,4),(0.,0.00104968525641989,
0.001741380883755,0.00175109663942472,0.00321596412665287,0.00348633037654304,
0.00350219327884944,0.00523393136927482,0.00525328991827416,0.00677027115516066,
0.00698461442054001,0.00700438655769888,0.00885850868698763,0.0104937842336623,
0.0105065798365484,0.0115780826059013,0.0122576764759731,0.0131332247956855,
0.0135709989555417,0.0140087731153979),.UNSPECIFIED.);
#5242=B_SPLINE_CURVE_WITH_KNOTS('',3,(#254326,#254327,#254328,#254329,#254330,
#254331,#254332,#254333,#254334,#254335,#254336,#254337,#254338,#254339,
#254340,#254341,#254342,#254343,#254344,#254345,#254346,#254347,#254348,
#254349,#254350,#254351,#254352,#254353,#254354,#254355,#254356,#254357,
#254358,#254359,#254360,#254361,#254362,#254363,#254364,#254365,#254366,
#254367,#254368,#254369,#254370,#254371,#254372,#254373,#254374,#254375,
#254376,#254377),.UNSPECIFIED.,.F.,.F.,(4,3,3,3,3,3,3,3,3,3,3,3,3,3,3,3,
3,4),(-3.16252941869288E-5,0.00137437432795194,0.00276766023004491,0.00349864849718778,
0.0035113563171365,0.00538023332080317,0.00702892228856249,0.00704872624461302,
0.00857771966000481,0.00879405918424986,0.00881347799615426,0.0105591960799372,
0.0105751229197931,0.0120513358492157,0.0123243329756246,0.0123340950401616,
0.0133922117446449,0.014089469871312),.UNSPECIFIED.);
#5243=B_SPLINE_CURVE_WITH_KNOTS('',3,(#254406,#254407,#254408,#254409,#254410,
#254411,#254412,#254413,#254414,#254415,#254416,#254417,#254418,#254419,
#254420,#254421,#254422,#254423,#254424,#254425,#254426,#254427,#254428,
#254429,#254430,#254431,#254432,#254433,#254434,#254435,#254436,#254437,
#254438,#254439,#254440,#254441,#254442,#254443,#254444,#254445,#254446,
#254447,#254448,#254449,#254450,#254451,#254452,#254453,#254454,#254455,
#254456,#254457,#254458,#254459,#254460,#254461,#254462,#254463),
 .UNSPECIFIED.,.F.,.F.,(4,3,3,3,3,3,3,3,3,3,3,3,3,3,3,3,3,3,3,4),(0.,0.00104968525301761,
0.001741380883755,0.00175109663942474,0.00321596410406456,0.0034863303765431,
0.00350219327884948,0.00523393136927486,0.00525328991827421,0.00677027117601199,
0.00698461442054009,0.00700438655769895,0.0088585086860334,0.0104937842336624,
0.0105065798365484,0.0115780826096491,0.0122576764759731,0.0131332247956855,
0.0135709989555417,0.0140087731153978),.UNSPECIFIED.);
#5244=B_SPLINE_CURVE_WITH_KNOTS('',3,(#254466,#254467,#254468,#254469,#254470,
#254471,#254472,#254473,#254474,#254475,#254476,#254477,#254478,#254479,
#254480,#254481,#254482,#254483,#254484,#254485,#254486,#254487,#254488,
#254489,#254490,#254491,#254492,#254493,#254494,#254495,#254496,#254497,
#254498,#254499,#254500,#254501,#254502,#254503,#254504,#254505,#254506,
#254507,#254508,#254509,#254510,#254511,#254512,#254513,#254514,#254515,
#254516,#254517),.UNSPECIFIED.,.F.,.F.,(4,3,3,3,3,3,3,3,3,3,3,3,3,3,3,3,
3,4),(-3.16252941868488E-5,0.00137437432439234,0.0027676602298183,0.00349864849718784,
0.00351135631713652,0.00538023331410978,0.00702892228856252,0.00704872624461304,
0.00857771966078142,0.00879405918424988,0.00881347799615428,0.0105591960799372,
0.0105751229197931,0.012051335889654,0.0123243329756246,0.0123340950401616,
0.0133922117516399,0.014089469871312),.UNSPECIFIED.);
#5245=B_SPLINE_CURVE_WITH_KNOTS('',3,(#254526,#254527,#254528,#254529,#254530,
#254531,#254532,#254533,#254534,#254535,#254536,#254537,#254538,#254539,
#254540,#254541,#254542,#254543,#254544,#254545,#254546,#254547,#254548,
#254549,#254550,#254551,#254552,#254553,#254554,#254555,#254556,#254557,
#254558,#254559,#254560,#254561,#254562,#254563,#254564,#254565,#254566,
#254567,#254568,#254569,#254570,#254571,#254572,#254573,#254574,#254575,
#254576,#254577,#254578,#254579,#254580,#254581,#254582,#254583),
 .UNSPECIFIED.,.F.,.F.,(4,3,3,3,3,3,3,3,3,3,3,3,3,3,3,3,3,3,3,4),(0.,0.00104968525999275,
0.00174138088375498,0.00175109663942472,0.00321596414413303,0.00348633037654304,
0.00350219327884944,0.00523393136927485,0.00525328991827416,0.00677027117696927,
0.00698461442053999,0.00700438655769888,0.00885850867811475,0.0104937842336624,
0.0105065798365484,0.0115780826069947,0.0122576764759731,0.0131332247956855,
0.0135709989555417,0.0140087731153979),.UNSPECIFIED.);
#5246=B_SPLINE_CURVE_WITH_KNOTS('',3,(#254589,#254590,#254591,#254592,#254593,
#254594),.UNSPECIFIED.,.F.,.F.,(4,2,4),(-2.85874066322165,-2.38320289569183,
-1.907665128162),.UNSPECIFIED.);
#5247=B_SPLINE_CURVE_WITH_KNOTS('',3,(#254599,#254600,#254601,#254602,#254603,
#254604,#254605,#254606,#254607,#254608,#254609,#254610,#254611,#254612,
#254613,#254614,#254615,#254616,#254617,#254618,#254619,#254620,#254621,
#254622,#254623,#254624,#254625,#254626,#254627,#254628,#254629,#254630,
#254631,#254632,#254633,#254634,#254635,#254636,#254637,#254638,#254639,
#254640,#254641,#254642,#254643,#254644,#254645,#254646,#254647,#254648,
#254649,#254650,#254651,#254652,#254653,#254654,#254655,#254656),
 .UNSPECIFIED.,.F.,.F.,(4,3,3,3,3,3,3,3,3,3,3,3,3,3,3,3,3,3,3,4),(0.,0.00131752569946196,
0.00263505139892392,0.00439593787358465,0.00526189587671845,0.00527010279784784,
0.0105240963355105,0.0105402055956957,0.0170741315263014,0.0210484972404,
0.0210804111913913,0.0263355116903984,0.0315906121894055,0.031620616787087,
0.0336558605474688,0.0356821662679883,0.0368793854111903,0.0388917800756179,
0.0408753537649422,0.0421608223827827),.UNSPECIFIED.);
#5248=B_SPLINE_CURVE_WITH_KNOTS('',3,(#254710,#254711,#254712,#254713,#254714,
#254715,#254716,#254717,#254718,#254719,#254720,#254721,#254722,#254723,
#254724,#254725,#254726,#254727,#254728,#254729,#254730,#254731,#254732,
#254733,#254734,#254735,#254736,#254737,#254738,#254739,#254740,#254741,
#254742,#254743,#254744,#254745,#254746,#254747,#254748,#254749,#254750,
#254751,#254752,#254753,#254754,#254755),.UNSPECIFIED.,.F.,.F.,(4,3,3,3,
3,3,3,3,3,3,3,3,3,3,3,4),(0.,0.000232179668578841,0.000466221379334127,
0.00069011536363699,0.0010353712589054,0.00138023072727398,0.00207034609091097,
0.00276046145454796,0.00345057681818495,0.00414069218182194,0.00444163650088071,
0.00474476786788454,0.00483080754545894,0.00514271123354814,0.00545551728654251,
0.00552092290909593),.UNSPECIFIED.);
#5249=B_SPLINE_CURVE_WITH_KNOTS('',3,(#254762,#254763,#254764,#254765,#254766,
#254767,#254768,#254769,#254770,#254771,#254772,#254773,#254774,#254775,
#254776,#254777,#254778,#254779,#254780,#254781,#254782,#254783,#254784,
#254785,#254786,#254787,#254788,#254789,#254790,#254791,#254792,#254793,
#254794,#254795,#254796,#254797,#254798,#254799,#254800,#254801,#254802,
#254803,#254804,#254805,#254806,#254807),.UNSPECIFIED.,.F.,.F.,(4,3,3,3,
3,3,3,3,3,3,3,3,3,3,3,4),(0.,0.000235240533226937,0.000472127618779121,
0.00068965544306545,0.00103448316459817,0.0013793108861309,0.00206896632919635,
0.0027586217722618,0.00344827721532725,0.0041379326583927,0.00442075645279172,
0.0047045278060221,0.00482758810145815,0.00512139192932336,0.00541413800930076,
0.0055172435445236),.UNSPECIFIED.);
#5250=B_SPLINE_CURVE_WITH_KNOTS('',3,(#254811,#254812,#254813,#254814),
 .UNSPECIFIED.,.F.,.F.,(4,4),(0.,0.0224906085590336),.UNSPECIFIED.);
#5251=B_SPLINE_CURVE_WITH_KNOTS('',3,(#254820,#254821,#254822,#254823,#254824,
#254825,#254826,#254827,#254828,#254829),.UNSPECIFIED.,.F.,.F.,(4,2,2,2,
4),(-0.0398721478365828,-0.0302776007344581,-0.019948876411194,-0.0096621711043431,
-4.21224481406135E-8),.UNSPECIFIED.);
#5252=B_SPLINE_CURVE_WITH_KNOTS('',3,(#254831,#254832,#254833,#254834,#254835,
#254836,#254837),.UNSPECIFIED.,.F.,.F.,(4,3,4),(-0.000246059622236046,0.,
1.60099170077638E-5),.UNSPECIFIED.);
#5253=B_SPLINE_CURVE_WITH_KNOTS('',3,(#254839,#254840,#254841,#254842,#254843,
#254844),.UNSPECIFIED.,.F.,.F.,(4,2,4),(-0.0148199167117932,-0.00741824557827452,
-2.07859943751379E-6),.UNSPECIFIED.);
#5254=B_SPLINE_CURVE_WITH_KNOTS('',3,(#254855,#254856,#254857,#254858),
 .UNSPECIFIED.,.F.,.F.,(4,4),(0.00255945989202331,0.0250500684510569),
 .UNSPECIFIED.);
#5255=B_SPLINE_CURVE_WITH_KNOTS('',3,(#254864,#254865,#254866,#254867,#254868,
#254869),.UNSPECIFIED.,.F.,.F.,(4,2,4),(2.07859913676084E-6,0.00741824557851883,
0.014819916713439),.UNSPECIFIED.);
#5256=B_SPLINE_CURVE_WITH_KNOTS('',3,(#254871,#254872,#254873,#254874,#254875,
#254876,#254877),.UNSPECIFIED.,.F.,.F.,(4,3,4),(0.000666505089407319,0.000682515006394785,
0.000928574628629964),.UNSPECIFIED.);
#5257=B_SPLINE_CURVE_WITH_KNOTS('',3,(#254878,#254879,#254880,#254881,#254882,
#254883,#254884,#254885,#254886,#254887),.UNSPECIFIED.,.F.,.F.,(4,2,2,2,
4),(1.04282415750237E-8,0.00965213814703536,0.0199382545415243,0.030267394120979,
0.0398723888738878),.UNSPECIFIED.);
#5258=B_SPLINE_CURVE_WITH_KNOTS('',3,(#254890,#254891,#254892,#254893,#254894,
#254895,#254896,#254897,#254898,#254899,#254900,#254901,#254902,#254903,
#254904,#254905,#254906,#254907,#254908,#254909,#254910,#254911,#254912,
#254913,#254914,#254915,#254916,#254917),.UNSPECIFIED.,.F.,.F.,(4,3,3,3,
3,3,3,3,3,4),(1.77758317468082E-12,0.00346922799309708,0.00495442825517768,
0.00743164238276653,0.00888406179046178,0.00990885651035537,0.0124762492994206,
0.0150579051677044,0.0176593450599696,0.0198177130127836),.UNSPECIFIED.);
#5259=B_SPLINE_CURVE_WITH_KNOTS('',3,(#254926,#254927,#254928,#254929,#254930,
#254931,#254932,#254933,#254934,#254935,#254936,#254937,#254938,#254939,
#254940,#254941,#254942,#254943,#254944,#254945,#254946,#254947,#254948,
#254949,#254950,#254951,#254952,#254953,#254954,#254955,#254956,#254957,
#254958,#254959,#254960,#254961,#254962),.UNSPECIFIED.,.F.,.F.,(4,3,3,3,
3,3,3,3,3,3,3,3,4),(0.,0.00168691413199172,0.00335228412618897,0.00495034605026231,
0.00800843391090747,0.00989931177900222,0.00990069210052463,0.0123758651256558,
0.0124257497720468,0.0148510381507869,0.0149523121298537,0.0179692979973849,
0.0198013842010493),.UNSPECIFIED.);
#5260=B_SPLINE_CURVE_WITH_KNOTS('',3,(#254964,#254965,#254966,#254967,#254968,
#254969),.UNSPECIFIED.,.F.,.F.,(4,2,4),(5.82408502082562E-10,0.0170530403484513,
0.0341060806969008),.UNSPECIFIED.);
#5261=B_SPLINE_CURVE_WITH_KNOTS('',3,(#254971,#254972,#254973,#254974,#254975,
#254976,#254977,#254978,#254979,#254980,#254981,#254982,#254983,#254984,
#254985,#254986),.UNSPECIFIED.,.F.,.F.,(4,2,2,2,2,2,2,4),(0.000399405979664551,
0.00293135834355028,0.00546331070743601,0.0105272154352075,0.0206550248907504,
0.0307828343462933,0.0358467390740648,0.0409106438018362),.UNSPECIFIED.);
#5262=B_SPLINE_CURVE_WITH_KNOTS('',3,(#254987,#254988,#254989,#254990,#254991,
#254992),.UNSPECIFIED.,.F.,.F.,(4,2,4),(1.4304896245382E-17,0.0170530431506666,
0.0341060857189264),.UNSPECIFIED.);
#5263=B_SPLINE_CURVE_WITH_KNOTS('',3,(#255006,#255007,#255008,#255009,#255010,
#255011,#255012,#255013,#255014,#255015,#255016,#255017,#255018,#255019,
#255020,#255021),.UNSPECIFIED.,.F.,.F.,(4,3,3,3,3,4),(0.,0.0174001654419337,
0.0175045710703209,0.0261885013107201,0.0339450683097833,0.0348003308838674),
 .UNSPECIFIED.);
#5264=B_SPLINE_CURVE_WITH_KNOTS('',3,(#255031,#255032,#255033,#255034,#255035,
#255036,#255037,#255038,#255039,#255040,#255041,#255042,#255043),
 .UNSPECIFIED.,.F.,.F.,(4,3,3,3,4),(1.73472347597681E-18,0.00776408085901727,
0.0172957528190991,0.0174001584052762,0.0348003168105524),.UNSPECIFIED.);
#5265=B_SPLINE_CURVE_WITH_KNOTS('',3,(#255101,#255102,#255103,#255104,#255105,
#255106,#255107,#255108,#255109,#255110,#255111,#255112,#255113,#255114,
#255115,#255116,#255117,#255118,#255119,#255120,#255121,#255122,#255123,
#255124,#255125,#255126,#255127,#255128,#255129,#255130,#255131,#255132,
#255133,#255134,#255135,#255136,#255137,#255138,#255139,#255140,#255141,
#255142,#255143,#255144,#255145,#255146,#255147,#255148,#255149,#255150,
#255151,#255152),.UNSPECIFIED.,.F.,.F.,(4,3,3,3,3,3,3,3,3,3,3,3,3,3,3,3,
3,4),(-1.27903842355164E-5,0.,1.7463453400642E-5,3.50634018027296E-5,5.46656284338268E-5,
6.42421178660838E-5,6.64687762176374E-5,7.98821467223567E-5,9.02009949650424E-5,
9.32955172270761E-5,0.000100882589541566,0.000107962219828767,0.000114708247948279,
0.00011645022918071,0.000125670415610406,0.00013794360194898,0.000148213929951037,
0.000149858708640316),.UNSPECIFIED.);
#5266=B_SPLINE_CURVE_WITH_KNOTS('',3,(#255154,#255155,#255156,#255157,#255158,
#255159,#255160),.UNSPECIFIED.,.F.,.F.,(4,3,4),(0.000236530395619719,0.00031959462537318,
0.000330551443059626),.UNSPECIFIED.);
#5267=B_SPLINE_CURVE_WITH_KNOTS('',3,(#255166,#255167,#255168,#255169,#255170,
#255171,#255172),.UNSPECIFIED.,.F.,.F.,(4,3,4),(-1.00797019180758E-5,7.30168454413691E-5,
8.39413455213995E-5),.UNSPECIFIED.);
#5268=B_SPLINE_CURVE_WITH_KNOTS('',3,(#255174,#255175,#255176,#255177,#255178,
#255179,#255180,#255181,#255182,#255183,#255184,#255185,#255186,#255187,
#255188,#255189,#255190,#255191,#255192,#255193,#255194,#255195,#255196,
#255197,#255198,#255199,#255200,#255201,#255202,#255203,#255204,#255205,
#255206,#255207,#255208,#255209,#255210,#255211,#255212,#255213,#255214,
#255215,#255216,#255217,#255218,#255219,#255220,#255221,#255222),
 .UNSPECIFIED.,.F.,.F.,(4,3,3,3,3,3,3,3,3,3,3,3,3,3,3,3,4),(7.70239753203427E-14,
1.55924936070291E-5,2.35799864220384E-5,3.11849871370342E-5,3.5511652671198E-5,
4.31537913197463E-5,5.12752739862805E-5,5.54871328695572E-5,6.55863816260145E-5,
7.74044245036072E-5,7.80454628060054E-5,8.48409347506814E-5,0.000103972508418179,
0.000121518636800461,0.000138783636112226,0.00014916663373815,0.000161957017967162),
 .UNSPECIFIED.);
#5269=B_SPLINE_CURVE_WITH_KNOTS('',3,(#255226,#255227,#255228,#255229,#255230,
#255231,#255232,#255233,#255234,#255235,#255236,#255237,#255238,#255239,
#255240,#255241,#255242,#255243,#255244,#255245,#255246,#255247,#255248,
#255249,#255250,#255251,#255252,#255253,#255254,#255255,#255256,#255257,
#255258,#255259,#255260,#255261,#255262,#255263,#255264,#255265,#255266,
#255267,#255268,#255269,#255270,#255271,#255272,#255273,#255274,#255275,
#255276,#255277),.UNSPECIFIED.,.F.,.F.,(4,3,3,3,3,3,3,3,3,3,3,3,3,3,3,3,
3,4),(-1.27903842356209E-5,0.,1.74634534073477E-5,3.50634018159729E-5,5.46656284561953E-5,
6.42421178650527E-5,6.64687762176552E-5,7.98821467213225E-5,9.02009949648931E-5,
9.32955172249898E-5,0.000100882589539224,0.000107962219826057,0.000114708247945179,
0.000116450229181048,0.000125670415610166,0.000137943601951022,0.000148213929942978,
0.000149858708640884),.UNSPECIFIED.);
#5270=B_SPLINE_CURVE_WITH_KNOTS('',3,(#255279,#255280,#255281,#255282,#255283,
#255284,#255285),.UNSPECIFIED.,.F.,.F.,(4,3,4),(0.000236530395620193,0.000319594623033558,
0.000330551443059687),.UNSPECIFIED.);
#5271=B_SPLINE_CURVE_WITH_KNOTS('',3,(#255303,#255304,#255305,#255306,#255307,
#255308,#255309),.UNSPECIFIED.,.F.,.F.,(4,3,4),(-1.00797019179348E-5,7.30168513305268E-5,
8.39413455215476E-5),.UNSPECIFIED.);
#5272=B_SPLINE_CURVE_WITH_KNOTS('',3,(#255310,#255311,#255312,#255313,#255314,
#255315,#255316,#255317,#255318,#255319,#255320,#255321,#255322,#255323,
#255324,#255325,#255326,#255327,#255328,#255329,#255330,#255331,#255332,
#255333,#255334,#255335,#255336,#255337,#255338,#255339,#255340,#255341,
#255342,#255343,#255344,#255345,#255346,#255347,#255348,#255349,#255350,
#255351,#255352,#255353,#255354,#255355,#255356,#255357,#255358),
 .UNSPECIFIED.,.F.,.F.,(4,3,3,3,3,3,3,3,3,3,3,3,3,3,3,3,4),(7.6239948049063E-14,
1.55924936059415E-5,2.35799886190525E-5,3.1184987135643E-5,3.5511663807096E-5,
4.31538029420733E-5,5.12752864215393E-5,5.54871407305369E-5,6.5586390413675E-5,
7.7404434382236E-5,7.80454628009842E-5,8.4840940844391E-5,0.00010397251409257,
0.000121518642655327,0.000138783642360409,0.000149166633737892,0.000161957017966969),
 .UNSPECIFIED.);
#5273=B_SPLINE_CURVE_WITH_KNOTS('',3,(#255365,#255366,#255367,#255368,#255369,
#255370,#255371,#255372,#255373,#255374,#255375,#255376,#255377,#255378,
#255379,#255380,#255381,#255382,#255383,#255384,#255385,#255386,#255387,
#255388,#255389,#255390,#255391,#255392,#255393,#255394,#255395,#255396,
#255397,#255398,#255399,#255400,#255401,#255402,#255403,#255404,#255405,
#255406,#255407,#255408,#255409,#255410,#255411,#255412,#255413,#255414,
#255415,#255416),.UNSPECIFIED.,.F.,.F.,(4,3,3,3,3,3,3,3,3,3,3,3,3,3,3,3,
3,4),(-1.27903842354479E-5,0.,1.74634534010109E-5,3.50634018038132E-5,5.46656284408684E-5,
6.42421178641914E-5,6.64687762172822E-5,7.98821467208371E-5,9.02009949633172E-5,
9.32955172243919E-5,0.000100882589539266,0.000107962219826603,0.000114708247946188,
0.000116450229181059,0.000125670415611108,0.000137943601956876,0.000148213929940526,
0.000149858708640885),.UNSPECIFIED.);
#5274=B_SPLINE_CURVE_WITH_KNOTS('',3,(#255418,#255419,#255420,#255421,#255422,
#255423,#255424),.UNSPECIFIED.,.F.,.F.,(4,3,4),(0.000236530395620128,0.000319594622622922,
0.000330551443059518),.UNSPECIFIED.);
#5275=B_SPLINE_CURVE_WITH_KNOTS('',3,(#255448,#255449,#255450,#255451,#255452,
#255453,#255454),.UNSPECIFIED.,.F.,.F.,(4,3,4),(-1.00797019178162E-5,7.30168515357015E-5,
8.3941345521282E-5),.UNSPECIFIED.);
#5276=B_SPLINE_CURVE_WITH_KNOTS('',3,(#255456,#255457,#255458,#255459,#255460,
#255461,#255462,#255463,#255464,#255465,#255466,#255467,#255468,#255469,
#255470,#255471,#255472,#255473,#255474,#255475,#255476,#255477,#255478,
#255479,#255480,#255481,#255482,#255483,#255484,#255485,#255486,#255487,
#255488,#255489,#255490,#255491,#255492,#255493,#255494,#255495,#255496,
#255497,#255498,#255499,#255500,#255501,#255502,#255503,#255504),
 .UNSPECIFIED.,.F.,.F.,(4,3,3,3,3,3,3,3,3,3,3,3,3,3,3,3,4),(6.92532125292866E-14,
1.55924936024845E-5,2.35799888310557E-5,3.11849871357157E-5,3.55116648883676E-5,
4.31538040729246E-5,5.12752876341333E-5,5.54871414935716E-5,6.55863912699049E-5,
7.74044353491455E-5,7.80454628014266E-5,8.48409414355659E-5,0.000103972514645705,
0.00012151864322897,0.000138783642975998,0.000149166633737459,0.000161957017966677),
 .UNSPECIFIED.);
#5277=B_SPLINE_CURVE_WITH_KNOTS('',3,(#255512,#255513,#255514,#255515,#255516,
#255517,#255518,#255519,#255520,#255521,#255522,#255523,#255524,#255525,
#255526,#255527,#255528,#255529,#255530,#255531,#255532,#255533,#255534,
#255535,#255536,#255537,#255538,#255539,#255540,#255541,#255542,#255543,
#255544,#255545,#255546,#255547,#255548,#255549,#255550,#255551,#255552,
#255553,#255554,#255555,#255556,#255557,#255558,#255559,#255560,#255561,
#255562,#255563),.UNSPECIFIED.,.F.,.F.,(4,3,3,3,3,3,3,3,3,3,3,3,3,3,3,3,
3,4),(-1.27903842354613E-5,0.,1.746345340453E-5,3.50634018098178E-5,5.46656284383532E-5,
6.42421178639721E-5,6.64687762142466E-5,7.98821467187808E-5,9.02009949657256E-5,
9.32955172233151E-5,0.000100882589538758,0.000107962219826646,0.000114708247946761,
0.00011645022918108,0.00012567041561163,0.000137943601961324,0.000148213929933755,
0.000149858708641606),.UNSPECIFIED.);
#5278=B_SPLINE_CURVE_WITH_KNOTS('',3,(#255565,#255566,#255567,#255568,#255569,
#255570,#255571),.UNSPECIFIED.,.F.,.F.,(4,3,4),(0.000236530395619718,0.000319594617376154,
0.000330551443059305),.UNSPECIFIED.);
#5279=B_SPLINE_CURVE_WITH_KNOTS('',3,(#255596,#255597,#255598,#255599),
 .UNSPECIFIED.,.F.,.F.,(4,4),(1.04083408558608E-17,0.000776824705292365),
 .UNSPECIFIED.);
#5280=B_SPLINE_CURVE_WITH_KNOTS('',3,(#255602,#255603,#255604,#255605),
 .UNSPECIFIED.,.F.,.F.,(4,4),(0.,0.000776824705292377),.UNSPECIFIED.);
#5281=B_SPLINE_CURVE_WITH_KNOTS('',3,(#255607,#255608,#255609,#255610),
 .UNSPECIFIED.,.F.,.F.,(4,4),(3.46944695195361E-18,0.000776824705292372),
 .UNSPECIFIED.);
#5282=B_SPLINE_CURVE_WITH_KNOTS('',3,(#255611,#255612,#255613,#255614),
 .UNSPECIFIED.,.F.,.F.,(4,4),(0.,0.000776824705292378),.UNSPECIFIED.);
#5283=B_SPLINE_CURVE_WITH_KNOTS('',3,(#255616,#255617,#255618,#255619),
 .UNSPECIFIED.,.F.,.F.,(4,4),(3.46944695195361E-18,0.000776824705292372),
 .UNSPECIFIED.);
#5284=B_SPLINE_CURVE_WITH_KNOTS('',3,(#255620,#255621,#255622,#255623),
 .UNSPECIFIED.,.F.,.F.,(4,4),(0.,0.00077682470529238),.UNSPECIFIED.);
#5285=B_SPLINE_CURVE_WITH_KNOTS('',3,(#255627,#255628,#255629,#255630,#255631,
#255632,#255633,#255634,#255635,#255636,#255637,#255638,#255639,#255640,
#255641,#255642,#255643,#255644,#255645,#255646,#255647,#255648,#255649,
#255650,#255651,#255652,#255653,#255654,#255655,#255656,#255657,#255658,
#255659,#255660,#255661,#255662,#255663,#255664,#255665,#255666,#255667,
#255668,#255669,#255670,#255671,#255672,#255673,#255674,#255675,#255676,
#255677,#255678,#255679,#255680,#255681,#255682,#255683,#255684,#255685,
#255686,#255687,#255688,#255689,#255690,#255691,#255692,#255693),
 .UNSPECIFIED.,.F.,.F.,(4,3,3,3,3,3,3,3,3,3,3,3,3,3,3,3,3,3,3,3,3,3,4),
(4.9065389333868E-18,0.000187317538506277,0.000370529360731883,0.000549649653517671,
0.000585186929066945,0.000747835352058225,0.00090905754882324,0.00106903584072748,
0.00117037385813389,0.00139504516879083,0.00161858460257625,0.00175556078720083,
0.00198345805102534,0.0020481542517343,0.00213117924281626,0.00219445098400102,
0.00221273807553437,0.00222891957305618,0.00223102516706771,0.00226084972327193,
0.0022675993501344,0.00232401155250101,0.00234074771626781),
 .UNSPECIFIED.);
#5286=B_SPLINE_CURVE_WITH_KNOTS('',3,(#255708,#255709,#255710,#255711,#255712,
#255713,#255714),.UNSPECIFIED.,.F.,.F.,(4,3,4),(-1.6148217724202E-5,0.000301256797926397,
0.000615737100014097),.UNSPECIFIED.);
#5287=B_SPLINE_CURVE_WITH_KNOTS('',3,(#255715,#255716,#255717,#255718),
 .UNSPECIFIED.,.F.,.F.,(4,4),(0.,0.000264303642305848),.UNSPECIFIED.);
#5288=B_SPLINE_CURVE_WITH_KNOTS('',3,(#255721,#255722,#255723,#255724,#255725,
#255726,#255727,#255728,#255729,#255730,#255731,#255732,#255733,#255734,
#255735,#255736,#255737,#255738,#255739,#255740,#255741,#255742,#255743,
#255744,#255745,#255746,#255747,#255748,#255749,#255750,#255751,#255752,
#255753,#255754,#255755,#255756,#255757,#255758,#255759,#255760,#255761,
#255762,#255763,#255764,#255765,#255766,#255767,#255768,#255769,#255770,
#255771,#255772,#255773,#255774,#255775,#255776,#255777,#255778,#255779,
#255780,#255781,#255782,#255783,#255784,#255785,#255786,#255787),
 .UNSPECIFIED.,.F.,.F.,(4,3,3,3,3,3,3,3,3,3,3,3,3,3,3,3,3,3,3,3,3,3,4),
(1.98780968783202E-9,5.73414915694073E-5,7.42300839654611E-5,0.000104673148245408,
0.000111344132043346,0.000127856077372199,0.00012990115608229,0.000148458180121234,
0.00023314346664102,0.000296914372432783,0.000529593879008388,0.000593826757055878,
0.000836090912058093,0.00108017083919709,0.00118765152630205,0.00135313333384191,
0.00151932196905603,0.00168746877222913,0.00178147629554822,0.00194158715598329,
0.00210403684094403,0.00227214417361886,0.00237530106479439),
 .UNSPECIFIED.);
#5289=B_SPLINE_CURVE_WITH_KNOTS('',3,(#255803,#255804,#255805,#255806),
 .UNSPECIFIED.,.F.,.F.,(4,4),(7.2194514417634E-17,0.000264303642294797),
 .UNSPECIFIED.);
#5290=B_SPLINE_CURVE_WITH_KNOTS('',3,(#255807,#255808,#255809,#255810,#255811,
#255812,#255813),.UNSPECIFIED.,.F.,.F.,(4,3,4),(3.46944695195361E-18,0.000317405080301234,
0.000631885317751415),.UNSPECIFIED.);
#5291=B_SPLINE_CURVE_WITH_KNOTS('',3,(#255817,#255818,#255819,#255820,#255821,
#255822,#255823,#255824,#255825,#255826,#255827,#255828,#255829,#255830,
#255831,#255832,#255833,#255834,#255835,#255836,#255837,#255838,#255839,
#255840,#255841,#255842,#255843,#255844,#255845,#255846,#255847,#255848,
#255849,#255850,#255851,#255852,#255853,#255854,#255855,#255856,#255857,
#255858,#255859,#255860,#255861,#255862,#255863,#255864,#255865,#255866,
#255867,#255868,#255869,#255870,#255871,#255872,#255873,#255874,#255875,
#255876,#255877,#255878,#255879,#255880,#255881,#255882,#255883),
 .UNSPECIFIED.,.F.,.F.,(4,3,3,3,3,3,3,3,3,3,3,3,3,3,3,3,3,3,3,3,3,3,4),
(4.23499971748596E-17,0.000187317538506265,0.000370529360731306,0.000549649653516587,
0.000585186929067176,0.000747835352058548,0.000909057548823778,0.00106903584072817,
0.00117037385813431,0.00139504516879073,0.00161858460257628,0.00175556078720144,
0.00198345805102,0.002048154251735,0.00213117924281676,0.00219445098400178,
0.00221273807553513,0.00222891957305701,0.00223102516706848,0.00226084972327255,
0.00226759935013518,0.00232401155250177,0.00234074771626859),
 .UNSPECIFIED.);
#5292=B_SPLINE_CURVE_WITH_KNOTS('',3,(#255897,#255898,#255899,#255900,#255901,
#255902,#255903),.UNSPECIFIED.,.F.,.F.,(4,3,4),(-1.61482177233483E-5,0.000301256721641648,
0.000615737100014892),.UNSPECIFIED.);
#5293=B_SPLINE_CURVE_WITH_KNOTS('',3,(#255904,#255905,#255906,#255907),
 .UNSPECIFIED.,.F.,.F.,(4,4),(0.,0.000264303642305846),.UNSPECIFIED.);
#5294=B_SPLINE_CURVE_WITH_KNOTS('',3,(#255910,#255911,#255912,#255913,#255914,
#255915,#255916,#255917,#255918,#255919),.UNSPECIFIED.,.F.,.F.,(4,3,3,4),
(-3.83013078967852E-5,0.,0.000144401167384903,0.000501272209488935),
 .UNSPECIFIED.);
#5295=B_SPLINE_CURVE_WITH_KNOTS('',3,(#255921,#255922,#255923,#255924,#255925,
#255926,#255927,#255928,#255929,#255930,#255931,#255932,#255933,#255934,
#255935,#255936,#255937,#255938,#255939,#255940),.UNSPECIFIED.,.F.,.F.,
(4,2,2,2,2,2,2,2,2,4),(4.7385767894594E-6,2.26507325412358E-5,4.05628882930122E-5,
7.63871997965703E-5,0.000148035822803692,0.000291333068817939,0.000577927560846451,
0.00115111654490347,0.00172430552896048,0.0022974945130175),
 .UNSPECIFIED.);
#5296=B_SPLINE_CURVE_WITH_KNOTS('',3,(#255955,#255956,#255957,#255958),
 .UNSPECIFIED.,.F.,.F.,(4,4),(0.,0.00026430364229488),.UNSPECIFIED.);
#5297=B_SPLINE_CURVE_WITH_KNOTS('',3,(#255959,#255960,#255961,#255962,#255963,
#255964,#255965),.UNSPECIFIED.,.F.,.F.,(4,3,4),(3.46944695195361E-18,0.000317404992696139,
0.000631885317751336),.UNSPECIFIED.);
#5298=B_SPLINE_CURVE_WITH_KNOTS('',3,(#255969,#255970,#255971,#255972,#255973,
#255974,#255975,#255976,#255977,#255978,#255979,#255980,#255981,#255982,
#255983,#255984,#255985,#255986,#255987,#255988,#255989,#255990,#255991,
#255992,#255993,#255994,#255995,#255996,#255997,#255998,#255999,#256000,
#256001,#256002,#256003,#256004,#256005,#256006,#256007,#256008,#256009,
#256010,#256011,#256012,#256013,#256014,#256015,#256016,#256017,#256018,
#256019,#256020,#256021,#256022,#256023,#256024,#256025,#256026,#256027,
#256028,#256029,#256030,#256031,#256032,#256033,#256034,#256035),
 .UNSPECIFIED.,.F.,.F.,(4,3,3,3,3,3,3,3,3,3,3,3,3,3,3,3,3,3,3,3,3,3,4),
(0.,0.000187317538506216,0.000370529360731649,0.000549649653517311,0.000585186929066575,
0.000747835352057596,0.000909057548822561,0.00106903584072672,0.00117037385813315,
0.00139504516878895,0.00161858460257515,0.00175556078719972,0.00198345805101906,
0.00204815425173301,0.00213117924281621,0.00219445098399965,0.00221273807553298,
0.00222891957305496,0.00223102516706631,0.00226084972326921,0.00226759935013298,
0.00232401155249693,0.0023407477162663),.UNSPECIFIED.);
#5299=B_SPLINE_CURVE_WITH_KNOTS('',3,(#256049,#256050,#256051,#256052,#256053,
#256054,#256055),.UNSPECIFIED.,.F.,.F.,(4,3,4),(-1.61482177236942E-5,0.000301257027968063,
0.000615737100014811),.UNSPECIFIED.);
#5300=B_SPLINE_CURVE_WITH_KNOTS('',3,(#256056,#256057,#256058,#256059),
 .UNSPECIFIED.,.F.,.F.,(4,4),(0.,0.000264303642305761),.UNSPECIFIED.);
#5301=B_SPLINE_CURVE_WITH_KNOTS('',3,(#256062,#256063,#256064,#256065,#256066,
#256067,#256068,#256069,#256070,#256071,#256072,#256073,#256074,#256075,
#256076,#256077,#256078,#256079,#256080,#256081,#256082,#256083,#256084,
#256085,#256086,#256087,#256088,#256089,#256090,#256091,#256092,#256093,
#256094,#256095,#256096,#256097,#256098,#256099,#256100,#256101,#256102,
#256103,#256104,#256105,#256106,#256107,#256108,#256109,#256110,#256111,
#256112,#256113,#256114,#256115,#256116,#256117,#256118,#256119,#256120,
#256121,#256122,#256123,#256124,#256125,#256126,#256127,#256128),
 .UNSPECIFIED.,.F.,.F.,(4,3,3,3,3,3,3,3,3,3,3,3,3,3,3,3,3,3,3,3,3,3,4),
(1.98061349608262E-9,5.73415218899911E-5,7.4230076566389E-5,0.000104673137737296,
0.000111344124542838,0.000127856070079246,0.000129901148531068,0.000148458172519298,
0.00023314347760765,0.000296914364425009,0.000529593869959597,0.000593826748236463,
0.00083609090671776,0.00108017083758895,0.00118765151585936,0.00135313332319783,
0.00151932195821436,0.00168746876119618,0.00178147628348225,0.00194158714386398,
0.00210403682877481,0.00227214416139509,0.00237530105110514),
 .UNSPECIFIED.);
#5302=B_SPLINE_CURVE_WITH_KNOTS('',3,(#256143,#256144,#256145,#256146),
 .UNSPECIFIED.,.F.,.F.,(4,4),(1.2509268882771E-17,0.000264303642294947),
 .UNSPECIFIED.);
#5303=B_SPLINE_CURVE_WITH_KNOTS('',3,(#256147,#256148,#256149,#256150,#256151,
#256152,#256153),.UNSPECIFIED.,.F.,.F.,(4,3,4),(0.,0.000317405083030208,
0.000631885317751385),.UNSPECIFIED.);
#5304=B_SPLINE_CURVE_WITH_KNOTS('',3,(#256167,#256168,#256169,#256170),
 .UNSPECIFIED.,.F.,.F.,(4,4),(0.,0.00026430364229487),.UNSPECIFIED.);
#5305=B_SPLINE_CURVE_WITH_KNOTS('',3,(#256171,#256172,#256173,#256174,#256175,
#256176,#256177),.UNSPECIFIED.,.F.,.F.,(4,3,4),(3.46944695195361E-18,0.000317405268168359,
0.000631885317751483),.UNSPECIFIED.);
#5306=B_SPLINE_CURVE_WITH_KNOTS('',3,(#256191,#256192,#256193,#256194,#256195,
#256196,#256197),.UNSPECIFIED.,.F.,.F.,(4,3,4),(-1.61482177234426E-5,0.000301256699244678,
0.000615737100014854),.UNSPECIFIED.);
#5307=B_SPLINE_CURVE_WITH_KNOTS('',3,(#256198,#256199,#256200,#256201),
 .UNSPECIFIED.,.F.,.F.,(4,4),(0.,0.000264303642305819),.UNSPECIFIED.);
#5308=B_SPLINE_CURVE_WITH_KNOTS('',3,(#256271,#256272,#256273,#256274,#256275,
#256276,#256277,#256278,#256279,#256280,#256281,#256282,#256283,#256284,
#256285,#256286,#256287,#256288,#256289,#256290,#256291,#256292,#256293,
#256294,#256295,#256296,#256297,#256298,#256299,#256300,#256301,#256302,
#256303,#256304,#256305,#256306,#256307,#256308,#256309,#256310,#256311,
#256312,#256313,#256314,#256315,#256316,#256317,#256318,#256319),
 .UNSPECIFIED.,.F.,.F.,(4,3,3,3,3,3,3,3,3,3,3,3,3,3,3,3,4),(-3.28957225289004E-5,
0.00123839561282373,0.00246284557240642,0.00350220228306729,0.00356136795860099,
0.00529933412363224,0.00703730028866348,0.00712550648875341,0.0081204335483374,
0.00890034485054549,0.00977320546531314,0.0105723982942597,0.0106614349564065,
0.0118079342051501,0.0123965937508694,0.0134149359774125,0.0141074962998559),
 .UNSPECIFIED.);
#5309=B_SPLINE_CURVE_WITH_KNOTS('',3,(#256323,#256324,#256325,#256326,#256327,
#256328,#256329,#256330,#256331,#256332,#256333,#256334,#256335,#256336,
#256337,#256338,#256339,#256340,#256341,#256342,#256343,#256344,#256345,
#256346,#256347,#256348,#256349,#256350,#256351,#256352,#256353,#256354,
#256355,#256356,#256357,#256358,#256359,#256360,#256361,#256362,#256363,
#256364,#256365,#256366,#256367,#256368,#256369,#256370,#256371),
 .UNSPECIFIED.,.F.,.F.,(4,3,3,3,3,3,3,3,3,3,3,3,3,3,3,3,4),(-3.28957225289004E-5,
0.00123839561282583,0.00246284557240834,0.00350220228306729,0.00356136795860099,
0.00529933412363224,0.00703730028866348,0.00712550648875342,0.00812043354833833,
0.00890034485054549,0.00977320546531023,0.0105723982942597,0.0106614349564065,
0.0118079342051527,0.0123965937508694,0.0134149359774119,0.0141074962998559),
 .UNSPECIFIED.);
#5310=B_SPLINE_CURVE_WITH_KNOTS('',3,(#256462,#256463,#256464,#256465,#256466,
#256467,#256468,#256469,#256470,#256471,#256472,#256473,#256474,#256475,
#256476,#256477,#256478,#256479,#256480,#256481,#256482,#256483,#256484,
#256485,#256486,#256487,#256488,#256489,#256490,#256491,#256492,#256493,
#256494,#256495,#256496,#256497,#256498,#256499,#256500,#256501,#256502,
#256503,#256504,#256505,#256506,#256507,#256508,#256509,#256510),
 .UNSPECIFIED.,.F.,.F.,(4,3,3,3,3,3,3,3,3,3,3,3,3,3,3,3,4),(-3.28957225289672E-5,
0.00123839562134457,0.0024628455650959,0.00350220228306722,0.00356136795860092,
0.00529933412363217,0.00703730028866341,0.00712550648875332,0.00812043354890156,
0.00890034485054153,0.00977320546595051,0.0105723982942596,0.0106614349564063,
0.0118079342061304,0.0123965937508664,0.0134149359795621,0.0141074962998558),
 .UNSPECIFIED.);
#5311=B_SPLINE_CURVE_WITH_KNOTS('',3,(#256514,#256515,#256516,#256517,#256518,
#256519,#256520,#256521,#256522,#256523,#256524,#256525,#256526,#256527,
#256528,#256529,#256530,#256531,#256532,#256533,#256534,#256535,#256536,
#256537,#256538,#256539,#256540,#256541,#256542,#256543,#256544,#256545,
#256546,#256547,#256548,#256549,#256550,#256551,#256552,#256553,#256554,
#256555,#256556,#256557,#256558,#256559,#256560,#256561,#256562),
 .UNSPECIFIED.,.F.,.F.,(4,3,3,3,3,3,3,3,3,3,3,3,3,3,3,3,4),(-3.28957225289672E-5,
0.0012383956213515,0.00246284556510125,0.00350220228306722,0.00356136795860093,
0.00529933412363217,0.00703730028866341,0.00712550648875329,0.00812043354890009,
0.0089003448505415,0.00977320546595016,0.0105723982942596,0.0106614349564063,
0.01180793420613,0.0123965937508664,0.0134149359795605,0.0141074962998558),
 .UNSPECIFIED.);
#5312=B_SPLINE_CURVE_WITH_KNOTS('',3,(#256654,#256655,#256656,#256657,#256658,
#256659,#256660,#256661,#256662,#256663,#256664,#256665,#256666,#256667,
#256668,#256669,#256670,#256671,#256672,#256673,#256674,#256675,#256676,
#256677,#256678,#256679,#256680,#256681,#256682,#256683,#256684,#256685,
#256686,#256687,#256688,#256689,#256690,#256691,#256692,#256693,#256694,
#256695,#256696,#256697,#256698,#256699,#256700,#256701,#256702),
 .UNSPECIFIED.,.F.,.F.,(4,3,3,3,3,3,3,3,3,3,3,3,3,3,3,3,4),(-3.28957225289672E-5,
0.00123839562262854,0.00246284556740731,0.00350220228306722,0.0035613679586009,
0.00529933412363216,0.00703730028866341,0.00712550648875328,0.00812043354869755,
0.00890034485054217,0.00977320546566178,0.0105723982942596,0.0106614349564064,
0.0118079342049588,0.0123965937508674,0.0134149359781372,0.0141074962998558),
 .UNSPECIFIED.);
#5313=B_SPLINE_CURVE_WITH_KNOTS('',3,(#256706,#256707,#256708,#256709,#256710,
#256711,#256712,#256713,#256714,#256715,#256716,#256717,#256718,#256719,
#256720,#256721,#256722,#256723,#256724,#256725,#256726,#256727,#256728,
#256729,#256730,#256731,#256732,#256733,#256734,#256735,#256736,#256737,
#256738,#256739,#256740,#256741,#256742,#256743,#256744,#256745,#256746,
#256747,#256748,#256749,#256750,#256751,#256752,#256753,#256754),
 .UNSPECIFIED.,.F.,.F.,(4,3,3,3,3,3,3,3,3,3,3,3,3,3,3,3,4),(-3.28957225289672E-5,
0.00123839562262829,0.00246284556740624,0.00350220228306722,0.00356136795860091,
0.00529933412363216,0.00703730028866341,0.0071255064887533,0.00812043354869597,
0.00890034485054217,0.00977320546566605,0.0105723982942596,0.0106614349564064,
0.0118079342049593,0.0123965937508674,0.0134149359781345,0.0141074962998558),
 .UNSPECIFIED.);
#5314=B_SPLINE_CURVE_WITH_KNOTS('',3,(#256848,#256849,#256850,#256851,#256852,
#256853,#256854,#256855,#256856,#256857,#256858,#256859,#256860,#256861,
#256862,#256863,#256864,#256865,#256866,#256867,#256868,#256869,#256870,
#256871,#256872,#256873,#256874,#256875,#256876,#256877,#256878,#256879,
#256880,#256881,#256882,#256883,#256884,#256885,#256886,#256887,#256888,
#256889,#256890,#256891,#256892,#256893,#256894,#256895,#256896,#256897,
#256898,#256899,#256900,#256901,#256902,#256903,#256904,#256905,#256906,
#256907,#256908,#256909,#256910,#256911,#256912,#256913,#256914,#256915,
#256916,#256917,#256918,#256919,#256920,#256921,#256922,#256923,#256924,
#256925,#256926,#256927,#256928,#256929,#256930,#256931,#256932,#256933,
#256934,#256935,#256936,#256937,#256938,#256939,#256940,#256941,#256942,
#256943,#256944,#256945,#256946,#256947),.UNSPECIFIED.,.F.,.F.,(4,3,3,3,
3,3,3,3,3,3,3,3,3,3,3,3,3,3,3,3,3,3,3,3,3,3,3,3,3,3,3,3,3,4),(1.42043634129218E-9,
8.96508234963807E-5,0.000177139225359939,0.000196453687302178,0.000222064227861235,
0.000285479098213833,0.000349005642415524,0.000361856879033328,0.000392907374604338,
0.000507356384677131,0.000595775533469028,0.000684346942788586,0.000773468971709804,
0.000785814749208658,0.000832772345389435,0.000952902380893138,0.00107741065969588,
0.00117872212381298,0.00121565072790586,0.00131178235002056,0.00141569811404612,
0.00142936137630885,0.00155931596577564,0.0015716294984173,0.00165375706712277,
0.00184401976952065,0.00204137976398503,0.0021285000374069,0.00230460243506521,
0.00235744424762594,0.00259423468405583,0.00263013820146309,0.00296211475305905,
0.00314325899683457),.UNSPECIFIED.);
#5315=B_SPLINE_CURVE_WITH_KNOTS('',3,(#256952,#256953,#256954,#256955,#256956,
#256957,#256958,#256959,#256960,#256961,#256962,#256963,#256964,#256965,
#256966,#256967,#256968,#256969,#256970,#256971,#256972,#256973,#256974,
#256975,#256976,#256977,#256978,#256979,#256980,#256981,#256982,#256983,
#256984,#256985,#256986,#256987,#256988,#256989,#256990,#256991,#256992,
#256993,#256994,#256995,#256996,#256997,#256998,#256999,#257000,#257001,
#257002,#257003,#257004,#257005,#257006,#257007,#257008,#257009,#257010,
#257011,#257012,#257013,#257014,#257015,#257016,#257017,#257018,#257019,
#257020,#257021,#257022,#257023,#257024,#257025,#257026,#257027,#257028,
#257029,#257030,#257031,#257032,#257033,#257034,#257035,#257036,#257037,
#257038,#257039,#257040,#257041,#257042,#257043,#257044,#257045,#257046,
#257047,#257048,#257049,#257050,#257051),.UNSPECIFIED.,.F.,.F.,(4,3,3,3,
3,3,3,3,3,3,3,3,3,3,3,3,3,3,3,3,3,3,3,3,3,3,3,3,3,3,3,3,3,4),(6.93889390390723E-18,
0.000232066433642932,0.000444177580050074,0.000518385099123644,0.000734102786663995,
0.00079015638993006,0.000993487732790287,0.00102299023054961,0.00119225943856918,
0.00134764700037811,0.00150263588856933,0.00158031277986011,0.00171536369190904,
0.00184243086348886,0.00194346242503313,0.00197539097482514,0.00208159421176549,
0.00218487525328951,0.00228393672716245,0.0023319957435332,0.00237046916979017,
0.00246124899505445,0.00255227503608586,0.00264431970448832,0.00265740253517428,
0.0027655473647552,0.00280202928405062,0.00287180839700997,0.00294158750996931,
0.00296308646223771,0.00302593425586122,0.00308943159919426,0.00315434926414339,
0.00316062418320347),.UNSPECIFIED.);
#5316=B_SPLINE_CURVE_WITH_KNOTS('',3,(#257053,#257054,#257055,#257056,#257057,
#257058,#257059,#257060,#257061,#257062,#257063,#257064,#257065,#257066,
#257067,#257068,#257069,#257070,#257071,#257072,#257073,#257074,#257075,
#257076,#257077,#257078,#257079,#257080,#257081,#257082,#257083,#257084,
#257085,#257086,#257087,#257088,#257089,#257090,#257091,#257092,#257093,
#257094,#257095,#257096,#257097,#257098,#257099,#257100,#257101,#257102,
#257103,#257104,#257105,#257106,#257107,#257108,#257109,#257110,#257111,
#257112,#257113,#257114,#257115,#257116,#257117,#257118,#257119,#257120,
#257121,#257122,#257123,#257124,#257125,#257126,#257127,#257128,#257129,
#257130,#257131,#257132,#257133,#257134,#257135,#257136,#257137,#257138,
#257139,#257140,#257141,#257142,#257143,#257144,#257145,#257146,#257147,
#257148,#257149,#257150,#257151,#257152),.UNSPECIFIED.,.F.,.F.,(4,3,3,3,
3,3,3,3,3,3,3,3,3,3,3,3,3,3,3,3,3,3,3,3,3,3,3,3,3,3,3,3,3,4),(1.42043608206403E-9,
8.96508236035631E-5,0.000177139225573717,0.000196453687302176,0.000222064227861251,
0.000285479098216081,0.0003490056424501,0.000361856879033412,0.000392907374604345,
0.000507356384677133,0.00059577553344614,0.000684346942743958,0.000773468971644799,
0.00078581474920867,0.000832772345389567,0.000952902380959916,0.00107741065982593,
0.001178722123813,0.00121565072790588,0.00131178235000143,0.00141569811400841,
0.00142936137630791,0.0015593159657081,0.00157162949841732,0.00165375706712266,
0.00184401976967872,0.00204137976426714,0.00212850003740968,0.00230460243517562,
0.00235744424762599,0.00259423468398172,0.002630138201466,0.00296211475105057,
0.00314325899683465),.UNSPECIFIED.);
#5317=B_SPLINE_CURVE_WITH_KNOTS('',3,(#257154,#257155,#257156,#257157,#257158,
#257159,#257160,#257161,#257162,#257163,#257164,#257165,#257166,#257167,
#257168,#257169,#257170,#257171,#257172,#257173,#257174,#257175,#257176,
#257177,#257178,#257179,#257180,#257181,#257182,#257183,#257184,#257185,
#257186,#257187,#257188,#257189,#257190,#257191,#257192,#257193,#257194,
#257195,#257196,#257197,#257198,#257199,#257200,#257201,#257202,#257203,
#257204,#257205,#257206,#257207,#257208,#257209,#257210,#257211,#257212,
#257213,#257214,#257215,#257216,#257217,#257218,#257219,#257220,#257221,
#257222,#257223,#257224,#257225,#257226,#257227,#257228,#257229,#257230,
#257231,#257232,#257233,#257234,#257235,#257236,#257237,#257238,#257239,
#257240,#257241,#257242,#257243,#257244),.UNSPECIFIED.,.F.,.F.,(4,3,3,3,
3,3,3,3,3,3,3,3,3,3,3,3,3,3,3,3,3,3,3,3,3,3,3,3,3,3,4),(7.76567327304113E-17,
0.00028555321634447,0.000553574635556241,0.000790156389930066,0.000990625082294371,
0.00101175876514238,0.00118107858470282,0.00133650434438385,0.00148689176226834,
0.00158031277986005,0.00171723652027668,0.00184679122665669,0.00192446598409234,
0.00197539097482506,0.00208289236625799,0.00218748593006637,0.0022881074172723,
0.0023115638194695,0.00237046916979006,0.00246035369911973,0.00255120401579351,
0.00263700098462238,0.00276554736475506,0.00278116187942606,0.00285032890543618,
0.0029194959314463,0.00296308646223756,0.00302598539539431,0.0030896083045167,
0.00315476369574107,0.00316062555972006),.UNSPECIFIED.);
#5318=B_SPLINE_CURVE_WITH_KNOTS('',3,(#257246,#257247,#257248,#257249,#257250,
#257251,#257252,#257253,#257254,#257255,#257256,#257257,#257258,#257259,
#257260,#257261,#257262,#257263,#257264,#257265,#257266,#257267,#257268,
#257269,#257270,#257271,#257272,#257273,#257274,#257275,#257276,#257277,
#257278,#257279,#257280,#257281,#257282,#257283,#257284,#257285,#257286,
#257287,#257288,#257289,#257290,#257291,#257292,#257293,#257294,#257295,
#257296,#257297,#257298,#257299,#257300,#257301,#257302,#257303,#257304,
#257305,#257306,#257307,#257308,#257309,#257310,#257311,#257312,#257313,
#257314,#257315,#257316,#257317,#257318,#257319,#257320,#257321,#257322,
#257323,#257324,#257325,#257326,#257327,#257328,#257329,#257330,#257331,
#257332,#257333,#257334,#257335,#257336,#257337,#257338,#257339,#257340,
#257341,#257342,#257343,#257344,#257345),.UNSPECIFIED.,.F.,.F.,(4,3,3,3,
3,3,3,3,3,3,3,3,3,3,3,3,3,3,3,3,3,3,3,3,3,3,3,3,3,3,3,3,3,4),(1.42043589704641E-9,
8.96508235406491E-5,0.000177139225437119,0.000196453687302197,0.000222064227860353,
0.000285479098225494,0.00034900564245659,0.000361856879032499,0.000392907374604361,
0.000507356384676228,0.000595775533459017,0.000684346942768234,0.000773468971677273,
0.000785814749208695,0.000832772345388566,0.000952902380893963,0.00107741065969749,
0.00117872212381303,0.00121565072790504,0.00131178235002272,0.00141569811405072,
0.00142936137630815,0.00155931596573497,0.00157162949841736,0.00165375706712212,
0.00184401976963584,0.00204137976419306,0.0021285000374072,0.00230460243515318,
0.00235744424762603,0.00259423468397992,0.00263013820146432,0.00296211475118288,
0.0031432589968347),.UNSPECIFIED.);
#5319=B_SPLINE_CURVE_WITH_KNOTS('',3,(#257347,#257348,#257349,#257350,#257351,
#257352,#257353,#257354,#257355,#257356,#257357,#257358,#257359,#257360,
#257361,#257362,#257363,#257364,#257365,#257366,#257367,#257368,#257369,
#257370,#257371,#257372,#257373,#257374,#257375,#257376,#257377,#257378,
#257379,#257380,#257381,#257382,#257383,#257384,#257385,#257386,#257387,
#257388,#257389,#257390,#257391,#257392,#257393,#257394,#257395,#257396,
#257397,#257398,#257399,#257400,#257401,#257402,#257403,#257404,#257405,
#257406,#257407,#257408,#257409,#257410,#257411,#257412,#257413,#257414,
#257415,#257416,#257417,#257418,#257419,#257420,#257421,#257422,#257423,
#257424,#257425,#257426,#257427,#257428,#257429,#257430,#257431,#257432,
#257433,#257434,#257435,#257436,#257437,#257438,#257439,#257440,#257441,
#257442,#257443,#257444,#257445,#257446),.UNSPECIFIED.,.F.,.F.,(4,3,3,3,
3,3,3,3,3,3,3,3,3,3,3,3,3,3,3,3,3,3,3,3,3,3,3,3,3,3,3,3,3,4),(3.46944695195361E-18,
0.000232066433521906,0.000444177579881847,0.000518385099121857,0.00073410278654322,
0.000790156389930058,0.00099348773274801,0.00102299023054891,0.00119225943856017,
0.0013476470003594,0.00150263588856866,0.00158031277986011,0.00171536369188439,
0.00184243086343882,0.00194346242503234,0.00197539097482514,0.00208159421173027,
0.0021848752532145,0.00228393672704159,0.0023319957435323,0.00237046916979017,
0.00246124899502891,0.00255227503603492,0.00264431970440927,0.00265740253517351,
0.0027655473647552,0.00280202928404987,0.00287180839700916,0.00294158750996845,
0.00296308646223771,0.00302593425587023,0.00308943159920767,0.00315434926415385,
0.00316062418320325),.UNSPECIFIED.);
#5320=B_SPLINE_CURVE_WITH_KNOTS('',3,(#257448,#257449,#257450,#257451,#257452,
#257453,#257454,#257455,#257456,#257457,#257458,#257459,#257460,#257461,
#257462,#257463,#257464,#257465,#257466,#257467,#257468,#257469,#257470,
#257471,#257472,#257473,#257474,#257475,#257476,#257477,#257478,#257479,
#257480,#257481,#257482,#257483,#257484,#257485,#257486,#257487,#257488,
#257489,#257490,#257491,#257492,#257493,#257494,#257495,#257496,#257497,
#257498,#257499,#257500,#257501,#257502,#257503,#257504,#257505,#257506,
#257507,#257508,#257509,#257510,#257511,#257512,#257513,#257514,#257515,
#257516,#257517,#257518,#257519,#257520,#257521,#257522,#257523,#257524,
#257525,#257526,#257527,#257528,#257529,#257530,#257531,#257532,#257533,
#257534,#257535,#257536,#257537,#257538,#257539,#257540,#257541,#257542,
#257543,#257544,#257545,#257546,#257547),.UNSPECIFIED.,.F.,.F.,(4,3,3,3,
3,3,3,3,3,3,3,3,3,3,3,3,3,3,3,3,3,3,3,3,3,3,3,3,3,3,3,3,3,4),(1.42043598509044E-9,
8.96508235342264E-5,0.00017713922542495,0.000196453687302173,0.000222064227861238,
0.000285479098223288,0.000349005642442205,0.00036185687903336,0.000392907374604334,
0.000507356384677039,0.000595775533454771,0.000684346942758704,0.000773468971665902,
0.000785814749208657,0.000832772345389472,0.00095290238088768,0.0010774106596845,
0.00117872212381298,0.00121565072790591,0.00131178235000832,0.00141569811402118,
0.0014293613763088,0.0015593159657519,0.0015716294984173,0.00165375706712255,
0.00184401976964395,0.0020413797642039,0.00212850003740835,0.00230460243515425,
0.00235744424762595,0.00259423468409489,0.00263013820146402,0.00296211475216053,
0.0031432589968346),.UNSPECIFIED.);
#5321=B_SPLINE_CURVE_WITH_KNOTS('',3,(#257552,#257553,#257554,#257555,#257556,
#257557,#257558,#257559,#257560,#257561,#257562,#257563,#257564,#257565,
#257566,#257567,#257568,#257569,#257570,#257571,#257572,#257573,#257574,
#257575,#257576,#257577,#257578,#257579,#257580,#257581,#257582,#257583,
#257584,#257585,#257586,#257587,#257588,#257589,#257590,#257591,#257592,
#257593,#257594,#257595,#257596,#257597,#257598,#257599,#257600,#257601,
#257602,#257603,#257604,#257605,#257606,#257607,#257608,#257609,#257610,
#257611,#257612,#257613,#257614,#257615,#257616,#257617,#257618,#257619,
#257620,#257621,#257622,#257623,#257624,#257625,#257626,#257627,#257628,
#257629,#257630,#257631,#257632,#257633,#257634,#257635,#257636,#257637,
#257638,#257639,#257640,#257641,#257642,#257643,#257644,#257645,#257646,
#257647,#257648,#257649,#257650,#257651),.UNSPECIFIED.,.F.,.F.,(4,3,3,3,
3,3,3,3,3,3,3,3,3,3,3,3,3,3,3,3,3,3,3,3,3,3,3,3,3,3,3,3,3,4),(6.93889390390723E-18,
0.000232066433641197,0.000444177580043925,0.000518385099123124,0.00073410278665711,
0.000790156389930058,0.000993487732784391,0.00102299023054913,0.00119225943858464,
0.00134764700041078,0.00150263588856873,0.00158031277986011,0.0017153636919325,
0.00184243086354218,0.00194346242503232,0.00197539097482513,0.00208159421175262,
0.00218487525326351,0.00228393672712271,0.00233199574353222,0.00237046916979016,
0.00246124899502871,0.00255227503603373,0.00264431970440758,0.0026574025351733,
0.00276554736475518,0.0028020292840497,0.00287180839700904,0.00294158750996837,
0.0029630864622377,0.00302593425586324,0.00308943159919611,0.00315434926414153,
0.00316062418320342),.UNSPECIFIED.);
#5322=B_SPLINE_CURVE_WITH_KNOTS('',3,(#257719,#257720,#257721,#257722,#257723,
#257724,#257725,#257726,#257727,#257728,#257729,#257730,#257731,#257732,
#257733,#257734,#257735,#257736,#257737,#257738,#257739,#257740,#257741,
#257742,#257743,#257744,#257745,#257746,#257747,#257748,#257749,#257750,
#257751,#257752,#257753,#257754,#257755,#257756,#257757,#257758,#257759,
#257760,#257761,#257762,#257763,#257764,#257765,#257766,#257767,#257768,
#257769,#257770,#257771,#257772,#257773,#257774,#257775,#257776,#257777,
#257778,#257779,#257780,#257781,#257782,#257783,#257784,#257785,#257786,
#257787,#257788,#257789,#257790,#257791,#257792,#257793,#257794,#257795,
#257796,#257797,#257798,#257799,#257800,#257801,#257802,#257803,#257804,
#257805,#257806,#257807,#257808,#257809,#257810,#257811,#257812,#257813,
#257814,#257815,#257816,#257817,#257818,#257819,#257820,#257821,#257822,
#257823,#257824,#257825,#257826,#257827,#257828,#257829,#257830,#257831,
#257832,#257833,#257834,#257835,#257836,#257837,#257838,#257839,#257840,
#257841,#257842,#257843,#257844,#257845,#257846,#257847,#257848,#257849,
#257850,#257851,#257852,#257853,#257854,#257855,#257856,#257857,#257858,
#257859,#257860,#257861,#257862,#257863,#257864,#257865,#257866,#257867,
#257868,#257869,#257870,#257871,#257872,#257873,#257874,#257875),
 .UNSPECIFIED.,.F.,.F.,(4,3,3,3,3,3,3,3,3,3,3,3,3,3,3,3,3,3,3,3,3,3,3,3,
3,3,3,3,3,3,3,3,3,3,3,3,3,3,3,3,3,3,3,3,3,3,3,3,3,3,3,3,4),(6.7720902829718E-17,
4.10182404401297E-5,4.87365934461908E-5,8.48991743434339E-5,0.000100950649804241,
0.000144177502975245,0.00015950443871374,0.000183552069859812,0.000204873519796485,
0.000207599701005883,0.000228271330673476,0.000247545550387866,0.000265562240286856,
0.00028198101272654,0.00028897409501864,0.000314246599144076,0.000319008877427412,
0.000335084346478968,0.000341191974140351,0.000360114345590793,0.000376222888385349,
0.000387536967904427,0.000398062148035578,0.000398761096784253,0.00040134372044755,
0.000415942457382944,0.000428117175977391,0.000438082433319717,0.000455134767349359,
0.000469444387012387,0.000478513316141094,0.000488773476917098,0.000516028797194734,
0.000543665383177674,0.000571301969160615,0.000614049546779864,0.00063801775485477,
0.000716147133287823,0.000844915617942006,0.000857475220032229,0.000957026632282125,
0.00114329303177871,0.00127603550970948,0.0014210220315045,0.00160971753355524,
0.00179821625845706,0.0019140532645642,0.00198770968410965,0.00213898443966606,
0.0022789813273605,0.00241552617338971,0.00253842863988512,0.00255207101941893),
 .UNSPECIFIED.);
#5323=B_SPLINE_CURVE_WITH_KNOTS('',3,(#257876,#257877,#257878,#257879,#257880,
#257881,#257882,#257883,#257884,#257885,#257886,#257887,#257888),
 .UNSPECIFIED.,.F.,.F.,(4,3,3,3,4),(2.95802686519878E-17,6.33504396955935E-5,
0.000127359484775983,0.000192332933960853,0.000199794734077019),
 .UNSPECIFIED.);
#5324=B_SPLINE_CURVE_WITH_KNOTS('',3,(#257953,#257954,#257955,#257956,#257957,
#257958,#257959,#257960,#257961,#257962,#257963,#257964,#257965),
 .UNSPECIFIED.,.F.,.F.,(4,3,3,3,4),(1.30709403380831E-8,6.47809505539985E-5,
0.000128843980536247,0.000191999731800387,0.000199807394155651),
 .UNSPECIFIED.);
#5325=B_SPLINE_CURVE_WITH_KNOTS('',3,(#257966,#257967,#257968,#257969,#257970,
#257971,#257972,#257973,#257974,#257975,#257976,#257977,#257978,#257979,
#257980,#257981,#257982,#257983,#257984,#257985,#257986,#257987,#257988,
#257989,#257990,#257991,#257992,#257993,#257994,#257995,#257996,#257997,
#257998,#257999,#258000,#258001,#258002,#258003,#258004,#258005,#258006,
#258007,#258008,#258009,#258010,#258011,#258012,#258013,#258014,#258015,
#258016,#258017,#258018,#258019,#258020,#258021,#258022,#258023,#258024,
#258025,#258026,#258027,#258028,#258029,#258030,#258031,#258032,#258033,
#258034,#258035,#258036,#258037,#258038,#258039,#258040,#258041,#258042,
#258043,#258044,#258045,#258046,#258047,#258048,#258049,#258050,#258051,
#258052,#258053,#258054,#258055,#258056,#258057,#258058,#258059,#258060,
#258061,#258062,#258063,#258064,#258065,#258066,#258067,#258068,#258069,
#258070,#258071,#258072,#258073,#258074,#258075,#258076,#258077,#258078,
#258079,#258080,#258081,#258082,#258083,#258084,#258085,#258086,#258087,
#258088,#258089,#258090,#258091,#258092,#258093,#258094,#258095,#258096,
#258097,#258098,#258099,#258100,#258101,#258102,#258103,#258104,#258105,
#258106,#258107,#258108,#258109,#258110,#258111,#258112,#258113,#258114,
#258115,#258116,#258117,#258118,#258119),.UNSPECIFIED.,.F.,.F.,(4,3,3,3,
3,3,3,3,3,3,3,3,3,3,3,3,3,3,3,3,3,3,3,3,3,3,3,3,3,3,3,3,3,3,3,3,3,3,3,3,
3,3,3,3,3,3,3,3,3,3,3,4),(0.,0.000185828670303492,0.000382716193704216,
0.000559934895967205,0.000631076048494892,0.000828487317476088,0.00103761547331349,
0.00111698223038901,0.00126215209698978,0.00146547701524327,0.00157769012123723,
0.00167319966665239,0.00179700293119311,0.00181236538820063,0.00189322814548469,
0.0019236575551527,0.00195311374872379,0.0019744410311806,0.00199411982899787,
0.00201373802954043,0.00203411668352692,0.00203842287855105,0.00205099715760843,
0.00207138344075605,0.00209424343179354,0.0021061580023323,0.00212252899831673,
0.00214057390931081,0.00215045406625544,0.00216323449344539,0.00217718293490172,
0.00219274290031516,0.00220789813799093,0.00220876616973217,0.00222335836349227,
0.00224350969408024,0.0022482563035986,0.00226071864757904,0.00227459317807681,
0.00228941445633327,0.00230590048913228,0.00231448813766505,0.00233284153072107,
0.0023534591125159,0.00236653518185591,0.00241507181483341,0.00241846009663411,
0.0024531315509032,0.00247060413398639,0.0025112586054267,0.00252226520021835,
0.00252430419397965),.UNSPECIFIED.);
#5326=B_SPLINE_CURVE_WITH_KNOTS('',3,(#258187,#258188,#258189,#258190,#258191,
#258192,#258193,#258194,#258195,#258196,#258197,#258198,#258199,#258200,
#258201,#258202,#258203,#258204,#258205,#258206,#258207,#258208,#258209,
#258210,#258211,#258212,#258213,#258214,#258215,#258216,#258217,#258218,
#258219,#258220,#258221,#258222,#258223,#258224,#258225,#258226,#258227,
#258228,#258229,#258230,#258231,#258232,#258233,#258234,#258235,#258236,
#258237,#258238,#258239,#258240,#258241,#258242,#258243,#258244,#258245,
#258246,#258247,#258248,#258249,#258250,#258251,#258252,#258253,#258254,
#258255,#258256,#258257,#258258,#258259,#258260,#258261,#258262,#258263,
#258264,#258265,#258266,#258267,#258268,#258269,#258270,#258271,#258272,
#258273,#258274,#258275,#258276,#258277,#258278,#258279,#258280,#258281,
#258282,#258283,#258284,#258285,#258286,#258287,#258288,#258289,#258290,
#258291,#258292,#258293,#258294,#258295,#258296,#258297,#258298,#258299,
#258300,#258301,#258302,#258303,#258304,#258305,#258306,#258307,#258308,
#258309,#258310,#258311,#258312,#258313,#258314,#258315,#258316,#258317,
#258318,#258319,#258320,#258321,#258322,#258323,#258324,#258325,#258326,
#258327,#258328,#258329,#258330,#258331,#258332,#258333,#258334,#258335,
#258336,#258337,#258338,#258339,#258340,#258341,#258342,#258343),
 .UNSPECIFIED.,.F.,.F.,(4,3,3,3,3,3,3,3,3,3,3,3,3,3,3,3,3,3,3,3,3,3,3,3,
3,3,3,3,3,3,3,3,3,3,3,3,3,3,3,3,3,3,3,3,3,3,3,3,3,3,3,3,4),(2.4532694666934E-16,
4.10182404382943E-5,4.87365934320212E-5,8.48991743424062E-5,0.000100950649789678,
0.000144177502945797,0.000159504438714265,0.000183552069852738,0.000204873519784471,
0.00020759970099121,0.000228271330655785,0.000247545550365401,0.000265562240258363,
0.00028198101269087,0.00028897409500906,0.000314246599079761,0.000319008877428285,
0.000335084346452271,0.000341191974135023,0.000360114345606934,0.000376222888380103,
0.00038753696789393,0.000398062148021026,0.00039876109678529,0.000401343720445582,
0.000415942457351562,0.000428117175926856,0.000438082433318889,0.00045513476735202,
0.000469444387017119,0.000478513316142295,0.000488773476917066,0.000516028797212078,
0.000543665383186523,0.000571301969160969,0.000614049546817563,0.000638017754856327,
0.000716147133288671,0.000844915617965103,0.000857475220033525,0.000957026632284375,
0.00114329303187666,0.00127603550971242,0.00142102203150686,0.00160971753352521,
0.0017982162583827,0.0019140532645685,0.00198770968411401,0.00213898444013934,
0.00227898132821245,0.00241552617381852,0.00253842864049211,0.00255207101942458),
 .UNSPECIFIED.);
#5327=B_SPLINE_CURVE_WITH_KNOTS('',3,(#258344,#258345,#258346,#258347,#258348,
#258349,#258350,#258351,#258352,#258353,#258354,#258355,#258356),
 .UNSPECIFIED.,.F.,.F.,(4,3,3,3,4),(4.9065389333868E-18,6.3350439619856E-5,
0.000127359484550393,0.000192332933484367,0.000199794734076953),
 .UNSPECIFIED.);
#5328=B_SPLINE_CURVE_WITH_KNOTS('',3,(#258421,#258422,#258423,#258424,#258425,
#258426,#258427,#258428,#258429,#258430,#258431,#258432,#258433),
 .UNSPECIFIED.,.F.,.F.,(4,3,3,3,4),(1.30709403943339E-8,6.47809508571854E-5,
0.000128843981032926,0.000191999732342699,0.00019980739415557),
 .UNSPECIFIED.);
#5329=B_SPLINE_CURVE_WITH_KNOTS('',3,(#258434,#258435,#258436,#258437,#258438,
#258439,#258440,#258441,#258442,#258443,#258444,#258445,#258446,#258447,
#258448,#258449,#258450,#258451,#258452,#258453,#258454,#258455,#258456,
#258457,#258458,#258459,#258460,#258461,#258462,#258463,#258464,#258465,
#258466,#258467,#258468,#258469,#258470,#258471,#258472,#258473,#258474,
#258475,#258476,#258477,#258478,#258479,#258480,#258481,#258482,#258483,
#258484,#258485,#258486,#258487,#258488,#258489,#258490,#258491,#258492,
#258493,#258494,#258495,#258496,#258497,#258498,#258499,#258500,#258501,
#258502,#258503,#258504,#258505,#258506,#258507,#258508,#258509,#258510,
#258511,#258512,#258513,#258514,#258515,#258516,#258517,#258518,#258519,
#258520,#258521,#258522,#258523,#258524,#258525,#258526,#258527,#258528,
#258529,#258530,#258531,#258532,#258533,#258534,#258535,#258536,#258537,
#258538,#258539,#258540,#258541,#258542,#258543,#258544,#258545,#258546,
#258547,#258548,#258549,#258550,#258551,#258552,#258553,#258554,#258555,
#258556,#258557,#258558,#258559,#258560,#258561,#258562,#258563,#258564,
#258565,#258566,#258567,#258568,#258569,#258570,#258571,#258572,#258573,
#258574,#258575,#258576,#258577,#258578,#258579,#258580,#258581,#258582,
#258583,#258584,#258585,#258586,#258587),.UNSPECIFIED.,.F.,.F.,(4,3,3,3,
3,3,3,3,3,3,3,3,3,3,3,3,3,3,3,3,3,3,3,3,3,3,3,3,3,3,3,3,3,3,3,3,3,3,3,3,
3,3,3,3,3,3,3,3,3,3,3,4),(0.,0.000185828671060948,0.00038271619533701,0.000559934896067518,
0.000631076048494951,0.000828487317448596,0.00103761547327565,0.00111698223059055,
0.0012621520969899,0.00146547701548244,0.00157769012123739,0.00167319966695433,
0.00179700293135962,0.00181236538852903,0.00189322814548488,0.00192365755511324,
0.00195311374909541,0.00197444103160466,0.00199411982937103,0.00201373802987178,
0.00203411668383433,0.00203842287913242,0.00205099715760863,0.00207138344065033,
0.00209424343157988,0.00210615800318399,0.00212252899910065,0.00214057391002469,
0.00215045406732086,0.00216323449445623,0.00217718293585703,0.00219274290122226,
0.00220789813945474,0.00220876616973239,0.00222335836372349,0.00224350969435737,
0.00224825630573298,0.00226071864973988,0.00227459318032408,0.00228941445870785,
0.00230590049174731,0.00231448814155603,0.00233284153412959,0.00235345911575492,
0.00236653518185614,0.00241507181112009,0.00241846010128728,0.00245313155701541,
0.00247060413857423,0.00251125861000287,0.00252226520475691,0.0025243041939799),
 .UNSPECIFIED.);
#5330=B_SPLINE_CURVE_WITH_KNOTS('',3,(#258655,#258656,#258657,#258658,#258659,
#258660,#258661,#258662,#258663,#258664,#258665,#258666,#258667,#258668,
#258669,#258670,#258671,#258672,#258673,#258674,#258675,#258676,#258677,
#258678,#258679,#258680,#258681,#258682,#258683,#258684,#258685,#258686,
#258687,#258688,#258689,#258690,#258691,#258692,#258693,#258694,#258695,
#258696,#258697,#258698,#258699,#258700,#258701,#258702,#258703,#258704,
#258705,#258706,#258707,#258708,#258709,#258710,#258711,#258712,#258713,
#258714,#258715,#258716,#258717,#258718,#258719,#258720,#258721,#258722,
#258723,#258724,#258725,#258726,#258727,#258728,#258729,#258730,#258731,
#258732,#258733,#258734,#258735,#258736,#258737,#258738,#258739,#258740,
#258741,#258742,#258743,#258744,#258745,#258746,#258747,#258748,#258749,
#258750,#258751,#258752,#258753,#258754,#258755,#258756,#258757,#258758,
#258759,#258760,#258761,#258762,#258763,#258764,#258765,#258766,#258767,
#258768,#258769,#258770,#258771,#258772,#258773,#258774,#258775,#258776,
#258777,#258778,#258779,#258780,#258781,#258782,#258783,#258784,#258785,
#258786,#258787,#258788,#258789,#258790,#258791,#258792,#258793,#258794,
#258795,#258796,#258797,#258798,#258799,#258800,#258801,#258802,#258803,
#258804,#258805,#258806,#258807,#258808,#258809,#258810,#258811),
 .UNSPECIFIED.,.F.,.F.,(4,3,3,3,3,3,3,3,3,3,3,3,3,3,3,3,3,3,3,3,3,3,3,3,
3,3,3,3,3,3,3,3,3,3,3,3,3,3,3,3,3,3,3,3,3,3,3,3,3,3,3,3,4),(4.18021567944388E-16,
4.10182404324863E-5,4.8736593467773E-5,8.48991743663496E-5,0.000100950649826721,
0.000144177502986782,0.000159504438714103,0.000183552069870851,0.000204873519798632,
0.000207599701027599,0.000228271330692523,0.000247545550402923,0.000265562240297104,
0.000281981012731784,0.00028897409503117,0.000314246599158208,0.000319008877427789,
0.000335084346479877,0.000341191974148699,0.000360114345617055,0.00037622288839528,
0.000387536967911221,0.000398062148039941,0.000398761096784631,0.000401343720451845,
0.000415942457358753,0.000428117175935046,0.000438082433322659,0.000455134767347245,
0.000469444387007091,0.000478513316141474,0.00048877347691912,0.000516028797196325,
0.000543665383179294,0.000571301969162262,0.000614049546796093,0.000638017754855134,
0.00071614713328926,0.00084491561809254,0.000857475220033438,0.000957026632282486,
0.00114329303185101,0.00127603550970984,0.00142102203150565,0.00160971753353858,
0.00179821625839819,0.00191405326456454,0.00198770968411041,0.00213898443977125,
0.00227898132754153,0.00241552617348039,0.00253842863999955,0.00255207101941925),
 .UNSPECIFIED.);
#5331=B_SPLINE_CURVE_WITH_KNOTS('',3,(#258812,#258813,#258814,#258815,#258816,
#258817,#258818,#258819,#258820,#258821,#258822,#258823,#258824),
 .UNSPECIFIED.,.F.,.F.,(4,3,3,3,4),(0.,6.33504396296269E-5,0.000127359484566964,
0.00019233293350393,0.000199794734076948),.UNSPECIFIED.);
#5332=B_SPLINE_CURVE_WITH_KNOTS('',3,(#258883,#258884,#258885,#258886,#258887,
#258888,#258889,#258890,#258891,#258892,#258893,#258894,#258895),
 .UNSPECIFIED.,.F.,.F.,(4,3,3,3,4),(2.22293795268E-9,6.4770213458298E-5,
0.00012883335096098,0.00019198917072549,0.000199807394155362),
 .UNSPECIFIED.);
#5333=B_SPLINE_CURVE_WITH_KNOTS('',3,(#258897,#258898,#258899,#258900,#258901,
#258902,#258903,#258904,#258905,#258906,#258907,#258908,#258909,#258910,
#258911,#258912,#258913,#258914,#258915,#258916,#258917,#258918,#258919,
#258920,#258921,#258922,#258923,#258924,#258925,#258926,#258927,#258928,
#258929,#258930,#258931,#258932,#258933,#258934,#258935,#258936,#258937,
#258938,#258939,#258940,#258941,#258942,#258943,#258944,#258945,#258946,
#258947,#258948,#258949,#258950,#258951,#258952,#258953,#258954,#258955,
#258956,#258957,#258958,#258959,#258960,#258961,#258962,#258963,#258964,
#258965,#258966,#258967,#258968,#258969,#258970,#258971,#258972,#258973,
#258974,#258975,#258976,#258977,#258978,#258979,#258980,#258981,#258982,
#258983,#258984,#258985,#258986,#258987,#258988,#258989,#258990,#258991,
#258992,#258993,#258994,#258995,#258996,#258997,#258998,#258999,#259000,
#259001,#259002,#259003,#259004,#259005),.UNSPECIFIED.,.F.,.F.,(4,3,3,3,
3,3,3,3,3,3,3,3,3,3,3,3,3,3,3,3,3,3,3,3,3,3,3,3,3,3,3,3,3,3,3,3,4),(0.,
0.000141625141903644,0.00028605408553883,0.000431017935692696,0.000576069710995619,
0.000624076123138545,0.00079602838556846,0.00096948848303351,0.00114602454208786,
0.00124815224627709,0.0013835380435854,0.00152204450729419,0.00156019030784637,
0.00164202290670349,0.00172485230055762,0.00180786034566625,0.00187222836941565,
0.00191560917303388,0.00195712980570751,0.00199416155797507,0.00202824740020027,
0.00206354484838072,0.00206596024805153,0.00210374901736408,0.00210625691559258,
0.00214321751039884,0.00218002903358911,0.00218426643098488,0.00222069855051545,
0.00226227594637718,0.00227202713580122,0.00228055942654725,0.00233446236996583,
0.00234028546176949,0.00240654563051095,0.00247393114839013,0.0024963044925541),
 .UNSPECIFIED.);
#5334=B_SPLINE_CURVE_WITH_KNOTS('',3,(#259068,#259069,#259070,#259071,#259072,
#259073,#259074,#259075,#259076,#259077,#259078,#259079,#259080),
 .UNSPECIFIED.,.F.,.F.,(4,3,3,3,4),(1.30709404307573E-8,6.47809509226653E-5,
0.000128843981149524,0.000191999732492249,0.000199807394155828),
 .UNSPECIFIED.);
#5335=B_SPLINE_CURVE_WITH_KNOTS('',3,(#259081,#259082,#259083,#259084,#259085,
#259086,#259087,#259088,#259089,#259090,#259091,#259092,#259093,#259094,
#259095,#259096,#259097,#259098,#259099,#259100,#259101,#259102,#259103,
#259104,#259105,#259106,#259107,#259108,#259109,#259110,#259111,#259112,
#259113,#259114,#259115,#259116,#259117,#259118,#259119,#259120,#259121,
#259122,#259123,#259124,#259125,#259126,#259127,#259128,#259129,#259130,
#259131,#259132,#259133,#259134,#259135,#259136,#259137,#259138,#259139,
#259140,#259141,#259142,#259143,#259144,#259145,#259146,#259147,#259148,
#259149,#259150,#259151,#259152,#259153,#259154,#259155,#259156,#259157,
#259158,#259159,#259160,#259161,#259162,#259163,#259164,#259165,#259166,
#259167,#259168,#259169,#259170,#259171,#259172,#259173,#259174,#259175,
#259176,#259177,#259178,#259179,#259180,#259181,#259182,#259183,#259184,
#259185,#259186,#259187,#259188,#259189,#259190,#259191,#259192,#259193,
#259194,#259195,#259196,#259197,#259198,#259199,#259200,#259201,#259202,
#259203,#259204,#259205,#259206,#259207,#259208,#259209,#259210,#259211,
#259212,#259213,#259214,#259215,#259216,#259217,#259218,#259219,#259220,
#259221,#259222,#259223,#259224,#259225,#259226,#259227,#259228,#259229,
#259230,#259231,#259232,#259233,#259234),.UNSPECIFIED.,.F.,.F.,(4,3,3,3,
3,3,3,3,3,3,3,3,3,3,3,3,3,3,3,3,3,3,3,3,3,3,3,3,3,3,3,3,3,3,3,3,3,3,3,3,
3,3,3,3,3,3,3,3,3,3,3,4),(0.,0.000185828671079349,0.000382716195553923,
0.000559934894934763,0.000631076048495516,0.000828487317318044,0.00103761547308088,
0.00111698222831438,0.00126215209699103,0.00146547701368322,0.00157769012123879,
0.00167319966354923,0.00179700292900438,0.00181236538482168,0.00189322814548654,
0.00192365755549693,0.00195311374490067,0.00197444102681827,0.0019941198250935,
0.0020137380259943,0.0020341166801399,0.00203842287257104,0.00205099715761042,
0.00207138344176387,0.00209424343380434,0.00210615799356767,0.0021225289902399,
0.00214057390194255,0.00215045405528944,0.00216323448310569,0.00217718292521093,
0.00219274289121646,0.00220789812292523,0.0022087661697343,0.00222335836113128,
0.0022435096912273,0.00224825628163283,0.0022607186253873,0.00227459315504108,
0.00228941443202955,0.00230590046238967,0.002314488097619,0.00233284149563267,
0.00235345907916819,0.00236653518185818,0.00241507185297962,0.0024184600487372,
0.00245313148794348,0.00247060408675825,0.00251125855826495,0.00252226515349361,
0.00252430419398206),.UNSPECIFIED.);
#5336=B_SPLINE_CURVE_WITH_KNOTS('',3,(#259305,#259306,#259307,#259308,#259309,
#259310,#259311,#259312,#259313,#259314,#259315,#259316,#259317,#259318,
#259319,#259320,#259321,#259322,#259323,#259324,#259325,#259326,#259327,
#259328,#259329,#259330,#259331,#259332,#259333,#259334,#259335,#259336,
#259337,#259338,#259339,#259340,#259341,#259342,#259343,#259344,#259345,
#259346,#259347,#259348,#259349,#259350,#259351,#259352,#259353,#259354,
#259355,#259356,#259357,#259358,#259359,#259360,#259361,#259362,#259363,
#259364,#259365,#259366,#259367,#259368,#259369,#259370,#259371,#259372,
#259373,#259374,#259375,#259376,#259377,#259378,#259379,#259380,#259381,
#259382,#259383,#259384,#259385,#259386,#259387,#259388,#259389,#259390,
#259391,#259392,#259393,#259394,#259395,#259396,#259397,#259398,#259399,
#259400,#259401,#259402,#259403,#259404,#259405,#259406,#259407,#259408,
#259409,#259410,#259411,#259412,#259413,#259414,#259415,#259416,#259417,
#259418,#259419,#259420,#259421,#259422,#259423,#259424,#259425,#259426,
#259427,#259428,#259429,#259430,#259431,#259432,#259433,#259434,#259435,
#259436,#259437,#259438,#259439,#259440,#259441,#259442,#259443,#259444,
#259445,#259446,#259447,#259448,#259449,#259450,#259451,#259452,#259453,
#259454,#259455,#259456,#259457,#259458,#259459,#259460,#259461),
 .UNSPECIFIED.,.F.,.F.,(4,3,3,3,3,3,3,3,3,3,3,3,3,3,3,3,3,3,3,3,3,3,3,3,
3,3,3,3,3,3,3,3,3,3,3,3,3,3,3,3,3,3,3,3,3,3,3,3,3,3,3,3,4),(1.59179194089066E-16,
4.10182404321299E-5,4.87365934503859E-5,8.48991743553393E-5,0.000100950649807767,
0.000144177502998116,0.00015950443871382,0.000183552069860929,0.000204873519804175,
0.000207599701008038,0.000228271330675712,0.000247545550391478,0.000265562240292495,
0.000281981012734991,0.000288974095020833,0.000314246599120257,0.000319008877427481,
0.000335084346465828,0.000341191974142289,0.0003601143455919,0.000376222888387497,
0.000387536967906843,0.000398062148038267,0.000398761096784301,0.000401343720448768,
0.000415942457365449,0.000428117175948292,0.000438082433320561,0.000455134767335398,
0.000469444386988523,0.000478513316141121,0.000488773476917633,0.000516028797205843,
0.000543665383183412,0.000571301969160981,0.000614049546779688,0.000638017754854762,
0.000716147133288069,0.000844915617838834,0.000857475220032411,0.000957026632282044,
0.00114329303175841,0.00127603550970933,0.00142102203150452,0.00160971753356947,
0.00179821625849527,0.0019140532645639,0.00198770968410954,0.00213898444007436,
0.00227898132810696,0.00241552617376272,0.00253842864042649,0.00255207101941848),
 .UNSPECIFIED.);
#5337=B_SPLINE_CURVE_WITH_KNOTS('',3,(#259462,#259463,#259464,#259465,#259466,
#259467,#259468,#259469,#259470,#259471,#259472,#259473,#259474),
 .UNSPECIFIED.,.F.,.F.,(4,3,3,3,4),(0.,6.33504393148245E-5,0.000127359483688777,
0.00019233293172222,0.000199794734076686),.UNSPECIFIED.);
#5338=B_SPLINE_CURVE_WITH_KNOTS('',3,(#259487,#259488,#259489,#259490,#259491,
#259492,#259493,#259494,#259495,#259496,#259497,#259498,#259499,#259500,
#259501,#259502,#259503,#259504,#259505,#259506,#259507,#259508,#259509,
#259510,#259511,#259512,#259513,#259514,#259515,#259516,#259517,#259518,
#259519,#259520,#259521,#259522,#259523,#259524,#259525,#259526,#259527,
#259528,#259529,#259530,#259531,#259532,#259533,#259534,#259535,#259536,
#259537,#259538),.UNSPECIFIED.,.F.,.F.,(4,3,3,3,3,3,3,3,3,3,3,3,3,3,3,3,
3,4),(0.,0.000158823224858671,0.000317052051105456,0.000468924589491904,
0.00047967179401345,0.000658381832507577,0.000717650779103897,0.000878959899787774,
0.000937849178983809,0.000953578178040417,0.00118717940744276,0.00135200974701517,
0.00140677376847571,0.00141855942378738,0.00156529908011683,0.00171075963989374,
0.0018547794947342,0.00187569835796762),.UNSPECIFIED.);
#5339=B_SPLINE_CURVE_WITH_KNOTS('',3,(#259554,#259555,#259556,#259557,#259558,
#259559),.UNSPECIFIED.,.F.,.F.,(4,2,4),(-0.0664084835399893,-0.0331810811129581,
-2.20931276191819E-6),.UNSPECIFIED.);
#5340=B_SPLINE_CURVE_WITH_KNOTS('',3,(#259572,#259573,#259574,#259575,#259576,
#259577,#259578,#259579,#259580,#259581,#259582,#259583,#259584,#259585,
#259586,#259587,#259588,#259589,#259590,#259591,#259592,#259593,#259594,
#259595,#259596,#259597,#259598,#259599,#259600,#259601,#259602,#259603,
#259604,#259605,#259606,#259607,#259608,#259609,#259610,#259611),
 .UNSPECIFIED.,.F.,.F.,(4,3,3,3,3,3,3,3,3,3,3,3,3,4),(0.,0.000161852329700689,
0.000326653855066742,0.000456473147090736,0.000468231828707601,0.000687452602017532,
0.000863637906863081,0.000920751357275229,0.000936463657415201,0.00115607960829242,
0.0013377019175669,0.00139315075344184,0.00168563754506796,0.00187292731483044),
 .UNSPECIFIED.);
#5341=B_SPLINE_CURVE_WITH_KNOTS('',3,(#259627,#259628,#259629,#259630,#259631,
#259632),.UNSPECIFIED.,.F.,.F.,(4,2,4),(-0.0663140791229485,-0.0332720824825186,
-2.08023336209506E-7),.UNSPECIFIED.);
#5342=B_SPLINE_CURVE_WITH_KNOTS('',3,(#259715,#259716,#259717,#259718,#259719,
#259720,#259721,#259722,#259723,#259724),.UNSPECIFIED.,.F.,.F.,(4,3,3,4),
(-2.45811799075953E-5,0.000216663649658451,0.000460938450737844,0.000512405873606687),
 .UNSPECIFIED.);
#5343=B_SPLINE_CURVE_WITH_KNOTS('',3,(#260836,#260837,#260838,#260839,#260840,
#260841,#260842,#260843,#260844,#260845,#260846,#260847,#260848,#260849),
 .UNSPECIFIED.,.F.,.F.,(4,2,2,2,2,2,4),(0.471695282412039,0.547619803692722,
0.63289106477561,0.74233944143791,0.840749628642468,0.94339056482327,0.944354806358975),
 .UNSPECIFIED.);
#5344=B_SPLINE_CURVE_WITH_KNOTS('',3,(#260894,#260895,#260896,#260897,#260898,
#260899,#260900,#260901,#260902,#260903,#260904,#260905,#260906,#260907),
 .UNSPECIFIED.,.F.,.F.,(4,2,2,2,2,2,4),(-0.471695282403551,-0.395770761124079,
-0.31049950004257,-0.201051123381967,-0.102640936178941,0.,0.000964241535706043),
 .UNSPECIFIED.);
#5345=B_SPLINE_CURVE_WITH_KNOTS('',3,(#260997,#260998,#260999,#261000,#261001,
#261002,#261003,#261004,#261005,#261006,#261007,#261008,#261009,#261010,
#261011,#261012,#261013,#261014,#261015,#261016,#261017,#261018,#261019,
#261020,#261021,#261022,#261023,#261024,#261025,#261026,#261027,#261028,
#261029,#261030,#261031,#261032,#261033,#261034,#261035,#261036,#261037,
#261038,#261039,#261040,#261041,#261042,#261043,#261044,#261045,#261046,
#261047,#261048,#261049,#261050,#261051,#261052,#261053,#261054,#261055,
#261056,#261057,#261058,#261059,#261060,#261061,#261062,#261063,#261064,
#261065,#261066,#261067,#261068,#261069,#261070,#261071,#261072,#261073,
#261074,#261075,#261076,#261077,#261078,#261079,#261080,#261081,#261082,
#261083,#261084,#261085,#261086,#261087,#261088,#261089,#261090,#261091,
#261092,#261093,#261094,#261095,#261096,#261097,#261098,#261099,#261100,
#261101,#261102,#261103,#261104,#261105,#261106,#261107,#261108,#261109,
#261110,#261111,#261112,#261113,#261114,#261115,#261116,#261117,#261118,
#261119,#261120,#261121,#261122,#261123,#261124,#261125,#261126,#261127,
#261128,#261129,#261130,#261131,#261132,#261133,#261134,#261135,#261136,
#261137,#261138,#261139,#261140,#261141,#261142,#261143,#261144,#261145,
#261146,#261147,#261148,#261149,#261150,#261151,#261152,#261153,#261154,
#261155,#261156,#261157,#261158,#261159,#261160,#261161,#261162,#261163,
#261164,#261165,#261166,#261167,#261168,#261169,#261170,#261171,#261172,
#261173,#261174,#261175,#261176,#261177,#261178,#261179,#261180,#261181,
#261182,#261183,#261184,#261185,#261186,#261187,#261188,#261189,#261190,
#261191,#261192,#261193,#261194,#261195,#261196,#261197,#261198,#261199,
#261200,#261201,#261202,#261203,#261204,#261205,#261206,#261207,#261208,
#261209,#261210,#261211,#261212,#261213,#261214,#261215,#261216,#261217,
#261218,#261219,#261220,#261221,#261222),.UNSPECIFIED.,.F.,.F.,(4,3,3,3,
3,3,3,3,3,3,3,3,3,3,3,3,3,3,3,3,3,3,3,3,3,3,3,3,3,3,3,3,3,3,3,3,3,3,3,3,
3,3,3,3,3,3,3,3,3,3,3,3,3,3,3,3,3,3,3,3,3,3,3,3,3,3,3,3,3,3,3,3,3,3,3,4),
(0.517250288622702,0.523255252567395,0.529317273923346,0.532336217100087,
0.54742214558073,0.554965109821051,0.558736591941211,0.560984868363799,
0.562508074061372,0.575309787848133,0.587670338105941,0.59267993102266,
0.594690385794448,0.59645141314282,0.600222895262981,0.607765859503303,
0.61563385168986,0.622851787983946,0.626623270104107,0.630394752224268,
0.63793771646459,0.64603114658351,0.653023644945233,0.657541656586839,0.661717061888072,
0.665801492151527,0.668109573425877,0.680867615175072,0.68319550190652,
0.688004367601044,0.690738466146842,0.698281430387163,0.713367358867807,
0.722548733192488,0.72845328734845,0.741175990591504,0.753961138408387,
0.758625144309736,0.769291746524225,0.779988105774088,0.788797001271023,
0.796496519523186,0.804170797139037,0.811964278685929,0.818968858232309,
0.831626226508475,0.834054786712953,0.841597750953274,0.843483492013354,
0.844855917285564,0.845369233073435,0.849140715193595,0.857152162195407,
0.864226643674235,0.871769607914556,0.875275194327448,0.878806455714996,
0.879312572154876,0.887281929206424,0.894398500635516,0.901941464875837,
0.905712946995997,0.907623388041,0.909484429116157,0.921918691453167,0.924570357596798,
0.929478920092114,0.934567603084776,0.939344380756149,0.939656286077438,
0.954742214558079,0.96068040362499,0.966603908881514,0.969828143038719,
0.988792740999909,1.),.UNSPECIFIED.);
#5346=B_SPLINE_CURVE_WITH_KNOTS('',3,(#261226,#261227,#261228,#261229,#261230,
#261231,#261232,#261233,#261234,#261235,#261236,#261237,#261238,#261239,
#261240,#261241,#261242,#261243,#261244,#261245,#261246,#261247,#261248,
#261249,#261250,#261251,#261252,#261253,#261254,#261255,#261256,#261257,
#261258,#261259,#261260,#261261,#261262),.UNSPECIFIED.,.F.,.F.,(4,3,3,3,
3,3,3,3,3,3,3,3,4),(0.,0.0468962635573076,0.0985681948353279,0.120655574161669,
0.180983361242503,0.231914910914981,0.241311148323338,0.291000585436755,
0.346352184925574,0.361966722485007,0.422294509538762,0.471550853402632,
0.482622296592518),.UNSPECIFIED.);
#5347=B_SPLINE_CURVE_WITH_KNOTS('',3,(#261267,#261268,#261269,#261270,#261271,
#261272),.UNSPECIFIED.,.F.,.F.,(4,2,4),(-0.0139153924787358,-0.00694184678164755,
0.),.UNSPECIFIED.);
#5348=B_SPLINE_CURVE_WITH_KNOTS('',3,(#261275,#261276,#261277,#261278,#261279,
#261280,#261281,#261282,#261283,#261284,#261285,#261286,#261287,#261288,
#261289,#261290,#261291,#261292,#261293,#261294,#261295,#261296,#261297,
#261298,#261299,#261300,#261301,#261302,#261303,#261304,#261305,#261306,
#261307,#261308,#261309,#261310,#261311,#261312,#261313,#261314,#261315,
#261316,#261317),.UNSPECIFIED.,.F.,.F.,(4,3,3,3,3,3,3,3,3,3,3,3,3,3,4),
(0.499862670899252,0.507408441954982,0.514954213010712,0.530045755122171,
0.56022883934509,0.620595007790929,0.680961176236767,0.731927837407809,
0.741327344682605,0.790836072123878,0.801693513128444,0.862059681574282,
0.922425850020121,0.971634165151682,0.982792018465959),.UNSPECIFIED.);
#5349=B_SPLINE_CURVE_WITH_KNOTS('',3,(#261318,#261319,#261320,#261321,#261322,
#261323),.UNSPECIFIED.,.F.,.F.,(4,2,4),(0.482622296646676,0.491242483772964,
0.499862670899252),.UNSPECIFIED.);
#5350=B_SPLINE_CURVE_WITH_KNOTS('',3,(#261330,#261331,#261332,#261333,#261334,
#261335,#261336,#261337,#261338,#261339,#261340,#261341,#261342,#261343,
#261344,#261345,#261346,#261347,#261348,#261349,#261350,#261351,#261352,
#261353,#261354,#261355,#261356,#261357,#261358,#261359,#261360,#261361,
#261362,#261363,#261364,#261365,#261366,#261367,#261368,#261369,#261370,
#261371,#261372,#261373,#261374,#261375,#261376,#261377,#261378,#261379,
#261380,#261381,#261382,#261383,#261384,#261385,#261386,#261387,#261388,
#261389,#261390,#261391,#261392,#261393,#261394,#261395,#261396,#261397,
#261398,#261399,#261400,#261401,#261402,#261403,#261404,#261405,#261406,
#261407,#261408,#261409),.UNSPECIFIED.,.F.,.F.,(4,2,2,1,2,2,2,2,2,1,2,2,
2,2,2,2,2,2,1,2,2,2,2,2,2,1,2,2,2,2,2,2,2,2,2,2,2,2,2,2,2,4),(0.0173426649164943,
0.03242039763714,0.0474981303577856,0.0550369967181086,0.0588064298982699,
0.0625758630784312,0.0776535957990762,0.0927313285197211,0.0965007616998823,
0.100270194880043,0.107809061240366,0.122886793961012,0.130425660321335,
0.137964526681658,0.153042259402304,0.16811999212295,0.183197724843596,
0.190736591203919,0.198275457564241,0.213353190284887,0.228430923005532,
0.258586388446823,0.288741853888114,0.318897319329405,0.33397505205005,
0.341513918410373,0.343398635000453,0.345283351590534,0.349052784770696,
0.364130517491342,0.371669383851665,0.379208250211988,0.394285982932634,
0.401824849292957,0.405594282473119,0.409363715653281,0.424441448373927,
0.431980314734249,0.439519181094572,0.454596913815217,0.469674646535862,
0.499830111977151),.UNSPECIFIED.);
#5351=B_SPLINE_CURVE_WITH_KNOTS('',3,(#261494,#261495,#261496,#261497,#261498,
#261499,#261500,#261501,#261502,#261503,#261504,#261505,#261506,#261507,
#261508,#261509,#261510,#261511,#261512,#261513,#261514,#261515,#261516,
#261517,#261518,#261519,#261520,#261521,#261522,#261523,#261524,#261525,
#261526,#261527),.UNSPECIFIED.,.T.,.F.,(4,2,2,2,2,2,2,2,2,2,2,2,2,2,2,2,
4),(-0.765447565020067,-0.717607092096355,-0.669766619172642,-0.621926146468846,
-0.574085673765051,-0.526245201061255,-0.478404728357459,-0.430564255433746,
-0.382723782510034,-0.334883309586321,-0.287042836662609,-0.239202363958813,
-0.191361891255017,-0.143521418551221,-0.0956809458474253,-0.0478404729237126,
0.),.UNSPECIFIED.);
#5352=B_SPLINE_CURVE_WITH_KNOTS('',3,(#261531,#261532,#261533,#261534,#261535,
#261536,#261537,#261538,#261539,#261540,#261541,#261542,#261543,#261544,
#261545,#261546,#261547,#261548),.UNSPECIFIED.,.F.,.F.,(4,2,2,2,2,2,2,2,
4),(0.956809167700879,1.00464962597846,1.05249008425605,1.10033054274855,
1.14817100124105,1.19601145973356,1.24385191822606,1.29169237650364,1.33953283478123),
 .UNSPECIFIED.);
#5353=B_SPLINE_CURVE_WITH_KNOTS('',3,(#261549,#261550,#261551,#261552,#261553,
#261554,#261555,#261556,#261557,#261558,#261559,#261560,#261561,#261562,
#261563,#261564,#261565,#261566,#261567),.UNSPECIFIED.,.F.,.F.,(4,2,2,2,
3,2,2,2,4),(0.574085500620527,0.621925958898112,0.669766417175697,0.7176068756682,
0.765447334160703,0.813287792653206,0.861128251145709,0.908968709423294,
0.956809167700879),.UNSPECIFIED.);
#5354=B_SPLINE_CURVE_WITH_KNOTS('',3,(#261873,#261874,#261875,#261876,#261877,
#261878,#261879,#261880,#261881,#261882),.UNSPECIFIED.,.F.,.F.,(4,2,2,2,
4),(19.6371758899578,19.7291819054161,19.9154716265794,20.0518637703248,
20.1905913221304),.UNSPECIFIED.);
#5355=B_SPLINE_CURVE_WITH_KNOTS('',3,(#261888,#261889,#261890,#261891,#261892,
#261893,#261894,#261895,#261896,#261897,#261898,#261899,#261900,#261901,
#261902,#261903,#261904,#261905,#261906,#261907,#261908,#261909,#261910,
#261911,#261912,#261913,#261914,#261915,#261916,#261917,#261918,#261919,
#261920,#261921,#261922,#261923),.UNSPECIFIED.,.F.,.F.,(4,2,2,2,2,2,2,2,
2,2,2,2,2,2,2,2,2,4),(16.6532889927069,16.7775365014372,16.9626226669129,
17.1467233234454,17.331948216841,17.5158171192104,17.7011850850757,17.884830555016,
18.0703454741475,18.2537770495698,18.4394423104237,18.6226706701434,18.808489146925,
18.9915260123618,19.1775000503537,19.3603580661552,19.5464894746256,19.6371758899578),
 .UNSPECIFIED.);
#5356=B_SPLINE_CURVE_WITH_KNOTS('',3,(#261926,#261927,#261928,#261929,#261930,
#261931,#261932,#261933,#261934,#261935,#261936,#261937),.UNSPECIFIED.,
 .F.,.F.,(4,2,2,2,2,4),(9.99999997842682E-7,0.10581475344356,0.211369364467524,
0.394149985478841,0.581856914636482,0.656719561619648),.UNSPECIFIED.);
#5357=B_SPLINE_CURVE_WITH_KNOTS('',3,(#261942,#261943,#261944,#261945,#261946,
#261947,#261948,#261949,#261950,#261951,#261952,#261953,#261954,#261955,
#261956,#261957,#261958,#261959,#261960,#261961,#261962,#261963,#261964,
#261965,#261966,#261967,#261968,#261969,#261970,#261971,#261972,#261973,
#261974,#261975,#261976,#261977),.UNSPECIFIED.,.F.,.F.,(4,2,2,2,2,2,2,2,
2,2,2,2,2,2,2,2,2,4),(13.6684718789331,13.8194715122135,14.0036466813659,
14.1897487733689,14.3740161516353,14.5598650655264,14.7442311750837,14.9298255267918,
15.1142967841269,15.2996362197495,15.4842188879179,15.6693041664741,15.8540043062326,
16.0388373706964,16.223660791414,16.4082448250315,16.5931970363782,16.6532889927069),
 .UNSPECIFIED.);
#5358=B_SPLINE_CURVE_WITH_KNOTS('',3,(#261978,#261979,#261980,#261981,#261982,
#261983,#261984,#261985,#261986,#261987,#261988,#261989,#261990,#261991,
#261992,#261993,#261994,#261995,#261996,#261997,#261998,#261999,#262000,
#262001,#262002,#262003,#262004,#262005,#262006,#262007,#262008,#262009,
#262010,#262011,#262012,#262013),.UNSPECIFIED.,.F.,.F.,(4,2,2,2,2,2,2,2,
2,2,2,2,2,2,2,2,2,4),(0.656719561619648,0.764725887991887,0.952274080930713,
1.1352463285811,1.3226346599957,1.50572511626435,1.69295320251444,1.87617682495507,
2.06324476751678,2.24661625179435,2.43352466543164,2.61705847632778,2.80380850385605,
2.9875183338738,3.17411164750623,3.3580104164237,3.54444922709864,3.65228028819508),
 .UNSPECIFIED.);
#5359=B_SPLINE_CURVE_WITH_KNOTS('',3,(#262018,#262019,#262020,#262021,#262022,
#262023,#262024,#262025,#262026,#262027,#262028,#262029,#262030,#262031,
#262032,#262033,#262034,#262035,#262036,#262037,#262038,#262039,#262040,
#262041,#262042,#262043,#262044,#262045,#262046,#262047,#262048,#262049,
#262050,#262051,#262052,#262053),.UNSPECIFIED.,.F.,.F.,(4,2,2,2,2,2,2,2,
2,2,2,2,2,2,2,2,2,4),(10.6812382920827,10.851104857409,11.0347760974326,
11.2227618551089,11.4064741773505,11.5942433522979,11.7780027399581,11.9655491785976,
12.1493617836479,12.3366796007057,12.5205517225559,12.70763538643,12.8915734467528,
13.0784178707585,13.262428384412,13.4490290228049,13.6331185648837,13.6684718789331),
 .UNSPECIFIED.);
#5360=B_SPLINE_CURVE_WITH_KNOTS('',3,(#262054,#262055,#262056,#262057,#262058,
#262059,#262060,#262061,#262062,#262063,#262064,#262065,#262066,#262067,
#262068,#262069,#262070,#262071,#262072,#262073,#262074,#262075,#262076,
#262077,#262078,#262079,#262080,#262081,#262082,#262083,#262084,#262085,
#262086,#262087,#262088,#262089),.UNSPECIFIED.,.F.,.F.,(4,2,2,2,2,2,2,2,
2,2,2,2,2,2,2,2,2,4),(3.65228028819508,3.72854896313467,3.91483601545956,
4.0991477302083,4.28528628974196,4.4698198735951,4.65581370674877,4.84057784699934,
5.02643119406342,5.21143331699024,5.39715085899416,5.58239709631972,5.76798391659603,
5.95347909584702,6.13894063729285,6.32468829481463,6.51003031391758,6.64823144772819),
 .UNSPECIFIED.);
#5361=B_SPLINE_CURVE_WITH_KNOTS('',3,(#262094,#262095,#262096,#262097,#262098,
#262099,#262100,#262101,#262102,#262103,#262104,#262105,#262106,#262107,
#262108,#262109,#262110,#262111,#262112,#262113,#262114,#262115,#262116,
#262117,#262118,#262119,#262120,#262121,#262122,#262123,#262124,#262125,
#262126,#262127,#262128,#262129),.UNSPECIFIED.,.F.,.F.,(4,2,2,2,2,2,2,2,
2,2,2,2,2,2,2,2,2,4),(7.68984726224192,7.87165082930837,8.05518424630617,
8.24467155348332,8.42820570351524,8.61752739710676,8.80106654162163,8.99021654601221,
9.1737651724291,9.36273725215303,9.54630007523764,9.73508786455127,9.91866982592597,
10.1072668645547,10.2908731300591,10.479272905576,10.6629088601877,10.6812382920827),
 .UNSPECIFIED.);
#5362=B_SPLINE_CURVE_WITH_KNOTS('',3,(#262130,#262131,#262132,#262133,#262134,
#262135,#262136,#262137,#262138,#262139,#262140,#262141,#262142,#262143,
#262144,#262145,#262146,#262147,#262148,#262149,#262150,#262151,#262152,
#262153,#262154,#262155,#262156,#262157,#262158,#262159,#262160,#262161,
#262162,#262163,#262164,#262165),.UNSPECIFIED.,.F.,.F.,(4,2,2,2,2,2,2,2,
2,2,2,2,2,2,2,2,2,4),(6.64823144772819,6.69603272863731,6.88126124736131,
7.06751949288279,7.2526407494927,7.43915476174748,7.62417516159594,7.81094381907317,
7.99586988628593,8.17853506541196,8.3680551644229,8.55076973151589,8.74041126811349,
8.92318029343516,9.11294010138734,9.29576794379529,9.48564293206951,9.64577796424255),
 .UNSPECIFIED.);
#5363=B_SPLINE_CURVE_WITH_KNOTS('',3,(#262170,#262171,#262172,#262173,#262174,
#262175,#262176,#262177,#262178,#262179,#262180,#262181,#262182,#262183,
#262184,#262185,#262186,#262187,#262188,#262189,#262190,#262191,#262192,
#262193,#262194,#262195,#262196,#262197,#262198,#262199,#262200,#262201,
#262202,#262203,#262204,#262205),.UNSPECIFIED.,.F.,.F.,(4,2,2,2,2,2,2,2,
2,2,2,2,2,2,2,2,2,4),(4.69284812497761,4.87484108509642,5.06568438140767,
5.24914386949795,5.43990900710179,5.62329592544057,5.81398174998649,5.99729558403202,
6.18790085575909,6.37114111792534,6.56166450699332,6.74483074944173,6.93527083128246,
7.11836266102155,7.3087179117712,7.49173500832329,7.68200380040828,7.68984726224192),
 .UNSPECIFIED.);
#5364=B_SPLINE_CURVE_WITH_KNOTS('',3,(#262206,#262207,#262208,#262209,#262210,
#262211,#262212,#262213,#262214,#262215,#262216,#262217,#262218,#262219,
#262220,#262221,#262222,#262223,#262224,#262225,#262226,#262227,#262228,
#262229,#262230,#262231,#262232,#262233,#262234,#262235,#262236,#262237,
#262238,#262239,#262240,#262241),.UNSPECIFIED.,.F.,.F.,(4,2,2,2,2,2,2,2,
2,2,2,2,2,2,2,2,2,4),(9.64577796424255,9.66853329364696,9.85852045979922,
10.0414764425067,10.2315728834384,10.4145970462681,10.6047999665764,10.7878943819427,
10.9782011001008,11.1613674084466,11.3517753610505,11.5350148228858,11.7255215672028,
11.9088351120028,12.0994383270449,12.2828265986255,12.47352408496,12.6469505891598),
 .UNSPECIFIED.);
#5365=B_SPLINE_CURVE_WITH_KNOTS('',3,(#262246,#262247,#262248,#262249,#262250,
#262251,#262252,#262253,#262254,#262255,#262256,#262257,#262258,#262259,
#262260,#262261,#262262,#262263,#262264,#262265,#262266,#262267,#262268,
#262269,#262270,#262271,#262272,#262273,#262274,#262275,#262276,#262277,
#262278,#262279,#262280,#262281,#262282,#262283),.UNSPECIFIED.,.F.,.F.,
(4,2,2,2,2,2,2,2,2,2,2,2,2,2,2,2,2,2,4),(1.69140295334555,1.6939489277295,
1.87761272004276,2.06833630149064,2.25202774081888,2.44286910038617,2.62659054726916,
2.81754600595523,3.00129966734393,3.19236576281363,3.37615370027557,3.56729963547581,
3.75104405717415,3.9421156884852,4.12578967937756,4.3167861485705,4.5003891765768,
4.69130955801646,4.69284812497761),.UNSPECIFIED.);
#5366=B_SPLINE_CURVE_WITH_KNOTS('',3,(#262284,#262285,#262286,#262287,#262288,
#262289,#262290,#262291,#262292,#262293,#262294,#262295,#262296,#262297,
#262298,#262299,#262300,#262301,#262302,#262303,#262304,#262305,#262306,
#262307,#262308,#262309,#262310,#262311,#262312,#262313,#262314,#262315,
#262316,#262317,#262318,#262319),.UNSPECIFIED.,.F.,.F.,(4,2,2,2,2,2,2,2,
2,2,2,2,2,2,2,2,2,4),(12.6469505891598,12.6569874831093,12.8477771616045,
13.0313158798829,13.2221957895684,13.4058098493005,13.5967781445068,13.7804674250698,
13.9715223719929,14.1552866375716,14.3464266103928,14.5302655334145,14.721489010089,
14.9054021915795,15.0967077493918,15.2806947365115,15.4720810474833,15.6534010530854),
 .UNSPECIFIED.);
#5367=B_SPLINE_CURVE_WITH_KNOTS('',3,(#262326,#262327,#262328,#262329,#262330,
#262331,#262332,#262333,#262334,#262335,#262336,#262337,#262338,#262339,
#262340,#262341,#262342,#262343,#262344,#262345,#262346,#262347),
 .UNSPECIFIED.,.F.,.F.,(4,2,2,2,2,2,2,2,2,2,4),(1.0000000306154E-6,0.0999528028591011,
0.19788302817369,0.38146309163929,0.571674110669096,0.755270677145627,0.945616475624153,
1.12923260286766,1.31970857888015,1.50334713803867,1.69140295334555),
 .UNSPECIFIED.);
#5368=B_SPLINE_CURVE_WITH_KNOTS('',3,(#262348,#262349,#262350,#262351,#262352,
#262353,#262354,#262355,#262356,#262357,#262358,#262359,#262360,#262361,
#262362,#262363,#262364,#262365,#262366,#262367,#262368,#262369,#262370,
#262371,#262372,#262373,#262374,#262375,#262376,#262377,#262378,#262379,
#262380,#262381,#262382,#262383,#262384,#262385),.UNSPECIFIED.,.F.,.F.,
(4,2,2,2,2,2,2,2,2,2,2,2,2,2,2,2,2,2,4),(15.6534010530854,15.6561413485049,
15.8476071747258,16.031740271715,16.2232844606574,16.4074898201077,16.5991112999749,
16.7833883816353,16.9750861567836,17.1594344209024,17.3512075673696,17.5356002898847,
17.7273598918852,17.9117164451164,18.103368086355,18.2876904108166,18.4792308121127,
18.6635209866941,18.6649773663315),.UNSPECIFIED.);
#5369=B_SPLINE_CURVE_WITH_KNOTS('',3,(#262406,#262407,#262408,#262409,#262410,
#262411,#262412,#262413,#262414,#262415,#262416,#262417,#262418,#262419,
#262420,#262421,#262422,#262423,#262424,#262425),.UNSPECIFIED.,.F.,.F.,
(4,2,2,2,2,2,2,2,2,4),(18.6649773663315,18.8549465390401,19.0392066732075,
19.2305137878141,19.4147463775256,19.605931123255,19.7901387116017,19.9811969260739,
20.1223735917246,20.2610225738873),.UNSPECIFIED.);
#5370=B_SPLINE_CURVE_WITH_KNOTS('',3,(#263400,#263401,#263402,#263403,#263404,
#263405,#263406,#263407,#263408,#263409),.UNSPECIFIED.,.F.,.F.,(4,2,2,2,
4),(19.6371758899503,19.7291819054085,19.9154716265718,20.0518637703173,
20.1905913221229),.UNSPECIFIED.);
#5371=B_SPLINE_CURVE_WITH_KNOTS('',3,(#263415,#263416,#263417,#263418,#263419,
#263420,#263421,#263422,#263423,#263424,#263425,#263426,#263427,#263428,
#263429,#263430,#263431,#263432,#263433,#263434,#263435,#263436,#263437,
#263438,#263439,#263440,#263441,#263442,#263443,#263444,#263445,#263446,
#263447,#263448,#263449,#263450),.UNSPECIFIED.,.F.,.F.,(4,2,2,2,2,2,2,2,
2,2,2,2,2,2,2,2,2,4),(16.6532889927,16.7775365014302,16.9626226669059,17.1467233234384,
17.3319482168339,17.5158171192032,17.7011850850685,17.8848305550088,18.0703454741403,
18.2537770495626,18.4394423104164,18.6226706701361,18.8084891469176,18.9915260123544,
19.1775000503463,19.3603580661478,19.5464894746181,19.6371758899503),
 .UNSPECIFIED.);
#5372=B_SPLINE_CURVE_WITH_KNOTS('',3,(#263453,#263454,#263455,#263456,#263457,
#263458,#263459,#263460,#263461,#263462,#263463,#263464),.UNSPECIFIED.,
 .F.,.F.,(4,2,2,2,2,4),(9.99999998777405E-7,0.105814753443105,0.211369364466581,
0.3941499854778,0.581856914635303,0.656719561619345),.UNSPECIFIED.);
#5373=B_SPLINE_CURVE_WITH_KNOTS('',3,(#263469,#263470,#263471,#263472,#263473,
#263474,#263475,#263476,#263477,#263478,#263479,#263480,#263481,#263482,
#263483,#263484,#263485,#263486,#263487,#263488,#263489,#263490,#263491,
#263492,#263493,#263494,#263495,#263496,#263497,#263498,#263499,#263500,
#263501,#263502,#263503,#263504),.UNSPECIFIED.,.F.,.F.,(4,2,2,2,2,2,2,2,
2,2,2,2,2,2,2,2,2,4),(13.6684718789269,13.8194715122071,14.0036466813595,
14.1897487733625,14.3740161516288,14.5598650655198,14.7442311750771,14.9298255267851,
15.1142967841201,15.2996362197427,15.4842188879111,15.6693041664674,15.8540043062258,
16.0388373706896,16.2236607914072,16.4082448250246,16.5931970363712,16.6532889927),
 .UNSPECIFIED.);
#5374=B_SPLINE_CURVE_WITH_KNOTS('',3,(#263505,#263506,#263507,#263508,#263509,
#263510,#263511,#263512,#263513,#263514,#263515,#263516,#263517,#263518,
#263519,#263520,#263521,#263522,#263523,#263524,#263525,#263526,#263527,
#263528,#263529,#263530,#263531,#263532,#263533,#263534,#263535,#263536,
#263537,#263538,#263539,#263540),.UNSPECIFIED.,.F.,.F.,(4,2,2,2,2,2,2,2,
2,2,2,2,2,2,2,2,2,4),(0.656719561619345,0.764725887990629,0.95227408092929,
1.13524632857959,1.32263465999408,1.50572511626269,1.69295320251266,1.87617682495327,
2.06324476751485,2.24661625179239,2.43352466542956,2.61705847632565,2.80380850385381,
2.98751833387153,3.17411164750387,3.35801041642132,3.54444922709616,3.65228028819351),
 .UNSPECIFIED.);
#5375=B_SPLINE_CURVE_WITH_KNOTS('',3,(#263545,#263546,#263547,#263548,#263549,
#263550,#263551,#263552,#263553,#263554,#263555,#263556,#263557,#263558,
#263559,#263560,#263561,#263562,#263563,#263564,#263565,#263566,#263567,
#263568,#263569,#263570,#263571,#263572,#263573,#263574,#263575,#263576,
#263577,#263578,#263579,#263580),.UNSPECIFIED.,.F.,.F.,(4,2,2,2,2,2,2,2,
2,2,2,2,2,2,2,2,2,4),(10.6812382920774,10.8511048574036,11.0347760974271,
11.2227618551033,11.4064741773449,11.5942433522923,11.7780027399524,11.9655491785918,
12.1493617836421,12.3366796006998,12.5205517225499,12.7076353864239,12.8915734467467,
13.0784178707524,13.2624283844058,13.4490290227987,13.6331185648774,13.6684718789269),
 .UNSPECIFIED.);
#5376=B_SPLINE_CURVE_WITH_KNOTS('',3,(#263581,#263582,#263583,#263584,#263585,
#263586,#263587,#263588,#263589,#263590,#263591,#263592,#263593,#263594,
#263595,#263596,#263597,#263598,#263599,#263600,#263601,#263602,#263603,
#263604,#263605,#263606,#263607,#263608,#263609,#263610,#263611,#263612,
#263613,#263614,#263615,#263616),.UNSPECIFIED.,.F.,.F.,(4,2,2,2,2,2,2,2,
2,2,2,2,2,2,2,2,2,4),(3.65228028819351,3.72854896313221,3.91483601545701,
4.09914773020572,4.28528628973924,4.46981987359233,4.65581370674584,4.84057784699636,
5.0264311940603,5.21143331698707,5.39715085899084,5.58239709631633,5.76798391659248,
5.95347909584341,6.13894063728909,6.32468829481084,6.51003031391372,6.64823144772506),
 .UNSPECIFIED.);
#5377=B_SPLINE_CURVE_WITH_KNOTS('',3,(#263621,#263622,#263623,#263624,#263625,
#263626,#263627,#263628,#263629,#263630,#263631,#263632,#263633,#263634,
#263635,#263636,#263637,#263638,#263639,#263640,#263641,#263642,#263643,
#263644,#263645,#263646,#263647,#263648,#263649,#263650,#263651,#263652,
#263653,#263654,#263655,#263656),.UNSPECIFIED.,.F.,.F.,(4,2,2,2,2,2,2,2,
2,2,2,2,2,2,2,2,2,4),(7.689847262238,7.87165082930434,8.05518424630204,
8.24467155347909,8.42820570351091,8.61752739710234,8.8010665416171,8.99021654600758,
9.1737651724244,9.36273725214825,9.5463000752328,9.73508786454633,9.91866982592094,
10.1072668645495,10.2908731300539,10.4792729055708,10.6629088601823,10.6812382920774),
 .UNSPECIFIED.);
#5378=B_SPLINE_CURVE_WITH_KNOTS('',3,(#263657,#263658,#263659,#263660,#263661,
#263662,#263663,#263664,#263665,#263666,#263667,#263668,#263669,#263670,
#263671,#263672,#263673,#263674,#263675,#263676,#263677,#263678,#263679,
#263680,#263681,#263682,#263683,#263684,#263685,#263686,#263687,#263688,
#263689,#263690,#263691,#263692),.UNSPECIFIED.,.F.,.F.,(4,2,2,2,2,2,2,2,
2,2,2,2,2,2,2,2,2,4),(6.64823144772506,6.69603272863345,6.88126124735736,
7.06751949287885,7.25264074948867,7.43915476174343,7.6241751615918,7.81094381906902,
7.99586988628166,8.17853506540754,8.36805516441837,8.55076973151126,8.74041126810875,
8.92318029343032,9.11294010138241,9.29576794379026,9.48564293206439,9.64577796423785),
 .UNSPECIFIED.);
#5379=B_SPLINE_CURVE_WITH_KNOTS('',3,(#263697,#263698,#263699,#263700,#263701,
#263702,#263703,#263704,#263705,#263706,#263707,#263708,#263709,#263710,
#263711,#263712,#263713,#263714,#263715,#263716,#263717,#263718,#263719,
#263720,#263721,#263722,#263723,#263724,#263725,#263726,#263727,#263728,
#263729,#263730,#263731,#263732),.UNSPECIFIED.,.F.,.F.,(4,2,2,2,2,2,2,2,
2,2,2,2,2,2,2,2,2,4),(4.69284812497508,4.87484108509382,5.06568438140499,
5.2491438694952,5.43990900709896,5.62329592543766,5.8139817499835,5.99729558402895,
6.18790085575593,6.37114111792207,6.56166450698997,6.74483074943831,6.93527083127893,
7.11836266101793,7.30871791176746,7.49173500831945,7.68200380040434,7.689847262238),
 .UNSPECIFIED.);
#5380=B_SPLINE_CURVE_WITH_KNOTS('',3,(#263733,#263734,#263735,#263736,#263737,
#263738,#263739,#263740,#263741,#263742,#263743,#263744,#263745,#263746,
#263747,#263748,#263749,#263750,#263751,#263752,#263753,#263754,#263755,
#263756,#263757,#263758,#263759,#263760,#263761,#263762,#263763,#263764,
#263765,#263766,#263767,#263768),.UNSPECIFIED.,.F.,.F.,(4,2,2,2,2,2,2,2,
2,2,2,2,2,2,2,2,2,4),(9.64577796423785,9.66853329364174,9.8585204597939,
10.0414764425013,10.2315728834329,10.4145970462625,10.6047999665707,10.7878943819369,
10.9782011000949,11.1613674084406,11.3517753610445,11.5350148228797,11.7255215671966,
11.9088351119965,12.0994383270385,12.2828265986191,12.4735240849535,12.6469505891534),
 .UNSPECIFIED.);
#5381=B_SPLINE_CURVE_WITH_KNOTS('',3,(#263773,#263774,#263775,#263776,#263777,
#263778,#263779,#263780,#263781,#263782,#263783,#263784,#263785,#263786,
#263787,#263788,#263789,#263790,#263791,#263792,#263793,#263794,#263795,
#263796,#263797,#263798,#263799,#263800,#263801,#263802,#263803,#263804,
#263805,#263806,#263807,#263808,#263809,#263810),.UNSPECIFIED.,.F.,.F.,
(4,2,2,2,2,2,2,2,2,2,2,2,2,2,2,2,2,2,4),(1.69140295334456,1.6939489277285,
1.87761272004166,2.06833630148944,2.25202774081757,2.44286910038474,2.62659054726762,
2.81754600595354,3.00129966734211,3.19236576281171,3.37615370027357,3.56729963547373,
3.75104405717199,3.94211568848297,4.12578967937525,4.31678614856811,4.50038917657433,
4.69130955801392,4.69284812497508),.UNSPECIFIED.);
#5382=B_SPLINE_CURVE_WITH_KNOTS('',3,(#263811,#263812,#263813,#263814,#263815,
#263816,#263817,#263818,#263819,#263820,#263821,#263822,#263823,#263824,
#263825,#263826,#263827,#263828,#263829,#263830,#263831,#263832,#263833,
#263834,#263835,#263836,#263837,#263838,#263839,#263840,#263841,#263842,
#263843,#263844,#263845,#263846),.UNSPECIFIED.,.F.,.F.,(4,2,2,2,2,2,2,2,
2,2,2,2,2,2,2,2,2,4),(12.6469505891534,12.6569874831027,12.8477771615977,
13.031315879876,13.2221957895613,13.4058098492933,13.5967781444994,13.7804674250622,
13.9715223719852,14.1552866375637,14.3464266103848,14.5302655334064,14.7214890100807,
14.9054021915711,15.0967077493834,15.2806947365029,15.4720810474746,15.6534010530768),
 .UNSPECIFIED.);
#5383=B_SPLINE_CURVE_WITH_KNOTS('',3,(#263853,#263854,#263855,#263856,#263857,
#263858,#263859,#263860,#263861,#263862,#263863,#263864,#263865,#263866,
#263867,#263868,#263869,#263870,#263871,#263872,#263873,#263874),
 .UNSPECIFIED.,.F.,.F.,(4,2,2,2,2,2,2,2,2,2,4),(9.99999998962388E-7,0.0999528028590244,
0.197883028173547,0.381463091639027,0.571674110668726,0.755270677145161,
0.945616475623583,1.12923260286698,1.31970857887937,1.50334713803778,1.69140295334456),
 .UNSPECIFIED.);
#5384=B_SPLINE_CURVE_WITH_KNOTS('',3,(#263875,#263876,#263877,#263878,#263879,
#263880,#263881,#263882,#263883,#263884,#263885,#263886,#263887,#263888,
#263889,#263890,#263891,#263892,#263893,#263894,#263895,#263896,#263897,
#263898,#263899,#263900,#263901,#263902,#263903,#263904,#263905,#263906,
#263907,#263908,#263909,#263910,#263911,#263912),.UNSPECIFIED.,.F.,.F.,
(4,2,2,2,2,2,2,2,2,2,2,2,2,2,2,2,2,2,4),(15.6534010530768,15.6561413484961,
15.8476071747169,16.031740271706,16.2232844606483,16.4074898200985,16.5991112999656,
16.7833883816259,16.975086156774,17.1594344208927,17.3512075673597,17.5356002898748,
17.7273598918751,17.9117164451062,18.1033680863446,18.2876904108061,18.479230812102,
18.6635209866833,18.6649773663208),.UNSPECIFIED.);
#5385=B_SPLINE_CURVE_WITH_KNOTS('',3,(#263933,#263934,#263935,#263936,#263937,
#263938,#263939,#263940,#263941,#263942,#263943,#263944,#263945,#263946,
#263947,#263948,#263949,#263950,#263951,#263952),.UNSPECIFIED.,.F.,.F.,
(4,2,2,2,2,2,2,2,2,4),(18.6649773663208,18.8549465390291,19.0392066731962,
19.2305137878026,19.414746377514,19.6059311232431,19.7901387115896,19.9811969260615,
20.1223735917122,20.2610225738747),.UNSPECIFIED.);
#5386=B_SPLINE_CURVE_WITH_KNOTS('',3,(#264727,#264728,#264729,#264730,#264731,
#264732,#264733,#264734,#264735,#264736,#264737,#264738,#264739,#264740,
#264741,#264742,#264743,#264744),.UNSPECIFIED.,.F.,.F.,(4,2,2,2,2,2,2,2,
4),(-2.15416629289221,-1.97465268640277,-1.79513907991332,-1.61562497092073,
-1.43611086192814,-1.25659675293555,-1.07708264394295,-0.897569037453512,
-0.718055430964069),.UNSPECIFIED.);
#5387=B_SPLINE_CURVE_WITH_KNOTS('',3,(#264746,#264747,#264748,#264749,#264750,
#264751,#264752,#264753,#264754,#264755,#264756,#264757,#264758,#264759,
#264760,#264761,#264762,#264763,#264764),.UNSPECIFIED.,.F.,.F.,(4,2,2,2,
3,2,2,2,4),(-0.718055430964069,-0.538541824474627,-0.359028217985184,-0.179514108992592,
0.,0.179514108992592,0.359028217985184,0.538541824474627,0.71805543096407),
 .UNSPECIFIED.);
#5388=B_SPLINE_CURVE_WITH_KNOTS('',3,(#264767,#264768,#264769,#264770,#264771,
#264772,#264773,#264774,#264775,#264776,#264777,#264778,#264779,#264780,
#264781,#264782,#264783,#264784,#264785),.UNSPECIFIED.,.F.,.F.,(4,2,2,2,
3,2,2,2,4),(2.15416629289221,2.33367989938165,2.51319350587109,2.69270761486369,
2.87222172385628,3.05173583284887,3.23124994184146,3.4107635483309,3.59027715482035),
 .UNSPECIFIED.);
#5389=B_SPLINE_CURVE_WITH_KNOTS('',3,(#264786,#264787,#264788,#264789,#264790,
#264791,#264792,#264793,#264794,#264795,#264796,#264797,#264798,#264799,
#264800,#264801,#264802,#264803),.UNSPECIFIED.,.F.,.F.,(4,2,2,2,2,2,2,2,
4),(3.59027715482035,3.76979076130979,3.94930436779923,4.12881847679182,
4.30833258578442,4.48784669477701,4.6673608037696,4.84687441025904,5.02638801674849),
 .UNSPECIFIED.);
#5390=B_SPLINE_CURVE_WITH_KNOTS('',3,(#264807,#264808,#264809,#264810,#264811,
#264812,#264813,#264814,#264815,#264816,#264817,#264818,#264819,#264820,
#264821,#264822,#264823,#264824,#264825,#264826,#264827,#264828,#264829,
#264830,#264831,#264832,#264833,#264834,#264835,#264836,#264837,#264838,
#264839,#264840),.UNSPECIFIED.,.T.,.F.,(4,2,2,2,2,2,2,2,2,2,2,2,2,2,2,2,
4),(0.,0.179580636707928,0.359161273415856,0.538740676948295,0.718320080480733,
0.897899484013172,1.07747888754561,1.25705952425354,1.43664016096147,1.61622079766939,
1.79580143437732,1.97538083790976,2.1549602414422,2.33453964497464,2.51411904850708,
2.693699685215,2.87328032192293),.UNSPECIFIED.);
#5391=B_SPLINE_CURVE_WITH_KNOTS('',3,(#264845,#264846,#264847,#264848,#264849,
#264850,#264851,#264852,#264853,#264854,#264855,#264856,#264857,#264858,
#264859,#264860,#264861,#264862,#264863),.UNSPECIFIED.,.F.,.F.,(4,2,2,2,
3,2,2,2,4),(2.1549602414422,2.33453964497464,2.51411904850708,2.693699685215,
2.87328032192293,3.05286095863086,3.23244159533879,3.41202099887123,3.59160040240367),
 .UNSPECIFIED.);
#5392=B_SPLINE_CURVE_WITH_KNOTS('',3,(#264864,#264865,#264866,#264867,#264868,
#264869,#264870,#264871,#264872,#264873,#264874,#264875,#264876,#264877,
#264878,#264879,#264880,#264881),.UNSPECIFIED.,.F.,.F.,(4,2,2,2,2,2,2,2,
4),(0.718320080480733,0.897899484013172,1.07747888754561,1.25705952425354,
1.43664016096147,1.61622079766939,1.79580143437732,1.97538083790976,2.1549602414422),
 .UNSPECIFIED.);
#5393=B_SPLINE_CURVE_WITH_KNOTS('',3,(#265324,#265325,#265326,#265327,#265328,
#265329,#265330,#265331),.UNSPECIFIED.,.F.,.F.,(4,2,2,4),(0.,2.02488294737315,
3.03870599509108,4.05123165236865),.UNSPECIFIED.);
#5394=B_SPLINE_CURVE_WITH_KNOTS('',3,(#265681,#265682,#265683,#265684,#265685,
#265686,#265687,#265688),.UNSPECIFIED.,.F.,.F.,(4,2,2,4),(0.,0.862850707214511,
1.72670633018526,3.45306151607852),.UNSPECIFIED.);
#5395=B_SPLINE_CURVE_WITH_KNOTS('',3,(#266028,#266029,#266030,#266031,#266032,
#266033,#266034,#266035),.UNSPECIFIED.,.F.,.F.,(4,2,2,4),(0.,0.862850707214148,
1.72670633018495,3.45306151607877),.UNSPECIFIED.);
#5396=B_SPLINE_CURVE_WITH_KNOTS('',3,(#266387,#266388,#266389,#266390,#266391,
#266392,#266393,#266394),.UNSPECIFIED.,.F.,.F.,(4,2,2,4),(0.,2.02488294737321,
3.03870599509107,4.05123165236849),.UNSPECIFIED.);
#5397=B_SPLINE_CURVE_WITH_KNOTS('',3,(#266579,#266580,#266581,#266582,#266583,
#266584,#266585,#266586,#266587,#266588,#266589,#266590,#266591,#266592,
#266593,#266594,#266595,#266596,#266597,#266598,#266599,#266600,#266601,
#266602,#266603,#266604,#266605,#266606,#266607,#266608,#266609,#266610,
#266611,#266612),.UNSPECIFIED.,.T.,.F.,(4,2,2,2,2,2,2,2,2,2,2,2,2,2,2,2,
4),(-4.61268662524521,-4.32400022458411,-4.03531382392301,-3.74741439642846,
-3.4595149689339,-3.17161554143936,-2.88371611394482,-2.59502971328371,
-2.30634331262261,-2.0176569119615,-1.7289705113004,-1.44107108380585,-1.15317165631131,
-0.865272228816758,-0.577372801322204,-0.288686400661102,0.),
 .UNSPECIFIED.);
#5398=B_SPLINE_CURVE_WITH_KNOTS('',3,(#266618,#266619,#266620,#266621,#266622,
#266623),.UNSPECIFIED.,.F.,.F.,(4,2,4),(0.,1.49684231771425,2.9926077413886),
 .UNSPECIFIED.);
#5399=B_SPLINE_CURVE_WITH_KNOTS('',3,(#266625,#266626,#266627,#266628,#266629,
#266630,#266631,#266632,#266633,#266634),.UNSPECIFIED.,.F.,.F.,(4,2,2,2,
4),(0.,0.176967107626664,0.344626505766095,0.512071202888707,0.688806050530056),
 .UNSPECIFIED.);
#5400=B_SPLINE_CURVE_WITH_KNOTS('',3,(#266636,#266637,#266638,#266639,#266640,
#266641),.UNSPECIFIED.,.F.,.F.,(4,2,4),(0.,1.49683920424661,2.99526264517898),
 .UNSPECIFIED.);
#5401=B_SPLINE_CURVE_WITH_KNOTS('',3,(#266642,#266643,#266644,#266645,#266646,
#266647,#266648,#266649,#266650,#266651),.UNSPECIFIED.,.F.,.F.,(4,2,2,2,
4),(0.,0.168709295937694,0.329326671396797,0.489872998360341,0.65852259063737),
 .UNSPECIFIED.);
#5402=B_SPLINE_CURVE_WITH_KNOTS('',3,(#266655,#266656,#266657,#266658,#266659,
#266660,#266661,#266662,#266663,#266664,#266665,#266666,#266667,#266668,
#266669,#266670,#266671,#266672,#266673),.UNSPECIFIED.,.F.,.F.,(4,2,2,2,
3,2,2,2,4),(-1.1531716563113,-0.86527222881675,-0.577372801322203,-0.288686400661101,
1.77635683940025E-15,0.288686400661104,0.577372801322206,0.865272228816754,
1.1531716563113),.UNSPECIFIED.);
#5403=B_SPLINE_CURVE_WITH_KNOTS('',3,(#266677,#266678,#266679,#266680,#266681,
#266682,#266683,#266684,#266685,#266686,#266687,#266688,#266689,#266690,
#266691,#266692,#266693,#266694),.UNSPECIFIED.,.F.,.F.,(4,2,2,2,2,2,2,2,
4),(1.1531716563113,1.44107108380585,1.7289705113004,2.0176569119615,2.3063433126226,
2.59502971328371,2.88371611394481,3.17161554143936,3.45951496893391),
 .UNSPECIFIED.);
#5404=B_SPLINE_CURVE_WITH_KNOTS('',3,(#266697,#266698,#266699,#266700,#266701,
#266702),.UNSPECIFIED.,.F.,.F.,(4,2,4),(0.,1.496842317777,2.99260774148207),
 .UNSPECIFIED.);
#5405=B_SPLINE_CURVE_WITH_KNOTS('',3,(#266704,#266705,#266706,#266707,#266708,
#266709,#266710,#266711,#266712,#266713),.UNSPECIFIED.,.F.,.F.,(4,2,2,2,
4),(0.,0.176967107626414,0.34462650576522,0.512071202887293,0.688806050528579),
 .UNSPECIFIED.);
#5406=B_SPLINE_CURVE_WITH_KNOTS('',3,(#266715,#266716,#266717,#266718,#266719,
#266720),.UNSPECIFIED.,.F.,.F.,(4,2,4),(0.,1.49683920424566,2.99526264511799),
 .UNSPECIFIED.);
#5407=B_SPLINE_CURVE_WITH_KNOTS('',3,(#266721,#266722,#266723,#266724,#266725,
#266726,#266727,#266728,#266729,#266730),.UNSPECIFIED.,.F.,.F.,(4,2,2,2,
4),(0.,0.168709295937647,0.329326671396668,0.489872998360253,0.658522590637766),
 .UNSPECIFIED.);
#5408=B_SPLINE_CURVE_WITH_KNOTS('',3,(#266734,#266735,#266736,#266737,#266738,
#266739,#266740,#266741,#266742,#266743,#266744,#266745,#266746,#266747,
#266748,#266749,#266750,#266751),.UNSPECIFIED.,.F.,.F.,(4,2,2,2,2,2,2,2,
4),(1.1531716563113,1.44107108380585,1.7289705113004,2.01765691196151,2.30634331262261,
2.59502971328371,2.88371611394481,3.17161554143937,3.45951496893392),
 .UNSPECIFIED.);
#5409=B_SPLINE_CURVE_WITH_KNOTS('',3,(#266755,#266756,#266757,#266758,#266759,
#266760,#266761,#266762,#266763,#266764,#266765,#266766,#266767,#266768,
#266769,#266770,#266771,#266772,#266773),.UNSPECIFIED.,.F.,.F.,(4,2,2,2,
3,2,2,2,4),(3.45951496893392,3.74741439642846,4.035313823923,4.32400022458411,
4.61268662524521,4.90137302590632,5.19005942656742,5.47795885406197,5.76585828155651),
 .UNSPECIFIED.);
#5410=B_SPLINE_CURVE_WITH_KNOTS('',3,(#266776,#266777,#266778,#266779,#266780,
#266781,#266782,#266783,#266784,#266785),.UNSPECIFIED.,.F.,.F.,(4,2,2,2,
4),(-0.658522598895983,-0.489809349878546,-0.32920232171901,-0.168645651361104,
0.),.UNSPECIFIED.);
#5411=B_SPLINE_CURVE_WITH_KNOTS('',3,(#266787,#266788,#266789,#266790,#266791,
#266792),.UNSPECIFIED.,.F.,.F.,(4,2,4),(-2.99260774139286,-1.49684228178934,
0.),.UNSPECIFIED.);
#5412=B_SPLINE_CURVE_WITH_KNOTS('',3,(#266794,#266795,#266796,#266797,#266798,
#266799,#266800,#266801,#266802,#266803),.UNSPECIFIED.,.F.,.F.,(4,2,2,2,
4),(-0.688806220570509,-0.51183539502754,-0.344166623478192,-0.176731189784664,
0.),.UNSPECIFIED.);
#5413=B_SPLINE_CURVE_WITH_KNOTS('',3,(#266804,#266805,#266806,#266807,#266808,
#266809),.UNSPECIFIED.,.F.,.F.,(4,2,4),(-2.99526264006051,-1.49683924471816,
0.),.UNSPECIFIED.);
#5414=B_SPLINE_CURVE_WITH_KNOTS('',3,(#266813,#266814,#266815,#266816,#266817,
#266818,#266819,#266820,#266821,#266822,#266823,#266824,#266825,#266826,
#266827,#266828,#266829,#266830),.UNSPECIFIED.,.F.,.F.,(4,2,2,2,2,2,2,2,
4),(1.15317165631131,1.44107108380585,1.7289705113004,2.0176569119615,2.30634331262261,
2.59502971328371,2.88371611394481,3.17161554143936,3.4595149689339),
 .UNSPECIFIED.);
#5415=B_SPLINE_CURVE_WITH_KNOTS('',3,(#266834,#266835,#266836,#266837,#266838,
#266839,#266840,#266841,#266842,#266843,#266844,#266845,#266846,#266847,
#266848,#266849,#266850,#266851,#266852),.UNSPECIFIED.,.F.,.F.,(4,2,2,2,
3,2,2,2,4),(-1.1531716563113,-0.865272228816753,-0.577372801322205,-0.288686400661102,
1.55431223447522E-15,0.288686400661105,0.577372801322209,0.865272228816757,
1.15317165631131),.UNSPECIFIED.);
#5416=B_SPLINE_CURVE_WITH_KNOTS('',3,(#266855,#266856,#266857,#266858,#266859,
#266860,#266861,#266862,#266863,#266864),.UNSPECIFIED.,.F.,.F.,(4,2,2,2,
4),(-0.688806220570527,-0.511835395027638,-0.344166623478395,-0.17673118978486,
0.),.UNSPECIFIED.);
#5417=B_SPLINE_CURVE_WITH_KNOTS('',3,(#266866,#266867,#266868,#266869,#266870,
#266871),.UNSPECIFIED.,.F.,.F.,(4,2,4),(-2.99526263988214,-1.49683924469841,
0.),.UNSPECIFIED.);
#5418=B_SPLINE_CURVE_WITH_KNOTS('',3,(#266873,#266874,#266875,#266876,#266877,
#266878,#266879,#266880,#266881,#266882),.UNSPECIFIED.,.F.,.F.,(4,2,2,2,
4),(-0.658522598898453,-0.489809349881006,-0.3292023217204,-0.168645651361312,
0.),.UNSPECIFIED.);
#5419=B_SPLINE_CURVE_WITH_KNOTS('',3,(#266883,#266884,#266885,#266886,#266887,
#266888),.UNSPECIFIED.,.F.,.F.,(4,2,4),(-2.99260774142664,-1.49684228180428,
0.),.UNSPECIFIED.);
#5420=B_SPLINE_CURVE_WITH_KNOTS('',3,(#266892,#266893,#266894,#266895,#266896,
#266897,#266898,#266899,#266900,#266901,#266902,#266903,#266904,#266905,
#266906,#266907,#266908,#266909),.UNSPECIFIED.,.F.,.F.,(4,2,2,2,2,2,2,2,
4),(-3.4595149689339,-3.17161554143936,-2.88371611394481,-2.59502971328371,
-2.3063433126226,-2.0176569119615,-1.7289705113004,-1.44107108380585,-1.1531716563113),
 .UNSPECIFIED.);
#5421=B_SPLINE_CURVE_WITH_KNOTS('',3,(#266913,#266914,#266915,#266916,#266917,
#266918,#266919,#266920,#266921,#266922,#266923,#266924,#266925,#266926,
#266927,#266928,#266929,#266930,#266931),.UNSPECIFIED.,.F.,.F.,(4,2,2,2,
3,2,2,2,4),(-1.1531716563113,-0.865272228816754,-0.577372801322206,-0.288686400661103,
0.,0.288686400661104,0.577372801322206,0.865272228816754,1.1531716563113),
 .UNSPECIFIED.);
#5422=B_SPLINE_CURVE_WITH_KNOTS('',3,(#266934,#266935,#266936,#266937,#266938,
#266939),.UNSPECIFIED.,.F.,.F.,(4,2,4),(0.,1.49683920421981,2.99526264506199),
 .UNSPECIFIED.);
#5423=B_SPLINE_CURVE_WITH_KNOTS('',3,(#266941,#266942,#266943,#266944,#266945,
#266946,#266947,#266948,#266949,#266950),.UNSPECIFIED.,.F.,.F.,(4,2,2,2,
4),(0.,0.168709295937734,0.329326671397018,0.48987299836074,0.658522590638148),
 .UNSPECIFIED.);
#5424=B_SPLINE_CURVE_WITH_KNOTS('',3,(#266952,#266953,#266954,#266955,#266956,
#266957),.UNSPECIFIED.,.F.,.F.,(4,2,4),(0.,1.49684231774429,2.99260774143943),
 .UNSPECIFIED.);
#5425=B_SPLINE_CURVE_WITH_KNOTS('',3,(#266958,#266959,#266960,#266961,#266962,
#266963,#266964,#266965,#266966,#266967),.UNSPECIFIED.,.F.,.F.,(4,2,2,2,
4),(0.,0.176967107626893,0.344626505766581,0.512071202889326,0.688806050530784),
 .UNSPECIFIED.);
#5426=B_SPLINE_CURVE_WITH_KNOTS('',3,(#266970,#266971,#266972,#266973,#266974,
#266975,#266976,#266977,#266978,#266979),.UNSPECIFIED.,.F.,.F.,(4,2,2,2,
4),(-0.658522598896504,-0.489809349878851,-0.329202321719165,-0.168645651361139,
0.),.UNSPECIFIED.);
#5427=B_SPLINE_CURVE_WITH_KNOTS('',3,(#266981,#266982,#266983,#266984,#266985,
#266986),.UNSPECIFIED.,.F.,.F.,(4,2,4),(-2.99260774147142,-1.49684228182412,
0.),.UNSPECIFIED.);
#5428=B_SPLINE_CURVE_WITH_KNOTS('',3,(#266988,#266989,#266990,#266991,#266992,
#266993,#266994,#266995,#266996,#266997),.UNSPECIFIED.,.F.,.F.,(4,2,2,2,
4),(-0.688806220566902,-0.511835395024936,-0.344166623476774,-0.176731189784255,
0.),.UNSPECIFIED.);
#5429=B_SPLINE_CURVE_WITH_KNOTS('',3,(#266998,#266999,#267000,#267001,#267002,
#267003),.UNSPECIFIED.,.F.,.F.,(4,2,4),(-2.9952626398682,-1.49683924471003,
0.),.UNSPECIFIED.);
#5430=B_SPLINE_CURVE_WITH_KNOTS('',3,(#267007,#267008,#267009,#267010,#267011,
#267012,#267013,#267014,#267015,#267016,#267017,#267018,#267019,#267020,
#267021,#267022,#267023,#267024,#267025),.UNSPECIFIED.,.F.,.F.,(4,2,2,2,
3,2,2,2,4),(3.4595149689339,3.74741439642845,4.035313823923,4.3240002245841,
4.61268662524521,4.90137302590631,5.19005942656741,5.47795885406196,5.76585828155651),
 .UNSPECIFIED.);
#5431=B_SPLINE_CURVE_WITH_KNOTS('',3,(#267029,#267030,#267031,#267032,#267033,
#267034,#267035,#267036,#267037,#267038,#267039,#267040,#267041,#267042,
#267043,#267044,#267045,#267046),.UNSPECIFIED.,.F.,.F.,(4,2,2,2,2,2,2,2,
4),(5.76585828155651,6.05375770905105,6.3416571365456,6.6303435372067,6.91902993786781,
7.20771633852891,7.49640273919001,7.78430216668456,8.07220159417911),
 .UNSPECIFIED.);
#5432=B_SPLINE_CURVE_WITH_KNOTS('',3,(#267049,#267050,#267051,#267052,#267053,
#267054),.UNSPECIFIED.,.F.,.F.,(4,2,4),(0.,1.49684231777726,2.99260774149539),
 .UNSPECIFIED.);
#5433=B_SPLINE_CURVE_WITH_KNOTS('',3,(#267056,#267057,#267058,#267059,#267060,
#267061,#267062,#267063,#267064,#267065),.UNSPECIFIED.,.F.,.F.,(4,2,2,2,
4),(0.,0.176967107626481,0.344626505765638,0.512071202888007,0.688806050529249),
 .UNSPECIFIED.);
#5434=B_SPLINE_CURVE_WITH_KNOTS('',3,(#267067,#267068,#267069,#267070,#267071,
#267072),.UNSPECIFIED.,.F.,.F.,(4,2,4),(0.,1.49683920427303,2.9952626452325),
 .UNSPECIFIED.);
#5435=B_SPLINE_CURVE_WITH_KNOTS('',3,(#267073,#267074,#267075,#267076,#267077,
#267078,#267079,#267080,#267081,#267082),.UNSPECIFIED.,.F.,.F.,(4,2,2,2,
4),(0.,0.168709295937688,0.329326671396385,0.489872998359487,0.658522590636729),
 .UNSPECIFIED.);
#5436=B_SPLINE_CURVE_WITH_KNOTS('',3,(#267085,#267086,#267087,#267088,#267089,
#267090,#267091,#267092,#267093,#267094),.UNSPECIFIED.,.F.,.F.,(4,2,2,2,
4),(-0.688806220572771,-0.511835395028998,-0.34416662347923,-0.176731189785183,
0.),.UNSPECIFIED.);
#5437=B_SPLINE_CURVE_WITH_KNOTS('',3,(#267096,#267097,#267098,#267099,#267100,
#267101),.UNSPECIFIED.,.F.,.F.,(4,2,4),(-2.99526263994789,-1.49683924471765,
0.),.UNSPECIFIED.);
#5438=B_SPLINE_CURVE_WITH_KNOTS('',3,(#267103,#267104,#267105,#267106,#267107,
#267108,#267109,#267110,#267111,#267112),.UNSPECIFIED.,.F.,.F.,(4,2,2,2,
4),(-0.658522598893829,-0.489809349877018,-0.329202321717993,-0.168645651360644,
0.),.UNSPECIFIED.);
#5439=B_SPLINE_CURVE_WITH_KNOTS('',3,(#267113,#267114,#267115,#267116,#267117,
#267118),.UNSPECIFIED.,.F.,.F.,(4,2,4),(-2.99260774145968,-1.496842281811,
0.),.UNSPECIFIED.);
#5440=B_SPLINE_CURVE_WITH_KNOTS('',3,(#268102,#268103,#268104,#268105,#268106,
#268107,#268108),.UNSPECIFIED.,.F.,.F.,(4,3,4),(-8.06482196325813E-5,0.,
0.00573600054306479),.UNSPECIFIED.);
#5441=B_SPLINE_CURVE_WITH_KNOTS('',3,(#268112,#268113,#268114,#268115),
 .UNSPECIFIED.,.F.,.F.,(4,4),(0.,0.00872457834628637),.UNSPECIFIED.);
#5442=B_SPLINE_CURVE_WITH_KNOTS('',3,(#268116,#268117,#268118,#268119,#268120,
#268121,#268122),.UNSPECIFIED.,.F.,.F.,(4,3,4),(4.79067216416971E-16,0.00573600054306518,
0.00581664876269783),.UNSPECIFIED.);
#5443=B_SPLINE_CURVE_WITH_KNOTS('',3,(#268125,#268126,#268127,#268128),
 .UNSPECIFIED.,.F.,.F.,(4,4),(0.,0.0087245783462611),.UNSPECIFIED.);
#5444=B_SPLINE_CURVE_WITH_KNOTS('',3,(#271700,#271701,#271702,#271703),
 .UNSPECIFIED.,.F.,.F.,(4,4),(0.,0.00872457834628661),.UNSPECIFIED.);
#5445=B_SPLINE_CURVE_WITH_KNOTS('',3,(#271704,#271705,#271706,#271707,#271708,
#271709,#271710),.UNSPECIFIED.,.F.,.F.,(4,3,4),(-8.0648219632873E-5,0.,
0.00573600054306445),.UNSPECIFIED.);
#5446=B_SPLINE_CURVE_WITH_KNOTS('',3,(#271714,#271715,#271716,#271717),
 .UNSPECIFIED.,.F.,.F.,(4,4),(0.,0.008724578346262),.UNSPECIFIED.);
#5447=B_SPLINE_CURVE_WITH_KNOTS('',3,(#271718,#271719,#271720,#271721,#271722,
#271723,#271724),.UNSPECIFIED.,.F.,.F.,(4,3,4),(1.81429262580847E-14,0.00573600054306257,
0.00581664876269541),.UNSPECIFIED.);
#5448=B_SPLINE_CURVE_WITH_KNOTS('',3,(#272380,#272381,#272382,#272383),
 .UNSPECIFIED.,.F.,.F.,(4,4),(9.54097911787244E-18,0.00872457834626197),
 .UNSPECIFIED.);
#5449=B_SPLINE_CURVE_WITH_KNOTS('',3,(#272384,#272385,#272386,#272387,#272388,
#272389,#272390),.UNSPECIFIED.,.F.,.F.,(4,3,4),(0.,0.00573600054306478,
0.00581664876269765),.UNSPECIFIED.);
#5450=B_SPLINE_CURVE_WITH_KNOTS('',3,(#272719,#272720,#272721,#272722),
 .UNSPECIFIED.,.F.,.F.,(4,4),(0.,0.00872457834628667),.UNSPECIFIED.);
#5451=B_SPLINE_CURVE_WITH_KNOTS('',3,(#272724,#272725,#272726,#272727,#272728,
#272729,#272730),.UNSPECIFIED.,.F.,.F.,(4,3,4),(6.2375853683061E-16,0.00573600054306585,
0.00581664876269842),.UNSPECIFIED.);
#5452=B_SPLINE_CURVE_WITH_KNOTS('',3,(#273060,#273061,#273062,#273063,#273064,
#273065,#273066),.UNSPECIFIED.,.F.,.F.,(4,3,4),(-8.06482196327907E-5,0.,
0.00573600054306464),.UNSPECIFIED.);
#5453=B_SPLINE_CURVE_WITH_KNOTS('',3,(#273069,#273070,#273071,#273072),
 .UNSPECIFIED.,.F.,.F.,(4,4),(0.,0.0087245783462611),.UNSPECIFIED.);
#5454=B_SPLINE_CURVE_WITH_KNOTS('',3,(#273401,#273402,#273403,#273404,#273405,
#273406,#273407),.UNSPECIFIED.,.F.,.F.,(4,3,4),(-8.06482196325413E-5,0.,
0.00573600054306597),.UNSPECIFIED.);
#5455=B_SPLINE_CURVE_WITH_KNOTS('',3,(#273410,#273411,#273412,#273413),
 .UNSPECIFIED.,.F.,.F.,(4,4),(0.,0.00872457834628645),.UNSPECIFIED.);
#5456=B_SPLINE_CURVE_WITH_KNOTS('',3,(#273943,#273944,#273945,#273946,#273947,
#273948,#273949,#273950,#273951,#273952),.UNSPECIFIED.,.F.,.F.,(4,3,3,4),
(0.,0.000338853006806234,0.000677883858435526,0.00084344531229996),
 .UNSPECIFIED.);
#5457=B_SPLINE_CURVE_WITH_KNOTS('',3,(#273956,#273957,#273958,#273959,#273960,
#273961,#273962,#273963,#273964,#273965),.UNSPECIFIED.,.F.,.F.,(4,3,3,4),
(0.,0.000336488810998176,0.000673156284667907,0.000840479374202616),
 .UNSPECIFIED.);
#5458=B_SPLINE_CURVE_WITH_KNOTS('',3,(#273970,#273971,#273972,#273973,#273974,
#273975,#273976,#273977,#273978,#273979),.UNSPECIFIED.,.F.,.F.,(4,3,3,4),
(0.,0.000336488811000739,0.000673156284671631,0.000840479374202609),
 .UNSPECIFIED.);
#5459=B_SPLINE_CURVE_WITH_KNOTS('',3,(#273985,#273986,#273987,#273988,#273989,
#273990,#273991,#273992,#273993,#273994),.UNSPECIFIED.,.F.,.F.,(4,3,3,4),
(0.,0.000338853006809123,0.000677883858442031,0.000843445312299953),
 .UNSPECIFIED.);
#5460=SHAPE_REPRESENTATION_RELATIONSHIP('SRR','None',#276488,#5466);
#5461=SHAPE_REPRESENTATION_RELATIONSHIP('SRR','None',#276489,#5467);
#5462=SHAPE_REPRESENTATION_RELATIONSHIP('SRR','None',#276490,#5468);
#5463=SHAPE_REPRESENTATION_RELATIONSHIP('SRR','None',#276491,#5469);
#5464=SHAPE_REPRESENTATION_RELATIONSHIP('SRR','None',#276492,#5470);
#5465=SHAPE_REPRESENTATION_RELATIONSHIP('SRR','None',#276493,#5471);
#5466=ADVANCED_BREP_SHAPE_REPRESENTATION('',(#5501),#276456);
#5467=ADVANCED_BREP_SHAPE_REPRESENTATION('',(#5502,#5503),#276457);
#5468=ADVANCED_BREP_SHAPE_REPRESENTATION('',(#5504,#5505,#5506,#5507,#5508,
#5509,#5510,#5511,#5512,#5513,#5514,#5515,#5516,#5517,#5518,#5519,#5520,
#5521,#5522,#5523,#5524),#276458);
#5469=ADVANCED_BREP_SHAPE_REPRESENTATION('',(#5525,#5526,#5527),#276459);
#5470=ADVANCED_BREP_SHAPE_REPRESENTATION('',(#5528),#276460);
#5471=ADVANCED_BREP_SHAPE_REPRESENTATION('',(#44),#276461);
#5472=STYLED_ITEM('',(#276527),#5501);
#5473=STYLED_ITEM('',(#276528),#5502);
#5474=STYLED_ITEM('',(#276528),#5503);
#5475=STYLED_ITEM('',(#276529),#5504);
#5476=STYLED_ITEM('',(#276529),#5505);
#5477=STYLED_ITEM('',(#276529),#5506);
#5478=STYLED_ITEM('',(#276529),#5507);
#5479=STYLED_ITEM('',(#276529),#5508);
#5480=STYLED_ITEM('',(#276529),#5509);
#5481=STYLED_ITEM('',(#276529),#5510);
#5482=STYLED_ITEM('',(#276529),#5511);
#5483=STYLED_ITEM('',(#276529),#5512);
#5484=STYLED_ITEM('',(#276529),#5513);
#5485=STYLED_ITEM('',(#276529),#5514);
#5486=STYLED_ITEM('',(#276529),#5515);
#5487=STYLED_ITEM('',(#276529),#5516);
#5488=STYLED_ITEM('',(#276529),#5517);
#5489=STYLED_ITEM('',(#276529),#5518);
#5490=STYLED_ITEM('',(#276529),#5519);
#5491=STYLED_ITEM('',(#276529),#5520);
#5492=STYLED_ITEM('',(#276529),#5521);
#5493=STYLED_ITEM('',(#276529),#5522);
#5494=STYLED_ITEM('',(#276529),#5523);
#5495=STYLED_ITEM('',(#276529),#5524);
#5496=STYLED_ITEM('',(#276530),#5525);
#5497=STYLED_ITEM('',(#276530),#5526);
#5498=STYLED_ITEM('',(#276530),#5527);
#5499=STYLED_ITEM('',(#276527),#5528);
#5500=STYLED_ITEM('',(#276527),#44);
#5501=MANIFOLD_SOLID_BREP('Body1',#98697);
#5502=MANIFOLD_SOLID_BREP('Body1',#98698);
#5503=MANIFOLD_SOLID_BREP('Body2',#98699);
#5504=MANIFOLD_SOLID_BREP('Body1',#98700);
#5505=MANIFOLD_SOLID_BREP('Body2',#98701);
#5506=MANIFOLD_SOLID_BREP('Body3',#98702);
#5507=MANIFOLD_SOLID_BREP('Body4',#98703);
#5508=MANIFOLD_SOLID_BREP('Body5',#98704);
#5509=MANIFOLD_SOLID_BREP('Body6',#98705);
#5510=MANIFOLD_SOLID_BREP('Body7',#98706);
#5511=MANIFOLD_SOLID_BREP('Body8',#98707);
#5512=MANIFOLD_SOLID_BREP('Body9',#98708);
#5513=MANIFOLD_SOLID_BREP('Body10',#98709);
#5514=MANIFOLD_SOLID_BREP('Body11',#98710);
#5515=MANIFOLD_SOLID_BREP('Body12',#98711);
#5516=MANIFOLD_SOLID_BREP('Body13',#98712);
#5517=MANIFOLD_SOLID_BREP('Body14',#98713);
#5518=MANIFOLD_SOLID_BREP('Body15',#98714);
#5519=MANIFOLD_SOLID_BREP('Body16',#98715);
#5520=MANIFOLD_SOLID_BREP('Body17',#98716);
#5521=MANIFOLD_SOLID_BREP('Body18',#98717);
#5522=MANIFOLD_SOLID_BREP('Body19',#98718);
#5523=MANIFOLD_SOLID_BREP('Body20',#98719);
#5524=MANIFOLD_SOLID_BREP('Body21',#98720);
#5525=MANIFOLD_SOLID_BREP('Body1',#98721);
#5526=MANIFOLD_SOLID_BREP('Body2',#98722);
#5527=MANIFOLD_SOLID_BREP('Body3',#98723);
#5528=MANIFOLD_SOLID_BREP('Body1',#98724);
#5529=TOROIDAL_SURFACE('',#98859,23.,2.);
#5530=TOROIDAL_SURFACE('',#98866,23.,2.);
#5531=TOROIDAL_SURFACE('',#98868,23.,2.);
#5532=TOROIDAL_SURFACE('',#98874,23.,2.);
#5533=TOROIDAL_SURFACE('',#98876,9.25400000000018,0.254);
#5534=TOROIDAL_SURFACE('',#98881,11.0630000000002,0.254);
#5535=TOROIDAL_SURFACE('',#98940,4.30674336537535,1.57226);
#5536=TOROIDAL_SURFACE('',#98962,2.71842830011631,0.635000000000008);
#5537=TOROIDAL_SURFACE('',#98969,2.1119189867422,0.317500000000003);
#5538=TOROIDAL_SURFACE('',#99037,50.254,0.254);
#5539=TOROIDAL_SURFACE('',#99042,51.016,0.254);
#5540=TOROIDAL_SURFACE('',#99053,56.621,0.254);
#5541=TOROIDAL_SURFACE('',#99058,55.859,0.254);
#5542=TOROIDAL_SURFACE('',#99077,59.0285554514622,0.127);
#5543=TOROIDAL_SURFACE('',#99082,62.8464445485378,0.127);
#5544=TOROIDAL_SURFACE('',#99087,59.0285554514622,0.127);
#5545=TOROIDAL_SURFACE('',#99092,62.8464445485378,0.127);
#5546=TOROIDAL_SURFACE('',#99098,58.2189663438286,0.635);
#5547=TOROIDAL_SURFACE('',#99103,58.3085779254084,0.635);
#5548=TOROIDAL_SURFACE('',#99107,63.5664220745916,0.635);
#5549=TOROIDAL_SURFACE('',#99112,63.6560336561714,0.635);
#5550=TOROIDAL_SURFACE('',#99381,60.0045305169095,0.635);
#5551=TOROIDAL_SURFACE('',#99384,61.8704694830905,0.635);
#5552=TOROIDAL_SURFACE('',#99387,61.0131030316259,0.254);
#5553=TOROIDAL_SURFACE('',#99390,60.8618969683742,0.254);
#5554=TOROIDAL_SURFACE('',#99410,60.0045305169095,0.635);
#5555=TOROIDAL_SURFACE('',#99413,61.8704694830905,0.635);
#5556=TOROIDAL_SURFACE('',#99416,61.0131030316259,0.254);
#5557=TOROIDAL_SURFACE('',#99419,60.8618969683742,0.254);
#5558=TOROIDAL_SURFACE('',#99439,60.0045305169095,0.635);
#5559=TOROIDAL_SURFACE('',#99442,61.8704694830905,0.635);
#5560=TOROIDAL_SURFACE('',#99445,61.0131030316259,0.254);
#5561=TOROIDAL_SURFACE('',#99448,60.8618969683742,0.254);
#5562=TOROIDAL_SURFACE('',#99468,60.0045305169095,0.635);
#5563=TOROIDAL_SURFACE('',#99471,61.8704694830905,0.635);
#5564=TOROIDAL_SURFACE('',#99474,61.0131030316259,0.254);
#5565=TOROIDAL_SURFACE('',#99477,60.8618969683742,0.254);
#5566=TOROIDAL_SURFACE('',#99497,60.0045305169095,0.635);
#5567=TOROIDAL_SURFACE('',#99500,61.8704694830905,0.635);
#5568=TOROIDAL_SURFACE('',#99503,61.0131030316259,0.254);
#5569=TOROIDAL_SURFACE('',#99506,60.8618969683742,0.254);
#5570=TOROIDAL_SURFACE('',#99526,60.0045305169095,0.635);
#5571=TOROIDAL_SURFACE('',#99529,61.8704694830905,0.635);
#5572=TOROIDAL_SURFACE('',#99532,61.0131030316259,0.254);
#5573=TOROIDAL_SURFACE('',#99535,60.8618969683742,0.254);
#5574=TOROIDAL_SURFACE('',#99555,60.0045305169095,0.635);
#5575=TOROIDAL_SURFACE('',#99558,61.8704694830905,0.635);
#5576=TOROIDAL_SURFACE('',#99561,61.0131030316259,0.254);
#5577=TOROIDAL_SURFACE('',#99564,60.8618969683742,0.254);
#5578=TOROIDAL_SURFACE('',#99584,60.0045305169095,0.635);
#5579=TOROIDAL_SURFACE('',#99587,61.8704694830905,0.635);
#5580=TOROIDAL_SURFACE('',#99590,61.0131030316259,0.254);
#5581=TOROIDAL_SURFACE('',#99593,60.8618969683742,0.254);
#5582=TOROIDAL_SURFACE('',#99613,60.0045305169095,0.635);
#5583=TOROIDAL_SURFACE('',#99616,61.8704694830905,0.635);
#5584=TOROIDAL_SURFACE('',#99619,61.0131030316259,0.254);
#5585=TOROIDAL_SURFACE('',#99622,60.8618969683742,0.254);
#5586=TOROIDAL_SURFACE('',#99642,60.0045305169095,0.635);
#5587=TOROIDAL_SURFACE('',#99645,61.8704694830905,0.635);
#5588=TOROIDAL_SURFACE('',#99648,61.0131030316259,0.254);
#5589=TOROIDAL_SURFACE('',#99651,60.8618969683742,0.254);
#5590=TOROIDAL_SURFACE('',#99671,60.0045305169095,0.635);
#5591=TOROIDAL_SURFACE('',#99674,61.8704694830905,0.635);
#5592=TOROIDAL_SURFACE('',#99677,61.0131030316259,0.254);
#5593=TOROIDAL_SURFACE('',#99680,60.8618969683742,0.254);
#5594=TOROIDAL_SURFACE('',#99700,60.0045305169095,0.635);
#5595=TOROIDAL_SURFACE('',#99703,61.8704694830905,0.635);
#5596=TOROIDAL_SURFACE('',#99706,61.0131030316259,0.254);
#5597=TOROIDAL_SURFACE('',#99709,60.8618969683742,0.254);
#5598=TOROIDAL_SURFACE('',#99729,60.0045305169095,0.635);
#5599=TOROIDAL_SURFACE('',#99732,61.8704694830905,0.635);
#5600=TOROIDAL_SURFACE('',#99735,61.0131030316259,0.254);
#5601=TOROIDAL_SURFACE('',#99738,60.8618969683742,0.254);
#5602=TOROIDAL_SURFACE('',#99758,60.0045305169095,0.635);
#5603=TOROIDAL_SURFACE('',#99761,61.8704694830905,0.635);
#5604=TOROIDAL_SURFACE('',#99764,61.0131030316259,0.254);
#5605=TOROIDAL_SURFACE('',#99767,60.8618969683742,0.254);
#5606=TOROIDAL_SURFACE('',#99787,60.0045305169095,0.635);
#5607=TOROIDAL_SURFACE('',#99790,61.8704694830905,0.635);
#5608=TOROIDAL_SURFACE('',#99793,61.0131030316259,0.254);
#5609=TOROIDAL_SURFACE('',#99796,60.8618969683742,0.254);
#5610=TOROIDAL_SURFACE('',#99816,60.0045305169095,0.635);
#5611=TOROIDAL_SURFACE('',#99819,61.8704694830905,0.635);
#5612=TOROIDAL_SURFACE('',#99822,61.0131030316259,0.254);
#5613=TOROIDAL_SURFACE('',#99825,60.8618969683742,0.254);
#5614=TOROIDAL_SURFACE('',#99845,60.0045305169095,0.635);
#5615=TOROIDAL_SURFACE('',#99848,61.8704694830905,0.635);
#5616=TOROIDAL_SURFACE('',#99851,61.0131030316259,0.254);
#5617=TOROIDAL_SURFACE('',#99854,60.8618969683742,0.254);
#5618=TOROIDAL_SURFACE('',#99874,60.0045305169095,0.635);
#5619=TOROIDAL_SURFACE('',#99877,61.8704694830905,0.635);
#5620=TOROIDAL_SURFACE('',#99880,61.0131030316259,0.254);
#5621=TOROIDAL_SURFACE('',#99883,60.8618969683742,0.254);
#5622=TOROIDAL_SURFACE('',#99903,60.0045305169095,0.635);
#5623=TOROIDAL_SURFACE('',#99906,61.8704694830905,0.635);
#5624=TOROIDAL_SURFACE('',#99909,61.0131030316259,0.254);
#5625=TOROIDAL_SURFACE('',#99912,60.8618969683742,0.254);
#5626=TOROIDAL_SURFACE('',#99932,60.0045305169095,0.635);
#5627=TOROIDAL_SURFACE('',#99935,61.8704694830905,0.635);
#5628=TOROIDAL_SURFACE('',#99938,61.0131030316259,0.254);
#5629=TOROIDAL_SURFACE('',#99941,60.8618969683742,0.254);
#5630=TOROIDAL_SURFACE('',#99961,60.0045305169095,0.635);
#5631=TOROIDAL_SURFACE('',#99964,61.8704694830905,0.635);
#5632=TOROIDAL_SURFACE('',#99967,61.0131030316259,0.254);
#5633=TOROIDAL_SURFACE('',#99970,60.8618969683742,0.254);
#5634=TOROIDAL_SURFACE('',#99990,60.0045305169095,0.635);
#5635=TOROIDAL_SURFACE('',#99993,61.8704694830905,0.635);
#5636=TOROIDAL_SURFACE('',#99996,61.0131030316259,0.254);
#5637=TOROIDAL_SURFACE('',#99999,60.8618969683742,0.254);
#5638=TOROIDAL_SURFACE('',#100019,60.0045305169095,0.635);
#5639=TOROIDAL_SURFACE('',#100022,61.8704694830905,0.635);
#5640=TOROIDAL_SURFACE('',#100025,61.0131030316259,0.254);
#5641=TOROIDAL_SURFACE('',#100028,60.8618969683742,0.254);
#5642=TOROIDAL_SURFACE('',#100048,60.0045305169095,0.635);
#5643=TOROIDAL_SURFACE('',#100051,61.8704694830905,0.635);
#5644=TOROIDAL_SURFACE('',#100054,61.0131030316259,0.254);
#5645=TOROIDAL_SURFACE('',#100057,60.8618969683742,0.254);
#5646=TOROIDAL_SURFACE('',#100077,60.0045305169095,0.635);
#5647=TOROIDAL_SURFACE('',#100080,61.8704694830905,0.635);
#5648=TOROIDAL_SURFACE('',#100083,61.0131030316259,0.254);
#5649=TOROIDAL_SURFACE('',#100086,60.8618969683742,0.254);
#5650=TOROIDAL_SURFACE('',#100106,60.0045305169095,0.635);
#5651=TOROIDAL_SURFACE('',#100109,61.8704694830905,0.635);
#5652=TOROIDAL_SURFACE('',#100112,61.0131030316259,0.254);
#5653=TOROIDAL_SURFACE('',#100115,60.8618969683742,0.254);
#5654=TOROIDAL_SURFACE('',#100135,60.0045305169095,0.635);
#5655=TOROIDAL_SURFACE('',#100138,61.8704694830905,0.635);
#5656=TOROIDAL_SURFACE('',#100141,61.0131030316259,0.254);
#5657=TOROIDAL_SURFACE('',#100144,60.8618969683742,0.254);
#5658=TOROIDAL_SURFACE('',#100164,60.0045305169095,0.635);
#5659=TOROIDAL_SURFACE('',#100167,61.8704694830905,0.635);
#5660=TOROIDAL_SURFACE('',#100170,61.0131030316259,0.254);
#5661=TOROIDAL_SURFACE('',#100173,60.8618969683742,0.254);
#5662=TOROIDAL_SURFACE('',#100193,60.0045305169095,0.635);
#5663=TOROIDAL_SURFACE('',#100196,61.8704694830905,0.635);
#5664=TOROIDAL_SURFACE('',#100199,61.0131030316259,0.254);
#5665=TOROIDAL_SURFACE('',#100202,60.8618969683742,0.254);
#5666=TOROIDAL_SURFACE('',#100222,60.0045305169095,0.635);
#5667=TOROIDAL_SURFACE('',#100225,61.8704694830905,0.635);
#5668=TOROIDAL_SURFACE('',#100228,61.0131030316259,0.254);
#5669=TOROIDAL_SURFACE('',#100231,60.8618969683742,0.254);
#5670=TOROIDAL_SURFACE('',#100251,60.0045305169095,0.635);
#5671=TOROIDAL_SURFACE('',#100254,61.8704694830905,0.635);
#5672=TOROIDAL_SURFACE('',#100257,61.0131030316259,0.254);
#5673=TOROIDAL_SURFACE('',#100260,60.8618969683742,0.254);
#5674=TOROIDAL_SURFACE('',#100280,60.0045305169095,0.635);
#5675=TOROIDAL_SURFACE('',#100283,61.8704694830905,0.635);
#5676=TOROIDAL_SURFACE('',#100286,61.0131030316259,0.254);
#5677=TOROIDAL_SURFACE('',#100289,60.8618969683742,0.254);
#5678=TOROIDAL_SURFACE('',#100309,60.0045305169095,0.635);
#5679=TOROIDAL_SURFACE('',#100312,61.8704694830905,0.635);
#5680=TOROIDAL_SURFACE('',#100315,61.0131030316259,0.254);
#5681=TOROIDAL_SURFACE('',#100318,60.8618969683742,0.254);
#5682=TOROIDAL_SURFACE('',#100338,60.0045305169095,0.635);
#5683=TOROIDAL_SURFACE('',#100341,61.8704694830905,0.635);
#5684=TOROIDAL_SURFACE('',#100344,61.0131030316259,0.254);
#5685=TOROIDAL_SURFACE('',#100347,60.8618969683742,0.254);
#5686=TOROIDAL_SURFACE('',#100367,60.0045305169095,0.635);
#5687=TOROIDAL_SURFACE('',#100370,61.8704694830905,0.635);
#5688=TOROIDAL_SURFACE('',#100373,61.0131030316259,0.254);
#5689=TOROIDAL_SURFACE('',#100376,60.8618969683742,0.254);
#5690=TOROIDAL_SURFACE('',#100396,60.0045305169095,0.635);
#5691=TOROIDAL_SURFACE('',#100399,61.8704694830905,0.635);
#5692=TOROIDAL_SURFACE('',#100402,61.0131030316259,0.254);
#5693=TOROIDAL_SURFACE('',#100405,60.8618969683742,0.254);
#5694=TOROIDAL_SURFACE('',#100425,60.0045305169095,0.635);
#5695=TOROIDAL_SURFACE('',#100428,61.8704694830905,0.635);
#5696=TOROIDAL_SURFACE('',#100431,61.0131030316259,0.254);
#5697=TOROIDAL_SURFACE('',#100434,60.8618969683742,0.254);
#5698=TOROIDAL_SURFACE('',#100454,60.0045305169095,0.635);
#5699=TOROIDAL_SURFACE('',#100457,61.8704694830905,0.635);
#5700=TOROIDAL_SURFACE('',#100460,61.0131030316259,0.254);
#5701=TOROIDAL_SURFACE('',#100463,60.8618969683742,0.254);
#5702=TOROIDAL_SURFACE('',#100483,60.0045305169095,0.635);
#5703=TOROIDAL_SURFACE('',#100486,61.8704694830905,0.635);
#5704=TOROIDAL_SURFACE('',#100489,61.0131030316259,0.254);
#5705=TOROIDAL_SURFACE('',#100492,60.8618969683742,0.254);
#5706=TOROIDAL_SURFACE('',#100512,60.0045305169095,0.635);
#5707=TOROIDAL_SURFACE('',#100515,61.8704694830905,0.635);
#5708=TOROIDAL_SURFACE('',#100518,61.0131030316259,0.254);
#5709=TOROIDAL_SURFACE('',#100521,60.8618969683742,0.254);
#5710=TOROIDAL_SURFACE('',#100541,60.0045305169095,0.635);
#5711=TOROIDAL_SURFACE('',#100544,61.8704694830905,0.635);
#5712=TOROIDAL_SURFACE('',#100547,61.0131030316259,0.254);
#5713=TOROIDAL_SURFACE('',#100550,60.8618969683742,0.254);
#5714=TOROIDAL_SURFACE('',#100570,60.0045305169095,0.635);
#5715=TOROIDAL_SURFACE('',#100573,61.8704694830905,0.635);
#5716=TOROIDAL_SURFACE('',#100576,61.0131030316259,0.254);
#5717=TOROIDAL_SURFACE('',#100579,60.8618969683742,0.254);
#5718=TOROIDAL_SURFACE('',#100599,60.0045305169095,0.635);
#5719=TOROIDAL_SURFACE('',#100602,61.8704694830905,0.635);
#5720=TOROIDAL_SURFACE('',#100605,61.0131030316259,0.254);
#5721=TOROIDAL_SURFACE('',#100608,60.8618969683742,0.254);
#5722=TOROIDAL_SURFACE('',#100628,60.0045305169095,0.635);
#5723=TOROIDAL_SURFACE('',#100631,61.8704694830905,0.635);
#5724=TOROIDAL_SURFACE('',#100634,61.0131030316259,0.254);
#5725=TOROIDAL_SURFACE('',#100637,60.8618969683742,0.254);
#5726=TOROIDAL_SURFACE('',#100657,60.0045305169095,0.635);
#5727=TOROIDAL_SURFACE('',#100660,61.8704694830905,0.635);
#5728=TOROIDAL_SURFACE('',#100663,61.0131030316259,0.254);
#5729=TOROIDAL_SURFACE('',#100666,60.8618969683742,0.254);
#5730=TOROIDAL_SURFACE('',#100686,60.0045305169095,0.635);
#5731=TOROIDAL_SURFACE('',#100689,61.8704694830905,0.635);
#5732=TOROIDAL_SURFACE('',#100692,61.0131030316259,0.254);
#5733=TOROIDAL_SURFACE('',#100695,60.8618969683742,0.254);
#5734=TOROIDAL_SURFACE('',#100715,60.0045305169095,0.635);
#5735=TOROIDAL_SURFACE('',#100718,61.8704694830905,0.635);
#5736=TOROIDAL_SURFACE('',#100721,61.0131030316259,0.254);
#5737=TOROIDAL_SURFACE('',#100724,60.8618969683742,0.254);
#5738=TOROIDAL_SURFACE('',#100744,60.0045305169095,0.635);
#5739=TOROIDAL_SURFACE('',#100747,61.8704694830905,0.635);
#5740=TOROIDAL_SURFACE('',#100750,61.0131030316259,0.254);
#5741=TOROIDAL_SURFACE('',#100753,60.8618969683742,0.254);
#5742=TOROIDAL_SURFACE('',#100773,60.0045305169095,0.635);
#5743=TOROIDAL_SURFACE('',#100776,61.8704694830905,0.635);
#5744=TOROIDAL_SURFACE('',#100779,61.0131030316259,0.254);
#5745=TOROIDAL_SURFACE('',#100782,60.8618969683742,0.254);
#5746=TOROIDAL_SURFACE('',#100802,60.0045305169095,0.635);
#5747=TOROIDAL_SURFACE('',#100805,61.8704694830905,0.635);
#5748=TOROIDAL_SURFACE('',#100808,61.0131030316259,0.254);
#5749=TOROIDAL_SURFACE('',#100811,60.8618969683742,0.254);
#5750=TOROIDAL_SURFACE('',#100831,60.0045305169095,0.635);
#5751=TOROIDAL_SURFACE('',#100834,61.8704694830905,0.635);
#5752=TOROIDAL_SURFACE('',#100837,61.0131030316259,0.254);
#5753=TOROIDAL_SURFACE('',#100840,60.8618969683742,0.254);
#5754=TOROIDAL_SURFACE('',#100860,60.0045305169095,0.635);
#5755=TOROIDAL_SURFACE('',#100863,61.8704694830905,0.635);
#5756=TOROIDAL_SURFACE('',#100866,61.0131030316259,0.254);
#5757=TOROIDAL_SURFACE('',#100869,60.8618969683742,0.254);
#5758=TOROIDAL_SURFACE('',#100889,60.0045305169095,0.635);
#5759=TOROIDAL_SURFACE('',#100892,61.8704694830905,0.635);
#5760=TOROIDAL_SURFACE('',#100895,61.0131030316259,0.254);
#5761=TOROIDAL_SURFACE('',#100898,60.8618969683742,0.254);
#5762=TOROIDAL_SURFACE('',#100918,60.0045305169095,0.635);
#5763=TOROIDAL_SURFACE('',#100921,61.8704694830905,0.635);
#5764=TOROIDAL_SURFACE('',#100924,61.0131030316259,0.254);
#5765=TOROIDAL_SURFACE('',#100927,60.8618969683742,0.254);
#5766=TOROIDAL_SURFACE('',#100947,60.0045305169095,0.635);
#5767=TOROIDAL_SURFACE('',#100950,61.8704694830905,0.635);
#5768=TOROIDAL_SURFACE('',#100953,61.0131030316259,0.254);
#5769=TOROIDAL_SURFACE('',#100956,60.8618969683742,0.254);
#5770=TOROIDAL_SURFACE('',#100976,60.0045305169095,0.635);
#5771=TOROIDAL_SURFACE('',#100979,61.8704694830905,0.635);
#5772=TOROIDAL_SURFACE('',#100982,61.0131030316259,0.254);
#5773=TOROIDAL_SURFACE('',#100985,60.8618969683742,0.254);
#5774=TOROIDAL_SURFACE('',#101005,60.0045305169095,0.635);
#5775=TOROIDAL_SURFACE('',#101008,61.8704694830905,0.635);
#5776=TOROIDAL_SURFACE('',#101011,61.0131030316259,0.254);
#5777=TOROIDAL_SURFACE('',#101014,60.8618969683742,0.254);
#5778=TOROIDAL_SURFACE('',#101034,60.0045305169095,0.635);
#5779=TOROIDAL_SURFACE('',#101037,61.8704694830905,0.635);
#5780=TOROIDAL_SURFACE('',#101040,61.0131030316259,0.254);
#5781=TOROIDAL_SURFACE('',#101043,60.8618969683742,0.254);
#5782=TOROIDAL_SURFACE('',#101063,60.0045305169095,0.635);
#5783=TOROIDAL_SURFACE('',#101066,61.8704694830905,0.635);
#5784=TOROIDAL_SURFACE('',#101069,61.0131030316259,0.254);
#5785=TOROIDAL_SURFACE('',#101072,60.8618969683742,0.254);
#5786=TOROIDAL_SURFACE('',#101095,60.0045305169095,0.635);
#5787=TOROIDAL_SURFACE('',#101098,61.8704694830905,0.635);
#5788=TOROIDAL_SURFACE('',#101101,61.0131030316259,0.254);
#5789=TOROIDAL_SURFACE('',#101104,60.8618969683742,0.254);
#5790=TOROIDAL_SURFACE('',#101139,62.8464445485378,0.127);
#5791=TOROIDAL_SURFACE('',#101149,59.0285554514622,0.127);
#5792=TOROIDAL_SURFACE('',#102064,62.8464445485378,0.127);
#5793=TOROIDAL_SURFACE('',#102074,59.0285554514622,0.127);
#5794=TOROIDAL_SURFACE('',#102108,62.8464445485378,0.127);
#5795=TOROIDAL_SURFACE('',#102118,59.0285554514622,0.127);
#5796=TOROIDAL_SURFACE('',#102152,62.8464445485378,0.127);
#5797=TOROIDAL_SURFACE('',#102162,59.0285554514622,0.127);
#5798=TOROIDAL_SURFACE('',#102196,62.8464445485378,0.127);
#5799=TOROIDAL_SURFACE('',#102206,59.0285554514622,0.127);
#5800=TOROIDAL_SURFACE('',#102240,62.8464445485378,0.127);
#5801=TOROIDAL_SURFACE('',#102250,59.0285554514622,0.127);
#5802=TOROIDAL_SURFACE('',#102284,62.8464445485378,0.127);
#5803=TOROIDAL_SURFACE('',#102294,59.0285554514622,0.127);
#5804=TOROIDAL_SURFACE('',#102328,62.8464445485378,0.127);
#5805=TOROIDAL_SURFACE('',#102338,59.0285554514622,0.127);
#5806=TOROIDAL_SURFACE('',#102372,62.8464445485378,0.127);
#5807=TOROIDAL_SURFACE('',#102382,59.0285554514622,0.127);
#5808=TOROIDAL_SURFACE('',#102416,62.8464445485378,0.127);
#5809=TOROIDAL_SURFACE('',#102426,59.0285554514622,0.127);
#5810=TOROIDAL_SURFACE('',#102460,62.8464445485378,0.127);
#5811=TOROIDAL_SURFACE('',#102470,59.0285554514622,0.127);
#5812=TOROIDAL_SURFACE('',#102504,62.8464445485378,0.127);
#5813=TOROIDAL_SURFACE('',#102514,59.0285554514622,0.127);
#5814=TOROIDAL_SURFACE('',#102548,62.8464445485378,0.127);
#5815=TOROIDAL_SURFACE('',#102558,59.0285554514622,0.127);
#5816=TOROIDAL_SURFACE('',#102592,62.8464445485378,0.127);
#5817=TOROIDAL_SURFACE('',#102602,59.0285554514622,0.127);
#5818=TOROIDAL_SURFACE('',#102636,62.8464445485378,0.127);
#5819=TOROIDAL_SURFACE('',#102646,59.0285554514622,0.127);
#5820=TOROIDAL_SURFACE('',#102680,62.8464445485378,0.127);
#5821=TOROIDAL_SURFACE('',#102690,59.0285554514622,0.127);
#5822=TOROIDAL_SURFACE('',#102724,62.8464445485378,0.127);
#5823=TOROIDAL_SURFACE('',#102734,59.0285554514622,0.127);
#5824=TOROIDAL_SURFACE('',#102768,62.8464445485378,0.127);
#5825=TOROIDAL_SURFACE('',#102778,59.0285554514622,0.127);
#5826=TOROIDAL_SURFACE('',#102812,62.8464445485378,0.127);
#5827=TOROIDAL_SURFACE('',#102822,59.0285554514622,0.127);
#5828=TOROIDAL_SURFACE('',#102856,62.8464445485378,0.127);
#5829=TOROIDAL_SURFACE('',#102866,59.0285554514622,0.127);
#5830=TOROIDAL_SURFACE('',#102900,62.8464445485378,0.127);
#5831=TOROIDAL_SURFACE('',#102910,59.0285554514622,0.127);
#5832=TOROIDAL_SURFACE('',#102944,62.8464445485378,0.127);
#5833=TOROIDAL_SURFACE('',#102954,59.0285554514622,0.127);
#5834=TOROIDAL_SURFACE('',#102988,62.8464445485378,0.127);
#5835=TOROIDAL_SURFACE('',#102998,59.0285554514622,0.127);
#5836=TOROIDAL_SURFACE('',#103032,62.8464445485378,0.127);
#5837=TOROIDAL_SURFACE('',#103042,59.0285554514622,0.127);
#5838=TOROIDAL_SURFACE('',#103076,62.8464445485378,0.127);
#5839=TOROIDAL_SURFACE('',#103086,59.0285554514622,0.127);
#5840=TOROIDAL_SURFACE('',#103120,62.8464445485378,0.127);
#5841=TOROIDAL_SURFACE('',#103130,59.0285554514622,0.127);
#5842=TOROIDAL_SURFACE('',#103164,62.8464445485378,0.127);
#5843=TOROIDAL_SURFACE('',#103174,59.0285554514622,0.127);
#5844=TOROIDAL_SURFACE('',#103208,62.8464445485378,0.127);
#5845=TOROIDAL_SURFACE('',#103218,59.0285554514622,0.127);
#5846=TOROIDAL_SURFACE('',#103252,62.8464445485378,0.127);
#5847=TOROIDAL_SURFACE('',#103262,59.0285554514622,0.127);
#5848=TOROIDAL_SURFACE('',#103296,62.8464445485378,0.127);
#5849=TOROIDAL_SURFACE('',#103306,59.0285554514622,0.127);
#5850=TOROIDAL_SURFACE('',#103378,62.8464445485378,0.127);
#5851=TOROIDAL_SURFACE('',#103388,59.0285554514622,0.127);
#5852=TOROIDAL_SURFACE('',#103422,62.8464445485378,0.127);
#5853=TOROIDAL_SURFACE('',#103432,59.0285554514622,0.127);
#5854=TOROIDAL_SURFACE('',#103466,62.8464445485378,0.127);
#5855=TOROIDAL_SURFACE('',#103476,59.0285554514622,0.127);
#5856=TOROIDAL_SURFACE('',#103510,62.8464445485378,0.127);
#5857=TOROIDAL_SURFACE('',#103520,59.0285554514622,0.127);
#5858=TOROIDAL_SURFACE('',#103554,62.8464445485378,0.127);
#5859=TOROIDAL_SURFACE('',#103564,59.0285554514622,0.127);
#5860=TOROIDAL_SURFACE('',#103598,62.8464445485378,0.127);
#5861=TOROIDAL_SURFACE('',#103608,59.0285554514622,0.127);
#5862=TOROIDAL_SURFACE('',#103642,62.8464445485378,0.127);
#5863=TOROIDAL_SURFACE('',#103652,59.0285554514622,0.127);
#5864=TOROIDAL_SURFACE('',#103686,62.8464445485378,0.127);
#5865=TOROIDAL_SURFACE('',#103696,59.0285554514622,0.127);
#5866=TOROIDAL_SURFACE('',#103730,62.8464445485378,0.127);
#5867=TOROIDAL_SURFACE('',#103740,59.0285554514622,0.127);
#5868=TOROIDAL_SURFACE('',#103774,62.8464445485378,0.127);
#5869=TOROIDAL_SURFACE('',#103784,59.0285554514622,0.127);
#5870=TOROIDAL_SURFACE('',#103818,62.8464445485378,0.127);
#5871=TOROIDAL_SURFACE('',#103828,59.0285554514622,0.127);
#5872=TOROIDAL_SURFACE('',#103862,62.8464445485378,0.127);
#5873=TOROIDAL_SURFACE('',#103872,59.0285554514622,0.127);
#5874=TOROIDAL_SURFACE('',#103906,62.8464445485378,0.127);
#5875=TOROIDAL_SURFACE('',#103916,59.0285554514622,0.127);
#5876=TOROIDAL_SURFACE('',#103950,62.8464445485378,0.127);
#5877=TOROIDAL_SURFACE('',#103960,59.0285554514622,0.127);
#5878=TOROIDAL_SURFACE('',#104032,62.8464445485378,0.127);
#5879=TOROIDAL_SURFACE('',#104042,59.0285554514622,0.127);
#5880=TOROIDAL_SURFACE('',#104076,62.8464445485378,0.127);
#5881=TOROIDAL_SURFACE('',#104086,59.0285554514622,0.127);
#5882=TOROIDAL_SURFACE('',#104120,62.8464445485378,0.127);
#5883=TOROIDAL_SURFACE('',#104130,59.0285554514622,0.127);
#5884=TOROIDAL_SURFACE('',#104164,62.8464445485378,0.127);
#5885=TOROIDAL_SURFACE('',#104174,59.0285554514622,0.127);
#5886=TOROIDAL_SURFACE('',#104208,62.8464445485378,0.127);
#5887=TOROIDAL_SURFACE('',#104218,59.0285554514622,0.127);
#5888=TOROIDAL_SURFACE('',#104252,62.8464445485378,0.127);
#5889=TOROIDAL_SURFACE('',#104262,59.0285554514622,0.127);
#5890=TOROIDAL_SURFACE('',#104296,62.8464445485378,0.127);
#5891=TOROIDAL_SURFACE('',#104306,59.0285554514622,0.127);
#5892=TOROIDAL_SURFACE('',#104340,62.8464445485378,0.127);
#5893=TOROIDAL_SURFACE('',#104350,59.0285554514622,0.127);
#5894=TOROIDAL_SURFACE('',#104384,62.8464445485378,0.127);
#5895=TOROIDAL_SURFACE('',#104394,59.0285554514622,0.127);
#5896=TOROIDAL_SURFACE('',#104428,62.8464445485378,0.127);
#5897=TOROIDAL_SURFACE('',#104438,59.0285554514622,0.127);
#5898=TOROIDAL_SURFACE('',#104472,62.8464445485378,0.127);
#5899=TOROIDAL_SURFACE('',#104482,59.0285554514622,0.127);
#5900=TOROIDAL_SURFACE('',#104516,62.8464445485378,0.127);
#5901=TOROIDAL_SURFACE('',#104526,59.0285554514622,0.127);
#5902=TOROIDAL_SURFACE('',#104560,62.8464445485378,0.127);
#5903=TOROIDAL_SURFACE('',#104570,59.0285554514622,0.127);
#5904=TOROIDAL_SURFACE('',#104604,62.8464445485378,0.127);
#5905=TOROIDAL_SURFACE('',#104614,59.0285554514622,0.127);
#5906=TOROIDAL_SURFACE('',#104631,59.0285554514622,0.127);
#5907=TOROIDAL_SURFACE('',#104636,62.8464445485378,0.127);
#5908=TOROIDAL_SURFACE('',#104641,59.0285554514622,0.127);
#5909=TOROIDAL_SURFACE('',#104646,62.8464445485378,0.127);
#5910=TOROIDAL_SURFACE('',#104652,58.2189663438286,0.635);
#5911=TOROIDAL_SURFACE('',#104657,58.3085779254084,0.635);
#5912=TOROIDAL_SURFACE('',#104661,63.5664220745916,0.635);
#5913=TOROIDAL_SURFACE('',#104666,63.6560336561714,0.635);
#5914=TOROIDAL_SURFACE('',#104935,60.0045305169095,0.635);
#5915=TOROIDAL_SURFACE('',#104938,61.8704694830905,0.635);
#5916=TOROIDAL_SURFACE('',#104941,61.0131030316259,0.254);
#5917=TOROIDAL_SURFACE('',#104944,60.8618969683742,0.254);
#5918=TOROIDAL_SURFACE('',#104964,60.0045305169095,0.635);
#5919=TOROIDAL_SURFACE('',#104967,61.8704694830905,0.635);
#5920=TOROIDAL_SURFACE('',#104970,61.0131030316259,0.254);
#5921=TOROIDAL_SURFACE('',#104973,60.8618969683742,0.254);
#5922=TOROIDAL_SURFACE('',#104993,60.0045305169095,0.635);
#5923=TOROIDAL_SURFACE('',#104996,61.8704694830905,0.635);
#5924=TOROIDAL_SURFACE('',#104999,61.0131030316259,0.254);
#5925=TOROIDAL_SURFACE('',#105002,60.8618969683742,0.254);
#5926=TOROIDAL_SURFACE('',#105022,60.0045305169095,0.635);
#5927=TOROIDAL_SURFACE('',#105025,61.8704694830905,0.635);
#5928=TOROIDAL_SURFACE('',#105028,61.0131030316259,0.254);
#5929=TOROIDAL_SURFACE('',#105031,60.8618969683742,0.254);
#5930=TOROIDAL_SURFACE('',#105051,60.0045305169095,0.635);
#5931=TOROIDAL_SURFACE('',#105054,61.8704694830905,0.635);
#5932=TOROIDAL_SURFACE('',#105057,61.0131030316259,0.254);
#5933=TOROIDAL_SURFACE('',#105060,60.8618969683742,0.254);
#5934=TOROIDAL_SURFACE('',#105080,60.0045305169095,0.635);
#5935=TOROIDAL_SURFACE('',#105083,61.8704694830905,0.635);
#5936=TOROIDAL_SURFACE('',#105086,61.0131030316259,0.254);
#5937=TOROIDAL_SURFACE('',#105089,60.8618969683742,0.254);
#5938=TOROIDAL_SURFACE('',#105109,60.0045305169095,0.635);
#5939=TOROIDAL_SURFACE('',#105112,61.8704694830905,0.635);
#5940=TOROIDAL_SURFACE('',#105115,61.0131030316259,0.254);
#5941=TOROIDAL_SURFACE('',#105118,60.8618969683742,0.254);
#5942=TOROIDAL_SURFACE('',#105138,60.0045305169095,0.635);
#5943=TOROIDAL_SURFACE('',#105141,61.8704694830905,0.635);
#5944=TOROIDAL_SURFACE('',#105144,61.0131030316259,0.254);
#5945=TOROIDAL_SURFACE('',#105147,60.8618969683742,0.254);
#5946=TOROIDAL_SURFACE('',#105167,60.0045305169095,0.635);
#5947=TOROIDAL_SURFACE('',#105170,61.8704694830905,0.635);
#5948=TOROIDAL_SURFACE('',#105173,61.0131030316259,0.254);
#5949=TOROIDAL_SURFACE('',#105176,60.8618969683742,0.254);
#5950=TOROIDAL_SURFACE('',#105196,60.0045305169095,0.635);
#5951=TOROIDAL_SURFACE('',#105199,61.8704694830905,0.635);
#5952=TOROIDAL_SURFACE('',#105202,61.0131030316259,0.254);
#5953=TOROIDAL_SURFACE('',#105205,60.8618969683742,0.254);
#5954=TOROIDAL_SURFACE('',#105225,60.0045305169095,0.635);
#5955=TOROIDAL_SURFACE('',#105228,61.8704694830905,0.635);
#5956=TOROIDAL_SURFACE('',#105231,61.0131030316259,0.254);
#5957=TOROIDAL_SURFACE('',#105234,60.8618969683742,0.254);
#5958=TOROIDAL_SURFACE('',#105254,60.0045305169095,0.635);
#5959=TOROIDAL_SURFACE('',#105257,61.8704694830905,0.635);
#5960=TOROIDAL_SURFACE('',#105260,61.0131030316259,0.254);
#5961=TOROIDAL_SURFACE('',#105263,60.8618969683742,0.254);
#5962=TOROIDAL_SURFACE('',#105283,60.0045305169095,0.635);
#5963=TOROIDAL_SURFACE('',#105286,61.8704694830905,0.635);
#5964=TOROIDAL_SURFACE('',#105289,61.0131030316259,0.254);
#5965=TOROIDAL_SURFACE('',#105292,60.8618969683742,0.254);
#5966=TOROIDAL_SURFACE('',#105312,60.0045305169095,0.635);
#5967=TOROIDAL_SURFACE('',#105315,61.8704694830905,0.635);
#5968=TOROIDAL_SURFACE('',#105318,61.0131030316259,0.254);
#5969=TOROIDAL_SURFACE('',#105321,60.8618969683742,0.254);
#5970=TOROIDAL_SURFACE('',#105341,60.0045305169095,0.635);
#5971=TOROIDAL_SURFACE('',#105344,61.8704694830905,0.635);
#5972=TOROIDAL_SURFACE('',#105347,61.0131030316259,0.254);
#5973=TOROIDAL_SURFACE('',#105350,60.8618969683742,0.254);
#5974=TOROIDAL_SURFACE('',#105370,60.0045305169095,0.635);
#5975=TOROIDAL_SURFACE('',#105373,61.8704694830905,0.635);
#5976=TOROIDAL_SURFACE('',#105376,61.0131030316259,0.254);
#5977=TOROIDAL_SURFACE('',#105379,60.8618969683742,0.254);
#5978=TOROIDAL_SURFACE('',#105399,60.0045305169095,0.635);
#5979=TOROIDAL_SURFACE('',#105402,61.8704694830905,0.635);
#5980=TOROIDAL_SURFACE('',#105405,61.0131030316259,0.254);
#5981=TOROIDAL_SURFACE('',#105408,60.8618969683742,0.254);
#5982=TOROIDAL_SURFACE('',#105428,60.0045305169095,0.635);
#5983=TOROIDAL_SURFACE('',#105431,61.8704694830905,0.635);
#5984=TOROIDAL_SURFACE('',#105434,61.0131030316259,0.254);
#5985=TOROIDAL_SURFACE('',#105437,60.8618969683742,0.254);
#5986=TOROIDAL_SURFACE('',#105457,60.0045305169095,0.635);
#5987=TOROIDAL_SURFACE('',#105460,61.8704694830905,0.635);
#5988=TOROIDAL_SURFACE('',#105463,61.0131030316259,0.254);
#5989=TOROIDAL_SURFACE('',#105466,60.8618969683742,0.254);
#5990=TOROIDAL_SURFACE('',#105486,60.0045305169095,0.635);
#5991=TOROIDAL_SURFACE('',#105489,61.8704694830905,0.635);
#5992=TOROIDAL_SURFACE('',#105492,61.0131030316259,0.254);
#5993=TOROIDAL_SURFACE('',#105495,60.8618969683742,0.254);
#5994=TOROIDAL_SURFACE('',#105515,60.0045305169095,0.635);
#5995=TOROIDAL_SURFACE('',#105518,61.8704694830905,0.635);
#5996=TOROIDAL_SURFACE('',#105521,61.0131030316259,0.254);
#5997=TOROIDAL_SURFACE('',#105524,60.8618969683742,0.254);
#5998=TOROIDAL_SURFACE('',#105544,60.0045305169095,0.635);
#5999=TOROIDAL_SURFACE('',#105547,61.8704694830905,0.635);
#6000=TOROIDAL_SURFACE('',#105550,61.0131030316259,0.254);
#6001=TOROIDAL_SURFACE('',#105553,60.8618969683742,0.254);
#6002=TOROIDAL_SURFACE('',#105573,60.0045305169095,0.635);
#6003=TOROIDAL_SURFACE('',#105576,61.8704694830905,0.635);
#6004=TOROIDAL_SURFACE('',#105579,61.0131030316259,0.254);
#6005=TOROIDAL_SURFACE('',#105582,60.8618969683742,0.254);
#6006=TOROIDAL_SURFACE('',#105602,60.0045305169095,0.635);
#6007=TOROIDAL_SURFACE('',#105605,61.8704694830905,0.635);
#6008=TOROIDAL_SURFACE('',#105608,61.0131030316259,0.254);
#6009=TOROIDAL_SURFACE('',#105611,60.8618969683742,0.254);
#6010=TOROIDAL_SURFACE('',#105631,60.0045305169095,0.635);
#6011=TOROIDAL_SURFACE('',#105634,61.8704694830905,0.635);
#6012=TOROIDAL_SURFACE('',#105637,61.0131030316259,0.254);
#6013=TOROIDAL_SURFACE('',#105640,60.8618969683742,0.254);
#6014=TOROIDAL_SURFACE('',#105660,60.0045305169095,0.635);
#6015=TOROIDAL_SURFACE('',#105663,61.8704694830905,0.635);
#6016=TOROIDAL_SURFACE('',#105666,61.0131030316259,0.254);
#6017=TOROIDAL_SURFACE('',#105669,60.8618969683742,0.254);
#6018=TOROIDAL_SURFACE('',#105689,60.0045305169095,0.635);
#6019=TOROIDAL_SURFACE('',#105692,61.8704694830905,0.635);
#6020=TOROIDAL_SURFACE('',#105695,61.0131030316259,0.254);
#6021=TOROIDAL_SURFACE('',#105698,60.8618969683742,0.254);
#6022=TOROIDAL_SURFACE('',#105718,60.0045305169095,0.635);
#6023=TOROIDAL_SURFACE('',#105721,61.8704694830905,0.635);
#6024=TOROIDAL_SURFACE('',#105724,61.0131030316259,0.254);
#6025=TOROIDAL_SURFACE('',#105727,60.8618969683742,0.254);
#6026=TOROIDAL_SURFACE('',#105747,60.0045305169095,0.635);
#6027=TOROIDAL_SURFACE('',#105750,61.8704694830905,0.635);
#6028=TOROIDAL_SURFACE('',#105753,61.0131030316259,0.254);
#6029=TOROIDAL_SURFACE('',#105756,60.8618969683742,0.254);
#6030=TOROIDAL_SURFACE('',#105776,60.0045305169095,0.635);
#6031=TOROIDAL_SURFACE('',#105779,61.8704694830905,0.635);
#6032=TOROIDAL_SURFACE('',#105782,61.0131030316259,0.254);
#6033=TOROIDAL_SURFACE('',#105785,60.8618969683742,0.254);
#6034=TOROIDAL_SURFACE('',#105805,60.0045305169095,0.635);
#6035=TOROIDAL_SURFACE('',#105808,61.8704694830905,0.635);
#6036=TOROIDAL_SURFACE('',#105811,61.0131030316259,0.254);
#6037=TOROIDAL_SURFACE('',#105814,60.8618969683742,0.254);
#6038=TOROIDAL_SURFACE('',#105834,60.0045305169095,0.635);
#6039=TOROIDAL_SURFACE('',#105837,61.8704694830905,0.635);
#6040=TOROIDAL_SURFACE('',#105840,61.0131030316259,0.254);
#6041=TOROIDAL_SURFACE('',#105843,60.8618969683742,0.254);
#6042=TOROIDAL_SURFACE('',#105863,60.0045305169095,0.635);
#6043=TOROIDAL_SURFACE('',#105866,61.8704694830905,0.635);
#6044=TOROIDAL_SURFACE('',#105869,61.0131030316259,0.254);
#6045=TOROIDAL_SURFACE('',#105872,60.8618969683742,0.254);
#6046=TOROIDAL_SURFACE('',#105892,60.0045305169095,0.635);
#6047=TOROIDAL_SURFACE('',#105895,61.8704694830905,0.635);
#6048=TOROIDAL_SURFACE('',#105898,61.0131030316259,0.254);
#6049=TOROIDAL_SURFACE('',#105901,60.8618969683742,0.254);
#6050=TOROIDAL_SURFACE('',#105921,60.0045305169095,0.635);
#6051=TOROIDAL_SURFACE('',#105924,61.8704694830905,0.635);
#6052=TOROIDAL_SURFACE('',#105927,61.0131030316259,0.254);
#6053=TOROIDAL_SURFACE('',#105930,60.8618969683742,0.254);
#6054=TOROIDAL_SURFACE('',#105950,60.0045305169095,0.635);
#6055=TOROIDAL_SURFACE('',#105953,61.8704694830905,0.635);
#6056=TOROIDAL_SURFACE('',#105956,61.0131030316259,0.254);
#6057=TOROIDAL_SURFACE('',#105959,60.8618969683742,0.254);
#6058=TOROIDAL_SURFACE('',#105979,60.0045305169095,0.635);
#6059=TOROIDAL_SURFACE('',#105982,61.8704694830905,0.635);
#6060=TOROIDAL_SURFACE('',#105985,61.0131030316259,0.254);
#6061=TOROIDAL_SURFACE('',#105988,60.8618969683742,0.254);
#6062=TOROIDAL_SURFACE('',#106008,60.0045305169095,0.635);
#6063=TOROIDAL_SURFACE('',#106011,61.8704694830905,0.635);
#6064=TOROIDAL_SURFACE('',#106014,61.0131030316259,0.254);
#6065=TOROIDAL_SURFACE('',#106017,60.8618969683742,0.254);
#6066=TOROIDAL_SURFACE('',#106037,60.0045305169095,0.635);
#6067=TOROIDAL_SURFACE('',#106040,61.8704694830905,0.635);
#6068=TOROIDAL_SURFACE('',#106043,61.0131030316259,0.254);
#6069=TOROIDAL_SURFACE('',#106046,60.8618969683742,0.254);
#6070=TOROIDAL_SURFACE('',#106066,60.0045305169095,0.635);
#6071=TOROIDAL_SURFACE('',#106069,61.8704694830905,0.635);
#6072=TOROIDAL_SURFACE('',#106072,61.0131030316259,0.254);
#6073=TOROIDAL_SURFACE('',#106075,60.8618969683742,0.254);
#6074=TOROIDAL_SURFACE('',#106095,60.0045305169095,0.635);
#6075=TOROIDAL_SURFACE('',#106098,61.8704694830905,0.635);
#6076=TOROIDAL_SURFACE('',#106101,61.0131030316259,0.254);
#6077=TOROIDAL_SURFACE('',#106104,60.8618969683742,0.254);
#6078=TOROIDAL_SURFACE('',#106124,60.0045305169095,0.635);
#6079=TOROIDAL_SURFACE('',#106127,61.8704694830905,0.635);
#6080=TOROIDAL_SURFACE('',#106130,61.0131030316259,0.254);
#6081=TOROIDAL_SURFACE('',#106133,60.8618969683742,0.254);
#6082=TOROIDAL_SURFACE('',#106153,60.0045305169095,0.635);
#6083=TOROIDAL_SURFACE('',#106156,61.8704694830905,0.635);
#6084=TOROIDAL_SURFACE('',#106159,61.0131030316259,0.254);
#6085=TOROIDAL_SURFACE('',#106162,60.8618969683742,0.254);
#6086=TOROIDAL_SURFACE('',#106182,60.0045305169095,0.635);
#6087=TOROIDAL_SURFACE('',#106185,61.8704694830905,0.635);
#6088=TOROIDAL_SURFACE('',#106188,61.0131030316259,0.254);
#6089=TOROIDAL_SURFACE('',#106191,60.8618969683742,0.254);
#6090=TOROIDAL_SURFACE('',#106211,60.0045305169095,0.635);
#6091=TOROIDAL_SURFACE('',#106214,61.8704694830905,0.635);
#6092=TOROIDAL_SURFACE('',#106217,61.0131030316259,0.254);
#6093=TOROIDAL_SURFACE('',#106220,60.8618969683742,0.254);
#6094=TOROIDAL_SURFACE('',#106240,60.0045305169095,0.635);
#6095=TOROIDAL_SURFACE('',#106243,61.8704694830905,0.635);
#6096=TOROIDAL_SURFACE('',#106246,61.0131030316259,0.254);
#6097=TOROIDAL_SURFACE('',#106249,60.8618969683742,0.254);
#6098=TOROIDAL_SURFACE('',#106269,60.0045305169095,0.635);
#6099=TOROIDAL_SURFACE('',#106272,61.8704694830905,0.635);
#6100=TOROIDAL_SURFACE('',#106275,61.0131030316259,0.254);
#6101=TOROIDAL_SURFACE('',#106278,60.8618969683742,0.254);
#6102=TOROIDAL_SURFACE('',#106298,60.0045305169095,0.635);
#6103=TOROIDAL_SURFACE('',#106301,61.8704694830905,0.635);
#6104=TOROIDAL_SURFACE('',#106304,61.0131030316259,0.254);
#6105=TOROIDAL_SURFACE('',#106307,60.8618969683742,0.254);
#6106=TOROIDAL_SURFACE('',#106327,60.0045305169095,0.635);
#6107=TOROIDAL_SURFACE('',#106330,61.8704694830905,0.635);
#6108=TOROIDAL_SURFACE('',#106333,61.0131030316259,0.254);
#6109=TOROIDAL_SURFACE('',#106336,60.8618969683742,0.254);
#6110=TOROIDAL_SURFACE('',#106356,60.0045305169095,0.635);
#6111=TOROIDAL_SURFACE('',#106359,61.8704694830905,0.635);
#6112=TOROIDAL_SURFACE('',#106362,61.0131030316259,0.254);
#6113=TOROIDAL_SURFACE('',#106365,60.8618969683742,0.254);
#6114=TOROIDAL_SURFACE('',#106385,60.0045305169095,0.635);
#6115=TOROIDAL_SURFACE('',#106388,61.8704694830905,0.635);
#6116=TOROIDAL_SURFACE('',#106391,61.0131030316259,0.254);
#6117=TOROIDAL_SURFACE('',#106394,60.8618969683742,0.254);
#6118=TOROIDAL_SURFACE('',#106414,60.0045305169095,0.635);
#6119=TOROIDAL_SURFACE('',#106417,61.8704694830905,0.635);
#6120=TOROIDAL_SURFACE('',#106420,61.0131030316259,0.254);
#6121=TOROIDAL_SURFACE('',#106423,60.8618969683742,0.254);
#6122=TOROIDAL_SURFACE('',#106443,60.0045305169095,0.635);
#6123=TOROIDAL_SURFACE('',#106446,61.8704694830905,0.635);
#6124=TOROIDAL_SURFACE('',#106449,61.0131030316259,0.254);
#6125=TOROIDAL_SURFACE('',#106452,60.8618969683742,0.254);
#6126=TOROIDAL_SURFACE('',#106472,60.0045305169095,0.635);
#6127=TOROIDAL_SURFACE('',#106475,61.8704694830905,0.635);
#6128=TOROIDAL_SURFACE('',#106478,61.0131030316259,0.254);
#6129=TOROIDAL_SURFACE('',#106481,60.8618969683742,0.254);
#6130=TOROIDAL_SURFACE('',#106501,60.0045305169095,0.635);
#6131=TOROIDAL_SURFACE('',#106504,61.8704694830905,0.635);
#6132=TOROIDAL_SURFACE('',#106507,61.0131030316259,0.254);
#6133=TOROIDAL_SURFACE('',#106510,60.8618969683742,0.254);
#6134=TOROIDAL_SURFACE('',#106530,60.0045305169095,0.635);
#6135=TOROIDAL_SURFACE('',#106533,61.8704694830905,0.635);
#6136=TOROIDAL_SURFACE('',#106536,61.0131030316259,0.254);
#6137=TOROIDAL_SURFACE('',#106539,60.8618969683742,0.254);
#6138=TOROIDAL_SURFACE('',#106559,60.0045305169095,0.635);
#6139=TOROIDAL_SURFACE('',#106562,61.8704694830905,0.635);
#6140=TOROIDAL_SURFACE('',#106565,61.0131030316259,0.254);
#6141=TOROIDAL_SURFACE('',#106568,60.8618969683742,0.254);
#6142=TOROIDAL_SURFACE('',#106588,60.0045305169095,0.635);
#6143=TOROIDAL_SURFACE('',#106591,61.8704694830905,0.635);
#6144=TOROIDAL_SURFACE('',#106594,61.0131030316259,0.254);
#6145=TOROIDAL_SURFACE('',#106597,60.8618969683742,0.254);
#6146=TOROIDAL_SURFACE('',#106617,60.0045305169095,0.635);
#6147=TOROIDAL_SURFACE('',#106620,61.8704694830905,0.635);
#6148=TOROIDAL_SURFACE('',#106623,61.0131030316259,0.254);
#6149=TOROIDAL_SURFACE('',#106626,60.8618969683742,0.254);
#6150=TOROIDAL_SURFACE('',#106649,60.0045305169095,0.635);
#6151=TOROIDAL_SURFACE('',#106652,61.8704694830905,0.635);
#6152=TOROIDAL_SURFACE('',#106655,61.0131030316259,0.254);
#6153=TOROIDAL_SURFACE('',#106658,60.8618969683742,0.254);
#6154=TOROIDAL_SURFACE('',#106693,62.8464445485378,0.127);
#6155=TOROIDAL_SURFACE('',#106703,59.0285554514622,0.127);
#6156=TOROIDAL_SURFACE('',#107618,62.8464445485378,0.127);
#6157=TOROIDAL_SURFACE('',#107628,59.0285554514622,0.127);
#6158=TOROIDAL_SURFACE('',#107662,62.8464445485378,0.127);
#6159=TOROIDAL_SURFACE('',#107672,59.0285554514622,0.127);
#6160=TOROIDAL_SURFACE('',#107706,62.8464445485378,0.127);
#6161=TOROIDAL_SURFACE('',#107716,59.0285554514622,0.127);
#6162=TOROIDAL_SURFACE('',#107750,62.8464445485378,0.127);
#6163=TOROIDAL_SURFACE('',#107760,59.0285554514622,0.127);
#6164=TOROIDAL_SURFACE('',#107794,62.8464445485378,0.127);
#6165=TOROIDAL_SURFACE('',#107804,59.0285554514622,0.127);
#6166=TOROIDAL_SURFACE('',#107838,62.8464445485378,0.127);
#6167=TOROIDAL_SURFACE('',#107848,59.0285554514622,0.127);
#6168=TOROIDAL_SURFACE('',#107882,62.8464445485378,0.127);
#6169=TOROIDAL_SURFACE('',#107892,59.0285554514622,0.127);
#6170=TOROIDAL_SURFACE('',#107926,62.8464445485378,0.127);
#6171=TOROIDAL_SURFACE('',#107936,59.0285554514622,0.127);
#6172=TOROIDAL_SURFACE('',#107970,62.8464445485378,0.127);
#6173=TOROIDAL_SURFACE('',#107980,59.0285554514622,0.127);
#6174=TOROIDAL_SURFACE('',#108014,62.8464445485378,0.127);
#6175=TOROIDAL_SURFACE('',#108024,59.0285554514622,0.127);
#6176=TOROIDAL_SURFACE('',#108058,62.8464445485378,0.127);
#6177=TOROIDAL_SURFACE('',#108068,59.0285554514622,0.127);
#6178=TOROIDAL_SURFACE('',#108102,62.8464445485378,0.127);
#6179=TOROIDAL_SURFACE('',#108112,59.0285554514622,0.127);
#6180=TOROIDAL_SURFACE('',#108146,62.8464445485378,0.127);
#6181=TOROIDAL_SURFACE('',#108156,59.0285554514622,0.127);
#6182=TOROIDAL_SURFACE('',#108190,62.8464445485378,0.127);
#6183=TOROIDAL_SURFACE('',#108200,59.0285554514622,0.127);
#6184=TOROIDAL_SURFACE('',#108234,62.8464445485378,0.127);
#6185=TOROIDAL_SURFACE('',#108244,59.0285554514622,0.127);
#6186=TOROIDAL_SURFACE('',#108278,62.8464445485378,0.127);
#6187=TOROIDAL_SURFACE('',#108288,59.0285554514622,0.127);
#6188=TOROIDAL_SURFACE('',#108322,62.8464445485378,0.127);
#6189=TOROIDAL_SURFACE('',#108332,59.0285554514622,0.127);
#6190=TOROIDAL_SURFACE('',#108366,62.8464445485378,0.127);
#6191=TOROIDAL_SURFACE('',#108376,59.0285554514622,0.127);
#6192=TOROIDAL_SURFACE('',#108410,62.8464445485378,0.127);
#6193=TOROIDAL_SURFACE('',#108420,59.0285554514622,0.127);
#6194=TOROIDAL_SURFACE('',#108454,62.8464445485378,0.127);
#6195=TOROIDAL_SURFACE('',#108464,59.0285554514622,0.127);
#6196=TOROIDAL_SURFACE('',#108498,62.8464445485378,0.127);
#6197=TOROIDAL_SURFACE('',#108508,59.0285554514622,0.127);
#6198=TOROIDAL_SURFACE('',#108542,62.8464445485378,0.127);
#6199=TOROIDAL_SURFACE('',#108552,59.0285554514622,0.127);
#6200=TOROIDAL_SURFACE('',#108586,62.8464445485378,0.127);
#6201=TOROIDAL_SURFACE('',#108596,59.0285554514622,0.127);
#6202=TOROIDAL_SURFACE('',#108630,62.8464445485378,0.127);
#6203=TOROIDAL_SURFACE('',#108640,59.0285554514622,0.127);
#6204=TOROIDAL_SURFACE('',#108674,62.8464445485378,0.127);
#6205=TOROIDAL_SURFACE('',#108684,59.0285554514622,0.127);
#6206=TOROIDAL_SURFACE('',#108718,62.8464445485378,0.127);
#6207=TOROIDAL_SURFACE('',#108728,59.0285554514622,0.127);
#6208=TOROIDAL_SURFACE('',#108762,62.8464445485378,0.127);
#6209=TOROIDAL_SURFACE('',#108772,59.0285554514622,0.127);
#6210=TOROIDAL_SURFACE('',#108806,62.8464445485378,0.127);
#6211=TOROIDAL_SURFACE('',#108816,59.0285554514622,0.127);
#6212=TOROIDAL_SURFACE('',#108850,62.8464445485378,0.127);
#6213=TOROIDAL_SURFACE('',#108860,59.0285554514622,0.127);
#6214=TOROIDAL_SURFACE('',#108932,62.8464445485378,0.127);
#6215=TOROIDAL_SURFACE('',#108942,59.0285554514622,0.127);
#6216=TOROIDAL_SURFACE('',#108976,62.8464445485378,0.127);
#6217=TOROIDAL_SURFACE('',#108986,59.0285554514622,0.127);
#6218=TOROIDAL_SURFACE('',#109020,62.8464445485378,0.127);
#6219=TOROIDAL_SURFACE('',#109030,59.0285554514622,0.127);
#6220=TOROIDAL_SURFACE('',#109064,62.8464445485378,0.127);
#6221=TOROIDAL_SURFACE('',#109074,59.0285554514622,0.127);
#6222=TOROIDAL_SURFACE('',#109108,62.8464445485378,0.127);
#6223=TOROIDAL_SURFACE('',#109118,59.0285554514622,0.127);
#6224=TOROIDAL_SURFACE('',#109152,62.8464445485378,0.127);
#6225=TOROIDAL_SURFACE('',#109162,59.0285554514622,0.127);
#6226=TOROIDAL_SURFACE('',#109196,62.8464445485378,0.127);
#6227=TOROIDAL_SURFACE('',#109206,59.0285554514622,0.127);
#6228=TOROIDAL_SURFACE('',#109240,62.8464445485378,0.127);
#6229=TOROIDAL_SURFACE('',#109250,59.0285554514622,0.127);
#6230=TOROIDAL_SURFACE('',#109284,62.8464445485378,0.127);
#6231=TOROIDAL_SURFACE('',#109294,59.0285554514622,0.127);
#6232=TOROIDAL_SURFACE('',#109328,62.8464445485378,0.127);
#6233=TOROIDAL_SURFACE('',#109338,59.0285554514622,0.127);
#6234=TOROIDAL_SURFACE('',#109372,62.8464445485378,0.127);
#6235=TOROIDAL_SURFACE('',#109382,59.0285554514622,0.127);
#6236=TOROIDAL_SURFACE('',#109416,62.8464445485378,0.127);
#6237=TOROIDAL_SURFACE('',#109426,59.0285554514622,0.127);
#6238=TOROIDAL_SURFACE('',#109460,62.8464445485378,0.127);
#6239=TOROIDAL_SURFACE('',#109470,59.0285554514622,0.127);
#6240=TOROIDAL_SURFACE('',#109504,62.8464445485378,0.127);
#6241=TOROIDAL_SURFACE('',#109514,59.0285554514622,0.127);
#6242=TOROIDAL_SURFACE('',#109586,62.8464445485378,0.127);
#6243=TOROIDAL_SURFACE('',#109596,59.0285554514622,0.127);
#6244=TOROIDAL_SURFACE('',#109630,62.8464445485378,0.127);
#6245=TOROIDAL_SURFACE('',#109640,59.0285554514622,0.127);
#6246=TOROIDAL_SURFACE('',#109674,62.8464445485378,0.127);
#6247=TOROIDAL_SURFACE('',#109684,59.0285554514622,0.127);
#6248=TOROIDAL_SURFACE('',#109718,62.8464445485378,0.127);
#6249=TOROIDAL_SURFACE('',#109728,59.0285554514622,0.127);
#6250=TOROIDAL_SURFACE('',#109762,62.8464445485378,0.127);
#6251=TOROIDAL_SURFACE('',#109772,59.0285554514622,0.127);
#6252=TOROIDAL_SURFACE('',#109806,62.8464445485378,0.127);
#6253=TOROIDAL_SURFACE('',#109816,59.0285554514622,0.127);
#6254=TOROIDAL_SURFACE('',#109850,62.8464445485378,0.127);
#6255=TOROIDAL_SURFACE('',#109860,59.0285554514622,0.127);
#6256=TOROIDAL_SURFACE('',#109894,62.8464445485378,0.127);
#6257=TOROIDAL_SURFACE('',#109904,59.0285554514622,0.127);
#6258=TOROIDAL_SURFACE('',#109938,62.8464445485378,0.127);
#6259=TOROIDAL_SURFACE('',#109948,59.0285554514622,0.127);
#6260=TOROIDAL_SURFACE('',#109982,62.8464445485378,0.127);
#6261=TOROIDAL_SURFACE('',#109992,59.0285554514622,0.127);
#6262=TOROIDAL_SURFACE('',#110026,62.8464445485378,0.127);
#6263=TOROIDAL_SURFACE('',#110036,59.0285554514622,0.127);
#6264=TOROIDAL_SURFACE('',#110070,62.8464445485378,0.127);
#6265=TOROIDAL_SURFACE('',#110080,59.0285554514622,0.127);
#6266=TOROIDAL_SURFACE('',#110114,62.8464445485378,0.127);
#6267=TOROIDAL_SURFACE('',#110124,59.0285554514622,0.127);
#6268=TOROIDAL_SURFACE('',#110158,62.8464445485378,0.127);
#6269=TOROIDAL_SURFACE('',#110168,59.0285554514622,0.127);
#6270=TOROIDAL_SURFACE('',#110185,65.381,0.127);
#6271=TOROIDAL_SURFACE('',#110189,68.623,0.127);
#6272=TOROIDAL_SURFACE('',#110193,68.877,0.127);
#6273=TOROIDAL_SURFACE('',#110207,65.0762,0.0762);
#6274=TOROIDAL_SURFACE('',#110211,65.1778,0.0762);
#6275=TOROIDAL_SURFACE('',#110221,71.3206076480316,0.8255);
#6276=TOROIDAL_SURFACE('',#110225,74.6340699810941,2.54);
#6277=TOROIDAL_SURFACE('',#110230,23.73,1.27);
#6278=TOROIDAL_SURFACE('',#110235,23.73,1.27);
#6279=TOROIDAL_SURFACE('',#110252,81.905,1.905);
#6280=TOROIDAL_SURFACE('',#110263,73.65,6.35);
#6281=TOROIDAL_SURFACE('',#110390,73.65,6.35);
#6282=TOROIDAL_SURFACE('',#110392,73.65,6.35);
#6283=TOROIDAL_SURFACE('',#110394,73.65,6.35);
#6284=TOROIDAL_SURFACE('',#110395,73.65,6.35);
#6285=TOROIDAL_SURFACE('',#110414,81.905,1.905);
#6286=TOROIDAL_SURFACE('',#110416,26.905,1.905);
#6287=TOROIDAL_SURFACE('',#110422,26.905,1.905);
#6288=TOROIDAL_SURFACE('',#110426,26.905,1.905);
#6289=TOROIDAL_SURFACE('',#110431,26.905,1.905);
#6290=TOROIDAL_SURFACE('',#110435,81.905,1.905);
#6291=TOROIDAL_SURFACE('',#110436,26.905,1.905);
#6292=TOROIDAL_SURFACE('',#110441,26.905,1.905);
#6293=TOROIDAL_SURFACE('',#110451,23.73,1.27);
#6294=TOROIDAL_SURFACE('',#110460,23.73,1.27);
#6295=TOROIDAL_SURFACE('',#110464,82.2472021719721,2.54);
#6296=TOROIDAL_SURFACE('',#110467,82.2472021719721,2.54);
#6297=TOROIDAL_SURFACE('',#110470,82.2472021719721,2.54);
#6298=TOROIDAL_SURFACE('',#110474,82.2472021719721,2.54);
#6299=TOROIDAL_SURFACE('',#110506,78.7299999999993,2.54);
#6300=TOROIDAL_SURFACE('',#110510,1.8415,0.0635);
#6301=TOROIDAL_SURFACE('',#110515,1.8415,0.0635);
#6302=TOROIDAL_SURFACE('',#110531,66.2265441972308,0.127);
#6303=TOROIDAL_SURFACE('',#110536,66.3535441972308,0.127);
#6304=TOROIDAL_SURFACE('',#110548,56.0881943187058,0.381);
#6305=TOROIDAL_SURFACE('',#110552,50.889,0.381);
#6306=TOROIDAL_SURFACE('',#110557,50.381,0.381);
#6307=TOROIDAL_SURFACE('',#110562,56.7377745952251,0.254);
#6308=TOROIDAL_SURFACE('',#110566,57.4087519663171,0.254);
#6309=TOROIDAL_SURFACE('',#110717,74.8702478255888,1.5875);
#6310=TOROIDAL_SURFACE('',#110799,23.73,0.762);
#6311=TOROIDAL_SURFACE('',#110806,23.73,0.762);
#6312=TOROIDAL_SURFACE('',#110808,23.73,0.762);
#6313=TOROIDAL_SURFACE('',#110814,23.73,0.762);
#6314=TOROIDAL_SURFACE('',#110940,10.,5.);
#6315=TOROIDAL_SURFACE('',#110947,10.,5.);
#6316=TOROIDAL_SURFACE('',#110949,10.,5.);
#6317=TOROIDAL_SURFACE('',#110955,10.,5.);
#6318=TOROIDAL_SURFACE('',#110956,10.,5.);
#6319=TOROIDAL_SURFACE('',#110964,10.,5.);
#6320=TOROIDAL_SURFACE('',#110968,10.,5.);
#6321=TOROIDAL_SURFACE('',#110975,10.,5.);
#6322=FACE_BOUND('',#13733,.T.);
#6323=FACE_BOUND('',#13751,.T.);
#6324=FACE_BOUND('',#13752,.T.);
#6325=FACE_BOUND('',#13753,.T.);
#6326=FACE_BOUND('',#13754,.T.);
#6327=FACE_BOUND('',#13755,.T.);
#6328=FACE_BOUND('',#13757,.T.);
#6329=FACE_BOUND('',#13758,.T.);
#6330=FACE_BOUND('',#13759,.T.);
#6331=FACE_BOUND('',#13760,.T.);
#6332=FACE_BOUND('',#13761,.T.);
#6333=FACE_BOUND('',#13785,.T.);
#6334=FACE_BOUND('',#13786,.T.);
#6335=FACE_BOUND('',#13787,.T.);
#6336=FACE_BOUND('',#13789,.T.);
#6337=FACE_BOUND('',#13790,.T.);
#6338=FACE_BOUND('',#13791,.T.);
#6339=FACE_BOUND('',#13793,.T.);
#6340=FACE_BOUND('',#13795,.T.);
#6341=FACE_BOUND('',#13805,.T.);
#6342=FACE_BOUND('',#13806,.T.);
#6343=FACE_BOUND('',#13808,.T.);
#6344=FACE_BOUND('',#13830,.T.);
#6345=FACE_BOUND('',#13831,.T.);
#6346=FACE_BOUND('',#13832,.T.);
#6347=FACE_BOUND('',#13841,.T.);
#6348=FACE_BOUND('',#13843,.T.);
#6349=FACE_BOUND('',#13851,.T.);
#6350=FACE_BOUND('',#13857,.T.);
#6351=FACE_BOUND('',#13866,.T.);
#6352=FACE_BOUND('',#13886,.T.);
#6353=FACE_BOUND('',#13888,.T.);
#6354=FACE_BOUND('',#13892,.T.);
#6355=FACE_BOUND('',#13894,.T.);
#6356=FACE_BOUND('',#13898,.T.);
#6357=FACE_BOUND('',#13900,.T.);
#6358=FACE_BOUND('',#13904,.T.);
#6359=FACE_BOUND('',#13906,.T.);
#6360=FACE_BOUND('',#13912,.T.);
#6361=FACE_BOUND('',#13914,.T.);
#6362=FACE_BOUND('',#13920,.T.);
#6363=FACE_BOUND('',#13922,.T.);
#6364=FACE_BOUND('',#13926,.T.);
#6365=FACE_BOUND('',#13928,.T.);
#6366=FACE_BOUND('',#14475,.T.);
#6367=FACE_BOUND('',#14482,.T.);
#6368=FACE_BOUND('',#14484,.T.);
#6369=FACE_BOUND('',#17011,.T.);
#6370=FACE_BOUND('',#17018,.T.);
#6371=FACE_BOUND('',#17020,.T.);
#6372=FACE_BOUND('',#19008,.T.);
#6373=FACE_BOUND('',#19010,.T.);
#6374=FACE_BOUND('',#19012,.T.);
#6375=FACE_BOUND('',#19018,.T.);
#6376=FACE_BOUND('',#19020,.T.);
#6377=FACE_BOUND('',#19057,.T.);
#6378=FACE_BOUND('',#19067,.T.);
#6379=FACE_BOUND('',#19070,.T.);
#6380=FACE_BOUND('',#19073,.T.);
#6381=FACE_BOUND('',#19075,.T.);
#6382=FACE_BOUND('',#19088,.T.);
#6383=FACE_BOUND('',#19089,.T.);
#6384=FACE_BOUND('',#19090,.T.);
#6385=FACE_BOUND('',#19091,.T.);
#6386=FACE_BOUND('',#19092,.T.);
#6387=FACE_BOUND('',#19094,.T.);
#6388=FACE_BOUND('',#19096,.T.);
#6389=FACE_BOUND('',#19216,.T.);
#6390=FACE_BOUND('',#19222,.T.);
#6391=FACE_BOUND('',#19224,.T.);
#6392=FACE_BOUND('',#19226,.T.);
#6393=FACE_BOUND('',#19228,.T.);
#6394=FACE_BOUND('',#19241,.T.);
#6395=FACE_BOUND('',#19243,.T.);
#6396=FACE_BOUND('',#19245,.T.);
#6397=FACE_BOUND('',#19247,.T.);
#6398=FACE_BOUND('',#19249,.T.);
#6399=FACE_BOUND('',#19269,.T.);
#6400=FACE_BOUND('',#19305,.T.);
#6401=FACE_BOUND('',#19327,.T.);
#6402=FACE_BOUND('',#19331,.T.);
#6403=FACE_BOUND('',#19333,.T.);
#6404=FACE_BOUND('',#19335,.T.);
#6405=FACE_BOUND('',#19360,.T.);
#6406=FACE_BOUND('',#19361,.T.);
#6407=FACE_BOUND('',#19362,.T.);
#6408=FACE_BOUND('',#19363,.T.);
#6409=FACE_BOUND('',#19364,.T.);
#6410=FACE_BOUND('',#19366,.T.);
#6411=FACE_BOUND('',#19368,.T.);
#6412=FACE_BOUND('',#19370,.T.);
#6413=FACE_BOUND('',#19372,.T.);
#6414=FACE_BOUND('',#19374,.T.);
#6415=FACE_BOUND('',#19392,.T.);
#6416=FACE_BOUND('',#19393,.T.);
#6417=FACE_BOUND('',#19394,.T.);
#6418=FACE_BOUND('',#19395,.T.);
#6419=FACE_BOUND('',#19396,.T.);
#6420=FACE_BOUND('',#19399,.T.);
#6421=FACE_BOUND('',#19401,.T.);
#6422=FACE_BOUND('',#19403,.T.);
#6423=FACE_BOUND('',#19405,.T.);
#6424=FACE_BOUND('',#19410,.T.);
#6425=FACE_BOUND('',#19429,.T.);
#6426=FACE_BOUND('',#19431,.T.);
#6427=FACE_BOUND('',#19433,.T.);
#6428=FACE_BOUND('',#19435,.T.);
#6429=FACE_BOUND('',#19437,.T.);
#6430=FACE_BOUND('',#19438,.T.);
#6431=FACE_BOUND('',#19440,.T.);
#6432=FACE_BOUND('',#19441,.T.);
#6433=FACE_BOUND('',#19443,.T.);
#6434=FACE_BOUND('',#19444,.T.);
#6435=FACE_BOUND('',#19450,.T.);
#6436=FACE_BOUND('',#19468,.T.);
#6437=FACE_BOUND('',#19474,.T.);
#6438=FACE_BOUND('',#19478,.T.);
#6439=FACE_BOUND('',#19482,.T.);
#6440=FACE_BOUND('',#19486,.T.);
#6441=FACE_BOUND('',#19490,.T.);
#6442=FACE_BOUND('',#19499,.T.);
#6443=FACE_BOUND('',#19546,.T.);
#6444=FACE_BOUND('',#19950,.T.);
#6445=FACE_BOUND('',#19956,.T.);
#6446=PLANE('',#98816);
#6447=PLANE('',#98817);
#6448=PLANE('',#98818);
#6449=PLANE('',#98819);
#6450=PLANE('',#98820);
#6451=PLANE('',#98821);
#6452=PLANE('',#98822);
#6453=PLANE('',#98823);
#6454=PLANE('',#98824);
#6455=PLANE('',#98825);
#6456=PLANE('',#98826);
#6457=PLANE('',#98827);
#6458=PLANE('',#98828);
#6459=PLANE('',#98829);
#6460=PLANE('',#98830);
#6461=PLANE('',#98831);
#6462=PLANE('',#98832);
#6463=PLANE('',#98833);
#6464=PLANE('',#98834);
#6465=PLANE('',#98835);
#6466=PLANE('',#98836);
#6467=PLANE('',#98837);
#6468=PLANE('',#98842);
#6469=PLANE('',#98847);
#6470=PLANE('',#98848);
#6471=PLANE('',#98849);
#6472=PLANE('',#98850);
#6473=PLANE('',#98894);
#6474=PLANE('',#98895);
#6475=PLANE('',#98936);
#6476=PLANE('',#98937);
#6477=PLANE('',#98938);
#6478=PLANE('',#98975);
#6479=PLANE('',#98976);
#6480=PLANE('',#98982);
#6481=PLANE('',#98983);
#6482=PLANE('',#98994);
#6483=PLANE('',#98995);
#6484=PLANE('',#98996);
#6485=PLANE('',#98997);
#6486=PLANE('',#98998);
#6487=PLANE('',#98999);
#6488=PLANE('',#99011);
#6489=PLANE('',#99012);
#6490=PLANE('',#99019);
#6491=PLANE('',#99020);
#6492=PLANE('',#99027);
#6493=PLANE('',#99028);
#6494=PLANE('',#99035);
#6495=PLANE('',#99036);
#6496=PLANE('',#99051);
#6497=PLANE('',#99052);
#6498=PLANE('',#99067);
#6499=PLANE('',#99068);
#6500=PLANE('',#99075);
#6501=PLANE('',#99076);
#6502=PLANE('',#99364);
#6503=PLANE('',#99371);
#6504=PLANE('',#99379);
#6505=PLANE('',#99393);
#6506=PLANE('',#99400);
#6507=PLANE('',#99408);
#6508=PLANE('',#99422);
#6509=PLANE('',#99429);
#6510=PLANE('',#99437);
#6511=PLANE('',#99451);
#6512=PLANE('',#99458);
#6513=PLANE('',#99466);
#6514=PLANE('',#99480);
#6515=PLANE('',#99487);
#6516=PLANE('',#99495);
#6517=PLANE('',#99509);
#6518=PLANE('',#99516);
#6519=PLANE('',#99524);
#6520=PLANE('',#99538);
#6521=PLANE('',#99545);
#6522=PLANE('',#99553);
#6523=PLANE('',#99567);
#6524=PLANE('',#99574);
#6525=PLANE('',#99582);
#6526=PLANE('',#99596);
#6527=PLANE('',#99603);
#6528=PLANE('',#99611);
#6529=PLANE('',#99625);
#6530=PLANE('',#99632);
#6531=PLANE('',#99640);
#6532=PLANE('',#99654);
#6533=PLANE('',#99661);
#6534=PLANE('',#99669);
#6535=PLANE('',#99683);
#6536=PLANE('',#99690);
#6537=PLANE('',#99698);
#6538=PLANE('',#99712);
#6539=PLANE('',#99719);
#6540=PLANE('',#99727);
#6541=PLANE('',#99741);
#6542=PLANE('',#99748);
#6543=PLANE('',#99756);
#6544=PLANE('',#99770);
#6545=PLANE('',#99777);
#6546=PLANE('',#99785);
#6547=PLANE('',#99799);
#6548=PLANE('',#99806);
#6549=PLANE('',#99814);
#6550=PLANE('',#99828);
#6551=PLANE('',#99835);
#6552=PLANE('',#99843);
#6553=PLANE('',#99857);
#6554=PLANE('',#99864);
#6555=PLANE('',#99872);
#6556=PLANE('',#99886);
#6557=PLANE('',#99893);
#6558=PLANE('',#99901);
#6559=PLANE('',#99915);
#6560=PLANE('',#99922);
#6561=PLANE('',#99930);
#6562=PLANE('',#99944);
#6563=PLANE('',#99951);
#6564=PLANE('',#99959);
#6565=PLANE('',#99973);
#6566=PLANE('',#99980);
#6567=PLANE('',#99988);
#6568=PLANE('',#100002);
#6569=PLANE('',#100009);
#6570=PLANE('',#100017);
#6571=PLANE('',#100031);
#6572=PLANE('',#100038);
#6573=PLANE('',#100046);
#6574=PLANE('',#100060);
#6575=PLANE('',#100067);
#6576=PLANE('',#100075);
#6577=PLANE('',#100089);
#6578=PLANE('',#100096);
#6579=PLANE('',#100104);
#6580=PLANE('',#100118);
#6581=PLANE('',#100125);
#6582=PLANE('',#100133);
#6583=PLANE('',#100147);
#6584=PLANE('',#100154);
#6585=PLANE('',#100162);
#6586=PLANE('',#100176);
#6587=PLANE('',#100183);
#6588=PLANE('',#100191);
#6589=PLANE('',#100205);
#6590=PLANE('',#100212);
#6591=PLANE('',#100220);
#6592=PLANE('',#100234);
#6593=PLANE('',#100241);
#6594=PLANE('',#100249);
#6595=PLANE('',#100263);
#6596=PLANE('',#100270);
#6597=PLANE('',#100278);
#6598=PLANE('',#100292);
#6599=PLANE('',#100299);
#6600=PLANE('',#100307);
#6601=PLANE('',#100321);
#6602=PLANE('',#100328);
#6603=PLANE('',#100336);
#6604=PLANE('',#100350);
#6605=PLANE('',#100357);
#6606=PLANE('',#100365);
#6607=PLANE('',#100379);
#6608=PLANE('',#100386);
#6609=PLANE('',#100394);
#6610=PLANE('',#100408);
#6611=PLANE('',#100415);
#6612=PLANE('',#100423);
#6613=PLANE('',#100437);
#6614=PLANE('',#100444);
#6615=PLANE('',#100452);
#6616=PLANE('',#100466);
#6617=PLANE('',#100473);
#6618=PLANE('',#100481);
#6619=PLANE('',#100495);
#6620=PLANE('',#100502);
#6621=PLANE('',#100510);
#6622=PLANE('',#100524);
#6623=PLANE('',#100531);
#6624=PLANE('',#100539);
#6625=PLANE('',#100553);
#6626=PLANE('',#100560);
#6627=PLANE('',#100568);
#6628=PLANE('',#100582);
#6629=PLANE('',#100589);
#6630=PLANE('',#100597);
#6631=PLANE('',#100611);
#6632=PLANE('',#100618);
#6633=PLANE('',#100626);
#6634=PLANE('',#100640);
#6635=PLANE('',#100647);
#6636=PLANE('',#100655);
#6637=PLANE('',#100669);
#6638=PLANE('',#100676);
#6639=PLANE('',#100684);
#6640=PLANE('',#100698);
#6641=PLANE('',#100705);
#6642=PLANE('',#100713);
#6643=PLANE('',#100727);
#6644=PLANE('',#100734);
#6645=PLANE('',#100742);
#6646=PLANE('',#100756);
#6647=PLANE('',#100763);
#6648=PLANE('',#100771);
#6649=PLANE('',#100785);
#6650=PLANE('',#100792);
#6651=PLANE('',#100800);
#6652=PLANE('',#100814);
#6653=PLANE('',#100821);
#6654=PLANE('',#100829);
#6655=PLANE('',#100843);
#6656=PLANE('',#100850);
#6657=PLANE('',#100858);
#6658=PLANE('',#100872);
#6659=PLANE('',#100879);
#6660=PLANE('',#100887);
#6661=PLANE('',#100901);
#6662=PLANE('',#100908);
#6663=PLANE('',#100916);
#6664=PLANE('',#100930);
#6665=PLANE('',#100937);
#6666=PLANE('',#100945);
#6667=PLANE('',#100959);
#6668=PLANE('',#100966);
#6669=PLANE('',#100974);
#6670=PLANE('',#100988);
#6671=PLANE('',#100995);
#6672=PLANE('',#101003);
#6673=PLANE('',#101017);
#6674=PLANE('',#101024);
#6675=PLANE('',#101032);
#6676=PLANE('',#101046);
#6677=PLANE('',#101053);
#6678=PLANE('',#101061);
#6679=PLANE('',#101075);
#6680=PLANE('',#101076);
#6681=PLANE('',#101083);
#6682=PLANE('',#101091);
#6683=PLANE('',#101093);
#6684=PLANE('',#101094);
#6685=PLANE('',#101107);
#6686=PLANE('',#101110);
#6687=PLANE('',#101115);
#6688=PLANE('',#101166);
#6689=PLANE('',#101169);
#6690=PLANE('',#101174);
#6691=PLANE('',#101179);
#6692=PLANE('',#101182);
#6693=PLANE('',#101187);
#6694=PLANE('',#101192);
#6695=PLANE('',#101195);
#6696=PLANE('',#101200);
#6697=PLANE('',#101205);
#6698=PLANE('',#101208);
#6699=PLANE('',#101213);
#6700=PLANE('',#101218);
#6701=PLANE('',#101221);
#6702=PLANE('',#101226);
#6703=PLANE('',#101231);
#6704=PLANE('',#101234);
#6705=PLANE('',#101239);
#6706=PLANE('',#101244);
#6707=PLANE('',#101247);
#6708=PLANE('',#101252);
#6709=PLANE('',#101257);
#6710=PLANE('',#101260);
#6711=PLANE('',#101265);
#6712=PLANE('',#101270);
#6713=PLANE('',#101273);
#6714=PLANE('',#101278);
#6715=PLANE('',#101283);
#6716=PLANE('',#101286);
#6717=PLANE('',#101291);
#6718=PLANE('',#101296);
#6719=PLANE('',#101299);
#6720=PLANE('',#101304);
#6721=PLANE('',#101309);
#6722=PLANE('',#101312);
#6723=PLANE('',#101317);
#6724=PLANE('',#101322);
#6725=PLANE('',#101325);
#6726=PLANE('',#101330);
#6727=PLANE('',#101335);
#6728=PLANE('',#101338);
#6729=PLANE('',#101343);
#6730=PLANE('',#101348);
#6731=PLANE('',#101351);
#6732=PLANE('',#101356);
#6733=PLANE('',#101361);
#6734=PLANE('',#101364);
#6735=PLANE('',#101369);
#6736=PLANE('',#101374);
#6737=PLANE('',#101377);
#6738=PLANE('',#101382);
#6739=PLANE('',#101387);
#6740=PLANE('',#101390);
#6741=PLANE('',#101395);
#6742=PLANE('',#101400);
#6743=PLANE('',#101403);
#6744=PLANE('',#101408);
#6745=PLANE('',#101413);
#6746=PLANE('',#101416);
#6747=PLANE('',#101421);
#6748=PLANE('',#101426);
#6749=PLANE('',#101429);
#6750=PLANE('',#101434);
#6751=PLANE('',#101439);
#6752=PLANE('',#101442);
#6753=PLANE('',#101447);
#6754=PLANE('',#101452);
#6755=PLANE('',#101455);
#6756=PLANE('',#101460);
#6757=PLANE('',#101465);
#6758=PLANE('',#101468);
#6759=PLANE('',#101473);
#6760=PLANE('',#101478);
#6761=PLANE('',#101481);
#6762=PLANE('',#101486);
#6763=PLANE('',#101491);
#6764=PLANE('',#101494);
#6765=PLANE('',#101499);
#6766=PLANE('',#101504);
#6767=PLANE('',#101507);
#6768=PLANE('',#101512);
#6769=PLANE('',#101517);
#6770=PLANE('',#101520);
#6771=PLANE('',#101525);
#6772=PLANE('',#101530);
#6773=PLANE('',#101533);
#6774=PLANE('',#101538);
#6775=PLANE('',#101543);
#6776=PLANE('',#101544);
#6777=PLANE('',#101549);
#6778=PLANE('',#101554);
#6779=PLANE('',#101557);
#6780=PLANE('',#101562);
#6781=PLANE('',#101567);
#6782=PLANE('',#101570);
#6783=PLANE('',#101575);
#6784=PLANE('',#101580);
#6785=PLANE('',#101583);
#6786=PLANE('',#101588);
#6787=PLANE('',#101593);
#6788=PLANE('',#101596);
#6789=PLANE('',#101601);
#6790=PLANE('',#101606);
#6791=PLANE('',#101609);
#6792=PLANE('',#101614);
#6793=PLANE('',#101619);
#6794=PLANE('',#101622);
#6795=PLANE('',#101627);
#6796=PLANE('',#101632);
#6797=PLANE('',#101635);
#6798=PLANE('',#101640);
#6799=PLANE('',#101645);
#6800=PLANE('',#101648);
#6801=PLANE('',#101653);
#6802=PLANE('',#101658);
#6803=PLANE('',#101661);
#6804=PLANE('',#101666);
#6805=PLANE('',#101671);
#6806=PLANE('',#101674);
#6807=PLANE('',#101679);
#6808=PLANE('',#101684);
#6809=PLANE('',#101687);
#6810=PLANE('',#101692);
#6811=PLANE('',#101697);
#6812=PLANE('',#101700);
#6813=PLANE('',#101705);
#6814=PLANE('',#101710);
#6815=PLANE('',#101713);
#6816=PLANE('',#101718);
#6817=PLANE('',#101723);
#6818=PLANE('',#101726);
#6819=PLANE('',#101731);
#6820=PLANE('',#101736);
#6821=PLANE('',#101737);
#6822=PLANE('',#101742);
#6823=PLANE('',#101747);
#6824=PLANE('',#101750);
#6825=PLANE('',#101755);
#6826=PLANE('',#101760);
#6827=PLANE('',#101763);
#6828=PLANE('',#101768);
#6829=PLANE('',#101773);
#6830=PLANE('',#101776);
#6831=PLANE('',#101781);
#6832=PLANE('',#101786);
#6833=PLANE('',#101789);
#6834=PLANE('',#101794);
#6835=PLANE('',#101799);
#6836=PLANE('',#101802);
#6837=PLANE('',#101807);
#6838=PLANE('',#101812);
#6839=PLANE('',#101815);
#6840=PLANE('',#101820);
#6841=PLANE('',#101825);
#6842=PLANE('',#101828);
#6843=PLANE('',#101833);
#6844=PLANE('',#101838);
#6845=PLANE('',#101841);
#6846=PLANE('',#101846);
#6847=PLANE('',#101851);
#6848=PLANE('',#101854);
#6849=PLANE('',#101859);
#6850=PLANE('',#101864);
#6851=PLANE('',#101867);
#6852=PLANE('',#101872);
#6853=PLANE('',#101877);
#6854=PLANE('',#101880);
#6855=PLANE('',#101885);
#6856=PLANE('',#101890);
#6857=PLANE('',#101893);
#6858=PLANE('',#101898);
#6859=PLANE('',#101903);
#6860=PLANE('',#101906);
#6861=PLANE('',#101911);
#6862=PLANE('',#101916);
#6863=PLANE('',#101919);
#6864=PLANE('',#101924);
#6865=PLANE('',#104918);
#6866=PLANE('',#104925);
#6867=PLANE('',#104933);
#6868=PLANE('',#104947);
#6869=PLANE('',#104954);
#6870=PLANE('',#104962);
#6871=PLANE('',#104976);
#6872=PLANE('',#104983);
#6873=PLANE('',#104991);
#6874=PLANE('',#105005);
#6875=PLANE('',#105012);
#6876=PLANE('',#105020);
#6877=PLANE('',#105034);
#6878=PLANE('',#105041);
#6879=PLANE('',#105049);
#6880=PLANE('',#105063);
#6881=PLANE('',#105070);
#6882=PLANE('',#105078);
#6883=PLANE('',#105092);
#6884=PLANE('',#105099);
#6885=PLANE('',#105107);
#6886=PLANE('',#105121);
#6887=PLANE('',#105128);
#6888=PLANE('',#105136);
#6889=PLANE('',#105150);
#6890=PLANE('',#105157);
#6891=PLANE('',#105165);
#6892=PLANE('',#105179);
#6893=PLANE('',#105186);
#6894=PLANE('',#105194);
#6895=PLANE('',#105208);
#6896=PLANE('',#105215);
#6897=PLANE('',#105223);
#6898=PLANE('',#105237);
#6899=PLANE('',#105244);
#6900=PLANE('',#105252);
#6901=PLANE('',#105266);
#6902=PLANE('',#105273);
#6903=PLANE('',#105281);
#6904=PLANE('',#105295);
#6905=PLANE('',#105302);
#6906=PLANE('',#105310);
#6907=PLANE('',#105324);
#6908=PLANE('',#105331);
#6909=PLANE('',#105339);
#6910=PLANE('',#105353);
#6911=PLANE('',#105360);
#6912=PLANE('',#105368);
#6913=PLANE('',#105382);
#6914=PLANE('',#105389);
#6915=PLANE('',#105397);
#6916=PLANE('',#105411);
#6917=PLANE('',#105418);
#6918=PLANE('',#105426);
#6919=PLANE('',#105440);
#6920=PLANE('',#105447);
#6921=PLANE('',#105455);
#6922=PLANE('',#105469);
#6923=PLANE('',#105476);
#6924=PLANE('',#105484);
#6925=PLANE('',#105498);
#6926=PLANE('',#105505);
#6927=PLANE('',#105513);
#6928=PLANE('',#105527);
#6929=PLANE('',#105534);
#6930=PLANE('',#105542);
#6931=PLANE('',#105556);
#6932=PLANE('',#105563);
#6933=PLANE('',#105571);
#6934=PLANE('',#105585);
#6935=PLANE('',#105592);
#6936=PLANE('',#105600);
#6937=PLANE('',#105614);
#6938=PLANE('',#105621);
#6939=PLANE('',#105629);
#6940=PLANE('',#105643);
#6941=PLANE('',#105650);
#6942=PLANE('',#105658);
#6943=PLANE('',#105672);
#6944=PLANE('',#105679);
#6945=PLANE('',#105687);
#6946=PLANE('',#105701);
#6947=PLANE('',#105708);
#6948=PLANE('',#105716);
#6949=PLANE('',#105730);
#6950=PLANE('',#105737);
#6951=PLANE('',#105745);
#6952=PLANE('',#105759);
#6953=PLANE('',#105766);
#6954=PLANE('',#105774);
#6955=PLANE('',#105788);
#6956=PLANE('',#105795);
#6957=PLANE('',#105803);
#6958=PLANE('',#105817);
#6959=PLANE('',#105824);
#6960=PLANE('',#105832);
#6961=PLANE('',#105846);
#6962=PLANE('',#105853);
#6963=PLANE('',#105861);
#6964=PLANE('',#105875);
#6965=PLANE('',#105882);
#6966=PLANE('',#105890);
#6967=PLANE('',#105904);
#6968=PLANE('',#105911);
#6969=PLANE('',#105919);
#6970=PLANE('',#105933);
#6971=PLANE('',#105940);
#6972=PLANE('',#105948);
#6973=PLANE('',#105962);
#6974=PLANE('',#105969);
#6975=PLANE('',#105977);
#6976=PLANE('',#105991);
#6977=PLANE('',#105998);
#6978=PLANE('',#106006);
#6979=PLANE('',#106020);
#6980=PLANE('',#106027);
#6981=PLANE('',#106035);
#6982=PLANE('',#106049);
#6983=PLANE('',#106056);
#6984=PLANE('',#106064);
#6985=PLANE('',#106078);
#6986=PLANE('',#106085);
#6987=PLANE('',#106093);
#6988=PLANE('',#106107);
#6989=PLANE('',#106114);
#6990=PLANE('',#106122);
#6991=PLANE('',#106136);
#6992=PLANE('',#106143);
#6993=PLANE('',#106151);
#6994=PLANE('',#106165);
#6995=PLANE('',#106172);
#6996=PLANE('',#106180);
#6997=PLANE('',#106194);
#6998=PLANE('',#106201);
#6999=PLANE('',#106209);
#7000=PLANE('',#106223);
#7001=PLANE('',#106230);
#7002=PLANE('',#106238);
#7003=PLANE('',#106252);
#7004=PLANE('',#106259);
#7005=PLANE('',#106267);
#7006=PLANE('',#106281);
#7007=PLANE('',#106288);
#7008=PLANE('',#106296);
#7009=PLANE('',#106310);
#7010=PLANE('',#106317);
#7011=PLANE('',#106325);
#7012=PLANE('',#106339);
#7013=PLANE('',#106346);
#7014=PLANE('',#106354);
#7015=PLANE('',#106368);
#7016=PLANE('',#106375);
#7017=PLANE('',#106383);
#7018=PLANE('',#106397);
#7019=PLANE('',#106404);
#7020=PLANE('',#106412);
#7021=PLANE('',#106426);
#7022=PLANE('',#106433);
#7023=PLANE('',#106441);
#7024=PLANE('',#106455);
#7025=PLANE('',#106462);
#7026=PLANE('',#106470);
#7027=PLANE('',#106484);
#7028=PLANE('',#106491);
#7029=PLANE('',#106499);
#7030=PLANE('',#106513);
#7031=PLANE('',#106520);
#7032=PLANE('',#106528);
#7033=PLANE('',#106542);
#7034=PLANE('',#106549);
#7035=PLANE('',#106557);
#7036=PLANE('',#106571);
#7037=PLANE('',#106578);
#7038=PLANE('',#106586);
#7039=PLANE('',#106600);
#7040=PLANE('',#106607);
#7041=PLANE('',#106615);
#7042=PLANE('',#106629);
#7043=PLANE('',#106630);
#7044=PLANE('',#106637);
#7045=PLANE('',#106645);
#7046=PLANE('',#106647);
#7047=PLANE('',#106648);
#7048=PLANE('',#106661);
#7049=PLANE('',#106664);
#7050=PLANE('',#106669);
#7051=PLANE('',#106720);
#7052=PLANE('',#106723);
#7053=PLANE('',#106728);
#7054=PLANE('',#106733);
#7055=PLANE('',#106736);
#7056=PLANE('',#106741);
#7057=PLANE('',#106746);
#7058=PLANE('',#106749);
#7059=PLANE('',#106754);
#7060=PLANE('',#106759);
#7061=PLANE('',#106762);
#7062=PLANE('',#106767);
#7063=PLANE('',#106772);
#7064=PLANE('',#106775);
#7065=PLANE('',#106780);
#7066=PLANE('',#106785);
#7067=PLANE('',#106788);
#7068=PLANE('',#106793);
#7069=PLANE('',#106798);
#7070=PLANE('',#106801);
#7071=PLANE('',#106806);
#7072=PLANE('',#106811);
#7073=PLANE('',#106814);
#7074=PLANE('',#106819);
#7075=PLANE('',#106824);
#7076=PLANE('',#106827);
#7077=PLANE('',#106832);
#7078=PLANE('',#106837);
#7079=PLANE('',#106840);
#7080=PLANE('',#106845);
#7081=PLANE('',#106850);
#7082=PLANE('',#106853);
#7083=PLANE('',#106858);
#7084=PLANE('',#106863);
#7085=PLANE('',#106866);
#7086=PLANE('',#106871);
#7087=PLANE('',#106876);
#7088=PLANE('',#106879);
#7089=PLANE('',#106884);
#7090=PLANE('',#106889);
#7091=PLANE('',#106892);
#7092=PLANE('',#106897);
#7093=PLANE('',#106902);
#7094=PLANE('',#106905);
#7095=PLANE('',#106910);
#7096=PLANE('',#106915);
#7097=PLANE('',#106918);
#7098=PLANE('',#106923);
#7099=PLANE('',#106928);
#7100=PLANE('',#106931);
#7101=PLANE('',#106936);
#7102=PLANE('',#106941);
#7103=PLANE('',#106944);
#7104=PLANE('',#106949);
#7105=PLANE('',#106954);
#7106=PLANE('',#106957);
#7107=PLANE('',#106962);
#7108=PLANE('',#106967);
#7109=PLANE('',#106970);
#7110=PLANE('',#106975);
#7111=PLANE('',#106980);
#7112=PLANE('',#106983);
#7113=PLANE('',#106988);
#7114=PLANE('',#106993);
#7115=PLANE('',#106996);
#7116=PLANE('',#107001);
#7117=PLANE('',#107006);
#7118=PLANE('',#107009);
#7119=PLANE('',#107014);
#7120=PLANE('',#107019);
#7121=PLANE('',#107022);
#7122=PLANE('',#107027);
#7123=PLANE('',#107032);
#7124=PLANE('',#107035);
#7125=PLANE('',#107040);
#7126=PLANE('',#107045);
#7127=PLANE('',#107048);
#7128=PLANE('',#107053);
#7129=PLANE('',#107058);
#7130=PLANE('',#107061);
#7131=PLANE('',#107066);
#7132=PLANE('',#107071);
#7133=PLANE('',#107074);
#7134=PLANE('',#107079);
#7135=PLANE('',#107084);
#7136=PLANE('',#107087);
#7137=PLANE('',#107092);
#7138=PLANE('',#107097);
#7139=PLANE('',#107098);
#7140=PLANE('',#107103);
#7141=PLANE('',#107108);
#7142=PLANE('',#107111);
#7143=PLANE('',#107116);
#7144=PLANE('',#107121);
#7145=PLANE('',#107124);
#7146=PLANE('',#107129);
#7147=PLANE('',#107134);
#7148=PLANE('',#107137);
#7149=PLANE('',#107142);
#7150=PLANE('',#107147);
#7151=PLANE('',#107150);
#7152=PLANE('',#107155);
#7153=PLANE('',#107160);
#7154=PLANE('',#107163);
#7155=PLANE('',#107168);
#7156=PLANE('',#107173);
#7157=PLANE('',#107176);
#7158=PLANE('',#107181);
#7159=PLANE('',#107186);
#7160=PLANE('',#107189);
#7161=PLANE('',#107194);
#7162=PLANE('',#107199);
#7163=PLANE('',#107202);
#7164=PLANE('',#107207);
#7165=PLANE('',#107212);
#7166=PLANE('',#107215);
#7167=PLANE('',#107220);
#7168=PLANE('',#107225);
#7169=PLANE('',#107228);
#7170=PLANE('',#107233);
#7171=PLANE('',#107238);
#7172=PLANE('',#107241);
#7173=PLANE('',#107246);
#7174=PLANE('',#107251);
#7175=PLANE('',#107254);
#7176=PLANE('',#107259);
#7177=PLANE('',#107264);
#7178=PLANE('',#107267);
#7179=PLANE('',#107272);
#7180=PLANE('',#107277);
#7181=PLANE('',#107280);
#7182=PLANE('',#107285);
#7183=PLANE('',#107290);
#7184=PLANE('',#107291);
#7185=PLANE('',#107296);
#7186=PLANE('',#107301);
#7187=PLANE('',#107304);
#7188=PLANE('',#107309);
#7189=PLANE('',#107314);
#7190=PLANE('',#107317);
#7191=PLANE('',#107322);
#7192=PLANE('',#107327);
#7193=PLANE('',#107330);
#7194=PLANE('',#107335);
#7195=PLANE('',#107340);
#7196=PLANE('',#107343);
#7197=PLANE('',#107348);
#7198=PLANE('',#107353);
#7199=PLANE('',#107356);
#7200=PLANE('',#107361);
#7201=PLANE('',#107366);
#7202=PLANE('',#107369);
#7203=PLANE('',#107374);
#7204=PLANE('',#107379);
#7205=PLANE('',#107382);
#7206=PLANE('',#107387);
#7207=PLANE('',#107392);
#7208=PLANE('',#107395);
#7209=PLANE('',#107400);
#7210=PLANE('',#107405);
#7211=PLANE('',#107408);
#7212=PLANE('',#107413);
#7213=PLANE('',#107418);
#7214=PLANE('',#107421);
#7215=PLANE('',#107426);
#7216=PLANE('',#107431);
#7217=PLANE('',#107434);
#7218=PLANE('',#107439);
#7219=PLANE('',#107444);
#7220=PLANE('',#107447);
#7221=PLANE('',#107452);
#7222=PLANE('',#107457);
#7223=PLANE('',#107460);
#7224=PLANE('',#107465);
#7225=PLANE('',#107470);
#7226=PLANE('',#107473);
#7227=PLANE('',#107478);
#7228=PLANE('',#110204);
#7229=PLANE('',#110205);
#7230=PLANE('',#110206);
#7231=PLANE('',#110219);
#7232=PLANE('',#110220);
#7233=PLANE('',#110302);
#7234=PLANE('',#110303);
#7235=PLANE('',#110304);
#7236=PLANE('',#110313);
#7237=PLANE('',#110317);
#7238=PLANE('',#110321);
#7239=PLANE('',#110325);
#7240=PLANE('',#110329);
#7241=PLANE('',#110330);
#7242=PLANE('',#110332);
#7243=PLANE('',#110334);
#7244=PLANE('',#110341);
#7245=PLANE('',#110344);
#7246=PLANE('',#110350);
#7247=PLANE('',#110355);
#7248=PLANE('',#110361);
#7249=PLANE('',#110363);
#7250=PLANE('',#110365);
#7251=PLANE('',#110366);
#7252=PLANE('',#110367);
#7253=PLANE('',#110368);
#7254=PLANE('',#110372);
#7255=PLANE('',#110373);
#7256=PLANE('',#110374);
#7257=PLANE('',#110380);
#7258=PLANE('',#110381);
#7259=PLANE('',#110382);
#7260=PLANE('',#110385);
#7261=PLANE('',#110387);
#7262=PLANE('',#110388);
#7263=PLANE('',#110389);
#7264=PLANE('',#110530);
#7265=PLANE('',#110546);
#7266=PLANE('',#110547);
#7267=PLANE('',#110582);
#7268=PLANE('',#110583);
#7269=PLANE('',#110584);
#7270=PLANE('',#110585);
#7271=PLANE('',#110586);
#7272=PLANE('',#110617);
#7273=PLANE('',#110618);
#7274=PLANE('',#110631);
#7275=PLANE('',#110632);
#7276=PLANE('',#110633);
#7277=PLANE('',#110634);
#7278=PLANE('',#110635);
#7279=PLANE('',#110636);
#7280=PLANE('',#110637);
#7281=PLANE('',#110669);
#7282=PLANE('',#110670);
#7283=PLANE('',#110683);
#7284=PLANE('',#110684);
#7285=PLANE('',#110685);
#7286=PLANE('',#110686);
#7287=PLANE('',#110687);
#7288=PLANE('',#110688);
#7289=PLANE('',#110689);
#7290=PLANE('',#110709);
#7291=PLANE('',#110710);
#7292=PLANE('',#110760);
#7293=PLANE('',#110764);
#7294=PLANE('',#110768);
#7295=PLANE('',#110772);
#7296=PLANE('',#110773);
#7297=PLANE('',#110778);
#7298=PLANE('',#110779);
#7299=PLANE('',#110780);
#7300=PLANE('',#110781);
#7301=PLANE('',#110782);
#7302=PLANE('',#110789);
#7303=PLANE('',#110792);
#7304=PLANE('',#110795);
#7305=PLANE('',#110798);
#7306=PLANE('',#110815);
#7307=PLANE('',#110819);
#7308=PLANE('',#110822);
#7309=PLANE('',#110823);
#7310=PLANE('',#110824);
#7311=PLANE('',#110827);
#7312=PLANE('',#110828);
#7313=PLANE('',#110829);
#7314=PLANE('',#110832);
#7315=PLANE('',#110833);
#7316=PLANE('',#110835);
#7317=PLANE('',#110836);
#7318=PLANE('',#110837);
#7319=PLANE('',#110838);
#7320=PLANE('',#110859);
#7321=PLANE('',#110862);
#7322=PLANE('',#110865);
#7323=PLANE('',#110867);
#7324=PLANE('',#110869);
#7325=PLANE('',#110871);
#7326=PLANE('',#110873);
#7327=PLANE('',#110874);
#7328=PLANE('',#110876);
#7329=PLANE('',#110877);
#7330=PLANE('',#110880);
#7331=PLANE('',#110881);
#7332=PLANE('',#110882);
#7333=PLANE('',#110883);
#7334=PLANE('',#110884);
#7335=PLANE('',#110893);
#7336=PLANE('',#110894);
#7337=PLANE('',#110895);
#7338=PLANE('',#110896);
#7339=PLANE('',#110933);
#7340=PLANE('',#110934);
#7341=PLANE('',#110935);
#7342=PLANE('',#110936);
#7343=PLANE('',#110937);
#7344=PLANE('',#110976);
#7345=PLANE('',#110977);
#7346=PLANE('',#110978);
#7347=PLANE('',#110979);
#7348=PLANE('',#110980);
#7349=PLANE('',#110981);
#7350=PLANE('',#110982);
#7351=PLANE('',#110983);
#7352=PLANE('',#110984);
#7353=PLANE('',#110985);
#7354=PLANE('',#110990);
#7355=PLANE('',#110998);
#7356=PLANE('',#110999);
#7357=PLANE('',#111002);
#7358=PLANE('',#111005);
#7359=PLANE('',#111008);
#7360=PLANE('',#111011);
#7361=PLANE('',#111014);
#7362=PLANE('',#111017);
#7363=PLANE('',#111020);
#7364=PLANE('',#111021);
#7365=PLANE('',#111026);
#7366=PLANE('',#111029);
#7367=PLANE('',#111032);
#7368=PLANE('',#111035);
#7369=PLANE('',#111038);
#7370=PLANE('',#111039);
#7371=PLANE('',#111064);
#7372=PLANE('',#111090);
#7373=PLANE('',#111092);
#7374=PLANE('',#111094);
#7375=PLANE('',#111095);
#7376=PLANE('',#111096);
#7377=PLANE('',#111098);
#7378=PLANE('',#111100);
#7379=PLANE('',#111102);
#7380=PLANE('',#111104);
#7381=PLANE('',#111106);
#7382=PLANE('',#111108);
#7383=PLANE('',#111109);
#7384=PLANE('',#111110);
#7385=PLANE('',#111112);
#7386=PLANE('',#111114);
#7387=PLANE('',#111116);
#7388=PLANE('',#111118);
#7389=PLANE('',#111120);
#7390=PLANE('',#111122);
#7391=PLANE('',#111123);
#7392=PLANE('',#111124);
#7393=PLANE('',#111126);
#7394=PLANE('',#111128);
#7395=PLANE('',#111130);
#7396=PLANE('',#111132);
#7397=PLANE('',#111134);
#7398=PLANE('',#111136);
#7399=PLANE('',#111137);
#7400=PLANE('',#111138);
#7401=PLANE('',#111140);
#7402=PLANE('',#111142);
#7403=PLANE('',#111144);
#7404=PLANE('',#111148);
#7405=PLANE('',#111156);
#7406=PLANE('',#111159);
#7407=PLANE('',#111162);
#7408=PLANE('',#111165);
#7409=PLANE('',#111168);
#7410=PLANE('',#111169);
#7411=PLANE('',#111172);
#7412=PLANE('',#111175);
#7413=PLANE('',#111178);
#7414=PLANE('',#111179);
#7415=PLANE('',#111184);
#7416=PLANE('',#111187);
#7417=PLANE('',#111190);
#7418=PLANE('',#111193);
#7419=PLANE('',#111196);
#7420=PLANE('',#111200);
#7421=PLANE('',#111208);
#7422=PLANE('',#111211);
#7423=PLANE('',#111214);
#7424=PLANE('',#111217);
#7425=PLANE('',#111220);
#7426=PLANE('',#111223);
#7427=PLANE('',#111226);
#7428=PLANE('',#111227);
#7429=PLANE('',#111230);
#7430=PLANE('',#111231);
#7431=PLANE('',#111236);
#7432=PLANE('',#111239);
#7433=PLANE('',#111242);
#7434=PLANE('',#111245);
#7435=PLANE('',#111248);
#7436=PLANE('',#111252);
#7437=PLANE('',#111260);
#7438=PLANE('',#111263);
#7439=PLANE('',#111266);
#7440=PLANE('',#111269);
#7441=PLANE('',#111272);
#7442=PLANE('',#111275);
#7443=PLANE('',#111278);
#7444=PLANE('',#111279);
#7445=PLANE('',#111282);
#7446=PLANE('',#111283);
#7447=PLANE('',#111288);
#7448=PLANE('',#111291);
#7449=PLANE('',#111294);
#7450=PLANE('',#111297);
#7451=PLANE('',#111300);
#7452=PLANE('',#111301);
#7453=PLANE('',#111302);
#7454=PLANE('',#111303);
#7455=PLANE('',#111304);
#7456=PLANE('',#111305);
#7457=PLANE('',#111309);
#7458=PLANE('',#111313);
#7459=PLANE('',#111317);
#7460=PLANE('',#111321);
#7461=PLANE('',#111322);
#7462=PLANE('',#111323);
#7463=PLANE('',#111324);
#7464=PLANE('',#111325);
#7465=PLANE('',#111326);
#7466=PLANE('',#111327);
#7467=PLANE('',#111328);
#7468=PLANE('',#111332);
#7469=PLANE('',#111336);
#7470=PLANE('',#111340);
#7471=PLANE('',#111344);
#7472=PLANE('',#111345);
#7473=PLANE('',#111346);
#7474=PLANE('',#111347);
#7475=PLANE('',#111351);
#7476=PLANE('',#111355);
#7477=PLANE('',#111359);
#7478=PLANE('',#111363);
#7479=PLANE('',#111364);
#7480=PLANE('',#111365);
#7481=PLANE('',#111366);
#7482=PLANE('',#111370);
#7483=PLANE('',#111371);
#7484=PLANE('',#111372);
#7485=PLANE('',#111373);
#7486=PLANE('',#111377);
#7487=PLANE('',#111381);
#7488=PLANE('',#111385);
#7489=PLANE('',#111389);
#7490=PLANE('',#111390);
#7491=PLANE('',#111391);
#7492=PLANE('',#111392);
#7493=PLANE('',#111396);
#7494=PLANE('',#111400);
#7495=PLANE('',#111404);
#7496=PLANE('',#111408);
#7497=PLANE('',#111409);
#7498=PLANE('',#111410);
#7499=PLANE('',#111411);
#7500=PLANE('',#111412);
#7501=PLANE('',#111413);
#7502=PLANE('',#111414);
#7503=PLANE('',#111418);
#7504=PLANE('',#111422);
#7505=PLANE('',#111426);
#7506=PLANE('',#111430);
#7507=PLANE('',#111431);
#7508=PLANE('',#111432);
#7509=PLANE('',#111433);
#7510=PLANE('',#111437);
#7511=PLANE('',#111441);
#7512=PLANE('',#111445);
#7513=PLANE('',#111449);
#7514=PLANE('',#111450);
#7515=PLANE('',#111451);
#7516=PLANE('',#111452);
#7517=PLANE('',#111456);
#7518=PLANE('',#111457);
#7519=PLANE('',#111458);
#7520=PLANE('',#111459);
#7521=PLANE('',#111463);
#7522=PLANE('',#111467);
#7523=PLANE('',#111471);
#7524=PLANE('',#111475);
#7525=PLANE('',#111476);
#7526=PLANE('',#111477);
#7527=PLANE('',#111478);
#7528=PLANE('',#111482);
#7529=PLANE('',#111486);
#7530=PLANE('',#111490);
#7531=PLANE('',#111494);
#7532=PLANE('',#111495);
#7533=PLANE('',#111496);
#7534=PLANE('',#111497);
#7535=PLANE('',#111498);
#7536=PLANE('',#111499);
#7537=PLANE('',#111500);
#7538=PLANE('',#111504);
#7539=PLANE('',#111508);
#7540=PLANE('',#111512);
#7541=PLANE('',#111516);
#7542=PLANE('',#111517);
#7543=PLANE('',#111518);
#7544=PLANE('',#111519);
#7545=PLANE('',#111523);
#7546=PLANE('',#111527);
#7547=PLANE('',#111531);
#7548=PLANE('',#111535);
#7549=PLANE('',#111536);
#7550=PLANE('',#111537);
#7551=PLANE('',#111538);
#7552=PLANE('',#111542);
#7553=PLANE('',#111543);
#7554=PLANE('',#111544);
#7555=PLANE('',#111545);
#7556=PLANE('',#111549);
#7557=PLANE('',#111553);
#7558=PLANE('',#111557);
#7559=PLANE('',#111561);
#7560=PLANE('',#111562);
#7561=PLANE('',#111563);
#7562=PLANE('',#111564);
#7563=PLANE('',#111568);
#7564=PLANE('',#111572);
#7565=PLANE('',#111576);
#7566=PLANE('',#111580);
#7567=PLANE('',#111581);
#7568=PLANE('',#111582);
#7569=PLANE('',#111583);
#7570=PLANE('',#111584);
#7571=PLANE('',#111585);
#7572=PLANE('',#111589);
#7573=PLANE('',#111593);
#7574=PLANE('',#111597);
#7575=PLANE('',#111601);
#7576=PLANE('',#111602);
#7577=PLANE('',#111603);
#7578=PLANE('',#111604);
#7579=PLANE('',#111608);
#7580=PLANE('',#111612);
#7581=PLANE('',#111616);
#7582=PLANE('',#111620);
#7583=PLANE('',#111621);
#7584=PLANE('',#111622);
#7585=PLANE('',#111623);
#7586=PLANE('',#111627);
#7587=PLANE('',#111628);
#7588=PLANE('',#111629);
#7589=PLANE('',#111630);
#7590=PLANE('',#111634);
#7591=PLANE('',#111638);
#7592=PLANE('',#111642);
#7593=PLANE('',#111646);
#7594=PLANE('',#111647);
#7595=PLANE('',#111648);
#7596=PLANE('',#111649);
#7597=PLANE('',#111650);
#7598=PLANE('',#111651);
#7599=PLANE('',#111652);
#7600=PLANE('',#111653);
#7601=PLANE('',#111654);
#7602=PLANE('',#111655);
#7603=PLANE('',#111656);
#7604=PLANE('',#111657);
#7605=PLANE('',#111658);
#7606=PLANE('',#111659);
#7607=PLANE('',#111660);
#7608=PLANE('',#111661);
#7609=PLANE('',#111662);
#7610=PLANE('',#111663);
#7611=PLANE('',#111664);
#7612=PLANE('',#111665);
#7613=PLANE('',#111666);
#7614=FACE_OUTER_BOUND('',#13724,.T.);
#7615=FACE_OUTER_BOUND('',#13725,.T.);
#7616=FACE_OUTER_BOUND('',#13726,.T.);
#7617=FACE_OUTER_BOUND('',#13727,.T.);
#7618=FACE_OUTER_BOUND('',#13728,.T.);
#7619=FACE_OUTER_BOUND('',#13729,.T.);
#7620=FACE_OUTER_BOUND('',#13730,.T.);
#7621=FACE_OUTER_BOUND('',#13731,.T.);
#7622=FACE_OUTER_BOUND('',#13732,.T.);
#7623=FACE_OUTER_BOUND('',#13734,.T.);
#7624=FACE_OUTER_BOUND('',#13735,.T.);
#7625=FACE_OUTER_BOUND('',#13736,.T.);
#7626=FACE_OUTER_BOUND('',#13737,.T.);
#7627=FACE_OUTER_BOUND('',#13738,.T.);
#7628=FACE_OUTER_BOUND('',#13739,.T.);
#7629=FACE_OUTER_BOUND('',#13740,.T.);
#7630=FACE_OUTER_BOUND('',#13741,.T.);
#7631=FACE_OUTER_BOUND('',#13742,.T.);
#7632=FACE_OUTER_BOUND('',#13743,.T.);
#7633=FACE_OUTER_BOUND('',#13744,.T.);
#7634=FACE_OUTER_BOUND('',#13745,.T.);
#7635=FACE_OUTER_BOUND('',#13746,.T.);
#7636=FACE_OUTER_BOUND('',#13747,.T.);
#7637=FACE_OUTER_BOUND('',#13748,.T.);
#7638=FACE_OUTER_BOUND('',#13749,.T.);
#7639=FACE_OUTER_BOUND('',#13750,.T.);
#7640=FACE_OUTER_BOUND('',#13756,.T.);
#7641=FACE_OUTER_BOUND('',#13762,.T.);
#7642=FACE_OUTER_BOUND('',#13763,.T.);
#7643=FACE_OUTER_BOUND('',#13764,.T.);
#7644=FACE_OUTER_BOUND('',#13765,.T.);
#7645=FACE_OUTER_BOUND('',#13766,.T.);
#7646=FACE_OUTER_BOUND('',#13767,.T.);
#7647=FACE_OUTER_BOUND('',#13768,.T.);
#7648=FACE_OUTER_BOUND('',#13769,.T.);
#7649=FACE_OUTER_BOUND('',#13770,.T.);
#7650=FACE_OUTER_BOUND('',#13771,.T.);
#7651=FACE_OUTER_BOUND('',#13772,.T.);
#7652=FACE_OUTER_BOUND('',#13773,.T.);
#7653=FACE_OUTER_BOUND('',#13774,.T.);
#7654=FACE_OUTER_BOUND('',#13775,.T.);
#7655=FACE_OUTER_BOUND('',#13776,.T.);
#7656=FACE_OUTER_BOUND('',#13777,.T.);
#7657=FACE_OUTER_BOUND('',#13778,.T.);
#7658=FACE_OUTER_BOUND('',#13779,.T.);
#7659=FACE_OUTER_BOUND('',#13780,.T.);
#7660=FACE_OUTER_BOUND('',#13781,.T.);
#7661=FACE_OUTER_BOUND('',#13782,.T.);
#7662=FACE_OUTER_BOUND('',#13783,.T.);
#7663=FACE_OUTER_BOUND('',#13784,.T.);
#7664=FACE_OUTER_BOUND('',#13788,.T.);
#7665=FACE_OUTER_BOUND('',#13792,.T.);
#7666=FACE_OUTER_BOUND('',#13794,.T.);
#7667=FACE_OUTER_BOUND('',#13796,.T.);
#7668=FACE_OUTER_BOUND('',#13797,.T.);
#7669=FACE_OUTER_BOUND('',#13798,.T.);
#7670=FACE_OUTER_BOUND('',#13799,.T.);
#7671=FACE_OUTER_BOUND('',#13800,.T.);
#7672=FACE_OUTER_BOUND('',#13801,.T.);
#7673=FACE_OUTER_BOUND('',#13802,.T.);
#7674=FACE_OUTER_BOUND('',#13803,.T.);
#7675=FACE_OUTER_BOUND('',#13804,.T.);
#7676=FACE_OUTER_BOUND('',#13807,.T.);
#7677=FACE_OUTER_BOUND('',#13809,.T.);
#7678=FACE_OUTER_BOUND('',#13810,.T.);
#7679=FACE_OUTER_BOUND('',#13811,.T.);
#7680=FACE_OUTER_BOUND('',#13812,.T.);
#7681=FACE_OUTER_BOUND('',#13813,.T.);
#7682=FACE_OUTER_BOUND('',#13814,.T.);
#7683=FACE_OUTER_BOUND('',#13815,.T.);
#7684=FACE_OUTER_BOUND('',#13816,.T.);
#7685=FACE_OUTER_BOUND('',#13817,.T.);
#7686=FACE_OUTER_BOUND('',#13818,.T.);
#7687=FACE_OUTER_BOUND('',#13819,.T.);
#7688=FACE_OUTER_BOUND('',#13820,.T.);
#7689=FACE_OUTER_BOUND('',#13821,.T.);
#7690=FACE_OUTER_BOUND('',#13822,.T.);
#7691=FACE_OUTER_BOUND('',#13823,.T.);
#7692=FACE_OUTER_BOUND('',#13824,.T.);
#7693=FACE_OUTER_BOUND('',#13825,.T.);
#7694=FACE_OUTER_BOUND('',#13826,.T.);
#7695=FACE_OUTER_BOUND('',#13827,.T.);
#7696=FACE_OUTER_BOUND('',#13828,.T.);
#7697=FACE_OUTER_BOUND('',#13829,.T.);
#7698=FACE_OUTER_BOUND('',#13833,.T.);
#7699=FACE_OUTER_BOUND('',#13834,.T.);
#7700=FACE_OUTER_BOUND('',#13835,.T.);
#7701=FACE_OUTER_BOUND('',#13836,.T.);
#7702=FACE_OUTER_BOUND('',#13837,.T.);
#7703=FACE_OUTER_BOUND('',#13838,.T.);
#7704=FACE_OUTER_BOUND('',#13839,.T.);
#7705=FACE_OUTER_BOUND('',#13840,.T.);
#7706=FACE_OUTER_BOUND('',#13842,.T.);
#7707=FACE_OUTER_BOUND('',#13844,.T.);
#7708=FACE_OUTER_BOUND('',#13845,.T.);
#7709=FACE_OUTER_BOUND('',#13846,.T.);
#7710=FACE_OUTER_BOUND('',#13847,.T.);
#7711=FACE_OUTER_BOUND('',#13848,.T.);
#7712=FACE_OUTER_BOUND('',#13849,.T.);
#7713=FACE_OUTER_BOUND('',#13850,.T.);
#7714=FACE_OUTER_BOUND('',#13852,.T.);
#7715=FACE_OUTER_BOUND('',#13853,.T.);
#7716=FACE_OUTER_BOUND('',#13854,.T.);
#7717=FACE_OUTER_BOUND('',#13855,.T.);
#7718=FACE_OUTER_BOUND('',#13856,.T.);
#7719=FACE_OUTER_BOUND('',#13858,.T.);
#7720=FACE_OUTER_BOUND('',#13859,.T.);
#7721=FACE_OUTER_BOUND('',#13860,.T.);
#7722=FACE_OUTER_BOUND('',#13861,.T.);
#7723=FACE_OUTER_BOUND('',#13862,.T.);
#7724=FACE_OUTER_BOUND('',#13863,.T.);
#7725=FACE_OUTER_BOUND('',#13864,.T.);
#7726=FACE_OUTER_BOUND('',#13865,.T.);
#7727=FACE_OUTER_BOUND('',#13867,.T.);
#7728=FACE_OUTER_BOUND('',#13868,.T.);
#7729=FACE_OUTER_BOUND('',#13869,.T.);
#7730=FACE_OUTER_BOUND('',#13870,.T.);
#7731=FACE_OUTER_BOUND('',#13871,.T.);
#7732=FACE_OUTER_BOUND('',#13872,.T.);
#7733=FACE_OUTER_BOUND('',#13873,.T.);
#7734=FACE_OUTER_BOUND('',#13874,.T.);
#7735=FACE_OUTER_BOUND('',#13875,.T.);
#7736=FACE_OUTER_BOUND('',#13876,.T.);
#7737=FACE_OUTER_BOUND('',#13877,.T.);
#7738=FACE_OUTER_BOUND('',#13878,.T.);
#7739=FACE_OUTER_BOUND('',#13879,.T.);
#7740=FACE_OUTER_BOUND('',#13880,.T.);
#7741=FACE_OUTER_BOUND('',#13881,.T.);
#7742=FACE_OUTER_BOUND('',#13882,.T.);
#7743=FACE_OUTER_BOUND('',#13883,.T.);
#7744=FACE_OUTER_BOUND('',#13884,.T.);
#7745=FACE_OUTER_BOUND('',#13885,.T.);
#7746=FACE_OUTER_BOUND('',#13887,.T.);
#7747=FACE_OUTER_BOUND('',#13889,.T.);
#7748=FACE_OUTER_BOUND('',#13890,.T.);
#7749=FACE_OUTER_BOUND('',#13891,.T.);
#7750=FACE_OUTER_BOUND('',#13893,.T.);
#7751=FACE_OUTER_BOUND('',#13895,.T.);
#7752=FACE_OUTER_BOUND('',#13896,.T.);
#7753=FACE_OUTER_BOUND('',#13897,.T.);
#7754=FACE_OUTER_BOUND('',#13899,.T.);
#7755=FACE_OUTER_BOUND('',#13901,.T.);
#7756=FACE_OUTER_BOUND('',#13902,.T.);
#7757=FACE_OUTER_BOUND('',#13903,.T.);
#7758=FACE_OUTER_BOUND('',#13905,.T.);
#7759=FACE_OUTER_BOUND('',#13907,.T.);
#7760=FACE_OUTER_BOUND('',#13908,.T.);
#7761=FACE_OUTER_BOUND('',#13909,.T.);
#7762=FACE_OUTER_BOUND('',#13910,.T.);
#7763=FACE_OUTER_BOUND('',#13911,.T.);
#7764=FACE_OUTER_BOUND('',#13913,.T.);
#7765=FACE_OUTER_BOUND('',#13915,.T.);
#7766=FACE_OUTER_BOUND('',#13916,.T.);
#7767=FACE_OUTER_BOUND('',#13917,.T.);
#7768=FACE_OUTER_BOUND('',#13918,.T.);
#7769=FACE_OUTER_BOUND('',#13919,.T.);
#7770=FACE_OUTER_BOUND('',#13921,.T.);
#7771=FACE_OUTER_BOUND('',#13923,.T.);
#7772=FACE_OUTER_BOUND('',#13924,.T.);
#7773=FACE_OUTER_BOUND('',#13925,.T.);
#7774=FACE_OUTER_BOUND('',#13927,.T.);
#7775=FACE_OUTER_BOUND('',#13929,.T.);
#7776=FACE_OUTER_BOUND('',#13930,.T.);
#7777=FACE_OUTER_BOUND('',#13931,.T.);
#7778=FACE_OUTER_BOUND('',#13932,.T.);
#7779=FACE_OUTER_BOUND('',#13933,.T.);
#7780=FACE_OUTER_BOUND('',#13934,.T.);
#7781=FACE_OUTER_BOUND('',#13935,.T.);
#7782=FACE_OUTER_BOUND('',#13936,.T.);
#7783=FACE_OUTER_BOUND('',#13937,.T.);
#7784=FACE_OUTER_BOUND('',#13938,.T.);
#7785=FACE_OUTER_BOUND('',#13939,.T.);
#7786=FACE_OUTER_BOUND('',#13940,.T.);
#7787=FACE_OUTER_BOUND('',#13941,.T.);
#7788=FACE_OUTER_BOUND('',#13942,.T.);
#7789=FACE_OUTER_BOUND('',#13943,.T.);
#7790=FACE_OUTER_BOUND('',#13944,.T.);
#7791=FACE_OUTER_BOUND('',#13945,.T.);
#7792=FACE_OUTER_BOUND('',#13946,.T.);
#7793=FACE_OUTER_BOUND('',#13947,.T.);
#7794=FACE_OUTER_BOUND('',#13948,.T.);
#7795=FACE_OUTER_BOUND('',#13949,.T.);
#7796=FACE_OUTER_BOUND('',#13950,.T.);
#7797=FACE_OUTER_BOUND('',#13951,.T.);
#7798=FACE_OUTER_BOUND('',#13952,.T.);
#7799=FACE_OUTER_BOUND('',#13953,.T.);
#7800=FACE_OUTER_BOUND('',#13954,.T.);
#7801=FACE_OUTER_BOUND('',#13955,.T.);
#7802=FACE_OUTER_BOUND('',#13956,.T.);
#7803=FACE_OUTER_BOUND('',#13957,.T.);
#7804=FACE_OUTER_BOUND('',#13958,.T.);
#7805=FACE_OUTER_BOUND('',#13959,.T.);
#7806=FACE_OUTER_BOUND('',#13960,.T.);
#7807=FACE_OUTER_BOUND('',#13961,.T.);
#7808=FACE_OUTER_BOUND('',#13962,.T.);
#7809=FACE_OUTER_BOUND('',#13963,.T.);
#7810=FACE_OUTER_BOUND('',#13964,.T.);
#7811=FACE_OUTER_BOUND('',#13965,.T.);
#7812=FACE_OUTER_BOUND('',#13966,.T.);
#7813=FACE_OUTER_BOUND('',#13967,.T.);
#7814=FACE_OUTER_BOUND('',#13968,.T.);
#7815=FACE_OUTER_BOUND('',#13969,.T.);
#7816=FACE_OUTER_BOUND('',#13970,.T.);
#7817=FACE_OUTER_BOUND('',#13971,.T.);
#7818=FACE_OUTER_BOUND('',#13972,.T.);
#7819=FACE_OUTER_BOUND('',#13973,.T.);
#7820=FACE_OUTER_BOUND('',#13974,.T.);
#7821=FACE_OUTER_BOUND('',#13975,.T.);
#7822=FACE_OUTER_BOUND('',#13976,.T.);
#7823=FACE_OUTER_BOUND('',#13977,.T.);
#7824=FACE_OUTER_BOUND('',#13978,.T.);
#7825=FACE_OUTER_BOUND('',#13979,.T.);
#7826=FACE_OUTER_BOUND('',#13980,.T.);
#7827=FACE_OUTER_BOUND('',#13981,.T.);
#7828=FACE_OUTER_BOUND('',#13982,.T.);
#7829=FACE_OUTER_BOUND('',#13983,.T.);
#7830=FACE_OUTER_BOUND('',#13984,.T.);
#7831=FACE_OUTER_BOUND('',#13985,.T.);
#7832=FACE_OUTER_BOUND('',#13986,.T.);
#7833=FACE_OUTER_BOUND('',#13987,.T.);
#7834=FACE_OUTER_BOUND('',#13988,.T.);
#7835=FACE_OUTER_BOUND('',#13989,.T.);
#7836=FACE_OUTER_BOUND('',#13990,.T.);
#7837=FACE_OUTER_BOUND('',#13991,.T.);
#7838=FACE_OUTER_BOUND('',#13992,.T.);
#7839=FACE_OUTER_BOUND('',#13993,.T.);
#7840=FACE_OUTER_BOUND('',#13994,.T.);
#7841=FACE_OUTER_BOUND('',#13995,.T.);
#7842=FACE_OUTER_BOUND('',#13996,.T.);
#7843=FACE_OUTER_BOUND('',#13997,.T.);
#7844=FACE_OUTER_BOUND('',#13998,.T.);
#7845=FACE_OUTER_BOUND('',#13999,.T.);
#7846=FACE_OUTER_BOUND('',#14000,.T.);
#7847=FACE_OUTER_BOUND('',#14001,.T.);
#7848=FACE_OUTER_BOUND('',#14002,.T.);
#7849=FACE_OUTER_BOUND('',#14003,.T.);
#7850=FACE_OUTER_BOUND('',#14004,.T.);
#7851=FACE_OUTER_BOUND('',#14005,.T.);
#7852=FACE_OUTER_BOUND('',#14006,.T.);
#7853=FACE_OUTER_BOUND('',#14007,.T.);
#7854=FACE_OUTER_BOUND('',#14008,.T.);
#7855=FACE_OUTER_BOUND('',#14009,.T.);
#7856=FACE_OUTER_BOUND('',#14010,.T.);
#7857=FACE_OUTER_BOUND('',#14011,.T.);
#7858=FACE_OUTER_BOUND('',#14012,.T.);
#7859=FACE_OUTER_BOUND('',#14013,.T.);
#7860=FACE_OUTER_BOUND('',#14014,.T.);
#7861=FACE_OUTER_BOUND('',#14015,.T.);
#7862=FACE_OUTER_BOUND('',#14016,.T.);
#7863=FACE_OUTER_BOUND('',#14017,.T.);
#7864=FACE_OUTER_BOUND('',#14018,.T.);
#7865=FACE_OUTER_BOUND('',#14019,.T.);
#7866=FACE_OUTER_BOUND('',#14020,.T.);
#7867=FACE_OUTER_BOUND('',#14021,.T.);
#7868=FACE_OUTER_BOUND('',#14022,.T.);
#7869=FACE_OUTER_BOUND('',#14023,.T.);
#7870=FACE_OUTER_BOUND('',#14024,.T.);
#7871=FACE_OUTER_BOUND('',#14025,.T.);
#7872=FACE_OUTER_BOUND('',#14026,.T.);
#7873=FACE_OUTER_BOUND('',#14027,.T.);
#7874=FACE_OUTER_BOUND('',#14028,.T.);
#7875=FACE_OUTER_BOUND('',#14029,.T.);
#7876=FACE_OUTER_BOUND('',#14030,.T.);
#7877=FACE_OUTER_BOUND('',#14031,.T.);
#7878=FACE_OUTER_BOUND('',#14032,.T.);
#7879=FACE_OUTER_BOUND('',#14033,.T.);
#7880=FACE_OUTER_BOUND('',#14034,.T.);
#7881=FACE_OUTER_BOUND('',#14035,.T.);
#7882=FACE_OUTER_BOUND('',#14036,.T.);
#7883=FACE_OUTER_BOUND('',#14037,.T.);
#7884=FACE_OUTER_BOUND('',#14038,.T.);
#7885=FACE_OUTER_BOUND('',#14039,.T.);
#7886=FACE_OUTER_BOUND('',#14040,.T.);
#7887=FACE_OUTER_BOUND('',#14041,.T.);
#7888=FACE_OUTER_BOUND('',#14042,.T.);
#7889=FACE_OUTER_BOUND('',#14043,.T.);
#7890=FACE_OUTER_BOUND('',#14044,.T.);
#7891=FACE_OUTER_BOUND('',#14045,.T.);
#7892=FACE_OUTER_BOUND('',#14046,.T.);
#7893=FACE_OUTER_BOUND('',#14047,.T.);
#7894=FACE_OUTER_BOUND('',#14048,.T.);
#7895=FACE_OUTER_BOUND('',#14049,.T.);
#7896=FACE_OUTER_BOUND('',#14050,.T.);
#7897=FACE_OUTER_BOUND('',#14051,.T.);
#7898=FACE_OUTER_BOUND('',#14052,.T.);
#7899=FACE_OUTER_BOUND('',#14053,.T.);
#7900=FACE_OUTER_BOUND('',#14054,.T.);
#7901=FACE_OUTER_BOUND('',#14055,.T.);
#7902=FACE_OUTER_BOUND('',#14056,.T.);
#7903=FACE_OUTER_BOUND('',#14057,.T.);
#7904=FACE_OUTER_BOUND('',#14058,.T.);
#7905=FACE_OUTER_BOUND('',#14059,.T.);
#7906=FACE_OUTER_BOUND('',#14060,.T.);
#7907=FACE_OUTER_BOUND('',#14061,.T.);
#7908=FACE_OUTER_BOUND('',#14062,.T.);
#7909=FACE_OUTER_BOUND('',#14063,.T.);
#7910=FACE_OUTER_BOUND('',#14064,.T.);
#7911=FACE_OUTER_BOUND('',#14065,.T.);
#7912=FACE_OUTER_BOUND('',#14066,.T.);
#7913=FACE_OUTER_BOUND('',#14067,.T.);
#7914=FACE_OUTER_BOUND('',#14068,.T.);
#7915=FACE_OUTER_BOUND('',#14069,.T.);
#7916=FACE_OUTER_BOUND('',#14070,.T.);
#7917=FACE_OUTER_BOUND('',#14071,.T.);
#7918=FACE_OUTER_BOUND('',#14072,.T.);
#7919=FACE_OUTER_BOUND('',#14073,.T.);
#7920=FACE_OUTER_BOUND('',#14074,.T.);
#7921=FACE_OUTER_BOUND('',#14075,.T.);
#7922=FACE_OUTER_BOUND('',#14076,.T.);
#7923=FACE_OUTER_BOUND('',#14077,.T.);
#7924=FACE_OUTER_BOUND('',#14078,.T.);
#7925=FACE_OUTER_BOUND('',#14079,.T.);
#7926=FACE_OUTER_BOUND('',#14080,.T.);
#7927=FACE_OUTER_BOUND('',#14081,.T.);
#7928=FACE_OUTER_BOUND('',#14082,.T.);
#7929=FACE_OUTER_BOUND('',#14083,.T.);
#7930=FACE_OUTER_BOUND('',#14084,.T.);
#7931=FACE_OUTER_BOUND('',#14085,.T.);
#7932=FACE_OUTER_BOUND('',#14086,.T.);
#7933=FACE_OUTER_BOUND('',#14087,.T.);
#7934=FACE_OUTER_BOUND('',#14088,.T.);
#7935=FACE_OUTER_BOUND('',#14089,.T.);
#7936=FACE_OUTER_BOUND('',#14090,.T.);
#7937=FACE_OUTER_BOUND('',#14091,.T.);
#7938=FACE_OUTER_BOUND('',#14092,.T.);
#7939=FACE_OUTER_BOUND('',#14093,.T.);
#7940=FACE_OUTER_BOUND('',#14094,.T.);
#7941=FACE_OUTER_BOUND('',#14095,.T.);
#7942=FACE_OUTER_BOUND('',#14096,.T.);
#7943=FACE_OUTER_BOUND('',#14097,.T.);
#7944=FACE_OUTER_BOUND('',#14098,.T.);
#7945=FACE_OUTER_BOUND('',#14099,.T.);
#7946=FACE_OUTER_BOUND('',#14100,.T.);
#7947=FACE_OUTER_BOUND('',#14101,.T.);
#7948=FACE_OUTER_BOUND('',#14102,.T.);
#7949=FACE_OUTER_BOUND('',#14103,.T.);
#7950=FACE_OUTER_BOUND('',#14104,.T.);
#7951=FACE_OUTER_BOUND('',#14105,.T.);
#7952=FACE_OUTER_BOUND('',#14106,.T.);
#7953=FACE_OUTER_BOUND('',#14107,.T.);
#7954=FACE_OUTER_BOUND('',#14108,.T.);
#7955=FACE_OUTER_BOUND('',#14109,.T.);
#7956=FACE_OUTER_BOUND('',#14110,.T.);
#7957=FACE_OUTER_BOUND('',#14111,.T.);
#7958=FACE_OUTER_BOUND('',#14112,.T.);
#7959=FACE_OUTER_BOUND('',#14113,.T.);
#7960=FACE_OUTER_BOUND('',#14114,.T.);
#7961=FACE_OUTER_BOUND('',#14115,.T.);
#7962=FACE_OUTER_BOUND('',#14116,.T.);
#7963=FACE_OUTER_BOUND('',#14117,.T.);
#7964=FACE_OUTER_BOUND('',#14118,.T.);
#7965=FACE_OUTER_BOUND('',#14119,.T.);
#7966=FACE_OUTER_BOUND('',#14120,.T.);
#7967=FACE_OUTER_BOUND('',#14121,.T.);
#7968=FACE_OUTER_BOUND('',#14122,.T.);
#7969=FACE_OUTER_BOUND('',#14123,.T.);
#7970=FACE_OUTER_BOUND('',#14124,.T.);
#7971=FACE_OUTER_BOUND('',#14125,.T.);
#7972=FACE_OUTER_BOUND('',#14126,.T.);
#7973=FACE_OUTER_BOUND('',#14127,.T.);
#7974=FACE_OUTER_BOUND('',#14128,.T.);
#7975=FACE_OUTER_BOUND('',#14129,.T.);
#7976=FACE_OUTER_BOUND('',#14130,.T.);
#7977=FACE_OUTER_BOUND('',#14131,.T.);
#7978=FACE_OUTER_BOUND('',#14132,.T.);
#7979=FACE_OUTER_BOUND('',#14133,.T.);
#7980=FACE_OUTER_BOUND('',#14134,.T.);
#7981=FACE_OUTER_BOUND('',#14135,.T.);
#7982=FACE_OUTER_BOUND('',#14136,.T.);
#7983=FACE_OUTER_BOUND('',#14137,.T.);
#7984=FACE_OUTER_BOUND('',#14138,.T.);
#7985=FACE_OUTER_BOUND('',#14139,.T.);
#7986=FACE_OUTER_BOUND('',#14140,.T.);
#7987=FACE_OUTER_BOUND('',#14141,.T.);
#7988=FACE_OUTER_BOUND('',#14142,.T.);
#7989=FACE_OUTER_BOUND('',#14143,.T.);
#7990=FACE_OUTER_BOUND('',#14144,.T.);
#7991=FACE_OUTER_BOUND('',#14145,.T.);
#7992=FACE_OUTER_BOUND('',#14146,.T.);
#7993=FACE_OUTER_BOUND('',#14147,.T.);
#7994=FACE_OUTER_BOUND('',#14148,.T.);
#7995=FACE_OUTER_BOUND('',#14149,.T.);
#7996=FACE_OUTER_BOUND('',#14150,.T.);
#7997=FACE_OUTER_BOUND('',#14151,.T.);
#7998=FACE_OUTER_BOUND('',#14152,.T.);
#7999=FACE_OUTER_BOUND('',#14153,.T.);
#8000=FACE_OUTER_BOUND('',#14154,.T.);
#8001=FACE_OUTER_BOUND('',#14155,.T.);
#8002=FACE_OUTER_BOUND('',#14156,.T.);
#8003=FACE_OUTER_BOUND('',#14157,.T.);
#8004=FACE_OUTER_BOUND('',#14158,.T.);
#8005=FACE_OUTER_BOUND('',#14159,.T.);
#8006=FACE_OUTER_BOUND('',#14160,.T.);
#8007=FACE_OUTER_BOUND('',#14161,.T.);
#8008=FACE_OUTER_BOUND('',#14162,.T.);
#8009=FACE_OUTER_BOUND('',#14163,.T.);
#8010=FACE_OUTER_BOUND('',#14164,.T.);
#8011=FACE_OUTER_BOUND('',#14165,.T.);
#8012=FACE_OUTER_BOUND('',#14166,.T.);
#8013=FACE_OUTER_BOUND('',#14167,.T.);
#8014=FACE_OUTER_BOUND('',#14168,.T.);
#8015=FACE_OUTER_BOUND('',#14169,.T.);
#8016=FACE_OUTER_BOUND('',#14170,.T.);
#8017=FACE_OUTER_BOUND('',#14171,.T.);
#8018=FACE_OUTER_BOUND('',#14172,.T.);
#8019=FACE_OUTER_BOUND('',#14173,.T.);
#8020=FACE_OUTER_BOUND('',#14174,.T.);
#8021=FACE_OUTER_BOUND('',#14175,.T.);
#8022=FACE_OUTER_BOUND('',#14176,.T.);
#8023=FACE_OUTER_BOUND('',#14177,.T.);
#8024=FACE_OUTER_BOUND('',#14178,.T.);
#8025=FACE_OUTER_BOUND('',#14179,.T.);
#8026=FACE_OUTER_BOUND('',#14180,.T.);
#8027=FACE_OUTER_BOUND('',#14181,.T.);
#8028=FACE_OUTER_BOUND('',#14182,.T.);
#8029=FACE_OUTER_BOUND('',#14183,.T.);
#8030=FACE_OUTER_BOUND('',#14184,.T.);
#8031=FACE_OUTER_BOUND('',#14185,.T.);
#8032=FACE_OUTER_BOUND('',#14186,.T.);
#8033=FACE_OUTER_BOUND('',#14187,.T.);
#8034=FACE_OUTER_BOUND('',#14188,.T.);
#8035=FACE_OUTER_BOUND('',#14189,.T.);
#8036=FACE_OUTER_BOUND('',#14190,.T.);
#8037=FACE_OUTER_BOUND('',#14191,.T.);
#8038=FACE_OUTER_BOUND('',#14192,.T.);
#8039=FACE_OUTER_BOUND('',#14193,.T.);
#8040=FACE_OUTER_BOUND('',#14194,.T.);
#8041=FACE_OUTER_BOUND('',#14195,.T.);
#8042=FACE_OUTER_BOUND('',#14196,.T.);
#8043=FACE_OUTER_BOUND('',#14197,.T.);
#8044=FACE_OUTER_BOUND('',#14198,.T.);
#8045=FACE_OUTER_BOUND('',#14199,.T.);
#8046=FACE_OUTER_BOUND('',#14200,.T.);
#8047=FACE_OUTER_BOUND('',#14201,.T.);
#8048=FACE_OUTER_BOUND('',#14202,.T.);
#8049=FACE_OUTER_BOUND('',#14203,.T.);
#8050=FACE_OUTER_BOUND('',#14204,.T.);
#8051=FACE_OUTER_BOUND('',#14205,.T.);
#8052=FACE_OUTER_BOUND('',#14206,.T.);
#8053=FACE_OUTER_BOUND('',#14207,.T.);
#8054=FACE_OUTER_BOUND('',#14208,.T.);
#8055=FACE_OUTER_BOUND('',#14209,.T.);
#8056=FACE_OUTER_BOUND('',#14210,.T.);
#8057=FACE_OUTER_BOUND('',#14211,.T.);
#8058=FACE_OUTER_BOUND('',#14212,.T.);
#8059=FACE_OUTER_BOUND('',#14213,.T.);
#8060=FACE_OUTER_BOUND('',#14214,.T.);
#8061=FACE_OUTER_BOUND('',#14215,.T.);
#8062=FACE_OUTER_BOUND('',#14216,.T.);
#8063=FACE_OUTER_BOUND('',#14217,.T.);
#8064=FACE_OUTER_BOUND('',#14218,.T.);
#8065=FACE_OUTER_BOUND('',#14219,.T.);
#8066=FACE_OUTER_BOUND('',#14220,.T.);
#8067=FACE_OUTER_BOUND('',#14221,.T.);
#8068=FACE_OUTER_BOUND('',#14222,.T.);
#8069=FACE_OUTER_BOUND('',#14223,.T.);
#8070=FACE_OUTER_BOUND('',#14224,.T.);
#8071=FACE_OUTER_BOUND('',#14225,.T.);
#8072=FACE_OUTER_BOUND('',#14226,.T.);
#8073=FACE_OUTER_BOUND('',#14227,.T.);
#8074=FACE_OUTER_BOUND('',#14228,.T.);
#8075=FACE_OUTER_BOUND('',#14229,.T.);
#8076=FACE_OUTER_BOUND('',#14230,.T.);
#8077=FACE_OUTER_BOUND('',#14231,.T.);
#8078=FACE_OUTER_BOUND('',#14232,.T.);
#8079=FACE_OUTER_BOUND('',#14233,.T.);
#8080=FACE_OUTER_BOUND('',#14234,.T.);
#8081=FACE_OUTER_BOUND('',#14235,.T.);
#8082=FACE_OUTER_BOUND('',#14236,.T.);
#8083=FACE_OUTER_BOUND('',#14237,.T.);
#8084=FACE_OUTER_BOUND('',#14238,.T.);
#8085=FACE_OUTER_BOUND('',#14239,.T.);
#8086=FACE_OUTER_BOUND('',#14240,.T.);
#8087=FACE_OUTER_BOUND('',#14241,.T.);
#8088=FACE_OUTER_BOUND('',#14242,.T.);
#8089=FACE_OUTER_BOUND('',#14243,.T.);
#8090=FACE_OUTER_BOUND('',#14244,.T.);
#8091=FACE_OUTER_BOUND('',#14245,.T.);
#8092=FACE_OUTER_BOUND('',#14246,.T.);
#8093=FACE_OUTER_BOUND('',#14247,.T.);
#8094=FACE_OUTER_BOUND('',#14248,.T.);
#8095=FACE_OUTER_BOUND('',#14249,.T.);
#8096=FACE_OUTER_BOUND('',#14250,.T.);
#8097=FACE_OUTER_BOUND('',#14251,.T.);
#8098=FACE_OUTER_BOUND('',#14252,.T.);
#8099=FACE_OUTER_BOUND('',#14253,.T.);
#8100=FACE_OUTER_BOUND('',#14254,.T.);
#8101=FACE_OUTER_BOUND('',#14255,.T.);
#8102=FACE_OUTER_BOUND('',#14256,.T.);
#8103=FACE_OUTER_BOUND('',#14257,.T.);
#8104=FACE_OUTER_BOUND('',#14258,.T.);
#8105=FACE_OUTER_BOUND('',#14259,.T.);
#8106=FACE_OUTER_BOUND('',#14260,.T.);
#8107=FACE_OUTER_BOUND('',#14261,.T.);
#8108=FACE_OUTER_BOUND('',#14262,.T.);
#8109=FACE_OUTER_BOUND('',#14263,.T.);
#8110=FACE_OUTER_BOUND('',#14264,.T.);
#8111=FACE_OUTER_BOUND('',#14265,.T.);
#8112=FACE_OUTER_BOUND('',#14266,.T.);
#8113=FACE_OUTER_BOUND('',#14267,.T.);
#8114=FACE_OUTER_BOUND('',#14268,.T.);
#8115=FACE_OUTER_BOUND('',#14269,.T.);
#8116=FACE_OUTER_BOUND('',#14270,.T.);
#8117=FACE_OUTER_BOUND('',#14271,.T.);
#8118=FACE_OUTER_BOUND('',#14272,.T.);
#8119=FACE_OUTER_BOUND('',#14273,.T.);
#8120=FACE_OUTER_BOUND('',#14274,.T.);
#8121=FACE_OUTER_BOUND('',#14275,.T.);
#8122=FACE_OUTER_BOUND('',#14276,.T.);
#8123=FACE_OUTER_BOUND('',#14277,.T.);
#8124=FACE_OUTER_BOUND('',#14278,.T.);
#8125=FACE_OUTER_BOUND('',#14279,.T.);
#8126=FACE_OUTER_BOUND('',#14280,.T.);
#8127=FACE_OUTER_BOUND('',#14281,.T.);
#8128=FACE_OUTER_BOUND('',#14282,.T.);
#8129=FACE_OUTER_BOUND('',#14283,.T.);
#8130=FACE_OUTER_BOUND('',#14284,.T.);
#8131=FACE_OUTER_BOUND('',#14285,.T.);
#8132=FACE_OUTER_BOUND('',#14286,.T.);
#8133=FACE_OUTER_BOUND('',#14287,.T.);
#8134=FACE_OUTER_BOUND('',#14288,.T.);
#8135=FACE_OUTER_BOUND('',#14289,.T.);
#8136=FACE_OUTER_BOUND('',#14290,.T.);
#8137=FACE_OUTER_BOUND('',#14291,.T.);
#8138=FACE_OUTER_BOUND('',#14292,.T.);
#8139=FACE_OUTER_BOUND('',#14293,.T.);
#8140=FACE_OUTER_BOUND('',#14294,.T.);
#8141=FACE_OUTER_BOUND('',#14295,.T.);
#8142=FACE_OUTER_BOUND('',#14296,.T.);
#8143=FACE_OUTER_BOUND('',#14297,.T.);
#8144=FACE_OUTER_BOUND('',#14298,.T.);
#8145=FACE_OUTER_BOUND('',#14299,.T.);
#8146=FACE_OUTER_BOUND('',#14300,.T.);
#8147=FACE_OUTER_BOUND('',#14301,.T.);
#8148=FACE_OUTER_BOUND('',#14302,.T.);
#8149=FACE_OUTER_BOUND('',#14303,.T.);
#8150=FACE_OUTER_BOUND('',#14304,.T.);
#8151=FACE_OUTER_BOUND('',#14305,.T.);
#8152=FACE_OUTER_BOUND('',#14306,.T.);
#8153=FACE_OUTER_BOUND('',#14307,.T.);
#8154=FACE_OUTER_BOUND('',#14308,.T.);
#8155=FACE_OUTER_BOUND('',#14309,.T.);
#8156=FACE_OUTER_BOUND('',#14310,.T.);
#8157=FACE_OUTER_BOUND('',#14311,.T.);
#8158=FACE_OUTER_BOUND('',#14312,.T.);
#8159=FACE_OUTER_BOUND('',#14313,.T.);
#8160=FACE_OUTER_BOUND('',#14314,.T.);
#8161=FACE_OUTER_BOUND('',#14315,.T.);
#8162=FACE_OUTER_BOUND('',#14316,.T.);
#8163=FACE_OUTER_BOUND('',#14317,.T.);
#8164=FACE_OUTER_BOUND('',#14318,.T.);
#8165=FACE_OUTER_BOUND('',#14319,.T.);
#8166=FACE_OUTER_BOUND('',#14320,.T.);
#8167=FACE_OUTER_BOUND('',#14321,.T.);
#8168=FACE_OUTER_BOUND('',#14322,.T.);
#8169=FACE_OUTER_BOUND('',#14323,.T.);
#8170=FACE_OUTER_BOUND('',#14324,.T.);
#8171=FACE_OUTER_BOUND('',#14325,.T.);
#8172=FACE_OUTER_BOUND('',#14326,.T.);
#8173=FACE_OUTER_BOUND('',#14327,.T.);
#8174=FACE_OUTER_BOUND('',#14328,.T.);
#8175=FACE_OUTER_BOUND('',#14329,.T.);
#8176=FACE_OUTER_BOUND('',#14330,.T.);
#8177=FACE_OUTER_BOUND('',#14331,.T.);
#8178=FACE_OUTER_BOUND('',#14332,.T.);
#8179=FACE_OUTER_BOUND('',#14333,.T.);
#8180=FACE_OUTER_BOUND('',#14334,.T.);
#8181=FACE_OUTER_BOUND('',#14335,.T.);
#8182=FACE_OUTER_BOUND('',#14336,.T.);
#8183=FACE_OUTER_BOUND('',#14337,.T.);
#8184=FACE_OUTER_BOUND('',#14338,.T.);
#8185=FACE_OUTER_BOUND('',#14339,.T.);
#8186=FACE_OUTER_BOUND('',#14340,.T.);
#8187=FACE_OUTER_BOUND('',#14341,.T.);
#8188=FACE_OUTER_BOUND('',#14342,.T.);
#8189=FACE_OUTER_BOUND('',#14343,.T.);
#8190=FACE_OUTER_BOUND('',#14344,.T.);
#8191=FACE_OUTER_BOUND('',#14345,.T.);
#8192=FACE_OUTER_BOUND('',#14346,.T.);
#8193=FACE_OUTER_BOUND('',#14347,.T.);
#8194=FACE_OUTER_BOUND('',#14348,.T.);
#8195=FACE_OUTER_BOUND('',#14349,.T.);
#8196=FACE_OUTER_BOUND('',#14350,.T.);
#8197=FACE_OUTER_BOUND('',#14351,.T.);
#8198=FACE_OUTER_BOUND('',#14352,.T.);
#8199=FACE_OUTER_BOUND('',#14353,.T.);
#8200=FACE_OUTER_BOUND('',#14354,.T.);
#8201=FACE_OUTER_BOUND('',#14355,.T.);
#8202=FACE_OUTER_BOUND('',#14356,.T.);
#8203=FACE_OUTER_BOUND('',#14357,.T.);
#8204=FACE_OUTER_BOUND('',#14358,.T.);
#8205=FACE_OUTER_BOUND('',#14359,.T.);
#8206=FACE_OUTER_BOUND('',#14360,.T.);
#8207=FACE_OUTER_BOUND('',#14361,.T.);
#8208=FACE_OUTER_BOUND('',#14362,.T.);
#8209=FACE_OUTER_BOUND('',#14363,.T.);
#8210=FACE_OUTER_BOUND('',#14364,.T.);
#8211=FACE_OUTER_BOUND('',#14365,.T.);
#8212=FACE_OUTER_BOUND('',#14366,.T.);
#8213=FACE_OUTER_BOUND('',#14367,.T.);
#8214=FACE_OUTER_BOUND('',#14368,.T.);
#8215=FACE_OUTER_BOUND('',#14369,.T.);
#8216=FACE_OUTER_BOUND('',#14370,.T.);
#8217=FACE_OUTER_BOUND('',#14371,.T.);
#8218=FACE_OUTER_BOUND('',#14372,.T.);
#8219=FACE_OUTER_BOUND('',#14373,.T.);
#8220=FACE_OUTER_BOUND('',#14374,.T.);
#8221=FACE_OUTER_BOUND('',#14375,.T.);
#8222=FACE_OUTER_BOUND('',#14376,.T.);
#8223=FACE_OUTER_BOUND('',#14377,.T.);
#8224=FACE_OUTER_BOUND('',#14378,.T.);
#8225=FACE_OUTER_BOUND('',#14379,.T.);
#8226=FACE_OUTER_BOUND('',#14380,.T.);
#8227=FACE_OUTER_BOUND('',#14381,.T.);
#8228=FACE_OUTER_BOUND('',#14382,.T.);
#8229=FACE_OUTER_BOUND('',#14383,.T.);
#8230=FACE_OUTER_BOUND('',#14384,.T.);
#8231=FACE_OUTER_BOUND('',#14385,.T.);
#8232=FACE_OUTER_BOUND('',#14386,.T.);
#8233=FACE_OUTER_BOUND('',#14387,.T.);
#8234=FACE_OUTER_BOUND('',#14388,.T.);
#8235=FACE_OUTER_BOUND('',#14389,.T.);
#8236=FACE_OUTER_BOUND('',#14390,.T.);
#8237=FACE_OUTER_BOUND('',#14391,.T.);
#8238=FACE_OUTER_BOUND('',#14392,.T.);
#8239=FACE_OUTER_BOUND('',#14393,.T.);
#8240=FACE_OUTER_BOUND('',#14394,.T.);
#8241=FACE_OUTER_BOUND('',#14395,.T.);
#8242=FACE_OUTER_BOUND('',#14396,.T.);
#8243=FACE_OUTER_BOUND('',#14397,.T.);
#8244=FACE_OUTER_BOUND('',#14398,.T.);
#8245=FACE_OUTER_BOUND('',#14399,.T.);
#8246=FACE_OUTER_BOUND('',#14400,.T.);
#8247=FACE_OUTER_BOUND('',#14401,.T.);
#8248=FACE_OUTER_BOUND('',#14402,.T.);
#8249=FACE_OUTER_BOUND('',#14403,.T.);
#8250=FACE_OUTER_BOUND('',#14404,.T.);
#8251=FACE_OUTER_BOUND('',#14405,.T.);
#8252=FACE_OUTER_BOUND('',#14406,.T.);
#8253=FACE_OUTER_BOUND('',#14407,.T.);
#8254=FACE_OUTER_BOUND('',#14408,.T.);
#8255=FACE_OUTER_BOUND('',#14409,.T.);
#8256=FACE_OUTER_BOUND('',#14410,.T.);
#8257=FACE_OUTER_BOUND('',#14411,.T.);
#8258=FACE_OUTER_BOUND('',#14412,.T.);
#8259=FACE_OUTER_BOUND('',#14413,.T.);
#8260=FACE_OUTER_BOUND('',#14414,.T.);
#8261=FACE_OUTER_BOUND('',#14415,.T.);
#8262=FACE_OUTER_BOUND('',#14416,.T.);
#8263=FACE_OUTER_BOUND('',#14417,.T.);
#8264=FACE_OUTER_BOUND('',#14418,.T.);
#8265=FACE_OUTER_BOUND('',#14419,.T.);
#8266=FACE_OUTER_BOUND('',#14420,.T.);
#8267=FACE_OUTER_BOUND('',#14421,.T.);
#8268=FACE_OUTER_BOUND('',#14422,.T.);
#8269=FACE_OUTER_BOUND('',#14423,.T.);
#8270=FACE_OUTER_BOUND('',#14424,.T.);
#8271=FACE_OUTER_BOUND('',#14425,.T.);
#8272=FACE_OUTER_BOUND('',#14426,.T.);
#8273=FACE_OUTER_BOUND('',#14427,.T.);
#8274=FACE_OUTER_BOUND('',#14428,.T.);
#8275=FACE_OUTER_BOUND('',#14429,.T.);
#8276=FACE_OUTER_BOUND('',#14430,.T.);
#8277=FACE_OUTER_BOUND('',#14431,.T.);
#8278=FACE_OUTER_BOUND('',#14432,.T.);
#8279=FACE_OUTER_BOUND('',#14433,.T.);
#8280=FACE_OUTER_BOUND('',#14434,.T.);
#8281=FACE_OUTER_BOUND('',#14435,.T.);
#8282=FACE_OUTER_BOUND('',#14436,.T.);
#8283=FACE_OUTER_BOUND('',#14437,.T.);
#8284=FACE_OUTER_BOUND('',#14438,.T.);
#8285=FACE_OUTER_BOUND('',#14439,.T.);
#8286=FACE_OUTER_BOUND('',#14440,.T.);
#8287=FACE_OUTER_BOUND('',#14441,.T.);
#8288=FACE_OUTER_BOUND('',#14442,.T.);
#8289=FACE_OUTER_BOUND('',#14443,.T.);
#8290=FACE_OUTER_BOUND('',#14444,.T.);
#8291=FACE_OUTER_BOUND('',#14445,.T.);
#8292=FACE_OUTER_BOUND('',#14446,.T.);
#8293=FACE_OUTER_BOUND('',#14447,.T.);
#8294=FACE_OUTER_BOUND('',#14448,.T.);
#8295=FACE_OUTER_BOUND('',#14449,.T.);
#8296=FACE_OUTER_BOUND('',#14450,.T.);
#8297=FACE_OUTER_BOUND('',#14451,.T.);
#8298=FACE_OUTER_BOUND('',#14452,.T.);
#8299=FACE_OUTER_BOUND('',#14453,.T.);
#8300=FACE_OUTER_BOUND('',#14454,.T.);
#8301=FACE_OUTER_BOUND('',#14455,.T.);
#8302=FACE_OUTER_BOUND('',#14456,.T.);
#8303=FACE_OUTER_BOUND('',#14457,.T.);
#8304=FACE_OUTER_BOUND('',#14458,.T.);
#8305=FACE_OUTER_BOUND('',#14459,.T.);
#8306=FACE_OUTER_BOUND('',#14460,.T.);
#8307=FACE_OUTER_BOUND('',#14461,.T.);
#8308=FACE_OUTER_BOUND('',#14462,.T.);
#8309=FACE_OUTER_BOUND('',#14463,.T.);
#8310=FACE_OUTER_BOUND('',#14464,.T.);
#8311=FACE_OUTER_BOUND('',#14465,.T.);
#8312=FACE_OUTER_BOUND('',#14466,.T.);
#8313=FACE_OUTER_BOUND('',#14467,.T.);
#8314=FACE_OUTER_BOUND('',#14468,.T.);
#8315=FACE_OUTER_BOUND('',#14469,.T.);
#8316=FACE_OUTER_BOUND('',#14470,.T.);
#8317=FACE_OUTER_BOUND('',#14471,.T.);
#8318=FACE_OUTER_BOUND('',#14472,.T.);
#8319=FACE_OUTER_BOUND('',#14473,.T.);
#8320=FACE_OUTER_BOUND('',#14474,.T.);
#8321=FACE_OUTER_BOUND('',#14476,.T.);
#8322=FACE_OUTER_BOUND('',#14477,.T.);
#8323=FACE_OUTER_BOUND('',#14478,.T.);
#8324=FACE_OUTER_BOUND('',#14479,.T.);
#8325=FACE_OUTER_BOUND('',#14480,.T.);
#8326=FACE_OUTER_BOUND('',#14481,.T.);
#8327=FACE_OUTER_BOUND('',#14483,.T.);
#8328=FACE_OUTER_BOUND('',#14485,.T.);
#8329=FACE_OUTER_BOUND('',#14486,.T.);
#8330=FACE_OUTER_BOUND('',#14487,.T.);
#8331=FACE_OUTER_BOUND('',#14488,.T.);
#8332=FACE_OUTER_BOUND('',#14489,.T.);
#8333=FACE_OUTER_BOUND('',#14490,.T.);
#8334=FACE_OUTER_BOUND('',#14491,.T.);
#8335=FACE_OUTER_BOUND('',#14492,.T.);
#8336=FACE_OUTER_BOUND('',#14493,.T.);
#8337=FACE_OUTER_BOUND('',#14494,.T.);
#8338=FACE_OUTER_BOUND('',#14495,.T.);
#8339=FACE_OUTER_BOUND('',#14496,.T.);
#8340=FACE_OUTER_BOUND('',#14497,.T.);
#8341=FACE_OUTER_BOUND('',#14498,.T.);
#8342=FACE_OUTER_BOUND('',#14499,.T.);
#8343=FACE_OUTER_BOUND('',#14500,.T.);
#8344=FACE_OUTER_BOUND('',#14501,.T.);
#8345=FACE_OUTER_BOUND('',#14502,.T.);
#8346=FACE_OUTER_BOUND('',#14503,.T.);
#8347=FACE_OUTER_BOUND('',#14504,.T.);
#8348=FACE_OUTER_BOUND('',#14505,.T.);
#8349=FACE_OUTER_BOUND('',#14506,.T.);
#8350=FACE_OUTER_BOUND('',#14507,.T.);
#8351=FACE_OUTER_BOUND('',#14508,.T.);
#8352=FACE_OUTER_BOUND('',#14509,.T.);
#8353=FACE_OUTER_BOUND('',#14510,.T.);
#8354=FACE_OUTER_BOUND('',#14511,.T.);
#8355=FACE_OUTER_BOUND('',#14512,.T.);
#8356=FACE_OUTER_BOUND('',#14513,.T.);
#8357=FACE_OUTER_BOUND('',#14514,.T.);
#8358=FACE_OUTER_BOUND('',#14515,.T.);
#8359=FACE_OUTER_BOUND('',#14516,.T.);
#8360=FACE_OUTER_BOUND('',#14517,.T.);
#8361=FACE_OUTER_BOUND('',#14518,.T.);
#8362=FACE_OUTER_BOUND('',#14519,.T.);
#8363=FACE_OUTER_BOUND('',#14520,.T.);
#8364=FACE_OUTER_BOUND('',#14521,.T.);
#8365=FACE_OUTER_BOUND('',#14522,.T.);
#8366=FACE_OUTER_BOUND('',#14523,.T.);
#8367=FACE_OUTER_BOUND('',#14524,.T.);
#8368=FACE_OUTER_BOUND('',#14525,.T.);
#8369=FACE_OUTER_BOUND('',#14526,.T.);
#8370=FACE_OUTER_BOUND('',#14527,.T.);
#8371=FACE_OUTER_BOUND('',#14528,.T.);
#8372=FACE_OUTER_BOUND('',#14529,.T.);
#8373=FACE_OUTER_BOUND('',#14530,.T.);
#8374=FACE_OUTER_BOUND('',#14531,.T.);
#8375=FACE_OUTER_BOUND('',#14532,.T.);
#8376=FACE_OUTER_BOUND('',#14533,.T.);
#8377=FACE_OUTER_BOUND('',#14534,.T.);
#8378=FACE_OUTER_BOUND('',#14535,.T.);
#8379=FACE_OUTER_BOUND('',#14536,.T.);
#8380=FACE_OUTER_BOUND('',#14537,.T.);
#8381=FACE_OUTER_BOUND('',#14538,.T.);
#8382=FACE_OUTER_BOUND('',#14539,.T.);
#8383=FACE_OUTER_BOUND('',#14540,.T.);
#8384=FACE_OUTER_BOUND('',#14541,.T.);
#8385=FACE_OUTER_BOUND('',#14542,.T.);
#8386=FACE_OUTER_BOUND('',#14543,.T.);
#8387=FACE_OUTER_BOUND('',#14544,.T.);
#8388=FACE_OUTER_BOUND('',#14545,.T.);
#8389=FACE_OUTER_BOUND('',#14546,.T.);
#8390=FACE_OUTER_BOUND('',#14547,.T.);
#8391=FACE_OUTER_BOUND('',#14548,.T.);
#8392=FACE_OUTER_BOUND('',#14549,.T.);
#8393=FACE_OUTER_BOUND('',#14550,.T.);
#8394=FACE_OUTER_BOUND('',#14551,.T.);
#8395=FACE_OUTER_BOUND('',#14552,.T.);
#8396=FACE_OUTER_BOUND('',#14553,.T.);
#8397=FACE_OUTER_BOUND('',#14554,.T.);
#8398=FACE_OUTER_BOUND('',#14555,.T.);
#8399=FACE_OUTER_BOUND('',#14556,.T.);
#8400=FACE_OUTER_BOUND('',#14557,.T.);
#8401=FACE_OUTER_BOUND('',#14558,.T.);
#8402=FACE_OUTER_BOUND('',#14559,.T.);
#8403=FACE_OUTER_BOUND('',#14560,.T.);
#8404=FACE_OUTER_BOUND('',#14561,.T.);
#8405=FACE_OUTER_BOUND('',#14562,.T.);
#8406=FACE_OUTER_BOUND('',#14563,.T.);
#8407=FACE_OUTER_BOUND('',#14564,.T.);
#8408=FACE_OUTER_BOUND('',#14565,.T.);
#8409=FACE_OUTER_BOUND('',#14566,.T.);
#8410=FACE_OUTER_BOUND('',#14567,.T.);
#8411=FACE_OUTER_BOUND('',#14568,.T.);
#8412=FACE_OUTER_BOUND('',#14569,.T.);
#8413=FACE_OUTER_BOUND('',#14570,.T.);
#8414=FACE_OUTER_BOUND('',#14571,.T.);
#8415=FACE_OUTER_BOUND('',#14572,.T.);
#8416=FACE_OUTER_BOUND('',#14573,.T.);
#8417=FACE_OUTER_BOUND('',#14574,.T.);
#8418=FACE_OUTER_BOUND('',#14575,.T.);
#8419=FACE_OUTER_BOUND('',#14576,.T.);
#8420=FACE_OUTER_BOUND('',#14577,.T.);
#8421=FACE_OUTER_BOUND('',#14578,.T.);
#8422=FACE_OUTER_BOUND('',#14579,.T.);
#8423=FACE_OUTER_BOUND('',#14580,.T.);
#8424=FACE_OUTER_BOUND('',#14581,.T.);
#8425=FACE_OUTER_BOUND('',#14582,.T.);
#8426=FACE_OUTER_BOUND('',#14583,.T.);
#8427=FACE_OUTER_BOUND('',#14584,.T.);
#8428=FACE_OUTER_BOUND('',#14585,.T.);
#8429=FACE_OUTER_BOUND('',#14586,.T.);
#8430=FACE_OUTER_BOUND('',#14587,.T.);
#8431=FACE_OUTER_BOUND('',#14588,.T.);
#8432=FACE_OUTER_BOUND('',#14589,.T.);
#8433=FACE_OUTER_BOUND('',#14590,.T.);
#8434=FACE_OUTER_BOUND('',#14591,.T.);
#8435=FACE_OUTER_BOUND('',#14592,.T.);
#8436=FACE_OUTER_BOUND('',#14593,.T.);
#8437=FACE_OUTER_BOUND('',#14594,.T.);
#8438=FACE_OUTER_BOUND('',#14595,.T.);
#8439=FACE_OUTER_BOUND('',#14596,.T.);
#8440=FACE_OUTER_BOUND('',#14597,.T.);
#8441=FACE_OUTER_BOUND('',#14598,.T.);
#8442=FACE_OUTER_BOUND('',#14599,.T.);
#8443=FACE_OUTER_BOUND('',#14600,.T.);
#8444=FACE_OUTER_BOUND('',#14601,.T.);
#8445=FACE_OUTER_BOUND('',#14602,.T.);
#8446=FACE_OUTER_BOUND('',#14603,.T.);
#8447=FACE_OUTER_BOUND('',#14604,.T.);
#8448=FACE_OUTER_BOUND('',#14605,.T.);
#8449=FACE_OUTER_BOUND('',#14606,.T.);
#8450=FACE_OUTER_BOUND('',#14607,.T.);
#8451=FACE_OUTER_BOUND('',#14608,.T.);
#8452=FACE_OUTER_BOUND('',#14609,.T.);
#8453=FACE_OUTER_BOUND('',#14610,.T.);
#8454=FACE_OUTER_BOUND('',#14611,.T.);
#8455=FACE_OUTER_BOUND('',#14612,.T.);
#8456=FACE_OUTER_BOUND('',#14613,.T.);
#8457=FACE_OUTER_BOUND('',#14614,.T.);
#8458=FACE_OUTER_BOUND('',#14615,.T.);
#8459=FACE_OUTER_BOUND('',#14616,.T.);
#8460=FACE_OUTER_BOUND('',#14617,.T.);
#8461=FACE_OUTER_BOUND('',#14618,.T.);
#8462=FACE_OUTER_BOUND('',#14619,.T.);
#8463=FACE_OUTER_BOUND('',#14620,.T.);
#8464=FACE_OUTER_BOUND('',#14621,.T.);
#8465=FACE_OUTER_BOUND('',#14622,.T.);
#8466=FACE_OUTER_BOUND('',#14623,.T.);
#8467=FACE_OUTER_BOUND('',#14624,.T.);
#8468=FACE_OUTER_BOUND('',#14625,.T.);
#8469=FACE_OUTER_BOUND('',#14626,.T.);
#8470=FACE_OUTER_BOUND('',#14627,.T.);
#8471=FACE_OUTER_BOUND('',#14628,.T.);
#8472=FACE_OUTER_BOUND('',#14629,.T.);
#8473=FACE_OUTER_BOUND('',#14630,.T.);
#8474=FACE_OUTER_BOUND('',#14631,.T.);
#8475=FACE_OUTER_BOUND('',#14632,.T.);
#8476=FACE_OUTER_BOUND('',#14633,.T.);
#8477=FACE_OUTER_BOUND('',#14634,.T.);
#8478=FACE_OUTER_BOUND('',#14635,.T.);
#8479=FACE_OUTER_BOUND('',#14636,.T.);
#8480=FACE_OUTER_BOUND('',#14637,.T.);
#8481=FACE_OUTER_BOUND('',#14638,.T.);
#8482=FACE_OUTER_BOUND('',#14639,.T.);
#8483=FACE_OUTER_BOUND('',#14640,.T.);
#8484=FACE_OUTER_BOUND('',#14641,.T.);
#8485=FACE_OUTER_BOUND('',#14642,.T.);
#8486=FACE_OUTER_BOUND('',#14643,.T.);
#8487=FACE_OUTER_BOUND('',#14644,.T.);
#8488=FACE_OUTER_BOUND('',#14645,.T.);
#8489=FACE_OUTER_BOUND('',#14646,.T.);
#8490=FACE_OUTER_BOUND('',#14647,.T.);
#8491=FACE_OUTER_BOUND('',#14648,.T.);
#8492=FACE_OUTER_BOUND('',#14649,.T.);
#8493=FACE_OUTER_BOUND('',#14650,.T.);
#8494=FACE_OUTER_BOUND('',#14651,.T.);
#8495=FACE_OUTER_BOUND('',#14652,.T.);
#8496=FACE_OUTER_BOUND('',#14653,.T.);
#8497=FACE_OUTER_BOUND('',#14654,.T.);
#8498=FACE_OUTER_BOUND('',#14655,.T.);
#8499=FACE_OUTER_BOUND('',#14656,.T.);
#8500=FACE_OUTER_BOUND('',#14657,.T.);
#8501=FACE_OUTER_BOUND('',#14658,.T.);
#8502=FACE_OUTER_BOUND('',#14659,.T.);
#8503=FACE_OUTER_BOUND('',#14660,.T.);
#8504=FACE_OUTER_BOUND('',#14661,.T.);
#8505=FACE_OUTER_BOUND('',#14662,.T.);
#8506=FACE_OUTER_BOUND('',#14663,.T.);
#8507=FACE_OUTER_BOUND('',#14664,.T.);
#8508=FACE_OUTER_BOUND('',#14665,.T.);
#8509=FACE_OUTER_BOUND('',#14666,.T.);
#8510=FACE_OUTER_BOUND('',#14667,.T.);
#8511=FACE_OUTER_BOUND('',#14668,.T.);
#8512=FACE_OUTER_BOUND('',#14669,.T.);
#8513=FACE_OUTER_BOUND('',#14670,.T.);
#8514=FACE_OUTER_BOUND('',#14671,.T.);
#8515=FACE_OUTER_BOUND('',#14672,.T.);
#8516=FACE_OUTER_BOUND('',#14673,.T.);
#8517=FACE_OUTER_BOUND('',#14674,.T.);
#8518=FACE_OUTER_BOUND('',#14675,.T.);
#8519=FACE_OUTER_BOUND('',#14676,.T.);
#8520=FACE_OUTER_BOUND('',#14677,.T.);
#8521=FACE_OUTER_BOUND('',#14678,.T.);
#8522=FACE_OUTER_BOUND('',#14679,.T.);
#8523=FACE_OUTER_BOUND('',#14680,.T.);
#8524=FACE_OUTER_BOUND('',#14681,.T.);
#8525=FACE_OUTER_BOUND('',#14682,.T.);
#8526=FACE_OUTER_BOUND('',#14683,.T.);
#8527=FACE_OUTER_BOUND('',#14684,.T.);
#8528=FACE_OUTER_BOUND('',#14685,.T.);
#8529=FACE_OUTER_BOUND('',#14686,.T.);
#8530=FACE_OUTER_BOUND('',#14687,.T.);
#8531=FACE_OUTER_BOUND('',#14688,.T.);
#8532=FACE_OUTER_BOUND('',#14689,.T.);
#8533=FACE_OUTER_BOUND('',#14690,.T.);
#8534=FACE_OUTER_BOUND('',#14691,.T.);
#8535=FACE_OUTER_BOUND('',#14692,.T.);
#8536=FACE_OUTER_BOUND('',#14693,.T.);
#8537=FACE_OUTER_BOUND('',#14694,.T.);
#8538=FACE_OUTER_BOUND('',#14695,.T.);
#8539=FACE_OUTER_BOUND('',#14696,.T.);
#8540=FACE_OUTER_BOUND('',#14697,.T.);
#8541=FACE_OUTER_BOUND('',#14698,.T.);
#8542=FACE_OUTER_BOUND('',#14699,.T.);
#8543=FACE_OUTER_BOUND('',#14700,.T.);
#8544=FACE_OUTER_BOUND('',#14701,.T.);
#8545=FACE_OUTER_BOUND('',#14702,.T.);
#8546=FACE_OUTER_BOUND('',#14703,.T.);
#8547=FACE_OUTER_BOUND('',#14704,.T.);
#8548=FACE_OUTER_BOUND('',#14705,.T.);
#8549=FACE_OUTER_BOUND('',#14706,.T.);
#8550=FACE_OUTER_BOUND('',#14707,.T.);
#8551=FACE_OUTER_BOUND('',#14708,.T.);
#8552=FACE_OUTER_BOUND('',#14709,.T.);
#8553=FACE_OUTER_BOUND('',#14710,.T.);
#8554=FACE_OUTER_BOUND('',#14711,.T.);
#8555=FACE_OUTER_BOUND('',#14712,.T.);
#8556=FACE_OUTER_BOUND('',#14713,.T.);
#8557=FACE_OUTER_BOUND('',#14714,.T.);
#8558=FACE_OUTER_BOUND('',#14715,.T.);
#8559=FACE_OUTER_BOUND('',#14716,.T.);
#8560=FACE_OUTER_BOUND('',#14717,.T.);
#8561=FACE_OUTER_BOUND('',#14718,.T.);
#8562=FACE_OUTER_BOUND('',#14719,.T.);
#8563=FACE_OUTER_BOUND('',#14720,.T.);
#8564=FACE_OUTER_BOUND('',#14721,.T.);
#8565=FACE_OUTER_BOUND('',#14722,.T.);
#8566=FACE_OUTER_BOUND('',#14723,.T.);
#8567=FACE_OUTER_BOUND('',#14724,.T.);
#8568=FACE_OUTER_BOUND('',#14725,.T.);
#8569=FACE_OUTER_BOUND('',#14726,.T.);
#8570=FACE_OUTER_BOUND('',#14727,.T.);
#8571=FACE_OUTER_BOUND('',#14728,.T.);
#8572=FACE_OUTER_BOUND('',#14729,.T.);
#8573=FACE_OUTER_BOUND('',#14730,.T.);
#8574=FACE_OUTER_BOUND('',#14731,.T.);
#8575=FACE_OUTER_BOUND('',#14732,.T.);
#8576=FACE_OUTER_BOUND('',#14733,.T.);
#8577=FACE_OUTER_BOUND('',#14734,.T.);
#8578=FACE_OUTER_BOUND('',#14735,.T.);
#8579=FACE_OUTER_BOUND('',#14736,.T.);
#8580=FACE_OUTER_BOUND('',#14737,.T.);
#8581=FACE_OUTER_BOUND('',#14738,.T.);
#8582=FACE_OUTER_BOUND('',#14739,.T.);
#8583=FACE_OUTER_BOUND('',#14740,.T.);
#8584=FACE_OUTER_BOUND('',#14741,.T.);
#8585=FACE_OUTER_BOUND('',#14742,.T.);
#8586=FACE_OUTER_BOUND('',#14743,.T.);
#8587=FACE_OUTER_BOUND('',#14744,.T.);
#8588=FACE_OUTER_BOUND('',#14745,.T.);
#8589=FACE_OUTER_BOUND('',#14746,.T.);
#8590=FACE_OUTER_BOUND('',#14747,.T.);
#8591=FACE_OUTER_BOUND('',#14748,.T.);
#8592=FACE_OUTER_BOUND('',#14749,.T.);
#8593=FACE_OUTER_BOUND('',#14750,.T.);
#8594=FACE_OUTER_BOUND('',#14751,.T.);
#8595=FACE_OUTER_BOUND('',#14752,.T.);
#8596=FACE_OUTER_BOUND('',#14753,.T.);
#8597=FACE_OUTER_BOUND('',#14754,.T.);
#8598=FACE_OUTER_BOUND('',#14755,.T.);
#8599=FACE_OUTER_BOUND('',#14756,.T.);
#8600=FACE_OUTER_BOUND('',#14757,.T.);
#8601=FACE_OUTER_BOUND('',#14758,.T.);
#8602=FACE_OUTER_BOUND('',#14759,.T.);
#8603=FACE_OUTER_BOUND('',#14760,.T.);
#8604=FACE_OUTER_BOUND('',#14761,.T.);
#8605=FACE_OUTER_BOUND('',#14762,.T.);
#8606=FACE_OUTER_BOUND('',#14763,.T.);
#8607=FACE_OUTER_BOUND('',#14764,.T.);
#8608=FACE_OUTER_BOUND('',#14765,.T.);
#8609=FACE_OUTER_BOUND('',#14766,.T.);
#8610=FACE_OUTER_BOUND('',#14767,.T.);
#8611=FACE_OUTER_BOUND('',#14768,.T.);
#8612=FACE_OUTER_BOUND('',#14769,.T.);
#8613=FACE_OUTER_BOUND('',#14770,.T.);
#8614=FACE_OUTER_BOUND('',#14771,.T.);
#8615=FACE_OUTER_BOUND('',#14772,.T.);
#8616=FACE_OUTER_BOUND('',#14773,.T.);
#8617=FACE_OUTER_BOUND('',#14774,.T.);
#8618=FACE_OUTER_BOUND('',#14775,.T.);
#8619=FACE_OUTER_BOUND('',#14776,.T.);
#8620=FACE_OUTER_BOUND('',#14777,.T.);
#8621=FACE_OUTER_BOUND('',#14778,.T.);
#8622=FACE_OUTER_BOUND('',#14779,.T.);
#8623=FACE_OUTER_BOUND('',#14780,.T.);
#8624=FACE_OUTER_BOUND('',#14781,.T.);
#8625=FACE_OUTER_BOUND('',#14782,.T.);
#8626=FACE_OUTER_BOUND('',#14783,.T.);
#8627=FACE_OUTER_BOUND('',#14784,.T.);
#8628=FACE_OUTER_BOUND('',#14785,.T.);
#8629=FACE_OUTER_BOUND('',#14786,.T.);
#8630=FACE_OUTER_BOUND('',#14787,.T.);
#8631=FACE_OUTER_BOUND('',#14788,.T.);
#8632=FACE_OUTER_BOUND('',#14789,.T.);
#8633=FACE_OUTER_BOUND('',#14790,.T.);
#8634=FACE_OUTER_BOUND('',#14791,.T.);
#8635=FACE_OUTER_BOUND('',#14792,.T.);
#8636=FACE_OUTER_BOUND('',#14793,.T.);
#8637=FACE_OUTER_BOUND('',#14794,.T.);
#8638=FACE_OUTER_BOUND('',#14795,.T.);
#8639=FACE_OUTER_BOUND('',#14796,.T.);
#8640=FACE_OUTER_BOUND('',#14797,.T.);
#8641=FACE_OUTER_BOUND('',#14798,.T.);
#8642=FACE_OUTER_BOUND('',#14799,.T.);
#8643=FACE_OUTER_BOUND('',#14800,.T.);
#8644=FACE_OUTER_BOUND('',#14801,.T.);
#8645=FACE_OUTER_BOUND('',#14802,.T.);
#8646=FACE_OUTER_BOUND('',#14803,.T.);
#8647=FACE_OUTER_BOUND('',#14804,.T.);
#8648=FACE_OUTER_BOUND('',#14805,.T.);
#8649=FACE_OUTER_BOUND('',#14806,.T.);
#8650=FACE_OUTER_BOUND('',#14807,.T.);
#8651=FACE_OUTER_BOUND('',#14808,.T.);
#8652=FACE_OUTER_BOUND('',#14809,.T.);
#8653=FACE_OUTER_BOUND('',#14810,.T.);
#8654=FACE_OUTER_BOUND('',#14811,.T.);
#8655=FACE_OUTER_BOUND('',#14812,.T.);
#8656=FACE_OUTER_BOUND('',#14813,.T.);
#8657=FACE_OUTER_BOUND('',#14814,.T.);
#8658=FACE_OUTER_BOUND('',#14815,.T.);
#8659=FACE_OUTER_BOUND('',#14816,.T.);
#8660=FACE_OUTER_BOUND('',#14817,.T.);
#8661=FACE_OUTER_BOUND('',#14818,.T.);
#8662=FACE_OUTER_BOUND('',#14819,.T.);
#8663=FACE_OUTER_BOUND('',#14820,.T.);
#8664=FACE_OUTER_BOUND('',#14821,.T.);
#8665=FACE_OUTER_BOUND('',#14822,.T.);
#8666=FACE_OUTER_BOUND('',#14823,.T.);
#8667=FACE_OUTER_BOUND('',#14824,.T.);
#8668=FACE_OUTER_BOUND('',#14825,.T.);
#8669=FACE_OUTER_BOUND('',#14826,.T.);
#8670=FACE_OUTER_BOUND('',#14827,.T.);
#8671=FACE_OUTER_BOUND('',#14828,.T.);
#8672=FACE_OUTER_BOUND('',#14829,.T.);
#8673=FACE_OUTER_BOUND('',#14830,.T.);
#8674=FACE_OUTER_BOUND('',#14831,.T.);
#8675=FACE_OUTER_BOUND('',#14832,.T.);
#8676=FACE_OUTER_BOUND('',#14833,.T.);
#8677=FACE_OUTER_BOUND('',#14834,.T.);
#8678=FACE_OUTER_BOUND('',#14835,.T.);
#8679=FACE_OUTER_BOUND('',#14836,.T.);
#8680=FACE_OUTER_BOUND('',#14837,.T.);
#8681=FACE_OUTER_BOUND('',#14838,.T.);
#8682=FACE_OUTER_BOUND('',#14839,.T.);
#8683=FACE_OUTER_BOUND('',#14840,.T.);
#8684=FACE_OUTER_BOUND('',#14841,.T.);
#8685=FACE_OUTER_BOUND('',#14842,.T.);
#8686=FACE_OUTER_BOUND('',#14843,.T.);
#8687=FACE_OUTER_BOUND('',#14844,.T.);
#8688=FACE_OUTER_BOUND('',#14845,.T.);
#8689=FACE_OUTER_BOUND('',#14846,.T.);
#8690=FACE_OUTER_BOUND('',#14847,.T.);
#8691=FACE_OUTER_BOUND('',#14848,.T.);
#8692=FACE_OUTER_BOUND('',#14849,.T.);
#8693=FACE_OUTER_BOUND('',#14850,.T.);
#8694=FACE_OUTER_BOUND('',#14851,.T.);
#8695=FACE_OUTER_BOUND('',#14852,.T.);
#8696=FACE_OUTER_BOUND('',#14853,.T.);
#8697=FACE_OUTER_BOUND('',#14854,.T.);
#8698=FACE_OUTER_BOUND('',#14855,.T.);
#8699=FACE_OUTER_BOUND('',#14856,.T.);
#8700=FACE_OUTER_BOUND('',#14857,.T.);
#8701=FACE_OUTER_BOUND('',#14858,.T.);
#8702=FACE_OUTER_BOUND('',#14859,.T.);
#8703=FACE_OUTER_BOUND('',#14860,.T.);
#8704=FACE_OUTER_BOUND('',#14861,.T.);
#8705=FACE_OUTER_BOUND('',#14862,.T.);
#8706=FACE_OUTER_BOUND('',#14863,.T.);
#8707=FACE_OUTER_BOUND('',#14864,.T.);
#8708=FACE_OUTER_BOUND('',#14865,.T.);
#8709=FACE_OUTER_BOUND('',#14866,.T.);
#8710=FACE_OUTER_BOUND('',#14867,.T.);
#8711=FACE_OUTER_BOUND('',#14868,.T.);
#8712=FACE_OUTER_BOUND('',#14869,.T.);
#8713=FACE_OUTER_BOUND('',#14870,.T.);
#8714=FACE_OUTER_BOUND('',#14871,.T.);
#8715=FACE_OUTER_BOUND('',#14872,.T.);
#8716=FACE_OUTER_BOUND('',#14873,.T.);
#8717=FACE_OUTER_BOUND('',#14874,.T.);
#8718=FACE_OUTER_BOUND('',#14875,.T.);
#8719=FACE_OUTER_BOUND('',#14876,.T.);
#8720=FACE_OUTER_BOUND('',#14877,.T.);
#8721=FACE_OUTER_BOUND('',#14878,.T.);
#8722=FACE_OUTER_BOUND('',#14879,.T.);
#8723=FACE_OUTER_BOUND('',#14880,.T.);
#8724=FACE_OUTER_BOUND('',#14881,.T.);
#8725=FACE_OUTER_BOUND('',#14882,.T.);
#8726=FACE_OUTER_BOUND('',#14883,.T.);
#8727=FACE_OUTER_BOUND('',#14884,.T.);
#8728=FACE_OUTER_BOUND('',#14885,.T.);
#8729=FACE_OUTER_BOUND('',#14886,.T.);
#8730=FACE_OUTER_BOUND('',#14887,.T.);
#8731=FACE_OUTER_BOUND('',#14888,.T.);
#8732=FACE_OUTER_BOUND('',#14889,.T.);
#8733=FACE_OUTER_BOUND('',#14890,.T.);
#8734=FACE_OUTER_BOUND('',#14891,.T.);
#8735=FACE_OUTER_BOUND('',#14892,.T.);
#8736=FACE_OUTER_BOUND('',#14893,.T.);
#8737=FACE_OUTER_BOUND('',#14894,.T.);
#8738=FACE_OUTER_BOUND('',#14895,.T.);
#8739=FACE_OUTER_BOUND('',#14896,.T.);
#8740=FACE_OUTER_BOUND('',#14897,.T.);
#8741=FACE_OUTER_BOUND('',#14898,.T.);
#8742=FACE_OUTER_BOUND('',#14899,.T.);
#8743=FACE_OUTER_BOUND('',#14900,.T.);
#8744=FACE_OUTER_BOUND('',#14901,.T.);
#8745=FACE_OUTER_BOUND('',#14902,.T.);
#8746=FACE_OUTER_BOUND('',#14903,.T.);
#8747=FACE_OUTER_BOUND('',#14904,.T.);
#8748=FACE_OUTER_BOUND('',#14905,.T.);
#8749=FACE_OUTER_BOUND('',#14906,.T.);
#8750=FACE_OUTER_BOUND('',#14907,.T.);
#8751=FACE_OUTER_BOUND('',#14908,.T.);
#8752=FACE_OUTER_BOUND('',#14909,.T.);
#8753=FACE_OUTER_BOUND('',#14910,.T.);
#8754=FACE_OUTER_BOUND('',#14911,.T.);
#8755=FACE_OUTER_BOUND('',#14912,.T.);
#8756=FACE_OUTER_BOUND('',#14913,.T.);
#8757=FACE_OUTER_BOUND('',#14914,.T.);
#8758=FACE_OUTER_BOUND('',#14915,.T.);
#8759=FACE_OUTER_BOUND('',#14916,.T.);
#8760=FACE_OUTER_BOUND('',#14917,.T.);
#8761=FACE_OUTER_BOUND('',#14918,.T.);
#8762=FACE_OUTER_BOUND('',#14919,.T.);
#8763=FACE_OUTER_BOUND('',#14920,.T.);
#8764=FACE_OUTER_BOUND('',#14921,.T.);
#8765=FACE_OUTER_BOUND('',#14922,.T.);
#8766=FACE_OUTER_BOUND('',#14923,.T.);
#8767=FACE_OUTER_BOUND('',#14924,.T.);
#8768=FACE_OUTER_BOUND('',#14925,.T.);
#8769=FACE_OUTER_BOUND('',#14926,.T.);
#8770=FACE_OUTER_BOUND('',#14927,.T.);
#8771=FACE_OUTER_BOUND('',#14928,.T.);
#8772=FACE_OUTER_BOUND('',#14929,.T.);
#8773=FACE_OUTER_BOUND('',#14930,.T.);
#8774=FACE_OUTER_BOUND('',#14931,.T.);
#8775=FACE_OUTER_BOUND('',#14932,.T.);
#8776=FACE_OUTER_BOUND('',#14933,.T.);
#8777=FACE_OUTER_BOUND('',#14934,.T.);
#8778=FACE_OUTER_BOUND('',#14935,.T.);
#8779=FACE_OUTER_BOUND('',#14936,.T.);
#8780=FACE_OUTER_BOUND('',#14937,.T.);
#8781=FACE_OUTER_BOUND('',#14938,.T.);
#8782=FACE_OUTER_BOUND('',#14939,.T.);
#8783=FACE_OUTER_BOUND('',#14940,.T.);
#8784=FACE_OUTER_BOUND('',#14941,.T.);
#8785=FACE_OUTER_BOUND('',#14942,.T.);
#8786=FACE_OUTER_BOUND('',#14943,.T.);
#8787=FACE_OUTER_BOUND('',#14944,.T.);
#8788=FACE_OUTER_BOUND('',#14945,.T.);
#8789=FACE_OUTER_BOUND('',#14946,.T.);
#8790=FACE_OUTER_BOUND('',#14947,.T.);
#8791=FACE_OUTER_BOUND('',#14948,.T.);
#8792=FACE_OUTER_BOUND('',#14949,.T.);
#8793=FACE_OUTER_BOUND('',#14950,.T.);
#8794=FACE_OUTER_BOUND('',#14951,.T.);
#8795=FACE_OUTER_BOUND('',#14952,.T.);
#8796=FACE_OUTER_BOUND('',#14953,.T.);
#8797=FACE_OUTER_BOUND('',#14954,.T.);
#8798=FACE_OUTER_BOUND('',#14955,.T.);
#8799=FACE_OUTER_BOUND('',#14956,.T.);
#8800=FACE_OUTER_BOUND('',#14957,.T.);
#8801=FACE_OUTER_BOUND('',#14958,.T.);
#8802=FACE_OUTER_BOUND('',#14959,.T.);
#8803=FACE_OUTER_BOUND('',#14960,.T.);
#8804=FACE_OUTER_BOUND('',#14961,.T.);
#8805=FACE_OUTER_BOUND('',#14962,.T.);
#8806=FACE_OUTER_BOUND('',#14963,.T.);
#8807=FACE_OUTER_BOUND('',#14964,.T.);
#8808=FACE_OUTER_BOUND('',#14965,.T.);
#8809=FACE_OUTER_BOUND('',#14966,.T.);
#8810=FACE_OUTER_BOUND('',#14967,.T.);
#8811=FACE_OUTER_BOUND('',#14968,.T.);
#8812=FACE_OUTER_BOUND('',#14969,.T.);
#8813=FACE_OUTER_BOUND('',#14970,.T.);
#8814=FACE_OUTER_BOUND('',#14971,.T.);
#8815=FACE_OUTER_BOUND('',#14972,.T.);
#8816=FACE_OUTER_BOUND('',#14973,.T.);
#8817=FACE_OUTER_BOUND('',#14974,.T.);
#8818=FACE_OUTER_BOUND('',#14975,.T.);
#8819=FACE_OUTER_BOUND('',#14976,.T.);
#8820=FACE_OUTER_BOUND('',#14977,.T.);
#8821=FACE_OUTER_BOUND('',#14978,.T.);
#8822=FACE_OUTER_BOUND('',#14979,.T.);
#8823=FACE_OUTER_BOUND('',#14980,.T.);
#8824=FACE_OUTER_BOUND('',#14981,.T.);
#8825=FACE_OUTER_BOUND('',#14982,.T.);
#8826=FACE_OUTER_BOUND('',#14983,.T.);
#8827=FACE_OUTER_BOUND('',#14984,.T.);
#8828=FACE_OUTER_BOUND('',#14985,.T.);
#8829=FACE_OUTER_BOUND('',#14986,.T.);
#8830=FACE_OUTER_BOUND('',#14987,.T.);
#8831=FACE_OUTER_BOUND('',#14988,.T.);
#8832=FACE_OUTER_BOUND('',#14989,.T.);
#8833=FACE_OUTER_BOUND('',#14990,.T.);
#8834=FACE_OUTER_BOUND('',#14991,.T.);
#8835=FACE_OUTER_BOUND('',#14992,.T.);
#8836=FACE_OUTER_BOUND('',#14993,.T.);
#8837=FACE_OUTER_BOUND('',#14994,.T.);
#8838=FACE_OUTER_BOUND('',#14995,.T.);
#8839=FACE_OUTER_BOUND('',#14996,.T.);
#8840=FACE_OUTER_BOUND('',#14997,.T.);
#8841=FACE_OUTER_BOUND('',#14998,.T.);
#8842=FACE_OUTER_BOUND('',#14999,.T.);
#8843=FACE_OUTER_BOUND('',#15000,.T.);
#8844=FACE_OUTER_BOUND('',#15001,.T.);
#8845=FACE_OUTER_BOUND('',#15002,.T.);
#8846=FACE_OUTER_BOUND('',#15003,.T.);
#8847=FACE_OUTER_BOUND('',#15004,.T.);
#8848=FACE_OUTER_BOUND('',#15005,.T.);
#8849=FACE_OUTER_BOUND('',#15006,.T.);
#8850=FACE_OUTER_BOUND('',#15007,.T.);
#8851=FACE_OUTER_BOUND('',#15008,.T.);
#8852=FACE_OUTER_BOUND('',#15009,.T.);
#8853=FACE_OUTER_BOUND('',#15010,.T.);
#8854=FACE_OUTER_BOUND('',#15011,.T.);
#8855=FACE_OUTER_BOUND('',#15012,.T.);
#8856=FACE_OUTER_BOUND('',#15013,.T.);
#8857=FACE_OUTER_BOUND('',#15014,.T.);
#8858=FACE_OUTER_BOUND('',#15015,.T.);
#8859=FACE_OUTER_BOUND('',#15016,.T.);
#8860=FACE_OUTER_BOUND('',#15017,.T.);
#8861=FACE_OUTER_BOUND('',#15018,.T.);
#8862=FACE_OUTER_BOUND('',#15019,.T.);
#8863=FACE_OUTER_BOUND('',#15020,.T.);
#8864=FACE_OUTER_BOUND('',#15021,.T.);
#8865=FACE_OUTER_BOUND('',#15022,.T.);
#8866=FACE_OUTER_BOUND('',#15023,.T.);
#8867=FACE_OUTER_BOUND('',#15024,.T.);
#8868=FACE_OUTER_BOUND('',#15025,.T.);
#8869=FACE_OUTER_BOUND('',#15026,.T.);
#8870=FACE_OUTER_BOUND('',#15027,.T.);
#8871=FACE_OUTER_BOUND('',#15028,.T.);
#8872=FACE_OUTER_BOUND('',#15029,.T.);
#8873=FACE_OUTER_BOUND('',#15030,.T.);
#8874=FACE_OUTER_BOUND('',#15031,.T.);
#8875=FACE_OUTER_BOUND('',#15032,.T.);
#8876=FACE_OUTER_BOUND('',#15033,.T.);
#8877=FACE_OUTER_BOUND('',#15034,.T.);
#8878=FACE_OUTER_BOUND('',#15035,.T.);
#8879=FACE_OUTER_BOUND('',#15036,.T.);
#8880=FACE_OUTER_BOUND('',#15037,.T.);
#8881=FACE_OUTER_BOUND('',#15038,.T.);
#8882=FACE_OUTER_BOUND('',#15039,.T.);
#8883=FACE_OUTER_BOUND('',#15040,.T.);
#8884=FACE_OUTER_BOUND('',#15041,.T.);
#8885=FACE_OUTER_BOUND('',#15042,.T.);
#8886=FACE_OUTER_BOUND('',#15043,.T.);
#8887=FACE_OUTER_BOUND('',#15044,.T.);
#8888=FACE_OUTER_BOUND('',#15045,.T.);
#8889=FACE_OUTER_BOUND('',#15046,.T.);
#8890=FACE_OUTER_BOUND('',#15047,.T.);
#8891=FACE_OUTER_BOUND('',#15048,.T.);
#8892=FACE_OUTER_BOUND('',#15049,.T.);
#8893=FACE_OUTER_BOUND('',#15050,.T.);
#8894=FACE_OUTER_BOUND('',#15051,.T.);
#8895=FACE_OUTER_BOUND('',#15052,.T.);
#8896=FACE_OUTER_BOUND('',#15053,.T.);
#8897=FACE_OUTER_BOUND('',#15054,.T.);
#8898=FACE_OUTER_BOUND('',#15055,.T.);
#8899=FACE_OUTER_BOUND('',#15056,.T.);
#8900=FACE_OUTER_BOUND('',#15057,.T.);
#8901=FACE_OUTER_BOUND('',#15058,.T.);
#8902=FACE_OUTER_BOUND('',#15059,.T.);
#8903=FACE_OUTER_BOUND('',#15060,.T.);
#8904=FACE_OUTER_BOUND('',#15061,.T.);
#8905=FACE_OUTER_BOUND('',#15062,.T.);
#8906=FACE_OUTER_BOUND('',#15063,.T.);
#8907=FACE_OUTER_BOUND('',#15064,.T.);
#8908=FACE_OUTER_BOUND('',#15065,.T.);
#8909=FACE_OUTER_BOUND('',#15066,.T.);
#8910=FACE_OUTER_BOUND('',#15067,.T.);
#8911=FACE_OUTER_BOUND('',#15068,.T.);
#8912=FACE_OUTER_BOUND('',#15069,.T.);
#8913=FACE_OUTER_BOUND('',#15070,.T.);
#8914=FACE_OUTER_BOUND('',#15071,.T.);
#8915=FACE_OUTER_BOUND('',#15072,.T.);
#8916=FACE_OUTER_BOUND('',#15073,.T.);
#8917=FACE_OUTER_BOUND('',#15074,.T.);
#8918=FACE_OUTER_BOUND('',#15075,.T.);
#8919=FACE_OUTER_BOUND('',#15076,.T.);
#8920=FACE_OUTER_BOUND('',#15077,.T.);
#8921=FACE_OUTER_BOUND('',#15078,.T.);
#8922=FACE_OUTER_BOUND('',#15079,.T.);
#8923=FACE_OUTER_BOUND('',#15080,.T.);
#8924=FACE_OUTER_BOUND('',#15081,.T.);
#8925=FACE_OUTER_BOUND('',#15082,.T.);
#8926=FACE_OUTER_BOUND('',#15083,.T.);
#8927=FACE_OUTER_BOUND('',#15084,.T.);
#8928=FACE_OUTER_BOUND('',#15085,.T.);
#8929=FACE_OUTER_BOUND('',#15086,.T.);
#8930=FACE_OUTER_BOUND('',#15087,.T.);
#8931=FACE_OUTER_BOUND('',#15088,.T.);
#8932=FACE_OUTER_BOUND('',#15089,.T.);
#8933=FACE_OUTER_BOUND('',#15090,.T.);
#8934=FACE_OUTER_BOUND('',#15091,.T.);
#8935=FACE_OUTER_BOUND('',#15092,.T.);
#8936=FACE_OUTER_BOUND('',#15093,.T.);
#8937=FACE_OUTER_BOUND('',#15094,.T.);
#8938=FACE_OUTER_BOUND('',#15095,.T.);
#8939=FACE_OUTER_BOUND('',#15096,.T.);
#8940=FACE_OUTER_BOUND('',#15097,.T.);
#8941=FACE_OUTER_BOUND('',#15098,.T.);
#8942=FACE_OUTER_BOUND('',#15099,.T.);
#8943=FACE_OUTER_BOUND('',#15100,.T.);
#8944=FACE_OUTER_BOUND('',#15101,.T.);
#8945=FACE_OUTER_BOUND('',#15102,.T.);
#8946=FACE_OUTER_BOUND('',#15103,.T.);
#8947=FACE_OUTER_BOUND('',#15104,.T.);
#8948=FACE_OUTER_BOUND('',#15105,.T.);
#8949=FACE_OUTER_BOUND('',#15106,.T.);
#8950=FACE_OUTER_BOUND('',#15107,.T.);
#8951=FACE_OUTER_BOUND('',#15108,.T.);
#8952=FACE_OUTER_BOUND('',#15109,.T.);
#8953=FACE_OUTER_BOUND('',#15110,.T.);
#8954=FACE_OUTER_BOUND('',#15111,.T.);
#8955=FACE_OUTER_BOUND('',#15112,.T.);
#8956=FACE_OUTER_BOUND('',#15113,.T.);
#8957=FACE_OUTER_BOUND('',#15114,.T.);
#8958=FACE_OUTER_BOUND('',#15115,.T.);
#8959=FACE_OUTER_BOUND('',#15116,.T.);
#8960=FACE_OUTER_BOUND('',#15117,.T.);
#8961=FACE_OUTER_BOUND('',#15118,.T.);
#8962=FACE_OUTER_BOUND('',#15119,.T.);
#8963=FACE_OUTER_BOUND('',#15120,.T.);
#8964=FACE_OUTER_BOUND('',#15121,.T.);
#8965=FACE_OUTER_BOUND('',#15122,.T.);
#8966=FACE_OUTER_BOUND('',#15123,.T.);
#8967=FACE_OUTER_BOUND('',#15124,.T.);
#8968=FACE_OUTER_BOUND('',#15125,.T.);
#8969=FACE_OUTER_BOUND('',#15126,.T.);
#8970=FACE_OUTER_BOUND('',#15127,.T.);
#8971=FACE_OUTER_BOUND('',#15128,.T.);
#8972=FACE_OUTER_BOUND('',#15129,.T.);
#8973=FACE_OUTER_BOUND('',#15130,.T.);
#8974=FACE_OUTER_BOUND('',#15131,.T.);
#8975=FACE_OUTER_BOUND('',#15132,.T.);
#8976=FACE_OUTER_BOUND('',#15133,.T.);
#8977=FACE_OUTER_BOUND('',#15134,.T.);
#8978=FACE_OUTER_BOUND('',#15135,.T.);
#8979=FACE_OUTER_BOUND('',#15136,.T.);
#8980=FACE_OUTER_BOUND('',#15137,.T.);
#8981=FACE_OUTER_BOUND('',#15138,.T.);
#8982=FACE_OUTER_BOUND('',#15139,.T.);
#8983=FACE_OUTER_BOUND('',#15140,.T.);
#8984=FACE_OUTER_BOUND('',#15141,.T.);
#8985=FACE_OUTER_BOUND('',#15142,.T.);
#8986=FACE_OUTER_BOUND('',#15143,.T.);
#8987=FACE_OUTER_BOUND('',#15144,.T.);
#8988=FACE_OUTER_BOUND('',#15145,.T.);
#8989=FACE_OUTER_BOUND('',#15146,.T.);
#8990=FACE_OUTER_BOUND('',#15147,.T.);
#8991=FACE_OUTER_BOUND('',#15148,.T.);
#8992=FACE_OUTER_BOUND('',#15149,.T.);
#8993=FACE_OUTER_BOUND('',#15150,.T.);
#8994=FACE_OUTER_BOUND('',#15151,.T.);
#8995=FACE_OUTER_BOUND('',#15152,.T.);
#8996=FACE_OUTER_BOUND('',#15153,.T.);
#8997=FACE_OUTER_BOUND('',#15154,.T.);
#8998=FACE_OUTER_BOUND('',#15155,.T.);
#8999=FACE_OUTER_BOUND('',#15156,.T.);
#9000=FACE_OUTER_BOUND('',#15157,.T.);
#9001=FACE_OUTER_BOUND('',#15158,.T.);
#9002=FACE_OUTER_BOUND('',#15159,.T.);
#9003=FACE_OUTER_BOUND('',#15160,.T.);
#9004=FACE_OUTER_BOUND('',#15161,.T.);
#9005=FACE_OUTER_BOUND('',#15162,.T.);
#9006=FACE_OUTER_BOUND('',#15163,.T.);
#9007=FACE_OUTER_BOUND('',#15164,.T.);
#9008=FACE_OUTER_BOUND('',#15165,.T.);
#9009=FACE_OUTER_BOUND('',#15166,.T.);
#9010=FACE_OUTER_BOUND('',#15167,.T.);
#9011=FACE_OUTER_BOUND('',#15168,.T.);
#9012=FACE_OUTER_BOUND('',#15169,.T.);
#9013=FACE_OUTER_BOUND('',#15170,.T.);
#9014=FACE_OUTER_BOUND('',#15171,.T.);
#9015=FACE_OUTER_BOUND('',#15172,.T.);
#9016=FACE_OUTER_BOUND('',#15173,.T.);
#9017=FACE_OUTER_BOUND('',#15174,.T.);
#9018=FACE_OUTER_BOUND('',#15175,.T.);
#9019=FACE_OUTER_BOUND('',#15176,.T.);
#9020=FACE_OUTER_BOUND('',#15177,.T.);
#9021=FACE_OUTER_BOUND('',#15178,.T.);
#9022=FACE_OUTER_BOUND('',#15179,.T.);
#9023=FACE_OUTER_BOUND('',#15180,.T.);
#9024=FACE_OUTER_BOUND('',#15181,.T.);
#9025=FACE_OUTER_BOUND('',#15182,.T.);
#9026=FACE_OUTER_BOUND('',#15183,.T.);
#9027=FACE_OUTER_BOUND('',#15184,.T.);
#9028=FACE_OUTER_BOUND('',#15185,.T.);
#9029=FACE_OUTER_BOUND('',#15186,.T.);
#9030=FACE_OUTER_BOUND('',#15187,.T.);
#9031=FACE_OUTER_BOUND('',#15188,.T.);
#9032=FACE_OUTER_BOUND('',#15189,.T.);
#9033=FACE_OUTER_BOUND('',#15190,.T.);
#9034=FACE_OUTER_BOUND('',#15191,.T.);
#9035=FACE_OUTER_BOUND('',#15192,.T.);
#9036=FACE_OUTER_BOUND('',#15193,.T.);
#9037=FACE_OUTER_BOUND('',#15194,.T.);
#9038=FACE_OUTER_BOUND('',#15195,.T.);
#9039=FACE_OUTER_BOUND('',#15196,.T.);
#9040=FACE_OUTER_BOUND('',#15197,.T.);
#9041=FACE_OUTER_BOUND('',#15198,.T.);
#9042=FACE_OUTER_BOUND('',#15199,.T.);
#9043=FACE_OUTER_BOUND('',#15200,.T.);
#9044=FACE_OUTER_BOUND('',#15201,.T.);
#9045=FACE_OUTER_BOUND('',#15202,.T.);
#9046=FACE_OUTER_BOUND('',#15203,.T.);
#9047=FACE_OUTER_BOUND('',#15204,.T.);
#9048=FACE_OUTER_BOUND('',#15205,.T.);
#9049=FACE_OUTER_BOUND('',#15206,.T.);
#9050=FACE_OUTER_BOUND('',#15207,.T.);
#9051=FACE_OUTER_BOUND('',#15208,.T.);
#9052=FACE_OUTER_BOUND('',#15209,.T.);
#9053=FACE_OUTER_BOUND('',#15210,.T.);
#9054=FACE_OUTER_BOUND('',#15211,.T.);
#9055=FACE_OUTER_BOUND('',#15212,.T.);
#9056=FACE_OUTER_BOUND('',#15213,.T.);
#9057=FACE_OUTER_BOUND('',#15214,.T.);
#9058=FACE_OUTER_BOUND('',#15215,.T.);
#9059=FACE_OUTER_BOUND('',#15216,.T.);
#9060=FACE_OUTER_BOUND('',#15217,.T.);
#9061=FACE_OUTER_BOUND('',#15218,.T.);
#9062=FACE_OUTER_BOUND('',#15219,.T.);
#9063=FACE_OUTER_BOUND('',#15220,.T.);
#9064=FACE_OUTER_BOUND('',#15221,.T.);
#9065=FACE_OUTER_BOUND('',#15222,.T.);
#9066=FACE_OUTER_BOUND('',#15223,.T.);
#9067=FACE_OUTER_BOUND('',#15224,.T.);
#9068=FACE_OUTER_BOUND('',#15225,.T.);
#9069=FACE_OUTER_BOUND('',#15226,.T.);
#9070=FACE_OUTER_BOUND('',#15227,.T.);
#9071=FACE_OUTER_BOUND('',#15228,.T.);
#9072=FACE_OUTER_BOUND('',#15229,.T.);
#9073=FACE_OUTER_BOUND('',#15230,.T.);
#9074=FACE_OUTER_BOUND('',#15231,.T.);
#9075=FACE_OUTER_BOUND('',#15232,.T.);
#9076=FACE_OUTER_BOUND('',#15233,.T.);
#9077=FACE_OUTER_BOUND('',#15234,.T.);
#9078=FACE_OUTER_BOUND('',#15235,.T.);
#9079=FACE_OUTER_BOUND('',#15236,.T.);
#9080=FACE_OUTER_BOUND('',#15237,.T.);
#9081=FACE_OUTER_BOUND('',#15238,.T.);
#9082=FACE_OUTER_BOUND('',#15239,.T.);
#9083=FACE_OUTER_BOUND('',#15240,.T.);
#9084=FACE_OUTER_BOUND('',#15241,.T.);
#9085=FACE_OUTER_BOUND('',#15242,.T.);
#9086=FACE_OUTER_BOUND('',#15243,.T.);
#9087=FACE_OUTER_BOUND('',#15244,.T.);
#9088=FACE_OUTER_BOUND('',#15245,.T.);
#9089=FACE_OUTER_BOUND('',#15246,.T.);
#9090=FACE_OUTER_BOUND('',#15247,.T.);
#9091=FACE_OUTER_BOUND('',#15248,.T.);
#9092=FACE_OUTER_BOUND('',#15249,.T.);
#9093=FACE_OUTER_BOUND('',#15250,.T.);
#9094=FACE_OUTER_BOUND('',#15251,.T.);
#9095=FACE_OUTER_BOUND('',#15252,.T.);
#9096=FACE_OUTER_BOUND('',#15253,.T.);
#9097=FACE_OUTER_BOUND('',#15254,.T.);
#9098=FACE_OUTER_BOUND('',#15255,.T.);
#9099=FACE_OUTER_BOUND('',#15256,.T.);
#9100=FACE_OUTER_BOUND('',#15257,.T.);
#9101=FACE_OUTER_BOUND('',#15258,.T.);
#9102=FACE_OUTER_BOUND('',#15259,.T.);
#9103=FACE_OUTER_BOUND('',#15260,.T.);
#9104=FACE_OUTER_BOUND('',#15261,.T.);
#9105=FACE_OUTER_BOUND('',#15262,.T.);
#9106=FACE_OUTER_BOUND('',#15263,.T.);
#9107=FACE_OUTER_BOUND('',#15264,.T.);
#9108=FACE_OUTER_BOUND('',#15265,.T.);
#9109=FACE_OUTER_BOUND('',#15266,.T.);
#9110=FACE_OUTER_BOUND('',#15267,.T.);
#9111=FACE_OUTER_BOUND('',#15268,.T.);
#9112=FACE_OUTER_BOUND('',#15269,.T.);
#9113=FACE_OUTER_BOUND('',#15270,.T.);
#9114=FACE_OUTER_BOUND('',#15271,.T.);
#9115=FACE_OUTER_BOUND('',#15272,.T.);
#9116=FACE_OUTER_BOUND('',#15273,.T.);
#9117=FACE_OUTER_BOUND('',#15274,.T.);
#9118=FACE_OUTER_BOUND('',#15275,.T.);
#9119=FACE_OUTER_BOUND('',#15276,.T.);
#9120=FACE_OUTER_BOUND('',#15277,.T.);
#9121=FACE_OUTER_BOUND('',#15278,.T.);
#9122=FACE_OUTER_BOUND('',#15279,.T.);
#9123=FACE_OUTER_BOUND('',#15280,.T.);
#9124=FACE_OUTER_BOUND('',#15281,.T.);
#9125=FACE_OUTER_BOUND('',#15282,.T.);
#9126=FACE_OUTER_BOUND('',#15283,.T.);
#9127=FACE_OUTER_BOUND('',#15284,.T.);
#9128=FACE_OUTER_BOUND('',#15285,.T.);
#9129=FACE_OUTER_BOUND('',#15286,.T.);
#9130=FACE_OUTER_BOUND('',#15287,.T.);
#9131=FACE_OUTER_BOUND('',#15288,.T.);
#9132=FACE_OUTER_BOUND('',#15289,.T.);
#9133=FACE_OUTER_BOUND('',#15290,.T.);
#9134=FACE_OUTER_BOUND('',#15291,.T.);
#9135=FACE_OUTER_BOUND('',#15292,.T.);
#9136=FACE_OUTER_BOUND('',#15293,.T.);
#9137=FACE_OUTER_BOUND('',#15294,.T.);
#9138=FACE_OUTER_BOUND('',#15295,.T.);
#9139=FACE_OUTER_BOUND('',#15296,.T.);
#9140=FACE_OUTER_BOUND('',#15297,.T.);
#9141=FACE_OUTER_BOUND('',#15298,.T.);
#9142=FACE_OUTER_BOUND('',#15299,.T.);
#9143=FACE_OUTER_BOUND('',#15300,.T.);
#9144=FACE_OUTER_BOUND('',#15301,.T.);
#9145=FACE_OUTER_BOUND('',#15302,.T.);
#9146=FACE_OUTER_BOUND('',#15303,.T.);
#9147=FACE_OUTER_BOUND('',#15304,.T.);
#9148=FACE_OUTER_BOUND('',#15305,.T.);
#9149=FACE_OUTER_BOUND('',#15306,.T.);
#9150=FACE_OUTER_BOUND('',#15307,.T.);
#9151=FACE_OUTER_BOUND('',#15308,.T.);
#9152=FACE_OUTER_BOUND('',#15309,.T.);
#9153=FACE_OUTER_BOUND('',#15310,.T.);
#9154=FACE_OUTER_BOUND('',#15311,.T.);
#9155=FACE_OUTER_BOUND('',#15312,.T.);
#9156=FACE_OUTER_BOUND('',#15313,.T.);
#9157=FACE_OUTER_BOUND('',#15314,.T.);
#9158=FACE_OUTER_BOUND('',#15315,.T.);
#9159=FACE_OUTER_BOUND('',#15316,.T.);
#9160=FACE_OUTER_BOUND('',#15317,.T.);
#9161=FACE_OUTER_BOUND('',#15318,.T.);
#9162=FACE_OUTER_BOUND('',#15319,.T.);
#9163=FACE_OUTER_BOUND('',#15320,.T.);
#9164=FACE_OUTER_BOUND('',#15321,.T.);
#9165=FACE_OUTER_BOUND('',#15322,.T.);
#9166=FACE_OUTER_BOUND('',#15323,.T.);
#9167=FACE_OUTER_BOUND('',#15324,.T.);
#9168=FACE_OUTER_BOUND('',#15325,.T.);
#9169=FACE_OUTER_BOUND('',#15326,.T.);
#9170=FACE_OUTER_BOUND('',#15327,.T.);
#9171=FACE_OUTER_BOUND('',#15328,.T.);
#9172=FACE_OUTER_BOUND('',#15329,.T.);
#9173=FACE_OUTER_BOUND('',#15330,.T.);
#9174=FACE_OUTER_BOUND('',#15331,.T.);
#9175=FACE_OUTER_BOUND('',#15332,.T.);
#9176=FACE_OUTER_BOUND('',#15333,.T.);
#9177=FACE_OUTER_BOUND('',#15334,.T.);
#9178=FACE_OUTER_BOUND('',#15335,.T.);
#9179=FACE_OUTER_BOUND('',#15336,.T.);
#9180=FACE_OUTER_BOUND('',#15337,.T.);
#9181=FACE_OUTER_BOUND('',#15338,.T.);
#9182=FACE_OUTER_BOUND('',#15339,.T.);
#9183=FACE_OUTER_BOUND('',#15340,.T.);
#9184=FACE_OUTER_BOUND('',#15341,.T.);
#9185=FACE_OUTER_BOUND('',#15342,.T.);
#9186=FACE_OUTER_BOUND('',#15343,.T.);
#9187=FACE_OUTER_BOUND('',#15344,.T.);
#9188=FACE_OUTER_BOUND('',#15345,.T.);
#9189=FACE_OUTER_BOUND('',#15346,.T.);
#9190=FACE_OUTER_BOUND('',#15347,.T.);
#9191=FACE_OUTER_BOUND('',#15348,.T.);
#9192=FACE_OUTER_BOUND('',#15349,.T.);
#9193=FACE_OUTER_BOUND('',#15350,.T.);
#9194=FACE_OUTER_BOUND('',#15351,.T.);
#9195=FACE_OUTER_BOUND('',#15352,.T.);
#9196=FACE_OUTER_BOUND('',#15353,.T.);
#9197=FACE_OUTER_BOUND('',#15354,.T.);
#9198=FACE_OUTER_BOUND('',#15355,.T.);
#9199=FACE_OUTER_BOUND('',#15356,.T.);
#9200=FACE_OUTER_BOUND('',#15357,.T.);
#9201=FACE_OUTER_BOUND('',#15358,.T.);
#9202=FACE_OUTER_BOUND('',#15359,.T.);
#9203=FACE_OUTER_BOUND('',#15360,.T.);
#9204=FACE_OUTER_BOUND('',#15361,.T.);
#9205=FACE_OUTER_BOUND('',#15362,.T.);
#9206=FACE_OUTER_BOUND('',#15363,.T.);
#9207=FACE_OUTER_BOUND('',#15364,.T.);
#9208=FACE_OUTER_BOUND('',#15365,.T.);
#9209=FACE_OUTER_BOUND('',#15366,.T.);
#9210=FACE_OUTER_BOUND('',#15367,.T.);
#9211=FACE_OUTER_BOUND('',#15368,.T.);
#9212=FACE_OUTER_BOUND('',#15369,.T.);
#9213=FACE_OUTER_BOUND('',#15370,.T.);
#9214=FACE_OUTER_BOUND('',#15371,.T.);
#9215=FACE_OUTER_BOUND('',#15372,.T.);
#9216=FACE_OUTER_BOUND('',#15373,.T.);
#9217=FACE_OUTER_BOUND('',#15374,.T.);
#9218=FACE_OUTER_BOUND('',#15375,.T.);
#9219=FACE_OUTER_BOUND('',#15376,.T.);
#9220=FACE_OUTER_BOUND('',#15377,.T.);
#9221=FACE_OUTER_BOUND('',#15378,.T.);
#9222=FACE_OUTER_BOUND('',#15379,.T.);
#9223=FACE_OUTER_BOUND('',#15380,.T.);
#9224=FACE_OUTER_BOUND('',#15381,.T.);
#9225=FACE_OUTER_BOUND('',#15382,.T.);
#9226=FACE_OUTER_BOUND('',#15383,.T.);
#9227=FACE_OUTER_BOUND('',#15384,.T.);
#9228=FACE_OUTER_BOUND('',#15385,.T.);
#9229=FACE_OUTER_BOUND('',#15386,.T.);
#9230=FACE_OUTER_BOUND('',#15387,.T.);
#9231=FACE_OUTER_BOUND('',#15388,.T.);
#9232=FACE_OUTER_BOUND('',#15389,.T.);
#9233=FACE_OUTER_BOUND('',#15390,.T.);
#9234=FACE_OUTER_BOUND('',#15391,.T.);
#9235=FACE_OUTER_BOUND('',#15392,.T.);
#9236=FACE_OUTER_BOUND('',#15393,.T.);
#9237=FACE_OUTER_BOUND('',#15394,.T.);
#9238=FACE_OUTER_BOUND('',#15395,.T.);
#9239=FACE_OUTER_BOUND('',#15396,.T.);
#9240=FACE_OUTER_BOUND('',#15397,.T.);
#9241=FACE_OUTER_BOUND('',#15398,.T.);
#9242=FACE_OUTER_BOUND('',#15399,.T.);
#9243=FACE_OUTER_BOUND('',#15400,.T.);
#9244=FACE_OUTER_BOUND('',#15401,.T.);
#9245=FACE_OUTER_BOUND('',#15402,.T.);
#9246=FACE_OUTER_BOUND('',#15403,.T.);
#9247=FACE_OUTER_BOUND('',#15404,.T.);
#9248=FACE_OUTER_BOUND('',#15405,.T.);
#9249=FACE_OUTER_BOUND('',#15406,.T.);
#9250=FACE_OUTER_BOUND('',#15407,.T.);
#9251=FACE_OUTER_BOUND('',#15408,.T.);
#9252=FACE_OUTER_BOUND('',#15409,.T.);
#9253=FACE_OUTER_BOUND('',#15410,.T.);
#9254=FACE_OUTER_BOUND('',#15411,.T.);
#9255=FACE_OUTER_BOUND('',#15412,.T.);
#9256=FACE_OUTER_BOUND('',#15413,.T.);
#9257=FACE_OUTER_BOUND('',#15414,.T.);
#9258=FACE_OUTER_BOUND('',#15415,.T.);
#9259=FACE_OUTER_BOUND('',#15416,.T.);
#9260=FACE_OUTER_BOUND('',#15417,.T.);
#9261=FACE_OUTER_BOUND('',#15418,.T.);
#9262=FACE_OUTER_BOUND('',#15419,.T.);
#9263=FACE_OUTER_BOUND('',#15420,.T.);
#9264=FACE_OUTER_BOUND('',#15421,.T.);
#9265=FACE_OUTER_BOUND('',#15422,.T.);
#9266=FACE_OUTER_BOUND('',#15423,.T.);
#9267=FACE_OUTER_BOUND('',#15424,.T.);
#9268=FACE_OUTER_BOUND('',#15425,.T.);
#9269=FACE_OUTER_BOUND('',#15426,.T.);
#9270=FACE_OUTER_BOUND('',#15427,.T.);
#9271=FACE_OUTER_BOUND('',#15428,.T.);
#9272=FACE_OUTER_BOUND('',#15429,.T.);
#9273=FACE_OUTER_BOUND('',#15430,.T.);
#9274=FACE_OUTER_BOUND('',#15431,.T.);
#9275=FACE_OUTER_BOUND('',#15432,.T.);
#9276=FACE_OUTER_BOUND('',#15433,.T.);
#9277=FACE_OUTER_BOUND('',#15434,.T.);
#9278=FACE_OUTER_BOUND('',#15435,.T.);
#9279=FACE_OUTER_BOUND('',#15436,.T.);
#9280=FACE_OUTER_BOUND('',#15437,.T.);
#9281=FACE_OUTER_BOUND('',#15438,.T.);
#9282=FACE_OUTER_BOUND('',#15439,.T.);
#9283=FACE_OUTER_BOUND('',#15440,.T.);
#9284=FACE_OUTER_BOUND('',#15441,.T.);
#9285=FACE_OUTER_BOUND('',#15442,.T.);
#9286=FACE_OUTER_BOUND('',#15443,.T.);
#9287=FACE_OUTER_BOUND('',#15444,.T.);
#9288=FACE_OUTER_BOUND('',#15445,.T.);
#9289=FACE_OUTER_BOUND('',#15446,.T.);
#9290=FACE_OUTER_BOUND('',#15447,.T.);
#9291=FACE_OUTER_BOUND('',#15448,.T.);
#9292=FACE_OUTER_BOUND('',#15449,.T.);
#9293=FACE_OUTER_BOUND('',#15450,.T.);
#9294=FACE_OUTER_BOUND('',#15451,.T.);
#9295=FACE_OUTER_BOUND('',#15452,.T.);
#9296=FACE_OUTER_BOUND('',#15453,.T.);
#9297=FACE_OUTER_BOUND('',#15454,.T.);
#9298=FACE_OUTER_BOUND('',#15455,.T.);
#9299=FACE_OUTER_BOUND('',#15456,.T.);
#9300=FACE_OUTER_BOUND('',#15457,.T.);
#9301=FACE_OUTER_BOUND('',#15458,.T.);
#9302=FACE_OUTER_BOUND('',#15459,.T.);
#9303=FACE_OUTER_BOUND('',#15460,.T.);
#9304=FACE_OUTER_BOUND('',#15461,.T.);
#9305=FACE_OUTER_BOUND('',#15462,.T.);
#9306=FACE_OUTER_BOUND('',#15463,.T.);
#9307=FACE_OUTER_BOUND('',#15464,.T.);
#9308=FACE_OUTER_BOUND('',#15465,.T.);
#9309=FACE_OUTER_BOUND('',#15466,.T.);
#9310=FACE_OUTER_BOUND('',#15467,.T.);
#9311=FACE_OUTER_BOUND('',#15468,.T.);
#9312=FACE_OUTER_BOUND('',#15469,.T.);
#9313=FACE_OUTER_BOUND('',#15470,.T.);
#9314=FACE_OUTER_BOUND('',#15471,.T.);
#9315=FACE_OUTER_BOUND('',#15472,.T.);
#9316=FACE_OUTER_BOUND('',#15473,.T.);
#9317=FACE_OUTER_BOUND('',#15474,.T.);
#9318=FACE_OUTER_BOUND('',#15475,.T.);
#9319=FACE_OUTER_BOUND('',#15476,.T.);
#9320=FACE_OUTER_BOUND('',#15477,.T.);
#9321=FACE_OUTER_BOUND('',#15478,.T.);
#9322=FACE_OUTER_BOUND('',#15479,.T.);
#9323=FACE_OUTER_BOUND('',#15480,.T.);
#9324=FACE_OUTER_BOUND('',#15481,.T.);
#9325=FACE_OUTER_BOUND('',#15482,.T.);
#9326=FACE_OUTER_BOUND('',#15483,.T.);
#9327=FACE_OUTER_BOUND('',#15484,.T.);
#9328=FACE_OUTER_BOUND('',#15485,.T.);
#9329=FACE_OUTER_BOUND('',#15486,.T.);
#9330=FACE_OUTER_BOUND('',#15487,.T.);
#9331=FACE_OUTER_BOUND('',#15488,.T.);
#9332=FACE_OUTER_BOUND('',#15489,.T.);
#9333=FACE_OUTER_BOUND('',#15490,.T.);
#9334=FACE_OUTER_BOUND('',#15491,.T.);
#9335=FACE_OUTER_BOUND('',#15492,.T.);
#9336=FACE_OUTER_BOUND('',#15493,.T.);
#9337=FACE_OUTER_BOUND('',#15494,.T.);
#9338=FACE_OUTER_BOUND('',#15495,.T.);
#9339=FACE_OUTER_BOUND('',#15496,.T.);
#9340=FACE_OUTER_BOUND('',#15497,.T.);
#9341=FACE_OUTER_BOUND('',#15498,.T.);
#9342=FACE_OUTER_BOUND('',#15499,.T.);
#9343=FACE_OUTER_BOUND('',#15500,.T.);
#9344=FACE_OUTER_BOUND('',#15501,.T.);
#9345=FACE_OUTER_BOUND('',#15502,.T.);
#9346=FACE_OUTER_BOUND('',#15503,.T.);
#9347=FACE_OUTER_BOUND('',#15504,.T.);
#9348=FACE_OUTER_BOUND('',#15505,.T.);
#9349=FACE_OUTER_BOUND('',#15506,.T.);
#9350=FACE_OUTER_BOUND('',#15507,.T.);
#9351=FACE_OUTER_BOUND('',#15508,.T.);
#9352=FACE_OUTER_BOUND('',#15509,.T.);
#9353=FACE_OUTER_BOUND('',#15510,.T.);
#9354=FACE_OUTER_BOUND('',#15511,.T.);
#9355=FACE_OUTER_BOUND('',#15512,.T.);
#9356=FACE_OUTER_BOUND('',#15513,.T.);
#9357=FACE_OUTER_BOUND('',#15514,.T.);
#9358=FACE_OUTER_BOUND('',#15515,.T.);
#9359=FACE_OUTER_BOUND('',#15516,.T.);
#9360=FACE_OUTER_BOUND('',#15517,.T.);
#9361=FACE_OUTER_BOUND('',#15518,.T.);
#9362=FACE_OUTER_BOUND('',#15519,.T.);
#9363=FACE_OUTER_BOUND('',#15520,.T.);
#9364=FACE_OUTER_BOUND('',#15521,.T.);
#9365=FACE_OUTER_BOUND('',#15522,.T.);
#9366=FACE_OUTER_BOUND('',#15523,.T.);
#9367=FACE_OUTER_BOUND('',#15524,.T.);
#9368=FACE_OUTER_BOUND('',#15525,.T.);
#9369=FACE_OUTER_BOUND('',#15526,.T.);
#9370=FACE_OUTER_BOUND('',#15527,.T.);
#9371=FACE_OUTER_BOUND('',#15528,.T.);
#9372=FACE_OUTER_BOUND('',#15529,.T.);
#9373=FACE_OUTER_BOUND('',#15530,.T.);
#9374=FACE_OUTER_BOUND('',#15531,.T.);
#9375=FACE_OUTER_BOUND('',#15532,.T.);
#9376=FACE_OUTER_BOUND('',#15533,.T.);
#9377=FACE_OUTER_BOUND('',#15534,.T.);
#9378=FACE_OUTER_BOUND('',#15535,.T.);
#9379=FACE_OUTER_BOUND('',#15536,.T.);
#9380=FACE_OUTER_BOUND('',#15537,.T.);
#9381=FACE_OUTER_BOUND('',#15538,.T.);
#9382=FACE_OUTER_BOUND('',#15539,.T.);
#9383=FACE_OUTER_BOUND('',#15540,.T.);
#9384=FACE_OUTER_BOUND('',#15541,.T.);
#9385=FACE_OUTER_BOUND('',#15542,.T.);
#9386=FACE_OUTER_BOUND('',#15543,.T.);
#9387=FACE_OUTER_BOUND('',#15544,.T.);
#9388=FACE_OUTER_BOUND('',#15545,.T.);
#9389=FACE_OUTER_BOUND('',#15546,.T.);
#9390=FACE_OUTER_BOUND('',#15547,.T.);
#9391=FACE_OUTER_BOUND('',#15548,.T.);
#9392=FACE_OUTER_BOUND('',#15549,.T.);
#9393=FACE_OUTER_BOUND('',#15550,.T.);
#9394=FACE_OUTER_BOUND('',#15551,.T.);
#9395=FACE_OUTER_BOUND('',#15552,.T.);
#9396=FACE_OUTER_BOUND('',#15553,.T.);
#9397=FACE_OUTER_BOUND('',#15554,.T.);
#9398=FACE_OUTER_BOUND('',#15555,.T.);
#9399=FACE_OUTER_BOUND('',#15556,.T.);
#9400=FACE_OUTER_BOUND('',#15557,.T.);
#9401=FACE_OUTER_BOUND('',#15558,.T.);
#9402=FACE_OUTER_BOUND('',#15559,.T.);
#9403=FACE_OUTER_BOUND('',#15560,.T.);
#9404=FACE_OUTER_BOUND('',#15561,.T.);
#9405=FACE_OUTER_BOUND('',#15562,.T.);
#9406=FACE_OUTER_BOUND('',#15563,.T.);
#9407=FACE_OUTER_BOUND('',#15564,.T.);
#9408=FACE_OUTER_BOUND('',#15565,.T.);
#9409=FACE_OUTER_BOUND('',#15566,.T.);
#9410=FACE_OUTER_BOUND('',#15567,.T.);
#9411=FACE_OUTER_BOUND('',#15568,.T.);
#9412=FACE_OUTER_BOUND('',#15569,.T.);
#9413=FACE_OUTER_BOUND('',#15570,.T.);
#9414=FACE_OUTER_BOUND('',#15571,.T.);
#9415=FACE_OUTER_BOUND('',#15572,.T.);
#9416=FACE_OUTER_BOUND('',#15573,.T.);
#9417=FACE_OUTER_BOUND('',#15574,.T.);
#9418=FACE_OUTER_BOUND('',#15575,.T.);
#9419=FACE_OUTER_BOUND('',#15576,.T.);
#9420=FACE_OUTER_BOUND('',#15577,.T.);
#9421=FACE_OUTER_BOUND('',#15578,.T.);
#9422=FACE_OUTER_BOUND('',#15579,.T.);
#9423=FACE_OUTER_BOUND('',#15580,.T.);
#9424=FACE_OUTER_BOUND('',#15581,.T.);
#9425=FACE_OUTER_BOUND('',#15582,.T.);
#9426=FACE_OUTER_BOUND('',#15583,.T.);
#9427=FACE_OUTER_BOUND('',#15584,.T.);
#9428=FACE_OUTER_BOUND('',#15585,.T.);
#9429=FACE_OUTER_BOUND('',#15586,.T.);
#9430=FACE_OUTER_BOUND('',#15587,.T.);
#9431=FACE_OUTER_BOUND('',#15588,.T.);
#9432=FACE_OUTER_BOUND('',#15589,.T.);
#9433=FACE_OUTER_BOUND('',#15590,.T.);
#9434=FACE_OUTER_BOUND('',#15591,.T.);
#9435=FACE_OUTER_BOUND('',#15592,.T.);
#9436=FACE_OUTER_BOUND('',#15593,.T.);
#9437=FACE_OUTER_BOUND('',#15594,.T.);
#9438=FACE_OUTER_BOUND('',#15595,.T.);
#9439=FACE_OUTER_BOUND('',#15596,.T.);
#9440=FACE_OUTER_BOUND('',#15597,.T.);
#9441=FACE_OUTER_BOUND('',#15598,.T.);
#9442=FACE_OUTER_BOUND('',#15599,.T.);
#9443=FACE_OUTER_BOUND('',#15600,.T.);
#9444=FACE_OUTER_BOUND('',#15601,.T.);
#9445=FACE_OUTER_BOUND('',#15602,.T.);
#9446=FACE_OUTER_BOUND('',#15603,.T.);
#9447=FACE_OUTER_BOUND('',#15604,.T.);
#9448=FACE_OUTER_BOUND('',#15605,.T.);
#9449=FACE_OUTER_BOUND('',#15606,.T.);
#9450=FACE_OUTER_BOUND('',#15607,.T.);
#9451=FACE_OUTER_BOUND('',#15608,.T.);
#9452=FACE_OUTER_BOUND('',#15609,.T.);
#9453=FACE_OUTER_BOUND('',#15610,.T.);
#9454=FACE_OUTER_BOUND('',#15611,.T.);
#9455=FACE_OUTER_BOUND('',#15612,.T.);
#9456=FACE_OUTER_BOUND('',#15613,.T.);
#9457=FACE_OUTER_BOUND('',#15614,.T.);
#9458=FACE_OUTER_BOUND('',#15615,.T.);
#9459=FACE_OUTER_BOUND('',#15616,.T.);
#9460=FACE_OUTER_BOUND('',#15617,.T.);
#9461=FACE_OUTER_BOUND('',#15618,.T.);
#9462=FACE_OUTER_BOUND('',#15619,.T.);
#9463=FACE_OUTER_BOUND('',#15620,.T.);
#9464=FACE_OUTER_BOUND('',#15621,.T.);
#9465=FACE_OUTER_BOUND('',#15622,.T.);
#9466=FACE_OUTER_BOUND('',#15623,.T.);
#9467=FACE_OUTER_BOUND('',#15624,.T.);
#9468=FACE_OUTER_BOUND('',#15625,.T.);
#9469=FACE_OUTER_BOUND('',#15626,.T.);
#9470=FACE_OUTER_BOUND('',#15627,.T.);
#9471=FACE_OUTER_BOUND('',#15628,.T.);
#9472=FACE_OUTER_BOUND('',#15629,.T.);
#9473=FACE_OUTER_BOUND('',#15630,.T.);
#9474=FACE_OUTER_BOUND('',#15631,.T.);
#9475=FACE_OUTER_BOUND('',#15632,.T.);
#9476=FACE_OUTER_BOUND('',#15633,.T.);
#9477=FACE_OUTER_BOUND('',#15634,.T.);
#9478=FACE_OUTER_BOUND('',#15635,.T.);
#9479=FACE_OUTER_BOUND('',#15636,.T.);
#9480=FACE_OUTER_BOUND('',#15637,.T.);
#9481=FACE_OUTER_BOUND('',#15638,.T.);
#9482=FACE_OUTER_BOUND('',#15639,.T.);
#9483=FACE_OUTER_BOUND('',#15640,.T.);
#9484=FACE_OUTER_BOUND('',#15641,.T.);
#9485=FACE_OUTER_BOUND('',#15642,.T.);
#9486=FACE_OUTER_BOUND('',#15643,.T.);
#9487=FACE_OUTER_BOUND('',#15644,.T.);
#9488=FACE_OUTER_BOUND('',#15645,.T.);
#9489=FACE_OUTER_BOUND('',#15646,.T.);
#9490=FACE_OUTER_BOUND('',#15647,.T.);
#9491=FACE_OUTER_BOUND('',#15648,.T.);
#9492=FACE_OUTER_BOUND('',#15649,.T.);
#9493=FACE_OUTER_BOUND('',#15650,.T.);
#9494=FACE_OUTER_BOUND('',#15651,.T.);
#9495=FACE_OUTER_BOUND('',#15652,.T.);
#9496=FACE_OUTER_BOUND('',#15653,.T.);
#9497=FACE_OUTER_BOUND('',#15654,.T.);
#9498=FACE_OUTER_BOUND('',#15655,.T.);
#9499=FACE_OUTER_BOUND('',#15656,.T.);
#9500=FACE_OUTER_BOUND('',#15657,.T.);
#9501=FACE_OUTER_BOUND('',#15658,.T.);
#9502=FACE_OUTER_BOUND('',#15659,.T.);
#9503=FACE_OUTER_BOUND('',#15660,.T.);
#9504=FACE_OUTER_BOUND('',#15661,.T.);
#9505=FACE_OUTER_BOUND('',#15662,.T.);
#9506=FACE_OUTER_BOUND('',#15663,.T.);
#9507=FACE_OUTER_BOUND('',#15664,.T.);
#9508=FACE_OUTER_BOUND('',#15665,.T.);
#9509=FACE_OUTER_BOUND('',#15666,.T.);
#9510=FACE_OUTER_BOUND('',#15667,.T.);
#9511=FACE_OUTER_BOUND('',#15668,.T.);
#9512=FACE_OUTER_BOUND('',#15669,.T.);
#9513=FACE_OUTER_BOUND('',#15670,.T.);
#9514=FACE_OUTER_BOUND('',#15671,.T.);
#9515=FACE_OUTER_BOUND('',#15672,.T.);
#9516=FACE_OUTER_BOUND('',#15673,.T.);
#9517=FACE_OUTER_BOUND('',#15674,.T.);
#9518=FACE_OUTER_BOUND('',#15675,.T.);
#9519=FACE_OUTER_BOUND('',#15676,.T.);
#9520=FACE_OUTER_BOUND('',#15677,.T.);
#9521=FACE_OUTER_BOUND('',#15678,.T.);
#9522=FACE_OUTER_BOUND('',#15679,.T.);
#9523=FACE_OUTER_BOUND('',#15680,.T.);
#9524=FACE_OUTER_BOUND('',#15681,.T.);
#9525=FACE_OUTER_BOUND('',#15682,.T.);
#9526=FACE_OUTER_BOUND('',#15683,.T.);
#9527=FACE_OUTER_BOUND('',#15684,.T.);
#9528=FACE_OUTER_BOUND('',#15685,.T.);
#9529=FACE_OUTER_BOUND('',#15686,.T.);
#9530=FACE_OUTER_BOUND('',#15687,.T.);
#9531=FACE_OUTER_BOUND('',#15688,.T.);
#9532=FACE_OUTER_BOUND('',#15689,.T.);
#9533=FACE_OUTER_BOUND('',#15690,.T.);
#9534=FACE_OUTER_BOUND('',#15691,.T.);
#9535=FACE_OUTER_BOUND('',#15692,.T.);
#9536=FACE_OUTER_BOUND('',#15693,.T.);
#9537=FACE_OUTER_BOUND('',#15694,.T.);
#9538=FACE_OUTER_BOUND('',#15695,.T.);
#9539=FACE_OUTER_BOUND('',#15696,.T.);
#9540=FACE_OUTER_BOUND('',#15697,.T.);
#9541=FACE_OUTER_BOUND('',#15698,.T.);
#9542=FACE_OUTER_BOUND('',#15699,.T.);
#9543=FACE_OUTER_BOUND('',#15700,.T.);
#9544=FACE_OUTER_BOUND('',#15701,.T.);
#9545=FACE_OUTER_BOUND('',#15702,.T.);
#9546=FACE_OUTER_BOUND('',#15703,.T.);
#9547=FACE_OUTER_BOUND('',#15704,.T.);
#9548=FACE_OUTER_BOUND('',#15705,.T.);
#9549=FACE_OUTER_BOUND('',#15706,.T.);
#9550=FACE_OUTER_BOUND('',#15707,.T.);
#9551=FACE_OUTER_BOUND('',#15708,.T.);
#9552=FACE_OUTER_BOUND('',#15709,.T.);
#9553=FACE_OUTER_BOUND('',#15710,.T.);
#9554=FACE_OUTER_BOUND('',#15711,.T.);
#9555=FACE_OUTER_BOUND('',#15712,.T.);
#9556=FACE_OUTER_BOUND('',#15713,.T.);
#9557=FACE_OUTER_BOUND('',#15714,.T.);
#9558=FACE_OUTER_BOUND('',#15715,.T.);
#9559=FACE_OUTER_BOUND('',#15716,.T.);
#9560=FACE_OUTER_BOUND('',#15717,.T.);
#9561=FACE_OUTER_BOUND('',#15718,.T.);
#9562=FACE_OUTER_BOUND('',#15719,.T.);
#9563=FACE_OUTER_BOUND('',#15720,.T.);
#9564=FACE_OUTER_BOUND('',#15721,.T.);
#9565=FACE_OUTER_BOUND('',#15722,.T.);
#9566=FACE_OUTER_BOUND('',#15723,.T.);
#9567=FACE_OUTER_BOUND('',#15724,.T.);
#9568=FACE_OUTER_BOUND('',#15725,.T.);
#9569=FACE_OUTER_BOUND('',#15726,.T.);
#9570=FACE_OUTER_BOUND('',#15727,.T.);
#9571=FACE_OUTER_BOUND('',#15728,.T.);
#9572=FACE_OUTER_BOUND('',#15729,.T.);
#9573=FACE_OUTER_BOUND('',#15730,.T.);
#9574=FACE_OUTER_BOUND('',#15731,.T.);
#9575=FACE_OUTER_BOUND('',#15732,.T.);
#9576=FACE_OUTER_BOUND('',#15733,.T.);
#9577=FACE_OUTER_BOUND('',#15734,.T.);
#9578=FACE_OUTER_BOUND('',#15735,.T.);
#9579=FACE_OUTER_BOUND('',#15736,.T.);
#9580=FACE_OUTER_BOUND('',#15737,.T.);
#9581=FACE_OUTER_BOUND('',#15738,.T.);
#9582=FACE_OUTER_BOUND('',#15739,.T.);
#9583=FACE_OUTER_BOUND('',#15740,.T.);
#9584=FACE_OUTER_BOUND('',#15741,.T.);
#9585=FACE_OUTER_BOUND('',#15742,.T.);
#9586=FACE_OUTER_BOUND('',#15743,.T.);
#9587=FACE_OUTER_BOUND('',#15744,.T.);
#9588=FACE_OUTER_BOUND('',#15745,.T.);
#9589=FACE_OUTER_BOUND('',#15746,.T.);
#9590=FACE_OUTER_BOUND('',#15747,.T.);
#9591=FACE_OUTER_BOUND('',#15748,.T.);
#9592=FACE_OUTER_BOUND('',#15749,.T.);
#9593=FACE_OUTER_BOUND('',#15750,.T.);
#9594=FACE_OUTER_BOUND('',#15751,.T.);
#9595=FACE_OUTER_BOUND('',#15752,.T.);
#9596=FACE_OUTER_BOUND('',#15753,.T.);
#9597=FACE_OUTER_BOUND('',#15754,.T.);
#9598=FACE_OUTER_BOUND('',#15755,.T.);
#9599=FACE_OUTER_BOUND('',#15756,.T.);
#9600=FACE_OUTER_BOUND('',#15757,.T.);
#9601=FACE_OUTER_BOUND('',#15758,.T.);
#9602=FACE_OUTER_BOUND('',#15759,.T.);
#9603=FACE_OUTER_BOUND('',#15760,.T.);
#9604=FACE_OUTER_BOUND('',#15761,.T.);
#9605=FACE_OUTER_BOUND('',#15762,.T.);
#9606=FACE_OUTER_BOUND('',#15763,.T.);
#9607=FACE_OUTER_BOUND('',#15764,.T.);
#9608=FACE_OUTER_BOUND('',#15765,.T.);
#9609=FACE_OUTER_BOUND('',#15766,.T.);
#9610=FACE_OUTER_BOUND('',#15767,.T.);
#9611=FACE_OUTER_BOUND('',#15768,.T.);
#9612=FACE_OUTER_BOUND('',#15769,.T.);
#9613=FACE_OUTER_BOUND('',#15770,.T.);
#9614=FACE_OUTER_BOUND('',#15771,.T.);
#9615=FACE_OUTER_BOUND('',#15772,.T.);
#9616=FACE_OUTER_BOUND('',#15773,.T.);
#9617=FACE_OUTER_BOUND('',#15774,.T.);
#9618=FACE_OUTER_BOUND('',#15775,.T.);
#9619=FACE_OUTER_BOUND('',#15776,.T.);
#9620=FACE_OUTER_BOUND('',#15777,.T.);
#9621=FACE_OUTER_BOUND('',#15778,.T.);
#9622=FACE_OUTER_BOUND('',#15779,.T.);
#9623=FACE_OUTER_BOUND('',#15780,.T.);
#9624=FACE_OUTER_BOUND('',#15781,.T.);
#9625=FACE_OUTER_BOUND('',#15782,.T.);
#9626=FACE_OUTER_BOUND('',#15783,.T.);
#9627=FACE_OUTER_BOUND('',#15784,.T.);
#9628=FACE_OUTER_BOUND('',#15785,.T.);
#9629=FACE_OUTER_BOUND('',#15786,.T.);
#9630=FACE_OUTER_BOUND('',#15787,.T.);
#9631=FACE_OUTER_BOUND('',#15788,.T.);
#9632=FACE_OUTER_BOUND('',#15789,.T.);
#9633=FACE_OUTER_BOUND('',#15790,.T.);
#9634=FACE_OUTER_BOUND('',#15791,.T.);
#9635=FACE_OUTER_BOUND('',#15792,.T.);
#9636=FACE_OUTER_BOUND('',#15793,.T.);
#9637=FACE_OUTER_BOUND('',#15794,.T.);
#9638=FACE_OUTER_BOUND('',#15795,.T.);
#9639=FACE_OUTER_BOUND('',#15796,.T.);
#9640=FACE_OUTER_BOUND('',#15797,.T.);
#9641=FACE_OUTER_BOUND('',#15798,.T.);
#9642=FACE_OUTER_BOUND('',#15799,.T.);
#9643=FACE_OUTER_BOUND('',#15800,.T.);
#9644=FACE_OUTER_BOUND('',#15801,.T.);
#9645=FACE_OUTER_BOUND('',#15802,.T.);
#9646=FACE_OUTER_BOUND('',#15803,.T.);
#9647=FACE_OUTER_BOUND('',#15804,.T.);
#9648=FACE_OUTER_BOUND('',#15805,.T.);
#9649=FACE_OUTER_BOUND('',#15806,.T.);
#9650=FACE_OUTER_BOUND('',#15807,.T.);
#9651=FACE_OUTER_BOUND('',#15808,.T.);
#9652=FACE_OUTER_BOUND('',#15809,.T.);
#9653=FACE_OUTER_BOUND('',#15810,.T.);
#9654=FACE_OUTER_BOUND('',#15811,.T.);
#9655=FACE_OUTER_BOUND('',#15812,.T.);
#9656=FACE_OUTER_BOUND('',#15813,.T.);
#9657=FACE_OUTER_BOUND('',#15814,.T.);
#9658=FACE_OUTER_BOUND('',#15815,.T.);
#9659=FACE_OUTER_BOUND('',#15816,.T.);
#9660=FACE_OUTER_BOUND('',#15817,.T.);
#9661=FACE_OUTER_BOUND('',#15818,.T.);
#9662=FACE_OUTER_BOUND('',#15819,.T.);
#9663=FACE_OUTER_BOUND('',#15820,.T.);
#9664=FACE_OUTER_BOUND('',#15821,.T.);
#9665=FACE_OUTER_BOUND('',#15822,.T.);
#9666=FACE_OUTER_BOUND('',#15823,.T.);
#9667=FACE_OUTER_BOUND('',#15824,.T.);
#9668=FACE_OUTER_BOUND('',#15825,.T.);
#9669=FACE_OUTER_BOUND('',#15826,.T.);
#9670=FACE_OUTER_BOUND('',#15827,.T.);
#9671=FACE_OUTER_BOUND('',#15828,.T.);
#9672=FACE_OUTER_BOUND('',#15829,.T.);
#9673=FACE_OUTER_BOUND('',#15830,.T.);
#9674=FACE_OUTER_BOUND('',#15831,.T.);
#9675=FACE_OUTER_BOUND('',#15832,.T.);
#9676=FACE_OUTER_BOUND('',#15833,.T.);
#9677=FACE_OUTER_BOUND('',#15834,.T.);
#9678=FACE_OUTER_BOUND('',#15835,.T.);
#9679=FACE_OUTER_BOUND('',#15836,.T.);
#9680=FACE_OUTER_BOUND('',#15837,.T.);
#9681=FACE_OUTER_BOUND('',#15838,.T.);
#9682=FACE_OUTER_BOUND('',#15839,.T.);
#9683=FACE_OUTER_BOUND('',#15840,.T.);
#9684=FACE_OUTER_BOUND('',#15841,.T.);
#9685=FACE_OUTER_BOUND('',#15842,.T.);
#9686=FACE_OUTER_BOUND('',#15843,.T.);
#9687=FACE_OUTER_BOUND('',#15844,.T.);
#9688=FACE_OUTER_BOUND('',#15845,.T.);
#9689=FACE_OUTER_BOUND('',#15846,.T.);
#9690=FACE_OUTER_BOUND('',#15847,.T.);
#9691=FACE_OUTER_BOUND('',#15848,.T.);
#9692=FACE_OUTER_BOUND('',#15849,.T.);
#9693=FACE_OUTER_BOUND('',#15850,.T.);
#9694=FACE_OUTER_BOUND('',#15851,.T.);
#9695=FACE_OUTER_BOUND('',#15852,.T.);
#9696=FACE_OUTER_BOUND('',#15853,.T.);
#9697=FACE_OUTER_BOUND('',#15854,.T.);
#9698=FACE_OUTER_BOUND('',#15855,.T.);
#9699=FACE_OUTER_BOUND('',#15856,.T.);
#9700=FACE_OUTER_BOUND('',#15857,.T.);
#9701=FACE_OUTER_BOUND('',#15858,.T.);
#9702=FACE_OUTER_BOUND('',#15859,.T.);
#9703=FACE_OUTER_BOUND('',#15860,.T.);
#9704=FACE_OUTER_BOUND('',#15861,.T.);
#9705=FACE_OUTER_BOUND('',#15862,.T.);
#9706=FACE_OUTER_BOUND('',#15863,.T.);
#9707=FACE_OUTER_BOUND('',#15864,.T.);
#9708=FACE_OUTER_BOUND('',#15865,.T.);
#9709=FACE_OUTER_BOUND('',#15866,.T.);
#9710=FACE_OUTER_BOUND('',#15867,.T.);
#9711=FACE_OUTER_BOUND('',#15868,.T.);
#9712=FACE_OUTER_BOUND('',#15869,.T.);
#9713=FACE_OUTER_BOUND('',#15870,.T.);
#9714=FACE_OUTER_BOUND('',#15871,.T.);
#9715=FACE_OUTER_BOUND('',#15872,.T.);
#9716=FACE_OUTER_BOUND('',#15873,.T.);
#9717=FACE_OUTER_BOUND('',#15874,.T.);
#9718=FACE_OUTER_BOUND('',#15875,.T.);
#9719=FACE_OUTER_BOUND('',#15876,.T.);
#9720=FACE_OUTER_BOUND('',#15877,.T.);
#9721=FACE_OUTER_BOUND('',#15878,.T.);
#9722=FACE_OUTER_BOUND('',#15879,.T.);
#9723=FACE_OUTER_BOUND('',#15880,.T.);
#9724=FACE_OUTER_BOUND('',#15881,.T.);
#9725=FACE_OUTER_BOUND('',#15882,.T.);
#9726=FACE_OUTER_BOUND('',#15883,.T.);
#9727=FACE_OUTER_BOUND('',#15884,.T.);
#9728=FACE_OUTER_BOUND('',#15885,.T.);
#9729=FACE_OUTER_BOUND('',#15886,.T.);
#9730=FACE_OUTER_BOUND('',#15887,.T.);
#9731=FACE_OUTER_BOUND('',#15888,.T.);
#9732=FACE_OUTER_BOUND('',#15889,.T.);
#9733=FACE_OUTER_BOUND('',#15890,.T.);
#9734=FACE_OUTER_BOUND('',#15891,.T.);
#9735=FACE_OUTER_BOUND('',#15892,.T.);
#9736=FACE_OUTER_BOUND('',#15893,.T.);
#9737=FACE_OUTER_BOUND('',#15894,.T.);
#9738=FACE_OUTER_BOUND('',#15895,.T.);
#9739=FACE_OUTER_BOUND('',#15896,.T.);
#9740=FACE_OUTER_BOUND('',#15897,.T.);
#9741=FACE_OUTER_BOUND('',#15898,.T.);
#9742=FACE_OUTER_BOUND('',#15899,.T.);
#9743=FACE_OUTER_BOUND('',#15900,.T.);
#9744=FACE_OUTER_BOUND('',#15901,.T.);
#9745=FACE_OUTER_BOUND('',#15902,.T.);
#9746=FACE_OUTER_BOUND('',#15903,.T.);
#9747=FACE_OUTER_BOUND('',#15904,.T.);
#9748=FACE_OUTER_BOUND('',#15905,.T.);
#9749=FACE_OUTER_BOUND('',#15906,.T.);
#9750=FACE_OUTER_BOUND('',#15907,.T.);
#9751=FACE_OUTER_BOUND('',#15908,.T.);
#9752=FACE_OUTER_BOUND('',#15909,.T.);
#9753=FACE_OUTER_BOUND('',#15910,.T.);
#9754=FACE_OUTER_BOUND('',#15911,.T.);
#9755=FACE_OUTER_BOUND('',#15912,.T.);
#9756=FACE_OUTER_BOUND('',#15913,.T.);
#9757=FACE_OUTER_BOUND('',#15914,.T.);
#9758=FACE_OUTER_BOUND('',#15915,.T.);
#9759=FACE_OUTER_BOUND('',#15916,.T.);
#9760=FACE_OUTER_BOUND('',#15917,.T.);
#9761=FACE_OUTER_BOUND('',#15918,.T.);
#9762=FACE_OUTER_BOUND('',#15919,.T.);
#9763=FACE_OUTER_BOUND('',#15920,.T.);
#9764=FACE_OUTER_BOUND('',#15921,.T.);
#9765=FACE_OUTER_BOUND('',#15922,.T.);
#9766=FACE_OUTER_BOUND('',#15923,.T.);
#9767=FACE_OUTER_BOUND('',#15924,.T.);
#9768=FACE_OUTER_BOUND('',#15925,.T.);
#9769=FACE_OUTER_BOUND('',#15926,.T.);
#9770=FACE_OUTER_BOUND('',#15927,.T.);
#9771=FACE_OUTER_BOUND('',#15928,.T.);
#9772=FACE_OUTER_BOUND('',#15929,.T.);
#9773=FACE_OUTER_BOUND('',#15930,.T.);
#9774=FACE_OUTER_BOUND('',#15931,.T.);
#9775=FACE_OUTER_BOUND('',#15932,.T.);
#9776=FACE_OUTER_BOUND('',#15933,.T.);
#9777=FACE_OUTER_BOUND('',#15934,.T.);
#9778=FACE_OUTER_BOUND('',#15935,.T.);
#9779=FACE_OUTER_BOUND('',#15936,.T.);
#9780=FACE_OUTER_BOUND('',#15937,.T.);
#9781=FACE_OUTER_BOUND('',#15938,.T.);
#9782=FACE_OUTER_BOUND('',#15939,.T.);
#9783=FACE_OUTER_BOUND('',#15940,.T.);
#9784=FACE_OUTER_BOUND('',#15941,.T.);
#9785=FACE_OUTER_BOUND('',#15942,.T.);
#9786=FACE_OUTER_BOUND('',#15943,.T.);
#9787=FACE_OUTER_BOUND('',#15944,.T.);
#9788=FACE_OUTER_BOUND('',#15945,.T.);
#9789=FACE_OUTER_BOUND('',#15946,.T.);
#9790=FACE_OUTER_BOUND('',#15947,.T.);
#9791=FACE_OUTER_BOUND('',#15948,.T.);
#9792=FACE_OUTER_BOUND('',#15949,.T.);
#9793=FACE_OUTER_BOUND('',#15950,.T.);
#9794=FACE_OUTER_BOUND('',#15951,.T.);
#9795=FACE_OUTER_BOUND('',#15952,.T.);
#9796=FACE_OUTER_BOUND('',#15953,.T.);
#9797=FACE_OUTER_BOUND('',#15954,.T.);
#9798=FACE_OUTER_BOUND('',#15955,.T.);
#9799=FACE_OUTER_BOUND('',#15956,.T.);
#9800=FACE_OUTER_BOUND('',#15957,.T.);
#9801=FACE_OUTER_BOUND('',#15958,.T.);
#9802=FACE_OUTER_BOUND('',#15959,.T.);
#9803=FACE_OUTER_BOUND('',#15960,.T.);
#9804=FACE_OUTER_BOUND('',#15961,.T.);
#9805=FACE_OUTER_BOUND('',#15962,.T.);
#9806=FACE_OUTER_BOUND('',#15963,.T.);
#9807=FACE_OUTER_BOUND('',#15964,.T.);
#9808=FACE_OUTER_BOUND('',#15965,.T.);
#9809=FACE_OUTER_BOUND('',#15966,.T.);
#9810=FACE_OUTER_BOUND('',#15967,.T.);
#9811=FACE_OUTER_BOUND('',#15968,.T.);
#9812=FACE_OUTER_BOUND('',#15969,.T.);
#9813=FACE_OUTER_BOUND('',#15970,.T.);
#9814=FACE_OUTER_BOUND('',#15971,.T.);
#9815=FACE_OUTER_BOUND('',#15972,.T.);
#9816=FACE_OUTER_BOUND('',#15973,.T.);
#9817=FACE_OUTER_BOUND('',#15974,.T.);
#9818=FACE_OUTER_BOUND('',#15975,.T.);
#9819=FACE_OUTER_BOUND('',#15976,.T.);
#9820=FACE_OUTER_BOUND('',#15977,.T.);
#9821=FACE_OUTER_BOUND('',#15978,.T.);
#9822=FACE_OUTER_BOUND('',#15979,.T.);
#9823=FACE_OUTER_BOUND('',#15980,.T.);
#9824=FACE_OUTER_BOUND('',#15981,.T.);
#9825=FACE_OUTER_BOUND('',#15982,.T.);
#9826=FACE_OUTER_BOUND('',#15983,.T.);
#9827=FACE_OUTER_BOUND('',#15984,.T.);
#9828=FACE_OUTER_BOUND('',#15985,.T.);
#9829=FACE_OUTER_BOUND('',#15986,.T.);
#9830=FACE_OUTER_BOUND('',#15987,.T.);
#9831=FACE_OUTER_BOUND('',#15988,.T.);
#9832=FACE_OUTER_BOUND('',#15989,.T.);
#9833=FACE_OUTER_BOUND('',#15990,.T.);
#9834=FACE_OUTER_BOUND('',#15991,.T.);
#9835=FACE_OUTER_BOUND('',#15992,.T.);
#9836=FACE_OUTER_BOUND('',#15993,.T.);
#9837=FACE_OUTER_BOUND('',#15994,.T.);
#9838=FACE_OUTER_BOUND('',#15995,.T.);
#9839=FACE_OUTER_BOUND('',#15996,.T.);
#9840=FACE_OUTER_BOUND('',#15997,.T.);
#9841=FACE_OUTER_BOUND('',#15998,.T.);
#9842=FACE_OUTER_BOUND('',#15999,.T.);
#9843=FACE_OUTER_BOUND('',#16000,.T.);
#9844=FACE_OUTER_BOUND('',#16001,.T.);
#9845=FACE_OUTER_BOUND('',#16002,.T.);
#9846=FACE_OUTER_BOUND('',#16003,.T.);
#9847=FACE_OUTER_BOUND('',#16004,.T.);
#9848=FACE_OUTER_BOUND('',#16005,.T.);
#9849=FACE_OUTER_BOUND('',#16006,.T.);
#9850=FACE_OUTER_BOUND('',#16007,.T.);
#9851=FACE_OUTER_BOUND('',#16008,.T.);
#9852=FACE_OUTER_BOUND('',#16009,.T.);
#9853=FACE_OUTER_BOUND('',#16010,.T.);
#9854=FACE_OUTER_BOUND('',#16011,.T.);
#9855=FACE_OUTER_BOUND('',#16012,.T.);
#9856=FACE_OUTER_BOUND('',#16013,.T.);
#9857=FACE_OUTER_BOUND('',#16014,.T.);
#9858=FACE_OUTER_BOUND('',#16015,.T.);
#9859=FACE_OUTER_BOUND('',#16016,.T.);
#9860=FACE_OUTER_BOUND('',#16017,.T.);
#9861=FACE_OUTER_BOUND('',#16018,.T.);
#9862=FACE_OUTER_BOUND('',#16019,.T.);
#9863=FACE_OUTER_BOUND('',#16020,.T.);
#9864=FACE_OUTER_BOUND('',#16021,.T.);
#9865=FACE_OUTER_BOUND('',#16022,.T.);
#9866=FACE_OUTER_BOUND('',#16023,.T.);
#9867=FACE_OUTER_BOUND('',#16024,.T.);
#9868=FACE_OUTER_BOUND('',#16025,.T.);
#9869=FACE_OUTER_BOUND('',#16026,.T.);
#9870=FACE_OUTER_BOUND('',#16027,.T.);
#9871=FACE_OUTER_BOUND('',#16028,.T.);
#9872=FACE_OUTER_BOUND('',#16029,.T.);
#9873=FACE_OUTER_BOUND('',#16030,.T.);
#9874=FACE_OUTER_BOUND('',#16031,.T.);
#9875=FACE_OUTER_BOUND('',#16032,.T.);
#9876=FACE_OUTER_BOUND('',#16033,.T.);
#9877=FACE_OUTER_BOUND('',#16034,.T.);
#9878=FACE_OUTER_BOUND('',#16035,.T.);
#9879=FACE_OUTER_BOUND('',#16036,.T.);
#9880=FACE_OUTER_BOUND('',#16037,.T.);
#9881=FACE_OUTER_BOUND('',#16038,.T.);
#9882=FACE_OUTER_BOUND('',#16039,.T.);
#9883=FACE_OUTER_BOUND('',#16040,.T.);
#9884=FACE_OUTER_BOUND('',#16041,.T.);
#9885=FACE_OUTER_BOUND('',#16042,.T.);
#9886=FACE_OUTER_BOUND('',#16043,.T.);
#9887=FACE_OUTER_BOUND('',#16044,.T.);
#9888=FACE_OUTER_BOUND('',#16045,.T.);
#9889=FACE_OUTER_BOUND('',#16046,.T.);
#9890=FACE_OUTER_BOUND('',#16047,.T.);
#9891=FACE_OUTER_BOUND('',#16048,.T.);
#9892=FACE_OUTER_BOUND('',#16049,.T.);
#9893=FACE_OUTER_BOUND('',#16050,.T.);
#9894=FACE_OUTER_BOUND('',#16051,.T.);
#9895=FACE_OUTER_BOUND('',#16052,.T.);
#9896=FACE_OUTER_BOUND('',#16053,.T.);
#9897=FACE_OUTER_BOUND('',#16054,.T.);
#9898=FACE_OUTER_BOUND('',#16055,.T.);
#9899=FACE_OUTER_BOUND('',#16056,.T.);
#9900=FACE_OUTER_BOUND('',#16057,.T.);
#9901=FACE_OUTER_BOUND('',#16058,.T.);
#9902=FACE_OUTER_BOUND('',#16059,.T.);
#9903=FACE_OUTER_BOUND('',#16060,.T.);
#9904=FACE_OUTER_BOUND('',#16061,.T.);
#9905=FACE_OUTER_BOUND('',#16062,.T.);
#9906=FACE_OUTER_BOUND('',#16063,.T.);
#9907=FACE_OUTER_BOUND('',#16064,.T.);
#9908=FACE_OUTER_BOUND('',#16065,.T.);
#9909=FACE_OUTER_BOUND('',#16066,.T.);
#9910=FACE_OUTER_BOUND('',#16067,.T.);
#9911=FACE_OUTER_BOUND('',#16068,.T.);
#9912=FACE_OUTER_BOUND('',#16069,.T.);
#9913=FACE_OUTER_BOUND('',#16070,.T.);
#9914=FACE_OUTER_BOUND('',#16071,.T.);
#9915=FACE_OUTER_BOUND('',#16072,.T.);
#9916=FACE_OUTER_BOUND('',#16073,.T.);
#9917=FACE_OUTER_BOUND('',#16074,.T.);
#9918=FACE_OUTER_BOUND('',#16075,.T.);
#9919=FACE_OUTER_BOUND('',#16076,.T.);
#9920=FACE_OUTER_BOUND('',#16077,.T.);
#9921=FACE_OUTER_BOUND('',#16078,.T.);
#9922=FACE_OUTER_BOUND('',#16079,.T.);
#9923=FACE_OUTER_BOUND('',#16080,.T.);
#9924=FACE_OUTER_BOUND('',#16081,.T.);
#9925=FACE_OUTER_BOUND('',#16082,.T.);
#9926=FACE_OUTER_BOUND('',#16083,.T.);
#9927=FACE_OUTER_BOUND('',#16084,.T.);
#9928=FACE_OUTER_BOUND('',#16085,.T.);
#9929=FACE_OUTER_BOUND('',#16086,.T.);
#9930=FACE_OUTER_BOUND('',#16087,.T.);
#9931=FACE_OUTER_BOUND('',#16088,.T.);
#9932=FACE_OUTER_BOUND('',#16089,.T.);
#9933=FACE_OUTER_BOUND('',#16090,.T.);
#9934=FACE_OUTER_BOUND('',#16091,.T.);
#9935=FACE_OUTER_BOUND('',#16092,.T.);
#9936=FACE_OUTER_BOUND('',#16093,.T.);
#9937=FACE_OUTER_BOUND('',#16094,.T.);
#9938=FACE_OUTER_BOUND('',#16095,.T.);
#9939=FACE_OUTER_BOUND('',#16096,.T.);
#9940=FACE_OUTER_BOUND('',#16097,.T.);
#9941=FACE_OUTER_BOUND('',#16098,.T.);
#9942=FACE_OUTER_BOUND('',#16099,.T.);
#9943=FACE_OUTER_BOUND('',#16100,.T.);
#9944=FACE_OUTER_BOUND('',#16101,.T.);
#9945=FACE_OUTER_BOUND('',#16102,.T.);
#9946=FACE_OUTER_BOUND('',#16103,.T.);
#9947=FACE_OUTER_BOUND('',#16104,.T.);
#9948=FACE_OUTER_BOUND('',#16105,.T.);
#9949=FACE_OUTER_BOUND('',#16106,.T.);
#9950=FACE_OUTER_BOUND('',#16107,.T.);
#9951=FACE_OUTER_BOUND('',#16108,.T.);
#9952=FACE_OUTER_BOUND('',#16109,.T.);
#9953=FACE_OUTER_BOUND('',#16110,.T.);
#9954=FACE_OUTER_BOUND('',#16111,.T.);
#9955=FACE_OUTER_BOUND('',#16112,.T.);
#9956=FACE_OUTER_BOUND('',#16113,.T.);
#9957=FACE_OUTER_BOUND('',#16114,.T.);
#9958=FACE_OUTER_BOUND('',#16115,.T.);
#9959=FACE_OUTER_BOUND('',#16116,.T.);
#9960=FACE_OUTER_BOUND('',#16117,.T.);
#9961=FACE_OUTER_BOUND('',#16118,.T.);
#9962=FACE_OUTER_BOUND('',#16119,.T.);
#9963=FACE_OUTER_BOUND('',#16120,.T.);
#9964=FACE_OUTER_BOUND('',#16121,.T.);
#9965=FACE_OUTER_BOUND('',#16122,.T.);
#9966=FACE_OUTER_BOUND('',#16123,.T.);
#9967=FACE_OUTER_BOUND('',#16124,.T.);
#9968=FACE_OUTER_BOUND('',#16125,.T.);
#9969=FACE_OUTER_BOUND('',#16126,.T.);
#9970=FACE_OUTER_BOUND('',#16127,.T.);
#9971=FACE_OUTER_BOUND('',#16128,.T.);
#9972=FACE_OUTER_BOUND('',#16129,.T.);
#9973=FACE_OUTER_BOUND('',#16130,.T.);
#9974=FACE_OUTER_BOUND('',#16131,.T.);
#9975=FACE_OUTER_BOUND('',#16132,.T.);
#9976=FACE_OUTER_BOUND('',#16133,.T.);
#9977=FACE_OUTER_BOUND('',#16134,.T.);
#9978=FACE_OUTER_BOUND('',#16135,.T.);
#9979=FACE_OUTER_BOUND('',#16136,.T.);
#9980=FACE_OUTER_BOUND('',#16137,.T.);
#9981=FACE_OUTER_BOUND('',#16138,.T.);
#9982=FACE_OUTER_BOUND('',#16139,.T.);
#9983=FACE_OUTER_BOUND('',#16140,.T.);
#9984=FACE_OUTER_BOUND('',#16141,.T.);
#9985=FACE_OUTER_BOUND('',#16142,.T.);
#9986=FACE_OUTER_BOUND('',#16143,.T.);
#9987=FACE_OUTER_BOUND('',#16144,.T.);
#9988=FACE_OUTER_BOUND('',#16145,.T.);
#9989=FACE_OUTER_BOUND('',#16146,.T.);
#9990=FACE_OUTER_BOUND('',#16147,.T.);
#9991=FACE_OUTER_BOUND('',#16148,.T.);
#9992=FACE_OUTER_BOUND('',#16149,.T.);
#9993=FACE_OUTER_BOUND('',#16150,.T.);
#9994=FACE_OUTER_BOUND('',#16151,.T.);
#9995=FACE_OUTER_BOUND('',#16152,.T.);
#9996=FACE_OUTER_BOUND('',#16153,.T.);
#9997=FACE_OUTER_BOUND('',#16154,.T.);
#9998=FACE_OUTER_BOUND('',#16155,.T.);
#9999=FACE_OUTER_BOUND('',#16156,.T.);
#10000=FACE_OUTER_BOUND('',#16157,.T.);
#10001=FACE_OUTER_BOUND('',#16158,.T.);
#10002=FACE_OUTER_BOUND('',#16159,.T.);
#10003=FACE_OUTER_BOUND('',#16160,.T.);
#10004=FACE_OUTER_BOUND('',#16161,.T.);
#10005=FACE_OUTER_BOUND('',#16162,.T.);
#10006=FACE_OUTER_BOUND('',#16163,.T.);
#10007=FACE_OUTER_BOUND('',#16164,.T.);
#10008=FACE_OUTER_BOUND('',#16165,.T.);
#10009=FACE_OUTER_BOUND('',#16166,.T.);
#10010=FACE_OUTER_BOUND('',#16167,.T.);
#10011=FACE_OUTER_BOUND('',#16168,.T.);
#10012=FACE_OUTER_BOUND('',#16169,.T.);
#10013=FACE_OUTER_BOUND('',#16170,.T.);
#10014=FACE_OUTER_BOUND('',#16171,.T.);
#10015=FACE_OUTER_BOUND('',#16172,.T.);
#10016=FACE_OUTER_BOUND('',#16173,.T.);
#10017=FACE_OUTER_BOUND('',#16174,.T.);
#10018=FACE_OUTER_BOUND('',#16175,.T.);
#10019=FACE_OUTER_BOUND('',#16176,.T.);
#10020=FACE_OUTER_BOUND('',#16177,.T.);
#10021=FACE_OUTER_BOUND('',#16178,.T.);
#10022=FACE_OUTER_BOUND('',#16179,.T.);
#10023=FACE_OUTER_BOUND('',#16180,.T.);
#10024=FACE_OUTER_BOUND('',#16181,.T.);
#10025=FACE_OUTER_BOUND('',#16182,.T.);
#10026=FACE_OUTER_BOUND('',#16183,.T.);
#10027=FACE_OUTER_BOUND('',#16184,.T.);
#10028=FACE_OUTER_BOUND('',#16185,.T.);
#10029=FACE_OUTER_BOUND('',#16186,.T.);
#10030=FACE_OUTER_BOUND('',#16187,.T.);
#10031=FACE_OUTER_BOUND('',#16188,.T.);
#10032=FACE_OUTER_BOUND('',#16189,.T.);
#10033=FACE_OUTER_BOUND('',#16190,.T.);
#10034=FACE_OUTER_BOUND('',#16191,.T.);
#10035=FACE_OUTER_BOUND('',#16192,.T.);
#10036=FACE_OUTER_BOUND('',#16193,.T.);
#10037=FACE_OUTER_BOUND('',#16194,.T.);
#10038=FACE_OUTER_BOUND('',#16195,.T.);
#10039=FACE_OUTER_BOUND('',#16196,.T.);
#10040=FACE_OUTER_BOUND('',#16197,.T.);
#10041=FACE_OUTER_BOUND('',#16198,.T.);
#10042=FACE_OUTER_BOUND('',#16199,.T.);
#10043=FACE_OUTER_BOUND('',#16200,.T.);
#10044=FACE_OUTER_BOUND('',#16201,.T.);
#10045=FACE_OUTER_BOUND('',#16202,.T.);
#10046=FACE_OUTER_BOUND('',#16203,.T.);
#10047=FACE_OUTER_BOUND('',#16204,.T.);
#10048=FACE_OUTER_BOUND('',#16205,.T.);
#10049=FACE_OUTER_BOUND('',#16206,.T.);
#10050=FACE_OUTER_BOUND('',#16207,.T.);
#10051=FACE_OUTER_BOUND('',#16208,.T.);
#10052=FACE_OUTER_BOUND('',#16209,.T.);
#10053=FACE_OUTER_BOUND('',#16210,.T.);
#10054=FACE_OUTER_BOUND('',#16211,.T.);
#10055=FACE_OUTER_BOUND('',#16212,.T.);
#10056=FACE_OUTER_BOUND('',#16213,.T.);
#10057=FACE_OUTER_BOUND('',#16214,.T.);
#10058=FACE_OUTER_BOUND('',#16215,.T.);
#10059=FACE_OUTER_BOUND('',#16216,.T.);
#10060=FACE_OUTER_BOUND('',#16217,.T.);
#10061=FACE_OUTER_BOUND('',#16218,.T.);
#10062=FACE_OUTER_BOUND('',#16219,.T.);
#10063=FACE_OUTER_BOUND('',#16220,.T.);
#10064=FACE_OUTER_BOUND('',#16221,.T.);
#10065=FACE_OUTER_BOUND('',#16222,.T.);
#10066=FACE_OUTER_BOUND('',#16223,.T.);
#10067=FACE_OUTER_BOUND('',#16224,.T.);
#10068=FACE_OUTER_BOUND('',#16225,.T.);
#10069=FACE_OUTER_BOUND('',#16226,.T.);
#10070=FACE_OUTER_BOUND('',#16227,.T.);
#10071=FACE_OUTER_BOUND('',#16228,.T.);
#10072=FACE_OUTER_BOUND('',#16229,.T.);
#10073=FACE_OUTER_BOUND('',#16230,.T.);
#10074=FACE_OUTER_BOUND('',#16231,.T.);
#10075=FACE_OUTER_BOUND('',#16232,.T.);
#10076=FACE_OUTER_BOUND('',#16233,.T.);
#10077=FACE_OUTER_BOUND('',#16234,.T.);
#10078=FACE_OUTER_BOUND('',#16235,.T.);
#10079=FACE_OUTER_BOUND('',#16236,.T.);
#10080=FACE_OUTER_BOUND('',#16237,.T.);
#10081=FACE_OUTER_BOUND('',#16238,.T.);
#10082=FACE_OUTER_BOUND('',#16239,.T.);
#10083=FACE_OUTER_BOUND('',#16240,.T.);
#10084=FACE_OUTER_BOUND('',#16241,.T.);
#10085=FACE_OUTER_BOUND('',#16242,.T.);
#10086=FACE_OUTER_BOUND('',#16243,.T.);
#10087=FACE_OUTER_BOUND('',#16244,.T.);
#10088=FACE_OUTER_BOUND('',#16245,.T.);
#10089=FACE_OUTER_BOUND('',#16246,.T.);
#10090=FACE_OUTER_BOUND('',#16247,.T.);
#10091=FACE_OUTER_BOUND('',#16248,.T.);
#10092=FACE_OUTER_BOUND('',#16249,.T.);
#10093=FACE_OUTER_BOUND('',#16250,.T.);
#10094=FACE_OUTER_BOUND('',#16251,.T.);
#10095=FACE_OUTER_BOUND('',#16252,.T.);
#10096=FACE_OUTER_BOUND('',#16253,.T.);
#10097=FACE_OUTER_BOUND('',#16254,.T.);
#10098=FACE_OUTER_BOUND('',#16255,.T.);
#10099=FACE_OUTER_BOUND('',#16256,.T.);
#10100=FACE_OUTER_BOUND('',#16257,.T.);
#10101=FACE_OUTER_BOUND('',#16258,.T.);
#10102=FACE_OUTER_BOUND('',#16259,.T.);
#10103=FACE_OUTER_BOUND('',#16260,.T.);
#10104=FACE_OUTER_BOUND('',#16261,.T.);
#10105=FACE_OUTER_BOUND('',#16262,.T.);
#10106=FACE_OUTER_BOUND('',#16263,.T.);
#10107=FACE_OUTER_BOUND('',#16264,.T.);
#10108=FACE_OUTER_BOUND('',#16265,.T.);
#10109=FACE_OUTER_BOUND('',#16266,.T.);
#10110=FACE_OUTER_BOUND('',#16267,.T.);
#10111=FACE_OUTER_BOUND('',#16268,.T.);
#10112=FACE_OUTER_BOUND('',#16269,.T.);
#10113=FACE_OUTER_BOUND('',#16270,.T.);
#10114=FACE_OUTER_BOUND('',#16271,.T.);
#10115=FACE_OUTER_BOUND('',#16272,.T.);
#10116=FACE_OUTER_BOUND('',#16273,.T.);
#10117=FACE_OUTER_BOUND('',#16274,.T.);
#10118=FACE_OUTER_BOUND('',#16275,.T.);
#10119=FACE_OUTER_BOUND('',#16276,.T.);
#10120=FACE_OUTER_BOUND('',#16277,.T.);
#10121=FACE_OUTER_BOUND('',#16278,.T.);
#10122=FACE_OUTER_BOUND('',#16279,.T.);
#10123=FACE_OUTER_BOUND('',#16280,.T.);
#10124=FACE_OUTER_BOUND('',#16281,.T.);
#10125=FACE_OUTER_BOUND('',#16282,.T.);
#10126=FACE_OUTER_BOUND('',#16283,.T.);
#10127=FACE_OUTER_BOUND('',#16284,.T.);
#10128=FACE_OUTER_BOUND('',#16285,.T.);
#10129=FACE_OUTER_BOUND('',#16286,.T.);
#10130=FACE_OUTER_BOUND('',#16287,.T.);
#10131=FACE_OUTER_BOUND('',#16288,.T.);
#10132=FACE_OUTER_BOUND('',#16289,.T.);
#10133=FACE_OUTER_BOUND('',#16290,.T.);
#10134=FACE_OUTER_BOUND('',#16291,.T.);
#10135=FACE_OUTER_BOUND('',#16292,.T.);
#10136=FACE_OUTER_BOUND('',#16293,.T.);
#10137=FACE_OUTER_BOUND('',#16294,.T.);
#10138=FACE_OUTER_BOUND('',#16295,.T.);
#10139=FACE_OUTER_BOUND('',#16296,.T.);
#10140=FACE_OUTER_BOUND('',#16297,.T.);
#10141=FACE_OUTER_BOUND('',#16298,.T.);
#10142=FACE_OUTER_BOUND('',#16299,.T.);
#10143=FACE_OUTER_BOUND('',#16300,.T.);
#10144=FACE_OUTER_BOUND('',#16301,.T.);
#10145=FACE_OUTER_BOUND('',#16302,.T.);
#10146=FACE_OUTER_BOUND('',#16303,.T.);
#10147=FACE_OUTER_BOUND('',#16304,.T.);
#10148=FACE_OUTER_BOUND('',#16305,.T.);
#10149=FACE_OUTER_BOUND('',#16306,.T.);
#10150=FACE_OUTER_BOUND('',#16307,.T.);
#10151=FACE_OUTER_BOUND('',#16308,.T.);
#10152=FACE_OUTER_BOUND('',#16309,.T.);
#10153=FACE_OUTER_BOUND('',#16310,.T.);
#10154=FACE_OUTER_BOUND('',#16311,.T.);
#10155=FACE_OUTER_BOUND('',#16312,.T.);
#10156=FACE_OUTER_BOUND('',#16313,.T.);
#10157=FACE_OUTER_BOUND('',#16314,.T.);
#10158=FACE_OUTER_BOUND('',#16315,.T.);
#10159=FACE_OUTER_BOUND('',#16316,.T.);
#10160=FACE_OUTER_BOUND('',#16317,.T.);
#10161=FACE_OUTER_BOUND('',#16318,.T.);
#10162=FACE_OUTER_BOUND('',#16319,.T.);
#10163=FACE_OUTER_BOUND('',#16320,.T.);
#10164=FACE_OUTER_BOUND('',#16321,.T.);
#10165=FACE_OUTER_BOUND('',#16322,.T.);
#10166=FACE_OUTER_BOUND('',#16323,.T.);
#10167=FACE_OUTER_BOUND('',#16324,.T.);
#10168=FACE_OUTER_BOUND('',#16325,.T.);
#10169=FACE_OUTER_BOUND('',#16326,.T.);
#10170=FACE_OUTER_BOUND('',#16327,.T.);
#10171=FACE_OUTER_BOUND('',#16328,.T.);
#10172=FACE_OUTER_BOUND('',#16329,.T.);
#10173=FACE_OUTER_BOUND('',#16330,.T.);
#10174=FACE_OUTER_BOUND('',#16331,.T.);
#10175=FACE_OUTER_BOUND('',#16332,.T.);
#10176=FACE_OUTER_BOUND('',#16333,.T.);
#10177=FACE_OUTER_BOUND('',#16334,.T.);
#10178=FACE_OUTER_BOUND('',#16335,.T.);
#10179=FACE_OUTER_BOUND('',#16336,.T.);
#10180=FACE_OUTER_BOUND('',#16337,.T.);
#10181=FACE_OUTER_BOUND('',#16338,.T.);
#10182=FACE_OUTER_BOUND('',#16339,.T.);
#10183=FACE_OUTER_BOUND('',#16340,.T.);
#10184=FACE_OUTER_BOUND('',#16341,.T.);
#10185=FACE_OUTER_BOUND('',#16342,.T.);
#10186=FACE_OUTER_BOUND('',#16343,.T.);
#10187=FACE_OUTER_BOUND('',#16344,.T.);
#10188=FACE_OUTER_BOUND('',#16345,.T.);
#10189=FACE_OUTER_BOUND('',#16346,.T.);
#10190=FACE_OUTER_BOUND('',#16347,.T.);
#10191=FACE_OUTER_BOUND('',#16348,.T.);
#10192=FACE_OUTER_BOUND('',#16349,.T.);
#10193=FACE_OUTER_BOUND('',#16350,.T.);
#10194=FACE_OUTER_BOUND('',#16351,.T.);
#10195=FACE_OUTER_BOUND('',#16352,.T.);
#10196=FACE_OUTER_BOUND('',#16353,.T.);
#10197=FACE_OUTER_BOUND('',#16354,.T.);
#10198=FACE_OUTER_BOUND('',#16355,.T.);
#10199=FACE_OUTER_BOUND('',#16356,.T.);
#10200=FACE_OUTER_BOUND('',#16357,.T.);
#10201=FACE_OUTER_BOUND('',#16358,.T.);
#10202=FACE_OUTER_BOUND('',#16359,.T.);
#10203=FACE_OUTER_BOUND('',#16360,.T.);
#10204=FACE_OUTER_BOUND('',#16361,.T.);
#10205=FACE_OUTER_BOUND('',#16362,.T.);
#10206=FACE_OUTER_BOUND('',#16363,.T.);
#10207=FACE_OUTER_BOUND('',#16364,.T.);
#10208=FACE_OUTER_BOUND('',#16365,.T.);
#10209=FACE_OUTER_BOUND('',#16366,.T.);
#10210=FACE_OUTER_BOUND('',#16367,.T.);
#10211=FACE_OUTER_BOUND('',#16368,.T.);
#10212=FACE_OUTER_BOUND('',#16369,.T.);
#10213=FACE_OUTER_BOUND('',#16370,.T.);
#10214=FACE_OUTER_BOUND('',#16371,.T.);
#10215=FACE_OUTER_BOUND('',#16372,.T.);
#10216=FACE_OUTER_BOUND('',#16373,.T.);
#10217=FACE_OUTER_BOUND('',#16374,.T.);
#10218=FACE_OUTER_BOUND('',#16375,.T.);
#10219=FACE_OUTER_BOUND('',#16376,.T.);
#10220=FACE_OUTER_BOUND('',#16377,.T.);
#10221=FACE_OUTER_BOUND('',#16378,.T.);
#10222=FACE_OUTER_BOUND('',#16379,.T.);
#10223=FACE_OUTER_BOUND('',#16380,.T.);
#10224=FACE_OUTER_BOUND('',#16381,.T.);
#10225=FACE_OUTER_BOUND('',#16382,.T.);
#10226=FACE_OUTER_BOUND('',#16383,.T.);
#10227=FACE_OUTER_BOUND('',#16384,.T.);
#10228=FACE_OUTER_BOUND('',#16385,.T.);
#10229=FACE_OUTER_BOUND('',#16386,.T.);
#10230=FACE_OUTER_BOUND('',#16387,.T.);
#10231=FACE_OUTER_BOUND('',#16388,.T.);
#10232=FACE_OUTER_BOUND('',#16389,.T.);
#10233=FACE_OUTER_BOUND('',#16390,.T.);
#10234=FACE_OUTER_BOUND('',#16391,.T.);
#10235=FACE_OUTER_BOUND('',#16392,.T.);
#10236=FACE_OUTER_BOUND('',#16393,.T.);
#10237=FACE_OUTER_BOUND('',#16394,.T.);
#10238=FACE_OUTER_BOUND('',#16395,.T.);
#10239=FACE_OUTER_BOUND('',#16396,.T.);
#10240=FACE_OUTER_BOUND('',#16397,.T.);
#10241=FACE_OUTER_BOUND('',#16398,.T.);
#10242=FACE_OUTER_BOUND('',#16399,.T.);
#10243=FACE_OUTER_BOUND('',#16400,.T.);
#10244=FACE_OUTER_BOUND('',#16401,.T.);
#10245=FACE_OUTER_BOUND('',#16402,.T.);
#10246=FACE_OUTER_BOUND('',#16403,.T.);
#10247=FACE_OUTER_BOUND('',#16404,.T.);
#10248=FACE_OUTER_BOUND('',#16405,.T.);
#10249=FACE_OUTER_BOUND('',#16406,.T.);
#10250=FACE_OUTER_BOUND('',#16407,.T.);
#10251=FACE_OUTER_BOUND('',#16408,.T.);
#10252=FACE_OUTER_BOUND('',#16409,.T.);
#10253=FACE_OUTER_BOUND('',#16410,.T.);
#10254=FACE_OUTER_BOUND('',#16411,.T.);
#10255=FACE_OUTER_BOUND('',#16412,.T.);
#10256=FACE_OUTER_BOUND('',#16413,.T.);
#10257=FACE_OUTER_BOUND('',#16414,.T.);
#10258=FACE_OUTER_BOUND('',#16415,.T.);
#10259=FACE_OUTER_BOUND('',#16416,.T.);
#10260=FACE_OUTER_BOUND('',#16417,.T.);
#10261=FACE_OUTER_BOUND('',#16418,.T.);
#10262=FACE_OUTER_BOUND('',#16419,.T.);
#10263=FACE_OUTER_BOUND('',#16420,.T.);
#10264=FACE_OUTER_BOUND('',#16421,.T.);
#10265=FACE_OUTER_BOUND('',#16422,.T.);
#10266=FACE_OUTER_BOUND('',#16423,.T.);
#10267=FACE_OUTER_BOUND('',#16424,.T.);
#10268=FACE_OUTER_BOUND('',#16425,.T.);
#10269=FACE_OUTER_BOUND('',#16426,.T.);
#10270=FACE_OUTER_BOUND('',#16427,.T.);
#10271=FACE_OUTER_BOUND('',#16428,.T.);
#10272=FACE_OUTER_BOUND('',#16429,.T.);
#10273=FACE_OUTER_BOUND('',#16430,.T.);
#10274=FACE_OUTER_BOUND('',#16431,.T.);
#10275=FACE_OUTER_BOUND('',#16432,.T.);
#10276=FACE_OUTER_BOUND('',#16433,.T.);
#10277=FACE_OUTER_BOUND('',#16434,.T.);
#10278=FACE_OUTER_BOUND('',#16435,.T.);
#10279=FACE_OUTER_BOUND('',#16436,.T.);
#10280=FACE_OUTER_BOUND('',#16437,.T.);
#10281=FACE_OUTER_BOUND('',#16438,.T.);
#10282=FACE_OUTER_BOUND('',#16439,.T.);
#10283=FACE_OUTER_BOUND('',#16440,.T.);
#10284=FACE_OUTER_BOUND('',#16441,.T.);
#10285=FACE_OUTER_BOUND('',#16442,.T.);
#10286=FACE_OUTER_BOUND('',#16443,.T.);
#10287=FACE_OUTER_BOUND('',#16444,.T.);
#10288=FACE_OUTER_BOUND('',#16445,.T.);
#10289=FACE_OUTER_BOUND('',#16446,.T.);
#10290=FACE_OUTER_BOUND('',#16447,.T.);
#10291=FACE_OUTER_BOUND('',#16448,.T.);
#10292=FACE_OUTER_BOUND('',#16449,.T.);
#10293=FACE_OUTER_BOUND('',#16450,.T.);
#10294=FACE_OUTER_BOUND('',#16451,.T.);
#10295=FACE_OUTER_BOUND('',#16452,.T.);
#10296=FACE_OUTER_BOUND('',#16453,.T.);
#10297=FACE_OUTER_BOUND('',#16454,.T.);
#10298=FACE_OUTER_BOUND('',#16455,.T.);
#10299=FACE_OUTER_BOUND('',#16456,.T.);
#10300=FACE_OUTER_BOUND('',#16457,.T.);
#10301=FACE_OUTER_BOUND('',#16458,.T.);
#10302=FACE_OUTER_BOUND('',#16459,.T.);
#10303=FACE_OUTER_BOUND('',#16460,.T.);
#10304=FACE_OUTER_BOUND('',#16461,.T.);
#10305=FACE_OUTER_BOUND('',#16462,.T.);
#10306=FACE_OUTER_BOUND('',#16463,.T.);
#10307=FACE_OUTER_BOUND('',#16464,.T.);
#10308=FACE_OUTER_BOUND('',#16465,.T.);
#10309=FACE_OUTER_BOUND('',#16466,.T.);
#10310=FACE_OUTER_BOUND('',#16467,.T.);
#10311=FACE_OUTER_BOUND('',#16468,.T.);
#10312=FACE_OUTER_BOUND('',#16469,.T.);
#10313=FACE_OUTER_BOUND('',#16470,.T.);
#10314=FACE_OUTER_BOUND('',#16471,.T.);
#10315=FACE_OUTER_BOUND('',#16472,.T.);
#10316=FACE_OUTER_BOUND('',#16473,.T.);
#10317=FACE_OUTER_BOUND('',#16474,.T.);
#10318=FACE_OUTER_BOUND('',#16475,.T.);
#10319=FACE_OUTER_BOUND('',#16476,.T.);
#10320=FACE_OUTER_BOUND('',#16477,.T.);
#10321=FACE_OUTER_BOUND('',#16478,.T.);
#10322=FACE_OUTER_BOUND('',#16479,.T.);
#10323=FACE_OUTER_BOUND('',#16480,.T.);
#10324=FACE_OUTER_BOUND('',#16481,.T.);
#10325=FACE_OUTER_BOUND('',#16482,.T.);
#10326=FACE_OUTER_BOUND('',#16483,.T.);
#10327=FACE_OUTER_BOUND('',#16484,.T.);
#10328=FACE_OUTER_BOUND('',#16485,.T.);
#10329=FACE_OUTER_BOUND('',#16486,.T.);
#10330=FACE_OUTER_BOUND('',#16487,.T.);
#10331=FACE_OUTER_BOUND('',#16488,.T.);
#10332=FACE_OUTER_BOUND('',#16489,.T.);
#10333=FACE_OUTER_BOUND('',#16490,.T.);
#10334=FACE_OUTER_BOUND('',#16491,.T.);
#10335=FACE_OUTER_BOUND('',#16492,.T.);
#10336=FACE_OUTER_BOUND('',#16493,.T.);
#10337=FACE_OUTER_BOUND('',#16494,.T.);
#10338=FACE_OUTER_BOUND('',#16495,.T.);
#10339=FACE_OUTER_BOUND('',#16496,.T.);
#10340=FACE_OUTER_BOUND('',#16497,.T.);
#10341=FACE_OUTER_BOUND('',#16498,.T.);
#10342=FACE_OUTER_BOUND('',#16499,.T.);
#10343=FACE_OUTER_BOUND('',#16500,.T.);
#10344=FACE_OUTER_BOUND('',#16501,.T.);
#10345=FACE_OUTER_BOUND('',#16502,.T.);
#10346=FACE_OUTER_BOUND('',#16503,.T.);
#10347=FACE_OUTER_BOUND('',#16504,.T.);
#10348=FACE_OUTER_BOUND('',#16505,.T.);
#10349=FACE_OUTER_BOUND('',#16506,.T.);
#10350=FACE_OUTER_BOUND('',#16507,.T.);
#10351=FACE_OUTER_BOUND('',#16508,.T.);
#10352=FACE_OUTER_BOUND('',#16509,.T.);
#10353=FACE_OUTER_BOUND('',#16510,.T.);
#10354=FACE_OUTER_BOUND('',#16511,.T.);
#10355=FACE_OUTER_BOUND('',#16512,.T.);
#10356=FACE_OUTER_BOUND('',#16513,.T.);
#10357=FACE_OUTER_BOUND('',#16514,.T.);
#10358=FACE_OUTER_BOUND('',#16515,.T.);
#10359=FACE_OUTER_BOUND('',#16516,.T.);
#10360=FACE_OUTER_BOUND('',#16517,.T.);
#10361=FACE_OUTER_BOUND('',#16518,.T.);
#10362=FACE_OUTER_BOUND('',#16519,.T.);
#10363=FACE_OUTER_BOUND('',#16520,.T.);
#10364=FACE_OUTER_BOUND('',#16521,.T.);
#10365=FACE_OUTER_BOUND('',#16522,.T.);
#10366=FACE_OUTER_BOUND('',#16523,.T.);
#10367=FACE_OUTER_BOUND('',#16524,.T.);
#10368=FACE_OUTER_BOUND('',#16525,.T.);
#10369=FACE_OUTER_BOUND('',#16526,.T.);
#10370=FACE_OUTER_BOUND('',#16527,.T.);
#10371=FACE_OUTER_BOUND('',#16528,.T.);
#10372=FACE_OUTER_BOUND('',#16529,.T.);
#10373=FACE_OUTER_BOUND('',#16530,.T.);
#10374=FACE_OUTER_BOUND('',#16531,.T.);
#10375=FACE_OUTER_BOUND('',#16532,.T.);
#10376=FACE_OUTER_BOUND('',#16533,.T.);
#10377=FACE_OUTER_BOUND('',#16534,.T.);
#10378=FACE_OUTER_BOUND('',#16535,.T.);
#10379=FACE_OUTER_BOUND('',#16536,.T.);
#10380=FACE_OUTER_BOUND('',#16537,.T.);
#10381=FACE_OUTER_BOUND('',#16538,.T.);
#10382=FACE_OUTER_BOUND('',#16539,.T.);
#10383=FACE_OUTER_BOUND('',#16540,.T.);
#10384=FACE_OUTER_BOUND('',#16541,.T.);
#10385=FACE_OUTER_BOUND('',#16542,.T.);
#10386=FACE_OUTER_BOUND('',#16543,.T.);
#10387=FACE_OUTER_BOUND('',#16544,.T.);
#10388=FACE_OUTER_BOUND('',#16545,.T.);
#10389=FACE_OUTER_BOUND('',#16546,.T.);
#10390=FACE_OUTER_BOUND('',#16547,.T.);
#10391=FACE_OUTER_BOUND('',#16548,.T.);
#10392=FACE_OUTER_BOUND('',#16549,.T.);
#10393=FACE_OUTER_BOUND('',#16550,.T.);
#10394=FACE_OUTER_BOUND('',#16551,.T.);
#10395=FACE_OUTER_BOUND('',#16552,.T.);
#10396=FACE_OUTER_BOUND('',#16553,.T.);
#10397=FACE_OUTER_BOUND('',#16554,.T.);
#10398=FACE_OUTER_BOUND('',#16555,.T.);
#10399=FACE_OUTER_BOUND('',#16556,.T.);
#10400=FACE_OUTER_BOUND('',#16557,.T.);
#10401=FACE_OUTER_BOUND('',#16558,.T.);
#10402=FACE_OUTER_BOUND('',#16559,.T.);
#10403=FACE_OUTER_BOUND('',#16560,.T.);
#10404=FACE_OUTER_BOUND('',#16561,.T.);
#10405=FACE_OUTER_BOUND('',#16562,.T.);
#10406=FACE_OUTER_BOUND('',#16563,.T.);
#10407=FACE_OUTER_BOUND('',#16564,.T.);
#10408=FACE_OUTER_BOUND('',#16565,.T.);
#10409=FACE_OUTER_BOUND('',#16566,.T.);
#10410=FACE_OUTER_BOUND('',#16567,.T.);
#10411=FACE_OUTER_BOUND('',#16568,.T.);
#10412=FACE_OUTER_BOUND('',#16569,.T.);
#10413=FACE_OUTER_BOUND('',#16570,.T.);
#10414=FACE_OUTER_BOUND('',#16571,.T.);
#10415=FACE_OUTER_BOUND('',#16572,.T.);
#10416=FACE_OUTER_BOUND('',#16573,.T.);
#10417=FACE_OUTER_BOUND('',#16574,.T.);
#10418=FACE_OUTER_BOUND('',#16575,.T.);
#10419=FACE_OUTER_BOUND('',#16576,.T.);
#10420=FACE_OUTER_BOUND('',#16577,.T.);
#10421=FACE_OUTER_BOUND('',#16578,.T.);
#10422=FACE_OUTER_BOUND('',#16579,.T.);
#10423=FACE_OUTER_BOUND('',#16580,.T.);
#10424=FACE_OUTER_BOUND('',#16581,.T.);
#10425=FACE_OUTER_BOUND('',#16582,.T.);
#10426=FACE_OUTER_BOUND('',#16583,.T.);
#10427=FACE_OUTER_BOUND('',#16584,.T.);
#10428=FACE_OUTER_BOUND('',#16585,.T.);
#10429=FACE_OUTER_BOUND('',#16586,.T.);
#10430=FACE_OUTER_BOUND('',#16587,.T.);
#10431=FACE_OUTER_BOUND('',#16588,.T.);
#10432=FACE_OUTER_BOUND('',#16589,.T.);
#10433=FACE_OUTER_BOUND('',#16590,.T.);
#10434=FACE_OUTER_BOUND('',#16591,.T.);
#10435=FACE_OUTER_BOUND('',#16592,.T.);
#10436=FACE_OUTER_BOUND('',#16593,.T.);
#10437=FACE_OUTER_BOUND('',#16594,.T.);
#10438=FACE_OUTER_BOUND('',#16595,.T.);
#10439=FACE_OUTER_BOUND('',#16596,.T.);
#10440=FACE_OUTER_BOUND('',#16597,.T.);
#10441=FACE_OUTER_BOUND('',#16598,.T.);
#10442=FACE_OUTER_BOUND('',#16599,.T.);
#10443=FACE_OUTER_BOUND('',#16600,.T.);
#10444=FACE_OUTER_BOUND('',#16601,.T.);
#10445=FACE_OUTER_BOUND('',#16602,.T.);
#10446=FACE_OUTER_BOUND('',#16603,.T.);
#10447=FACE_OUTER_BOUND('',#16604,.T.);
#10448=FACE_OUTER_BOUND('',#16605,.T.);
#10449=FACE_OUTER_BOUND('',#16606,.T.);
#10450=FACE_OUTER_BOUND('',#16607,.T.);
#10451=FACE_OUTER_BOUND('',#16608,.T.);
#10452=FACE_OUTER_BOUND('',#16609,.T.);
#10453=FACE_OUTER_BOUND('',#16610,.T.);
#10454=FACE_OUTER_BOUND('',#16611,.T.);
#10455=FACE_OUTER_BOUND('',#16612,.T.);
#10456=FACE_OUTER_BOUND('',#16613,.T.);
#10457=FACE_OUTER_BOUND('',#16614,.T.);
#10458=FACE_OUTER_BOUND('',#16615,.T.);
#10459=FACE_OUTER_BOUND('',#16616,.T.);
#10460=FACE_OUTER_BOUND('',#16617,.T.);
#10461=FACE_OUTER_BOUND('',#16618,.T.);
#10462=FACE_OUTER_BOUND('',#16619,.T.);
#10463=FACE_OUTER_BOUND('',#16620,.T.);
#10464=FACE_OUTER_BOUND('',#16621,.T.);
#10465=FACE_OUTER_BOUND('',#16622,.T.);
#10466=FACE_OUTER_BOUND('',#16623,.T.);
#10467=FACE_OUTER_BOUND('',#16624,.T.);
#10468=FACE_OUTER_BOUND('',#16625,.T.);
#10469=FACE_OUTER_BOUND('',#16626,.T.);
#10470=FACE_OUTER_BOUND('',#16627,.T.);
#10471=FACE_OUTER_BOUND('',#16628,.T.);
#10472=FACE_OUTER_BOUND('',#16629,.T.);
#10473=FACE_OUTER_BOUND('',#16630,.T.);
#10474=FACE_OUTER_BOUND('',#16631,.T.);
#10475=FACE_OUTER_BOUND('',#16632,.T.);
#10476=FACE_OUTER_BOUND('',#16633,.T.);
#10477=FACE_OUTER_BOUND('',#16634,.T.);
#10478=FACE_OUTER_BOUND('',#16635,.T.);
#10479=FACE_OUTER_BOUND('',#16636,.T.);
#10480=FACE_OUTER_BOUND('',#16637,.T.);
#10481=FACE_OUTER_BOUND('',#16638,.T.);
#10482=FACE_OUTER_BOUND('',#16639,.T.);
#10483=FACE_OUTER_BOUND('',#16640,.T.);
#10484=FACE_OUTER_BOUND('',#16641,.T.);
#10485=FACE_OUTER_BOUND('',#16642,.T.);
#10486=FACE_OUTER_BOUND('',#16643,.T.);
#10487=FACE_OUTER_BOUND('',#16644,.T.);
#10488=FACE_OUTER_BOUND('',#16645,.T.);
#10489=FACE_OUTER_BOUND('',#16646,.T.);
#10490=FACE_OUTER_BOUND('',#16647,.T.);
#10491=FACE_OUTER_BOUND('',#16648,.T.);
#10492=FACE_OUTER_BOUND('',#16649,.T.);
#10493=FACE_OUTER_BOUND('',#16650,.T.);
#10494=FACE_OUTER_BOUND('',#16651,.T.);
#10495=FACE_OUTER_BOUND('',#16652,.T.);
#10496=FACE_OUTER_BOUND('',#16653,.T.);
#10497=FACE_OUTER_BOUND('',#16654,.T.);
#10498=FACE_OUTER_BOUND('',#16655,.T.);
#10499=FACE_OUTER_BOUND('',#16656,.T.);
#10500=FACE_OUTER_BOUND('',#16657,.T.);
#10501=FACE_OUTER_BOUND('',#16658,.T.);
#10502=FACE_OUTER_BOUND('',#16659,.T.);
#10503=FACE_OUTER_BOUND('',#16660,.T.);
#10504=FACE_OUTER_BOUND('',#16661,.T.);
#10505=FACE_OUTER_BOUND('',#16662,.T.);
#10506=FACE_OUTER_BOUND('',#16663,.T.);
#10507=FACE_OUTER_BOUND('',#16664,.T.);
#10508=FACE_OUTER_BOUND('',#16665,.T.);
#10509=FACE_OUTER_BOUND('',#16666,.T.);
#10510=FACE_OUTER_BOUND('',#16667,.T.);
#10511=FACE_OUTER_BOUND('',#16668,.T.);
#10512=FACE_OUTER_BOUND('',#16669,.T.);
#10513=FACE_OUTER_BOUND('',#16670,.T.);
#10514=FACE_OUTER_BOUND('',#16671,.T.);
#10515=FACE_OUTER_BOUND('',#16672,.T.);
#10516=FACE_OUTER_BOUND('',#16673,.T.);
#10517=FACE_OUTER_BOUND('',#16674,.T.);
#10518=FACE_OUTER_BOUND('',#16675,.T.);
#10519=FACE_OUTER_BOUND('',#16676,.T.);
#10520=FACE_OUTER_BOUND('',#16677,.T.);
#10521=FACE_OUTER_BOUND('',#16678,.T.);
#10522=FACE_OUTER_BOUND('',#16679,.T.);
#10523=FACE_OUTER_BOUND('',#16680,.T.);
#10524=FACE_OUTER_BOUND('',#16681,.T.);
#10525=FACE_OUTER_BOUND('',#16682,.T.);
#10526=FACE_OUTER_BOUND('',#16683,.T.);
#10527=FACE_OUTER_BOUND('',#16684,.T.);
#10528=FACE_OUTER_BOUND('',#16685,.T.);
#10529=FACE_OUTER_BOUND('',#16686,.T.);
#10530=FACE_OUTER_BOUND('',#16687,.T.);
#10531=FACE_OUTER_BOUND('',#16688,.T.);
#10532=FACE_OUTER_BOUND('',#16689,.T.);
#10533=FACE_OUTER_BOUND('',#16690,.T.);
#10534=FACE_OUTER_BOUND('',#16691,.T.);
#10535=FACE_OUTER_BOUND('',#16692,.T.);
#10536=FACE_OUTER_BOUND('',#16693,.T.);
#10537=FACE_OUTER_BOUND('',#16694,.T.);
#10538=FACE_OUTER_BOUND('',#16695,.T.);
#10539=FACE_OUTER_BOUND('',#16696,.T.);
#10540=FACE_OUTER_BOUND('',#16697,.T.);
#10541=FACE_OUTER_BOUND('',#16698,.T.);
#10542=FACE_OUTER_BOUND('',#16699,.T.);
#10543=FACE_OUTER_BOUND('',#16700,.T.);
#10544=FACE_OUTER_BOUND('',#16701,.T.);
#10545=FACE_OUTER_BOUND('',#16702,.T.);
#10546=FACE_OUTER_BOUND('',#16703,.T.);
#10547=FACE_OUTER_BOUND('',#16704,.T.);
#10548=FACE_OUTER_BOUND('',#16705,.T.);
#10549=FACE_OUTER_BOUND('',#16706,.T.);
#10550=FACE_OUTER_BOUND('',#16707,.T.);
#10551=FACE_OUTER_BOUND('',#16708,.T.);
#10552=FACE_OUTER_BOUND('',#16709,.T.);
#10553=FACE_OUTER_BOUND('',#16710,.T.);
#10554=FACE_OUTER_BOUND('',#16711,.T.);
#10555=FACE_OUTER_BOUND('',#16712,.T.);
#10556=FACE_OUTER_BOUND('',#16713,.T.);
#10557=FACE_OUTER_BOUND('',#16714,.T.);
#10558=FACE_OUTER_BOUND('',#16715,.T.);
#10559=FACE_OUTER_BOUND('',#16716,.T.);
#10560=FACE_OUTER_BOUND('',#16717,.T.);
#10561=FACE_OUTER_BOUND('',#16718,.T.);
#10562=FACE_OUTER_BOUND('',#16719,.T.);
#10563=FACE_OUTER_BOUND('',#16720,.T.);
#10564=FACE_OUTER_BOUND('',#16721,.T.);
#10565=FACE_OUTER_BOUND('',#16722,.T.);
#10566=FACE_OUTER_BOUND('',#16723,.T.);
#10567=FACE_OUTER_BOUND('',#16724,.T.);
#10568=FACE_OUTER_BOUND('',#16725,.T.);
#10569=FACE_OUTER_BOUND('',#16726,.T.);
#10570=FACE_OUTER_BOUND('',#16727,.T.);
#10571=FACE_OUTER_BOUND('',#16728,.T.);
#10572=FACE_OUTER_BOUND('',#16729,.T.);
#10573=FACE_OUTER_BOUND('',#16730,.T.);
#10574=FACE_OUTER_BOUND('',#16731,.T.);
#10575=FACE_OUTER_BOUND('',#16732,.T.);
#10576=FACE_OUTER_BOUND('',#16733,.T.);
#10577=FACE_OUTER_BOUND('',#16734,.T.);
#10578=FACE_OUTER_BOUND('',#16735,.T.);
#10579=FACE_OUTER_BOUND('',#16736,.T.);
#10580=FACE_OUTER_BOUND('',#16737,.T.);
#10581=FACE_OUTER_BOUND('',#16738,.T.);
#10582=FACE_OUTER_BOUND('',#16739,.T.);
#10583=FACE_OUTER_BOUND('',#16740,.T.);
#10584=FACE_OUTER_BOUND('',#16741,.T.);
#10585=FACE_OUTER_BOUND('',#16742,.T.);
#10586=FACE_OUTER_BOUND('',#16743,.T.);
#10587=FACE_OUTER_BOUND('',#16744,.T.);
#10588=FACE_OUTER_BOUND('',#16745,.T.);
#10589=FACE_OUTER_BOUND('',#16746,.T.);
#10590=FACE_OUTER_BOUND('',#16747,.T.);
#10591=FACE_OUTER_BOUND('',#16748,.T.);
#10592=FACE_OUTER_BOUND('',#16749,.T.);
#10593=FACE_OUTER_BOUND('',#16750,.T.);
#10594=FACE_OUTER_BOUND('',#16751,.T.);
#10595=FACE_OUTER_BOUND('',#16752,.T.);
#10596=FACE_OUTER_BOUND('',#16753,.T.);
#10597=FACE_OUTER_BOUND('',#16754,.T.);
#10598=FACE_OUTER_BOUND('',#16755,.T.);
#10599=FACE_OUTER_BOUND('',#16756,.T.);
#10600=FACE_OUTER_BOUND('',#16757,.T.);
#10601=FACE_OUTER_BOUND('',#16758,.T.);
#10602=FACE_OUTER_BOUND('',#16759,.T.);
#10603=FACE_OUTER_BOUND('',#16760,.T.);
#10604=FACE_OUTER_BOUND('',#16761,.T.);
#10605=FACE_OUTER_BOUND('',#16762,.T.);
#10606=FACE_OUTER_BOUND('',#16763,.T.);
#10607=FACE_OUTER_BOUND('',#16764,.T.);
#10608=FACE_OUTER_BOUND('',#16765,.T.);
#10609=FACE_OUTER_BOUND('',#16766,.T.);
#10610=FACE_OUTER_BOUND('',#16767,.T.);
#10611=FACE_OUTER_BOUND('',#16768,.T.);
#10612=FACE_OUTER_BOUND('',#16769,.T.);
#10613=FACE_OUTER_BOUND('',#16770,.T.);
#10614=FACE_OUTER_BOUND('',#16771,.T.);
#10615=FACE_OUTER_BOUND('',#16772,.T.);
#10616=FACE_OUTER_BOUND('',#16773,.T.);
#10617=FACE_OUTER_BOUND('',#16774,.T.);
#10618=FACE_OUTER_BOUND('',#16775,.T.);
#10619=FACE_OUTER_BOUND('',#16776,.T.);
#10620=FACE_OUTER_BOUND('',#16777,.T.);
#10621=FACE_OUTER_BOUND('',#16778,.T.);
#10622=FACE_OUTER_BOUND('',#16779,.T.);
#10623=FACE_OUTER_BOUND('',#16780,.T.);
#10624=FACE_OUTER_BOUND('',#16781,.T.);
#10625=FACE_OUTER_BOUND('',#16782,.T.);
#10626=FACE_OUTER_BOUND('',#16783,.T.);
#10627=FACE_OUTER_BOUND('',#16784,.T.);
#10628=FACE_OUTER_BOUND('',#16785,.T.);
#10629=FACE_OUTER_BOUND('',#16786,.T.);
#10630=FACE_OUTER_BOUND('',#16787,.T.);
#10631=FACE_OUTER_BOUND('',#16788,.T.);
#10632=FACE_OUTER_BOUND('',#16789,.T.);
#10633=FACE_OUTER_BOUND('',#16790,.T.);
#10634=FACE_OUTER_BOUND('',#16791,.T.);
#10635=FACE_OUTER_BOUND('',#16792,.T.);
#10636=FACE_OUTER_BOUND('',#16793,.T.);
#10637=FACE_OUTER_BOUND('',#16794,.T.);
#10638=FACE_OUTER_BOUND('',#16795,.T.);
#10639=FACE_OUTER_BOUND('',#16796,.T.);
#10640=FACE_OUTER_BOUND('',#16797,.T.);
#10641=FACE_OUTER_BOUND('',#16798,.T.);
#10642=FACE_OUTER_BOUND('',#16799,.T.);
#10643=FACE_OUTER_BOUND('',#16800,.T.);
#10644=FACE_OUTER_BOUND('',#16801,.T.);
#10645=FACE_OUTER_BOUND('',#16802,.T.);
#10646=FACE_OUTER_BOUND('',#16803,.T.);
#10647=FACE_OUTER_BOUND('',#16804,.T.);
#10648=FACE_OUTER_BOUND('',#16805,.T.);
#10649=FACE_OUTER_BOUND('',#16806,.T.);
#10650=FACE_OUTER_BOUND('',#16807,.T.);
#10651=FACE_OUTER_BOUND('',#16808,.T.);
#10652=FACE_OUTER_BOUND('',#16809,.T.);
#10653=FACE_OUTER_BOUND('',#16810,.T.);
#10654=FACE_OUTER_BOUND('',#16811,.T.);
#10655=FACE_OUTER_BOUND('',#16812,.T.);
#10656=FACE_OUTER_BOUND('',#16813,.T.);
#10657=FACE_OUTER_BOUND('',#16814,.T.);
#10658=FACE_OUTER_BOUND('',#16815,.T.);
#10659=FACE_OUTER_BOUND('',#16816,.T.);
#10660=FACE_OUTER_BOUND('',#16817,.T.);
#10661=FACE_OUTER_BOUND('',#16818,.T.);
#10662=FACE_OUTER_BOUND('',#16819,.T.);
#10663=FACE_OUTER_BOUND('',#16820,.T.);
#10664=FACE_OUTER_BOUND('',#16821,.T.);
#10665=FACE_OUTER_BOUND('',#16822,.T.);
#10666=FACE_OUTER_BOUND('',#16823,.T.);
#10667=FACE_OUTER_BOUND('',#16824,.T.);
#10668=FACE_OUTER_BOUND('',#16825,.T.);
#10669=FACE_OUTER_BOUND('',#16826,.T.);
#10670=FACE_OUTER_BOUND('',#16827,.T.);
#10671=FACE_OUTER_BOUND('',#16828,.T.);
#10672=FACE_OUTER_BOUND('',#16829,.T.);
#10673=FACE_OUTER_BOUND('',#16830,.T.);
#10674=FACE_OUTER_BOUND('',#16831,.T.);
#10675=FACE_OUTER_BOUND('',#16832,.T.);
#10676=FACE_OUTER_BOUND('',#16833,.T.);
#10677=FACE_OUTER_BOUND('',#16834,.T.);
#10678=FACE_OUTER_BOUND('',#16835,.T.);
#10679=FACE_OUTER_BOUND('',#16836,.T.);
#10680=FACE_OUTER_BOUND('',#16837,.T.);
#10681=FACE_OUTER_BOUND('',#16838,.T.);
#10682=FACE_OUTER_BOUND('',#16839,.T.);
#10683=FACE_OUTER_BOUND('',#16840,.T.);
#10684=FACE_OUTER_BOUND('',#16841,.T.);
#10685=FACE_OUTER_BOUND('',#16842,.T.);
#10686=FACE_OUTER_BOUND('',#16843,.T.);
#10687=FACE_OUTER_BOUND('',#16844,.T.);
#10688=FACE_OUTER_BOUND('',#16845,.T.);
#10689=FACE_OUTER_BOUND('',#16846,.T.);
#10690=FACE_OUTER_BOUND('',#16847,.T.);
#10691=FACE_OUTER_BOUND('',#16848,.T.);
#10692=FACE_OUTER_BOUND('',#16849,.T.);
#10693=FACE_OUTER_BOUND('',#16850,.T.);
#10694=FACE_OUTER_BOUND('',#16851,.T.);
#10695=FACE_OUTER_BOUND('',#16852,.T.);
#10696=FACE_OUTER_BOUND('',#16853,.T.);
#10697=FACE_OUTER_BOUND('',#16854,.T.);
#10698=FACE_OUTER_BOUND('',#16855,.T.);
#10699=FACE_OUTER_BOUND('',#16856,.T.);
#10700=FACE_OUTER_BOUND('',#16857,.T.);
#10701=FACE_OUTER_BOUND('',#16858,.T.);
#10702=FACE_OUTER_BOUND('',#16859,.T.);
#10703=FACE_OUTER_BOUND('',#16860,.T.);
#10704=FACE_OUTER_BOUND('',#16861,.T.);
#10705=FACE_OUTER_BOUND('',#16862,.T.);
#10706=FACE_OUTER_BOUND('',#16863,.T.);
#10707=FACE_OUTER_BOUND('',#16864,.T.);
#10708=FACE_OUTER_BOUND('',#16865,.T.);
#10709=FACE_OUTER_BOUND('',#16866,.T.);
#10710=FACE_OUTER_BOUND('',#16867,.T.);
#10711=FACE_OUTER_BOUND('',#16868,.T.);
#10712=FACE_OUTER_BOUND('',#16869,.T.);
#10713=FACE_OUTER_BOUND('',#16870,.T.);
#10714=FACE_OUTER_BOUND('',#16871,.T.);
#10715=FACE_OUTER_BOUND('',#16872,.T.);
#10716=FACE_OUTER_BOUND('',#16873,.T.);
#10717=FACE_OUTER_BOUND('',#16874,.T.);
#10718=FACE_OUTER_BOUND('',#16875,.T.);
#10719=FACE_OUTER_BOUND('',#16876,.T.);
#10720=FACE_OUTER_BOUND('',#16877,.T.);
#10721=FACE_OUTER_BOUND('',#16878,.T.);
#10722=FACE_OUTER_BOUND('',#16879,.T.);
#10723=FACE_OUTER_BOUND('',#16880,.T.);
#10724=FACE_OUTER_BOUND('',#16881,.T.);
#10725=FACE_OUTER_BOUND('',#16882,.T.);
#10726=FACE_OUTER_BOUND('',#16883,.T.);
#10727=FACE_OUTER_BOUND('',#16884,.T.);
#10728=FACE_OUTER_BOUND('',#16885,.T.);
#10729=FACE_OUTER_BOUND('',#16886,.T.);
#10730=FACE_OUTER_BOUND('',#16887,.T.);
#10731=FACE_OUTER_BOUND('',#16888,.T.);
#10732=FACE_OUTER_BOUND('',#16889,.T.);
#10733=FACE_OUTER_BOUND('',#16890,.T.);
#10734=FACE_OUTER_BOUND('',#16891,.T.);
#10735=FACE_OUTER_BOUND('',#16892,.T.);
#10736=FACE_OUTER_BOUND('',#16893,.T.);
#10737=FACE_OUTER_BOUND('',#16894,.T.);
#10738=FACE_OUTER_BOUND('',#16895,.T.);
#10739=FACE_OUTER_BOUND('',#16896,.T.);
#10740=FACE_OUTER_BOUND('',#16897,.T.);
#10741=FACE_OUTER_BOUND('',#16898,.T.);
#10742=FACE_OUTER_BOUND('',#16899,.T.);
#10743=FACE_OUTER_BOUND('',#16900,.T.);
#10744=FACE_OUTER_BOUND('',#16901,.T.);
#10745=FACE_OUTER_BOUND('',#16902,.T.);
#10746=FACE_OUTER_BOUND('',#16903,.T.);
#10747=FACE_OUTER_BOUND('',#16904,.T.);
#10748=FACE_OUTER_BOUND('',#16905,.T.);
#10749=FACE_OUTER_BOUND('',#16906,.T.);
#10750=FACE_OUTER_BOUND('',#16907,.T.);
#10751=FACE_OUTER_BOUND('',#16908,.T.);
#10752=FACE_OUTER_BOUND('',#16909,.T.);
#10753=FACE_OUTER_BOUND('',#16910,.T.);
#10754=FACE_OUTER_BOUND('',#16911,.T.);
#10755=FACE_OUTER_BOUND('',#16912,.T.);
#10756=FACE_OUTER_BOUND('',#16913,.T.);
#10757=FACE_OUTER_BOUND('',#16914,.T.);
#10758=FACE_OUTER_BOUND('',#16915,.T.);
#10759=FACE_OUTER_BOUND('',#16916,.T.);
#10760=FACE_OUTER_BOUND('',#16917,.T.);
#10761=FACE_OUTER_BOUND('',#16918,.T.);
#10762=FACE_OUTER_BOUND('',#16919,.T.);
#10763=FACE_OUTER_BOUND('',#16920,.T.);
#10764=FACE_OUTER_BOUND('',#16921,.T.);
#10765=FACE_OUTER_BOUND('',#16922,.T.);
#10766=FACE_OUTER_BOUND('',#16923,.T.);
#10767=FACE_OUTER_BOUND('',#16924,.T.);
#10768=FACE_OUTER_BOUND('',#16925,.T.);
#10769=FACE_OUTER_BOUND('',#16926,.T.);
#10770=FACE_OUTER_BOUND('',#16927,.T.);
#10771=FACE_OUTER_BOUND('',#16928,.T.);
#10772=FACE_OUTER_BOUND('',#16929,.T.);
#10773=FACE_OUTER_BOUND('',#16930,.T.);
#10774=FACE_OUTER_BOUND('',#16931,.T.);
#10775=FACE_OUTER_BOUND('',#16932,.T.);
#10776=FACE_OUTER_BOUND('',#16933,.T.);
#10777=FACE_OUTER_BOUND('',#16934,.T.);
#10778=FACE_OUTER_BOUND('',#16935,.T.);
#10779=FACE_OUTER_BOUND('',#16936,.T.);
#10780=FACE_OUTER_BOUND('',#16937,.T.);
#10781=FACE_OUTER_BOUND('',#16938,.T.);
#10782=FACE_OUTER_BOUND('',#16939,.T.);
#10783=FACE_OUTER_BOUND('',#16940,.T.);
#10784=FACE_OUTER_BOUND('',#16941,.T.);
#10785=FACE_OUTER_BOUND('',#16942,.T.);
#10786=FACE_OUTER_BOUND('',#16943,.T.);
#10787=FACE_OUTER_BOUND('',#16944,.T.);
#10788=FACE_OUTER_BOUND('',#16945,.T.);
#10789=FACE_OUTER_BOUND('',#16946,.T.);
#10790=FACE_OUTER_BOUND('',#16947,.T.);
#10791=FACE_OUTER_BOUND('',#16948,.T.);
#10792=FACE_OUTER_BOUND('',#16949,.T.);
#10793=FACE_OUTER_BOUND('',#16950,.T.);
#10794=FACE_OUTER_BOUND('',#16951,.T.);
#10795=FACE_OUTER_BOUND('',#16952,.T.);
#10796=FACE_OUTER_BOUND('',#16953,.T.);
#10797=FACE_OUTER_BOUND('',#16954,.T.);
#10798=FACE_OUTER_BOUND('',#16955,.T.);
#10799=FACE_OUTER_BOUND('',#16956,.T.);
#10800=FACE_OUTER_BOUND('',#16957,.T.);
#10801=FACE_OUTER_BOUND('',#16958,.T.);
#10802=FACE_OUTER_BOUND('',#16959,.T.);
#10803=FACE_OUTER_BOUND('',#16960,.T.);
#10804=FACE_OUTER_BOUND('',#16961,.T.);
#10805=FACE_OUTER_BOUND('',#16962,.T.);
#10806=FACE_OUTER_BOUND('',#16963,.T.);
#10807=FACE_OUTER_BOUND('',#16964,.T.);
#10808=FACE_OUTER_BOUND('',#16965,.T.);
#10809=FACE_OUTER_BOUND('',#16966,.T.);
#10810=FACE_OUTER_BOUND('',#16967,.T.);
#10811=FACE_OUTER_BOUND('',#16968,.T.);
#10812=FACE_OUTER_BOUND('',#16969,.T.);
#10813=FACE_OUTER_BOUND('',#16970,.T.);
#10814=FACE_OUTER_BOUND('',#16971,.T.);
#10815=FACE_OUTER_BOUND('',#16972,.T.);
#10816=FACE_OUTER_BOUND('',#16973,.T.);
#10817=FACE_OUTER_BOUND('',#16974,.T.);
#10818=FACE_OUTER_BOUND('',#16975,.T.);
#10819=FACE_OUTER_BOUND('',#16976,.T.);
#10820=FACE_OUTER_BOUND('',#16977,.T.);
#10821=FACE_OUTER_BOUND('',#16978,.T.);
#10822=FACE_OUTER_BOUND('',#16979,.T.);
#10823=FACE_OUTER_BOUND('',#16980,.T.);
#10824=FACE_OUTER_BOUND('',#16981,.T.);
#10825=FACE_OUTER_BOUND('',#16982,.T.);
#10826=FACE_OUTER_BOUND('',#16983,.T.);
#10827=FACE_OUTER_BOUND('',#16984,.T.);
#10828=FACE_OUTER_BOUND('',#16985,.T.);
#10829=FACE_OUTER_BOUND('',#16986,.T.);
#10830=FACE_OUTER_BOUND('',#16987,.T.);
#10831=FACE_OUTER_BOUND('',#16988,.T.);
#10832=FACE_OUTER_BOUND('',#16989,.T.);
#10833=FACE_OUTER_BOUND('',#16990,.T.);
#10834=FACE_OUTER_BOUND('',#16991,.T.);
#10835=FACE_OUTER_BOUND('',#16992,.T.);
#10836=FACE_OUTER_BOUND('',#16993,.T.);
#10837=FACE_OUTER_BOUND('',#16994,.T.);
#10838=FACE_OUTER_BOUND('',#16995,.T.);
#10839=FACE_OUTER_BOUND('',#16996,.T.);
#10840=FACE_OUTER_BOUND('',#16997,.T.);
#10841=FACE_OUTER_BOUND('',#16998,.T.);
#10842=FACE_OUTER_BOUND('',#16999,.T.);
#10843=FACE_OUTER_BOUND('',#17000,.T.);
#10844=FACE_OUTER_BOUND('',#17001,.T.);
#10845=FACE_OUTER_BOUND('',#17002,.T.);
#10846=FACE_OUTER_BOUND('',#17003,.T.);
#10847=FACE_OUTER_BOUND('',#17004,.T.);
#10848=FACE_OUTER_BOUND('',#17005,.T.);
#10849=FACE_OUTER_BOUND('',#17006,.T.);
#10850=FACE_OUTER_BOUND('',#17007,.T.);
#10851=FACE_OUTER_BOUND('',#17008,.T.);
#10852=FACE_OUTER_BOUND('',#17009,.T.);
#10853=FACE_OUTER_BOUND('',#17010,.T.);
#10854=FACE_OUTER_BOUND('',#17012,.T.);
#10855=FACE_OUTER_BOUND('',#17013,.T.);
#10856=FACE_OUTER_BOUND('',#17014,.T.);
#10857=FACE_OUTER_BOUND('',#17015,.T.);
#10858=FACE_OUTER_BOUND('',#17016,.T.);
#10859=FACE_OUTER_BOUND('',#17017,.T.);
#10860=FACE_OUTER_BOUND('',#17019,.T.);
#10861=FACE_OUTER_BOUND('',#17021,.T.);
#10862=FACE_OUTER_BOUND('',#17022,.T.);
#10863=FACE_OUTER_BOUND('',#17023,.T.);
#10864=FACE_OUTER_BOUND('',#17024,.T.);
#10865=FACE_OUTER_BOUND('',#17025,.T.);
#10866=FACE_OUTER_BOUND('',#17026,.T.);
#10867=FACE_OUTER_BOUND('',#17027,.T.);
#10868=FACE_OUTER_BOUND('',#17028,.T.);
#10869=FACE_OUTER_BOUND('',#17029,.T.);
#10870=FACE_OUTER_BOUND('',#17030,.T.);
#10871=FACE_OUTER_BOUND('',#17031,.T.);
#10872=FACE_OUTER_BOUND('',#17032,.T.);
#10873=FACE_OUTER_BOUND('',#17033,.T.);
#10874=FACE_OUTER_BOUND('',#17034,.T.);
#10875=FACE_OUTER_BOUND('',#17035,.T.);
#10876=FACE_OUTER_BOUND('',#17036,.T.);
#10877=FACE_OUTER_BOUND('',#17037,.T.);
#10878=FACE_OUTER_BOUND('',#17038,.T.);
#10879=FACE_OUTER_BOUND('',#17039,.T.);
#10880=FACE_OUTER_BOUND('',#17040,.T.);
#10881=FACE_OUTER_BOUND('',#17041,.T.);
#10882=FACE_OUTER_BOUND('',#17042,.T.);
#10883=FACE_OUTER_BOUND('',#17043,.T.);
#10884=FACE_OUTER_BOUND('',#17044,.T.);
#10885=FACE_OUTER_BOUND('',#17045,.T.);
#10886=FACE_OUTER_BOUND('',#17046,.T.);
#10887=FACE_OUTER_BOUND('',#17047,.T.);
#10888=FACE_OUTER_BOUND('',#17048,.T.);
#10889=FACE_OUTER_BOUND('',#17049,.T.);
#10890=FACE_OUTER_BOUND('',#17050,.T.);
#10891=FACE_OUTER_BOUND('',#17051,.T.);
#10892=FACE_OUTER_BOUND('',#17052,.T.);
#10893=FACE_OUTER_BOUND('',#17053,.T.);
#10894=FACE_OUTER_BOUND('',#17054,.T.);
#10895=FACE_OUTER_BOUND('',#17055,.T.);
#10896=FACE_OUTER_BOUND('',#17056,.T.);
#10897=FACE_OUTER_BOUND('',#17057,.T.);
#10898=FACE_OUTER_BOUND('',#17058,.T.);
#10899=FACE_OUTER_BOUND('',#17059,.T.);
#10900=FACE_OUTER_BOUND('',#17060,.T.);
#10901=FACE_OUTER_BOUND('',#17061,.T.);
#10902=FACE_OUTER_BOUND('',#17062,.T.);
#10903=FACE_OUTER_BOUND('',#17063,.T.);
#10904=FACE_OUTER_BOUND('',#17064,.T.);
#10905=FACE_OUTER_BOUND('',#17065,.T.);
#10906=FACE_OUTER_BOUND('',#17066,.T.);
#10907=FACE_OUTER_BOUND('',#17067,.T.);
#10908=FACE_OUTER_BOUND('',#17068,.T.);
#10909=FACE_OUTER_BOUND('',#17069,.T.);
#10910=FACE_OUTER_BOUND('',#17070,.T.);
#10911=FACE_OUTER_BOUND('',#17071,.T.);
#10912=FACE_OUTER_BOUND('',#17072,.T.);
#10913=FACE_OUTER_BOUND('',#17073,.T.);
#10914=FACE_OUTER_BOUND('',#17074,.T.);
#10915=FACE_OUTER_BOUND('',#17075,.T.);
#10916=FACE_OUTER_BOUND('',#17076,.T.);
#10917=FACE_OUTER_BOUND('',#17077,.T.);
#10918=FACE_OUTER_BOUND('',#17078,.T.);
#10919=FACE_OUTER_BOUND('',#17079,.T.);
#10920=FACE_OUTER_BOUND('',#17080,.T.);
#10921=FACE_OUTER_BOUND('',#17081,.T.);
#10922=FACE_OUTER_BOUND('',#17082,.T.);
#10923=FACE_OUTER_BOUND('',#17083,.T.);
#10924=FACE_OUTER_BOUND('',#17084,.T.);
#10925=FACE_OUTER_BOUND('',#17085,.T.);
#10926=FACE_OUTER_BOUND('',#17086,.T.);
#10927=FACE_OUTER_BOUND('',#17087,.T.);
#10928=FACE_OUTER_BOUND('',#17088,.T.);
#10929=FACE_OUTER_BOUND('',#17089,.T.);
#10930=FACE_OUTER_BOUND('',#17090,.T.);
#10931=FACE_OUTER_BOUND('',#17091,.T.);
#10932=FACE_OUTER_BOUND('',#17092,.T.);
#10933=FACE_OUTER_BOUND('',#17093,.T.);
#10934=FACE_OUTER_BOUND('',#17094,.T.);
#10935=FACE_OUTER_BOUND('',#17095,.T.);
#10936=FACE_OUTER_BOUND('',#17096,.T.);
#10937=FACE_OUTER_BOUND('',#17097,.T.);
#10938=FACE_OUTER_BOUND('',#17098,.T.);
#10939=FACE_OUTER_BOUND('',#17099,.T.);
#10940=FACE_OUTER_BOUND('',#17100,.T.);
#10941=FACE_OUTER_BOUND('',#17101,.T.);
#10942=FACE_OUTER_BOUND('',#17102,.T.);
#10943=FACE_OUTER_BOUND('',#17103,.T.);
#10944=FACE_OUTER_BOUND('',#17104,.T.);
#10945=FACE_OUTER_BOUND('',#17105,.T.);
#10946=FACE_OUTER_BOUND('',#17106,.T.);
#10947=FACE_OUTER_BOUND('',#17107,.T.);
#10948=FACE_OUTER_BOUND('',#17108,.T.);
#10949=FACE_OUTER_BOUND('',#17109,.T.);
#10950=FACE_OUTER_BOUND('',#17110,.T.);
#10951=FACE_OUTER_BOUND('',#17111,.T.);
#10952=FACE_OUTER_BOUND('',#17112,.T.);
#10953=FACE_OUTER_BOUND('',#17113,.T.);
#10954=FACE_OUTER_BOUND('',#17114,.T.);
#10955=FACE_OUTER_BOUND('',#17115,.T.);
#10956=FACE_OUTER_BOUND('',#17116,.T.);
#10957=FACE_OUTER_BOUND('',#17117,.T.);
#10958=FACE_OUTER_BOUND('',#17118,.T.);
#10959=FACE_OUTER_BOUND('',#17119,.T.);
#10960=FACE_OUTER_BOUND('',#17120,.T.);
#10961=FACE_OUTER_BOUND('',#17121,.T.);
#10962=FACE_OUTER_BOUND('',#17122,.T.);
#10963=FACE_OUTER_BOUND('',#17123,.T.);
#10964=FACE_OUTER_BOUND('',#17124,.T.);
#10965=FACE_OUTER_BOUND('',#17125,.T.);
#10966=FACE_OUTER_BOUND('',#17126,.T.);
#10967=FACE_OUTER_BOUND('',#17127,.T.);
#10968=FACE_OUTER_BOUND('',#17128,.T.);
#10969=FACE_OUTER_BOUND('',#17129,.T.);
#10970=FACE_OUTER_BOUND('',#17130,.T.);
#10971=FACE_OUTER_BOUND('',#17131,.T.);
#10972=FACE_OUTER_BOUND('',#17132,.T.);
#10973=FACE_OUTER_BOUND('',#17133,.T.);
#10974=FACE_OUTER_BOUND('',#17134,.T.);
#10975=FACE_OUTER_BOUND('',#17135,.T.);
#10976=FACE_OUTER_BOUND('',#17136,.T.);
#10977=FACE_OUTER_BOUND('',#17137,.T.);
#10978=FACE_OUTER_BOUND('',#17138,.T.);
#10979=FACE_OUTER_BOUND('',#17139,.T.);
#10980=FACE_OUTER_BOUND('',#17140,.T.);
#10981=FACE_OUTER_BOUND('',#17141,.T.);
#10982=FACE_OUTER_BOUND('',#17142,.T.);
#10983=FACE_OUTER_BOUND('',#17143,.T.);
#10984=FACE_OUTER_BOUND('',#17144,.T.);
#10985=FACE_OUTER_BOUND('',#17145,.T.);
#10986=FACE_OUTER_BOUND('',#17146,.T.);
#10987=FACE_OUTER_BOUND('',#17147,.T.);
#10988=FACE_OUTER_BOUND('',#17148,.T.);
#10989=FACE_OUTER_BOUND('',#17149,.T.);
#10990=FACE_OUTER_BOUND('',#17150,.T.);
#10991=FACE_OUTER_BOUND('',#17151,.T.);
#10992=FACE_OUTER_BOUND('',#17152,.T.);
#10993=FACE_OUTER_BOUND('',#17153,.T.);
#10994=FACE_OUTER_BOUND('',#17154,.T.);
#10995=FACE_OUTER_BOUND('',#17155,.T.);
#10996=FACE_OUTER_BOUND('',#17156,.T.);
#10997=FACE_OUTER_BOUND('',#17157,.T.);
#10998=FACE_OUTER_BOUND('',#17158,.T.);
#10999=FACE_OUTER_BOUND('',#17159,.T.);
#11000=FACE_OUTER_BOUND('',#17160,.T.);
#11001=FACE_OUTER_BOUND('',#17161,.T.);
#11002=FACE_OUTER_BOUND('',#17162,.T.);
#11003=FACE_OUTER_BOUND('',#17163,.T.);
#11004=FACE_OUTER_BOUND('',#17164,.T.);
#11005=FACE_OUTER_BOUND('',#17165,.T.);
#11006=FACE_OUTER_BOUND('',#17166,.T.);
#11007=FACE_OUTER_BOUND('',#17167,.T.);
#11008=FACE_OUTER_BOUND('',#17168,.T.);
#11009=FACE_OUTER_BOUND('',#17169,.T.);
#11010=FACE_OUTER_BOUND('',#17170,.T.);
#11011=FACE_OUTER_BOUND('',#17171,.T.);
#11012=FACE_OUTER_BOUND('',#17172,.T.);
#11013=FACE_OUTER_BOUND('',#17173,.T.);
#11014=FACE_OUTER_BOUND('',#17174,.T.);
#11015=FACE_OUTER_BOUND('',#17175,.T.);
#11016=FACE_OUTER_BOUND('',#17176,.T.);
#11017=FACE_OUTER_BOUND('',#17177,.T.);
#11018=FACE_OUTER_BOUND('',#17178,.T.);
#11019=FACE_OUTER_BOUND('',#17179,.T.);
#11020=FACE_OUTER_BOUND('',#17180,.T.);
#11021=FACE_OUTER_BOUND('',#17181,.T.);
#11022=FACE_OUTER_BOUND('',#17182,.T.);
#11023=FACE_OUTER_BOUND('',#17183,.T.);
#11024=FACE_OUTER_BOUND('',#17184,.T.);
#11025=FACE_OUTER_BOUND('',#17185,.T.);
#11026=FACE_OUTER_BOUND('',#17186,.T.);
#11027=FACE_OUTER_BOUND('',#17187,.T.);
#11028=FACE_OUTER_BOUND('',#17188,.T.);
#11029=FACE_OUTER_BOUND('',#17189,.T.);
#11030=FACE_OUTER_BOUND('',#17190,.T.);
#11031=FACE_OUTER_BOUND('',#17191,.T.);
#11032=FACE_OUTER_BOUND('',#17192,.T.);
#11033=FACE_OUTER_BOUND('',#17193,.T.);
#11034=FACE_OUTER_BOUND('',#17194,.T.);
#11035=FACE_OUTER_BOUND('',#17195,.T.);
#11036=FACE_OUTER_BOUND('',#17196,.T.);
#11037=FACE_OUTER_BOUND('',#17197,.T.);
#11038=FACE_OUTER_BOUND('',#17198,.T.);
#11039=FACE_OUTER_BOUND('',#17199,.T.);
#11040=FACE_OUTER_BOUND('',#17200,.T.);
#11041=FACE_OUTER_BOUND('',#17201,.T.);
#11042=FACE_OUTER_BOUND('',#17202,.T.);
#11043=FACE_OUTER_BOUND('',#17203,.T.);
#11044=FACE_OUTER_BOUND('',#17204,.T.);
#11045=FACE_OUTER_BOUND('',#17205,.T.);
#11046=FACE_OUTER_BOUND('',#17206,.T.);
#11047=FACE_OUTER_BOUND('',#17207,.T.);
#11048=FACE_OUTER_BOUND('',#17208,.T.);
#11049=FACE_OUTER_BOUND('',#17209,.T.);
#11050=FACE_OUTER_BOUND('',#17210,.T.);
#11051=FACE_OUTER_BOUND('',#17211,.T.);
#11052=FACE_OUTER_BOUND('',#17212,.T.);
#11053=FACE_OUTER_BOUND('',#17213,.T.);
#11054=FACE_OUTER_BOUND('',#17214,.T.);
#11055=FACE_OUTER_BOUND('',#17215,.T.);
#11056=FACE_OUTER_BOUND('',#17216,.T.);
#11057=FACE_OUTER_BOUND('',#17217,.T.);
#11058=FACE_OUTER_BOUND('',#17218,.T.);
#11059=FACE_OUTER_BOUND('',#17219,.T.);
#11060=FACE_OUTER_BOUND('',#17220,.T.);
#11061=FACE_OUTER_BOUND('',#17221,.T.);
#11062=FACE_OUTER_BOUND('',#17222,.T.);
#11063=FACE_OUTER_BOUND('',#17223,.T.);
#11064=FACE_OUTER_BOUND('',#17224,.T.);
#11065=FACE_OUTER_BOUND('',#17225,.T.);
#11066=FACE_OUTER_BOUND('',#17226,.T.);
#11067=FACE_OUTER_BOUND('',#17227,.T.);
#11068=FACE_OUTER_BOUND('',#17228,.T.);
#11069=FACE_OUTER_BOUND('',#17229,.T.);
#11070=FACE_OUTER_BOUND('',#17230,.T.);
#11071=FACE_OUTER_BOUND('',#17231,.T.);
#11072=FACE_OUTER_BOUND('',#17232,.T.);
#11073=FACE_OUTER_BOUND('',#17233,.T.);
#11074=FACE_OUTER_BOUND('',#17234,.T.);
#11075=FACE_OUTER_BOUND('',#17235,.T.);
#11076=FACE_OUTER_BOUND('',#17236,.T.);
#11077=FACE_OUTER_BOUND('',#17237,.T.);
#11078=FACE_OUTER_BOUND('',#17238,.T.);
#11079=FACE_OUTER_BOUND('',#17239,.T.);
#11080=FACE_OUTER_BOUND('',#17240,.T.);
#11081=FACE_OUTER_BOUND('',#17241,.T.);
#11082=FACE_OUTER_BOUND('',#17242,.T.);
#11083=FACE_OUTER_BOUND('',#17243,.T.);
#11084=FACE_OUTER_BOUND('',#17244,.T.);
#11085=FACE_OUTER_BOUND('',#17245,.T.);
#11086=FACE_OUTER_BOUND('',#17246,.T.);
#11087=FACE_OUTER_BOUND('',#17247,.T.);
#11088=FACE_OUTER_BOUND('',#17248,.T.);
#11089=FACE_OUTER_BOUND('',#17249,.T.);
#11090=FACE_OUTER_BOUND('',#17250,.T.);
#11091=FACE_OUTER_BOUND('',#17251,.T.);
#11092=FACE_OUTER_BOUND('',#17252,.T.);
#11093=FACE_OUTER_BOUND('',#17253,.T.);
#11094=FACE_OUTER_BOUND('',#17254,.T.);
#11095=FACE_OUTER_BOUND('',#17255,.T.);
#11096=FACE_OUTER_BOUND('',#17256,.T.);
#11097=FACE_OUTER_BOUND('',#17257,.T.);
#11098=FACE_OUTER_BOUND('',#17258,.T.);
#11099=FACE_OUTER_BOUND('',#17259,.T.);
#11100=FACE_OUTER_BOUND('',#17260,.T.);
#11101=FACE_OUTER_BOUND('',#17261,.T.);
#11102=FACE_OUTER_BOUND('',#17262,.T.);
#11103=FACE_OUTER_BOUND('',#17263,.T.);
#11104=FACE_OUTER_BOUND('',#17264,.T.);
#11105=FACE_OUTER_BOUND('',#17265,.T.);
#11106=FACE_OUTER_BOUND('',#17266,.T.);
#11107=FACE_OUTER_BOUND('',#17267,.T.);
#11108=FACE_OUTER_BOUND('',#17268,.T.);
#11109=FACE_OUTER_BOUND('',#17269,.T.);
#11110=FACE_OUTER_BOUND('',#17270,.T.);
#11111=FACE_OUTER_BOUND('',#17271,.T.);
#11112=FACE_OUTER_BOUND('',#17272,.T.);
#11113=FACE_OUTER_BOUND('',#17273,.T.);
#11114=FACE_OUTER_BOUND('',#17274,.T.);
#11115=FACE_OUTER_BOUND('',#17275,.T.);
#11116=FACE_OUTER_BOUND('',#17276,.T.);
#11117=FACE_OUTER_BOUND('',#17277,.T.);
#11118=FACE_OUTER_BOUND('',#17278,.T.);
#11119=FACE_OUTER_BOUND('',#17279,.T.);
#11120=FACE_OUTER_BOUND('',#17280,.T.);
#11121=FACE_OUTER_BOUND('',#17281,.T.);
#11122=FACE_OUTER_BOUND('',#17282,.T.);
#11123=FACE_OUTER_BOUND('',#17283,.T.);
#11124=FACE_OUTER_BOUND('',#17284,.T.);
#11125=FACE_OUTER_BOUND('',#17285,.T.);
#11126=FACE_OUTER_BOUND('',#17286,.T.);
#11127=FACE_OUTER_BOUND('',#17287,.T.);
#11128=FACE_OUTER_BOUND('',#17288,.T.);
#11129=FACE_OUTER_BOUND('',#17289,.T.);
#11130=FACE_OUTER_BOUND('',#17290,.T.);
#11131=FACE_OUTER_BOUND('',#17291,.T.);
#11132=FACE_OUTER_BOUND('',#17292,.T.);
#11133=FACE_OUTER_BOUND('',#17293,.T.);
#11134=FACE_OUTER_BOUND('',#17294,.T.);
#11135=FACE_OUTER_BOUND('',#17295,.T.);
#11136=FACE_OUTER_BOUND('',#17296,.T.);
#11137=FACE_OUTER_BOUND('',#17297,.T.);
#11138=FACE_OUTER_BOUND('',#17298,.T.);
#11139=FACE_OUTER_BOUND('',#17299,.T.);
#11140=FACE_OUTER_BOUND('',#17300,.T.);
#11141=FACE_OUTER_BOUND('',#17301,.T.);
#11142=FACE_OUTER_BOUND('',#17302,.T.);
#11143=FACE_OUTER_BOUND('',#17303,.T.);
#11144=FACE_OUTER_BOUND('',#17304,.T.);
#11145=FACE_OUTER_BOUND('',#17305,.T.);
#11146=FACE_OUTER_BOUND('',#17306,.T.);
#11147=FACE_OUTER_BOUND('',#17307,.T.);
#11148=FACE_OUTER_BOUND('',#17308,.T.);
#11149=FACE_OUTER_BOUND('',#17309,.T.);
#11150=FACE_OUTER_BOUND('',#17310,.T.);
#11151=FACE_OUTER_BOUND('',#17311,.T.);
#11152=FACE_OUTER_BOUND('',#17312,.T.);
#11153=FACE_OUTER_BOUND('',#17313,.T.);
#11154=FACE_OUTER_BOUND('',#17314,.T.);
#11155=FACE_OUTER_BOUND('',#17315,.T.);
#11156=FACE_OUTER_BOUND('',#17316,.T.);
#11157=FACE_OUTER_BOUND('',#17317,.T.);
#11158=FACE_OUTER_BOUND('',#17318,.T.);
#11159=FACE_OUTER_BOUND('',#17319,.T.);
#11160=FACE_OUTER_BOUND('',#17320,.T.);
#11161=FACE_OUTER_BOUND('',#17321,.T.);
#11162=FACE_OUTER_BOUND('',#17322,.T.);
#11163=FACE_OUTER_BOUND('',#17323,.T.);
#11164=FACE_OUTER_BOUND('',#17324,.T.);
#11165=FACE_OUTER_BOUND('',#17325,.T.);
#11166=FACE_OUTER_BOUND('',#17326,.T.);
#11167=FACE_OUTER_BOUND('',#17327,.T.);
#11168=FACE_OUTER_BOUND('',#17328,.T.);
#11169=FACE_OUTER_BOUND('',#17329,.T.);
#11170=FACE_OUTER_BOUND('',#17330,.T.);
#11171=FACE_OUTER_BOUND('',#17331,.T.);
#11172=FACE_OUTER_BOUND('',#17332,.T.);
#11173=FACE_OUTER_BOUND('',#17333,.T.);
#11174=FACE_OUTER_BOUND('',#17334,.T.);
#11175=FACE_OUTER_BOUND('',#17335,.T.);
#11176=FACE_OUTER_BOUND('',#17336,.T.);
#11177=FACE_OUTER_BOUND('',#17337,.T.);
#11178=FACE_OUTER_BOUND('',#17338,.T.);
#11179=FACE_OUTER_BOUND('',#17339,.T.);
#11180=FACE_OUTER_BOUND('',#17340,.T.);
#11181=FACE_OUTER_BOUND('',#17341,.T.);
#11182=FACE_OUTER_BOUND('',#17342,.T.);
#11183=FACE_OUTER_BOUND('',#17343,.T.);
#11184=FACE_OUTER_BOUND('',#17344,.T.);
#11185=FACE_OUTER_BOUND('',#17345,.T.);
#11186=FACE_OUTER_BOUND('',#17346,.T.);
#11187=FACE_OUTER_BOUND('',#17347,.T.);
#11188=FACE_OUTER_BOUND('',#17348,.T.);
#11189=FACE_OUTER_BOUND('',#17349,.T.);
#11190=FACE_OUTER_BOUND('',#17350,.T.);
#11191=FACE_OUTER_BOUND('',#17351,.T.);
#11192=FACE_OUTER_BOUND('',#17352,.T.);
#11193=FACE_OUTER_BOUND('',#17353,.T.);
#11194=FACE_OUTER_BOUND('',#17354,.T.);
#11195=FACE_OUTER_BOUND('',#17355,.T.);
#11196=FACE_OUTER_BOUND('',#17356,.T.);
#11197=FACE_OUTER_BOUND('',#17357,.T.);
#11198=FACE_OUTER_BOUND('',#17358,.T.);
#11199=FACE_OUTER_BOUND('',#17359,.T.);
#11200=FACE_OUTER_BOUND('',#17360,.T.);
#11201=FACE_OUTER_BOUND('',#17361,.T.);
#11202=FACE_OUTER_BOUND('',#17362,.T.);
#11203=FACE_OUTER_BOUND('',#17363,.T.);
#11204=FACE_OUTER_BOUND('',#17364,.T.);
#11205=FACE_OUTER_BOUND('',#17365,.T.);
#11206=FACE_OUTER_BOUND('',#17366,.T.);
#11207=FACE_OUTER_BOUND('',#17367,.T.);
#11208=FACE_OUTER_BOUND('',#17368,.T.);
#11209=FACE_OUTER_BOUND('',#17369,.T.);
#11210=FACE_OUTER_BOUND('',#17370,.T.);
#11211=FACE_OUTER_BOUND('',#17371,.T.);
#11212=FACE_OUTER_BOUND('',#17372,.T.);
#11213=FACE_OUTER_BOUND('',#17373,.T.);
#11214=FACE_OUTER_BOUND('',#17374,.T.);
#11215=FACE_OUTER_BOUND('',#17375,.T.);
#11216=FACE_OUTER_BOUND('',#17376,.T.);
#11217=FACE_OUTER_BOUND('',#17377,.T.);
#11218=FACE_OUTER_BOUND('',#17378,.T.);
#11219=FACE_OUTER_BOUND('',#17379,.T.);
#11220=FACE_OUTER_BOUND('',#17380,.T.);
#11221=FACE_OUTER_BOUND('',#17381,.T.);
#11222=FACE_OUTER_BOUND('',#17382,.T.);
#11223=FACE_OUTER_BOUND('',#17383,.T.);
#11224=FACE_OUTER_BOUND('',#17384,.T.);
#11225=FACE_OUTER_BOUND('',#17385,.T.);
#11226=FACE_OUTER_BOUND('',#17386,.T.);
#11227=FACE_OUTER_BOUND('',#17387,.T.);
#11228=FACE_OUTER_BOUND('',#17388,.T.);
#11229=FACE_OUTER_BOUND('',#17389,.T.);
#11230=FACE_OUTER_BOUND('',#17390,.T.);
#11231=FACE_OUTER_BOUND('',#17391,.T.);
#11232=FACE_OUTER_BOUND('',#17392,.T.);
#11233=FACE_OUTER_BOUND('',#17393,.T.);
#11234=FACE_OUTER_BOUND('',#17394,.T.);
#11235=FACE_OUTER_BOUND('',#17395,.T.);
#11236=FACE_OUTER_BOUND('',#17396,.T.);
#11237=FACE_OUTER_BOUND('',#17397,.T.);
#11238=FACE_OUTER_BOUND('',#17398,.T.);
#11239=FACE_OUTER_BOUND('',#17399,.T.);
#11240=FACE_OUTER_BOUND('',#17400,.T.);
#11241=FACE_OUTER_BOUND('',#17401,.T.);
#11242=FACE_OUTER_BOUND('',#17402,.T.);
#11243=FACE_OUTER_BOUND('',#17403,.T.);
#11244=FACE_OUTER_BOUND('',#17404,.T.);
#11245=FACE_OUTER_BOUND('',#17405,.T.);
#11246=FACE_OUTER_BOUND('',#17406,.T.);
#11247=FACE_OUTER_BOUND('',#17407,.T.);
#11248=FACE_OUTER_BOUND('',#17408,.T.);
#11249=FACE_OUTER_BOUND('',#17409,.T.);
#11250=FACE_OUTER_BOUND('',#17410,.T.);
#11251=FACE_OUTER_BOUND('',#17411,.T.);
#11252=FACE_OUTER_BOUND('',#17412,.T.);
#11253=FACE_OUTER_BOUND('',#17413,.T.);
#11254=FACE_OUTER_BOUND('',#17414,.T.);
#11255=FACE_OUTER_BOUND('',#17415,.T.);
#11256=FACE_OUTER_BOUND('',#17416,.T.);
#11257=FACE_OUTER_BOUND('',#17417,.T.);
#11258=FACE_OUTER_BOUND('',#17418,.T.);
#11259=FACE_OUTER_BOUND('',#17419,.T.);
#11260=FACE_OUTER_BOUND('',#17420,.T.);
#11261=FACE_OUTER_BOUND('',#17421,.T.);
#11262=FACE_OUTER_BOUND('',#17422,.T.);
#11263=FACE_OUTER_BOUND('',#17423,.T.);
#11264=FACE_OUTER_BOUND('',#17424,.T.);
#11265=FACE_OUTER_BOUND('',#17425,.T.);
#11266=FACE_OUTER_BOUND('',#17426,.T.);
#11267=FACE_OUTER_BOUND('',#17427,.T.);
#11268=FACE_OUTER_BOUND('',#17428,.T.);
#11269=FACE_OUTER_BOUND('',#17429,.T.);
#11270=FACE_OUTER_BOUND('',#17430,.T.);
#11271=FACE_OUTER_BOUND('',#17431,.T.);
#11272=FACE_OUTER_BOUND('',#17432,.T.);
#11273=FACE_OUTER_BOUND('',#17433,.T.);
#11274=FACE_OUTER_BOUND('',#17434,.T.);
#11275=FACE_OUTER_BOUND('',#17435,.T.);
#11276=FACE_OUTER_BOUND('',#17436,.T.);
#11277=FACE_OUTER_BOUND('',#17437,.T.);
#11278=FACE_OUTER_BOUND('',#17438,.T.);
#11279=FACE_OUTER_BOUND('',#17439,.T.);
#11280=FACE_OUTER_BOUND('',#17440,.T.);
#11281=FACE_OUTER_BOUND('',#17441,.T.);
#11282=FACE_OUTER_BOUND('',#17442,.T.);
#11283=FACE_OUTER_BOUND('',#17443,.T.);
#11284=FACE_OUTER_BOUND('',#17444,.T.);
#11285=FACE_OUTER_BOUND('',#17445,.T.);
#11286=FACE_OUTER_BOUND('',#17446,.T.);
#11287=FACE_OUTER_BOUND('',#17447,.T.);
#11288=FACE_OUTER_BOUND('',#17448,.T.);
#11289=FACE_OUTER_BOUND('',#17449,.T.);
#11290=FACE_OUTER_BOUND('',#17450,.T.);
#11291=FACE_OUTER_BOUND('',#17451,.T.);
#11292=FACE_OUTER_BOUND('',#17452,.T.);
#11293=FACE_OUTER_BOUND('',#17453,.T.);
#11294=FACE_OUTER_BOUND('',#17454,.T.);
#11295=FACE_OUTER_BOUND('',#17455,.T.);
#11296=FACE_OUTER_BOUND('',#17456,.T.);
#11297=FACE_OUTER_BOUND('',#17457,.T.);
#11298=FACE_OUTER_BOUND('',#17458,.T.);
#11299=FACE_OUTER_BOUND('',#17459,.T.);
#11300=FACE_OUTER_BOUND('',#17460,.T.);
#11301=FACE_OUTER_BOUND('',#17461,.T.);
#11302=FACE_OUTER_BOUND('',#17462,.T.);
#11303=FACE_OUTER_BOUND('',#17463,.T.);
#11304=FACE_OUTER_BOUND('',#17464,.T.);
#11305=FACE_OUTER_BOUND('',#17465,.T.);
#11306=FACE_OUTER_BOUND('',#17466,.T.);
#11307=FACE_OUTER_BOUND('',#17467,.T.);
#11308=FACE_OUTER_BOUND('',#17468,.T.);
#11309=FACE_OUTER_BOUND('',#17469,.T.);
#11310=FACE_OUTER_BOUND('',#17470,.T.);
#11311=FACE_OUTER_BOUND('',#17471,.T.);
#11312=FACE_OUTER_BOUND('',#17472,.T.);
#11313=FACE_OUTER_BOUND('',#17473,.T.);
#11314=FACE_OUTER_BOUND('',#17474,.T.);
#11315=FACE_OUTER_BOUND('',#17475,.T.);
#11316=FACE_OUTER_BOUND('',#17476,.T.);
#11317=FACE_OUTER_BOUND('',#17477,.T.);
#11318=FACE_OUTER_BOUND('',#17478,.T.);
#11319=FACE_OUTER_BOUND('',#17479,.T.);
#11320=FACE_OUTER_BOUND('',#17480,.T.);
#11321=FACE_OUTER_BOUND('',#17481,.T.);
#11322=FACE_OUTER_BOUND('',#17482,.T.);
#11323=FACE_OUTER_BOUND('',#17483,.T.);
#11324=FACE_OUTER_BOUND('',#17484,.T.);
#11325=FACE_OUTER_BOUND('',#17485,.T.);
#11326=FACE_OUTER_BOUND('',#17486,.T.);
#11327=FACE_OUTER_BOUND('',#17487,.T.);
#11328=FACE_OUTER_BOUND('',#17488,.T.);
#11329=FACE_OUTER_BOUND('',#17489,.T.);
#11330=FACE_OUTER_BOUND('',#17490,.T.);
#11331=FACE_OUTER_BOUND('',#17491,.T.);
#11332=FACE_OUTER_BOUND('',#17492,.T.);
#11333=FACE_OUTER_BOUND('',#17493,.T.);
#11334=FACE_OUTER_BOUND('',#17494,.T.);
#11335=FACE_OUTER_BOUND('',#17495,.T.);
#11336=FACE_OUTER_BOUND('',#17496,.T.);
#11337=FACE_OUTER_BOUND('',#17497,.T.);
#11338=FACE_OUTER_BOUND('',#17498,.T.);
#11339=FACE_OUTER_BOUND('',#17499,.T.);
#11340=FACE_OUTER_BOUND('',#17500,.T.);
#11341=FACE_OUTER_BOUND('',#17501,.T.);
#11342=FACE_OUTER_BOUND('',#17502,.T.);
#11343=FACE_OUTER_BOUND('',#17503,.T.);
#11344=FACE_OUTER_BOUND('',#17504,.T.);
#11345=FACE_OUTER_BOUND('',#17505,.T.);
#11346=FACE_OUTER_BOUND('',#17506,.T.);
#11347=FACE_OUTER_BOUND('',#17507,.T.);
#11348=FACE_OUTER_BOUND('',#17508,.T.);
#11349=FACE_OUTER_BOUND('',#17509,.T.);
#11350=FACE_OUTER_BOUND('',#17510,.T.);
#11351=FACE_OUTER_BOUND('',#17511,.T.);
#11352=FACE_OUTER_BOUND('',#17512,.T.);
#11353=FACE_OUTER_BOUND('',#17513,.T.);
#11354=FACE_OUTER_BOUND('',#17514,.T.);
#11355=FACE_OUTER_BOUND('',#17515,.T.);
#11356=FACE_OUTER_BOUND('',#17516,.T.);
#11357=FACE_OUTER_BOUND('',#17517,.T.);
#11358=FACE_OUTER_BOUND('',#17518,.T.);
#11359=FACE_OUTER_BOUND('',#17519,.T.);
#11360=FACE_OUTER_BOUND('',#17520,.T.);
#11361=FACE_OUTER_BOUND('',#17521,.T.);
#11362=FACE_OUTER_BOUND('',#17522,.T.);
#11363=FACE_OUTER_BOUND('',#17523,.T.);
#11364=FACE_OUTER_BOUND('',#17524,.T.);
#11365=FACE_OUTER_BOUND('',#17525,.T.);
#11366=FACE_OUTER_BOUND('',#17526,.T.);
#11367=FACE_OUTER_BOUND('',#17527,.T.);
#11368=FACE_OUTER_BOUND('',#17528,.T.);
#11369=FACE_OUTER_BOUND('',#17529,.T.);
#11370=FACE_OUTER_BOUND('',#17530,.T.);
#11371=FACE_OUTER_BOUND('',#17531,.T.);
#11372=FACE_OUTER_BOUND('',#17532,.T.);
#11373=FACE_OUTER_BOUND('',#17533,.T.);
#11374=FACE_OUTER_BOUND('',#17534,.T.);
#11375=FACE_OUTER_BOUND('',#17535,.T.);
#11376=FACE_OUTER_BOUND('',#17536,.T.);
#11377=FACE_OUTER_BOUND('',#17537,.T.);
#11378=FACE_OUTER_BOUND('',#17538,.T.);
#11379=FACE_OUTER_BOUND('',#17539,.T.);
#11380=FACE_OUTER_BOUND('',#17540,.T.);
#11381=FACE_OUTER_BOUND('',#17541,.T.);
#11382=FACE_OUTER_BOUND('',#17542,.T.);
#11383=FACE_OUTER_BOUND('',#17543,.T.);
#11384=FACE_OUTER_BOUND('',#17544,.T.);
#11385=FACE_OUTER_BOUND('',#17545,.T.);
#11386=FACE_OUTER_BOUND('',#17546,.T.);
#11387=FACE_OUTER_BOUND('',#17547,.T.);
#11388=FACE_OUTER_BOUND('',#17548,.T.);
#11389=FACE_OUTER_BOUND('',#17549,.T.);
#11390=FACE_OUTER_BOUND('',#17550,.T.);
#11391=FACE_OUTER_BOUND('',#17551,.T.);
#11392=FACE_OUTER_BOUND('',#17552,.T.);
#11393=FACE_OUTER_BOUND('',#17553,.T.);
#11394=FACE_OUTER_BOUND('',#17554,.T.);
#11395=FACE_OUTER_BOUND('',#17555,.T.);
#11396=FACE_OUTER_BOUND('',#17556,.T.);
#11397=FACE_OUTER_BOUND('',#17557,.T.);
#11398=FACE_OUTER_BOUND('',#17558,.T.);
#11399=FACE_OUTER_BOUND('',#17559,.T.);
#11400=FACE_OUTER_BOUND('',#17560,.T.);
#11401=FACE_OUTER_BOUND('',#17561,.T.);
#11402=FACE_OUTER_BOUND('',#17562,.T.);
#11403=FACE_OUTER_BOUND('',#17563,.T.);
#11404=FACE_OUTER_BOUND('',#17564,.T.);
#11405=FACE_OUTER_BOUND('',#17565,.T.);
#11406=FACE_OUTER_BOUND('',#17566,.T.);
#11407=FACE_OUTER_BOUND('',#17567,.T.);
#11408=FACE_OUTER_BOUND('',#17568,.T.);
#11409=FACE_OUTER_BOUND('',#17569,.T.);
#11410=FACE_OUTER_BOUND('',#17570,.T.);
#11411=FACE_OUTER_BOUND('',#17571,.T.);
#11412=FACE_OUTER_BOUND('',#17572,.T.);
#11413=FACE_OUTER_BOUND('',#17573,.T.);
#11414=FACE_OUTER_BOUND('',#17574,.T.);
#11415=FACE_OUTER_BOUND('',#17575,.T.);
#11416=FACE_OUTER_BOUND('',#17576,.T.);
#11417=FACE_OUTER_BOUND('',#17577,.T.);
#11418=FACE_OUTER_BOUND('',#17578,.T.);
#11419=FACE_OUTER_BOUND('',#17579,.T.);
#11420=FACE_OUTER_BOUND('',#17580,.T.);
#11421=FACE_OUTER_BOUND('',#17581,.T.);
#11422=FACE_OUTER_BOUND('',#17582,.T.);
#11423=FACE_OUTER_BOUND('',#17583,.T.);
#11424=FACE_OUTER_BOUND('',#17584,.T.);
#11425=FACE_OUTER_BOUND('',#17585,.T.);
#11426=FACE_OUTER_BOUND('',#17586,.T.);
#11427=FACE_OUTER_BOUND('',#17587,.T.);
#11428=FACE_OUTER_BOUND('',#17588,.T.);
#11429=FACE_OUTER_BOUND('',#17589,.T.);
#11430=FACE_OUTER_BOUND('',#17590,.T.);
#11431=FACE_OUTER_BOUND('',#17591,.T.);
#11432=FACE_OUTER_BOUND('',#17592,.T.);
#11433=FACE_OUTER_BOUND('',#17593,.T.);
#11434=FACE_OUTER_BOUND('',#17594,.T.);
#11435=FACE_OUTER_BOUND('',#17595,.T.);
#11436=FACE_OUTER_BOUND('',#17596,.T.);
#11437=FACE_OUTER_BOUND('',#17597,.T.);
#11438=FACE_OUTER_BOUND('',#17598,.T.);
#11439=FACE_OUTER_BOUND('',#17599,.T.);
#11440=FACE_OUTER_BOUND('',#17600,.T.);
#11441=FACE_OUTER_BOUND('',#17601,.T.);
#11442=FACE_OUTER_BOUND('',#17602,.T.);
#11443=FACE_OUTER_BOUND('',#17603,.T.);
#11444=FACE_OUTER_BOUND('',#17604,.T.);
#11445=FACE_OUTER_BOUND('',#17605,.T.);
#11446=FACE_OUTER_BOUND('',#17606,.T.);
#11447=FACE_OUTER_BOUND('',#17607,.T.);
#11448=FACE_OUTER_BOUND('',#17608,.T.);
#11449=FACE_OUTER_BOUND('',#17609,.T.);
#11450=FACE_OUTER_BOUND('',#17610,.T.);
#11451=FACE_OUTER_BOUND('',#17611,.T.);
#11452=FACE_OUTER_BOUND('',#17612,.T.);
#11453=FACE_OUTER_BOUND('',#17613,.T.);
#11454=FACE_OUTER_BOUND('',#17614,.T.);
#11455=FACE_OUTER_BOUND('',#17615,.T.);
#11456=FACE_OUTER_BOUND('',#17616,.T.);
#11457=FACE_OUTER_BOUND('',#17617,.T.);
#11458=FACE_OUTER_BOUND('',#17618,.T.);
#11459=FACE_OUTER_BOUND('',#17619,.T.);
#11460=FACE_OUTER_BOUND('',#17620,.T.);
#11461=FACE_OUTER_BOUND('',#17621,.T.);
#11462=FACE_OUTER_BOUND('',#17622,.T.);
#11463=FACE_OUTER_BOUND('',#17623,.T.);
#11464=FACE_OUTER_BOUND('',#17624,.T.);
#11465=FACE_OUTER_BOUND('',#17625,.T.);
#11466=FACE_OUTER_BOUND('',#17626,.T.);
#11467=FACE_OUTER_BOUND('',#17627,.T.);
#11468=FACE_OUTER_BOUND('',#17628,.T.);
#11469=FACE_OUTER_BOUND('',#17629,.T.);
#11470=FACE_OUTER_BOUND('',#17630,.T.);
#11471=FACE_OUTER_BOUND('',#17631,.T.);
#11472=FACE_OUTER_BOUND('',#17632,.T.);
#11473=FACE_OUTER_BOUND('',#17633,.T.);
#11474=FACE_OUTER_BOUND('',#17634,.T.);
#11475=FACE_OUTER_BOUND('',#17635,.T.);
#11476=FACE_OUTER_BOUND('',#17636,.T.);
#11477=FACE_OUTER_BOUND('',#17637,.T.);
#11478=FACE_OUTER_BOUND('',#17638,.T.);
#11479=FACE_OUTER_BOUND('',#17639,.T.);
#11480=FACE_OUTER_BOUND('',#17640,.T.);
#11481=FACE_OUTER_BOUND('',#17641,.T.);
#11482=FACE_OUTER_BOUND('',#17642,.T.);
#11483=FACE_OUTER_BOUND('',#17643,.T.);
#11484=FACE_OUTER_BOUND('',#17644,.T.);
#11485=FACE_OUTER_BOUND('',#17645,.T.);
#11486=FACE_OUTER_BOUND('',#17646,.T.);
#11487=FACE_OUTER_BOUND('',#17647,.T.);
#11488=FACE_OUTER_BOUND('',#17648,.T.);
#11489=FACE_OUTER_BOUND('',#17649,.T.);
#11490=FACE_OUTER_BOUND('',#17650,.T.);
#11491=FACE_OUTER_BOUND('',#17651,.T.);
#11492=FACE_OUTER_BOUND('',#17652,.T.);
#11493=FACE_OUTER_BOUND('',#17653,.T.);
#11494=FACE_OUTER_BOUND('',#17654,.T.);
#11495=FACE_OUTER_BOUND('',#17655,.T.);
#11496=FACE_OUTER_BOUND('',#17656,.T.);
#11497=FACE_OUTER_BOUND('',#17657,.T.);
#11498=FACE_OUTER_BOUND('',#17658,.T.);
#11499=FACE_OUTER_BOUND('',#17659,.T.);
#11500=FACE_OUTER_BOUND('',#17660,.T.);
#11501=FACE_OUTER_BOUND('',#17661,.T.);
#11502=FACE_OUTER_BOUND('',#17662,.T.);
#11503=FACE_OUTER_BOUND('',#17663,.T.);
#11504=FACE_OUTER_BOUND('',#17664,.T.);
#11505=FACE_OUTER_BOUND('',#17665,.T.);
#11506=FACE_OUTER_BOUND('',#17666,.T.);
#11507=FACE_OUTER_BOUND('',#17667,.T.);
#11508=FACE_OUTER_BOUND('',#17668,.T.);
#11509=FACE_OUTER_BOUND('',#17669,.T.);
#11510=FACE_OUTER_BOUND('',#17670,.T.);
#11511=FACE_OUTER_BOUND('',#17671,.T.);
#11512=FACE_OUTER_BOUND('',#17672,.T.);
#11513=FACE_OUTER_BOUND('',#17673,.T.);
#11514=FACE_OUTER_BOUND('',#17674,.T.);
#11515=FACE_OUTER_BOUND('',#17675,.T.);
#11516=FACE_OUTER_BOUND('',#17676,.T.);
#11517=FACE_OUTER_BOUND('',#17677,.T.);
#11518=FACE_OUTER_BOUND('',#17678,.T.);
#11519=FACE_OUTER_BOUND('',#17679,.T.);
#11520=FACE_OUTER_BOUND('',#17680,.T.);
#11521=FACE_OUTER_BOUND('',#17681,.T.);
#11522=FACE_OUTER_BOUND('',#17682,.T.);
#11523=FACE_OUTER_BOUND('',#17683,.T.);
#11524=FACE_OUTER_BOUND('',#17684,.T.);
#11525=FACE_OUTER_BOUND('',#17685,.T.);
#11526=FACE_OUTER_BOUND('',#17686,.T.);
#11527=FACE_OUTER_BOUND('',#17687,.T.);
#11528=FACE_OUTER_BOUND('',#17688,.T.);
#11529=FACE_OUTER_BOUND('',#17689,.T.);
#11530=FACE_OUTER_BOUND('',#17690,.T.);
#11531=FACE_OUTER_BOUND('',#17691,.T.);
#11532=FACE_OUTER_BOUND('',#17692,.T.);
#11533=FACE_OUTER_BOUND('',#17693,.T.);
#11534=FACE_OUTER_BOUND('',#17694,.T.);
#11535=FACE_OUTER_BOUND('',#17695,.T.);
#11536=FACE_OUTER_BOUND('',#17696,.T.);
#11537=FACE_OUTER_BOUND('',#17697,.T.);
#11538=FACE_OUTER_BOUND('',#17698,.T.);
#11539=FACE_OUTER_BOUND('',#17699,.T.);
#11540=FACE_OUTER_BOUND('',#17700,.T.);
#11541=FACE_OUTER_BOUND('',#17701,.T.);
#11542=FACE_OUTER_BOUND('',#17702,.T.);
#11543=FACE_OUTER_BOUND('',#17703,.T.);
#11544=FACE_OUTER_BOUND('',#17704,.T.);
#11545=FACE_OUTER_BOUND('',#17705,.T.);
#11546=FACE_OUTER_BOUND('',#17706,.T.);
#11547=FACE_OUTER_BOUND('',#17707,.T.);
#11548=FACE_OUTER_BOUND('',#17708,.T.);
#11549=FACE_OUTER_BOUND('',#17709,.T.);
#11550=FACE_OUTER_BOUND('',#17710,.T.);
#11551=FACE_OUTER_BOUND('',#17711,.T.);
#11552=FACE_OUTER_BOUND('',#17712,.T.);
#11553=FACE_OUTER_BOUND('',#17713,.T.);
#11554=FACE_OUTER_BOUND('',#17714,.T.);
#11555=FACE_OUTER_BOUND('',#17715,.T.);
#11556=FACE_OUTER_BOUND('',#17716,.T.);
#11557=FACE_OUTER_BOUND('',#17717,.T.);
#11558=FACE_OUTER_BOUND('',#17718,.T.);
#11559=FACE_OUTER_BOUND('',#17719,.T.);
#11560=FACE_OUTER_BOUND('',#17720,.T.);
#11561=FACE_OUTER_BOUND('',#17721,.T.);
#11562=FACE_OUTER_BOUND('',#17722,.T.);
#11563=FACE_OUTER_BOUND('',#17723,.T.);
#11564=FACE_OUTER_BOUND('',#17724,.T.);
#11565=FACE_OUTER_BOUND('',#17725,.T.);
#11566=FACE_OUTER_BOUND('',#17726,.T.);
#11567=FACE_OUTER_BOUND('',#17727,.T.);
#11568=FACE_OUTER_BOUND('',#17728,.T.);
#11569=FACE_OUTER_BOUND('',#17729,.T.);
#11570=FACE_OUTER_BOUND('',#17730,.T.);
#11571=FACE_OUTER_BOUND('',#17731,.T.);
#11572=FACE_OUTER_BOUND('',#17732,.T.);
#11573=FACE_OUTER_BOUND('',#17733,.T.);
#11574=FACE_OUTER_BOUND('',#17734,.T.);
#11575=FACE_OUTER_BOUND('',#17735,.T.);
#11576=FACE_OUTER_BOUND('',#17736,.T.);
#11577=FACE_OUTER_BOUND('',#17737,.T.);
#11578=FACE_OUTER_BOUND('',#17738,.T.);
#11579=FACE_OUTER_BOUND('',#17739,.T.);
#11580=FACE_OUTER_BOUND('',#17740,.T.);
#11581=FACE_OUTER_BOUND('',#17741,.T.);
#11582=FACE_OUTER_BOUND('',#17742,.T.);
#11583=FACE_OUTER_BOUND('',#17743,.T.);
#11584=FACE_OUTER_BOUND('',#17744,.T.);
#11585=FACE_OUTER_BOUND('',#17745,.T.);
#11586=FACE_OUTER_BOUND('',#17746,.T.);
#11587=FACE_OUTER_BOUND('',#17747,.T.);
#11588=FACE_OUTER_BOUND('',#17748,.T.);
#11589=FACE_OUTER_BOUND('',#17749,.T.);
#11590=FACE_OUTER_BOUND('',#17750,.T.);
#11591=FACE_OUTER_BOUND('',#17751,.T.);
#11592=FACE_OUTER_BOUND('',#17752,.T.);
#11593=FACE_OUTER_BOUND('',#17753,.T.);
#11594=FACE_OUTER_BOUND('',#17754,.T.);
#11595=FACE_OUTER_BOUND('',#17755,.T.);
#11596=FACE_OUTER_BOUND('',#17756,.T.);
#11597=FACE_OUTER_BOUND('',#17757,.T.);
#11598=FACE_OUTER_BOUND('',#17758,.T.);
#11599=FACE_OUTER_BOUND('',#17759,.T.);
#11600=FACE_OUTER_BOUND('',#17760,.T.);
#11601=FACE_OUTER_BOUND('',#17761,.T.);
#11602=FACE_OUTER_BOUND('',#17762,.T.);
#11603=FACE_OUTER_BOUND('',#17763,.T.);
#11604=FACE_OUTER_BOUND('',#17764,.T.);
#11605=FACE_OUTER_BOUND('',#17765,.T.);
#11606=FACE_OUTER_BOUND('',#17766,.T.);
#11607=FACE_OUTER_BOUND('',#17767,.T.);
#11608=FACE_OUTER_BOUND('',#17768,.T.);
#11609=FACE_OUTER_BOUND('',#17769,.T.);
#11610=FACE_OUTER_BOUND('',#17770,.T.);
#11611=FACE_OUTER_BOUND('',#17771,.T.);
#11612=FACE_OUTER_BOUND('',#17772,.T.);
#11613=FACE_OUTER_BOUND('',#17773,.T.);
#11614=FACE_OUTER_BOUND('',#17774,.T.);
#11615=FACE_OUTER_BOUND('',#17775,.T.);
#11616=FACE_OUTER_BOUND('',#17776,.T.);
#11617=FACE_OUTER_BOUND('',#17777,.T.);
#11618=FACE_OUTER_BOUND('',#17778,.T.);
#11619=FACE_OUTER_BOUND('',#17779,.T.);
#11620=FACE_OUTER_BOUND('',#17780,.T.);
#11621=FACE_OUTER_BOUND('',#17781,.T.);
#11622=FACE_OUTER_BOUND('',#17782,.T.);
#11623=FACE_OUTER_BOUND('',#17783,.T.);
#11624=FACE_OUTER_BOUND('',#17784,.T.);
#11625=FACE_OUTER_BOUND('',#17785,.T.);
#11626=FACE_OUTER_BOUND('',#17786,.T.);
#11627=FACE_OUTER_BOUND('',#17787,.T.);
#11628=FACE_OUTER_BOUND('',#17788,.T.);
#11629=FACE_OUTER_BOUND('',#17789,.T.);
#11630=FACE_OUTER_BOUND('',#17790,.T.);
#11631=FACE_OUTER_BOUND('',#17791,.T.);
#11632=FACE_OUTER_BOUND('',#17792,.T.);
#11633=FACE_OUTER_BOUND('',#17793,.T.);
#11634=FACE_OUTER_BOUND('',#17794,.T.);
#11635=FACE_OUTER_BOUND('',#17795,.T.);
#11636=FACE_OUTER_BOUND('',#17796,.T.);
#11637=FACE_OUTER_BOUND('',#17797,.T.);
#11638=FACE_OUTER_BOUND('',#17798,.T.);
#11639=FACE_OUTER_BOUND('',#17799,.T.);
#11640=FACE_OUTER_BOUND('',#17800,.T.);
#11641=FACE_OUTER_BOUND('',#17801,.T.);
#11642=FACE_OUTER_BOUND('',#17802,.T.);
#11643=FACE_OUTER_BOUND('',#17803,.T.);
#11644=FACE_OUTER_BOUND('',#17804,.T.);
#11645=FACE_OUTER_BOUND('',#17805,.T.);
#11646=FACE_OUTER_BOUND('',#17806,.T.);
#11647=FACE_OUTER_BOUND('',#17807,.T.);
#11648=FACE_OUTER_BOUND('',#17808,.T.);
#11649=FACE_OUTER_BOUND('',#17809,.T.);
#11650=FACE_OUTER_BOUND('',#17810,.T.);
#11651=FACE_OUTER_BOUND('',#17811,.T.);
#11652=FACE_OUTER_BOUND('',#17812,.T.);
#11653=FACE_OUTER_BOUND('',#17813,.T.);
#11654=FACE_OUTER_BOUND('',#17814,.T.);
#11655=FACE_OUTER_BOUND('',#17815,.T.);
#11656=FACE_OUTER_BOUND('',#17816,.T.);
#11657=FACE_OUTER_BOUND('',#17817,.T.);
#11658=FACE_OUTER_BOUND('',#17818,.T.);
#11659=FACE_OUTER_BOUND('',#17819,.T.);
#11660=FACE_OUTER_BOUND('',#17820,.T.);
#11661=FACE_OUTER_BOUND('',#17821,.T.);
#11662=FACE_OUTER_BOUND('',#17822,.T.);
#11663=FACE_OUTER_BOUND('',#17823,.T.);
#11664=FACE_OUTER_BOUND('',#17824,.T.);
#11665=FACE_OUTER_BOUND('',#17825,.T.);
#11666=FACE_OUTER_BOUND('',#17826,.T.);
#11667=FACE_OUTER_BOUND('',#17827,.T.);
#11668=FACE_OUTER_BOUND('',#17828,.T.);
#11669=FACE_OUTER_BOUND('',#17829,.T.);
#11670=FACE_OUTER_BOUND('',#17830,.T.);
#11671=FACE_OUTER_BOUND('',#17831,.T.);
#11672=FACE_OUTER_BOUND('',#17832,.T.);
#11673=FACE_OUTER_BOUND('',#17833,.T.);
#11674=FACE_OUTER_BOUND('',#17834,.T.);
#11675=FACE_OUTER_BOUND('',#17835,.T.);
#11676=FACE_OUTER_BOUND('',#17836,.T.);
#11677=FACE_OUTER_BOUND('',#17837,.T.);
#11678=FACE_OUTER_BOUND('',#17838,.T.);
#11679=FACE_OUTER_BOUND('',#17839,.T.);
#11680=FACE_OUTER_BOUND('',#17840,.T.);
#11681=FACE_OUTER_BOUND('',#17841,.T.);
#11682=FACE_OUTER_BOUND('',#17842,.T.);
#11683=FACE_OUTER_BOUND('',#17843,.T.);
#11684=FACE_OUTER_BOUND('',#17844,.T.);
#11685=FACE_OUTER_BOUND('',#17845,.T.);
#11686=FACE_OUTER_BOUND('',#17846,.T.);
#11687=FACE_OUTER_BOUND('',#17847,.T.);
#11688=FACE_OUTER_BOUND('',#17848,.T.);
#11689=FACE_OUTER_BOUND('',#17849,.T.);
#11690=FACE_OUTER_BOUND('',#17850,.T.);
#11691=FACE_OUTER_BOUND('',#17851,.T.);
#11692=FACE_OUTER_BOUND('',#17852,.T.);
#11693=FACE_OUTER_BOUND('',#17853,.T.);
#11694=FACE_OUTER_BOUND('',#17854,.T.);
#11695=FACE_OUTER_BOUND('',#17855,.T.);
#11696=FACE_OUTER_BOUND('',#17856,.T.);
#11697=FACE_OUTER_BOUND('',#17857,.T.);
#11698=FACE_OUTER_BOUND('',#17858,.T.);
#11699=FACE_OUTER_BOUND('',#17859,.T.);
#11700=FACE_OUTER_BOUND('',#17860,.T.);
#11701=FACE_OUTER_BOUND('',#17861,.T.);
#11702=FACE_OUTER_BOUND('',#17862,.T.);
#11703=FACE_OUTER_BOUND('',#17863,.T.);
#11704=FACE_OUTER_BOUND('',#17864,.T.);
#11705=FACE_OUTER_BOUND('',#17865,.T.);
#11706=FACE_OUTER_BOUND('',#17866,.T.);
#11707=FACE_OUTER_BOUND('',#17867,.T.);
#11708=FACE_OUTER_BOUND('',#17868,.T.);
#11709=FACE_OUTER_BOUND('',#17869,.T.);
#11710=FACE_OUTER_BOUND('',#17870,.T.);
#11711=FACE_OUTER_BOUND('',#17871,.T.);
#11712=FACE_OUTER_BOUND('',#17872,.T.);
#11713=FACE_OUTER_BOUND('',#17873,.T.);
#11714=FACE_OUTER_BOUND('',#17874,.T.);
#11715=FACE_OUTER_BOUND('',#17875,.T.);
#11716=FACE_OUTER_BOUND('',#17876,.T.);
#11717=FACE_OUTER_BOUND('',#17877,.T.);
#11718=FACE_OUTER_BOUND('',#17878,.T.);
#11719=FACE_OUTER_BOUND('',#17879,.T.);
#11720=FACE_OUTER_BOUND('',#17880,.T.);
#11721=FACE_OUTER_BOUND('',#17881,.T.);
#11722=FACE_OUTER_BOUND('',#17882,.T.);
#11723=FACE_OUTER_BOUND('',#17883,.T.);
#11724=FACE_OUTER_BOUND('',#17884,.T.);
#11725=FACE_OUTER_BOUND('',#17885,.T.);
#11726=FACE_OUTER_BOUND('',#17886,.T.);
#11727=FACE_OUTER_BOUND('',#17887,.T.);
#11728=FACE_OUTER_BOUND('',#17888,.T.);
#11729=FACE_OUTER_BOUND('',#17889,.T.);
#11730=FACE_OUTER_BOUND('',#17890,.T.);
#11731=FACE_OUTER_BOUND('',#17891,.T.);
#11732=FACE_OUTER_BOUND('',#17892,.T.);
#11733=FACE_OUTER_BOUND('',#17893,.T.);
#11734=FACE_OUTER_BOUND('',#17894,.T.);
#11735=FACE_OUTER_BOUND('',#17895,.T.);
#11736=FACE_OUTER_BOUND('',#17896,.T.);
#11737=FACE_OUTER_BOUND('',#17897,.T.);
#11738=FACE_OUTER_BOUND('',#17898,.T.);
#11739=FACE_OUTER_BOUND('',#17899,.T.);
#11740=FACE_OUTER_BOUND('',#17900,.T.);
#11741=FACE_OUTER_BOUND('',#17901,.T.);
#11742=FACE_OUTER_BOUND('',#17902,.T.);
#11743=FACE_OUTER_BOUND('',#17903,.T.);
#11744=FACE_OUTER_BOUND('',#17904,.T.);
#11745=FACE_OUTER_BOUND('',#17905,.T.);
#11746=FACE_OUTER_BOUND('',#17906,.T.);
#11747=FACE_OUTER_BOUND('',#17907,.T.);
#11748=FACE_OUTER_BOUND('',#17908,.T.);
#11749=FACE_OUTER_BOUND('',#17909,.T.);
#11750=FACE_OUTER_BOUND('',#17910,.T.);
#11751=FACE_OUTER_BOUND('',#17911,.T.);
#11752=FACE_OUTER_BOUND('',#17912,.T.);
#11753=FACE_OUTER_BOUND('',#17913,.T.);
#11754=FACE_OUTER_BOUND('',#17914,.T.);
#11755=FACE_OUTER_BOUND('',#17915,.T.);
#11756=FACE_OUTER_BOUND('',#17916,.T.);
#11757=FACE_OUTER_BOUND('',#17917,.T.);
#11758=FACE_OUTER_BOUND('',#17918,.T.);
#11759=FACE_OUTER_BOUND('',#17919,.T.);
#11760=FACE_OUTER_BOUND('',#17920,.T.);
#11761=FACE_OUTER_BOUND('',#17921,.T.);
#11762=FACE_OUTER_BOUND('',#17922,.T.);
#11763=FACE_OUTER_BOUND('',#17923,.T.);
#11764=FACE_OUTER_BOUND('',#17924,.T.);
#11765=FACE_OUTER_BOUND('',#17925,.T.);
#11766=FACE_OUTER_BOUND('',#17926,.T.);
#11767=FACE_OUTER_BOUND('',#17927,.T.);
#11768=FACE_OUTER_BOUND('',#17928,.T.);
#11769=FACE_OUTER_BOUND('',#17929,.T.);
#11770=FACE_OUTER_BOUND('',#17930,.T.);
#11771=FACE_OUTER_BOUND('',#17931,.T.);
#11772=FACE_OUTER_BOUND('',#17932,.T.);
#11773=FACE_OUTER_BOUND('',#17933,.T.);
#11774=FACE_OUTER_BOUND('',#17934,.T.);
#11775=FACE_OUTER_BOUND('',#17935,.T.);
#11776=FACE_OUTER_BOUND('',#17936,.T.);
#11777=FACE_OUTER_BOUND('',#17937,.T.);
#11778=FACE_OUTER_BOUND('',#17938,.T.);
#11779=FACE_OUTER_BOUND('',#17939,.T.);
#11780=FACE_OUTER_BOUND('',#17940,.T.);
#11781=FACE_OUTER_BOUND('',#17941,.T.);
#11782=FACE_OUTER_BOUND('',#17942,.T.);
#11783=FACE_OUTER_BOUND('',#17943,.T.);
#11784=FACE_OUTER_BOUND('',#17944,.T.);
#11785=FACE_OUTER_BOUND('',#17945,.T.);
#11786=FACE_OUTER_BOUND('',#17946,.T.);
#11787=FACE_OUTER_BOUND('',#17947,.T.);
#11788=FACE_OUTER_BOUND('',#17948,.T.);
#11789=FACE_OUTER_BOUND('',#17949,.T.);
#11790=FACE_OUTER_BOUND('',#17950,.T.);
#11791=FACE_OUTER_BOUND('',#17951,.T.);
#11792=FACE_OUTER_BOUND('',#17952,.T.);
#11793=FACE_OUTER_BOUND('',#17953,.T.);
#11794=FACE_OUTER_BOUND('',#17954,.T.);
#11795=FACE_OUTER_BOUND('',#17955,.T.);
#11796=FACE_OUTER_BOUND('',#17956,.T.);
#11797=FACE_OUTER_BOUND('',#17957,.T.);
#11798=FACE_OUTER_BOUND('',#17958,.T.);
#11799=FACE_OUTER_BOUND('',#17959,.T.);
#11800=FACE_OUTER_BOUND('',#17960,.T.);
#11801=FACE_OUTER_BOUND('',#17961,.T.);
#11802=FACE_OUTER_BOUND('',#17962,.T.);
#11803=FACE_OUTER_BOUND('',#17963,.T.);
#11804=FACE_OUTER_BOUND('',#17964,.T.);
#11805=FACE_OUTER_BOUND('',#17965,.T.);
#11806=FACE_OUTER_BOUND('',#17966,.T.);
#11807=FACE_OUTER_BOUND('',#17967,.T.);
#11808=FACE_OUTER_BOUND('',#17968,.T.);
#11809=FACE_OUTER_BOUND('',#17969,.T.);
#11810=FACE_OUTER_BOUND('',#17970,.T.);
#11811=FACE_OUTER_BOUND('',#17971,.T.);
#11812=FACE_OUTER_BOUND('',#17972,.T.);
#11813=FACE_OUTER_BOUND('',#17973,.T.);
#11814=FACE_OUTER_BOUND('',#17974,.T.);
#11815=FACE_OUTER_BOUND('',#17975,.T.);
#11816=FACE_OUTER_BOUND('',#17976,.T.);
#11817=FACE_OUTER_BOUND('',#17977,.T.);
#11818=FACE_OUTER_BOUND('',#17978,.T.);
#11819=FACE_OUTER_BOUND('',#17979,.T.);
#11820=FACE_OUTER_BOUND('',#17980,.T.);
#11821=FACE_OUTER_BOUND('',#17981,.T.);
#11822=FACE_OUTER_BOUND('',#17982,.T.);
#11823=FACE_OUTER_BOUND('',#17983,.T.);
#11824=FACE_OUTER_BOUND('',#17984,.T.);
#11825=FACE_OUTER_BOUND('',#17985,.T.);
#11826=FACE_OUTER_BOUND('',#17986,.T.);
#11827=FACE_OUTER_BOUND('',#17987,.T.);
#11828=FACE_OUTER_BOUND('',#17988,.T.);
#11829=FACE_OUTER_BOUND('',#17989,.T.);
#11830=FACE_OUTER_BOUND('',#17990,.T.);
#11831=FACE_OUTER_BOUND('',#17991,.T.);
#11832=FACE_OUTER_BOUND('',#17992,.T.);
#11833=FACE_OUTER_BOUND('',#17993,.T.);
#11834=FACE_OUTER_BOUND('',#17994,.T.);
#11835=FACE_OUTER_BOUND('',#17995,.T.);
#11836=FACE_OUTER_BOUND('',#17996,.T.);
#11837=FACE_OUTER_BOUND('',#17997,.T.);
#11838=FACE_OUTER_BOUND('',#17998,.T.);
#11839=FACE_OUTER_BOUND('',#17999,.T.);
#11840=FACE_OUTER_BOUND('',#18000,.T.);
#11841=FACE_OUTER_BOUND('',#18001,.T.);
#11842=FACE_OUTER_BOUND('',#18002,.T.);
#11843=FACE_OUTER_BOUND('',#18003,.T.);
#11844=FACE_OUTER_BOUND('',#18004,.T.);
#11845=FACE_OUTER_BOUND('',#18005,.T.);
#11846=FACE_OUTER_BOUND('',#18006,.T.);
#11847=FACE_OUTER_BOUND('',#18007,.T.);
#11848=FACE_OUTER_BOUND('',#18008,.T.);
#11849=FACE_OUTER_BOUND('',#18009,.T.);
#11850=FACE_OUTER_BOUND('',#18010,.T.);
#11851=FACE_OUTER_BOUND('',#18011,.T.);
#11852=FACE_OUTER_BOUND('',#18012,.T.);
#11853=FACE_OUTER_BOUND('',#18013,.T.);
#11854=FACE_OUTER_BOUND('',#18014,.T.);
#11855=FACE_OUTER_BOUND('',#18015,.T.);
#11856=FACE_OUTER_BOUND('',#18016,.T.);
#11857=FACE_OUTER_BOUND('',#18017,.T.);
#11858=FACE_OUTER_BOUND('',#18018,.T.);
#11859=FACE_OUTER_BOUND('',#18019,.T.);
#11860=FACE_OUTER_BOUND('',#18020,.T.);
#11861=FACE_OUTER_BOUND('',#18021,.T.);
#11862=FACE_OUTER_BOUND('',#18022,.T.);
#11863=FACE_OUTER_BOUND('',#18023,.T.);
#11864=FACE_OUTER_BOUND('',#18024,.T.);
#11865=FACE_OUTER_BOUND('',#18025,.T.);
#11866=FACE_OUTER_BOUND('',#18026,.T.);
#11867=FACE_OUTER_BOUND('',#18027,.T.);
#11868=FACE_OUTER_BOUND('',#18028,.T.);
#11869=FACE_OUTER_BOUND('',#18029,.T.);
#11870=FACE_OUTER_BOUND('',#18030,.T.);
#11871=FACE_OUTER_BOUND('',#18031,.T.);
#11872=FACE_OUTER_BOUND('',#18032,.T.);
#11873=FACE_OUTER_BOUND('',#18033,.T.);
#11874=FACE_OUTER_BOUND('',#18034,.T.);
#11875=FACE_OUTER_BOUND('',#18035,.T.);
#11876=FACE_OUTER_BOUND('',#18036,.T.);
#11877=FACE_OUTER_BOUND('',#18037,.T.);
#11878=FACE_OUTER_BOUND('',#18038,.T.);
#11879=FACE_OUTER_BOUND('',#18039,.T.);
#11880=FACE_OUTER_BOUND('',#18040,.T.);
#11881=FACE_OUTER_BOUND('',#18041,.T.);
#11882=FACE_OUTER_BOUND('',#18042,.T.);
#11883=FACE_OUTER_BOUND('',#18043,.T.);
#11884=FACE_OUTER_BOUND('',#18044,.T.);
#11885=FACE_OUTER_BOUND('',#18045,.T.);
#11886=FACE_OUTER_BOUND('',#18046,.T.);
#11887=FACE_OUTER_BOUND('',#18047,.T.);
#11888=FACE_OUTER_BOUND('',#18048,.T.);
#11889=FACE_OUTER_BOUND('',#18049,.T.);
#11890=FACE_OUTER_BOUND('',#18050,.T.);
#11891=FACE_OUTER_BOUND('',#18051,.T.);
#11892=FACE_OUTER_BOUND('',#18052,.T.);
#11893=FACE_OUTER_BOUND('',#18053,.T.);
#11894=FACE_OUTER_BOUND('',#18054,.T.);
#11895=FACE_OUTER_BOUND('',#18055,.T.);
#11896=FACE_OUTER_BOUND('',#18056,.T.);
#11897=FACE_OUTER_BOUND('',#18057,.T.);
#11898=FACE_OUTER_BOUND('',#18058,.T.);
#11899=FACE_OUTER_BOUND('',#18059,.T.);
#11900=FACE_OUTER_BOUND('',#18060,.T.);
#11901=FACE_OUTER_BOUND('',#18061,.T.);
#11902=FACE_OUTER_BOUND('',#18062,.T.);
#11903=FACE_OUTER_BOUND('',#18063,.T.);
#11904=FACE_OUTER_BOUND('',#18064,.T.);
#11905=FACE_OUTER_BOUND('',#18065,.T.);
#11906=FACE_OUTER_BOUND('',#18066,.T.);
#11907=FACE_OUTER_BOUND('',#18067,.T.);
#11908=FACE_OUTER_BOUND('',#18068,.T.);
#11909=FACE_OUTER_BOUND('',#18069,.T.);
#11910=FACE_OUTER_BOUND('',#18070,.T.);
#11911=FACE_OUTER_BOUND('',#18071,.T.);
#11912=FACE_OUTER_BOUND('',#18072,.T.);
#11913=FACE_OUTER_BOUND('',#18073,.T.);
#11914=FACE_OUTER_BOUND('',#18074,.T.);
#11915=FACE_OUTER_BOUND('',#18075,.T.);
#11916=FACE_OUTER_BOUND('',#18076,.T.);
#11917=FACE_OUTER_BOUND('',#18077,.T.);
#11918=FACE_OUTER_BOUND('',#18078,.T.);
#11919=FACE_OUTER_BOUND('',#18079,.T.);
#11920=FACE_OUTER_BOUND('',#18080,.T.);
#11921=FACE_OUTER_BOUND('',#18081,.T.);
#11922=FACE_OUTER_BOUND('',#18082,.T.);
#11923=FACE_OUTER_BOUND('',#18083,.T.);
#11924=FACE_OUTER_BOUND('',#18084,.T.);
#11925=FACE_OUTER_BOUND('',#18085,.T.);
#11926=FACE_OUTER_BOUND('',#18086,.T.);
#11927=FACE_OUTER_BOUND('',#18087,.T.);
#11928=FACE_OUTER_BOUND('',#18088,.T.);
#11929=FACE_OUTER_BOUND('',#18089,.T.);
#11930=FACE_OUTER_BOUND('',#18090,.T.);
#11931=FACE_OUTER_BOUND('',#18091,.T.);
#11932=FACE_OUTER_BOUND('',#18092,.T.);
#11933=FACE_OUTER_BOUND('',#18093,.T.);
#11934=FACE_OUTER_BOUND('',#18094,.T.);
#11935=FACE_OUTER_BOUND('',#18095,.T.);
#11936=FACE_OUTER_BOUND('',#18096,.T.);
#11937=FACE_OUTER_BOUND('',#18097,.T.);
#11938=FACE_OUTER_BOUND('',#18098,.T.);
#11939=FACE_OUTER_BOUND('',#18099,.T.);
#11940=FACE_OUTER_BOUND('',#18100,.T.);
#11941=FACE_OUTER_BOUND('',#18101,.T.);
#11942=FACE_OUTER_BOUND('',#18102,.T.);
#11943=FACE_OUTER_BOUND('',#18103,.T.);
#11944=FACE_OUTER_BOUND('',#18104,.T.);
#11945=FACE_OUTER_BOUND('',#18105,.T.);
#11946=FACE_OUTER_BOUND('',#18106,.T.);
#11947=FACE_OUTER_BOUND('',#18107,.T.);
#11948=FACE_OUTER_BOUND('',#18108,.T.);
#11949=FACE_OUTER_BOUND('',#18109,.T.);
#11950=FACE_OUTER_BOUND('',#18110,.T.);
#11951=FACE_OUTER_BOUND('',#18111,.T.);
#11952=FACE_OUTER_BOUND('',#18112,.T.);
#11953=FACE_OUTER_BOUND('',#18113,.T.);
#11954=FACE_OUTER_BOUND('',#18114,.T.);
#11955=FACE_OUTER_BOUND('',#18115,.T.);
#11956=FACE_OUTER_BOUND('',#18116,.T.);
#11957=FACE_OUTER_BOUND('',#18117,.T.);
#11958=FACE_OUTER_BOUND('',#18118,.T.);
#11959=FACE_OUTER_BOUND('',#18119,.T.);
#11960=FACE_OUTER_BOUND('',#18120,.T.);
#11961=FACE_OUTER_BOUND('',#18121,.T.);
#11962=FACE_OUTER_BOUND('',#18122,.T.);
#11963=FACE_OUTER_BOUND('',#18123,.T.);
#11964=FACE_OUTER_BOUND('',#18124,.T.);
#11965=FACE_OUTER_BOUND('',#18125,.T.);
#11966=FACE_OUTER_BOUND('',#18126,.T.);
#11967=FACE_OUTER_BOUND('',#18127,.T.);
#11968=FACE_OUTER_BOUND('',#18128,.T.);
#11969=FACE_OUTER_BOUND('',#18129,.T.);
#11970=FACE_OUTER_BOUND('',#18130,.T.);
#11971=FACE_OUTER_BOUND('',#18131,.T.);
#11972=FACE_OUTER_BOUND('',#18132,.T.);
#11973=FACE_OUTER_BOUND('',#18133,.T.);
#11974=FACE_OUTER_BOUND('',#18134,.T.);
#11975=FACE_OUTER_BOUND('',#18135,.T.);
#11976=FACE_OUTER_BOUND('',#18136,.T.);
#11977=FACE_OUTER_BOUND('',#18137,.T.);
#11978=FACE_OUTER_BOUND('',#18138,.T.);
#11979=FACE_OUTER_BOUND('',#18139,.T.);
#11980=FACE_OUTER_BOUND('',#18140,.T.);
#11981=FACE_OUTER_BOUND('',#18141,.T.);
#11982=FACE_OUTER_BOUND('',#18142,.T.);
#11983=FACE_OUTER_BOUND('',#18143,.T.);
#11984=FACE_OUTER_BOUND('',#18144,.T.);
#11985=FACE_OUTER_BOUND('',#18145,.T.);
#11986=FACE_OUTER_BOUND('',#18146,.T.);
#11987=FACE_OUTER_BOUND('',#18147,.T.);
#11988=FACE_OUTER_BOUND('',#18148,.T.);
#11989=FACE_OUTER_BOUND('',#18149,.T.);
#11990=FACE_OUTER_BOUND('',#18150,.T.);
#11991=FACE_OUTER_BOUND('',#18151,.T.);
#11992=FACE_OUTER_BOUND('',#18152,.T.);
#11993=FACE_OUTER_BOUND('',#18153,.T.);
#11994=FACE_OUTER_BOUND('',#18154,.T.);
#11995=FACE_OUTER_BOUND('',#18155,.T.);
#11996=FACE_OUTER_BOUND('',#18156,.T.);
#11997=FACE_OUTER_BOUND('',#18157,.T.);
#11998=FACE_OUTER_BOUND('',#18158,.T.);
#11999=FACE_OUTER_BOUND('',#18159,.T.);
#12000=FACE_OUTER_BOUND('',#18160,.T.);
#12001=FACE_OUTER_BOUND('',#18161,.T.);
#12002=FACE_OUTER_BOUND('',#18162,.T.);
#12003=FACE_OUTER_BOUND('',#18163,.T.);
#12004=FACE_OUTER_BOUND('',#18164,.T.);
#12005=FACE_OUTER_BOUND('',#18165,.T.);
#12006=FACE_OUTER_BOUND('',#18166,.T.);
#12007=FACE_OUTER_BOUND('',#18167,.T.);
#12008=FACE_OUTER_BOUND('',#18168,.T.);
#12009=FACE_OUTER_BOUND('',#18169,.T.);
#12010=FACE_OUTER_BOUND('',#18170,.T.);
#12011=FACE_OUTER_BOUND('',#18171,.T.);
#12012=FACE_OUTER_BOUND('',#18172,.T.);
#12013=FACE_OUTER_BOUND('',#18173,.T.);
#12014=FACE_OUTER_BOUND('',#18174,.T.);
#12015=FACE_OUTER_BOUND('',#18175,.T.);
#12016=FACE_OUTER_BOUND('',#18176,.T.);
#12017=FACE_OUTER_BOUND('',#18177,.T.);
#12018=FACE_OUTER_BOUND('',#18178,.T.);
#12019=FACE_OUTER_BOUND('',#18179,.T.);
#12020=FACE_OUTER_BOUND('',#18180,.T.);
#12021=FACE_OUTER_BOUND('',#18181,.T.);
#12022=FACE_OUTER_BOUND('',#18182,.T.);
#12023=FACE_OUTER_BOUND('',#18183,.T.);
#12024=FACE_OUTER_BOUND('',#18184,.T.);
#12025=FACE_OUTER_BOUND('',#18185,.T.);
#12026=FACE_OUTER_BOUND('',#18186,.T.);
#12027=FACE_OUTER_BOUND('',#18187,.T.);
#12028=FACE_OUTER_BOUND('',#18188,.T.);
#12029=FACE_OUTER_BOUND('',#18189,.T.);
#12030=FACE_OUTER_BOUND('',#18190,.T.);
#12031=FACE_OUTER_BOUND('',#18191,.T.);
#12032=FACE_OUTER_BOUND('',#18192,.T.);
#12033=FACE_OUTER_BOUND('',#18193,.T.);
#12034=FACE_OUTER_BOUND('',#18194,.T.);
#12035=FACE_OUTER_BOUND('',#18195,.T.);
#12036=FACE_OUTER_BOUND('',#18196,.T.);
#12037=FACE_OUTER_BOUND('',#18197,.T.);
#12038=FACE_OUTER_BOUND('',#18198,.T.);
#12039=FACE_OUTER_BOUND('',#18199,.T.);
#12040=FACE_OUTER_BOUND('',#18200,.T.);
#12041=FACE_OUTER_BOUND('',#18201,.T.);
#12042=FACE_OUTER_BOUND('',#18202,.T.);
#12043=FACE_OUTER_BOUND('',#18203,.T.);
#12044=FACE_OUTER_BOUND('',#18204,.T.);
#12045=FACE_OUTER_BOUND('',#18205,.T.);
#12046=FACE_OUTER_BOUND('',#18206,.T.);
#12047=FACE_OUTER_BOUND('',#18207,.T.);
#12048=FACE_OUTER_BOUND('',#18208,.T.);
#12049=FACE_OUTER_BOUND('',#18209,.T.);
#12050=FACE_OUTER_BOUND('',#18210,.T.);
#12051=FACE_OUTER_BOUND('',#18211,.T.);
#12052=FACE_OUTER_BOUND('',#18212,.T.);
#12053=FACE_OUTER_BOUND('',#18213,.T.);
#12054=FACE_OUTER_BOUND('',#18214,.T.);
#12055=FACE_OUTER_BOUND('',#18215,.T.);
#12056=FACE_OUTER_BOUND('',#18216,.T.);
#12057=FACE_OUTER_BOUND('',#18217,.T.);
#12058=FACE_OUTER_BOUND('',#18218,.T.);
#12059=FACE_OUTER_BOUND('',#18219,.T.);
#12060=FACE_OUTER_BOUND('',#18220,.T.);
#12061=FACE_OUTER_BOUND('',#18221,.T.);
#12062=FACE_OUTER_BOUND('',#18222,.T.);
#12063=FACE_OUTER_BOUND('',#18223,.T.);
#12064=FACE_OUTER_BOUND('',#18224,.T.);
#12065=FACE_OUTER_BOUND('',#18225,.T.);
#12066=FACE_OUTER_BOUND('',#18226,.T.);
#12067=FACE_OUTER_BOUND('',#18227,.T.);
#12068=FACE_OUTER_BOUND('',#18228,.T.);
#12069=FACE_OUTER_BOUND('',#18229,.T.);
#12070=FACE_OUTER_BOUND('',#18230,.T.);
#12071=FACE_OUTER_BOUND('',#18231,.T.);
#12072=FACE_OUTER_BOUND('',#18232,.T.);
#12073=FACE_OUTER_BOUND('',#18233,.T.);
#12074=FACE_OUTER_BOUND('',#18234,.T.);
#12075=FACE_OUTER_BOUND('',#18235,.T.);
#12076=FACE_OUTER_BOUND('',#18236,.T.);
#12077=FACE_OUTER_BOUND('',#18237,.T.);
#12078=FACE_OUTER_BOUND('',#18238,.T.);
#12079=FACE_OUTER_BOUND('',#18239,.T.);
#12080=FACE_OUTER_BOUND('',#18240,.T.);
#12081=FACE_OUTER_BOUND('',#18241,.T.);
#12082=FACE_OUTER_BOUND('',#18242,.T.);
#12083=FACE_OUTER_BOUND('',#18243,.T.);
#12084=FACE_OUTER_BOUND('',#18244,.T.);
#12085=FACE_OUTER_BOUND('',#18245,.T.);
#12086=FACE_OUTER_BOUND('',#18246,.T.);
#12087=FACE_OUTER_BOUND('',#18247,.T.);
#12088=FACE_OUTER_BOUND('',#18248,.T.);
#12089=FACE_OUTER_BOUND('',#18249,.T.);
#12090=FACE_OUTER_BOUND('',#18250,.T.);
#12091=FACE_OUTER_BOUND('',#18251,.T.);
#12092=FACE_OUTER_BOUND('',#18252,.T.);
#12093=FACE_OUTER_BOUND('',#18253,.T.);
#12094=FACE_OUTER_BOUND('',#18254,.T.);
#12095=FACE_OUTER_BOUND('',#18255,.T.);
#12096=FACE_OUTER_BOUND('',#18256,.T.);
#12097=FACE_OUTER_BOUND('',#18257,.T.);
#12098=FACE_OUTER_BOUND('',#18258,.T.);
#12099=FACE_OUTER_BOUND('',#18259,.T.);
#12100=FACE_OUTER_BOUND('',#18260,.T.);
#12101=FACE_OUTER_BOUND('',#18261,.T.);
#12102=FACE_OUTER_BOUND('',#18262,.T.);
#12103=FACE_OUTER_BOUND('',#18263,.T.);
#12104=FACE_OUTER_BOUND('',#18264,.T.);
#12105=FACE_OUTER_BOUND('',#18265,.T.);
#12106=FACE_OUTER_BOUND('',#18266,.T.);
#12107=FACE_OUTER_BOUND('',#18267,.T.);
#12108=FACE_OUTER_BOUND('',#18268,.T.);
#12109=FACE_OUTER_BOUND('',#18269,.T.);
#12110=FACE_OUTER_BOUND('',#18270,.T.);
#12111=FACE_OUTER_BOUND('',#18271,.T.);
#12112=FACE_OUTER_BOUND('',#18272,.T.);
#12113=FACE_OUTER_BOUND('',#18273,.T.);
#12114=FACE_OUTER_BOUND('',#18274,.T.);
#12115=FACE_OUTER_BOUND('',#18275,.T.);
#12116=FACE_OUTER_BOUND('',#18276,.T.);
#12117=FACE_OUTER_BOUND('',#18277,.T.);
#12118=FACE_OUTER_BOUND('',#18278,.T.);
#12119=FACE_OUTER_BOUND('',#18279,.T.);
#12120=FACE_OUTER_BOUND('',#18280,.T.);
#12121=FACE_OUTER_BOUND('',#18281,.T.);
#12122=FACE_OUTER_BOUND('',#18282,.T.);
#12123=FACE_OUTER_BOUND('',#18283,.T.);
#12124=FACE_OUTER_BOUND('',#18284,.T.);
#12125=FACE_OUTER_BOUND('',#18285,.T.);
#12126=FACE_OUTER_BOUND('',#18286,.T.);
#12127=FACE_OUTER_BOUND('',#18287,.T.);
#12128=FACE_OUTER_BOUND('',#18288,.T.);
#12129=FACE_OUTER_BOUND('',#18289,.T.);
#12130=FACE_OUTER_BOUND('',#18290,.T.);
#12131=FACE_OUTER_BOUND('',#18291,.T.);
#12132=FACE_OUTER_BOUND('',#18292,.T.);
#12133=FACE_OUTER_BOUND('',#18293,.T.);
#12134=FACE_OUTER_BOUND('',#18294,.T.);
#12135=FACE_OUTER_BOUND('',#18295,.T.);
#12136=FACE_OUTER_BOUND('',#18296,.T.);
#12137=FACE_OUTER_BOUND('',#18297,.T.);
#12138=FACE_OUTER_BOUND('',#18298,.T.);
#12139=FACE_OUTER_BOUND('',#18299,.T.);
#12140=FACE_OUTER_BOUND('',#18300,.T.);
#12141=FACE_OUTER_BOUND('',#18301,.T.);
#12142=FACE_OUTER_BOUND('',#18302,.T.);
#12143=FACE_OUTER_BOUND('',#18303,.T.);
#12144=FACE_OUTER_BOUND('',#18304,.T.);
#12145=FACE_OUTER_BOUND('',#18305,.T.);
#12146=FACE_OUTER_BOUND('',#18306,.T.);
#12147=FACE_OUTER_BOUND('',#18307,.T.);
#12148=FACE_OUTER_BOUND('',#18308,.T.);
#12149=FACE_OUTER_BOUND('',#18309,.T.);
#12150=FACE_OUTER_BOUND('',#18310,.T.);
#12151=FACE_OUTER_BOUND('',#18311,.T.);
#12152=FACE_OUTER_BOUND('',#18312,.T.);
#12153=FACE_OUTER_BOUND('',#18313,.T.);
#12154=FACE_OUTER_BOUND('',#18314,.T.);
#12155=FACE_OUTER_BOUND('',#18315,.T.);
#12156=FACE_OUTER_BOUND('',#18316,.T.);
#12157=FACE_OUTER_BOUND('',#18317,.T.);
#12158=FACE_OUTER_BOUND('',#18318,.T.);
#12159=FACE_OUTER_BOUND('',#18319,.T.);
#12160=FACE_OUTER_BOUND('',#18320,.T.);
#12161=FACE_OUTER_BOUND('',#18321,.T.);
#12162=FACE_OUTER_BOUND('',#18322,.T.);
#12163=FACE_OUTER_BOUND('',#18323,.T.);
#12164=FACE_OUTER_BOUND('',#18324,.T.);
#12165=FACE_OUTER_BOUND('',#18325,.T.);
#12166=FACE_OUTER_BOUND('',#18326,.T.);
#12167=FACE_OUTER_BOUND('',#18327,.T.);
#12168=FACE_OUTER_BOUND('',#18328,.T.);
#12169=FACE_OUTER_BOUND('',#18329,.T.);
#12170=FACE_OUTER_BOUND('',#18330,.T.);
#12171=FACE_OUTER_BOUND('',#18331,.T.);
#12172=FACE_OUTER_BOUND('',#18332,.T.);
#12173=FACE_OUTER_BOUND('',#18333,.T.);
#12174=FACE_OUTER_BOUND('',#18334,.T.);
#12175=FACE_OUTER_BOUND('',#18335,.T.);
#12176=FACE_OUTER_BOUND('',#18336,.T.);
#12177=FACE_OUTER_BOUND('',#18337,.T.);
#12178=FACE_OUTER_BOUND('',#18338,.T.);
#12179=FACE_OUTER_BOUND('',#18339,.T.);
#12180=FACE_OUTER_BOUND('',#18340,.T.);
#12181=FACE_OUTER_BOUND('',#18341,.T.);
#12182=FACE_OUTER_BOUND('',#18342,.T.);
#12183=FACE_OUTER_BOUND('',#18343,.T.);
#12184=FACE_OUTER_BOUND('',#18344,.T.);
#12185=FACE_OUTER_BOUND('',#18345,.T.);
#12186=FACE_OUTER_BOUND('',#18346,.T.);
#12187=FACE_OUTER_BOUND('',#18347,.T.);
#12188=FACE_OUTER_BOUND('',#18348,.T.);
#12189=FACE_OUTER_BOUND('',#18349,.T.);
#12190=FACE_OUTER_BOUND('',#18350,.T.);
#12191=FACE_OUTER_BOUND('',#18351,.T.);
#12192=FACE_OUTER_BOUND('',#18352,.T.);
#12193=FACE_OUTER_BOUND('',#18353,.T.);
#12194=FACE_OUTER_BOUND('',#18354,.T.);
#12195=FACE_OUTER_BOUND('',#18355,.T.);
#12196=FACE_OUTER_BOUND('',#18356,.T.);
#12197=FACE_OUTER_BOUND('',#18357,.T.);
#12198=FACE_OUTER_BOUND('',#18358,.T.);
#12199=FACE_OUTER_BOUND('',#18359,.T.);
#12200=FACE_OUTER_BOUND('',#18360,.T.);
#12201=FACE_OUTER_BOUND('',#18361,.T.);
#12202=FACE_OUTER_BOUND('',#18362,.T.);
#12203=FACE_OUTER_BOUND('',#18363,.T.);
#12204=FACE_OUTER_BOUND('',#18364,.T.);
#12205=FACE_OUTER_BOUND('',#18365,.T.);
#12206=FACE_OUTER_BOUND('',#18366,.T.);
#12207=FACE_OUTER_BOUND('',#18367,.T.);
#12208=FACE_OUTER_BOUND('',#18368,.T.);
#12209=FACE_OUTER_BOUND('',#18369,.T.);
#12210=FACE_OUTER_BOUND('',#18370,.T.);
#12211=FACE_OUTER_BOUND('',#18371,.T.);
#12212=FACE_OUTER_BOUND('',#18372,.T.);
#12213=FACE_OUTER_BOUND('',#18373,.T.);
#12214=FACE_OUTER_BOUND('',#18374,.T.);
#12215=FACE_OUTER_BOUND('',#18375,.T.);
#12216=FACE_OUTER_BOUND('',#18376,.T.);
#12217=FACE_OUTER_BOUND('',#18377,.T.);
#12218=FACE_OUTER_BOUND('',#18378,.T.);
#12219=FACE_OUTER_BOUND('',#18379,.T.);
#12220=FACE_OUTER_BOUND('',#18380,.T.);
#12221=FACE_OUTER_BOUND('',#18381,.T.);
#12222=FACE_OUTER_BOUND('',#18382,.T.);
#12223=FACE_OUTER_BOUND('',#18383,.T.);
#12224=FACE_OUTER_BOUND('',#18384,.T.);
#12225=FACE_OUTER_BOUND('',#18385,.T.);
#12226=FACE_OUTER_BOUND('',#18386,.T.);
#12227=FACE_OUTER_BOUND('',#18387,.T.);
#12228=FACE_OUTER_BOUND('',#18388,.T.);
#12229=FACE_OUTER_BOUND('',#18389,.T.);
#12230=FACE_OUTER_BOUND('',#18390,.T.);
#12231=FACE_OUTER_BOUND('',#18391,.T.);
#12232=FACE_OUTER_BOUND('',#18392,.T.);
#12233=FACE_OUTER_BOUND('',#18393,.T.);
#12234=FACE_OUTER_BOUND('',#18394,.T.);
#12235=FACE_OUTER_BOUND('',#18395,.T.);
#12236=FACE_OUTER_BOUND('',#18396,.T.);
#12237=FACE_OUTER_BOUND('',#18397,.T.);
#12238=FACE_OUTER_BOUND('',#18398,.T.);
#12239=FACE_OUTER_BOUND('',#18399,.T.);
#12240=FACE_OUTER_BOUND('',#18400,.T.);
#12241=FACE_OUTER_BOUND('',#18401,.T.);
#12242=FACE_OUTER_BOUND('',#18402,.T.);
#12243=FACE_OUTER_BOUND('',#18403,.T.);
#12244=FACE_OUTER_BOUND('',#18404,.T.);
#12245=FACE_OUTER_BOUND('',#18405,.T.);
#12246=FACE_OUTER_BOUND('',#18406,.T.);
#12247=FACE_OUTER_BOUND('',#18407,.T.);
#12248=FACE_OUTER_BOUND('',#18408,.T.);
#12249=FACE_OUTER_BOUND('',#18409,.T.);
#12250=FACE_OUTER_BOUND('',#18410,.T.);
#12251=FACE_OUTER_BOUND('',#18411,.T.);
#12252=FACE_OUTER_BOUND('',#18412,.T.);
#12253=FACE_OUTER_BOUND('',#18413,.T.);
#12254=FACE_OUTER_BOUND('',#18414,.T.);
#12255=FACE_OUTER_BOUND('',#18415,.T.);
#12256=FACE_OUTER_BOUND('',#18416,.T.);
#12257=FACE_OUTER_BOUND('',#18417,.T.);
#12258=FACE_OUTER_BOUND('',#18418,.T.);
#12259=FACE_OUTER_BOUND('',#18419,.T.);
#12260=FACE_OUTER_BOUND('',#18420,.T.);
#12261=FACE_OUTER_BOUND('',#18421,.T.);
#12262=FACE_OUTER_BOUND('',#18422,.T.);
#12263=FACE_OUTER_BOUND('',#18423,.T.);
#12264=FACE_OUTER_BOUND('',#18424,.T.);
#12265=FACE_OUTER_BOUND('',#18425,.T.);
#12266=FACE_OUTER_BOUND('',#18426,.T.);
#12267=FACE_OUTER_BOUND('',#18427,.T.);
#12268=FACE_OUTER_BOUND('',#18428,.T.);
#12269=FACE_OUTER_BOUND('',#18429,.T.);
#12270=FACE_OUTER_BOUND('',#18430,.T.);
#12271=FACE_OUTER_BOUND('',#18431,.T.);
#12272=FACE_OUTER_BOUND('',#18432,.T.);
#12273=FACE_OUTER_BOUND('',#18433,.T.);
#12274=FACE_OUTER_BOUND('',#18434,.T.);
#12275=FACE_OUTER_BOUND('',#18435,.T.);
#12276=FACE_OUTER_BOUND('',#18436,.T.);
#12277=FACE_OUTER_BOUND('',#18437,.T.);
#12278=FACE_OUTER_BOUND('',#18438,.T.);
#12279=FACE_OUTER_BOUND('',#18439,.T.);
#12280=FACE_OUTER_BOUND('',#18440,.T.);
#12281=FACE_OUTER_BOUND('',#18441,.T.);
#12282=FACE_OUTER_BOUND('',#18442,.T.);
#12283=FACE_OUTER_BOUND('',#18443,.T.);
#12284=FACE_OUTER_BOUND('',#18444,.T.);
#12285=FACE_OUTER_BOUND('',#18445,.T.);
#12286=FACE_OUTER_BOUND('',#18446,.T.);
#12287=FACE_OUTER_BOUND('',#18447,.T.);
#12288=FACE_OUTER_BOUND('',#18448,.T.);
#12289=FACE_OUTER_BOUND('',#18449,.T.);
#12290=FACE_OUTER_BOUND('',#18450,.T.);
#12291=FACE_OUTER_BOUND('',#18451,.T.);
#12292=FACE_OUTER_BOUND('',#18452,.T.);
#12293=FACE_OUTER_BOUND('',#18453,.T.);
#12294=FACE_OUTER_BOUND('',#18454,.T.);
#12295=FACE_OUTER_BOUND('',#18455,.T.);
#12296=FACE_OUTER_BOUND('',#18456,.T.);
#12297=FACE_OUTER_BOUND('',#18457,.T.);
#12298=FACE_OUTER_BOUND('',#18458,.T.);
#12299=FACE_OUTER_BOUND('',#18459,.T.);
#12300=FACE_OUTER_BOUND('',#18460,.T.);
#12301=FACE_OUTER_BOUND('',#18461,.T.);
#12302=FACE_OUTER_BOUND('',#18462,.T.);
#12303=FACE_OUTER_BOUND('',#18463,.T.);
#12304=FACE_OUTER_BOUND('',#18464,.T.);
#12305=FACE_OUTER_BOUND('',#18465,.T.);
#12306=FACE_OUTER_BOUND('',#18466,.T.);
#12307=FACE_OUTER_BOUND('',#18467,.T.);
#12308=FACE_OUTER_BOUND('',#18468,.T.);
#12309=FACE_OUTER_BOUND('',#18469,.T.);
#12310=FACE_OUTER_BOUND('',#18470,.T.);
#12311=FACE_OUTER_BOUND('',#18471,.T.);
#12312=FACE_OUTER_BOUND('',#18472,.T.);
#12313=FACE_OUTER_BOUND('',#18473,.T.);
#12314=FACE_OUTER_BOUND('',#18474,.T.);
#12315=FACE_OUTER_BOUND('',#18475,.T.);
#12316=FACE_OUTER_BOUND('',#18476,.T.);
#12317=FACE_OUTER_BOUND('',#18477,.T.);
#12318=FACE_OUTER_BOUND('',#18478,.T.);
#12319=FACE_OUTER_BOUND('',#18479,.T.);
#12320=FACE_OUTER_BOUND('',#18480,.T.);
#12321=FACE_OUTER_BOUND('',#18481,.T.);
#12322=FACE_OUTER_BOUND('',#18482,.T.);
#12323=FACE_OUTER_BOUND('',#18483,.T.);
#12324=FACE_OUTER_BOUND('',#18484,.T.);
#12325=FACE_OUTER_BOUND('',#18485,.T.);
#12326=FACE_OUTER_BOUND('',#18486,.T.);
#12327=FACE_OUTER_BOUND('',#18487,.T.);
#12328=FACE_OUTER_BOUND('',#18488,.T.);
#12329=FACE_OUTER_BOUND('',#18489,.T.);
#12330=FACE_OUTER_BOUND('',#18490,.T.);
#12331=FACE_OUTER_BOUND('',#18491,.T.);
#12332=FACE_OUTER_BOUND('',#18492,.T.);
#12333=FACE_OUTER_BOUND('',#18493,.T.);
#12334=FACE_OUTER_BOUND('',#18494,.T.);
#12335=FACE_OUTER_BOUND('',#18495,.T.);
#12336=FACE_OUTER_BOUND('',#18496,.T.);
#12337=FACE_OUTER_BOUND('',#18497,.T.);
#12338=FACE_OUTER_BOUND('',#18498,.T.);
#12339=FACE_OUTER_BOUND('',#18499,.T.);
#12340=FACE_OUTER_BOUND('',#18500,.T.);
#12341=FACE_OUTER_BOUND('',#18501,.T.);
#12342=FACE_OUTER_BOUND('',#18502,.T.);
#12343=FACE_OUTER_BOUND('',#18503,.T.);
#12344=FACE_OUTER_BOUND('',#18504,.T.);
#12345=FACE_OUTER_BOUND('',#18505,.T.);
#12346=FACE_OUTER_BOUND('',#18506,.T.);
#12347=FACE_OUTER_BOUND('',#18507,.T.);
#12348=FACE_OUTER_BOUND('',#18508,.T.);
#12349=FACE_OUTER_BOUND('',#18509,.T.);
#12350=FACE_OUTER_BOUND('',#18510,.T.);
#12351=FACE_OUTER_BOUND('',#18511,.T.);
#12352=FACE_OUTER_BOUND('',#18512,.T.);
#12353=FACE_OUTER_BOUND('',#18513,.T.);
#12354=FACE_OUTER_BOUND('',#18514,.T.);
#12355=FACE_OUTER_BOUND('',#18515,.T.);
#12356=FACE_OUTER_BOUND('',#18516,.T.);
#12357=FACE_OUTER_BOUND('',#18517,.T.);
#12358=FACE_OUTER_BOUND('',#18518,.T.);
#12359=FACE_OUTER_BOUND('',#18519,.T.);
#12360=FACE_OUTER_BOUND('',#18520,.T.);
#12361=FACE_OUTER_BOUND('',#18521,.T.);
#12362=FACE_OUTER_BOUND('',#18522,.T.);
#12363=FACE_OUTER_BOUND('',#18523,.T.);
#12364=FACE_OUTER_BOUND('',#18524,.T.);
#12365=FACE_OUTER_BOUND('',#18525,.T.);
#12366=FACE_OUTER_BOUND('',#18526,.T.);
#12367=FACE_OUTER_BOUND('',#18527,.T.);
#12368=FACE_OUTER_BOUND('',#18528,.T.);
#12369=FACE_OUTER_BOUND('',#18529,.T.);
#12370=FACE_OUTER_BOUND('',#18530,.T.);
#12371=FACE_OUTER_BOUND('',#18531,.T.);
#12372=FACE_OUTER_BOUND('',#18532,.T.);
#12373=FACE_OUTER_BOUND('',#18533,.T.);
#12374=FACE_OUTER_BOUND('',#18534,.T.);
#12375=FACE_OUTER_BOUND('',#18535,.T.);
#12376=FACE_OUTER_BOUND('',#18536,.T.);
#12377=FACE_OUTER_BOUND('',#18537,.T.);
#12378=FACE_OUTER_BOUND('',#18538,.T.);
#12379=FACE_OUTER_BOUND('',#18539,.T.);
#12380=FACE_OUTER_BOUND('',#18540,.T.);
#12381=FACE_OUTER_BOUND('',#18541,.T.);
#12382=FACE_OUTER_BOUND('',#18542,.T.);
#12383=FACE_OUTER_BOUND('',#18543,.T.);
#12384=FACE_OUTER_BOUND('',#18544,.T.);
#12385=FACE_OUTER_BOUND('',#18545,.T.);
#12386=FACE_OUTER_BOUND('',#18546,.T.);
#12387=FACE_OUTER_BOUND('',#18547,.T.);
#12388=FACE_OUTER_BOUND('',#18548,.T.);
#12389=FACE_OUTER_BOUND('',#18549,.T.);
#12390=FACE_OUTER_BOUND('',#18550,.T.);
#12391=FACE_OUTER_BOUND('',#18551,.T.);
#12392=FACE_OUTER_BOUND('',#18552,.T.);
#12393=FACE_OUTER_BOUND('',#18553,.T.);
#12394=FACE_OUTER_BOUND('',#18554,.T.);
#12395=FACE_OUTER_BOUND('',#18555,.T.);
#12396=FACE_OUTER_BOUND('',#18556,.T.);
#12397=FACE_OUTER_BOUND('',#18557,.T.);
#12398=FACE_OUTER_BOUND('',#18558,.T.);
#12399=FACE_OUTER_BOUND('',#18559,.T.);
#12400=FACE_OUTER_BOUND('',#18560,.T.);
#12401=FACE_OUTER_BOUND('',#18561,.T.);
#12402=FACE_OUTER_BOUND('',#18562,.T.);
#12403=FACE_OUTER_BOUND('',#18563,.T.);
#12404=FACE_OUTER_BOUND('',#18564,.T.);
#12405=FACE_OUTER_BOUND('',#18565,.T.);
#12406=FACE_OUTER_BOUND('',#18566,.T.);
#12407=FACE_OUTER_BOUND('',#18567,.T.);
#12408=FACE_OUTER_BOUND('',#18568,.T.);
#12409=FACE_OUTER_BOUND('',#18569,.T.);
#12410=FACE_OUTER_BOUND('',#18570,.T.);
#12411=FACE_OUTER_BOUND('',#18571,.T.);
#12412=FACE_OUTER_BOUND('',#18572,.T.);
#12413=FACE_OUTER_BOUND('',#18573,.T.);
#12414=FACE_OUTER_BOUND('',#18574,.T.);
#12415=FACE_OUTER_BOUND('',#18575,.T.);
#12416=FACE_OUTER_BOUND('',#18576,.T.);
#12417=FACE_OUTER_BOUND('',#18577,.T.);
#12418=FACE_OUTER_BOUND('',#18578,.T.);
#12419=FACE_OUTER_BOUND('',#18579,.T.);
#12420=FACE_OUTER_BOUND('',#18580,.T.);
#12421=FACE_OUTER_BOUND('',#18581,.T.);
#12422=FACE_OUTER_BOUND('',#18582,.T.);
#12423=FACE_OUTER_BOUND('',#18583,.T.);
#12424=FACE_OUTER_BOUND('',#18584,.T.);
#12425=FACE_OUTER_BOUND('',#18585,.T.);
#12426=FACE_OUTER_BOUND('',#18586,.T.);
#12427=FACE_OUTER_BOUND('',#18587,.T.);
#12428=FACE_OUTER_BOUND('',#18588,.T.);
#12429=FACE_OUTER_BOUND('',#18589,.T.);
#12430=FACE_OUTER_BOUND('',#18590,.T.);
#12431=FACE_OUTER_BOUND('',#18591,.T.);
#12432=FACE_OUTER_BOUND('',#18592,.T.);
#12433=FACE_OUTER_BOUND('',#18593,.T.);
#12434=FACE_OUTER_BOUND('',#18594,.T.);
#12435=FACE_OUTER_BOUND('',#18595,.T.);
#12436=FACE_OUTER_BOUND('',#18596,.T.);
#12437=FACE_OUTER_BOUND('',#18597,.T.);
#12438=FACE_OUTER_BOUND('',#18598,.T.);
#12439=FACE_OUTER_BOUND('',#18599,.T.);
#12440=FACE_OUTER_BOUND('',#18600,.T.);
#12441=FACE_OUTER_BOUND('',#18601,.T.);
#12442=FACE_OUTER_BOUND('',#18602,.T.);
#12443=FACE_OUTER_BOUND('',#18603,.T.);
#12444=FACE_OUTER_BOUND('',#18604,.T.);
#12445=FACE_OUTER_BOUND('',#18605,.T.);
#12446=FACE_OUTER_BOUND('',#18606,.T.);
#12447=FACE_OUTER_BOUND('',#18607,.T.);
#12448=FACE_OUTER_BOUND('',#18608,.T.);
#12449=FACE_OUTER_BOUND('',#18609,.T.);
#12450=FACE_OUTER_BOUND('',#18610,.T.);
#12451=FACE_OUTER_BOUND('',#18611,.T.);
#12452=FACE_OUTER_BOUND('',#18612,.T.);
#12453=FACE_OUTER_BOUND('',#18613,.T.);
#12454=FACE_OUTER_BOUND('',#18614,.T.);
#12455=FACE_OUTER_BOUND('',#18615,.T.);
#12456=FACE_OUTER_BOUND('',#18616,.T.);
#12457=FACE_OUTER_BOUND('',#18617,.T.);
#12458=FACE_OUTER_BOUND('',#18618,.T.);
#12459=FACE_OUTER_BOUND('',#18619,.T.);
#12460=FACE_OUTER_BOUND('',#18620,.T.);
#12461=FACE_OUTER_BOUND('',#18621,.T.);
#12462=FACE_OUTER_BOUND('',#18622,.T.);
#12463=FACE_OUTER_BOUND('',#18623,.T.);
#12464=FACE_OUTER_BOUND('',#18624,.T.);
#12465=FACE_OUTER_BOUND('',#18625,.T.);
#12466=FACE_OUTER_BOUND('',#18626,.T.);
#12467=FACE_OUTER_BOUND('',#18627,.T.);
#12468=FACE_OUTER_BOUND('',#18628,.T.);
#12469=FACE_OUTER_BOUND('',#18629,.T.);
#12470=FACE_OUTER_BOUND('',#18630,.T.);
#12471=FACE_OUTER_BOUND('',#18631,.T.);
#12472=FACE_OUTER_BOUND('',#18632,.T.);
#12473=FACE_OUTER_BOUND('',#18633,.T.);
#12474=FACE_OUTER_BOUND('',#18634,.T.);
#12475=FACE_OUTER_BOUND('',#18635,.T.);
#12476=FACE_OUTER_BOUND('',#18636,.T.);
#12477=FACE_OUTER_BOUND('',#18637,.T.);
#12478=FACE_OUTER_BOUND('',#18638,.T.);
#12479=FACE_OUTER_BOUND('',#18639,.T.);
#12480=FACE_OUTER_BOUND('',#18640,.T.);
#12481=FACE_OUTER_BOUND('',#18641,.T.);
#12482=FACE_OUTER_BOUND('',#18642,.T.);
#12483=FACE_OUTER_BOUND('',#18643,.T.);
#12484=FACE_OUTER_BOUND('',#18644,.T.);
#12485=FACE_OUTER_BOUND('',#18645,.T.);
#12486=FACE_OUTER_BOUND('',#18646,.T.);
#12487=FACE_OUTER_BOUND('',#18647,.T.);
#12488=FACE_OUTER_BOUND('',#18648,.T.);
#12489=FACE_OUTER_BOUND('',#18649,.T.);
#12490=FACE_OUTER_BOUND('',#18650,.T.);
#12491=FACE_OUTER_BOUND('',#18651,.T.);
#12492=FACE_OUTER_BOUND('',#18652,.T.);
#12493=FACE_OUTER_BOUND('',#18653,.T.);
#12494=FACE_OUTER_BOUND('',#18654,.T.);
#12495=FACE_OUTER_BOUND('',#18655,.T.);
#12496=FACE_OUTER_BOUND('',#18656,.T.);
#12497=FACE_OUTER_BOUND('',#18657,.T.);
#12498=FACE_OUTER_BOUND('',#18658,.T.);
#12499=FACE_OUTER_BOUND('',#18659,.T.);
#12500=FACE_OUTER_BOUND('',#18660,.T.);
#12501=FACE_OUTER_BOUND('',#18661,.T.);
#12502=FACE_OUTER_BOUND('',#18662,.T.);
#12503=FACE_OUTER_BOUND('',#18663,.T.);
#12504=FACE_OUTER_BOUND('',#18664,.T.);
#12505=FACE_OUTER_BOUND('',#18665,.T.);
#12506=FACE_OUTER_BOUND('',#18666,.T.);
#12507=FACE_OUTER_BOUND('',#18667,.T.);
#12508=FACE_OUTER_BOUND('',#18668,.T.);
#12509=FACE_OUTER_BOUND('',#18669,.T.);
#12510=FACE_OUTER_BOUND('',#18670,.T.);
#12511=FACE_OUTER_BOUND('',#18671,.T.);
#12512=FACE_OUTER_BOUND('',#18672,.T.);
#12513=FACE_OUTER_BOUND('',#18673,.T.);
#12514=FACE_OUTER_BOUND('',#18674,.T.);
#12515=FACE_OUTER_BOUND('',#18675,.T.);
#12516=FACE_OUTER_BOUND('',#18676,.T.);
#12517=FACE_OUTER_BOUND('',#18677,.T.);
#12518=FACE_OUTER_BOUND('',#18678,.T.);
#12519=FACE_OUTER_BOUND('',#18679,.T.);
#12520=FACE_OUTER_BOUND('',#18680,.T.);
#12521=FACE_OUTER_BOUND('',#18681,.T.);
#12522=FACE_OUTER_BOUND('',#18682,.T.);
#12523=FACE_OUTER_BOUND('',#18683,.T.);
#12524=FACE_OUTER_BOUND('',#18684,.T.);
#12525=FACE_OUTER_BOUND('',#18685,.T.);
#12526=FACE_OUTER_BOUND('',#18686,.T.);
#12527=FACE_OUTER_BOUND('',#18687,.T.);
#12528=FACE_OUTER_BOUND('',#18688,.T.);
#12529=FACE_OUTER_BOUND('',#18689,.T.);
#12530=FACE_OUTER_BOUND('',#18690,.T.);
#12531=FACE_OUTER_BOUND('',#18691,.T.);
#12532=FACE_OUTER_BOUND('',#18692,.T.);
#12533=FACE_OUTER_BOUND('',#18693,.T.);
#12534=FACE_OUTER_BOUND('',#18694,.T.);
#12535=FACE_OUTER_BOUND('',#18695,.T.);
#12536=FACE_OUTER_BOUND('',#18696,.T.);
#12537=FACE_OUTER_BOUND('',#18697,.T.);
#12538=FACE_OUTER_BOUND('',#18698,.T.);
#12539=FACE_OUTER_BOUND('',#18699,.T.);
#12540=FACE_OUTER_BOUND('',#18700,.T.);
#12541=FACE_OUTER_BOUND('',#18701,.T.);
#12542=FACE_OUTER_BOUND('',#18702,.T.);
#12543=FACE_OUTER_BOUND('',#18703,.T.);
#12544=FACE_OUTER_BOUND('',#18704,.T.);
#12545=FACE_OUTER_BOUND('',#18705,.T.);
#12546=FACE_OUTER_BOUND('',#18706,.T.);
#12547=FACE_OUTER_BOUND('',#18707,.T.);
#12548=FACE_OUTER_BOUND('',#18708,.T.);
#12549=FACE_OUTER_BOUND('',#18709,.T.);
#12550=FACE_OUTER_BOUND('',#18710,.T.);
#12551=FACE_OUTER_BOUND('',#18711,.T.);
#12552=FACE_OUTER_BOUND('',#18712,.T.);
#12553=FACE_OUTER_BOUND('',#18713,.T.);
#12554=FACE_OUTER_BOUND('',#18714,.T.);
#12555=FACE_OUTER_BOUND('',#18715,.T.);
#12556=FACE_OUTER_BOUND('',#18716,.T.);
#12557=FACE_OUTER_BOUND('',#18717,.T.);
#12558=FACE_OUTER_BOUND('',#18718,.T.);
#12559=FACE_OUTER_BOUND('',#18719,.T.);
#12560=FACE_OUTER_BOUND('',#18720,.T.);
#12561=FACE_OUTER_BOUND('',#18721,.T.);
#12562=FACE_OUTER_BOUND('',#18722,.T.);
#12563=FACE_OUTER_BOUND('',#18723,.T.);
#12564=FACE_OUTER_BOUND('',#18724,.T.);
#12565=FACE_OUTER_BOUND('',#18725,.T.);
#12566=FACE_OUTER_BOUND('',#18726,.T.);
#12567=FACE_OUTER_BOUND('',#18727,.T.);
#12568=FACE_OUTER_BOUND('',#18728,.T.);
#12569=FACE_OUTER_BOUND('',#18729,.T.);
#12570=FACE_OUTER_BOUND('',#18730,.T.);
#12571=FACE_OUTER_BOUND('',#18731,.T.);
#12572=FACE_OUTER_BOUND('',#18732,.T.);
#12573=FACE_OUTER_BOUND('',#18733,.T.);
#12574=FACE_OUTER_BOUND('',#18734,.T.);
#12575=FACE_OUTER_BOUND('',#18735,.T.);
#12576=FACE_OUTER_BOUND('',#18736,.T.);
#12577=FACE_OUTER_BOUND('',#18737,.T.);
#12578=FACE_OUTER_BOUND('',#18738,.T.);
#12579=FACE_OUTER_BOUND('',#18739,.T.);
#12580=FACE_OUTER_BOUND('',#18740,.T.);
#12581=FACE_OUTER_BOUND('',#18741,.T.);
#12582=FACE_OUTER_BOUND('',#18742,.T.);
#12583=FACE_OUTER_BOUND('',#18743,.T.);
#12584=FACE_OUTER_BOUND('',#18744,.T.);
#12585=FACE_OUTER_BOUND('',#18745,.T.);
#12586=FACE_OUTER_BOUND('',#18746,.T.);
#12587=FACE_OUTER_BOUND('',#18747,.T.);
#12588=FACE_OUTER_BOUND('',#18748,.T.);
#12589=FACE_OUTER_BOUND('',#18749,.T.);
#12590=FACE_OUTER_BOUND('',#18750,.T.);
#12591=FACE_OUTER_BOUND('',#18751,.T.);
#12592=FACE_OUTER_BOUND('',#18752,.T.);
#12593=FACE_OUTER_BOUND('',#18753,.T.);
#12594=FACE_OUTER_BOUND('',#18754,.T.);
#12595=FACE_OUTER_BOUND('',#18755,.T.);
#12596=FACE_OUTER_BOUND('',#18756,.T.);
#12597=FACE_OUTER_BOUND('',#18757,.T.);
#12598=FACE_OUTER_BOUND('',#18758,.T.);
#12599=FACE_OUTER_BOUND('',#18759,.T.);
#12600=FACE_OUTER_BOUND('',#18760,.T.);
#12601=FACE_OUTER_BOUND('',#18761,.T.);
#12602=FACE_OUTER_BOUND('',#18762,.T.);
#12603=FACE_OUTER_BOUND('',#18763,.T.);
#12604=FACE_OUTER_BOUND('',#18764,.T.);
#12605=FACE_OUTER_BOUND('',#18765,.T.);
#12606=FACE_OUTER_BOUND('',#18766,.T.);
#12607=FACE_OUTER_BOUND('',#18767,.T.);
#12608=FACE_OUTER_BOUND('',#18768,.T.);
#12609=FACE_OUTER_BOUND('',#18769,.T.);
#12610=FACE_OUTER_BOUND('',#18770,.T.);
#12611=FACE_OUTER_BOUND('',#18771,.T.);
#12612=FACE_OUTER_BOUND('',#18772,.T.);
#12613=FACE_OUTER_BOUND('',#18773,.T.);
#12614=FACE_OUTER_BOUND('',#18774,.T.);
#12615=FACE_OUTER_BOUND('',#18775,.T.);
#12616=FACE_OUTER_BOUND('',#18776,.T.);
#12617=FACE_OUTER_BOUND('',#18777,.T.);
#12618=FACE_OUTER_BOUND('',#18778,.T.);
#12619=FACE_OUTER_BOUND('',#18779,.T.);
#12620=FACE_OUTER_BOUND('',#18780,.T.);
#12621=FACE_OUTER_BOUND('',#18781,.T.);
#12622=FACE_OUTER_BOUND('',#18782,.T.);
#12623=FACE_OUTER_BOUND('',#18783,.T.);
#12624=FACE_OUTER_BOUND('',#18784,.T.);
#12625=FACE_OUTER_BOUND('',#18785,.T.);
#12626=FACE_OUTER_BOUND('',#18786,.T.);
#12627=FACE_OUTER_BOUND('',#18787,.T.);
#12628=FACE_OUTER_BOUND('',#18788,.T.);
#12629=FACE_OUTER_BOUND('',#18789,.T.);
#12630=FACE_OUTER_BOUND('',#18790,.T.);
#12631=FACE_OUTER_BOUND('',#18791,.T.);
#12632=FACE_OUTER_BOUND('',#18792,.T.);
#12633=FACE_OUTER_BOUND('',#18793,.T.);
#12634=FACE_OUTER_BOUND('',#18794,.T.);
#12635=FACE_OUTER_BOUND('',#18795,.T.);
#12636=FACE_OUTER_BOUND('',#18796,.T.);
#12637=FACE_OUTER_BOUND('',#18797,.T.);
#12638=FACE_OUTER_BOUND('',#18798,.T.);
#12639=FACE_OUTER_BOUND('',#18799,.T.);
#12640=FACE_OUTER_BOUND('',#18800,.T.);
#12641=FACE_OUTER_BOUND('',#18801,.T.);
#12642=FACE_OUTER_BOUND('',#18802,.T.);
#12643=FACE_OUTER_BOUND('',#18803,.T.);
#12644=FACE_OUTER_BOUND('',#18804,.T.);
#12645=FACE_OUTER_BOUND('',#18805,.T.);
#12646=FACE_OUTER_BOUND('',#18806,.T.);
#12647=FACE_OUTER_BOUND('',#18807,.T.);
#12648=FACE_OUTER_BOUND('',#18808,.T.);
#12649=FACE_OUTER_BOUND('',#18809,.T.);
#12650=FACE_OUTER_BOUND('',#18810,.T.);
#12651=FACE_OUTER_BOUND('',#18811,.T.);
#12652=FACE_OUTER_BOUND('',#18812,.T.);
#12653=FACE_OUTER_BOUND('',#18813,.T.);
#12654=FACE_OUTER_BOUND('',#18814,.T.);
#12655=FACE_OUTER_BOUND('',#18815,.T.);
#12656=FACE_OUTER_BOUND('',#18816,.T.);
#12657=FACE_OUTER_BOUND('',#18817,.T.);
#12658=FACE_OUTER_BOUND('',#18818,.T.);
#12659=FACE_OUTER_BOUND('',#18819,.T.);
#12660=FACE_OUTER_BOUND('',#18820,.T.);
#12661=FACE_OUTER_BOUND('',#18821,.T.);
#12662=FACE_OUTER_BOUND('',#18822,.T.);
#12663=FACE_OUTER_BOUND('',#18823,.T.);
#12664=FACE_OUTER_BOUND('',#18824,.T.);
#12665=FACE_OUTER_BOUND('',#18825,.T.);
#12666=FACE_OUTER_BOUND('',#18826,.T.);
#12667=FACE_OUTER_BOUND('',#18827,.T.);
#12668=FACE_OUTER_BOUND('',#18828,.T.);
#12669=FACE_OUTER_BOUND('',#18829,.T.);
#12670=FACE_OUTER_BOUND('',#18830,.T.);
#12671=FACE_OUTER_BOUND('',#18831,.T.);
#12672=FACE_OUTER_BOUND('',#18832,.T.);
#12673=FACE_OUTER_BOUND('',#18833,.T.);
#12674=FACE_OUTER_BOUND('',#18834,.T.);
#12675=FACE_OUTER_BOUND('',#18835,.T.);
#12676=FACE_OUTER_BOUND('',#18836,.T.);
#12677=FACE_OUTER_BOUND('',#18837,.T.);
#12678=FACE_OUTER_BOUND('',#18838,.T.);
#12679=FACE_OUTER_BOUND('',#18839,.T.);
#12680=FACE_OUTER_BOUND('',#18840,.T.);
#12681=FACE_OUTER_BOUND('',#18841,.T.);
#12682=FACE_OUTER_BOUND('',#18842,.T.);
#12683=FACE_OUTER_BOUND('',#18843,.T.);
#12684=FACE_OUTER_BOUND('',#18844,.T.);
#12685=FACE_OUTER_BOUND('',#18845,.T.);
#12686=FACE_OUTER_BOUND('',#18846,.T.);
#12687=FACE_OUTER_BOUND('',#18847,.T.);
#12688=FACE_OUTER_BOUND('',#18848,.T.);
#12689=FACE_OUTER_BOUND('',#18849,.T.);
#12690=FACE_OUTER_BOUND('',#18850,.T.);
#12691=FACE_OUTER_BOUND('',#18851,.T.);
#12692=FACE_OUTER_BOUND('',#18852,.T.);
#12693=FACE_OUTER_BOUND('',#18853,.T.);
#12694=FACE_OUTER_BOUND('',#18854,.T.);
#12695=FACE_OUTER_BOUND('',#18855,.T.);
#12696=FACE_OUTER_BOUND('',#18856,.T.);
#12697=FACE_OUTER_BOUND('',#18857,.T.);
#12698=FACE_OUTER_BOUND('',#18858,.T.);
#12699=FACE_OUTER_BOUND('',#18859,.T.);
#12700=FACE_OUTER_BOUND('',#18860,.T.);
#12701=FACE_OUTER_BOUND('',#18861,.T.);
#12702=FACE_OUTER_BOUND('',#18862,.T.);
#12703=FACE_OUTER_BOUND('',#18863,.T.);
#12704=FACE_OUTER_BOUND('',#18864,.T.);
#12705=FACE_OUTER_BOUND('',#18865,.T.);
#12706=FACE_OUTER_BOUND('',#18866,.T.);
#12707=FACE_OUTER_BOUND('',#18867,.T.);
#12708=FACE_OUTER_BOUND('',#18868,.T.);
#12709=FACE_OUTER_BOUND('',#18869,.T.);
#12710=FACE_OUTER_BOUND('',#18870,.T.);
#12711=FACE_OUTER_BOUND('',#18871,.T.);
#12712=FACE_OUTER_BOUND('',#18872,.T.);
#12713=FACE_OUTER_BOUND('',#18873,.T.);
#12714=FACE_OUTER_BOUND('',#18874,.T.);
#12715=FACE_OUTER_BOUND('',#18875,.T.);
#12716=FACE_OUTER_BOUND('',#18876,.T.);
#12717=FACE_OUTER_BOUND('',#18877,.T.);
#12718=FACE_OUTER_BOUND('',#18878,.T.);
#12719=FACE_OUTER_BOUND('',#18879,.T.);
#12720=FACE_OUTER_BOUND('',#18880,.T.);
#12721=FACE_OUTER_BOUND('',#18881,.T.);
#12722=FACE_OUTER_BOUND('',#18882,.T.);
#12723=FACE_OUTER_BOUND('',#18883,.T.);
#12724=FACE_OUTER_BOUND('',#18884,.T.);
#12725=FACE_OUTER_BOUND('',#18885,.T.);
#12726=FACE_OUTER_BOUND('',#18886,.T.);
#12727=FACE_OUTER_BOUND('',#18887,.T.);
#12728=FACE_OUTER_BOUND('',#18888,.T.);
#12729=FACE_OUTER_BOUND('',#18889,.T.);
#12730=FACE_OUTER_BOUND('',#18890,.T.);
#12731=FACE_OUTER_BOUND('',#18891,.T.);
#12732=FACE_OUTER_BOUND('',#18892,.T.);
#12733=FACE_OUTER_BOUND('',#18893,.T.);
#12734=FACE_OUTER_BOUND('',#18894,.T.);
#12735=FACE_OUTER_BOUND('',#18895,.T.);
#12736=FACE_OUTER_BOUND('',#18896,.T.);
#12737=FACE_OUTER_BOUND('',#18897,.T.);
#12738=FACE_OUTER_BOUND('',#18898,.T.);
#12739=FACE_OUTER_BOUND('',#18899,.T.);
#12740=FACE_OUTER_BOUND('',#18900,.T.);
#12741=FACE_OUTER_BOUND('',#18901,.T.);
#12742=FACE_OUTER_BOUND('',#18902,.T.);
#12743=FACE_OUTER_BOUND('',#18903,.T.);
#12744=FACE_OUTER_BOUND('',#18904,.T.);
#12745=FACE_OUTER_BOUND('',#18905,.T.);
#12746=FACE_OUTER_BOUND('',#18906,.T.);
#12747=FACE_OUTER_BOUND('',#18907,.T.);
#12748=FACE_OUTER_BOUND('',#18908,.T.);
#12749=FACE_OUTER_BOUND('',#18909,.T.);
#12750=FACE_OUTER_BOUND('',#18910,.T.);
#12751=FACE_OUTER_BOUND('',#18911,.T.);
#12752=FACE_OUTER_BOUND('',#18912,.T.);
#12753=FACE_OUTER_BOUND('',#18913,.T.);
#12754=FACE_OUTER_BOUND('',#18914,.T.);
#12755=FACE_OUTER_BOUND('',#18915,.T.);
#12756=FACE_OUTER_BOUND('',#18916,.T.);
#12757=FACE_OUTER_BOUND('',#18917,.T.);
#12758=FACE_OUTER_BOUND('',#18918,.T.);
#12759=FACE_OUTER_BOUND('',#18919,.T.);
#12760=FACE_OUTER_BOUND('',#18920,.T.);
#12761=FACE_OUTER_BOUND('',#18921,.T.);
#12762=FACE_OUTER_BOUND('',#18922,.T.);
#12763=FACE_OUTER_BOUND('',#18923,.T.);
#12764=FACE_OUTER_BOUND('',#18924,.T.);
#12765=FACE_OUTER_BOUND('',#18925,.T.);
#12766=FACE_OUTER_BOUND('',#18926,.T.);
#12767=FACE_OUTER_BOUND('',#18927,.T.);
#12768=FACE_OUTER_BOUND('',#18928,.T.);
#12769=FACE_OUTER_BOUND('',#18929,.T.);
#12770=FACE_OUTER_BOUND('',#18930,.T.);
#12771=FACE_OUTER_BOUND('',#18931,.T.);
#12772=FACE_OUTER_BOUND('',#18932,.T.);
#12773=FACE_OUTER_BOUND('',#18933,.T.);
#12774=FACE_OUTER_BOUND('',#18934,.T.);
#12775=FACE_OUTER_BOUND('',#18935,.T.);
#12776=FACE_OUTER_BOUND('',#18936,.T.);
#12777=FACE_OUTER_BOUND('',#18937,.T.);
#12778=FACE_OUTER_BOUND('',#18938,.T.);
#12779=FACE_OUTER_BOUND('',#18939,.T.);
#12780=FACE_OUTER_BOUND('',#18940,.T.);
#12781=FACE_OUTER_BOUND('',#18941,.T.);
#12782=FACE_OUTER_BOUND('',#18942,.T.);
#12783=FACE_OUTER_BOUND('',#18943,.T.);
#12784=FACE_OUTER_BOUND('',#18944,.T.);
#12785=FACE_OUTER_BOUND('',#18945,.T.);
#12786=FACE_OUTER_BOUND('',#18946,.T.);
#12787=FACE_OUTER_BOUND('',#18947,.T.);
#12788=FACE_OUTER_BOUND('',#18948,.T.);
#12789=FACE_OUTER_BOUND('',#18949,.T.);
#12790=FACE_OUTER_BOUND('',#18950,.T.);
#12791=FACE_OUTER_BOUND('',#18951,.T.);
#12792=FACE_OUTER_BOUND('',#18952,.T.);
#12793=FACE_OUTER_BOUND('',#18953,.T.);
#12794=FACE_OUTER_BOUND('',#18954,.T.);
#12795=FACE_OUTER_BOUND('',#18955,.T.);
#12796=FACE_OUTER_BOUND('',#18956,.T.);
#12797=FACE_OUTER_BOUND('',#18957,.T.);
#12798=FACE_OUTER_BOUND('',#18958,.T.);
#12799=FACE_OUTER_BOUND('',#18959,.T.);
#12800=FACE_OUTER_BOUND('',#18960,.T.);
#12801=FACE_OUTER_BOUND('',#18961,.T.);
#12802=FACE_OUTER_BOUND('',#18962,.T.);
#12803=FACE_OUTER_BOUND('',#18963,.T.);
#12804=FACE_OUTER_BOUND('',#18964,.T.);
#12805=FACE_OUTER_BOUND('',#18965,.T.);
#12806=FACE_OUTER_BOUND('',#18966,.T.);
#12807=FACE_OUTER_BOUND('',#18967,.T.);
#12808=FACE_OUTER_BOUND('',#18968,.T.);
#12809=FACE_OUTER_BOUND('',#18969,.T.);
#12810=FACE_OUTER_BOUND('',#18970,.T.);
#12811=FACE_OUTER_BOUND('',#18971,.T.);
#12812=FACE_OUTER_BOUND('',#18972,.T.);
#12813=FACE_OUTER_BOUND('',#18973,.T.);
#12814=FACE_OUTER_BOUND('',#18974,.T.);
#12815=FACE_OUTER_BOUND('',#18975,.T.);
#12816=FACE_OUTER_BOUND('',#18976,.T.);
#12817=FACE_OUTER_BOUND('',#18977,.T.);
#12818=FACE_OUTER_BOUND('',#18978,.T.);
#12819=FACE_OUTER_BOUND('',#18979,.T.);
#12820=FACE_OUTER_BOUND('',#18980,.T.);
#12821=FACE_OUTER_BOUND('',#18981,.T.);
#12822=FACE_OUTER_BOUND('',#18982,.T.);
#12823=FACE_OUTER_BOUND('',#18983,.T.);
#12824=FACE_OUTER_BOUND('',#18984,.T.);
#12825=FACE_OUTER_BOUND('',#18985,.T.);
#12826=FACE_OUTER_BOUND('',#18986,.T.);
#12827=FACE_OUTER_BOUND('',#18987,.T.);
#12828=FACE_OUTER_BOUND('',#18988,.T.);
#12829=FACE_OUTER_BOUND('',#18989,.T.);
#12830=FACE_OUTER_BOUND('',#18990,.T.);
#12831=FACE_OUTER_BOUND('',#18991,.T.);
#12832=FACE_OUTER_BOUND('',#18992,.T.);
#12833=FACE_OUTER_BOUND('',#18993,.T.);
#12834=FACE_OUTER_BOUND('',#18994,.T.);
#12835=FACE_OUTER_BOUND('',#18995,.T.);
#12836=FACE_OUTER_BOUND('',#18996,.T.);
#12837=FACE_OUTER_BOUND('',#18997,.T.);
#12838=FACE_OUTER_BOUND('',#18998,.T.);
#12839=FACE_OUTER_BOUND('',#18999,.T.);
#12840=FACE_OUTER_BOUND('',#19000,.T.);
#12841=FACE_OUTER_BOUND('',#19001,.T.);
#12842=FACE_OUTER_BOUND('',#19002,.T.);
#12843=FACE_OUTER_BOUND('',#19003,.T.);
#12844=FACE_OUTER_BOUND('',#19004,.T.);
#12845=FACE_OUTER_BOUND('',#19005,.T.);
#12846=FACE_OUTER_BOUND('',#19006,.T.);
#12847=FACE_OUTER_BOUND('',#19007,.T.);
#12848=FACE_OUTER_BOUND('',#19009,.T.);
#12849=FACE_OUTER_BOUND('',#19011,.T.);
#12850=FACE_OUTER_BOUND('',#19013,.T.);
#12851=FACE_OUTER_BOUND('',#19014,.T.);
#12852=FACE_OUTER_BOUND('',#19015,.T.);
#12853=FACE_OUTER_BOUND('',#19016,.T.);
#12854=FACE_OUTER_BOUND('',#19017,.T.);
#12855=FACE_OUTER_BOUND('',#19019,.T.);
#12856=FACE_OUTER_BOUND('',#19021,.T.);
#12857=FACE_OUTER_BOUND('',#19022,.T.);
#12858=FACE_OUTER_BOUND('',#19023,.T.);
#12859=FACE_OUTER_BOUND('',#19024,.T.);
#12860=FACE_OUTER_BOUND('',#19025,.T.);
#12861=FACE_OUTER_BOUND('',#19026,.T.);
#12862=FACE_OUTER_BOUND('',#19027,.T.);
#12863=FACE_OUTER_BOUND('',#19028,.T.);
#12864=FACE_OUTER_BOUND('',#19029,.T.);
#12865=FACE_OUTER_BOUND('',#19030,.T.);
#12866=FACE_OUTER_BOUND('',#19031,.T.);
#12867=FACE_OUTER_BOUND('',#19032,.T.);
#12868=FACE_OUTER_BOUND('',#19033,.T.);
#12869=FACE_OUTER_BOUND('',#19034,.T.);
#12870=FACE_OUTER_BOUND('',#19035,.T.);
#12871=FACE_OUTER_BOUND('',#19036,.T.);
#12872=FACE_OUTER_BOUND('',#19037,.T.);
#12873=FACE_OUTER_BOUND('',#19038,.T.);
#12874=FACE_OUTER_BOUND('',#19039,.T.);
#12875=FACE_OUTER_BOUND('',#19040,.T.);
#12876=FACE_OUTER_BOUND('',#19041,.T.);
#12877=FACE_OUTER_BOUND('',#19042,.T.);
#12878=FACE_OUTER_BOUND('',#19043,.T.);
#12879=FACE_OUTER_BOUND('',#19044,.T.);
#12880=FACE_OUTER_BOUND('',#19045,.T.);
#12881=FACE_OUTER_BOUND('',#19046,.T.);
#12882=FACE_OUTER_BOUND('',#19047,.T.);
#12883=FACE_OUTER_BOUND('',#19048,.T.);
#12884=FACE_OUTER_BOUND('',#19049,.T.);
#12885=FACE_OUTER_BOUND('',#19050,.T.);
#12886=FACE_OUTER_BOUND('',#19051,.T.);
#12887=FACE_OUTER_BOUND('',#19052,.T.);
#12888=FACE_OUTER_BOUND('',#19053,.T.);
#12889=FACE_OUTER_BOUND('',#19054,.T.);
#12890=FACE_OUTER_BOUND('',#19055,.T.);
#12891=FACE_OUTER_BOUND('',#19056,.T.);
#12892=FACE_OUTER_BOUND('',#19058,.T.);
#12893=FACE_OUTER_BOUND('',#19059,.T.);
#12894=FACE_OUTER_BOUND('',#19060,.T.);
#12895=FACE_OUTER_BOUND('',#19061,.T.);
#12896=FACE_OUTER_BOUND('',#19062,.T.);
#12897=FACE_OUTER_BOUND('',#19063,.T.);
#12898=FACE_OUTER_BOUND('',#19064,.T.);
#12899=FACE_OUTER_BOUND('',#19065,.T.);
#12900=FACE_OUTER_BOUND('',#19066,.T.);
#12901=FACE_OUTER_BOUND('',#19068,.T.);
#12902=FACE_OUTER_BOUND('',#19069,.T.);
#12903=FACE_OUTER_BOUND('',#19071,.T.);
#12904=FACE_OUTER_BOUND('',#19072,.T.);
#12905=FACE_OUTER_BOUND('',#19074,.T.);
#12906=FACE_OUTER_BOUND('',#19076,.T.);
#12907=FACE_OUTER_BOUND('',#19077,.T.);
#12908=FACE_OUTER_BOUND('',#19078,.T.);
#12909=FACE_OUTER_BOUND('',#19079,.T.);
#12910=FACE_OUTER_BOUND('',#19080,.T.);
#12911=FACE_OUTER_BOUND('',#19081,.T.);
#12912=FACE_OUTER_BOUND('',#19082,.T.);
#12913=FACE_OUTER_BOUND('',#19083,.T.);
#12914=FACE_OUTER_BOUND('',#19084,.T.);
#12915=FACE_OUTER_BOUND('',#19085,.T.);
#12916=FACE_OUTER_BOUND('',#19086,.T.);
#12917=FACE_OUTER_BOUND('',#19087,.T.);
#12918=FACE_OUTER_BOUND('',#19093,.T.);
#12919=FACE_OUTER_BOUND('',#19095,.T.);
#12920=FACE_OUTER_BOUND('',#19097,.T.);
#12921=FACE_OUTER_BOUND('',#19098,.T.);
#12922=FACE_OUTER_BOUND('',#19099,.T.);
#12923=FACE_OUTER_BOUND('',#19100,.T.);
#12924=FACE_OUTER_BOUND('',#19101,.T.);
#12925=FACE_OUTER_BOUND('',#19102,.T.);
#12926=FACE_OUTER_BOUND('',#19103,.T.);
#12927=FACE_OUTER_BOUND('',#19104,.T.);
#12928=FACE_OUTER_BOUND('',#19105,.T.);
#12929=FACE_OUTER_BOUND('',#19106,.T.);
#12930=FACE_OUTER_BOUND('',#19107,.T.);
#12931=FACE_OUTER_BOUND('',#19108,.T.);
#12932=FACE_OUTER_BOUND('',#19109,.T.);
#12933=FACE_OUTER_BOUND('',#19110,.T.);
#12934=FACE_OUTER_BOUND('',#19111,.T.);
#12935=FACE_OUTER_BOUND('',#19112,.T.);
#12936=FACE_OUTER_BOUND('',#19113,.T.);
#12937=FACE_OUTER_BOUND('',#19114,.T.);
#12938=FACE_OUTER_BOUND('',#19115,.T.);
#12939=FACE_OUTER_BOUND('',#19116,.T.);
#12940=FACE_OUTER_BOUND('',#19117,.T.);
#12941=FACE_OUTER_BOUND('',#19118,.T.);
#12942=FACE_OUTER_BOUND('',#19119,.T.);
#12943=FACE_OUTER_BOUND('',#19120,.T.);
#12944=FACE_OUTER_BOUND('',#19121,.T.);
#12945=FACE_OUTER_BOUND('',#19122,.T.);
#12946=FACE_OUTER_BOUND('',#19123,.T.);
#12947=FACE_OUTER_BOUND('',#19124,.T.);
#12948=FACE_OUTER_BOUND('',#19125,.T.);
#12949=FACE_OUTER_BOUND('',#19126,.T.);
#12950=FACE_OUTER_BOUND('',#19127,.T.);
#12951=FACE_OUTER_BOUND('',#19128,.T.);
#12952=FACE_OUTER_BOUND('',#19129,.T.);
#12953=FACE_OUTER_BOUND('',#19130,.T.);
#12954=FACE_OUTER_BOUND('',#19131,.T.);
#12955=FACE_OUTER_BOUND('',#19132,.T.);
#12956=FACE_OUTER_BOUND('',#19133,.T.);
#12957=FACE_OUTER_BOUND('',#19134,.T.);
#12958=FACE_OUTER_BOUND('',#19135,.T.);
#12959=FACE_OUTER_BOUND('',#19136,.T.);
#12960=FACE_OUTER_BOUND('',#19137,.T.);
#12961=FACE_OUTER_BOUND('',#19138,.T.);
#12962=FACE_OUTER_BOUND('',#19139,.T.);
#12963=FACE_OUTER_BOUND('',#19140,.T.);
#12964=FACE_OUTER_BOUND('',#19141,.T.);
#12965=FACE_OUTER_BOUND('',#19142,.T.);
#12966=FACE_OUTER_BOUND('',#19143,.T.);
#12967=FACE_OUTER_BOUND('',#19144,.T.);
#12968=FACE_OUTER_BOUND('',#19145,.T.);
#12969=FACE_OUTER_BOUND('',#19146,.T.);
#12970=FACE_OUTER_BOUND('',#19147,.T.);
#12971=FACE_OUTER_BOUND('',#19148,.T.);
#12972=FACE_OUTER_BOUND('',#19149,.T.);
#12973=FACE_OUTER_BOUND('',#19150,.T.);
#12974=FACE_OUTER_BOUND('',#19151,.T.);
#12975=FACE_OUTER_BOUND('',#19152,.T.);
#12976=FACE_OUTER_BOUND('',#19153,.T.);
#12977=FACE_OUTER_BOUND('',#19154,.T.);
#12978=FACE_OUTER_BOUND('',#19155,.T.);
#12979=FACE_OUTER_BOUND('',#19156,.T.);
#12980=FACE_OUTER_BOUND('',#19157,.T.);
#12981=FACE_OUTER_BOUND('',#19158,.T.);
#12982=FACE_OUTER_BOUND('',#19159,.T.);
#12983=FACE_OUTER_BOUND('',#19160,.T.);
#12984=FACE_OUTER_BOUND('',#19161,.T.);
#12985=FACE_OUTER_BOUND('',#19162,.T.);
#12986=FACE_OUTER_BOUND('',#19163,.T.);
#12987=FACE_OUTER_BOUND('',#19164,.T.);
#12988=FACE_OUTER_BOUND('',#19165,.T.);
#12989=FACE_OUTER_BOUND('',#19166,.T.);
#12990=FACE_OUTER_BOUND('',#19167,.T.);
#12991=FACE_OUTER_BOUND('',#19168,.T.);
#12992=FACE_OUTER_BOUND('',#19169,.T.);
#12993=FACE_OUTER_BOUND('',#19170,.T.);
#12994=FACE_OUTER_BOUND('',#19171,.T.);
#12995=FACE_OUTER_BOUND('',#19172,.T.);
#12996=FACE_OUTER_BOUND('',#19173,.T.);
#12997=FACE_OUTER_BOUND('',#19174,.T.);
#12998=FACE_OUTER_BOUND('',#19175,.T.);
#12999=FACE_OUTER_BOUND('',#19176,.T.);
#13000=FACE_OUTER_BOUND('',#19177,.T.);
#13001=FACE_OUTER_BOUND('',#19178,.T.);
#13002=FACE_OUTER_BOUND('',#19179,.T.);
#13003=FACE_OUTER_BOUND('',#19180,.T.);
#13004=FACE_OUTER_BOUND('',#19181,.T.);
#13005=FACE_OUTER_BOUND('',#19182,.T.);
#13006=FACE_OUTER_BOUND('',#19183,.T.);
#13007=FACE_OUTER_BOUND('',#19184,.T.);
#13008=FACE_OUTER_BOUND('',#19185,.T.);
#13009=FACE_OUTER_BOUND('',#19186,.T.);
#13010=FACE_OUTER_BOUND('',#19187,.T.);
#13011=FACE_OUTER_BOUND('',#19188,.T.);
#13012=FACE_OUTER_BOUND('',#19189,.T.);
#13013=FACE_OUTER_BOUND('',#19190,.T.);
#13014=FACE_OUTER_BOUND('',#19191,.T.);
#13015=FACE_OUTER_BOUND('',#19192,.T.);
#13016=FACE_OUTER_BOUND('',#19193,.T.);
#13017=FACE_OUTER_BOUND('',#19194,.T.);
#13018=FACE_OUTER_BOUND('',#19195,.T.);
#13019=FACE_OUTER_BOUND('',#19196,.T.);
#13020=FACE_OUTER_BOUND('',#19197,.T.);
#13021=FACE_OUTER_BOUND('',#19198,.T.);
#13022=FACE_OUTER_BOUND('',#19199,.T.);
#13023=FACE_OUTER_BOUND('',#19200,.T.);
#13024=FACE_OUTER_BOUND('',#19201,.T.);
#13025=FACE_OUTER_BOUND('',#19202,.T.);
#13026=FACE_OUTER_BOUND('',#19203,.T.);
#13027=FACE_OUTER_BOUND('',#19204,.T.);
#13028=FACE_OUTER_BOUND('',#19205,.T.);
#13029=FACE_OUTER_BOUND('',#19206,.T.);
#13030=FACE_OUTER_BOUND('',#19207,.T.);
#13031=FACE_OUTER_BOUND('',#19208,.T.);
#13032=FACE_OUTER_BOUND('',#19209,.T.);
#13033=FACE_OUTER_BOUND('',#19210,.T.);
#13034=FACE_OUTER_BOUND('',#19211,.T.);
#13035=FACE_OUTER_BOUND('',#19212,.T.);
#13036=FACE_OUTER_BOUND('',#19213,.T.);
#13037=FACE_OUTER_BOUND('',#19214,.T.);
#13038=FACE_OUTER_BOUND('',#19215,.T.);
#13039=FACE_OUTER_BOUND('',#19217,.T.);
#13040=FACE_OUTER_BOUND('',#19218,.T.);
#13041=FACE_OUTER_BOUND('',#19219,.T.);
#13042=FACE_OUTER_BOUND('',#19220,.T.);
#13043=FACE_OUTER_BOUND('',#19221,.T.);
#13044=FACE_OUTER_BOUND('',#19223,.T.);
#13045=FACE_OUTER_BOUND('',#19225,.T.);
#13046=FACE_OUTER_BOUND('',#19227,.T.);
#13047=FACE_OUTER_BOUND('',#19229,.T.);
#13048=FACE_OUTER_BOUND('',#19230,.T.);
#13049=FACE_OUTER_BOUND('',#19231,.T.);
#13050=FACE_OUTER_BOUND('',#19232,.T.);
#13051=FACE_OUTER_BOUND('',#19233,.T.);
#13052=FACE_OUTER_BOUND('',#19234,.T.);
#13053=FACE_OUTER_BOUND('',#19235,.T.);
#13054=FACE_OUTER_BOUND('',#19236,.T.);
#13055=FACE_OUTER_BOUND('',#19237,.T.);
#13056=FACE_OUTER_BOUND('',#19238,.T.);
#13057=FACE_OUTER_BOUND('',#19239,.T.);
#13058=FACE_OUTER_BOUND('',#19240,.T.);
#13059=FACE_OUTER_BOUND('',#19242,.T.);
#13060=FACE_OUTER_BOUND('',#19244,.T.);
#13061=FACE_OUTER_BOUND('',#19246,.T.);
#13062=FACE_OUTER_BOUND('',#19248,.T.);
#13063=FACE_OUTER_BOUND('',#19250,.T.);
#13064=FACE_OUTER_BOUND('',#19251,.T.);
#13065=FACE_OUTER_BOUND('',#19252,.T.);
#13066=FACE_OUTER_BOUND('',#19253,.T.);
#13067=FACE_OUTER_BOUND('',#19254,.T.);
#13068=FACE_OUTER_BOUND('',#19255,.T.);
#13069=FACE_OUTER_BOUND('',#19256,.T.);
#13070=FACE_OUTER_BOUND('',#19257,.T.);
#13071=FACE_OUTER_BOUND('',#19258,.T.);
#13072=FACE_OUTER_BOUND('',#19259,.T.);
#13073=FACE_OUTER_BOUND('',#19260,.T.);
#13074=FACE_OUTER_BOUND('',#19261,.T.);
#13075=FACE_OUTER_BOUND('',#19262,.T.);
#13076=FACE_OUTER_BOUND('',#19263,.T.);
#13077=FACE_OUTER_BOUND('',#19264,.T.);
#13078=FACE_OUTER_BOUND('',#19265,.T.);
#13079=FACE_OUTER_BOUND('',#19266,.T.);
#13080=FACE_OUTER_BOUND('',#19267,.T.);
#13081=FACE_OUTER_BOUND('',#19268,.T.);
#13082=FACE_OUTER_BOUND('',#19270,.T.);
#13083=FACE_OUTER_BOUND('',#19271,.T.);
#13084=FACE_OUTER_BOUND('',#19272,.T.);
#13085=FACE_OUTER_BOUND('',#19273,.T.);
#13086=FACE_OUTER_BOUND('',#19274,.T.);
#13087=FACE_OUTER_BOUND('',#19275,.T.);
#13088=FACE_OUTER_BOUND('',#19276,.T.);
#13089=FACE_OUTER_BOUND('',#19277,.T.);
#13090=FACE_OUTER_BOUND('',#19278,.T.);
#13091=FACE_OUTER_BOUND('',#19279,.T.);
#13092=FACE_OUTER_BOUND('',#19280,.T.);
#13093=FACE_OUTER_BOUND('',#19281,.T.);
#13094=FACE_OUTER_BOUND('',#19282,.T.);
#13095=FACE_OUTER_BOUND('',#19283,.T.);
#13096=FACE_OUTER_BOUND('',#19284,.T.);
#13097=FACE_OUTER_BOUND('',#19285,.T.);
#13098=FACE_OUTER_BOUND('',#19286,.T.);
#13099=FACE_OUTER_BOUND('',#19287,.T.);
#13100=FACE_OUTER_BOUND('',#19288,.T.);
#13101=FACE_OUTER_BOUND('',#19289,.T.);
#13102=FACE_OUTER_BOUND('',#19290,.T.);
#13103=FACE_OUTER_BOUND('',#19291,.T.);
#13104=FACE_OUTER_BOUND('',#19292,.T.);
#13105=FACE_OUTER_BOUND('',#19293,.T.);
#13106=FACE_OUTER_BOUND('',#19294,.T.);
#13107=FACE_OUTER_BOUND('',#19295,.T.);
#13108=FACE_OUTER_BOUND('',#19296,.T.);
#13109=FACE_OUTER_BOUND('',#19297,.T.);
#13110=FACE_OUTER_BOUND('',#19298,.T.);
#13111=FACE_OUTER_BOUND('',#19299,.T.);
#13112=FACE_OUTER_BOUND('',#19300,.T.);
#13113=FACE_OUTER_BOUND('',#19301,.T.);
#13114=FACE_OUTER_BOUND('',#19302,.T.);
#13115=FACE_OUTER_BOUND('',#19303,.T.);
#13116=FACE_OUTER_BOUND('',#19304,.T.);
#13117=FACE_OUTER_BOUND('',#19306,.T.);
#13118=FACE_OUTER_BOUND('',#19307,.T.);
#13119=FACE_OUTER_BOUND('',#19308,.T.);
#13120=FACE_OUTER_BOUND('',#19309,.T.);
#13121=FACE_OUTER_BOUND('',#19310,.T.);
#13122=FACE_OUTER_BOUND('',#19311,.T.);
#13123=FACE_OUTER_BOUND('',#19312,.T.);
#13124=FACE_OUTER_BOUND('',#19313,.T.);
#13125=FACE_OUTER_BOUND('',#19314,.T.);
#13126=FACE_OUTER_BOUND('',#19315,.T.);
#13127=FACE_OUTER_BOUND('',#19316,.T.);
#13128=FACE_OUTER_BOUND('',#19317,.T.);
#13129=FACE_OUTER_BOUND('',#19318,.T.);
#13130=FACE_OUTER_BOUND('',#19319,.T.);
#13131=FACE_OUTER_BOUND('',#19320,.T.);
#13132=FACE_OUTER_BOUND('',#19321,.T.);
#13133=FACE_OUTER_BOUND('',#19322,.T.);
#13134=FACE_OUTER_BOUND('',#19323,.T.);
#13135=FACE_OUTER_BOUND('',#19324,.T.);
#13136=FACE_OUTER_BOUND('',#19325,.T.);
#13137=FACE_OUTER_BOUND('',#19326,.T.);
#13138=FACE_OUTER_BOUND('',#19328,.T.);
#13139=FACE_OUTER_BOUND('',#19329,.T.);
#13140=FACE_OUTER_BOUND('',#19330,.T.);
#13141=FACE_OUTER_BOUND('',#19332,.T.);
#13142=FACE_OUTER_BOUND('',#19334,.T.);
#13143=FACE_OUTER_BOUND('',#19336,.T.);
#13144=FACE_OUTER_BOUND('',#19337,.T.);
#13145=FACE_OUTER_BOUND('',#19338,.T.);
#13146=FACE_OUTER_BOUND('',#19339,.T.);
#13147=FACE_OUTER_BOUND('',#19340,.T.);
#13148=FACE_OUTER_BOUND('',#19341,.T.);
#13149=FACE_OUTER_BOUND('',#19342,.T.);
#13150=FACE_OUTER_BOUND('',#19343,.T.);
#13151=FACE_OUTER_BOUND('',#19344,.T.);
#13152=FACE_OUTER_BOUND('',#19345,.T.);
#13153=FACE_OUTER_BOUND('',#19346,.T.);
#13154=FACE_OUTER_BOUND('',#19347,.T.);
#13155=FACE_OUTER_BOUND('',#19348,.T.);
#13156=FACE_OUTER_BOUND('',#19349,.T.);
#13157=FACE_OUTER_BOUND('',#19350,.T.);
#13158=FACE_OUTER_BOUND('',#19351,.T.);
#13159=FACE_OUTER_BOUND('',#19352,.T.);
#13160=FACE_OUTER_BOUND('',#19353,.T.);
#13161=FACE_OUTER_BOUND('',#19354,.T.);
#13162=FACE_OUTER_BOUND('',#19355,.T.);
#13163=FACE_OUTER_BOUND('',#19356,.T.);
#13164=FACE_OUTER_BOUND('',#19357,.T.);
#13165=FACE_OUTER_BOUND('',#19358,.T.);
#13166=FACE_OUTER_BOUND('',#19359,.T.);
#13167=FACE_OUTER_BOUND('',#19365,.T.);
#13168=FACE_OUTER_BOUND('',#19367,.T.);
#13169=FACE_OUTER_BOUND('',#19369,.T.);
#13170=FACE_OUTER_BOUND('',#19371,.T.);
#13171=FACE_OUTER_BOUND('',#19373,.T.);
#13172=FACE_OUTER_BOUND('',#19375,.T.);
#13173=FACE_OUTER_BOUND('',#19376,.T.);
#13174=FACE_OUTER_BOUND('',#19377,.T.);
#13175=FACE_OUTER_BOUND('',#19378,.T.);
#13176=FACE_OUTER_BOUND('',#19379,.T.);
#13177=FACE_OUTER_BOUND('',#19380,.T.);
#13178=FACE_OUTER_BOUND('',#19381,.T.);
#13179=FACE_OUTER_BOUND('',#19382,.T.);
#13180=FACE_OUTER_BOUND('',#19383,.T.);
#13181=FACE_OUTER_BOUND('',#19384,.T.);
#13182=FACE_OUTER_BOUND('',#19385,.T.);
#13183=FACE_OUTER_BOUND('',#19386,.T.);
#13184=FACE_OUTER_BOUND('',#19387,.T.);
#13185=FACE_OUTER_BOUND('',#19388,.T.);
#13186=FACE_OUTER_BOUND('',#19389,.T.);
#13187=FACE_OUTER_BOUND('',#19390,.T.);
#13188=FACE_OUTER_BOUND('',#19391,.T.);
#13189=FACE_OUTER_BOUND('',#19397,.T.);
#13190=FACE_OUTER_BOUND('',#19398,.T.);
#13191=FACE_OUTER_BOUND('',#19400,.T.);
#13192=FACE_OUTER_BOUND('',#19402,.T.);
#13193=FACE_OUTER_BOUND('',#19404,.T.);
#13194=FACE_OUTER_BOUND('',#19406,.T.);
#13195=FACE_OUTER_BOUND('',#19407,.T.);
#13196=FACE_OUTER_BOUND('',#19408,.T.);
#13197=FACE_OUTER_BOUND('',#19409,.T.);
#13198=FACE_OUTER_BOUND('',#19411,.T.);
#13199=FACE_OUTER_BOUND('',#19412,.T.);
#13200=FACE_OUTER_BOUND('',#19413,.T.);
#13201=FACE_OUTER_BOUND('',#19414,.T.);
#13202=FACE_OUTER_BOUND('',#19415,.T.);
#13203=FACE_OUTER_BOUND('',#19416,.T.);
#13204=FACE_OUTER_BOUND('',#19417,.T.);
#13205=FACE_OUTER_BOUND('',#19418,.T.);
#13206=FACE_OUTER_BOUND('',#19419,.T.);
#13207=FACE_OUTER_BOUND('',#19420,.T.);
#13208=FACE_OUTER_BOUND('',#19421,.T.);
#13209=FACE_OUTER_BOUND('',#19422,.T.);
#13210=FACE_OUTER_BOUND('',#19423,.T.);
#13211=FACE_OUTER_BOUND('',#19424,.T.);
#13212=FACE_OUTER_BOUND('',#19425,.T.);
#13213=FACE_OUTER_BOUND('',#19426,.T.);
#13214=FACE_OUTER_BOUND('',#19427,.T.);
#13215=FACE_OUTER_BOUND('',#19428,.T.);
#13216=FACE_OUTER_BOUND('',#19430,.T.);
#13217=FACE_OUTER_BOUND('',#19432,.T.);
#13218=FACE_OUTER_BOUND('',#19434,.T.);
#13219=FACE_OUTER_BOUND('',#19436,.T.);
#13220=FACE_OUTER_BOUND('',#19439,.T.);
#13221=FACE_OUTER_BOUND('',#19442,.T.);
#13222=FACE_OUTER_BOUND('',#19445,.T.);
#13223=FACE_OUTER_BOUND('',#19446,.T.);
#13224=FACE_OUTER_BOUND('',#19447,.T.);
#13225=FACE_OUTER_BOUND('',#19448,.T.);
#13226=FACE_OUTER_BOUND('',#19449,.T.);
#13227=FACE_OUTER_BOUND('',#19451,.T.);
#13228=FACE_OUTER_BOUND('',#19452,.T.);
#13229=FACE_OUTER_BOUND('',#19453,.T.);
#13230=FACE_OUTER_BOUND('',#19454,.T.);
#13231=FACE_OUTER_BOUND('',#19455,.T.);
#13232=FACE_OUTER_BOUND('',#19456,.T.);
#13233=FACE_OUTER_BOUND('',#19457,.T.);
#13234=FACE_OUTER_BOUND('',#19458,.T.);
#13235=FACE_OUTER_BOUND('',#19459,.T.);
#13236=FACE_OUTER_BOUND('',#19460,.T.);
#13237=FACE_OUTER_BOUND('',#19461,.T.);
#13238=FACE_OUTER_BOUND('',#19462,.T.);
#13239=FACE_OUTER_BOUND('',#19463,.T.);
#13240=FACE_OUTER_BOUND('',#19464,.T.);
#13241=FACE_OUTER_BOUND('',#19465,.T.);
#13242=FACE_OUTER_BOUND('',#19466,.T.);
#13243=FACE_OUTER_BOUND('',#19467,.T.);
#13244=FACE_OUTER_BOUND('',#19469,.T.);
#13245=FACE_OUTER_BOUND('',#19470,.T.);
#13246=FACE_OUTER_BOUND('',#19471,.T.);
#13247=FACE_OUTER_BOUND('',#19472,.T.);
#13248=FACE_OUTER_BOUND('',#19473,.T.);
#13249=FACE_OUTER_BOUND('',#19475,.T.);
#13250=FACE_OUTER_BOUND('',#19476,.T.);
#13251=FACE_OUTER_BOUND('',#19477,.T.);
#13252=FACE_OUTER_BOUND('',#19479,.T.);
#13253=FACE_OUTER_BOUND('',#19480,.T.);
#13254=FACE_OUTER_BOUND('',#19481,.T.);
#13255=FACE_OUTER_BOUND('',#19483,.T.);
#13256=FACE_OUTER_BOUND('',#19484,.T.);
#13257=FACE_OUTER_BOUND('',#19485,.T.);
#13258=FACE_OUTER_BOUND('',#19487,.T.);
#13259=FACE_OUTER_BOUND('',#19488,.T.);
#13260=FACE_OUTER_BOUND('',#19489,.T.);
#13261=FACE_OUTER_BOUND('',#19491,.T.);
#13262=FACE_OUTER_BOUND('',#19492,.T.);
#13263=FACE_OUTER_BOUND('',#19493,.T.);
#13264=FACE_OUTER_BOUND('',#19494,.T.);
#13265=FACE_OUTER_BOUND('',#19495,.T.);
#13266=FACE_OUTER_BOUND('',#19496,.T.);
#13267=FACE_OUTER_BOUND('',#19497,.T.);
#13268=FACE_OUTER_BOUND('',#19498,.T.);
#13269=FACE_OUTER_BOUND('',#19500,.T.);
#13270=FACE_OUTER_BOUND('',#19501,.T.);
#13271=FACE_OUTER_BOUND('',#19502,.T.);
#13272=FACE_OUTER_BOUND('',#19503,.T.);
#13273=FACE_OUTER_BOUND('',#19504,.T.);
#13274=FACE_OUTER_BOUND('',#19505,.T.);
#13275=FACE_OUTER_BOUND('',#19506,.T.);
#13276=FACE_OUTER_BOUND('',#19507,.T.);
#13277=FACE_OUTER_BOUND('',#19508,.T.);
#13278=FACE_OUTER_BOUND('',#19509,.T.);
#13279=FACE_OUTER_BOUND('',#19510,.T.);
#13280=FACE_OUTER_BOUND('',#19511,.T.);
#13281=FACE_OUTER_BOUND('',#19512,.T.);
#13282=FACE_OUTER_BOUND('',#19513,.T.);
#13283=FACE_OUTER_BOUND('',#19514,.T.);
#13284=FACE_OUTER_BOUND('',#19515,.T.);
#13285=FACE_OUTER_BOUND('',#19516,.T.);
#13286=FACE_OUTER_BOUND('',#19517,.T.);
#13287=FACE_OUTER_BOUND('',#19518,.T.);
#13288=FACE_OUTER_BOUND('',#19519,.T.);
#13289=FACE_OUTER_BOUND('',#19520,.T.);
#13290=FACE_OUTER_BOUND('',#19521,.T.);
#13291=FACE_OUTER_BOUND('',#19522,.T.);
#13292=FACE_OUTER_BOUND('',#19523,.T.);
#13293=FACE_OUTER_BOUND('',#19524,.T.);
#13294=FACE_OUTER_BOUND('',#19525,.T.);
#13295=FACE_OUTER_BOUND('',#19526,.T.);
#13296=FACE_OUTER_BOUND('',#19527,.T.);
#13297=FACE_OUTER_BOUND('',#19528,.T.);
#13298=FACE_OUTER_BOUND('',#19529,.T.);
#13299=FACE_OUTER_BOUND('',#19530,.T.);
#13300=FACE_OUTER_BOUND('',#19531,.T.);
#13301=FACE_OUTER_BOUND('',#19532,.T.);
#13302=FACE_OUTER_BOUND('',#19533,.T.);
#13303=FACE_OUTER_BOUND('',#19534,.T.);
#13304=FACE_OUTER_BOUND('',#19535,.T.);
#13305=FACE_OUTER_BOUND('',#19536,.T.);
#13306=FACE_OUTER_BOUND('',#19537,.T.);
#13307=FACE_OUTER_BOUND('',#19538,.T.);
#13308=FACE_OUTER_BOUND('',#19539,.T.);
#13309=FACE_OUTER_BOUND('',#19540,.T.);
#13310=FACE_OUTER_BOUND('',#19541,.T.);
#13311=FACE_OUTER_BOUND('',#19542,.T.);
#13312=FACE_OUTER_BOUND('',#19543,.T.);
#13313=FACE_OUTER_BOUND('',#19544,.T.);
#13314=FACE_OUTER_BOUND('',#19545,.T.);
#13315=FACE_OUTER_BOUND('',#19547,.T.);
#13316=FACE_OUTER_BOUND('',#19548,.T.);
#13317=FACE_OUTER_BOUND('',#19549,.T.);
#13318=FACE_OUTER_BOUND('',#19550,.T.);
#13319=FACE_OUTER_BOUND('',#19551,.T.);
#13320=FACE_OUTER_BOUND('',#19552,.T.);
#13321=FACE_OUTER_BOUND('',#19553,.T.);
#13322=FACE_OUTER_BOUND('',#19554,.T.);
#13323=FACE_OUTER_BOUND('',#19555,.T.);
#13324=FACE_OUTER_BOUND('',#19556,.T.);
#13325=FACE_OUTER_BOUND('',#19557,.T.);
#13326=FACE_OUTER_BOUND('',#19558,.T.);
#13327=FACE_OUTER_BOUND('',#19559,.T.);
#13328=FACE_OUTER_BOUND('',#19560,.T.);
#13329=FACE_OUTER_BOUND('',#19561,.T.);
#13330=FACE_OUTER_BOUND('',#19562,.T.);
#13331=FACE_OUTER_BOUND('',#19563,.T.);
#13332=FACE_OUTER_BOUND('',#19564,.T.);
#13333=FACE_OUTER_BOUND('',#19565,.T.);
#13334=FACE_OUTER_BOUND('',#19566,.T.);
#13335=FACE_OUTER_BOUND('',#19567,.T.);
#13336=FACE_OUTER_BOUND('',#19568,.T.);
#13337=FACE_OUTER_BOUND('',#19569,.T.);
#13338=FACE_OUTER_BOUND('',#19570,.T.);
#13339=FACE_OUTER_BOUND('',#19571,.T.);
#13340=FACE_OUTER_BOUND('',#19572,.T.);
#13341=FACE_OUTER_BOUND('',#19573,.T.);
#13342=FACE_OUTER_BOUND('',#19574,.T.);
#13343=FACE_OUTER_BOUND('',#19575,.T.);
#13344=FACE_OUTER_BOUND('',#19576,.T.);
#13345=FACE_OUTER_BOUND('',#19577,.T.);
#13346=FACE_OUTER_BOUND('',#19578,.T.);
#13347=FACE_OUTER_BOUND('',#19579,.T.);
#13348=FACE_OUTER_BOUND('',#19580,.T.);
#13349=FACE_OUTER_BOUND('',#19581,.T.);
#13350=FACE_OUTER_BOUND('',#19582,.T.);
#13351=FACE_OUTER_BOUND('',#19583,.T.);
#13352=FACE_OUTER_BOUND('',#19584,.T.);
#13353=FACE_OUTER_BOUND('',#19585,.T.);
#13354=FACE_OUTER_BOUND('',#19586,.T.);
#13355=FACE_OUTER_BOUND('',#19587,.T.);
#13356=FACE_OUTER_BOUND('',#19588,.T.);
#13357=FACE_OUTER_BOUND('',#19589,.T.);
#13358=FACE_OUTER_BOUND('',#19590,.T.);
#13359=FACE_OUTER_BOUND('',#19591,.T.);
#13360=FACE_OUTER_BOUND('',#19592,.T.);
#13361=FACE_OUTER_BOUND('',#19593,.T.);
#13362=FACE_OUTER_BOUND('',#19594,.T.);
#13363=FACE_OUTER_BOUND('',#19595,.T.);
#13364=FACE_OUTER_BOUND('',#19596,.T.);
#13365=FACE_OUTER_BOUND('',#19597,.T.);
#13366=FACE_OUTER_BOUND('',#19598,.T.);
#13367=FACE_OUTER_BOUND('',#19599,.T.);
#13368=FACE_OUTER_BOUND('',#19600,.T.);
#13369=FACE_OUTER_BOUND('',#19601,.T.);
#13370=FACE_OUTER_BOUND('',#19602,.T.);
#13371=FACE_OUTER_BOUND('',#19603,.T.);
#13372=FACE_OUTER_BOUND('',#19604,.T.);
#13373=FACE_OUTER_BOUND('',#19605,.T.);
#13374=FACE_OUTER_BOUND('',#19606,.T.);
#13375=FACE_OUTER_BOUND('',#19607,.T.);
#13376=FACE_OUTER_BOUND('',#19608,.T.);
#13377=FACE_OUTER_BOUND('',#19609,.T.);
#13378=FACE_OUTER_BOUND('',#19610,.T.);
#13379=FACE_OUTER_BOUND('',#19611,.T.);
#13380=FACE_OUTER_BOUND('',#19612,.T.);
#13381=FACE_OUTER_BOUND('',#19613,.T.);
#13382=FACE_OUTER_BOUND('',#19614,.T.);
#13383=FACE_OUTER_BOUND('',#19615,.T.);
#13384=FACE_OUTER_BOUND('',#19616,.T.);
#13385=FACE_OUTER_BOUND('',#19617,.T.);
#13386=FACE_OUTER_BOUND('',#19618,.T.);
#13387=FACE_OUTER_BOUND('',#19619,.T.);
#13388=FACE_OUTER_BOUND('',#19620,.T.);
#13389=FACE_OUTER_BOUND('',#19621,.T.);
#13390=FACE_OUTER_BOUND('',#19622,.T.);
#13391=FACE_OUTER_BOUND('',#19623,.T.);
#13392=FACE_OUTER_BOUND('',#19624,.T.);
#13393=FACE_OUTER_BOUND('',#19625,.T.);
#13394=FACE_OUTER_BOUND('',#19626,.T.);
#13395=FACE_OUTER_BOUND('',#19627,.T.);
#13396=FACE_OUTER_BOUND('',#19628,.T.);
#13397=FACE_OUTER_BOUND('',#19629,.T.);
#13398=FACE_OUTER_BOUND('',#19630,.T.);
#13399=FACE_OUTER_BOUND('',#19631,.T.);
#13400=FACE_OUTER_BOUND('',#19632,.T.);
#13401=FACE_OUTER_BOUND('',#19633,.T.);
#13402=FACE_OUTER_BOUND('',#19634,.T.);
#13403=FACE_OUTER_BOUND('',#19635,.T.);
#13404=FACE_OUTER_BOUND('',#19636,.T.);
#13405=FACE_OUTER_BOUND('',#19637,.T.);
#13406=FACE_OUTER_BOUND('',#19638,.T.);
#13407=FACE_OUTER_BOUND('',#19639,.T.);
#13408=FACE_OUTER_BOUND('',#19640,.T.);
#13409=FACE_OUTER_BOUND('',#19641,.T.);
#13410=FACE_OUTER_BOUND('',#19642,.T.);
#13411=FACE_OUTER_BOUND('',#19643,.T.);
#13412=FACE_OUTER_BOUND('',#19644,.T.);
#13413=FACE_OUTER_BOUND('',#19645,.T.);
#13414=FACE_OUTER_BOUND('',#19646,.T.);
#13415=FACE_OUTER_BOUND('',#19647,.T.);
#13416=FACE_OUTER_BOUND('',#19648,.T.);
#13417=FACE_OUTER_BOUND('',#19649,.T.);
#13418=FACE_OUTER_BOUND('',#19650,.T.);
#13419=FACE_OUTER_BOUND('',#19651,.T.);
#13420=FACE_OUTER_BOUND('',#19652,.T.);
#13421=FACE_OUTER_BOUND('',#19653,.T.);
#13422=FACE_OUTER_BOUND('',#19654,.T.);
#13423=FACE_OUTER_BOUND('',#19655,.T.);
#13424=FACE_OUTER_BOUND('',#19656,.T.);
#13425=FACE_OUTER_BOUND('',#19657,.T.);
#13426=FACE_OUTER_BOUND('',#19658,.T.);
#13427=FACE_OUTER_BOUND('',#19659,.T.);
#13428=FACE_OUTER_BOUND('',#19660,.T.);
#13429=FACE_OUTER_BOUND('',#19661,.T.);
#13430=FACE_OUTER_BOUND('',#19662,.T.);
#13431=FACE_OUTER_BOUND('',#19663,.T.);
#13432=FACE_OUTER_BOUND('',#19664,.T.);
#13433=FACE_OUTER_BOUND('',#19665,.T.);
#13434=FACE_OUTER_BOUND('',#19666,.T.);
#13435=FACE_OUTER_BOUND('',#19667,.T.);
#13436=FACE_OUTER_BOUND('',#19668,.T.);
#13437=FACE_OUTER_BOUND('',#19669,.T.);
#13438=FACE_OUTER_BOUND('',#19670,.T.);
#13439=FACE_OUTER_BOUND('',#19671,.T.);
#13440=FACE_OUTER_BOUND('',#19672,.T.);
#13441=FACE_OUTER_BOUND('',#19673,.T.);
#13442=FACE_OUTER_BOUND('',#19674,.T.);
#13443=FACE_OUTER_BOUND('',#19675,.T.);
#13444=FACE_OUTER_BOUND('',#19676,.T.);
#13445=FACE_OUTER_BOUND('',#19677,.T.);
#13446=FACE_OUTER_BOUND('',#19678,.T.);
#13447=FACE_OUTER_BOUND('',#19679,.T.);
#13448=FACE_OUTER_BOUND('',#19680,.T.);
#13449=FACE_OUTER_BOUND('',#19681,.T.);
#13450=FACE_OUTER_BOUND('',#19682,.T.);
#13451=FACE_OUTER_BOUND('',#19683,.T.);
#13452=FACE_OUTER_BOUND('',#19684,.T.);
#13453=FACE_OUTER_BOUND('',#19685,.T.);
#13454=FACE_OUTER_BOUND('',#19686,.T.);
#13455=FACE_OUTER_BOUND('',#19687,.T.);
#13456=FACE_OUTER_BOUND('',#19688,.T.);
#13457=FACE_OUTER_BOUND('',#19689,.T.);
#13458=FACE_OUTER_BOUND('',#19690,.T.);
#13459=FACE_OUTER_BOUND('',#19691,.T.);
#13460=FACE_OUTER_BOUND('',#19692,.T.);
#13461=FACE_OUTER_BOUND('',#19693,.T.);
#13462=FACE_OUTER_BOUND('',#19694,.T.);
#13463=FACE_OUTER_BOUND('',#19695,.T.);
#13464=FACE_OUTER_BOUND('',#19696,.T.);
#13465=FACE_OUTER_BOUND('',#19697,.T.);
#13466=FACE_OUTER_BOUND('',#19698,.T.);
#13467=FACE_OUTER_BOUND('',#19699,.T.);
#13468=FACE_OUTER_BOUND('',#19700,.T.);
#13469=FACE_OUTER_BOUND('',#19701,.T.);
#13470=FACE_OUTER_BOUND('',#19702,.T.);
#13471=FACE_OUTER_BOUND('',#19703,.T.);
#13472=FACE_OUTER_BOUND('',#19704,.T.);
#13473=FACE_OUTER_BOUND('',#19705,.T.);
#13474=FACE_OUTER_BOUND('',#19706,.T.);
#13475=FACE_OUTER_BOUND('',#19707,.T.);
#13476=FACE_OUTER_BOUND('',#19708,.T.);
#13477=FACE_OUTER_BOUND('',#19709,.T.);
#13478=FACE_OUTER_BOUND('',#19710,.T.);
#13479=FACE_OUTER_BOUND('',#19711,.T.);
#13480=FACE_OUTER_BOUND('',#19712,.T.);
#13481=FACE_OUTER_BOUND('',#19713,.T.);
#13482=FACE_OUTER_BOUND('',#19714,.T.);
#13483=FACE_OUTER_BOUND('',#19715,.T.);
#13484=FACE_OUTER_BOUND('',#19716,.T.);
#13485=FACE_OUTER_BOUND('',#19717,.T.);
#13486=FACE_OUTER_BOUND('',#19718,.T.);
#13487=FACE_OUTER_BOUND('',#19719,.T.);
#13488=FACE_OUTER_BOUND('',#19720,.T.);
#13489=FACE_OUTER_BOUND('',#19721,.T.);
#13490=FACE_OUTER_BOUND('',#19722,.T.);
#13491=FACE_OUTER_BOUND('',#19723,.T.);
#13492=FACE_OUTER_BOUND('',#19724,.T.);
#13493=FACE_OUTER_BOUND('',#19725,.T.);
#13494=FACE_OUTER_BOUND('',#19726,.T.);
#13495=FACE_OUTER_BOUND('',#19727,.T.);
#13496=FACE_OUTER_BOUND('',#19728,.T.);
#13497=FACE_OUTER_BOUND('',#19729,.T.);
#13498=FACE_OUTER_BOUND('',#19730,.T.);
#13499=FACE_OUTER_BOUND('',#19731,.T.);
#13500=FACE_OUTER_BOUND('',#19732,.T.);
#13501=FACE_OUTER_BOUND('',#19733,.T.);
#13502=FACE_OUTER_BOUND('',#19734,.T.);
#13503=FACE_OUTER_BOUND('',#19735,.T.);
#13504=FACE_OUTER_BOUND('',#19736,.T.);
#13505=FACE_OUTER_BOUND('',#19737,.T.);
#13506=FACE_OUTER_BOUND('',#19738,.T.);
#13507=FACE_OUTER_BOUND('',#19739,.T.);
#13508=FACE_OUTER_BOUND('',#19740,.T.);
#13509=FACE_OUTER_BOUND('',#19741,.T.);
#13510=FACE_OUTER_BOUND('',#19742,.T.);
#13511=FACE_OUTER_BOUND('',#19743,.T.);
#13512=FACE_OUTER_BOUND('',#19744,.T.);
#13513=FACE_OUTER_BOUND('',#19745,.T.);
#13514=FACE_OUTER_BOUND('',#19746,.T.);
#13515=FACE_OUTER_BOUND('',#19747,.T.);
#13516=FACE_OUTER_BOUND('',#19748,.T.);
#13517=FACE_OUTER_BOUND('',#19749,.T.);
#13518=FACE_OUTER_BOUND('',#19750,.T.);
#13519=FACE_OUTER_BOUND('',#19751,.T.);
#13520=FACE_OUTER_BOUND('',#19752,.T.);
#13521=FACE_OUTER_BOUND('',#19753,.T.);
#13522=FACE_OUTER_BOUND('',#19754,.T.);
#13523=FACE_OUTER_BOUND('',#19755,.T.);
#13524=FACE_OUTER_BOUND('',#19756,.T.);
#13525=FACE_OUTER_BOUND('',#19757,.T.);
#13526=FACE_OUTER_BOUND('',#19758,.T.);
#13527=FACE_OUTER_BOUND('',#19759,.T.);
#13528=FACE_OUTER_BOUND('',#19760,.T.);
#13529=FACE_OUTER_BOUND('',#19761,.T.);
#13530=FACE_OUTER_BOUND('',#19762,.T.);
#13531=FACE_OUTER_BOUND('',#19763,.T.);
#13532=FACE_OUTER_BOUND('',#19764,.T.);
#13533=FACE_OUTER_BOUND('',#19765,.T.);
#13534=FACE_OUTER_BOUND('',#19766,.T.);
#13535=FACE_OUTER_BOUND('',#19767,.T.);
#13536=FACE_OUTER_BOUND('',#19768,.T.);
#13537=FACE_OUTER_BOUND('',#19769,.T.);
#13538=FACE_OUTER_BOUND('',#19770,.T.);
#13539=FACE_OUTER_BOUND('',#19771,.T.);
#13540=FACE_OUTER_BOUND('',#19772,.T.);
#13541=FACE_OUTER_BOUND('',#19773,.T.);
#13542=FACE_OUTER_BOUND('',#19774,.T.);
#13543=FACE_OUTER_BOUND('',#19775,.T.);
#13544=FACE_OUTER_BOUND('',#19776,.T.);
#13545=FACE_OUTER_BOUND('',#19777,.T.);
#13546=FACE_OUTER_BOUND('',#19778,.T.);
#13547=FACE_OUTER_BOUND('',#19779,.T.);
#13548=FACE_OUTER_BOUND('',#19780,.T.);
#13549=FACE_OUTER_BOUND('',#19781,.T.);
#13550=FACE_OUTER_BOUND('',#19782,.T.);
#13551=FACE_OUTER_BOUND('',#19783,.T.);
#13552=FACE_OUTER_BOUND('',#19784,.T.);
#13553=FACE_OUTER_BOUND('',#19785,.T.);
#13554=FACE_OUTER_BOUND('',#19786,.T.);
#13555=FACE_OUTER_BOUND('',#19787,.T.);
#13556=FACE_OUTER_BOUND('',#19788,.T.);
#13557=FACE_OUTER_BOUND('',#19789,.T.);
#13558=FACE_OUTER_BOUND('',#19790,.T.);
#13559=FACE_OUTER_BOUND('',#19791,.T.);
#13560=FACE_OUTER_BOUND('',#19792,.T.);
#13561=FACE_OUTER_BOUND('',#19793,.T.);
#13562=FACE_OUTER_BOUND('',#19794,.T.);
#13563=FACE_OUTER_BOUND('',#19795,.T.);
#13564=FACE_OUTER_BOUND('',#19796,.T.);
#13565=FACE_OUTER_BOUND('',#19797,.T.);
#13566=FACE_OUTER_BOUND('',#19798,.T.);
#13567=FACE_OUTER_BOUND('',#19799,.T.);
#13568=FACE_OUTER_BOUND('',#19800,.T.);
#13569=FACE_OUTER_BOUND('',#19801,.T.);
#13570=FACE_OUTER_BOUND('',#19802,.T.);
#13571=FACE_OUTER_BOUND('',#19803,.T.);
#13572=FACE_OUTER_BOUND('',#19804,.T.);
#13573=FACE_OUTER_BOUND('',#19805,.T.);
#13574=FACE_OUTER_BOUND('',#19806,.T.);
#13575=FACE_OUTER_BOUND('',#19807,.T.);
#13576=FACE_OUTER_BOUND('',#19808,.T.);
#13577=FACE_OUTER_BOUND('',#19809,.T.);
#13578=FACE_OUTER_BOUND('',#19810,.T.);
#13579=FACE_OUTER_BOUND('',#19811,.T.);
#13580=FACE_OUTER_BOUND('',#19812,.T.);
#13581=FACE_OUTER_BOUND('',#19813,.T.);
#13582=FACE_OUTER_BOUND('',#19814,.T.);
#13583=FACE_OUTER_BOUND('',#19815,.T.);
#13584=FACE_OUTER_BOUND('',#19816,.T.);
#13585=FACE_OUTER_BOUND('',#19817,.T.);
#13586=FACE_OUTER_BOUND('',#19818,.T.);
#13587=FACE_OUTER_BOUND('',#19819,.T.);
#13588=FACE_OUTER_BOUND('',#19820,.T.);
#13589=FACE_OUTER_BOUND('',#19821,.T.);
#13590=FACE_OUTER_BOUND('',#19822,.T.);
#13591=FACE_OUTER_BOUND('',#19823,.T.);
#13592=FACE_OUTER_BOUND('',#19824,.T.);
#13593=FACE_OUTER_BOUND('',#19825,.T.);
#13594=FACE_OUTER_BOUND('',#19826,.T.);
#13595=FACE_OUTER_BOUND('',#19827,.T.);
#13596=FACE_OUTER_BOUND('',#19828,.T.);
#13597=FACE_OUTER_BOUND('',#19829,.T.);
#13598=FACE_OUTER_BOUND('',#19830,.T.);
#13599=FACE_OUTER_BOUND('',#19831,.T.);
#13600=FACE_OUTER_BOUND('',#19832,.T.);
#13601=FACE_OUTER_BOUND('',#19833,.T.);
#13602=FACE_OUTER_BOUND('',#19834,.T.);
#13603=FACE_OUTER_BOUND('',#19835,.T.);
#13604=FACE_OUTER_BOUND('',#19836,.T.);
#13605=FACE_OUTER_BOUND('',#19837,.T.);
#13606=FACE_OUTER_BOUND('',#19838,.T.);
#13607=FACE_OUTER_BOUND('',#19839,.T.);
#13608=FACE_OUTER_BOUND('',#19840,.T.);
#13609=FACE_OUTER_BOUND('',#19841,.T.);
#13610=FACE_OUTER_BOUND('',#19842,.T.);
#13611=FACE_OUTER_BOUND('',#19843,.T.);
#13612=FACE_OUTER_BOUND('',#19844,.T.);
#13613=FACE_OUTER_BOUND('',#19845,.T.);
#13614=FACE_OUTER_BOUND('',#19846,.T.);
#13615=FACE_OUTER_BOUND('',#19847,.T.);
#13616=FACE_OUTER_BOUND('',#19848,.T.);
#13617=FACE_OUTER_BOUND('',#19849,.T.);
#13618=FACE_OUTER_BOUND('',#19850,.T.);
#13619=FACE_OUTER_BOUND('',#19851,.T.);
#13620=FACE_OUTER_BOUND('',#19852,.T.);
#13621=FACE_OUTER_BOUND('',#19853,.T.);
#13622=FACE_OUTER_BOUND('',#19854,.T.);
#13623=FACE_OUTER_BOUND('',#19855,.T.);
#13624=FACE_OUTER_BOUND('',#19856,.T.);
#13625=FACE_OUTER_BOUND('',#19857,.T.);
#13626=FACE_OUTER_BOUND('',#19858,.T.);
#13627=FACE_OUTER_BOUND('',#19859,.T.);
#13628=FACE_OUTER_BOUND('',#19860,.T.);
#13629=FACE_OUTER_BOUND('',#19861,.T.);
#13630=FACE_OUTER_BOUND('',#19862,.T.);
#13631=FACE_OUTER_BOUND('',#19863,.T.);
#13632=FACE_OUTER_BOUND('',#19864,.T.);
#13633=FACE_OUTER_BOUND('',#19865,.T.);
#13634=FACE_OUTER_BOUND('',#19866,.T.);
#13635=FACE_OUTER_BOUND('',#19867,.T.);
#13636=FACE_OUTER_BOUND('',#19868,.T.);
#13637=FACE_OUTER_BOUND('',#19869,.T.);
#13638=FACE_OUTER_BOUND('',#19870,.T.);
#13639=FACE_OUTER_BOUND('',#19871,.T.);
#13640=FACE_OUTER_BOUND('',#19872,.T.);
#13641=FACE_OUTER_BOUND('',#19873,.T.);
#13642=FACE_OUTER_BOUND('',#19874,.T.);
#13643=FACE_OUTER_BOUND('',#19875,.T.);
#13644=FACE_OUTER_BOUND('',#19876,.T.);
#13645=FACE_OUTER_BOUND('',#19877,.T.);
#13646=FACE_OUTER_BOUND('',#19878,.T.);
#13647=FACE_OUTER_BOUND('',#19879,.T.);
#13648=FACE_OUTER_BOUND('',#19880,.T.);
#13649=FACE_OUTER_BOUND('',#19881,.T.);
#13650=FACE_OUTER_BOUND('',#19882,.T.);
#13651=FACE_OUTER_BOUND('',#19883,.T.);
#13652=FACE_OUTER_BOUND('',#19884,.T.);
#13653=FACE_OUTER_BOUND('',#19885,.T.);
#13654=FACE_OUTER_BOUND('',#19886,.T.);
#13655=FACE_OUTER_BOUND('',#19887,.T.);
#13656=FACE_OUTER_BOUND('',#19888,.T.);
#13657=FACE_OUTER_BOUND('',#19889,.T.);
#13658=FACE_OUTER_BOUND('',#19890,.T.);
#13659=FACE_OUTER_BOUND('',#19891,.T.);
#13660=FACE_OUTER_BOUND('',#19892,.T.);
#13661=FACE_OUTER_BOUND('',#19893,.T.);
#13662=FACE_OUTER_BOUND('',#19894,.T.);
#13663=FACE_OUTER_BOUND('',#19895,.T.);
#13664=FACE_OUTER_BOUND('',#19896,.T.);
#13665=FACE_OUTER_BOUND('',#19897,.T.);
#13666=FACE_OUTER_BOUND('',#19898,.T.);
#13667=FACE_OUTER_BOUND('',#19899,.T.);
#13668=FACE_OUTER_BOUND('',#19900,.T.);
#13669=FACE_OUTER_BOUND('',#19901,.T.);
#13670=FACE_OUTER_BOUND('',#19902,.T.);
#13671=FACE_OUTER_BOUND('',#19903,.T.);
#13672=FACE_OUTER_BOUND('',#19904,.T.);
#13673=FACE_OUTER_BOUND('',#19905,.T.);
#13674=FACE_OUTER_BOUND('',#19906,.T.);
#13675=FACE_OUTER_BOUND('',#19907,.T.);
#13676=FACE_OUTER_BOUND('',#19908,.T.);
#13677=FACE_OUTER_BOUND('',#19909,.T.);
#13678=FACE_OUTER_BOUND('',#19910,.T.);
#13679=FACE_OUTER_BOUND('',#19911,.T.);
#13680=FACE_OUTER_BOUND('',#19912,.T.);
#13681=FACE_OUTER_BOUND('',#19913,.T.);
#13682=FACE_OUTER_BOUND('',#19914,.T.);
#13683=FACE_OUTER_BOUND('',#19915,.T.);
#13684=FACE_OUTER_BOUND('',#19916,.T.);
#13685=FACE_OUTER_BOUND('',#19917,.T.);
#13686=FACE_OUTER_BOUND('',#19918,.T.);
#13687=FACE_OUTER_BOUND('',#19919,.T.);
#13688=FACE_OUTER_BOUND('',#19920,.T.);
#13689=FACE_OUTER_BOUND('',#19921,.T.);
#13690=FACE_OUTER_BOUND('',#19922,.T.);
#13691=FACE_OUTER_BOUND('',#19923,.T.);
#13692=FACE_OUTER_BOUND('',#19924,.T.);
#13693=FACE_OUTER_BOUND('',#19925,.T.);
#13694=FACE_OUTER_BOUND('',#19926,.T.);
#13695=FACE_OUTER_BOUND('',#19927,.T.);
#13696=FACE_OUTER_BOUND('',#19928,.T.);
#13697=FACE_OUTER_BOUND('',#19929,.T.);
#13698=FACE_OUTER_BOUND('',#19930,.T.);
#13699=FACE_OUTER_BOUND('',#19931,.T.);
#13700=FACE_OUTER_BOUND('',#19932,.T.);
#13701=FACE_OUTER_BOUND('',#19933,.T.);
#13702=FACE_OUTER_BOUND('',#19934,.T.);
#13703=FACE_OUTER_BOUND('',#19935,.T.);
#13704=FACE_OUTER_BOUND('',#19936,.T.);
#13705=FACE_OUTER_BOUND('',#19937,.T.);
#13706=FACE_OUTER_BOUND('',#19938,.T.);
#13707=FACE_OUTER_BOUND('',#19939,.T.);
#13708=FACE_OUTER_BOUND('',#19940,.T.);
#13709=FACE_OUTER_BOUND('',#19941,.T.);
#13710=FACE_OUTER_BOUND('',#19942,.T.);
#13711=FACE_OUTER_BOUND('',#19943,.T.);
#13712=FACE_OUTER_BOUND('',#19944,.T.);
#13713=FACE_OUTER_BOUND('',#19945,.T.);
#13714=FACE_OUTER_BOUND('',#19946,.T.);
#13715=FACE_OUTER_BOUND('',#19947,.T.);
#13716=FACE_OUTER_BOUND('',#19948,.T.);
#13717=FACE_OUTER_BOUND('',#19949,.T.);
#13718=FACE_OUTER_BOUND('',#19951,.T.);
#13719=FACE_OUTER_BOUND('',#19952,.T.);
#13720=FACE_OUTER_BOUND('',#19953,.T.);
#13721=FACE_OUTER_BOUND('',#19954,.T.);
#13722=FACE_OUTER_BOUND('',#19955,.T.);
#13723=FACE_OUTER_BOUND('',#19957,.T.);
#13724=EDGE_LOOP('',(#60425,#60426,#60427,#60428));
#13725=EDGE_LOOP('',(#60429,#60430,#60431,#60432));
#13726=EDGE_LOOP('',(#60433,#60434,#60435,#60436));
#13727=EDGE_LOOP('',(#60437,#60438,#60439,#60440));
#13728=EDGE_LOOP('',(#60441,#60442,#60443,#60444));
#13729=EDGE_LOOP('',(#60445,#60446,#60447,#60448));
#13730=EDGE_LOOP('',(#60449,#60450,#60451,#60452));
#13731=EDGE_LOOP('',(#60453,#60454,#60455,#60456));
#13732=EDGE_LOOP('',(#60457,#60458,#60459,#60460));
#13733=EDGE_LOOP('',(#60461,#60462,#60463,#60464));
#13734=EDGE_LOOP('',(#60465,#60466,#60467,#60468));
#13735=EDGE_LOOP('',(#60469,#60470,#60471,#60472));
#13736=EDGE_LOOP('',(#60473,#60474,#60475,#60476));
#13737=EDGE_LOOP('',(#60477,#60478,#60479,#60480));
#13738=EDGE_LOOP('',(#60481,#60482,#60483,#60484));
#13739=EDGE_LOOP('',(#60485,#60486,#60487,#60488));
#13740=EDGE_LOOP('',(#60489,#60490,#60491,#60492));
#13741=EDGE_LOOP('',(#60493,#60494,#60495,#60496));
#13742=EDGE_LOOP('',(#60497,#60498,#60499,#60500));
#13743=EDGE_LOOP('',(#60501,#60502,#60503,#60504));
#13744=EDGE_LOOP('',(#60505,#60506,#60507,#60508));
#13745=EDGE_LOOP('',(#60509,#60510,#60511,#60512));
#13746=EDGE_LOOP('',(#60513,#60514,#60515,#60516));
#13747=EDGE_LOOP('',(#60517,#60518,#60519,#60520));
#13748=EDGE_LOOP('',(#60521,#60522,#60523,#60524));
#13749=EDGE_LOOP('',(#60525,#60526,#60527,#60528));
#13750=EDGE_LOOP('',(#60529,#60530,#60531,#60532,#60533,#60534,#60535,#60536));
#13751=EDGE_LOOP('',(#60537));
#13752=EDGE_LOOP('',(#60538));
#13753=EDGE_LOOP('',(#60539));
#13754=EDGE_LOOP('',(#60540));
#13755=EDGE_LOOP('',(#60541,#60542,#60543,#60544));
#13756=EDGE_LOOP('',(#60545,#60546,#60547,#60548,#60549,#60550,#60551,#60552));
#13757=EDGE_LOOP('',(#60553,#60554,#60555,#60556));
#13758=EDGE_LOOP('',(#60557));
#13759=EDGE_LOOP('',(#60558));
#13760=EDGE_LOOP('',(#60559));
#13761=EDGE_LOOP('',(#60560));
#13762=EDGE_LOOP('',(#60561,#60562,#60563,#60564));
#13763=EDGE_LOOP('',(#60565,#60566,#60567,#60568));
#13764=EDGE_LOOP('',(#60569,#60570,#60571,#60572));
#13765=EDGE_LOOP('',(#60573,#60574,#60575,#60576));
#13766=EDGE_LOOP('',(#60577,#60578,#60579,#60580));
#13767=EDGE_LOOP('',(#60581,#60582,#60583,#60584));
#13768=EDGE_LOOP('',(#60585,#60586,#60587,#60588));
#13769=EDGE_LOOP('',(#60589,#60590,#60591,#60592));
#13770=EDGE_LOOP('',(#60593,#60594,#60595,#60596));
#13771=EDGE_LOOP('',(#60597,#60598,#60599,#60600));
#13772=EDGE_LOOP('',(#60601,#60602,#60603,#60604));
#13773=EDGE_LOOP('',(#60605,#60606,#60607,#60608));
#13774=EDGE_LOOP('',(#60609,#60610,#60611,#60612));
#13775=EDGE_LOOP('',(#60613,#60614,#60615,#60616));
#13776=EDGE_LOOP('',(#60617,#60618,#60619,#60620));
#13777=EDGE_LOOP('',(#60621,#60622,#60623,#60624));
#13778=EDGE_LOOP('',(#60625,#60626,#60627,#60628,#60629));
#13779=EDGE_LOOP('',(#60630,#60631,#60632,#60633,#60634));
#13780=EDGE_LOOP('',(#60635,#60636,#60637,#60638,#60639,#60640));
#13781=EDGE_LOOP('',(#60641,#60642,#60643,#60644,#60645,#60646));
#13782=EDGE_LOOP('',(#60647,#60648,#60649,#60650,#60651,#60652));
#13783=EDGE_LOOP('',(#60653,#60654,#60655,#60656,#60657,#60658));
#13784=EDGE_LOOP('',(#60659,#60660,#60661,#60662,#60663,#60664,#60665,#60666,
#60667));
#13785=EDGE_LOOP('',(#60668,#60669));
#13786=EDGE_LOOP('',(#60670,#60671));
#13787=EDGE_LOOP('',(#60672,#60673));
#13788=EDGE_LOOP('',(#60674,#60675,#60676,#60677,#60678,#60679,#60680,#60681,
#60682));
#13789=EDGE_LOOP('',(#60683,#60684));
#13790=EDGE_LOOP('',(#60685,#60686));
#13791=EDGE_LOOP('',(#60687,#60688));
#13792=EDGE_LOOP('',(#60689));
#13793=EDGE_LOOP('',(#60690));
#13794=EDGE_LOOP('',(#60691));
#13795=EDGE_LOOP('',(#60692));
#13796=EDGE_LOOP('',(#60693,#60694,#60695,#60696));
#13797=EDGE_LOOP('',(#60697,#60698,#60699,#60700));
#13798=EDGE_LOOP('',(#60701,#60702,#60703,#60704));
#13799=EDGE_LOOP('',(#60705,#60706,#60707,#60708));
#13800=EDGE_LOOP('',(#60709,#60710,#60711,#60712));
#13801=EDGE_LOOP('',(#60713,#60714,#60715,#60716));
#13802=EDGE_LOOP('',(#60717,#60718,#60719,#60720));
#13803=EDGE_LOOP('',(#60721,#60722,#60723,#60724));
#13804=EDGE_LOOP('',(#60725,#60726,#60727,#60728,#60729,#60730));
#13805=EDGE_LOOP('',(#60731,#60732));
#13806=EDGE_LOOP('',(#60733,#60734));
#13807=EDGE_LOOP('',(#60735,#60736,#60737,#60738,#60739,#60740));
#13808=EDGE_LOOP('',(#60741,#60742));
#13809=EDGE_LOOP('',(#60743,#60744,#60745,#60746));
#13810=EDGE_LOOP('',(#60747,#60748,#60749,#60750));
#13811=EDGE_LOOP('',(#60751,#60752,#60753,#60754));
#13812=EDGE_LOOP('',(#60755,#60756,#60757,#60758));
#13813=EDGE_LOOP('',(#60759,#60760,#60761,#60762));
#13814=EDGE_LOOP('',(#60763,#60764,#60765,#60766));
#13815=EDGE_LOOP('',(#60767,#60768,#60769,#60770));
#13816=EDGE_LOOP('',(#60771,#60772,#60773,#60774));
#13817=EDGE_LOOP('',(#60775,#60776,#60777,#60778));
#13818=EDGE_LOOP('',(#60779,#60780,#60781,#60782));
#13819=EDGE_LOOP('',(#60783,#60784,#60785,#60786));
#13820=EDGE_LOOP('',(#60787,#60788,#60789,#60790));
#13821=EDGE_LOOP('',(#60791,#60792,#60793,#60794));
#13822=EDGE_LOOP('',(#60795,#60796,#60797,#60798));
#13823=EDGE_LOOP('',(#60799,#60800,#60801,#60802,#60803,#60804));
#13824=EDGE_LOOP('',(#60805,#60806,#60807,#60808,#60809,#60810));
#13825=EDGE_LOOP('',(#60811,#60812,#60813,#60814,#60815,#60816));
#13826=EDGE_LOOP('',(#60817,#60818,#60819,#60820,#60821,#60822));
#13827=EDGE_LOOP('',(#60823,#60824,#60825,#60826));
#13828=EDGE_LOOP('',(#60827,#60828,#60829,#60830,#60831));
#13829=EDGE_LOOP('',(#60832,#60833,#60834,#60835,#60836,#60837,#60838,#60839));
#13830=EDGE_LOOP('',(#60840,#60841));
#13831=EDGE_LOOP('',(#60842,#60843));
#13832=EDGE_LOOP('',(#60844,#60845));
#13833=EDGE_LOOP('',(#60846,#60847,#60848,#60849,#60850,#60851,#60852,#60853,
#60854,#60855,#60856,#60857));
#13834=EDGE_LOOP('',(#60858,#60859,#60860,#60861,#60862,#60863,#60864,#60865,
#60866,#60867,#60868,#60869,#60870,#60871,#60872,#60873,#60874,#60875,#60876,
#60877));
#13835=EDGE_LOOP('',(#60878,#60879,#60880,#60881,#60882,#60883,#60884,#60885,
#60886,#60887,#60888,#60889,#60890,#60891,#60892,#60893,#60894,#60895,#60896,
#60897));
#13836=EDGE_LOOP('',(#60898,#60899,#60900,#60901,#60902,#60903,#60904,#60905,
#60906,#60907,#60908,#60909));
#13837=EDGE_LOOP('',(#60910,#60911,#60912,#60913));
#13838=EDGE_LOOP('',(#60914,#60915,#60916,#60917));
#13839=EDGE_LOOP('',(#60918,#60919,#60920,#60921,#60922,#60923,#60924,#60925));
#13840=EDGE_LOOP('',(#60926));
#13841=EDGE_LOOP('',(#60927));
#13842=EDGE_LOOP('',(#60928,#60929,#60930,#60931,#60932,#60933,#60934,#60935));
#13843=EDGE_LOOP('',(#60936));
#13844=EDGE_LOOP('',(#60937,#60938,#60939,#60940,#60941));
#13845=EDGE_LOOP('',(#60942,#60943,#60944,#60945));
#13846=EDGE_LOOP('',(#60946,#60947,#60948,#60949));
#13847=EDGE_LOOP('',(#60950,#60951,#60952,#60953));
#13848=EDGE_LOOP('',(#60954,#60955,#60956,#60957,#60958));
#13849=EDGE_LOOP('',(#60959,#60960,#60961,#60962,#60963,#60964,#60965,#60966,
#60967,#60968,#60969));
#13850=EDGE_LOOP('',(#60970));
#13851=EDGE_LOOP('',(#60971));
#13852=EDGE_LOOP('',(#60972,#60973,#60974,#60975,#60976));
#13853=EDGE_LOOP('',(#60977,#60978,#60979,#60980,#60981,#60982));
#13854=EDGE_LOOP('',(#60983,#60984,#60985,#60986,#60987));
#13855=EDGE_LOOP('',(#60988,#60989,#60990,#60991));
#13856=EDGE_LOOP('',(#60992));
#13857=EDGE_LOOP('',(#60993));
#13858=EDGE_LOOP('',(#60994));
#13859=EDGE_LOOP('',(#60995,#60996,#60997,#60998));
#13860=EDGE_LOOP('',(#60999,#61000,#61001,#61002));
#13861=EDGE_LOOP('',(#61003,#61004,#61005,#61006));
#13862=EDGE_LOOP('',(#61007,#61008,#61009,#61010));
#13863=EDGE_LOOP('',(#61011,#61012,#61013,#61014));
#13864=EDGE_LOOP('',(#61015));
#13865=EDGE_LOOP('',(#61016,#61017,#61018,#61019,#61020,#61021));
#13866=EDGE_LOOP('',(#61022));
#13867=EDGE_LOOP('',(#61023,#61024,#61025,#61026));
#13868=EDGE_LOOP('',(#61027,#61028,#61029,#61030));
#13869=EDGE_LOOP('',(#61031,#61032,#61033,#61034));
#13870=EDGE_LOOP('',(#61035,#61036,#61037,#61038));
#13871=EDGE_LOOP('',(#61039,#61040,#61041,#61042));
#13872=EDGE_LOOP('',(#61043,#61044,#61045,#61046,#61047,#61048));
#13873=EDGE_LOOP('',(#61049,#61050,#61051,#61052,#61053,#61054));
#13874=EDGE_LOOP('',(#61055,#61056,#61057,#61058,#61059,#61060));
#13875=EDGE_LOOP('',(#61061,#61062,#61063,#61064,#61065,#61066));
#13876=EDGE_LOOP('',(#61067,#61068,#61069,#61070,#61071,#61072));
#13877=EDGE_LOOP('',(#61073,#61074,#61075,#61076,#61077,#61078));
#13878=EDGE_LOOP('',(#61079,#61080,#61081,#61082));
#13879=EDGE_LOOP('',(#61083,#61084,#61085,#61086));
#13880=EDGE_LOOP('',(#61087,#61088,#61089,#61090));
#13881=EDGE_LOOP('',(#61091,#61092,#61093,#61094));
#13882=EDGE_LOOP('',(#61095,#61096,#61097,#61098));
#13883=EDGE_LOOP('',(#61099,#61100,#61101,#61102));
#13884=EDGE_LOOP('',(#61103,#61104,#61105,#61106));
#13885=EDGE_LOOP('',(#61107));
#13886=EDGE_LOOP('',(#61108));
#13887=EDGE_LOOP('',(#61109));
#13888=EDGE_LOOP('',(#61110));
#13889=EDGE_LOOP('',(#61111,#61112,#61113,#61114));
#13890=EDGE_LOOP('',(#61115,#61116,#61117,#61118));
#13891=EDGE_LOOP('',(#61119));
#13892=EDGE_LOOP('',(#61120));
#13893=EDGE_LOOP('',(#61121));
#13894=EDGE_LOOP('',(#61122));
#13895=EDGE_LOOP('',(#61123,#61124,#61125,#61126));
#13896=EDGE_LOOP('',(#61127,#61128,#61129,#61130));
#13897=EDGE_LOOP('',(#61131));
#13898=EDGE_LOOP('',(#61132));
#13899=EDGE_LOOP('',(#61133));
#13900=EDGE_LOOP('',(#61134));
#13901=EDGE_LOOP('',(#61135,#61136,#61137,#61138));
#13902=EDGE_LOOP('',(#61139,#61140,#61141,#61142));
#13903=EDGE_LOOP('',(#61143));
#13904=EDGE_LOOP('',(#61144));
#13905=EDGE_LOOP('',(#61145));
#13906=EDGE_LOOP('',(#61146));
#13907=EDGE_LOOP('',(#61147,#61148,#61149,#61150,#61151));
#13908=EDGE_LOOP('',(#61152,#61153,#61154,#61155,#61156));
#13909=EDGE_LOOP('',(#61157,#61158,#61159,#61160,#61161));
#13910=EDGE_LOOP('',(#61162,#61163,#61164,#61165,#61166));
#13911=EDGE_LOOP('',(#61167));
#13912=EDGE_LOOP('',(#61168));
#13913=EDGE_LOOP('',(#61169));
#13914=EDGE_LOOP('',(#61170));
#13915=EDGE_LOOP('',(#61171,#61172,#61173,#61174,#61175));
#13916=EDGE_LOOP('',(#61176,#61177,#61178,#61179,#61180));
#13917=EDGE_LOOP('',(#61181,#61182,#61183,#61184,#61185));
#13918=EDGE_LOOP('',(#61186,#61187,#61188,#61189,#61190));
#13919=EDGE_LOOP('',(#61191));
#13920=EDGE_LOOP('',(#61192));
#13921=EDGE_LOOP('',(#61193));
#13922=EDGE_LOOP('',(#61194));
#13923=EDGE_LOOP('',(#61195,#61196,#61197,#61198));
#13924=EDGE_LOOP('',(#61199,#61200,#61201,#61202));
#13925=EDGE_LOOP('',(#61203));
#13926=EDGE_LOOP('',(#61204));
#13927=EDGE_LOOP('',(#61205));
#13928=EDGE_LOOP('',(#61206));
#13929=EDGE_LOOP('',(#61207,#61208,#61209,#61210));
#13930=EDGE_LOOP('',(#61211,#61212,#61213,#61214));
#13931=EDGE_LOOP('',(#61215,#61216,#61217,#61218));
#13932=EDGE_LOOP('',(#61219,#61220,#61221,#61222,#61223));
#13933=EDGE_LOOP('',(#61224,#61225,#61226,#61227,#61228));
#13934=EDGE_LOOP('',(#61229,#61230,#61231,#61232));
#13935=EDGE_LOOP('',(#61233,#61234,#61235,#61236,#61237));
#13936=EDGE_LOOP('',(#61238,#61239,#61240,#61241));
#13937=EDGE_LOOP('',(#61242,#61243,#61244,#61245));
#13938=EDGE_LOOP('',(#61246,#61247,#61248,#61249));
#13939=EDGE_LOOP('',(#61250,#61251,#61252,#61253,#61254,#61255,#61256,#61257,
#61258,#61259,#61260,#61261,#61262,#61263,#61264,#61265,#61266,#61267,#61268,
#61269,#61270,#61271,#61272,#61273,#61274,#61275,#61276,#61277,#61278,#61279,
#61280,#61281,#61282,#61283,#61284,#61285,#61286,#61287,#61288,#61289,#61290,
#61291,#61292,#61293,#61294,#61295,#61296,#61297,#61298,#61299,#61300,#61301,
#61302,#61303,#61304,#61305,#61306,#61307,#61308,#61309,#61310,#61311,#61312,
#61313,#61314,#61315,#61316,#61317,#61318,#61319,#61320,#61321,#61322,#61323,
#61324,#61325,#61326,#61327,#61328,#61329,#61330,#61331,#61332,#61333,#61334,
#61335,#61336,#61337,#61338,#61339,#61340,#61341,#61342,#61343,#61344,#61345,
#61346,#61347,#61348,#61349,#61350,#61351,#61352,#61353,#61354,#61355,#61356,
#61357,#61358,#61359,#61360,#61361,#61362,#61363,#61364,#61365,#61366,#61367,
#61368,#61369,#61370,#61371,#61372,#61373,#61374,#61375,#61376,#61377,#61378,
#61379,#61380,#61381,#61382,#61383,#61384,#61385,#61386,#61387,#61388,#61389,
#61390,#61391,#61392,#61393,#61394,#61395,#61396,#61397,#61398,#61399,#61400,
#61401,#61402,#61403,#61404,#61405,#61406,#61407,#61408,#61409,#61410,#61411,
#61412,#61413,#61414,#61415,#61416,#61417,#61418,#61419,#61420,#61421,#61422,
#61423,#61424,#61425,#61426,#61427,#61428,#61429,#61430,#61431,#61432,#61433,
#61434,#61435,#61436,#61437,#61438,#61439,#61440,#61441,#61442,#61443,#61444,
#61445,#61446,#61447,#61448,#61449,#61450,#61451,#61452,#61453,#61454,#61455,
#61456,#61457,#61458,#61459,#61460,#61461,#61462,#61463,#61464,#61465,#61466,
#61467,#61468,#61469,#61470,#61471,#61472,#61473,#61474,#61475,#61476,#61477,
#61478,#61479,#61480,#61481,#61482,#61483,#61484,#61485,#61486,#61487,#61488,
#61489,#61490,#61491,#61492,#61493,#61494,#61495,#61496,#61497,#61498,#61499,
#61500,#61501,#61502,#61503,#61504,#61505,#61506,#61507,#61508,#61509,#61510,
#61511,#61512,#61513,#61514,#61515,#61516,#61517,#61518,#61519,#61520,#61521,
#61522,#61523,#61524,#61525,#61526,#61527,#61528,#61529,#61530,#61531,#61532,
#61533,#61534,#61535,#61536,#61537,#61538,#61539,#61540,#61541,#61542,#61543,
#61544,#61545,#61546,#61547,#61548,#61549,#61550,#61551,#61552,#61553,#61554,
#61555,#61556,#61557,#61558,#61559,#61560,#61561,#61562,#61563,#61564,#61565,
#61566,#61567,#61568,#61569,#61570,#61571,#61572,#61573,#61574,#61575,#61576,
#61577,#61578,#61579,#61580,#61581,#61582,#61583,#61584,#61585,#61586,#61587,
#61588,#61589,#61590,#61591,#61592,#61593,#61594,#61595,#61596,#61597,#61598,
#61599,#61600,#61601,#61602,#61603,#61604,#61605,#61606,#61607,#61608,#61609,
#61610,#61611,#61612,#61613,#61614));
#13940=EDGE_LOOP('',(#61615,#61616,#61617,#61618,#61619,#61620,#61621,#61622,
#61623,#61624,#61625,#61626,#61627,#61628,#61629,#61630,#61631,#61632,#61633,
#61634,#61635,#61636,#61637,#61638,#61639,#61640,#61641,#61642,#61643,#61644,
#61645,#61646,#61647,#61648,#61649,#61650,#61651,#61652,#61653,#61654,#61655,
#61656,#61657,#61658,#61659,#61660,#61661,#61662,#61663,#61664,#61665,#61666,
#61667,#61668,#61669,#61670,#61671,#61672,#61673,#61674,#61675,#61676,#61677,
#61678,#61679,#61680,#61681,#61682,#61683,#61684,#61685,#61686,#61687,#61688,
#61689,#61690,#61691,#61692,#61693,#61694,#61695,#61696,#61697,#61698,#61699,
#61700,#61701,#61702,#61703,#61704,#61705,#61706,#61707,#61708,#61709,#61710,
#61711,#61712,#61713,#61714,#61715,#61716,#61717,#61718,#61719,#61720,#61721,
#61722,#61723,#61724,#61725,#61726,#61727,#61728,#61729,#61730,#61731,#61732,
#61733,#61734,#61735,#61736,#61737,#61738,#61739,#61740,#61741,#61742,#61743,
#61744,#61745,#61746,#61747,#61748,#61749,#61750,#61751,#61752,#61753,#61754,
#61755,#61756,#61757,#61758,#61759,#61760,#61761,#61762,#61763,#61764,#61765,
#61766,#61767,#61768,#61769,#61770,#61771,#61772,#61773,#61774,#61775,#61776,
#61777,#61778,#61779,#61780,#61781,#61782,#61783,#61784,#61785,#61786,#61787,
#61788,#61789,#61790,#61791,#61792,#61793,#61794,#61795,#61796,#61797,#61798,
#61799,#61800,#61801,#61802,#61803,#61804,#61805,#61806,#61807,#61808,#61809,
#61810,#61811,#61812,#61813,#61814,#61815,#61816,#61817,#61818,#61819,#61820,
#61821,#61822,#61823,#61824,#61825,#61826,#61827,#61828,#61829,#61830,#61831,
#61832,#61833,#61834,#61835,#61836,#61837,#61838,#61839,#61840,#61841,#61842,
#61843,#61844,#61845,#61846,#61847,#61848,#61849,#61850,#61851,#61852,#61853,
#61854,#61855,#61856,#61857,#61858,#61859,#61860,#61861,#61862,#61863,#61864,
#61865,#61866,#61867,#61868,#61869,#61870,#61871,#61872,#61873,#61874,#61875,
#61876,#61877,#61878,#61879,#61880,#61881,#61882,#61883,#61884,#61885,#61886,
#61887,#61888,#61889,#61890,#61891,#61892,#61893,#61894,#61895,#61896,#61897,
#61898,#61899,#61900,#61901,#61902,#61903,#61904,#61905,#61906,#61907,#61908,
#61909,#61910,#61911,#61912,#61913,#61914,#61915,#61916,#61917,#61918,#61919,
#61920,#61921,#61922,#61923,#61924,#61925,#61926,#61927,#61928,#61929,#61930,
#61931,#61932,#61933,#61934,#61935,#61936,#61937,#61938,#61939,#61940,#61941,
#61942,#61943,#61944,#61945,#61946,#61947,#61948,#61949,#61950,#61951,#61952,
#61953,#61954,#61955,#61956,#61957,#61958,#61959,#61960,#61961,#61962,#61963,
#61964,#61965,#61966,#61967,#61968,#61969,#61970,#61971,#61972,#61973,#61974,
#61975,#61976,#61977,#61978));
#13941=EDGE_LOOP('',(#61979,#61980,#61981,#61982,#61983,#61984));
#13942=EDGE_LOOP('',(#61985,#61986,#61987,#61988,#61989));
#13943=EDGE_LOOP('',(#61990,#61991,#61992,#61993,#61994,#61995));
#13944=EDGE_LOOP('',(#61996,#61997,#61998,#61999));
#13945=EDGE_LOOP('',(#62000,#62001,#62002,#62003));
#13946=EDGE_LOOP('',(#62004,#62005,#62006,#62007,#62008,#62009));
#13947=EDGE_LOOP('',(#62010,#62011,#62012,#62013));
#13948=EDGE_LOOP('',(#62014,#62015,#62016,#62017));
#13949=EDGE_LOOP('',(#62018,#62019,#62020,#62021));
#13950=EDGE_LOOP('',(#62022,#62023,#62024,#62025));
#13951=EDGE_LOOP('',(#62026,#62027,#62028,#62029));
#13952=EDGE_LOOP('',(#62030,#62031,#62032,#62033,#62034,#62035));
#13953=EDGE_LOOP('',(#62036,#62037,#62038,#62039));
#13954=EDGE_LOOP('',(#62040,#62041,#62042,#62043));
#13955=EDGE_LOOP('',(#62044,#62045,#62046,#62047,#62048,#62049));
#13956=EDGE_LOOP('',(#62050,#62051,#62052,#62053));
#13957=EDGE_LOOP('',(#62054,#62055,#62056,#62057));
#13958=EDGE_LOOP('',(#62058,#62059,#62060,#62061));
#13959=EDGE_LOOP('',(#62062,#62063,#62064,#62065));
#13960=EDGE_LOOP('',(#62066,#62067,#62068,#62069));
#13961=EDGE_LOOP('',(#62070,#62071,#62072,#62073,#62074,#62075));
#13962=EDGE_LOOP('',(#62076,#62077,#62078,#62079));
#13963=EDGE_LOOP('',(#62080,#62081,#62082,#62083));
#13964=EDGE_LOOP('',(#62084,#62085,#62086,#62087,#62088,#62089));
#13965=EDGE_LOOP('',(#62090,#62091,#62092,#62093));
#13966=EDGE_LOOP('',(#62094,#62095,#62096,#62097));
#13967=EDGE_LOOP('',(#62098,#62099,#62100,#62101));
#13968=EDGE_LOOP('',(#62102,#62103,#62104,#62105));
#13969=EDGE_LOOP('',(#62106,#62107,#62108,#62109));
#13970=EDGE_LOOP('',(#62110,#62111,#62112,#62113,#62114,#62115));
#13971=EDGE_LOOP('',(#62116,#62117,#62118,#62119));
#13972=EDGE_LOOP('',(#62120,#62121,#62122,#62123));
#13973=EDGE_LOOP('',(#62124,#62125,#62126,#62127,#62128,#62129));
#13974=EDGE_LOOP('',(#62130,#62131,#62132,#62133));
#13975=EDGE_LOOP('',(#62134,#62135,#62136,#62137));
#13976=EDGE_LOOP('',(#62138,#62139,#62140,#62141));
#13977=EDGE_LOOP('',(#62142,#62143,#62144,#62145));
#13978=EDGE_LOOP('',(#62146,#62147,#62148,#62149));
#13979=EDGE_LOOP('',(#62150,#62151,#62152,#62153,#62154,#62155));
#13980=EDGE_LOOP('',(#62156,#62157,#62158,#62159));
#13981=EDGE_LOOP('',(#62160,#62161,#62162,#62163));
#13982=EDGE_LOOP('',(#62164,#62165,#62166,#62167,#62168,#62169));
#13983=EDGE_LOOP('',(#62170,#62171,#62172,#62173));
#13984=EDGE_LOOP('',(#62174,#62175,#62176,#62177));
#13985=EDGE_LOOP('',(#62178,#62179,#62180,#62181));
#13986=EDGE_LOOP('',(#62182,#62183,#62184,#62185));
#13987=EDGE_LOOP('',(#62186,#62187,#62188,#62189));
#13988=EDGE_LOOP('',(#62190,#62191,#62192,#62193,#62194,#62195));
#13989=EDGE_LOOP('',(#62196,#62197,#62198,#62199));
#13990=EDGE_LOOP('',(#62200,#62201,#62202,#62203));
#13991=EDGE_LOOP('',(#62204,#62205,#62206,#62207,#62208,#62209));
#13992=EDGE_LOOP('',(#62210,#62211,#62212,#62213));
#13993=EDGE_LOOP('',(#62214,#62215,#62216,#62217));
#13994=EDGE_LOOP('',(#62218,#62219,#62220,#62221));
#13995=EDGE_LOOP('',(#62222,#62223,#62224,#62225));
#13996=EDGE_LOOP('',(#62226,#62227,#62228,#62229));
#13997=EDGE_LOOP('',(#62230,#62231,#62232,#62233,#62234,#62235));
#13998=EDGE_LOOP('',(#62236,#62237,#62238,#62239));
#13999=EDGE_LOOP('',(#62240,#62241,#62242,#62243));
#14000=EDGE_LOOP('',(#62244,#62245,#62246,#62247,#62248,#62249));
#14001=EDGE_LOOP('',(#62250,#62251,#62252,#62253));
#14002=EDGE_LOOP('',(#62254,#62255,#62256,#62257));
#14003=EDGE_LOOP('',(#62258,#62259,#62260,#62261));
#14004=EDGE_LOOP('',(#62262,#62263,#62264,#62265));
#14005=EDGE_LOOP('',(#62266,#62267,#62268,#62269));
#14006=EDGE_LOOP('',(#62270,#62271,#62272,#62273,#62274,#62275));
#14007=EDGE_LOOP('',(#62276,#62277,#62278,#62279));
#14008=EDGE_LOOP('',(#62280,#62281,#62282,#62283));
#14009=EDGE_LOOP('',(#62284,#62285,#62286,#62287,#62288,#62289));
#14010=EDGE_LOOP('',(#62290,#62291,#62292,#62293));
#14011=EDGE_LOOP('',(#62294,#62295,#62296,#62297));
#14012=EDGE_LOOP('',(#62298,#62299,#62300,#62301));
#14013=EDGE_LOOP('',(#62302,#62303,#62304,#62305));
#14014=EDGE_LOOP('',(#62306,#62307,#62308,#62309));
#14015=EDGE_LOOP('',(#62310,#62311,#62312,#62313,#62314,#62315));
#14016=EDGE_LOOP('',(#62316,#62317,#62318,#62319));
#14017=EDGE_LOOP('',(#62320,#62321,#62322,#62323));
#14018=EDGE_LOOP('',(#62324,#62325,#62326,#62327,#62328,#62329));
#14019=EDGE_LOOP('',(#62330,#62331,#62332,#62333));
#14020=EDGE_LOOP('',(#62334,#62335,#62336,#62337));
#14021=EDGE_LOOP('',(#62338,#62339,#62340,#62341));
#14022=EDGE_LOOP('',(#62342,#62343,#62344,#62345));
#14023=EDGE_LOOP('',(#62346,#62347,#62348,#62349));
#14024=EDGE_LOOP('',(#62350,#62351,#62352,#62353,#62354,#62355));
#14025=EDGE_LOOP('',(#62356,#62357,#62358,#62359));
#14026=EDGE_LOOP('',(#62360,#62361,#62362,#62363));
#14027=EDGE_LOOP('',(#62364,#62365,#62366,#62367,#62368,#62369));
#14028=EDGE_LOOP('',(#62370,#62371,#62372,#62373));
#14029=EDGE_LOOP('',(#62374,#62375,#62376,#62377));
#14030=EDGE_LOOP('',(#62378,#62379,#62380,#62381));
#14031=EDGE_LOOP('',(#62382,#62383,#62384,#62385));
#14032=EDGE_LOOP('',(#62386,#62387,#62388,#62389));
#14033=EDGE_LOOP('',(#62390,#62391,#62392,#62393,#62394,#62395));
#14034=EDGE_LOOP('',(#62396,#62397,#62398,#62399));
#14035=EDGE_LOOP('',(#62400,#62401,#62402,#62403));
#14036=EDGE_LOOP('',(#62404,#62405,#62406,#62407,#62408,#62409));
#14037=EDGE_LOOP('',(#62410,#62411,#62412,#62413));
#14038=EDGE_LOOP('',(#62414,#62415,#62416,#62417));
#14039=EDGE_LOOP('',(#62418,#62419,#62420,#62421));
#14040=EDGE_LOOP('',(#62422,#62423,#62424,#62425));
#14041=EDGE_LOOP('',(#62426,#62427,#62428,#62429));
#14042=EDGE_LOOP('',(#62430,#62431,#62432,#62433,#62434,#62435));
#14043=EDGE_LOOP('',(#62436,#62437,#62438,#62439));
#14044=EDGE_LOOP('',(#62440,#62441,#62442,#62443));
#14045=EDGE_LOOP('',(#62444,#62445,#62446,#62447,#62448,#62449));
#14046=EDGE_LOOP('',(#62450,#62451,#62452,#62453));
#14047=EDGE_LOOP('',(#62454,#62455,#62456,#62457));
#14048=EDGE_LOOP('',(#62458,#62459,#62460,#62461));
#14049=EDGE_LOOP('',(#62462,#62463,#62464,#62465));
#14050=EDGE_LOOP('',(#62466,#62467,#62468,#62469));
#14051=EDGE_LOOP('',(#62470,#62471,#62472,#62473,#62474,#62475));
#14052=EDGE_LOOP('',(#62476,#62477,#62478,#62479));
#14053=EDGE_LOOP('',(#62480,#62481,#62482,#62483));
#14054=EDGE_LOOP('',(#62484,#62485,#62486,#62487,#62488,#62489));
#14055=EDGE_LOOP('',(#62490,#62491,#62492,#62493));
#14056=EDGE_LOOP('',(#62494,#62495,#62496,#62497));
#14057=EDGE_LOOP('',(#62498,#62499,#62500,#62501));
#14058=EDGE_LOOP('',(#62502,#62503,#62504,#62505));
#14059=EDGE_LOOP('',(#62506,#62507,#62508,#62509));
#14060=EDGE_LOOP('',(#62510,#62511,#62512,#62513,#62514,#62515));
#14061=EDGE_LOOP('',(#62516,#62517,#62518,#62519));
#14062=EDGE_LOOP('',(#62520,#62521,#62522,#62523));
#14063=EDGE_LOOP('',(#62524,#62525,#62526,#62527,#62528,#62529));
#14064=EDGE_LOOP('',(#62530,#62531,#62532,#62533));
#14065=EDGE_LOOP('',(#62534,#62535,#62536,#62537));
#14066=EDGE_LOOP('',(#62538,#62539,#62540,#62541));
#14067=EDGE_LOOP('',(#62542,#62543,#62544,#62545));
#14068=EDGE_LOOP('',(#62546,#62547,#62548,#62549));
#14069=EDGE_LOOP('',(#62550,#62551,#62552,#62553,#62554,#62555));
#14070=EDGE_LOOP('',(#62556,#62557,#62558,#62559));
#14071=EDGE_LOOP('',(#62560,#62561,#62562,#62563));
#14072=EDGE_LOOP('',(#62564,#62565,#62566,#62567,#62568,#62569));
#14073=EDGE_LOOP('',(#62570,#62571,#62572,#62573));
#14074=EDGE_LOOP('',(#62574,#62575,#62576,#62577));
#14075=EDGE_LOOP('',(#62578,#62579,#62580,#62581));
#14076=EDGE_LOOP('',(#62582,#62583,#62584,#62585));
#14077=EDGE_LOOP('',(#62586,#62587,#62588,#62589));
#14078=EDGE_LOOP('',(#62590,#62591,#62592,#62593,#62594,#62595));
#14079=EDGE_LOOP('',(#62596,#62597,#62598,#62599));
#14080=EDGE_LOOP('',(#62600,#62601,#62602,#62603));
#14081=EDGE_LOOP('',(#62604,#62605,#62606,#62607,#62608,#62609));
#14082=EDGE_LOOP('',(#62610,#62611,#62612,#62613));
#14083=EDGE_LOOP('',(#62614,#62615,#62616,#62617));
#14084=EDGE_LOOP('',(#62618,#62619,#62620,#62621));
#14085=EDGE_LOOP('',(#62622,#62623,#62624,#62625));
#14086=EDGE_LOOP('',(#62626,#62627,#62628,#62629));
#14087=EDGE_LOOP('',(#62630,#62631,#62632,#62633,#62634,#62635));
#14088=EDGE_LOOP('',(#62636,#62637,#62638,#62639));
#14089=EDGE_LOOP('',(#62640,#62641,#62642,#62643));
#14090=EDGE_LOOP('',(#62644,#62645,#62646,#62647,#62648,#62649));
#14091=EDGE_LOOP('',(#62650,#62651,#62652,#62653));
#14092=EDGE_LOOP('',(#62654,#62655,#62656,#62657));
#14093=EDGE_LOOP('',(#62658,#62659,#62660,#62661));
#14094=EDGE_LOOP('',(#62662,#62663,#62664,#62665));
#14095=EDGE_LOOP('',(#62666,#62667,#62668,#62669));
#14096=EDGE_LOOP('',(#62670,#62671,#62672,#62673,#62674,#62675));
#14097=EDGE_LOOP('',(#62676,#62677,#62678,#62679));
#14098=EDGE_LOOP('',(#62680,#62681,#62682,#62683));
#14099=EDGE_LOOP('',(#62684,#62685,#62686,#62687,#62688,#62689));
#14100=EDGE_LOOP('',(#62690,#62691,#62692,#62693));
#14101=EDGE_LOOP('',(#62694,#62695,#62696,#62697));
#14102=EDGE_LOOP('',(#62698,#62699,#62700,#62701));
#14103=EDGE_LOOP('',(#62702,#62703,#62704,#62705));
#14104=EDGE_LOOP('',(#62706,#62707,#62708,#62709));
#14105=EDGE_LOOP('',(#62710,#62711,#62712,#62713,#62714,#62715));
#14106=EDGE_LOOP('',(#62716,#62717,#62718,#62719));
#14107=EDGE_LOOP('',(#62720,#62721,#62722,#62723));
#14108=EDGE_LOOP('',(#62724,#62725,#62726,#62727,#62728,#62729));
#14109=EDGE_LOOP('',(#62730,#62731,#62732,#62733));
#14110=EDGE_LOOP('',(#62734,#62735,#62736,#62737));
#14111=EDGE_LOOP('',(#62738,#62739,#62740,#62741));
#14112=EDGE_LOOP('',(#62742,#62743,#62744,#62745));
#14113=EDGE_LOOP('',(#62746,#62747,#62748,#62749));
#14114=EDGE_LOOP('',(#62750,#62751,#62752,#62753,#62754,#62755));
#14115=EDGE_LOOP('',(#62756,#62757,#62758,#62759));
#14116=EDGE_LOOP('',(#62760,#62761,#62762,#62763));
#14117=EDGE_LOOP('',(#62764,#62765,#62766,#62767,#62768,#62769));
#14118=EDGE_LOOP('',(#62770,#62771,#62772,#62773));
#14119=EDGE_LOOP('',(#62774,#62775,#62776,#62777));
#14120=EDGE_LOOP('',(#62778,#62779,#62780,#62781));
#14121=EDGE_LOOP('',(#62782,#62783,#62784,#62785));
#14122=EDGE_LOOP('',(#62786,#62787,#62788,#62789));
#14123=EDGE_LOOP('',(#62790,#62791,#62792,#62793,#62794,#62795));
#14124=EDGE_LOOP('',(#62796,#62797,#62798,#62799));
#14125=EDGE_LOOP('',(#62800,#62801,#62802,#62803));
#14126=EDGE_LOOP('',(#62804,#62805,#62806,#62807,#62808,#62809));
#14127=EDGE_LOOP('',(#62810,#62811,#62812,#62813));
#14128=EDGE_LOOP('',(#62814,#62815,#62816,#62817));
#14129=EDGE_LOOP('',(#62818,#62819,#62820,#62821));
#14130=EDGE_LOOP('',(#62822,#62823,#62824,#62825));
#14131=EDGE_LOOP('',(#62826,#62827,#62828,#62829));
#14132=EDGE_LOOP('',(#62830,#62831,#62832,#62833,#62834,#62835));
#14133=EDGE_LOOP('',(#62836,#62837,#62838,#62839));
#14134=EDGE_LOOP('',(#62840,#62841,#62842,#62843));
#14135=EDGE_LOOP('',(#62844,#62845,#62846,#62847,#62848,#62849));
#14136=EDGE_LOOP('',(#62850,#62851,#62852,#62853));
#14137=EDGE_LOOP('',(#62854,#62855,#62856,#62857));
#14138=EDGE_LOOP('',(#62858,#62859,#62860,#62861));
#14139=EDGE_LOOP('',(#62862,#62863,#62864,#62865));
#14140=EDGE_LOOP('',(#62866,#62867,#62868,#62869));
#14141=EDGE_LOOP('',(#62870,#62871,#62872,#62873,#62874,#62875));
#14142=EDGE_LOOP('',(#62876,#62877,#62878,#62879));
#14143=EDGE_LOOP('',(#62880,#62881,#62882,#62883));
#14144=EDGE_LOOP('',(#62884,#62885,#62886,#62887,#62888,#62889));
#14145=EDGE_LOOP('',(#62890,#62891,#62892,#62893));
#14146=EDGE_LOOP('',(#62894,#62895,#62896,#62897));
#14147=EDGE_LOOP('',(#62898,#62899,#62900,#62901));
#14148=EDGE_LOOP('',(#62902,#62903,#62904,#62905));
#14149=EDGE_LOOP('',(#62906,#62907,#62908,#62909));
#14150=EDGE_LOOP('',(#62910,#62911,#62912,#62913,#62914,#62915));
#14151=EDGE_LOOP('',(#62916,#62917,#62918,#62919));
#14152=EDGE_LOOP('',(#62920,#62921,#62922,#62923));
#14153=EDGE_LOOP('',(#62924,#62925,#62926,#62927,#62928,#62929));
#14154=EDGE_LOOP('',(#62930,#62931,#62932,#62933));
#14155=EDGE_LOOP('',(#62934,#62935,#62936,#62937));
#14156=EDGE_LOOP('',(#62938,#62939,#62940,#62941));
#14157=EDGE_LOOP('',(#62942,#62943,#62944,#62945));
#14158=EDGE_LOOP('',(#62946,#62947,#62948,#62949));
#14159=EDGE_LOOP('',(#62950,#62951,#62952,#62953,#62954,#62955));
#14160=EDGE_LOOP('',(#62956,#62957,#62958,#62959));
#14161=EDGE_LOOP('',(#62960,#62961,#62962,#62963));
#14162=EDGE_LOOP('',(#62964,#62965,#62966,#62967,#62968,#62969));
#14163=EDGE_LOOP('',(#62970,#62971,#62972,#62973));
#14164=EDGE_LOOP('',(#62974,#62975,#62976,#62977));
#14165=EDGE_LOOP('',(#62978,#62979,#62980,#62981));
#14166=EDGE_LOOP('',(#62982,#62983,#62984,#62985));
#14167=EDGE_LOOP('',(#62986,#62987,#62988,#62989));
#14168=EDGE_LOOP('',(#62990,#62991,#62992,#62993,#62994,#62995));
#14169=EDGE_LOOP('',(#62996,#62997,#62998,#62999));
#14170=EDGE_LOOP('',(#63000,#63001,#63002,#63003));
#14171=EDGE_LOOP('',(#63004,#63005,#63006,#63007,#63008,#63009));
#14172=EDGE_LOOP('',(#63010,#63011,#63012,#63013));
#14173=EDGE_LOOP('',(#63014,#63015,#63016,#63017));
#14174=EDGE_LOOP('',(#63018,#63019,#63020,#63021));
#14175=EDGE_LOOP('',(#63022,#63023,#63024,#63025));
#14176=EDGE_LOOP('',(#63026,#63027,#63028,#63029));
#14177=EDGE_LOOP('',(#63030,#63031,#63032,#63033,#63034,#63035));
#14178=EDGE_LOOP('',(#63036,#63037,#63038,#63039));
#14179=EDGE_LOOP('',(#63040,#63041,#63042,#63043));
#14180=EDGE_LOOP('',(#63044,#63045,#63046,#63047,#63048,#63049));
#14181=EDGE_LOOP('',(#63050,#63051,#63052,#63053));
#14182=EDGE_LOOP('',(#63054,#63055,#63056,#63057));
#14183=EDGE_LOOP('',(#63058,#63059,#63060,#63061));
#14184=EDGE_LOOP('',(#63062,#63063,#63064,#63065));
#14185=EDGE_LOOP('',(#63066,#63067,#63068,#63069));
#14186=EDGE_LOOP('',(#63070,#63071,#63072,#63073,#63074,#63075));
#14187=EDGE_LOOP('',(#63076,#63077,#63078,#63079));
#14188=EDGE_LOOP('',(#63080,#63081,#63082,#63083));
#14189=EDGE_LOOP('',(#63084,#63085,#63086,#63087,#63088,#63089));
#14190=EDGE_LOOP('',(#63090,#63091,#63092,#63093));
#14191=EDGE_LOOP('',(#63094,#63095,#63096,#63097));
#14192=EDGE_LOOP('',(#63098,#63099,#63100,#63101));
#14193=EDGE_LOOP('',(#63102,#63103,#63104,#63105));
#14194=EDGE_LOOP('',(#63106,#63107,#63108,#63109));
#14195=EDGE_LOOP('',(#63110,#63111,#63112,#63113,#63114,#63115));
#14196=EDGE_LOOP('',(#63116,#63117,#63118,#63119));
#14197=EDGE_LOOP('',(#63120,#63121,#63122,#63123));
#14198=EDGE_LOOP('',(#63124,#63125,#63126,#63127,#63128,#63129));
#14199=EDGE_LOOP('',(#63130,#63131,#63132,#63133));
#14200=EDGE_LOOP('',(#63134,#63135,#63136,#63137));
#14201=EDGE_LOOP('',(#63138,#63139,#63140,#63141));
#14202=EDGE_LOOP('',(#63142,#63143,#63144,#63145));
#14203=EDGE_LOOP('',(#63146,#63147,#63148,#63149));
#14204=EDGE_LOOP('',(#63150,#63151,#63152,#63153,#63154,#63155));
#14205=EDGE_LOOP('',(#63156,#63157,#63158,#63159));
#14206=EDGE_LOOP('',(#63160,#63161,#63162,#63163));
#14207=EDGE_LOOP('',(#63164,#63165,#63166,#63167,#63168,#63169));
#14208=EDGE_LOOP('',(#63170,#63171,#63172,#63173));
#14209=EDGE_LOOP('',(#63174,#63175,#63176,#63177));
#14210=EDGE_LOOP('',(#63178,#63179,#63180,#63181));
#14211=EDGE_LOOP('',(#63182,#63183,#63184,#63185));
#14212=EDGE_LOOP('',(#63186,#63187,#63188,#63189));
#14213=EDGE_LOOP('',(#63190,#63191,#63192,#63193,#63194,#63195));
#14214=EDGE_LOOP('',(#63196,#63197,#63198,#63199));
#14215=EDGE_LOOP('',(#63200,#63201,#63202,#63203));
#14216=EDGE_LOOP('',(#63204,#63205,#63206,#63207,#63208,#63209));
#14217=EDGE_LOOP('',(#63210,#63211,#63212,#63213));
#14218=EDGE_LOOP('',(#63214,#63215,#63216,#63217));
#14219=EDGE_LOOP('',(#63218,#63219,#63220,#63221));
#14220=EDGE_LOOP('',(#63222,#63223,#63224,#63225));
#14221=EDGE_LOOP('',(#63226,#63227,#63228,#63229));
#14222=EDGE_LOOP('',(#63230,#63231,#63232,#63233,#63234,#63235));
#14223=EDGE_LOOP('',(#63236,#63237,#63238,#63239));
#14224=EDGE_LOOP('',(#63240,#63241,#63242,#63243));
#14225=EDGE_LOOP('',(#63244,#63245,#63246,#63247,#63248,#63249));
#14226=EDGE_LOOP('',(#63250,#63251,#63252,#63253));
#14227=EDGE_LOOP('',(#63254,#63255,#63256,#63257));
#14228=EDGE_LOOP('',(#63258,#63259,#63260,#63261));
#14229=EDGE_LOOP('',(#63262,#63263,#63264,#63265));
#14230=EDGE_LOOP('',(#63266,#63267,#63268,#63269));
#14231=EDGE_LOOP('',(#63270,#63271,#63272,#63273,#63274,#63275));
#14232=EDGE_LOOP('',(#63276,#63277,#63278,#63279));
#14233=EDGE_LOOP('',(#63280,#63281,#63282,#63283));
#14234=EDGE_LOOP('',(#63284,#63285,#63286,#63287,#63288,#63289));
#14235=EDGE_LOOP('',(#63290,#63291,#63292,#63293));
#14236=EDGE_LOOP('',(#63294,#63295,#63296,#63297));
#14237=EDGE_LOOP('',(#63298,#63299,#63300,#63301));
#14238=EDGE_LOOP('',(#63302,#63303,#63304,#63305));
#14239=EDGE_LOOP('',(#63306,#63307,#63308,#63309));
#14240=EDGE_LOOP('',(#63310,#63311,#63312,#63313,#63314,#63315));
#14241=EDGE_LOOP('',(#63316,#63317,#63318,#63319));
#14242=EDGE_LOOP('',(#63320,#63321,#63322,#63323));
#14243=EDGE_LOOP('',(#63324,#63325,#63326,#63327,#63328,#63329));
#14244=EDGE_LOOP('',(#63330,#63331,#63332,#63333));
#14245=EDGE_LOOP('',(#63334,#63335,#63336,#63337));
#14246=EDGE_LOOP('',(#63338,#63339,#63340,#63341));
#14247=EDGE_LOOP('',(#63342,#63343,#63344,#63345));
#14248=EDGE_LOOP('',(#63346,#63347,#63348,#63349));
#14249=EDGE_LOOP('',(#63350,#63351,#63352,#63353,#63354,#63355));
#14250=EDGE_LOOP('',(#63356,#63357,#63358,#63359));
#14251=EDGE_LOOP('',(#63360,#63361,#63362,#63363));
#14252=EDGE_LOOP('',(#63364,#63365,#63366,#63367,#63368,#63369));
#14253=EDGE_LOOP('',(#63370,#63371,#63372,#63373));
#14254=EDGE_LOOP('',(#63374,#63375,#63376,#63377));
#14255=EDGE_LOOP('',(#63378,#63379,#63380,#63381));
#14256=EDGE_LOOP('',(#63382,#63383,#63384,#63385));
#14257=EDGE_LOOP('',(#63386,#63387,#63388,#63389));
#14258=EDGE_LOOP('',(#63390,#63391,#63392,#63393,#63394,#63395));
#14259=EDGE_LOOP('',(#63396,#63397,#63398,#63399));
#14260=EDGE_LOOP('',(#63400,#63401,#63402,#63403));
#14261=EDGE_LOOP('',(#63404,#63405,#63406,#63407,#63408,#63409));
#14262=EDGE_LOOP('',(#63410,#63411,#63412,#63413));
#14263=EDGE_LOOP('',(#63414,#63415,#63416,#63417));
#14264=EDGE_LOOP('',(#63418,#63419,#63420,#63421));
#14265=EDGE_LOOP('',(#63422,#63423,#63424,#63425));
#14266=EDGE_LOOP('',(#63426,#63427,#63428,#63429));
#14267=EDGE_LOOP('',(#63430,#63431,#63432,#63433,#63434,#63435));
#14268=EDGE_LOOP('',(#63436,#63437,#63438,#63439));
#14269=EDGE_LOOP('',(#63440,#63441,#63442,#63443));
#14270=EDGE_LOOP('',(#63444,#63445,#63446,#63447,#63448,#63449));
#14271=EDGE_LOOP('',(#63450,#63451,#63452,#63453));
#14272=EDGE_LOOP('',(#63454,#63455,#63456,#63457));
#14273=EDGE_LOOP('',(#63458,#63459,#63460,#63461));
#14274=EDGE_LOOP('',(#63462,#63463,#63464,#63465));
#14275=EDGE_LOOP('',(#63466,#63467,#63468,#63469));
#14276=EDGE_LOOP('',(#63470,#63471,#63472,#63473,#63474,#63475));
#14277=EDGE_LOOP('',(#63476,#63477,#63478,#63479));
#14278=EDGE_LOOP('',(#63480,#63481,#63482,#63483));
#14279=EDGE_LOOP('',(#63484,#63485,#63486,#63487,#63488,#63489));
#14280=EDGE_LOOP('',(#63490,#63491,#63492,#63493));
#14281=EDGE_LOOP('',(#63494,#63495,#63496,#63497));
#14282=EDGE_LOOP('',(#63498,#63499,#63500,#63501));
#14283=EDGE_LOOP('',(#63502,#63503,#63504,#63505));
#14284=EDGE_LOOP('',(#63506,#63507,#63508,#63509));
#14285=EDGE_LOOP('',(#63510,#63511,#63512,#63513,#63514,#63515));
#14286=EDGE_LOOP('',(#63516,#63517,#63518,#63519));
#14287=EDGE_LOOP('',(#63520,#63521,#63522,#63523));
#14288=EDGE_LOOP('',(#63524,#63525,#63526,#63527,#63528,#63529));
#14289=EDGE_LOOP('',(#63530,#63531,#63532,#63533));
#14290=EDGE_LOOP('',(#63534,#63535,#63536,#63537));
#14291=EDGE_LOOP('',(#63538,#63539,#63540,#63541));
#14292=EDGE_LOOP('',(#63542,#63543,#63544,#63545));
#14293=EDGE_LOOP('',(#63546,#63547,#63548,#63549));
#14294=EDGE_LOOP('',(#63550,#63551,#63552,#63553,#63554,#63555));
#14295=EDGE_LOOP('',(#63556,#63557,#63558,#63559));
#14296=EDGE_LOOP('',(#63560,#63561,#63562,#63563));
#14297=EDGE_LOOP('',(#63564,#63565,#63566,#63567,#63568,#63569));
#14298=EDGE_LOOP('',(#63570,#63571,#63572,#63573));
#14299=EDGE_LOOP('',(#63574,#63575,#63576,#63577));
#14300=EDGE_LOOP('',(#63578,#63579,#63580,#63581));
#14301=EDGE_LOOP('',(#63582,#63583,#63584,#63585));
#14302=EDGE_LOOP('',(#63586,#63587,#63588,#63589));
#14303=EDGE_LOOP('',(#63590,#63591,#63592,#63593,#63594,#63595));
#14304=EDGE_LOOP('',(#63596,#63597,#63598,#63599));
#14305=EDGE_LOOP('',(#63600,#63601,#63602,#63603));
#14306=EDGE_LOOP('',(#63604,#63605,#63606,#63607,#63608,#63609));
#14307=EDGE_LOOP('',(#63610,#63611,#63612,#63613));
#14308=EDGE_LOOP('',(#63614,#63615,#63616,#63617));
#14309=EDGE_LOOP('',(#63618,#63619,#63620,#63621));
#14310=EDGE_LOOP('',(#63622,#63623,#63624,#63625));
#14311=EDGE_LOOP('',(#63626,#63627,#63628,#63629));
#14312=EDGE_LOOP('',(#63630,#63631,#63632,#63633,#63634,#63635));
#14313=EDGE_LOOP('',(#63636,#63637,#63638,#63639));
#14314=EDGE_LOOP('',(#63640,#63641,#63642,#63643));
#14315=EDGE_LOOP('',(#63644,#63645,#63646,#63647,#63648,#63649));
#14316=EDGE_LOOP('',(#63650,#63651,#63652,#63653));
#14317=EDGE_LOOP('',(#63654,#63655,#63656,#63657));
#14318=EDGE_LOOP('',(#63658,#63659,#63660,#63661));
#14319=EDGE_LOOP('',(#63662,#63663,#63664,#63665));
#14320=EDGE_LOOP('',(#63666,#63667,#63668,#63669));
#14321=EDGE_LOOP('',(#63670,#63671,#63672,#63673,#63674,#63675));
#14322=EDGE_LOOP('',(#63676,#63677,#63678,#63679));
#14323=EDGE_LOOP('',(#63680,#63681,#63682,#63683));
#14324=EDGE_LOOP('',(#63684,#63685,#63686,#63687,#63688,#63689));
#14325=EDGE_LOOP('',(#63690,#63691,#63692,#63693));
#14326=EDGE_LOOP('',(#63694,#63695,#63696,#63697));
#14327=EDGE_LOOP('',(#63698,#63699,#63700,#63701));
#14328=EDGE_LOOP('',(#63702,#63703,#63704,#63705));
#14329=EDGE_LOOP('',(#63706,#63707,#63708,#63709));
#14330=EDGE_LOOP('',(#63710,#63711,#63712,#63713,#63714,#63715));
#14331=EDGE_LOOP('',(#63716,#63717,#63718,#63719));
#14332=EDGE_LOOP('',(#63720,#63721,#63722,#63723));
#14333=EDGE_LOOP('',(#63724,#63725,#63726,#63727,#63728,#63729));
#14334=EDGE_LOOP('',(#63730,#63731,#63732,#63733));
#14335=EDGE_LOOP('',(#63734,#63735,#63736,#63737));
#14336=EDGE_LOOP('',(#63738,#63739,#63740,#63741));
#14337=EDGE_LOOP('',(#63742,#63743,#63744,#63745));
#14338=EDGE_LOOP('',(#63746,#63747,#63748,#63749));
#14339=EDGE_LOOP('',(#63750,#63751,#63752,#63753,#63754,#63755));
#14340=EDGE_LOOP('',(#63756,#63757,#63758,#63759));
#14341=EDGE_LOOP('',(#63760,#63761,#63762,#63763));
#14342=EDGE_LOOP('',(#63764,#63765,#63766,#63767,#63768,#63769));
#14343=EDGE_LOOP('',(#63770,#63771,#63772,#63773));
#14344=EDGE_LOOP('',(#63774,#63775,#63776,#63777));
#14345=EDGE_LOOP('',(#63778,#63779,#63780,#63781));
#14346=EDGE_LOOP('',(#63782,#63783,#63784,#63785));
#14347=EDGE_LOOP('',(#63786,#63787,#63788,#63789));
#14348=EDGE_LOOP('',(#63790,#63791,#63792,#63793,#63794,#63795));
#14349=EDGE_LOOP('',(#63796,#63797,#63798,#63799));
#14350=EDGE_LOOP('',(#63800,#63801,#63802,#63803));
#14351=EDGE_LOOP('',(#63804,#63805,#63806,#63807,#63808,#63809));
#14352=EDGE_LOOP('',(#63810,#63811,#63812,#63813));
#14353=EDGE_LOOP('',(#63814,#63815,#63816,#63817));
#14354=EDGE_LOOP('',(#63818,#63819,#63820,#63821));
#14355=EDGE_LOOP('',(#63822,#63823,#63824,#63825));
#14356=EDGE_LOOP('',(#63826,#63827,#63828,#63829));
#14357=EDGE_LOOP('',(#63830,#63831,#63832,#63833,#63834,#63835));
#14358=EDGE_LOOP('',(#63836,#63837,#63838,#63839));
#14359=EDGE_LOOP('',(#63840,#63841,#63842,#63843));
#14360=EDGE_LOOP('',(#63844,#63845,#63846,#63847,#63848,#63849));
#14361=EDGE_LOOP('',(#63850,#63851,#63852,#63853));
#14362=EDGE_LOOP('',(#63854,#63855,#63856,#63857));
#14363=EDGE_LOOP('',(#63858,#63859,#63860,#63861));
#14364=EDGE_LOOP('',(#63862,#63863,#63864,#63865));
#14365=EDGE_LOOP('',(#63866,#63867,#63868,#63869));
#14366=EDGE_LOOP('',(#63870,#63871,#63872,#63873,#63874,#63875));
#14367=EDGE_LOOP('',(#63876,#63877,#63878,#63879));
#14368=EDGE_LOOP('',(#63880,#63881,#63882,#63883));
#14369=EDGE_LOOP('',(#63884,#63885,#63886,#63887,#63888,#63889));
#14370=EDGE_LOOP('',(#63890,#63891,#63892,#63893));
#14371=EDGE_LOOP('',(#63894,#63895,#63896,#63897));
#14372=EDGE_LOOP('',(#63898,#63899,#63900,#63901));
#14373=EDGE_LOOP('',(#63902,#63903,#63904,#63905));
#14374=EDGE_LOOP('',(#63906,#63907,#63908,#63909));
#14375=EDGE_LOOP('',(#63910,#63911,#63912,#63913,#63914,#63915));
#14376=EDGE_LOOP('',(#63916,#63917,#63918,#63919));
#14377=EDGE_LOOP('',(#63920,#63921,#63922,#63923));
#14378=EDGE_LOOP('',(#63924,#63925,#63926,#63927,#63928,#63929));
#14379=EDGE_LOOP('',(#63930,#63931,#63932,#63933));
#14380=EDGE_LOOP('',(#63934,#63935,#63936,#63937));
#14381=EDGE_LOOP('',(#63938,#63939,#63940,#63941));
#14382=EDGE_LOOP('',(#63942,#63943,#63944,#63945));
#14383=EDGE_LOOP('',(#63946,#63947,#63948,#63949));
#14384=EDGE_LOOP('',(#63950,#63951,#63952,#63953,#63954,#63955));
#14385=EDGE_LOOP('',(#63956,#63957,#63958,#63959));
#14386=EDGE_LOOP('',(#63960,#63961,#63962,#63963));
#14387=EDGE_LOOP('',(#63964,#63965,#63966,#63967,#63968,#63969));
#14388=EDGE_LOOP('',(#63970,#63971,#63972,#63973));
#14389=EDGE_LOOP('',(#63974,#63975,#63976,#63977));
#14390=EDGE_LOOP('',(#63978,#63979,#63980,#63981));
#14391=EDGE_LOOP('',(#63982,#63983,#63984,#63985));
#14392=EDGE_LOOP('',(#63986,#63987,#63988,#63989));
#14393=EDGE_LOOP('',(#63990,#63991,#63992,#63993,#63994,#63995));
#14394=EDGE_LOOP('',(#63996,#63997,#63998,#63999));
#14395=EDGE_LOOP('',(#64000,#64001,#64002,#64003));
#14396=EDGE_LOOP('',(#64004,#64005,#64006,#64007,#64008,#64009));
#14397=EDGE_LOOP('',(#64010,#64011,#64012,#64013));
#14398=EDGE_LOOP('',(#64014,#64015,#64016,#64017));
#14399=EDGE_LOOP('',(#64018,#64019,#64020,#64021));
#14400=EDGE_LOOP('',(#64022,#64023,#64024,#64025));
#14401=EDGE_LOOP('',(#64026,#64027,#64028,#64029));
#14402=EDGE_LOOP('',(#64030,#64031,#64032,#64033,#64034,#64035));
#14403=EDGE_LOOP('',(#64036,#64037,#64038,#64039));
#14404=EDGE_LOOP('',(#64040,#64041,#64042,#64043));
#14405=EDGE_LOOP('',(#64044,#64045,#64046,#64047,#64048,#64049));
#14406=EDGE_LOOP('',(#64050,#64051,#64052,#64053));
#14407=EDGE_LOOP('',(#64054,#64055,#64056,#64057));
#14408=EDGE_LOOP('',(#64058,#64059,#64060,#64061));
#14409=EDGE_LOOP('',(#64062,#64063,#64064,#64065));
#14410=EDGE_LOOP('',(#64066,#64067,#64068,#64069));
#14411=EDGE_LOOP('',(#64070,#64071,#64072,#64073,#64074,#64075));
#14412=EDGE_LOOP('',(#64076,#64077,#64078,#64079));
#14413=EDGE_LOOP('',(#64080,#64081,#64082,#64083));
#14414=EDGE_LOOP('',(#64084,#64085,#64086,#64087,#64088,#64089));
#14415=EDGE_LOOP('',(#64090,#64091,#64092,#64093));
#14416=EDGE_LOOP('',(#64094,#64095,#64096,#64097));
#14417=EDGE_LOOP('',(#64098,#64099,#64100,#64101));
#14418=EDGE_LOOP('',(#64102,#64103,#64104,#64105));
#14419=EDGE_LOOP('',(#64106,#64107,#64108,#64109));
#14420=EDGE_LOOP('',(#64110,#64111,#64112,#64113,#64114,#64115));
#14421=EDGE_LOOP('',(#64116,#64117,#64118,#64119));
#14422=EDGE_LOOP('',(#64120,#64121,#64122,#64123));
#14423=EDGE_LOOP('',(#64124,#64125,#64126,#64127,#64128,#64129));
#14424=EDGE_LOOP('',(#64130,#64131,#64132,#64133));
#14425=EDGE_LOOP('',(#64134,#64135,#64136,#64137));
#14426=EDGE_LOOP('',(#64138,#64139,#64140,#64141));
#14427=EDGE_LOOP('',(#64142,#64143,#64144,#64145));
#14428=EDGE_LOOP('',(#64146,#64147,#64148,#64149));
#14429=EDGE_LOOP('',(#64150,#64151,#64152,#64153,#64154,#64155));
#14430=EDGE_LOOP('',(#64156,#64157,#64158,#64159));
#14431=EDGE_LOOP('',(#64160,#64161,#64162,#64163));
#14432=EDGE_LOOP('',(#64164,#64165,#64166,#64167,#64168,#64169));
#14433=EDGE_LOOP('',(#64170,#64171,#64172,#64173));
#14434=EDGE_LOOP('',(#64174,#64175,#64176,#64177));
#14435=EDGE_LOOP('',(#64178,#64179,#64180,#64181));
#14436=EDGE_LOOP('',(#64182,#64183,#64184,#64185));
#14437=EDGE_LOOP('',(#64186,#64187,#64188,#64189));
#14438=EDGE_LOOP('',(#64190,#64191,#64192,#64193,#64194,#64195));
#14439=EDGE_LOOP('',(#64196,#64197,#64198,#64199));
#14440=EDGE_LOOP('',(#64200,#64201,#64202,#64203));
#14441=EDGE_LOOP('',(#64204,#64205,#64206,#64207,#64208,#64209));
#14442=EDGE_LOOP('',(#64210,#64211,#64212,#64213));
#14443=EDGE_LOOP('',(#64214,#64215,#64216,#64217));
#14444=EDGE_LOOP('',(#64218,#64219,#64220,#64221));
#14445=EDGE_LOOP('',(#64222,#64223,#64224,#64225));
#14446=EDGE_LOOP('',(#64226,#64227,#64228,#64229));
#14447=EDGE_LOOP('',(#64230,#64231,#64232,#64233,#64234,#64235));
#14448=EDGE_LOOP('',(#64236,#64237,#64238,#64239));
#14449=EDGE_LOOP('',(#64240,#64241,#64242,#64243));
#14450=EDGE_LOOP('',(#64244,#64245,#64246,#64247,#64248,#64249));
#14451=EDGE_LOOP('',(#64250,#64251,#64252,#64253));
#14452=EDGE_LOOP('',(#64254,#64255,#64256,#64257));
#14453=EDGE_LOOP('',(#64258,#64259,#64260,#64261));
#14454=EDGE_LOOP('',(#64262,#64263,#64264,#64265));
#14455=EDGE_LOOP('',(#64266,#64267,#64268,#64269));
#14456=EDGE_LOOP('',(#64270,#64271,#64272,#64273,#64274,#64275));
#14457=EDGE_LOOP('',(#64276,#64277,#64278,#64279));
#14458=EDGE_LOOP('',(#64280,#64281,#64282,#64283));
#14459=EDGE_LOOP('',(#64284,#64285,#64286,#64287,#64288,#64289));
#14460=EDGE_LOOP('',(#64290,#64291,#64292,#64293));
#14461=EDGE_LOOP('',(#64294,#64295,#64296,#64297));
#14462=EDGE_LOOP('',(#64298,#64299,#64300,#64301));
#14463=EDGE_LOOP('',(#64302,#64303,#64304,#64305));
#14464=EDGE_LOOP('',(#64306,#64307,#64308,#64309));
#14465=EDGE_LOOP('',(#64310,#64311,#64312,#64313,#64314,#64315));
#14466=EDGE_LOOP('',(#64316,#64317,#64318,#64319));
#14467=EDGE_LOOP('',(#64320,#64321,#64322,#64323));
#14468=EDGE_LOOP('',(#64324,#64325,#64326,#64327,#64328,#64329));
#14469=EDGE_LOOP('',(#64330,#64331,#64332,#64333));
#14470=EDGE_LOOP('',(#64334,#64335,#64336,#64337));
#14471=EDGE_LOOP('',(#64338,#64339,#64340,#64341));
#14472=EDGE_LOOP('',(#64342,#64343,#64344,#64345));
#14473=EDGE_LOOP('',(#64346,#64347,#64348,#64349));
#14474=EDGE_LOOP('',(#64350));
#14475=EDGE_LOOP('',(#64351));
#14476=EDGE_LOOP('',(#64352,#64353,#64354,#64355,#64356,#64357));
#14477=EDGE_LOOP('',(#64358,#64359,#64360,#64361));
#14478=EDGE_LOOP('',(#64362,#64363,#64364,#64365));
#14479=EDGE_LOOP('',(#64366,#64367,#64368,#64369,#64370,#64371));
#14480=EDGE_LOOP('',(#64372,#64373,#64374,#64375));
#14481=EDGE_LOOP('',(#64376));
#14482=EDGE_LOOP('',(#64377));
#14483=EDGE_LOOP('',(#64378));
#14484=EDGE_LOOP('',(#64379));
#14485=EDGE_LOOP('',(#64380,#64381,#64382,#64383));
#14486=EDGE_LOOP('',(#64384,#64385,#64386,#64387));
#14487=EDGE_LOOP('',(#64388,#64389,#64390,#64391));
#14488=EDGE_LOOP('',(#64392,#64393,#64394,#64395));
#14489=EDGE_LOOP('',(#64396,#64397,#64398,#64399));
#14490=EDGE_LOOP('',(#64400,#64401,#64402,#64403,#64404,#64405,#64406,#64407,
#64408,#64409,#64410,#64411));
#14491=EDGE_LOOP('',(#64412,#64413,#64414,#64415,#64416,#64417,#64418,#64419,
#64420,#64421,#64422,#64423));
#14492=EDGE_LOOP('',(#64424,#64425,#64426,#64427));
#14493=EDGE_LOOP('',(#64428,#64429,#64430,#64431));
#14494=EDGE_LOOP('',(#64432,#64433,#64434,#64435));
#14495=EDGE_LOOP('',(#64436,#64437,#64438,#64439));
#14496=EDGE_LOOP('',(#64440,#64441,#64442,#64443,#64444));
#14497=EDGE_LOOP('',(#64445,#64446,#64447,#64448));
#14498=EDGE_LOOP('',(#64449,#64450,#64451,#64452));
#14499=EDGE_LOOP('',(#64453,#64454,#64455,#64456));
#14500=EDGE_LOOP('',(#64457,#64458,#64459,#64460));
#14501=EDGE_LOOP('',(#64461,#64462,#64463,#64464,#64465));
#14502=EDGE_LOOP('',(#64466,#64467,#64468,#64469));
#14503=EDGE_LOOP('',(#64470,#64471,#64472,#64473));
#14504=EDGE_LOOP('',(#64474,#64475,#64476,#64477));
#14505=EDGE_LOOP('',(#64478,#64479,#64480,#64481));
#14506=EDGE_LOOP('',(#64482,#64483,#64484,#64485));
#14507=EDGE_LOOP('',(#64486,#64487,#64488,#64489));
#14508=EDGE_LOOP('',(#64490,#64491,#64492,#64493));
#14509=EDGE_LOOP('',(#64494,#64495,#64496,#64497));
#14510=EDGE_LOOP('',(#64498,#64499,#64500,#64501));
#14511=EDGE_LOOP('',(#64502,#64503,#64504,#64505,#64506));
#14512=EDGE_LOOP('',(#64507,#64508,#64509,#64510,#64511));
#14513=EDGE_LOOP('',(#64512,#64513,#64514,#64515));
#14514=EDGE_LOOP('',(#64516,#64517,#64518,#64519));
#14515=EDGE_LOOP('',(#64520,#64521,#64522,#64523));
#14516=EDGE_LOOP('',(#64524,#64525,#64526,#64527));
#14517=EDGE_LOOP('',(#64528,#64529,#64530,#64531));
#14518=EDGE_LOOP('',(#64532,#64533,#64534,#64535));
#14519=EDGE_LOOP('',(#64536,#64537,#64538,#64539));
#14520=EDGE_LOOP('',(#64540,#64541,#64542,#64543));
#14521=EDGE_LOOP('',(#64544,#64545,#64546,#64547,#64548));
#14522=EDGE_LOOP('',(#64549,#64550,#64551,#64552));
#14523=EDGE_LOOP('',(#64553,#64554,#64555,#64556,#64557,#64558,#64559,#64560,
#64561,#64562,#64563,#64564));
#14524=EDGE_LOOP('',(#64565,#64566,#64567,#64568,#64569,#64570,#64571,#64572,
#64573,#64574,#64575,#64576));
#14525=EDGE_LOOP('',(#64577,#64578,#64579,#64580));
#14526=EDGE_LOOP('',(#64581,#64582,#64583,#64584,#64585,#64586,#64587,#64588,
#64589,#64590,#64591,#64592));
#14527=EDGE_LOOP('',(#64593,#64594,#64595,#64596,#64597,#64598,#64599,#64600,
#64601,#64602,#64603,#64604));
#14528=EDGE_LOOP('',(#64605,#64606,#64607,#64608));
#14529=EDGE_LOOP('',(#64609,#64610,#64611,#64612,#64613,#64614,#64615,#64616,
#64617,#64618,#64619,#64620));
#14530=EDGE_LOOP('',(#64621,#64622,#64623,#64624,#64625,#64626,#64627,#64628,
#64629,#64630,#64631,#64632));
#14531=EDGE_LOOP('',(#64633,#64634,#64635,#64636));
#14532=EDGE_LOOP('',(#64637,#64638,#64639,#64640,#64641,#64642,#64643,#64644,
#64645,#64646,#64647,#64648));
#14533=EDGE_LOOP('',(#64649,#64650,#64651,#64652,#64653,#64654,#64655,#64656,
#64657,#64658,#64659,#64660));
#14534=EDGE_LOOP('',(#64661,#64662,#64663,#64664));
#14535=EDGE_LOOP('',(#64665,#64666,#64667,#64668,#64669,#64670,#64671,#64672,
#64673,#64674,#64675,#64676));
#14536=EDGE_LOOP('',(#64677,#64678,#64679,#64680,#64681,#64682,#64683,#64684,
#64685,#64686,#64687,#64688));
#14537=EDGE_LOOP('',(#64689,#64690,#64691,#64692));
#14538=EDGE_LOOP('',(#64693,#64694,#64695,#64696,#64697,#64698,#64699,#64700,
#64701,#64702,#64703,#64704));
#14539=EDGE_LOOP('',(#64705,#64706,#64707,#64708,#64709,#64710,#64711,#64712,
#64713,#64714,#64715,#64716));
#14540=EDGE_LOOP('',(#64717,#64718,#64719,#64720));
#14541=EDGE_LOOP('',(#64721,#64722,#64723,#64724,#64725,#64726,#64727,#64728,
#64729,#64730,#64731,#64732));
#14542=EDGE_LOOP('',(#64733,#64734,#64735,#64736,#64737,#64738,#64739,#64740,
#64741,#64742,#64743,#64744));
#14543=EDGE_LOOP('',(#64745,#64746,#64747,#64748));
#14544=EDGE_LOOP('',(#64749,#64750,#64751,#64752,#64753,#64754,#64755,#64756,
#64757,#64758,#64759,#64760));
#14545=EDGE_LOOP('',(#64761,#64762,#64763,#64764,#64765,#64766,#64767,#64768,
#64769,#64770,#64771,#64772));
#14546=EDGE_LOOP('',(#64773,#64774,#64775,#64776));
#14547=EDGE_LOOP('',(#64777,#64778,#64779,#64780,#64781,#64782,#64783,#64784,
#64785,#64786,#64787,#64788));
#14548=EDGE_LOOP('',(#64789,#64790,#64791,#64792,#64793,#64794,#64795,#64796,
#64797,#64798,#64799,#64800));
#14549=EDGE_LOOP('',(#64801,#64802,#64803,#64804));
#14550=EDGE_LOOP('',(#64805,#64806,#64807,#64808,#64809,#64810,#64811,#64812,
#64813,#64814,#64815,#64816));
#14551=EDGE_LOOP('',(#64817,#64818,#64819,#64820,#64821,#64822,#64823,#64824,
#64825,#64826,#64827,#64828));
#14552=EDGE_LOOP('',(#64829,#64830,#64831,#64832));
#14553=EDGE_LOOP('',(#64833,#64834,#64835,#64836,#64837,#64838,#64839,#64840,
#64841,#64842,#64843,#64844));
#14554=EDGE_LOOP('',(#64845,#64846,#64847,#64848,#64849,#64850,#64851,#64852,
#64853,#64854,#64855,#64856));
#14555=EDGE_LOOP('',(#64857,#64858,#64859,#64860));
#14556=EDGE_LOOP('',(#64861,#64862,#64863,#64864,#64865,#64866,#64867,#64868,
#64869,#64870,#64871,#64872));
#14557=EDGE_LOOP('',(#64873,#64874,#64875,#64876,#64877,#64878,#64879,#64880,
#64881,#64882,#64883,#64884));
#14558=EDGE_LOOP('',(#64885,#64886,#64887,#64888));
#14559=EDGE_LOOP('',(#64889,#64890,#64891,#64892,#64893,#64894,#64895,#64896,
#64897,#64898,#64899,#64900));
#14560=EDGE_LOOP('',(#64901,#64902,#64903,#64904,#64905,#64906,#64907,#64908,
#64909,#64910,#64911,#64912));
#14561=EDGE_LOOP('',(#64913,#64914,#64915,#64916));
#14562=EDGE_LOOP('',(#64917,#64918,#64919,#64920,#64921,#64922,#64923,#64924,
#64925,#64926,#64927,#64928));
#14563=EDGE_LOOP('',(#64929,#64930,#64931,#64932,#64933,#64934,#64935,#64936,
#64937,#64938,#64939,#64940));
#14564=EDGE_LOOP('',(#64941,#64942,#64943,#64944));
#14565=EDGE_LOOP('',(#64945,#64946,#64947,#64948,#64949,#64950,#64951,#64952,
#64953,#64954,#64955,#64956));
#14566=EDGE_LOOP('',(#64957,#64958,#64959,#64960,#64961,#64962,#64963,#64964,
#64965,#64966,#64967,#64968));
#14567=EDGE_LOOP('',(#64969,#64970,#64971,#64972));
#14568=EDGE_LOOP('',(#64973,#64974,#64975,#64976,#64977,#64978,#64979,#64980,
#64981,#64982,#64983,#64984));
#14569=EDGE_LOOP('',(#64985,#64986,#64987,#64988,#64989,#64990,#64991,#64992,
#64993,#64994,#64995,#64996));
#14570=EDGE_LOOP('',(#64997,#64998,#64999,#65000));
#14571=EDGE_LOOP('',(#65001,#65002,#65003,#65004,#65005,#65006,#65007,#65008,
#65009,#65010,#65011,#65012));
#14572=EDGE_LOOP('',(#65013,#65014,#65015,#65016,#65017,#65018,#65019,#65020,
#65021,#65022,#65023,#65024));
#14573=EDGE_LOOP('',(#65025,#65026,#65027,#65028));
#14574=EDGE_LOOP('',(#65029,#65030,#65031,#65032,#65033,#65034,#65035,#65036,
#65037,#65038,#65039,#65040));
#14575=EDGE_LOOP('',(#65041,#65042,#65043,#65044,#65045,#65046,#65047,#65048,
#65049,#65050,#65051,#65052));
#14576=EDGE_LOOP('',(#65053,#65054,#65055,#65056));
#14577=EDGE_LOOP('',(#65057,#65058,#65059,#65060,#65061,#65062,#65063,#65064,
#65065,#65066,#65067,#65068));
#14578=EDGE_LOOP('',(#65069,#65070,#65071,#65072,#65073,#65074,#65075,#65076,
#65077,#65078,#65079,#65080));
#14579=EDGE_LOOP('',(#65081,#65082,#65083,#65084));
#14580=EDGE_LOOP('',(#65085,#65086,#65087,#65088,#65089,#65090,#65091,#65092,
#65093,#65094,#65095,#65096));
#14581=EDGE_LOOP('',(#65097,#65098,#65099,#65100,#65101,#65102,#65103,#65104,
#65105,#65106,#65107,#65108));
#14582=EDGE_LOOP('',(#65109,#65110,#65111,#65112));
#14583=EDGE_LOOP('',(#65113,#65114,#65115,#65116,#65117,#65118,#65119,#65120,
#65121,#65122,#65123,#65124));
#14584=EDGE_LOOP('',(#65125,#65126,#65127,#65128,#65129,#65130,#65131,#65132,
#65133,#65134,#65135,#65136));
#14585=EDGE_LOOP('',(#65137,#65138,#65139,#65140));
#14586=EDGE_LOOP('',(#65141,#65142,#65143,#65144,#65145,#65146,#65147,#65148,
#65149,#65150,#65151,#65152));
#14587=EDGE_LOOP('',(#65153,#65154,#65155,#65156,#65157,#65158,#65159,#65160,
#65161,#65162,#65163,#65164));
#14588=EDGE_LOOP('',(#65165,#65166,#65167,#65168));
#14589=EDGE_LOOP('',(#65169,#65170,#65171,#65172,#65173,#65174,#65175,#65176,
#65177,#65178,#65179,#65180));
#14590=EDGE_LOOP('',(#65181,#65182,#65183,#65184,#65185,#65186,#65187,#65188,
#65189,#65190,#65191,#65192));
#14591=EDGE_LOOP('',(#65193,#65194,#65195,#65196));
#14592=EDGE_LOOP('',(#65197,#65198,#65199,#65200,#65201,#65202,#65203,#65204,
#65205,#65206,#65207,#65208));
#14593=EDGE_LOOP('',(#65209,#65210,#65211,#65212,#65213,#65214,#65215,#65216,
#65217,#65218,#65219,#65220));
#14594=EDGE_LOOP('',(#65221,#65222,#65223,#65224));
#14595=EDGE_LOOP('',(#65225,#65226,#65227,#65228,#65229,#65230,#65231,#65232,
#65233,#65234,#65235,#65236));
#14596=EDGE_LOOP('',(#65237,#65238,#65239,#65240,#65241,#65242,#65243,#65244,
#65245,#65246,#65247,#65248));
#14597=EDGE_LOOP('',(#65249,#65250,#65251,#65252));
#14598=EDGE_LOOP('',(#65253,#65254,#65255,#65256,#65257,#65258,#65259,#65260,
#65261,#65262,#65263,#65264));
#14599=EDGE_LOOP('',(#65265,#65266,#65267,#65268,#65269,#65270,#65271,#65272,
#65273,#65274,#65275,#65276));
#14600=EDGE_LOOP('',(#65277,#65278,#65279,#65280));
#14601=EDGE_LOOP('',(#65281,#65282,#65283,#65284,#65285,#65286,#65287,#65288,
#65289,#65290,#65291,#65292));
#14602=EDGE_LOOP('',(#65293,#65294,#65295,#65296,#65297,#65298,#65299,#65300,
#65301,#65302,#65303,#65304));
#14603=EDGE_LOOP('',(#65305,#65306,#65307,#65308));
#14604=EDGE_LOOP('',(#65309,#65310,#65311,#65312,#65313,#65314,#65315,#65316,
#65317,#65318,#65319,#65320));
#14605=EDGE_LOOP('',(#65321,#65322,#65323,#65324,#65325,#65326,#65327,#65328,
#65329,#65330,#65331,#65332));
#14606=EDGE_LOOP('',(#65333,#65334,#65335,#65336));
#14607=EDGE_LOOP('',(#65337,#65338,#65339,#65340,#65341,#65342,#65343,#65344,
#65345,#65346,#65347,#65348));
#14608=EDGE_LOOP('',(#65349,#65350,#65351,#65352,#65353,#65354,#65355,#65356,
#65357,#65358,#65359,#65360));
#14609=EDGE_LOOP('',(#65361,#65362,#65363,#65364));
#14610=EDGE_LOOP('',(#65365,#65366,#65367,#65368,#65369,#65370,#65371,#65372,
#65373,#65374,#65375,#65376));
#14611=EDGE_LOOP('',(#65377,#65378,#65379,#65380,#65381,#65382,#65383,#65384,
#65385,#65386,#65387,#65388));
#14612=EDGE_LOOP('',(#65389,#65390,#65391,#65392));
#14613=EDGE_LOOP('',(#65393,#65394,#65395,#65396,#65397,#65398,#65399,#65400,
#65401,#65402,#65403,#65404));
#14614=EDGE_LOOP('',(#65405,#65406,#65407,#65408,#65409,#65410,#65411,#65412,
#65413,#65414,#65415,#65416));
#14615=EDGE_LOOP('',(#65417,#65418,#65419,#65420));
#14616=EDGE_LOOP('',(#65421,#65422,#65423,#65424,#65425,#65426,#65427,#65428,
#65429,#65430,#65431,#65432));
#14617=EDGE_LOOP('',(#65433,#65434,#65435,#65436,#65437,#65438,#65439,#65440,
#65441,#65442,#65443,#65444));
#14618=EDGE_LOOP('',(#65445,#65446,#65447,#65448));
#14619=EDGE_LOOP('',(#65449,#65450,#65451,#65452,#65453,#65454,#65455,#65456,
#65457,#65458,#65459,#65460));
#14620=EDGE_LOOP('',(#65461,#65462,#65463,#65464,#65465,#65466,#65467,#65468,
#65469,#65470,#65471,#65472));
#14621=EDGE_LOOP('',(#65473,#65474,#65475,#65476));
#14622=EDGE_LOOP('',(#65477,#65478,#65479,#65480,#65481,#65482,#65483,#65484,
#65485,#65486,#65487,#65488));
#14623=EDGE_LOOP('',(#65489,#65490,#65491,#65492,#65493,#65494,#65495,#65496,
#65497,#65498,#65499,#65500));
#14624=EDGE_LOOP('',(#65501,#65502,#65503,#65504));
#14625=EDGE_LOOP('',(#65505,#65506,#65507,#65508,#65509,#65510,#65511,#65512,
#65513,#65514,#65515,#65516));
#14626=EDGE_LOOP('',(#65517,#65518,#65519,#65520,#65521,#65522,#65523,#65524,
#65525,#65526,#65527,#65528));
#14627=EDGE_LOOP('',(#65529,#65530,#65531,#65532));
#14628=EDGE_LOOP('',(#65533,#65534,#65535,#65536,#65537,#65538,#65539,#65540,
#65541,#65542,#65543,#65544));
#14629=EDGE_LOOP('',(#65545,#65546,#65547,#65548,#65549,#65550,#65551,#65552,
#65553,#65554,#65555,#65556));
#14630=EDGE_LOOP('',(#65557,#65558,#65559,#65560));
#14631=EDGE_LOOP('',(#65561,#65562,#65563,#65564,#65565,#65566,#65567,#65568,
#65569,#65570,#65571,#65572));
#14632=EDGE_LOOP('',(#65573,#65574,#65575,#65576,#65577,#65578,#65579,#65580,
#65581,#65582,#65583,#65584));
#14633=EDGE_LOOP('',(#65585,#65586,#65587,#65588));
#14634=EDGE_LOOP('',(#65589,#65590,#65591,#65592,#65593,#65594,#65595,#65596,
#65597,#65598,#65599,#65600));
#14635=EDGE_LOOP('',(#65601,#65602,#65603,#65604,#65605,#65606,#65607,#65608,
#65609,#65610,#65611,#65612));
#14636=EDGE_LOOP('',(#65613,#65614,#65615,#65616));
#14637=EDGE_LOOP('',(#65617,#65618,#65619,#65620,#65621,#65622,#65623,#65624,
#65625,#65626,#65627,#65628));
#14638=EDGE_LOOP('',(#65629,#65630,#65631,#65632,#65633,#65634,#65635,#65636,
#65637,#65638,#65639,#65640));
#14639=EDGE_LOOP('',(#65641,#65642,#65643,#65644));
#14640=EDGE_LOOP('',(#65645,#65646,#65647,#65648,#65649,#65650,#65651,#65652,
#65653,#65654,#65655,#65656));
#14641=EDGE_LOOP('',(#65657,#65658,#65659,#65660,#65661,#65662,#65663,#65664,
#65665,#65666,#65667,#65668));
#14642=EDGE_LOOP('',(#65669,#65670,#65671,#65672));
#14643=EDGE_LOOP('',(#65673,#65674,#65675,#65676,#65677,#65678,#65679,#65680,
#65681,#65682,#65683,#65684));
#14644=EDGE_LOOP('',(#65685,#65686,#65687,#65688,#65689,#65690,#65691,#65692,
#65693,#65694,#65695,#65696));
#14645=EDGE_LOOP('',(#65697,#65698,#65699,#65700));
#14646=EDGE_LOOP('',(#65701,#65702,#65703,#65704,#65705,#65706,#65707,#65708,
#65709,#65710,#65711,#65712));
#14647=EDGE_LOOP('',(#65713,#65714,#65715,#65716,#65717,#65718,#65719,#65720,
#65721,#65722,#65723,#65724));
#14648=EDGE_LOOP('',(#65725,#65726,#65727,#65728));
#14649=EDGE_LOOP('',(#65729,#65730,#65731,#65732,#65733,#65734,#65735,#65736,
#65737,#65738,#65739,#65740));
#14650=EDGE_LOOP('',(#65741,#65742,#65743,#65744,#65745,#65746,#65747,#65748,
#65749,#65750,#65751,#65752));
#14651=EDGE_LOOP('',(#65753,#65754,#65755,#65756));
#14652=EDGE_LOOP('',(#65757,#65758,#65759,#65760,#65761,#65762,#65763,#65764,
#65765,#65766,#65767,#65768));
#14653=EDGE_LOOP('',(#65769,#65770,#65771,#65772,#65773,#65774,#65775,#65776,
#65777,#65778,#65779,#65780));
#14654=EDGE_LOOP('',(#65781,#65782,#65783,#65784));
#14655=EDGE_LOOP('',(#65785,#65786,#65787,#65788,#65789,#65790,#65791,#65792,
#65793,#65794,#65795,#65796));
#14656=EDGE_LOOP('',(#65797,#65798,#65799,#65800,#65801,#65802,#65803,#65804,
#65805,#65806,#65807,#65808));
#14657=EDGE_LOOP('',(#65809,#65810,#65811,#65812));
#14658=EDGE_LOOP('',(#65813,#65814,#65815,#65816,#65817,#65818,#65819,#65820,
#65821,#65822,#65823,#65824));
#14659=EDGE_LOOP('',(#65825,#65826,#65827,#65828,#65829,#65830,#65831,#65832,
#65833,#65834,#65835,#65836));
#14660=EDGE_LOOP('',(#65837,#65838,#65839,#65840));
#14661=EDGE_LOOP('',(#65841,#65842,#65843,#65844,#65845,#65846,#65847,#65848,
#65849,#65850,#65851,#65852));
#14662=EDGE_LOOP('',(#65853,#65854,#65855,#65856,#65857,#65858,#65859,#65860,
#65861,#65862,#65863,#65864));
#14663=EDGE_LOOP('',(#65865,#65866,#65867,#65868));
#14664=EDGE_LOOP('',(#65869,#65870,#65871,#65872,#65873,#65874,#65875,#65876,
#65877,#65878,#65879,#65880));
#14665=EDGE_LOOP('',(#65881,#65882,#65883,#65884,#65885,#65886,#65887,#65888,
#65889,#65890,#65891,#65892));
#14666=EDGE_LOOP('',(#65893,#65894,#65895,#65896));
#14667=EDGE_LOOP('',(#65897,#65898,#65899,#65900,#65901,#65902,#65903,#65904,
#65905,#65906,#65907,#65908));
#14668=EDGE_LOOP('',(#65909,#65910,#65911,#65912,#65913,#65914,#65915,#65916,
#65917,#65918,#65919,#65920));
#14669=EDGE_LOOP('',(#65921,#65922,#65923,#65924));
#14670=EDGE_LOOP('',(#65925,#65926,#65927,#65928,#65929,#65930,#65931,#65932,
#65933,#65934,#65935,#65936));
#14671=EDGE_LOOP('',(#65937,#65938,#65939,#65940,#65941,#65942,#65943,#65944,
#65945,#65946,#65947,#65948));
#14672=EDGE_LOOP('',(#65949,#65950,#65951,#65952));
#14673=EDGE_LOOP('',(#65953,#65954,#65955,#65956,#65957,#65958,#65959,#65960,
#65961,#65962,#65963,#65964));
#14674=EDGE_LOOP('',(#65965,#65966,#65967,#65968,#65969,#65970,#65971,#65972,
#65973,#65974,#65975,#65976));
#14675=EDGE_LOOP('',(#65977,#65978,#65979,#65980));
#14676=EDGE_LOOP('',(#65981,#65982,#65983,#65984,#65985,#65986,#65987,#65988,
#65989,#65990,#65991,#65992));
#14677=EDGE_LOOP('',(#65993,#65994,#65995,#65996,#65997,#65998,#65999,#66000,
#66001,#66002,#66003,#66004));
#14678=EDGE_LOOP('',(#66005,#66006,#66007,#66008));
#14679=EDGE_LOOP('',(#66009,#66010,#66011,#66012,#66013,#66014,#66015,#66016,
#66017,#66018,#66019,#66020));
#14680=EDGE_LOOP('',(#66021,#66022,#66023,#66024,#66025,#66026,#66027,#66028,
#66029,#66030,#66031,#66032));
#14681=EDGE_LOOP('',(#66033,#66034,#66035,#66036));
#14682=EDGE_LOOP('',(#66037,#66038,#66039,#66040,#66041,#66042,#66043,#66044,
#66045,#66046,#66047,#66048));
#14683=EDGE_LOOP('',(#66049,#66050,#66051,#66052,#66053,#66054,#66055,#66056,
#66057,#66058,#66059,#66060));
#14684=EDGE_LOOP('',(#66061,#66062,#66063,#66064));
#14685=EDGE_LOOP('',(#66065,#66066,#66067,#66068,#66069,#66070,#66071,#66072,
#66073,#66074,#66075,#66076));
#14686=EDGE_LOOP('',(#66077,#66078,#66079,#66080,#66081,#66082,#66083,#66084,
#66085,#66086,#66087,#66088));
#14687=EDGE_LOOP('',(#66089,#66090,#66091,#66092));
#14688=EDGE_LOOP('',(#66093,#66094,#66095,#66096,#66097,#66098,#66099,#66100,
#66101,#66102,#66103,#66104));
#14689=EDGE_LOOP('',(#66105,#66106,#66107,#66108,#66109,#66110,#66111,#66112,
#66113,#66114,#66115,#66116));
#14690=EDGE_LOOP('',(#66117,#66118,#66119,#66120));
#14691=EDGE_LOOP('',(#66121,#66122,#66123,#66124,#66125,#66126,#66127,#66128,
#66129,#66130,#66131,#66132));
#14692=EDGE_LOOP('',(#66133,#66134,#66135,#66136,#66137,#66138,#66139,#66140,
#66141,#66142,#66143,#66144));
#14693=EDGE_LOOP('',(#66145,#66146,#66147,#66148));
#14694=EDGE_LOOP('',(#66149,#66150,#66151,#66152,#66153,#66154,#66155,#66156,
#66157,#66158,#66159,#66160));
#14695=EDGE_LOOP('',(#66161,#66162,#66163,#66164,#66165,#66166,#66167,#66168,
#66169,#66170,#66171,#66172));
#14696=EDGE_LOOP('',(#66173,#66174,#66175,#66176));
#14697=EDGE_LOOP('',(#66177,#66178,#66179,#66180,#66181,#66182,#66183,#66184,
#66185,#66186,#66187,#66188));
#14698=EDGE_LOOP('',(#66189,#66190,#66191,#66192,#66193,#66194,#66195,#66196,
#66197,#66198,#66199,#66200));
#14699=EDGE_LOOP('',(#66201,#66202,#66203,#66204));
#14700=EDGE_LOOP('',(#66205,#66206,#66207,#66208));
#14701=EDGE_LOOP('',(#66209,#66210,#66211,#66212));
#14702=EDGE_LOOP('',(#66213,#66214,#66215,#66216));
#14703=EDGE_LOOP('',(#66217,#66218,#66219,#66220));
#14704=EDGE_LOOP('',(#66221,#66222,#66223,#66224));
#14705=EDGE_LOOP('',(#66225,#66226,#66227,#66228));
#14706=EDGE_LOOP('',(#66229,#66230,#66231,#66232));
#14707=EDGE_LOOP('',(#66233,#66234,#66235,#66236));
#14708=EDGE_LOOP('',(#66237,#66238,#66239,#66240));
#14709=EDGE_LOOP('',(#66241,#66242,#66243,#66244));
#14710=EDGE_LOOP('',(#66245,#66246,#66247,#66248));
#14711=EDGE_LOOP('',(#66249,#66250,#66251,#66252));
#14712=EDGE_LOOP('',(#66253,#66254,#66255,#66256));
#14713=EDGE_LOOP('',(#66257,#66258,#66259,#66260));
#14714=EDGE_LOOP('',(#66261,#66262,#66263,#66264));
#14715=EDGE_LOOP('',(#66265,#66266,#66267,#66268));
#14716=EDGE_LOOP('',(#66269,#66270,#66271,#66272));
#14717=EDGE_LOOP('',(#66273,#66274,#66275,#66276));
#14718=EDGE_LOOP('',(#66277,#66278,#66279,#66280));
#14719=EDGE_LOOP('',(#66281,#66282,#66283,#66284));
#14720=EDGE_LOOP('',(#66285,#66286,#66287,#66288));
#14721=EDGE_LOOP('',(#66289,#66290,#66291,#66292));
#14722=EDGE_LOOP('',(#66293,#66294,#66295,#66296));
#14723=EDGE_LOOP('',(#66297,#66298,#66299,#66300));
#14724=EDGE_LOOP('',(#66301,#66302,#66303,#66304));
#14725=EDGE_LOOP('',(#66305,#66306,#66307,#66308));
#14726=EDGE_LOOP('',(#66309,#66310,#66311,#66312));
#14727=EDGE_LOOP('',(#66313,#66314,#66315,#66316));
#14728=EDGE_LOOP('',(#66317,#66318,#66319,#66320));
#14729=EDGE_LOOP('',(#66321,#66322,#66323,#66324));
#14730=EDGE_LOOP('',(#66325,#66326,#66327,#66328));
#14731=EDGE_LOOP('',(#66329,#66330,#66331,#66332));
#14732=EDGE_LOOP('',(#66333,#66334,#66335,#66336));
#14733=EDGE_LOOP('',(#66337,#66338,#66339,#66340));
#14734=EDGE_LOOP('',(#66341,#66342,#66343,#66344));
#14735=EDGE_LOOP('',(#66345,#66346,#66347,#66348));
#14736=EDGE_LOOP('',(#66349,#66350,#66351,#66352));
#14737=EDGE_LOOP('',(#66353,#66354,#66355,#66356));
#14738=EDGE_LOOP('',(#66357,#66358,#66359,#66360));
#14739=EDGE_LOOP('',(#66361,#66362,#66363,#66364));
#14740=EDGE_LOOP('',(#66365,#66366,#66367,#66368));
#14741=EDGE_LOOP('',(#66369,#66370,#66371,#66372));
#14742=EDGE_LOOP('',(#66373,#66374,#66375,#66376));
#14743=EDGE_LOOP('',(#66377,#66378,#66379,#66380));
#14744=EDGE_LOOP('',(#66381,#66382,#66383,#66384));
#14745=EDGE_LOOP('',(#66385,#66386,#66387,#66388));
#14746=EDGE_LOOP('',(#66389,#66390,#66391,#66392));
#14747=EDGE_LOOP('',(#66393,#66394,#66395,#66396));
#14748=EDGE_LOOP('',(#66397,#66398,#66399,#66400));
#14749=EDGE_LOOP('',(#66401,#66402,#66403,#66404));
#14750=EDGE_LOOP('',(#66405,#66406,#66407,#66408));
#14751=EDGE_LOOP('',(#66409,#66410,#66411,#66412));
#14752=EDGE_LOOP('',(#66413,#66414,#66415,#66416));
#14753=EDGE_LOOP('',(#66417,#66418,#66419,#66420));
#14754=EDGE_LOOP('',(#66421,#66422,#66423,#66424));
#14755=EDGE_LOOP('',(#66425,#66426,#66427,#66428));
#14756=EDGE_LOOP('',(#66429,#66430,#66431,#66432));
#14757=EDGE_LOOP('',(#66433,#66434,#66435,#66436));
#14758=EDGE_LOOP('',(#66437,#66438,#66439,#66440));
#14759=EDGE_LOOP('',(#66441,#66442,#66443,#66444));
#14760=EDGE_LOOP('',(#66445,#66446,#66447,#66448));
#14761=EDGE_LOOP('',(#66449,#66450,#66451,#66452));
#14762=EDGE_LOOP('',(#66453,#66454,#66455,#66456));
#14763=EDGE_LOOP('',(#66457,#66458,#66459,#66460));
#14764=EDGE_LOOP('',(#66461,#66462,#66463,#66464));
#14765=EDGE_LOOP('',(#66465,#66466,#66467,#66468));
#14766=EDGE_LOOP('',(#66469,#66470,#66471,#66472));
#14767=EDGE_LOOP('',(#66473,#66474,#66475,#66476));
#14768=EDGE_LOOP('',(#66477,#66478,#66479,#66480));
#14769=EDGE_LOOP('',(#66481,#66482,#66483,#66484));
#14770=EDGE_LOOP('',(#66485,#66486,#66487,#66488));
#14771=EDGE_LOOP('',(#66489,#66490,#66491,#66492));
#14772=EDGE_LOOP('',(#66493,#66494,#66495,#66496));
#14773=EDGE_LOOP('',(#66497,#66498,#66499,#66500));
#14774=EDGE_LOOP('',(#66501,#66502,#66503,#66504));
#14775=EDGE_LOOP('',(#66505,#66506,#66507,#66508));
#14776=EDGE_LOOP('',(#66509,#66510,#66511,#66512));
#14777=EDGE_LOOP('',(#66513,#66514,#66515,#66516));
#14778=EDGE_LOOP('',(#66517,#66518,#66519,#66520));
#14779=EDGE_LOOP('',(#66521,#66522,#66523,#66524));
#14780=EDGE_LOOP('',(#66525,#66526,#66527,#66528));
#14781=EDGE_LOOP('',(#66529,#66530,#66531,#66532));
#14782=EDGE_LOOP('',(#66533,#66534,#66535,#66536));
#14783=EDGE_LOOP('',(#66537,#66538,#66539,#66540));
#14784=EDGE_LOOP('',(#66541,#66542,#66543,#66544));
#14785=EDGE_LOOP('',(#66545,#66546,#66547,#66548));
#14786=EDGE_LOOP('',(#66549,#66550,#66551,#66552));
#14787=EDGE_LOOP('',(#66553,#66554,#66555,#66556));
#14788=EDGE_LOOP('',(#66557,#66558,#66559,#66560));
#14789=EDGE_LOOP('',(#66561,#66562,#66563,#66564));
#14790=EDGE_LOOP('',(#66565,#66566,#66567,#66568));
#14791=EDGE_LOOP('',(#66569,#66570,#66571,#66572));
#14792=EDGE_LOOP('',(#66573,#66574,#66575,#66576));
#14793=EDGE_LOOP('',(#66577,#66578,#66579,#66580));
#14794=EDGE_LOOP('',(#66581,#66582,#66583,#66584));
#14795=EDGE_LOOP('',(#66585,#66586,#66587,#66588));
#14796=EDGE_LOOP('',(#66589,#66590,#66591,#66592));
#14797=EDGE_LOOP('',(#66593,#66594,#66595,#66596));
#14798=EDGE_LOOP('',(#66597,#66598,#66599,#66600));
#14799=EDGE_LOOP('',(#66601,#66602,#66603,#66604));
#14800=EDGE_LOOP('',(#66605,#66606,#66607,#66608));
#14801=EDGE_LOOP('',(#66609,#66610,#66611,#66612));
#14802=EDGE_LOOP('',(#66613,#66614,#66615,#66616));
#14803=EDGE_LOOP('',(#66617,#66618,#66619,#66620));
#14804=EDGE_LOOP('',(#66621,#66622,#66623,#66624));
#14805=EDGE_LOOP('',(#66625,#66626,#66627,#66628));
#14806=EDGE_LOOP('',(#66629,#66630,#66631,#66632));
#14807=EDGE_LOOP('',(#66633,#66634,#66635,#66636));
#14808=EDGE_LOOP('',(#66637,#66638,#66639,#66640));
#14809=EDGE_LOOP('',(#66641,#66642,#66643,#66644));
#14810=EDGE_LOOP('',(#66645,#66646,#66647,#66648));
#14811=EDGE_LOOP('',(#66649,#66650,#66651,#66652));
#14812=EDGE_LOOP('',(#66653,#66654,#66655,#66656));
#14813=EDGE_LOOP('',(#66657,#66658,#66659,#66660));
#14814=EDGE_LOOP('',(#66661,#66662,#66663,#66664));
#14815=EDGE_LOOP('',(#66665,#66666,#66667,#66668));
#14816=EDGE_LOOP('',(#66669,#66670,#66671,#66672));
#14817=EDGE_LOOP('',(#66673,#66674,#66675,#66676));
#14818=EDGE_LOOP('',(#66677,#66678,#66679,#66680));
#14819=EDGE_LOOP('',(#66681,#66682,#66683,#66684,#66685));
#14820=EDGE_LOOP('',(#66686,#66687,#66688,#66689));
#14821=EDGE_LOOP('',(#66690,#66691,#66692,#66693));
#14822=EDGE_LOOP('',(#66694,#66695,#66696,#66697));
#14823=EDGE_LOOP('',(#66698,#66699,#66700,#66701));
#14824=EDGE_LOOP('',(#66702,#66703,#66704,#66705,#66706));
#14825=EDGE_LOOP('',(#66707,#66708,#66709,#66710));
#14826=EDGE_LOOP('',(#66711,#66712,#66713,#66714));
#14827=EDGE_LOOP('',(#66715,#66716,#66717,#66718));
#14828=EDGE_LOOP('',(#66719,#66720,#66721,#66722));
#14829=EDGE_LOOP('',(#66723,#66724,#66725,#66726));
#14830=EDGE_LOOP('',(#66727,#66728,#66729,#66730));
#14831=EDGE_LOOP('',(#66731,#66732,#66733,#66734));
#14832=EDGE_LOOP('',(#66735,#66736,#66737,#66738));
#14833=EDGE_LOOP('',(#66739,#66740,#66741,#66742));
#14834=EDGE_LOOP('',(#66743,#66744,#66745,#66746));
#14835=EDGE_LOOP('',(#66747,#66748,#66749,#66750,#66751));
#14836=EDGE_LOOP('',(#66752,#66753,#66754,#66755));
#14837=EDGE_LOOP('',(#66756,#66757,#66758,#66759));
#14838=EDGE_LOOP('',(#66760,#66761,#66762,#66763));
#14839=EDGE_LOOP('',(#66764,#66765,#66766,#66767));
#14840=EDGE_LOOP('',(#66768,#66769,#66770,#66771));
#14841=EDGE_LOOP('',(#66772,#66773,#66774,#66775));
#14842=EDGE_LOOP('',(#66776,#66777,#66778,#66779));
#14843=EDGE_LOOP('',(#66780,#66781,#66782,#66783));
#14844=EDGE_LOOP('',(#66784,#66785,#66786,#66787,#66788));
#14845=EDGE_LOOP('',(#66789,#66790,#66791,#66792));
#14846=EDGE_LOOP('',(#66793,#66794,#66795,#66796));
#14847=EDGE_LOOP('',(#66797,#66798,#66799,#66800,#66801));
#14848=EDGE_LOOP('',(#66802,#66803,#66804,#66805));
#14849=EDGE_LOOP('',(#66806,#66807,#66808,#66809));
#14850=EDGE_LOOP('',(#66810,#66811,#66812,#66813));
#14851=EDGE_LOOP('',(#66814,#66815,#66816,#66817));
#14852=EDGE_LOOP('',(#66818,#66819,#66820,#66821,#66822));
#14853=EDGE_LOOP('',(#66823,#66824,#66825,#66826));
#14854=EDGE_LOOP('',(#66827,#66828,#66829,#66830));
#14855=EDGE_LOOP('',(#66831,#66832,#66833,#66834));
#14856=EDGE_LOOP('',(#66835,#66836,#66837,#66838));
#14857=EDGE_LOOP('',(#66839,#66840,#66841,#66842));
#14858=EDGE_LOOP('',(#66843,#66844,#66845,#66846));
#14859=EDGE_LOOP('',(#66847,#66848,#66849,#66850));
#14860=EDGE_LOOP('',(#66851,#66852,#66853,#66854));
#14861=EDGE_LOOP('',(#66855,#66856,#66857,#66858));
#14862=EDGE_LOOP('',(#66859,#66860,#66861,#66862));
#14863=EDGE_LOOP('',(#66863,#66864,#66865,#66866,#66867));
#14864=EDGE_LOOP('',(#66868,#66869,#66870,#66871));
#14865=EDGE_LOOP('',(#66872,#66873,#66874,#66875));
#14866=EDGE_LOOP('',(#66876,#66877,#66878,#66879));
#14867=EDGE_LOOP('',(#66880,#66881,#66882,#66883));
#14868=EDGE_LOOP('',(#66884,#66885,#66886,#66887));
#14869=EDGE_LOOP('',(#66888,#66889,#66890,#66891));
#14870=EDGE_LOOP('',(#66892,#66893,#66894,#66895));
#14871=EDGE_LOOP('',(#66896,#66897,#66898,#66899));
#14872=EDGE_LOOP('',(#66900,#66901,#66902,#66903,#66904));
#14873=EDGE_LOOP('',(#66905,#66906,#66907,#66908));
#14874=EDGE_LOOP('',(#66909,#66910,#66911,#66912));
#14875=EDGE_LOOP('',(#66913,#66914,#66915,#66916,#66917));
#14876=EDGE_LOOP('',(#66918,#66919,#66920,#66921));
#14877=EDGE_LOOP('',(#66922,#66923,#66924,#66925));
#14878=EDGE_LOOP('',(#66926,#66927,#66928,#66929));
#14879=EDGE_LOOP('',(#66930,#66931,#66932,#66933));
#14880=EDGE_LOOP('',(#66934,#66935,#66936,#66937,#66938));
#14881=EDGE_LOOP('',(#66939,#66940,#66941,#66942));
#14882=EDGE_LOOP('',(#66943,#66944,#66945,#66946));
#14883=EDGE_LOOP('',(#66947,#66948,#66949,#66950));
#14884=EDGE_LOOP('',(#66951,#66952,#66953,#66954));
#14885=EDGE_LOOP('',(#66955,#66956,#66957,#66958));
#14886=EDGE_LOOP('',(#66959,#66960,#66961,#66962));
#14887=EDGE_LOOP('',(#66963,#66964,#66965,#66966));
#14888=EDGE_LOOP('',(#66967,#66968,#66969,#66970));
#14889=EDGE_LOOP('',(#66971,#66972,#66973,#66974));
#14890=EDGE_LOOP('',(#66975,#66976,#66977,#66978));
#14891=EDGE_LOOP('',(#66979,#66980,#66981,#66982,#66983));
#14892=EDGE_LOOP('',(#66984,#66985,#66986,#66987));
#14893=EDGE_LOOP('',(#66988,#66989,#66990,#66991));
#14894=EDGE_LOOP('',(#66992,#66993,#66994,#66995));
#14895=EDGE_LOOP('',(#66996,#66997,#66998,#66999));
#14896=EDGE_LOOP('',(#67000,#67001,#67002,#67003));
#14897=EDGE_LOOP('',(#67004,#67005,#67006,#67007));
#14898=EDGE_LOOP('',(#67008,#67009,#67010,#67011));
#14899=EDGE_LOOP('',(#67012,#67013,#67014,#67015));
#14900=EDGE_LOOP('',(#67016,#67017,#67018,#67019,#67020));
#14901=EDGE_LOOP('',(#67021,#67022,#67023,#67024));
#14902=EDGE_LOOP('',(#67025,#67026,#67027,#67028));
#14903=EDGE_LOOP('',(#67029,#67030,#67031,#67032,#67033));
#14904=EDGE_LOOP('',(#67034,#67035,#67036,#67037));
#14905=EDGE_LOOP('',(#67038,#67039,#67040,#67041));
#14906=EDGE_LOOP('',(#67042,#67043,#67044,#67045));
#14907=EDGE_LOOP('',(#67046,#67047,#67048,#67049));
#14908=EDGE_LOOP('',(#67050,#67051,#67052,#67053,#67054));
#14909=EDGE_LOOP('',(#67055,#67056,#67057,#67058));
#14910=EDGE_LOOP('',(#67059,#67060,#67061,#67062));
#14911=EDGE_LOOP('',(#67063,#67064,#67065,#67066));
#14912=EDGE_LOOP('',(#67067,#67068,#67069,#67070));
#14913=EDGE_LOOP('',(#67071,#67072,#67073,#67074));
#14914=EDGE_LOOP('',(#67075,#67076,#67077,#67078));
#14915=EDGE_LOOP('',(#67079,#67080,#67081,#67082));
#14916=EDGE_LOOP('',(#67083,#67084,#67085,#67086));
#14917=EDGE_LOOP('',(#67087,#67088,#67089,#67090));
#14918=EDGE_LOOP('',(#67091,#67092,#67093,#67094));
#14919=EDGE_LOOP('',(#67095,#67096,#67097,#67098,#67099));
#14920=EDGE_LOOP('',(#67100,#67101,#67102,#67103));
#14921=EDGE_LOOP('',(#67104,#67105,#67106,#67107));
#14922=EDGE_LOOP('',(#67108,#67109,#67110,#67111));
#14923=EDGE_LOOP('',(#67112,#67113,#67114,#67115));
#14924=EDGE_LOOP('',(#67116,#67117,#67118,#67119));
#14925=EDGE_LOOP('',(#67120,#67121,#67122,#67123));
#14926=EDGE_LOOP('',(#67124,#67125,#67126,#67127));
#14927=EDGE_LOOP('',(#67128,#67129,#67130,#67131));
#14928=EDGE_LOOP('',(#67132,#67133,#67134,#67135,#67136));
#14929=EDGE_LOOP('',(#67137,#67138,#67139,#67140));
#14930=EDGE_LOOP('',(#67141,#67142,#67143,#67144));
#14931=EDGE_LOOP('',(#67145,#67146,#67147,#67148,#67149));
#14932=EDGE_LOOP('',(#67150,#67151,#67152,#67153));
#14933=EDGE_LOOP('',(#67154,#67155,#67156,#67157));
#14934=EDGE_LOOP('',(#67158,#67159,#67160,#67161));
#14935=EDGE_LOOP('',(#67162,#67163,#67164,#67165));
#14936=EDGE_LOOP('',(#67166,#67167,#67168,#67169,#67170));
#14937=EDGE_LOOP('',(#67171,#67172,#67173,#67174));
#14938=EDGE_LOOP('',(#67175,#67176,#67177,#67178));
#14939=EDGE_LOOP('',(#67179,#67180,#67181,#67182));
#14940=EDGE_LOOP('',(#67183,#67184,#67185,#67186));
#14941=EDGE_LOOP('',(#67187,#67188,#67189,#67190));
#14942=EDGE_LOOP('',(#67191,#67192,#67193,#67194));
#14943=EDGE_LOOP('',(#67195,#67196,#67197,#67198));
#14944=EDGE_LOOP('',(#67199,#67200,#67201,#67202));
#14945=EDGE_LOOP('',(#67203,#67204,#67205,#67206));
#14946=EDGE_LOOP('',(#67207,#67208,#67209,#67210));
#14947=EDGE_LOOP('',(#67211,#67212,#67213,#67214,#67215));
#14948=EDGE_LOOP('',(#67216,#67217,#67218,#67219));
#14949=EDGE_LOOP('',(#67220,#67221,#67222,#67223));
#14950=EDGE_LOOP('',(#67224,#67225,#67226,#67227));
#14951=EDGE_LOOP('',(#67228,#67229,#67230,#67231));
#14952=EDGE_LOOP('',(#67232,#67233,#67234,#67235));
#14953=EDGE_LOOP('',(#67236,#67237,#67238,#67239));
#14954=EDGE_LOOP('',(#67240,#67241,#67242,#67243));
#14955=EDGE_LOOP('',(#67244,#67245,#67246,#67247));
#14956=EDGE_LOOP('',(#67248,#67249,#67250,#67251,#67252));
#14957=EDGE_LOOP('',(#67253,#67254,#67255,#67256));
#14958=EDGE_LOOP('',(#67257,#67258,#67259,#67260));
#14959=EDGE_LOOP('',(#67261,#67262,#67263,#67264,#67265));
#14960=EDGE_LOOP('',(#67266,#67267,#67268,#67269));
#14961=EDGE_LOOP('',(#67270,#67271,#67272,#67273));
#14962=EDGE_LOOP('',(#67274,#67275,#67276,#67277));
#14963=EDGE_LOOP('',(#67278,#67279,#67280,#67281));
#14964=EDGE_LOOP('',(#67282,#67283,#67284,#67285,#67286));
#14965=EDGE_LOOP('',(#67287,#67288,#67289,#67290));
#14966=EDGE_LOOP('',(#67291,#67292,#67293,#67294));
#14967=EDGE_LOOP('',(#67295,#67296,#67297,#67298));
#14968=EDGE_LOOP('',(#67299,#67300,#67301,#67302));
#14969=EDGE_LOOP('',(#67303,#67304,#67305,#67306));
#14970=EDGE_LOOP('',(#67307,#67308,#67309,#67310));
#14971=EDGE_LOOP('',(#67311,#67312,#67313,#67314));
#14972=EDGE_LOOP('',(#67315,#67316,#67317,#67318));
#14973=EDGE_LOOP('',(#67319,#67320,#67321,#67322));
#14974=EDGE_LOOP('',(#67323,#67324,#67325,#67326));
#14975=EDGE_LOOP('',(#67327,#67328,#67329,#67330,#67331));
#14976=EDGE_LOOP('',(#67332,#67333,#67334,#67335));
#14977=EDGE_LOOP('',(#67336,#67337,#67338,#67339));
#14978=EDGE_LOOP('',(#67340,#67341,#67342,#67343));
#14979=EDGE_LOOP('',(#67344,#67345,#67346,#67347));
#14980=EDGE_LOOP('',(#67348,#67349,#67350,#67351));
#14981=EDGE_LOOP('',(#67352,#67353,#67354,#67355));
#14982=EDGE_LOOP('',(#67356,#67357,#67358,#67359));
#14983=EDGE_LOOP('',(#67360,#67361,#67362,#67363));
#14984=EDGE_LOOP('',(#67364,#67365,#67366,#67367,#67368));
#14985=EDGE_LOOP('',(#67369,#67370,#67371,#67372));
#14986=EDGE_LOOP('',(#67373,#67374,#67375,#67376));
#14987=EDGE_LOOP('',(#67377,#67378,#67379,#67380,#67381));
#14988=EDGE_LOOP('',(#67382,#67383,#67384,#67385));
#14989=EDGE_LOOP('',(#67386,#67387,#67388,#67389));
#14990=EDGE_LOOP('',(#67390,#67391,#67392,#67393));
#14991=EDGE_LOOP('',(#67394,#67395,#67396,#67397));
#14992=EDGE_LOOP('',(#67398,#67399,#67400,#67401,#67402));
#14993=EDGE_LOOP('',(#67403,#67404,#67405,#67406));
#14994=EDGE_LOOP('',(#67407,#67408,#67409,#67410));
#14995=EDGE_LOOP('',(#67411,#67412,#67413,#67414));
#14996=EDGE_LOOP('',(#67415,#67416,#67417,#67418));
#14997=EDGE_LOOP('',(#67419,#67420,#67421,#67422));
#14998=EDGE_LOOP('',(#67423,#67424,#67425,#67426));
#14999=EDGE_LOOP('',(#67427,#67428,#67429,#67430));
#15000=EDGE_LOOP('',(#67431,#67432,#67433,#67434));
#15001=EDGE_LOOP('',(#67435,#67436,#67437,#67438));
#15002=EDGE_LOOP('',(#67439,#67440,#67441,#67442));
#15003=EDGE_LOOP('',(#67443,#67444,#67445,#67446,#67447));
#15004=EDGE_LOOP('',(#67448,#67449,#67450,#67451));
#15005=EDGE_LOOP('',(#67452,#67453,#67454,#67455));
#15006=EDGE_LOOP('',(#67456,#67457,#67458,#67459));
#15007=EDGE_LOOP('',(#67460,#67461,#67462,#67463));
#15008=EDGE_LOOP('',(#67464,#67465,#67466,#67467));
#15009=EDGE_LOOP('',(#67468,#67469,#67470,#67471));
#15010=EDGE_LOOP('',(#67472,#67473,#67474,#67475));
#15011=EDGE_LOOP('',(#67476,#67477,#67478,#67479));
#15012=EDGE_LOOP('',(#67480,#67481,#67482,#67483,#67484));
#15013=EDGE_LOOP('',(#67485,#67486,#67487,#67488));
#15014=EDGE_LOOP('',(#67489,#67490,#67491,#67492));
#15015=EDGE_LOOP('',(#67493,#67494,#67495,#67496,#67497));
#15016=EDGE_LOOP('',(#67498,#67499,#67500,#67501));
#15017=EDGE_LOOP('',(#67502,#67503,#67504,#67505));
#15018=EDGE_LOOP('',(#67506,#67507,#67508,#67509));
#15019=EDGE_LOOP('',(#67510,#67511,#67512,#67513));
#15020=EDGE_LOOP('',(#67514,#67515,#67516,#67517,#67518));
#15021=EDGE_LOOP('',(#67519,#67520,#67521,#67522));
#15022=EDGE_LOOP('',(#67523,#67524,#67525,#67526));
#15023=EDGE_LOOP('',(#67527,#67528,#67529,#67530));
#15024=EDGE_LOOP('',(#67531,#67532,#67533,#67534));
#15025=EDGE_LOOP('',(#67535,#67536,#67537,#67538));
#15026=EDGE_LOOP('',(#67539,#67540,#67541,#67542));
#15027=EDGE_LOOP('',(#67543,#67544,#67545,#67546));
#15028=EDGE_LOOP('',(#67547,#67548,#67549,#67550));
#15029=EDGE_LOOP('',(#67551,#67552,#67553,#67554));
#15030=EDGE_LOOP('',(#67555,#67556,#67557,#67558));
#15031=EDGE_LOOP('',(#67559,#67560,#67561,#67562,#67563));
#15032=EDGE_LOOP('',(#67564,#67565,#67566,#67567));
#15033=EDGE_LOOP('',(#67568,#67569,#67570,#67571));
#15034=EDGE_LOOP('',(#67572,#67573,#67574,#67575));
#15035=EDGE_LOOP('',(#67576,#67577,#67578,#67579));
#15036=EDGE_LOOP('',(#67580,#67581,#67582,#67583));
#15037=EDGE_LOOP('',(#67584,#67585,#67586,#67587));
#15038=EDGE_LOOP('',(#67588,#67589,#67590,#67591));
#15039=EDGE_LOOP('',(#67592,#67593,#67594,#67595));
#15040=EDGE_LOOP('',(#67596,#67597,#67598,#67599,#67600));
#15041=EDGE_LOOP('',(#67601,#67602,#67603,#67604));
#15042=EDGE_LOOP('',(#67605,#67606,#67607,#67608));
#15043=EDGE_LOOP('',(#67609,#67610,#67611,#67612,#67613));
#15044=EDGE_LOOP('',(#67614,#67615,#67616,#67617));
#15045=EDGE_LOOP('',(#67618,#67619,#67620,#67621));
#15046=EDGE_LOOP('',(#67622,#67623,#67624,#67625));
#15047=EDGE_LOOP('',(#67626,#67627,#67628,#67629));
#15048=EDGE_LOOP('',(#67630,#67631,#67632,#67633,#67634));
#15049=EDGE_LOOP('',(#67635,#67636,#67637,#67638));
#15050=EDGE_LOOP('',(#67639,#67640,#67641,#67642));
#15051=EDGE_LOOP('',(#67643,#67644,#67645,#67646));
#15052=EDGE_LOOP('',(#67647,#67648,#67649,#67650));
#15053=EDGE_LOOP('',(#67651,#67652,#67653,#67654));
#15054=EDGE_LOOP('',(#67655,#67656,#67657,#67658));
#15055=EDGE_LOOP('',(#67659,#67660,#67661,#67662));
#15056=EDGE_LOOP('',(#67663,#67664,#67665,#67666));
#15057=EDGE_LOOP('',(#67667,#67668,#67669,#67670));
#15058=EDGE_LOOP('',(#67671,#67672,#67673,#67674));
#15059=EDGE_LOOP('',(#67675,#67676,#67677,#67678,#67679));
#15060=EDGE_LOOP('',(#67680,#67681,#67682,#67683));
#15061=EDGE_LOOP('',(#67684,#67685,#67686,#67687));
#15062=EDGE_LOOP('',(#67688,#67689,#67690,#67691));
#15063=EDGE_LOOP('',(#67692,#67693,#67694,#67695));
#15064=EDGE_LOOP('',(#67696,#67697,#67698,#67699));
#15065=EDGE_LOOP('',(#67700,#67701,#67702,#67703));
#15066=EDGE_LOOP('',(#67704,#67705,#67706,#67707));
#15067=EDGE_LOOP('',(#67708,#67709,#67710,#67711));
#15068=EDGE_LOOP('',(#67712,#67713,#67714,#67715,#67716));
#15069=EDGE_LOOP('',(#67717,#67718,#67719,#67720));
#15070=EDGE_LOOP('',(#67721,#67722,#67723,#67724));
#15071=EDGE_LOOP('',(#67725,#67726,#67727,#67728,#67729));
#15072=EDGE_LOOP('',(#67730,#67731,#67732,#67733));
#15073=EDGE_LOOP('',(#67734,#67735,#67736,#67737));
#15074=EDGE_LOOP('',(#67738,#67739,#67740,#67741));
#15075=EDGE_LOOP('',(#67742,#67743,#67744,#67745));
#15076=EDGE_LOOP('',(#67746,#67747,#67748,#67749,#67750));
#15077=EDGE_LOOP('',(#67751,#67752,#67753,#67754));
#15078=EDGE_LOOP('',(#67755,#67756,#67757,#67758));
#15079=EDGE_LOOP('',(#67759,#67760,#67761,#67762));
#15080=EDGE_LOOP('',(#67763,#67764,#67765,#67766));
#15081=EDGE_LOOP('',(#67767,#67768,#67769,#67770));
#15082=EDGE_LOOP('',(#67771,#67772,#67773,#67774));
#15083=EDGE_LOOP('',(#67775,#67776,#67777,#67778));
#15084=EDGE_LOOP('',(#67779,#67780,#67781,#67782));
#15085=EDGE_LOOP('',(#67783,#67784,#67785,#67786));
#15086=EDGE_LOOP('',(#67787,#67788,#67789,#67790));
#15087=EDGE_LOOP('',(#67791,#67792,#67793,#67794,#67795));
#15088=EDGE_LOOP('',(#67796,#67797,#67798,#67799));
#15089=EDGE_LOOP('',(#67800,#67801,#67802,#67803));
#15090=EDGE_LOOP('',(#67804,#67805,#67806,#67807));
#15091=EDGE_LOOP('',(#67808,#67809,#67810,#67811));
#15092=EDGE_LOOP('',(#67812,#67813,#67814,#67815));
#15093=EDGE_LOOP('',(#67816,#67817,#67818,#67819));
#15094=EDGE_LOOP('',(#67820,#67821,#67822,#67823));
#15095=EDGE_LOOP('',(#67824,#67825,#67826,#67827));
#15096=EDGE_LOOP('',(#67828,#67829,#67830,#67831,#67832));
#15097=EDGE_LOOP('',(#67833,#67834,#67835,#67836));
#15098=EDGE_LOOP('',(#67837,#67838,#67839,#67840));
#15099=EDGE_LOOP('',(#67841,#67842,#67843,#67844,#67845));
#15100=EDGE_LOOP('',(#67846,#67847,#67848,#67849));
#15101=EDGE_LOOP('',(#67850,#67851,#67852,#67853));
#15102=EDGE_LOOP('',(#67854,#67855,#67856,#67857));
#15103=EDGE_LOOP('',(#67858,#67859,#67860,#67861));
#15104=EDGE_LOOP('',(#67862,#67863,#67864,#67865,#67866));
#15105=EDGE_LOOP('',(#67867,#67868,#67869,#67870));
#15106=EDGE_LOOP('',(#67871,#67872,#67873,#67874));
#15107=EDGE_LOOP('',(#67875,#67876,#67877,#67878));
#15108=EDGE_LOOP('',(#67879,#67880,#67881,#67882));
#15109=EDGE_LOOP('',(#67883,#67884,#67885,#67886));
#15110=EDGE_LOOP('',(#67887,#67888,#67889,#67890));
#15111=EDGE_LOOP('',(#67891,#67892,#67893,#67894));
#15112=EDGE_LOOP('',(#67895,#67896,#67897,#67898));
#15113=EDGE_LOOP('',(#67899,#67900,#67901,#67902));
#15114=EDGE_LOOP('',(#67903,#67904,#67905,#67906));
#15115=EDGE_LOOP('',(#67907,#67908,#67909,#67910,#67911));
#15116=EDGE_LOOP('',(#67912,#67913,#67914,#67915));
#15117=EDGE_LOOP('',(#67916,#67917,#67918,#67919));
#15118=EDGE_LOOP('',(#67920,#67921,#67922,#67923));
#15119=EDGE_LOOP('',(#67924,#67925,#67926,#67927));
#15120=EDGE_LOOP('',(#67928,#67929,#67930,#67931));
#15121=EDGE_LOOP('',(#67932,#67933,#67934,#67935));
#15122=EDGE_LOOP('',(#67936,#67937,#67938,#67939));
#15123=EDGE_LOOP('',(#67940,#67941,#67942,#67943));
#15124=EDGE_LOOP('',(#67944,#67945,#67946,#67947,#67948));
#15125=EDGE_LOOP('',(#67949,#67950,#67951,#67952));
#15126=EDGE_LOOP('',(#67953,#67954,#67955,#67956));
#15127=EDGE_LOOP('',(#67957,#67958,#67959,#67960,#67961));
#15128=EDGE_LOOP('',(#67962,#67963,#67964,#67965));
#15129=EDGE_LOOP('',(#67966,#67967,#67968,#67969));
#15130=EDGE_LOOP('',(#67970,#67971,#67972,#67973));
#15131=EDGE_LOOP('',(#67974,#67975,#67976,#67977));
#15132=EDGE_LOOP('',(#67978,#67979,#67980,#67981,#67982));
#15133=EDGE_LOOP('',(#67983,#67984,#67985,#67986));
#15134=EDGE_LOOP('',(#67987,#67988,#67989,#67990));
#15135=EDGE_LOOP('',(#67991,#67992,#67993,#67994));
#15136=EDGE_LOOP('',(#67995,#67996,#67997,#67998));
#15137=EDGE_LOOP('',(#67999,#68000,#68001,#68002));
#15138=EDGE_LOOP('',(#68003,#68004,#68005,#68006));
#15139=EDGE_LOOP('',(#68007,#68008,#68009,#68010));
#15140=EDGE_LOOP('',(#68011,#68012,#68013,#68014));
#15141=EDGE_LOOP('',(#68015,#68016,#68017,#68018));
#15142=EDGE_LOOP('',(#68019,#68020,#68021,#68022));
#15143=EDGE_LOOP('',(#68023,#68024,#68025,#68026,#68027));
#15144=EDGE_LOOP('',(#68028,#68029,#68030,#68031));
#15145=EDGE_LOOP('',(#68032,#68033,#68034,#68035));
#15146=EDGE_LOOP('',(#68036,#68037,#68038,#68039));
#15147=EDGE_LOOP('',(#68040,#68041,#68042,#68043));
#15148=EDGE_LOOP('',(#68044,#68045,#68046,#68047));
#15149=EDGE_LOOP('',(#68048,#68049,#68050,#68051));
#15150=EDGE_LOOP('',(#68052,#68053,#68054,#68055));
#15151=EDGE_LOOP('',(#68056,#68057,#68058,#68059));
#15152=EDGE_LOOP('',(#68060,#68061,#68062,#68063,#68064));
#15153=EDGE_LOOP('',(#68065,#68066,#68067,#68068));
#15154=EDGE_LOOP('',(#68069,#68070,#68071,#68072));
#15155=EDGE_LOOP('',(#68073,#68074,#68075,#68076,#68077));
#15156=EDGE_LOOP('',(#68078,#68079,#68080,#68081));
#15157=EDGE_LOOP('',(#68082,#68083,#68084,#68085));
#15158=EDGE_LOOP('',(#68086,#68087,#68088,#68089));
#15159=EDGE_LOOP('',(#68090,#68091,#68092,#68093));
#15160=EDGE_LOOP('',(#68094,#68095,#68096,#68097,#68098));
#15161=EDGE_LOOP('',(#68099,#68100,#68101,#68102));
#15162=EDGE_LOOP('',(#68103,#68104,#68105,#68106));
#15163=EDGE_LOOP('',(#68107,#68108,#68109,#68110));
#15164=EDGE_LOOP('',(#68111,#68112,#68113,#68114));
#15165=EDGE_LOOP('',(#68115,#68116,#68117,#68118));
#15166=EDGE_LOOP('',(#68119,#68120,#68121,#68122));
#15167=EDGE_LOOP('',(#68123,#68124,#68125,#68126));
#15168=EDGE_LOOP('',(#68127,#68128,#68129,#68130));
#15169=EDGE_LOOP('',(#68131,#68132,#68133,#68134));
#15170=EDGE_LOOP('',(#68135,#68136,#68137,#68138));
#15171=EDGE_LOOP('',(#68139,#68140,#68141,#68142,#68143));
#15172=EDGE_LOOP('',(#68144,#68145,#68146,#68147));
#15173=EDGE_LOOP('',(#68148,#68149,#68150,#68151));
#15174=EDGE_LOOP('',(#68152,#68153,#68154,#68155));
#15175=EDGE_LOOP('',(#68156,#68157,#68158,#68159));
#15176=EDGE_LOOP('',(#68160,#68161,#68162,#68163));
#15177=EDGE_LOOP('',(#68164,#68165,#68166,#68167));
#15178=EDGE_LOOP('',(#68168,#68169,#68170,#68171));
#15179=EDGE_LOOP('',(#68172,#68173,#68174,#68175));
#15180=EDGE_LOOP('',(#68176,#68177,#68178,#68179,#68180));
#15181=EDGE_LOOP('',(#68181,#68182,#68183,#68184));
#15182=EDGE_LOOP('',(#68185,#68186,#68187,#68188));
#15183=EDGE_LOOP('',(#68189,#68190,#68191,#68192,#68193));
#15184=EDGE_LOOP('',(#68194,#68195,#68196,#68197));
#15185=EDGE_LOOP('',(#68198,#68199,#68200,#68201));
#15186=EDGE_LOOP('',(#68202,#68203,#68204,#68205));
#15187=EDGE_LOOP('',(#68206,#68207,#68208,#68209));
#15188=EDGE_LOOP('',(#68210,#68211,#68212,#68213,#68214));
#15189=EDGE_LOOP('',(#68215,#68216,#68217,#68218));
#15190=EDGE_LOOP('',(#68219,#68220,#68221,#68222));
#15191=EDGE_LOOP('',(#68223,#68224,#68225,#68226));
#15192=EDGE_LOOP('',(#68227,#68228,#68229,#68230));
#15193=EDGE_LOOP('',(#68231,#68232,#68233,#68234));
#15194=EDGE_LOOP('',(#68235,#68236,#68237,#68238));
#15195=EDGE_LOOP('',(#68239,#68240,#68241,#68242));
#15196=EDGE_LOOP('',(#68243,#68244,#68245,#68246));
#15197=EDGE_LOOP('',(#68247,#68248,#68249,#68250));
#15198=EDGE_LOOP('',(#68251,#68252,#68253,#68254));
#15199=EDGE_LOOP('',(#68255,#68256,#68257,#68258,#68259));
#15200=EDGE_LOOP('',(#68260,#68261,#68262,#68263));
#15201=EDGE_LOOP('',(#68264,#68265,#68266,#68267));
#15202=EDGE_LOOP('',(#68268,#68269,#68270,#68271));
#15203=EDGE_LOOP('',(#68272,#68273,#68274,#68275));
#15204=EDGE_LOOP('',(#68276,#68277,#68278,#68279));
#15205=EDGE_LOOP('',(#68280,#68281,#68282,#68283));
#15206=EDGE_LOOP('',(#68284,#68285,#68286,#68287));
#15207=EDGE_LOOP('',(#68288,#68289,#68290,#68291));
#15208=EDGE_LOOP('',(#68292,#68293,#68294,#68295,#68296));
#15209=EDGE_LOOP('',(#68297,#68298,#68299,#68300));
#15210=EDGE_LOOP('',(#68301,#68302,#68303,#68304));
#15211=EDGE_LOOP('',(#68305,#68306,#68307,#68308,#68309));
#15212=EDGE_LOOP('',(#68310,#68311,#68312,#68313));
#15213=EDGE_LOOP('',(#68314,#68315,#68316,#68317));
#15214=EDGE_LOOP('',(#68318,#68319,#68320,#68321));
#15215=EDGE_LOOP('',(#68322,#68323,#68324,#68325));
#15216=EDGE_LOOP('',(#68326,#68327,#68328,#68329,#68330));
#15217=EDGE_LOOP('',(#68331,#68332,#68333,#68334));
#15218=EDGE_LOOP('',(#68335,#68336,#68337,#68338));
#15219=EDGE_LOOP('',(#68339,#68340,#68341,#68342));
#15220=EDGE_LOOP('',(#68343,#68344,#68345,#68346));
#15221=EDGE_LOOP('',(#68347,#68348,#68349,#68350));
#15222=EDGE_LOOP('',(#68351,#68352,#68353,#68354));
#15223=EDGE_LOOP('',(#68355,#68356,#68357,#68358));
#15224=EDGE_LOOP('',(#68359,#68360,#68361,#68362));
#15225=EDGE_LOOP('',(#68363,#68364,#68365,#68366));
#15226=EDGE_LOOP('',(#68367,#68368,#68369,#68370));
#15227=EDGE_LOOP('',(#68371,#68372,#68373,#68374,#68375));
#15228=EDGE_LOOP('',(#68376,#68377,#68378,#68379));
#15229=EDGE_LOOP('',(#68380,#68381,#68382,#68383));
#15230=EDGE_LOOP('',(#68384,#68385,#68386,#68387));
#15231=EDGE_LOOP('',(#68388,#68389,#68390,#68391));
#15232=EDGE_LOOP('',(#68392,#68393,#68394,#68395));
#15233=EDGE_LOOP('',(#68396,#68397,#68398,#68399));
#15234=EDGE_LOOP('',(#68400,#68401,#68402,#68403));
#15235=EDGE_LOOP('',(#68404,#68405,#68406,#68407));
#15236=EDGE_LOOP('',(#68408,#68409,#68410,#68411,#68412));
#15237=EDGE_LOOP('',(#68413,#68414,#68415,#68416));
#15238=EDGE_LOOP('',(#68417,#68418,#68419,#68420));
#15239=EDGE_LOOP('',(#68421,#68422,#68423,#68424,#68425));
#15240=EDGE_LOOP('',(#68426,#68427,#68428,#68429));
#15241=EDGE_LOOP('',(#68430,#68431,#68432,#68433));
#15242=EDGE_LOOP('',(#68434,#68435,#68436,#68437));
#15243=EDGE_LOOP('',(#68438,#68439,#68440,#68441));
#15244=EDGE_LOOP('',(#68442,#68443,#68444,#68445,#68446));
#15245=EDGE_LOOP('',(#68447,#68448,#68449,#68450));
#15246=EDGE_LOOP('',(#68451,#68452,#68453,#68454));
#15247=EDGE_LOOP('',(#68455,#68456,#68457,#68458));
#15248=EDGE_LOOP('',(#68459,#68460,#68461,#68462));
#15249=EDGE_LOOP('',(#68463,#68464,#68465,#68466));
#15250=EDGE_LOOP('',(#68467,#68468,#68469,#68470));
#15251=EDGE_LOOP('',(#68471,#68472,#68473,#68474));
#15252=EDGE_LOOP('',(#68475,#68476,#68477,#68478));
#15253=EDGE_LOOP('',(#68479,#68480,#68481,#68482));
#15254=EDGE_LOOP('',(#68483,#68484,#68485,#68486));
#15255=EDGE_LOOP('',(#68487,#68488,#68489,#68490,#68491));
#15256=EDGE_LOOP('',(#68492,#68493,#68494,#68495));
#15257=EDGE_LOOP('',(#68496,#68497,#68498,#68499));
#15258=EDGE_LOOP('',(#68500,#68501,#68502,#68503));
#15259=EDGE_LOOP('',(#68504,#68505,#68506,#68507));
#15260=EDGE_LOOP('',(#68508,#68509,#68510,#68511));
#15261=EDGE_LOOP('',(#68512,#68513,#68514,#68515));
#15262=EDGE_LOOP('',(#68516,#68517,#68518,#68519));
#15263=EDGE_LOOP('',(#68520,#68521,#68522,#68523));
#15264=EDGE_LOOP('',(#68524,#68525,#68526,#68527,#68528));
#15265=EDGE_LOOP('',(#68529,#68530,#68531,#68532));
#15266=EDGE_LOOP('',(#68533,#68534,#68535,#68536));
#15267=EDGE_LOOP('',(#68537,#68538,#68539,#68540,#68541));
#15268=EDGE_LOOP('',(#68542,#68543,#68544,#68545));
#15269=EDGE_LOOP('',(#68546,#68547,#68548,#68549));
#15270=EDGE_LOOP('',(#68550,#68551,#68552,#68553));
#15271=EDGE_LOOP('',(#68554,#68555,#68556,#68557));
#15272=EDGE_LOOP('',(#68558,#68559,#68560,#68561,#68562));
#15273=EDGE_LOOP('',(#68563,#68564,#68565,#68566));
#15274=EDGE_LOOP('',(#68567,#68568,#68569,#68570));
#15275=EDGE_LOOP('',(#68571,#68572,#68573,#68574));
#15276=EDGE_LOOP('',(#68575,#68576,#68577,#68578));
#15277=EDGE_LOOP('',(#68579,#68580,#68581,#68582));
#15278=EDGE_LOOP('',(#68583,#68584,#68585,#68586));
#15279=EDGE_LOOP('',(#68587,#68588,#68589,#68590));
#15280=EDGE_LOOP('',(#68591,#68592,#68593,#68594));
#15281=EDGE_LOOP('',(#68595,#68596,#68597,#68598));
#15282=EDGE_LOOP('',(#68599,#68600,#68601,#68602));
#15283=EDGE_LOOP('',(#68603,#68604,#68605,#68606,#68607));
#15284=EDGE_LOOP('',(#68608,#68609,#68610,#68611));
#15285=EDGE_LOOP('',(#68612,#68613,#68614,#68615));
#15286=EDGE_LOOP('',(#68616,#68617,#68618,#68619));
#15287=EDGE_LOOP('',(#68620,#68621,#68622,#68623));
#15288=EDGE_LOOP('',(#68624,#68625,#68626,#68627));
#15289=EDGE_LOOP('',(#68628,#68629,#68630,#68631));
#15290=EDGE_LOOP('',(#68632,#68633,#68634,#68635));
#15291=EDGE_LOOP('',(#68636,#68637,#68638,#68639));
#15292=EDGE_LOOP('',(#68640,#68641,#68642,#68643,#68644));
#15293=EDGE_LOOP('',(#68645,#68646,#68647,#68648));
#15294=EDGE_LOOP('',(#68649,#68650,#68651,#68652));
#15295=EDGE_LOOP('',(#68653,#68654,#68655,#68656,#68657));
#15296=EDGE_LOOP('',(#68658,#68659,#68660,#68661));
#15297=EDGE_LOOP('',(#68662,#68663,#68664,#68665));
#15298=EDGE_LOOP('',(#68666,#68667,#68668,#68669));
#15299=EDGE_LOOP('',(#68670,#68671,#68672,#68673));
#15300=EDGE_LOOP('',(#68674,#68675,#68676,#68677,#68678));
#15301=EDGE_LOOP('',(#68679,#68680,#68681,#68682));
#15302=EDGE_LOOP('',(#68683,#68684,#68685,#68686));
#15303=EDGE_LOOP('',(#68687,#68688,#68689,#68690));
#15304=EDGE_LOOP('',(#68691,#68692,#68693,#68694));
#15305=EDGE_LOOP('',(#68695,#68696,#68697,#68698));
#15306=EDGE_LOOP('',(#68699,#68700,#68701,#68702));
#15307=EDGE_LOOP('',(#68703,#68704,#68705,#68706));
#15308=EDGE_LOOP('',(#68707,#68708,#68709,#68710));
#15309=EDGE_LOOP('',(#68711,#68712,#68713,#68714));
#15310=EDGE_LOOP('',(#68715,#68716,#68717,#68718));
#15311=EDGE_LOOP('',(#68719,#68720,#68721,#68722,#68723));
#15312=EDGE_LOOP('',(#68724,#68725,#68726,#68727));
#15313=EDGE_LOOP('',(#68728,#68729,#68730,#68731));
#15314=EDGE_LOOP('',(#68732,#68733,#68734,#68735));
#15315=EDGE_LOOP('',(#68736,#68737,#68738,#68739));
#15316=EDGE_LOOP('',(#68740,#68741,#68742,#68743));
#15317=EDGE_LOOP('',(#68744,#68745,#68746,#68747));
#15318=EDGE_LOOP('',(#68748,#68749,#68750,#68751));
#15319=EDGE_LOOP('',(#68752,#68753,#68754,#68755));
#15320=EDGE_LOOP('',(#68756,#68757,#68758,#68759,#68760));
#15321=EDGE_LOOP('',(#68761,#68762,#68763,#68764));
#15322=EDGE_LOOP('',(#68765,#68766,#68767,#68768));
#15323=EDGE_LOOP('',(#68769,#68770,#68771,#68772,#68773));
#15324=EDGE_LOOP('',(#68774,#68775,#68776,#68777));
#15325=EDGE_LOOP('',(#68778,#68779,#68780,#68781));
#15326=EDGE_LOOP('',(#68782,#68783,#68784,#68785));
#15327=EDGE_LOOP('',(#68786,#68787,#68788,#68789));
#15328=EDGE_LOOP('',(#68790,#68791,#68792,#68793,#68794));
#15329=EDGE_LOOP('',(#68795,#68796,#68797,#68798));
#15330=EDGE_LOOP('',(#68799,#68800,#68801,#68802));
#15331=EDGE_LOOP('',(#68803,#68804,#68805,#68806));
#15332=EDGE_LOOP('',(#68807,#68808,#68809,#68810));
#15333=EDGE_LOOP('',(#68811,#68812,#68813,#68814));
#15334=EDGE_LOOP('',(#68815,#68816,#68817,#68818));
#15335=EDGE_LOOP('',(#68819,#68820,#68821,#68822));
#15336=EDGE_LOOP('',(#68823,#68824,#68825,#68826));
#15337=EDGE_LOOP('',(#68827,#68828,#68829,#68830));
#15338=EDGE_LOOP('',(#68831,#68832,#68833,#68834));
#15339=EDGE_LOOP('',(#68835,#68836,#68837,#68838,#68839));
#15340=EDGE_LOOP('',(#68840,#68841,#68842,#68843));
#15341=EDGE_LOOP('',(#68844,#68845,#68846,#68847));
#15342=EDGE_LOOP('',(#68848,#68849,#68850,#68851));
#15343=EDGE_LOOP('',(#68852,#68853,#68854,#68855));
#15344=EDGE_LOOP('',(#68856,#68857,#68858,#68859));
#15345=EDGE_LOOP('',(#68860,#68861,#68862,#68863));
#15346=EDGE_LOOP('',(#68864,#68865,#68866,#68867));
#15347=EDGE_LOOP('',(#68868,#68869,#68870,#68871));
#15348=EDGE_LOOP('',(#68872,#68873,#68874,#68875,#68876));
#15349=EDGE_LOOP('',(#68877,#68878,#68879,#68880));
#15350=EDGE_LOOP('',(#68881,#68882,#68883,#68884));
#15351=EDGE_LOOP('',(#68885,#68886,#68887,#68888,#68889));
#15352=EDGE_LOOP('',(#68890,#68891,#68892,#68893));
#15353=EDGE_LOOP('',(#68894,#68895,#68896,#68897));
#15354=EDGE_LOOP('',(#68898,#68899,#68900,#68901));
#15355=EDGE_LOOP('',(#68902,#68903,#68904,#68905));
#15356=EDGE_LOOP('',(#68906,#68907,#68908,#68909,#68910));
#15357=EDGE_LOOP('',(#68911,#68912,#68913,#68914));
#15358=EDGE_LOOP('',(#68915,#68916,#68917,#68918));
#15359=EDGE_LOOP('',(#68919,#68920,#68921,#68922));
#15360=EDGE_LOOP('',(#68923,#68924,#68925,#68926));
#15361=EDGE_LOOP('',(#68927,#68928,#68929,#68930));
#15362=EDGE_LOOP('',(#68931,#68932,#68933,#68934));
#15363=EDGE_LOOP('',(#68935,#68936,#68937,#68938));
#15364=EDGE_LOOP('',(#68939,#68940,#68941,#68942));
#15365=EDGE_LOOP('',(#68943,#68944,#68945,#68946));
#15366=EDGE_LOOP('',(#68947,#68948,#68949,#68950));
#15367=EDGE_LOOP('',(#68951,#68952,#68953,#68954,#68955));
#15368=EDGE_LOOP('',(#68956,#68957,#68958,#68959));
#15369=EDGE_LOOP('',(#68960,#68961,#68962,#68963));
#15370=EDGE_LOOP('',(#68964,#68965,#68966,#68967));
#15371=EDGE_LOOP('',(#68968,#68969,#68970,#68971));
#15372=EDGE_LOOP('',(#68972,#68973,#68974,#68975));
#15373=EDGE_LOOP('',(#68976,#68977,#68978,#68979));
#15374=EDGE_LOOP('',(#68980,#68981,#68982,#68983));
#15375=EDGE_LOOP('',(#68984,#68985,#68986,#68987));
#15376=EDGE_LOOP('',(#68988,#68989,#68990,#68991,#68992));
#15377=EDGE_LOOP('',(#68993,#68994,#68995,#68996));
#15378=EDGE_LOOP('',(#68997,#68998,#68999,#69000));
#15379=EDGE_LOOP('',(#69001,#69002,#69003,#69004,#69005));
#15380=EDGE_LOOP('',(#69006,#69007,#69008,#69009));
#15381=EDGE_LOOP('',(#69010,#69011,#69012,#69013));
#15382=EDGE_LOOP('',(#69014,#69015,#69016,#69017));
#15383=EDGE_LOOP('',(#69018,#69019,#69020,#69021));
#15384=EDGE_LOOP('',(#69022,#69023,#69024,#69025,#69026));
#15385=EDGE_LOOP('',(#69027,#69028,#69029,#69030));
#15386=EDGE_LOOP('',(#69031,#69032,#69033,#69034));
#15387=EDGE_LOOP('',(#69035,#69036,#69037,#69038));
#15388=EDGE_LOOP('',(#69039,#69040,#69041,#69042));
#15389=EDGE_LOOP('',(#69043,#69044,#69045,#69046));
#15390=EDGE_LOOP('',(#69047,#69048,#69049,#69050));
#15391=EDGE_LOOP('',(#69051,#69052,#69053,#69054));
#15392=EDGE_LOOP('',(#69055,#69056,#69057,#69058));
#15393=EDGE_LOOP('',(#69059,#69060,#69061,#69062));
#15394=EDGE_LOOP('',(#69063,#69064,#69065,#69066));
#15395=EDGE_LOOP('',(#69067,#69068,#69069,#69070,#69071));
#15396=EDGE_LOOP('',(#69072,#69073,#69074,#69075));
#15397=EDGE_LOOP('',(#69076,#69077,#69078,#69079));
#15398=EDGE_LOOP('',(#69080,#69081,#69082,#69083));
#15399=EDGE_LOOP('',(#69084,#69085,#69086,#69087));
#15400=EDGE_LOOP('',(#69088,#69089,#69090,#69091));
#15401=EDGE_LOOP('',(#69092,#69093,#69094,#69095));
#15402=EDGE_LOOP('',(#69096,#69097,#69098,#69099));
#15403=EDGE_LOOP('',(#69100,#69101,#69102,#69103));
#15404=EDGE_LOOP('',(#69104,#69105,#69106,#69107,#69108));
#15405=EDGE_LOOP('',(#69109,#69110,#69111,#69112));
#15406=EDGE_LOOP('',(#69113,#69114,#69115,#69116));
#15407=EDGE_LOOP('',(#69117,#69118,#69119,#69120,#69121));
#15408=EDGE_LOOP('',(#69122,#69123,#69124,#69125));
#15409=EDGE_LOOP('',(#69126,#69127,#69128,#69129));
#15410=EDGE_LOOP('',(#69130,#69131,#69132,#69133));
#15411=EDGE_LOOP('',(#69134,#69135,#69136,#69137));
#15412=EDGE_LOOP('',(#69138,#69139,#69140,#69141,#69142));
#15413=EDGE_LOOP('',(#69143,#69144,#69145,#69146));
#15414=EDGE_LOOP('',(#69147,#69148,#69149,#69150));
#15415=EDGE_LOOP('',(#69151,#69152,#69153,#69154));
#15416=EDGE_LOOP('',(#69155,#69156,#69157,#69158));
#15417=EDGE_LOOP('',(#69159,#69160,#69161,#69162));
#15418=EDGE_LOOP('',(#69163,#69164,#69165,#69166));
#15419=EDGE_LOOP('',(#69167,#69168,#69169,#69170));
#15420=EDGE_LOOP('',(#69171,#69172,#69173,#69174));
#15421=EDGE_LOOP('',(#69175,#69176,#69177,#69178));
#15422=EDGE_LOOP('',(#69179,#69180,#69181,#69182));
#15423=EDGE_LOOP('',(#69183,#69184,#69185,#69186,#69187));
#15424=EDGE_LOOP('',(#69188,#69189,#69190,#69191));
#15425=EDGE_LOOP('',(#69192,#69193,#69194,#69195));
#15426=EDGE_LOOP('',(#69196,#69197,#69198,#69199));
#15427=EDGE_LOOP('',(#69200,#69201,#69202,#69203));
#15428=EDGE_LOOP('',(#69204,#69205,#69206,#69207));
#15429=EDGE_LOOP('',(#69208,#69209,#69210,#69211));
#15430=EDGE_LOOP('',(#69212,#69213,#69214,#69215));
#15431=EDGE_LOOP('',(#69216,#69217,#69218,#69219));
#15432=EDGE_LOOP('',(#69220,#69221,#69222,#69223,#69224));
#15433=EDGE_LOOP('',(#69225,#69226,#69227,#69228));
#15434=EDGE_LOOP('',(#69229,#69230,#69231,#69232));
#15435=EDGE_LOOP('',(#69233,#69234,#69235,#69236,#69237));
#15436=EDGE_LOOP('',(#69238,#69239,#69240,#69241));
#15437=EDGE_LOOP('',(#69242,#69243,#69244,#69245));
#15438=EDGE_LOOP('',(#69246,#69247,#69248,#69249));
#15439=EDGE_LOOP('',(#69250,#69251,#69252,#69253));
#15440=EDGE_LOOP('',(#69254,#69255,#69256,#69257,#69258));
#15441=EDGE_LOOP('',(#69259,#69260,#69261,#69262));
#15442=EDGE_LOOP('',(#69263,#69264,#69265,#69266));
#15443=EDGE_LOOP('',(#69267,#69268,#69269,#69270));
#15444=EDGE_LOOP('',(#69271,#69272,#69273,#69274));
#15445=EDGE_LOOP('',(#69275,#69276,#69277,#69278));
#15446=EDGE_LOOP('',(#69279,#69280,#69281,#69282));
#15447=EDGE_LOOP('',(#69283,#69284,#69285,#69286));
#15448=EDGE_LOOP('',(#69287,#69288,#69289,#69290));
#15449=EDGE_LOOP('',(#69291,#69292,#69293,#69294));
#15450=EDGE_LOOP('',(#69295,#69296,#69297,#69298));
#15451=EDGE_LOOP('',(#69299,#69300,#69301,#69302,#69303));
#15452=EDGE_LOOP('',(#69304,#69305,#69306,#69307));
#15453=EDGE_LOOP('',(#69308,#69309,#69310,#69311));
#15454=EDGE_LOOP('',(#69312,#69313,#69314,#69315));
#15455=EDGE_LOOP('',(#69316,#69317,#69318,#69319));
#15456=EDGE_LOOP('',(#69320,#69321,#69322,#69323));
#15457=EDGE_LOOP('',(#69324,#69325,#69326,#69327));
#15458=EDGE_LOOP('',(#69328,#69329,#69330,#69331));
#15459=EDGE_LOOP('',(#69332,#69333,#69334,#69335));
#15460=EDGE_LOOP('',(#69336,#69337,#69338,#69339,#69340));
#15461=EDGE_LOOP('',(#69341,#69342,#69343,#69344));
#15462=EDGE_LOOP('',(#69345,#69346,#69347,#69348));
#15463=EDGE_LOOP('',(#69349,#69350,#69351,#69352,#69353));
#15464=EDGE_LOOP('',(#69354,#69355,#69356,#69357));
#15465=EDGE_LOOP('',(#69358,#69359,#69360,#69361));
#15466=EDGE_LOOP('',(#69362,#69363,#69364,#69365));
#15467=EDGE_LOOP('',(#69366,#69367,#69368,#69369));
#15468=EDGE_LOOP('',(#69370,#69371,#69372,#69373,#69374));
#15469=EDGE_LOOP('',(#69375,#69376,#69377,#69378));
#15470=EDGE_LOOP('',(#69379,#69380,#69381,#69382));
#15471=EDGE_LOOP('',(#69383,#69384,#69385,#69386));
#15472=EDGE_LOOP('',(#69387,#69388,#69389,#69390));
#15473=EDGE_LOOP('',(#69391,#69392,#69393,#69394));
#15474=EDGE_LOOP('',(#69395,#69396,#69397,#69398));
#15475=EDGE_LOOP('',(#69399,#69400,#69401,#69402));
#15476=EDGE_LOOP('',(#69403,#69404,#69405,#69406));
#15477=EDGE_LOOP('',(#69407,#69408,#69409,#69410));
#15478=EDGE_LOOP('',(#69411,#69412,#69413,#69414));
#15479=EDGE_LOOP('',(#69415,#69416,#69417,#69418,#69419));
#15480=EDGE_LOOP('',(#69420,#69421,#69422,#69423));
#15481=EDGE_LOOP('',(#69424,#69425,#69426,#69427));
#15482=EDGE_LOOP('',(#69428,#69429,#69430,#69431));
#15483=EDGE_LOOP('',(#69432,#69433,#69434,#69435));
#15484=EDGE_LOOP('',(#69436,#69437,#69438,#69439));
#15485=EDGE_LOOP('',(#69440,#69441,#69442,#69443));
#15486=EDGE_LOOP('',(#69444,#69445,#69446,#69447));
#15487=EDGE_LOOP('',(#69448,#69449,#69450,#69451));
#15488=EDGE_LOOP('',(#69452,#69453,#69454,#69455,#69456));
#15489=EDGE_LOOP('',(#69457,#69458,#69459,#69460));
#15490=EDGE_LOOP('',(#69461,#69462,#69463,#69464));
#15491=EDGE_LOOP('',(#69465,#69466,#69467,#69468,#69469));
#15492=EDGE_LOOP('',(#69470,#69471,#69472,#69473));
#15493=EDGE_LOOP('',(#69474,#69475,#69476,#69477));
#15494=EDGE_LOOP('',(#69478,#69479,#69480,#69481));
#15495=EDGE_LOOP('',(#69482,#69483,#69484,#69485));
#15496=EDGE_LOOP('',(#69486,#69487,#69488,#69489,#69490));
#15497=EDGE_LOOP('',(#69491,#69492,#69493,#69494));
#15498=EDGE_LOOP('',(#69495,#69496,#69497,#69498));
#15499=EDGE_LOOP('',(#69499,#69500,#69501,#69502));
#15500=EDGE_LOOP('',(#69503,#69504,#69505,#69506));
#15501=EDGE_LOOP('',(#69507,#69508,#69509,#69510));
#15502=EDGE_LOOP('',(#69511,#69512,#69513,#69514));
#15503=EDGE_LOOP('',(#69515,#69516,#69517,#69518));
#15504=EDGE_LOOP('',(#69519,#69520,#69521,#69522));
#15505=EDGE_LOOP('',(#69523,#69524,#69525,#69526));
#15506=EDGE_LOOP('',(#69527,#69528,#69529,#69530));
#15507=EDGE_LOOP('',(#69531,#69532,#69533,#69534,#69535));
#15508=EDGE_LOOP('',(#69536,#69537,#69538,#69539));
#15509=EDGE_LOOP('',(#69540,#69541,#69542,#69543));
#15510=EDGE_LOOP('',(#69544,#69545,#69546,#69547));
#15511=EDGE_LOOP('',(#69548,#69549,#69550,#69551));
#15512=EDGE_LOOP('',(#69552,#69553,#69554,#69555));
#15513=EDGE_LOOP('',(#69556,#69557,#69558,#69559));
#15514=EDGE_LOOP('',(#69560,#69561,#69562,#69563));
#15515=EDGE_LOOP('',(#69564,#69565,#69566,#69567));
#15516=EDGE_LOOP('',(#69568,#69569,#69570,#69571,#69572));
#15517=EDGE_LOOP('',(#69573,#69574,#69575,#69576));
#15518=EDGE_LOOP('',(#69577,#69578,#69579,#69580));
#15519=EDGE_LOOP('',(#69581,#69582,#69583,#69584,#69585));
#15520=EDGE_LOOP('',(#69586,#69587,#69588,#69589));
#15521=EDGE_LOOP('',(#69590,#69591,#69592,#69593));
#15522=EDGE_LOOP('',(#69594,#69595,#69596,#69597));
#15523=EDGE_LOOP('',(#69598,#69599,#69600,#69601));
#15524=EDGE_LOOP('',(#69602,#69603,#69604,#69605,#69606));
#15525=EDGE_LOOP('',(#69607,#69608,#69609,#69610));
#15526=EDGE_LOOP('',(#69611,#69612,#69613,#69614));
#15527=EDGE_LOOP('',(#69615,#69616,#69617,#69618));
#15528=EDGE_LOOP('',(#69619,#69620,#69621,#69622));
#15529=EDGE_LOOP('',(#69623,#69624,#69625,#69626));
#15530=EDGE_LOOP('',(#69627,#69628,#69629,#69630));
#15531=EDGE_LOOP('',(#69631,#69632,#69633,#69634));
#15532=EDGE_LOOP('',(#69635,#69636,#69637,#69638));
#15533=EDGE_LOOP('',(#69639,#69640,#69641,#69642));
#15534=EDGE_LOOP('',(#69643,#69644,#69645,#69646));
#15535=EDGE_LOOP('',(#69647,#69648,#69649,#69650,#69651));
#15536=EDGE_LOOP('',(#69652,#69653,#69654,#69655));
#15537=EDGE_LOOP('',(#69656,#69657,#69658,#69659));
#15538=EDGE_LOOP('',(#69660,#69661,#69662,#69663));
#15539=EDGE_LOOP('',(#69664,#69665,#69666,#69667));
#15540=EDGE_LOOP('',(#69668,#69669,#69670,#69671));
#15541=EDGE_LOOP('',(#69672,#69673,#69674,#69675));
#15542=EDGE_LOOP('',(#69676,#69677,#69678,#69679));
#15543=EDGE_LOOP('',(#69680,#69681,#69682,#69683));
#15544=EDGE_LOOP('',(#69684,#69685,#69686,#69687,#69688));
#15545=EDGE_LOOP('',(#69689,#69690,#69691,#69692));
#15546=EDGE_LOOP('',(#69693,#69694,#69695,#69696));
#15547=EDGE_LOOP('',(#69697,#69698,#69699,#69700,#69701));
#15548=EDGE_LOOP('',(#69702,#69703,#69704,#69705));
#15549=EDGE_LOOP('',(#69706,#69707,#69708,#69709));
#15550=EDGE_LOOP('',(#69710,#69711,#69712,#69713));
#15551=EDGE_LOOP('',(#69714,#69715,#69716,#69717));
#15552=EDGE_LOOP('',(#69718,#69719,#69720,#69721,#69722));
#15553=EDGE_LOOP('',(#69723,#69724,#69725,#69726));
#15554=EDGE_LOOP('',(#69727,#69728,#69729,#69730));
#15555=EDGE_LOOP('',(#69731,#69732,#69733,#69734));
#15556=EDGE_LOOP('',(#69735,#69736,#69737,#69738));
#15557=EDGE_LOOP('',(#69739,#69740,#69741,#69742));
#15558=EDGE_LOOP('',(#69743,#69744,#69745,#69746));
#15559=EDGE_LOOP('',(#69747,#69748,#69749,#69750));
#15560=EDGE_LOOP('',(#69751,#69752,#69753,#69754));
#15561=EDGE_LOOP('',(#69755,#69756,#69757,#69758));
#15562=EDGE_LOOP('',(#69759,#69760,#69761,#69762));
#15563=EDGE_LOOP('',(#69763,#69764,#69765,#69766,#69767));
#15564=EDGE_LOOP('',(#69768,#69769,#69770,#69771));
#15565=EDGE_LOOP('',(#69772,#69773,#69774,#69775));
#15566=EDGE_LOOP('',(#69776,#69777,#69778,#69779));
#15567=EDGE_LOOP('',(#69780,#69781,#69782,#69783));
#15568=EDGE_LOOP('',(#69784,#69785,#69786,#69787));
#15569=EDGE_LOOP('',(#69788,#69789,#69790,#69791));
#15570=EDGE_LOOP('',(#69792,#69793,#69794,#69795));
#15571=EDGE_LOOP('',(#69796,#69797,#69798,#69799));
#15572=EDGE_LOOP('',(#69800,#69801,#69802,#69803,#69804));
#15573=EDGE_LOOP('',(#69805,#69806,#69807,#69808));
#15574=EDGE_LOOP('',(#69809,#69810,#69811,#69812));
#15575=EDGE_LOOP('',(#69813,#69814,#69815,#69816,#69817));
#15576=EDGE_LOOP('',(#69818,#69819,#69820,#69821));
#15577=EDGE_LOOP('',(#69822,#69823,#69824,#69825));
#15578=EDGE_LOOP('',(#69826,#69827,#69828,#69829));
#15579=EDGE_LOOP('',(#69830,#69831,#69832,#69833));
#15580=EDGE_LOOP('',(#69834,#69835,#69836,#69837,#69838));
#15581=EDGE_LOOP('',(#69839,#69840,#69841,#69842));
#15582=EDGE_LOOP('',(#69843,#69844,#69845,#69846));
#15583=EDGE_LOOP('',(#69847,#69848,#69849,#69850));
#15584=EDGE_LOOP('',(#69851,#69852,#69853,#69854));
#15585=EDGE_LOOP('',(#69855,#69856,#69857,#69858));
#15586=EDGE_LOOP('',(#69859,#69860,#69861,#69862));
#15587=EDGE_LOOP('',(#69863,#69864,#69865,#69866));
#15588=EDGE_LOOP('',(#69867,#69868,#69869,#69870));
#15589=EDGE_LOOP('',(#69871,#69872,#69873,#69874));
#15590=EDGE_LOOP('',(#69875,#69876,#69877,#69878));
#15591=EDGE_LOOP('',(#69879,#69880,#69881,#69882,#69883));
#15592=EDGE_LOOP('',(#69884,#69885,#69886,#69887));
#15593=EDGE_LOOP('',(#69888,#69889,#69890,#69891));
#15594=EDGE_LOOP('',(#69892,#69893,#69894,#69895));
#15595=EDGE_LOOP('',(#69896,#69897,#69898,#69899));
#15596=EDGE_LOOP('',(#69900,#69901,#69902,#69903));
#15597=EDGE_LOOP('',(#69904,#69905,#69906,#69907));
#15598=EDGE_LOOP('',(#69908,#69909,#69910,#69911));
#15599=EDGE_LOOP('',(#69912,#69913,#69914,#69915));
#15600=EDGE_LOOP('',(#69916,#69917,#69918,#69919,#69920));
#15601=EDGE_LOOP('',(#69921,#69922,#69923,#69924));
#15602=EDGE_LOOP('',(#69925,#69926,#69927,#69928));
#15603=EDGE_LOOP('',(#69929,#69930,#69931,#69932,#69933));
#15604=EDGE_LOOP('',(#69934,#69935,#69936,#69937));
#15605=EDGE_LOOP('',(#69938,#69939,#69940,#69941));
#15606=EDGE_LOOP('',(#69942,#69943,#69944,#69945));
#15607=EDGE_LOOP('',(#69946,#69947,#69948,#69949));
#15608=EDGE_LOOP('',(#69950,#69951,#69952,#69953,#69954));
#15609=EDGE_LOOP('',(#69955,#69956,#69957,#69958));
#15610=EDGE_LOOP('',(#69959,#69960,#69961,#69962));
#15611=EDGE_LOOP('',(#69963,#69964,#69965,#69966));
#15612=EDGE_LOOP('',(#69967,#69968,#69969,#69970));
#15613=EDGE_LOOP('',(#69971,#69972,#69973,#69974));
#15614=EDGE_LOOP('',(#69975,#69976,#69977,#69978));
#15615=EDGE_LOOP('',(#69979,#69980,#69981,#69982));
#15616=EDGE_LOOP('',(#69983,#69984,#69985,#69986));
#15617=EDGE_LOOP('',(#69987,#69988,#69989,#69990));
#15618=EDGE_LOOP('',(#69991,#69992,#69993,#69994));
#15619=EDGE_LOOP('',(#69995,#69996,#69997,#69998,#69999));
#15620=EDGE_LOOP('',(#70000,#70001,#70002,#70003));
#15621=EDGE_LOOP('',(#70004,#70005,#70006,#70007));
#15622=EDGE_LOOP('',(#70008,#70009,#70010,#70011));
#15623=EDGE_LOOP('',(#70012,#70013,#70014,#70015));
#15624=EDGE_LOOP('',(#70016,#70017,#70018,#70019));
#15625=EDGE_LOOP('',(#70020,#70021,#70022,#70023));
#15626=EDGE_LOOP('',(#70024,#70025,#70026,#70027));
#15627=EDGE_LOOP('',(#70028,#70029,#70030,#70031));
#15628=EDGE_LOOP('',(#70032,#70033,#70034,#70035,#70036));
#15629=EDGE_LOOP('',(#70037,#70038,#70039,#70040));
#15630=EDGE_LOOP('',(#70041,#70042,#70043,#70044));
#15631=EDGE_LOOP('',(#70045,#70046,#70047,#70048,#70049));
#15632=EDGE_LOOP('',(#70050,#70051,#70052,#70053));
#15633=EDGE_LOOP('',(#70054,#70055,#70056,#70057));
#15634=EDGE_LOOP('',(#70058,#70059,#70060,#70061));
#15635=EDGE_LOOP('',(#70062,#70063,#70064,#70065));
#15636=EDGE_LOOP('',(#70066,#70067,#70068,#70069,#70070));
#15637=EDGE_LOOP('',(#70071,#70072,#70073,#70074));
#15638=EDGE_LOOP('',(#70075,#70076,#70077,#70078));
#15639=EDGE_LOOP('',(#70079,#70080,#70081,#70082));
#15640=EDGE_LOOP('',(#70083,#70084,#70085,#70086));
#15641=EDGE_LOOP('',(#70087,#70088,#70089,#70090));
#15642=EDGE_LOOP('',(#70091,#70092,#70093,#70094));
#15643=EDGE_LOOP('',(#70095,#70096,#70097,#70098));
#15644=EDGE_LOOP('',(#70099,#70100,#70101,#70102));
#15645=EDGE_LOOP('',(#70103,#70104,#70105,#70106,#70107));
#15646=EDGE_LOOP('',(#70108,#70109,#70110,#70111));
#15647=EDGE_LOOP('',(#70112,#70113,#70114,#70115));
#15648=EDGE_LOOP('',(#70116,#70117,#70118,#70119));
#15649=EDGE_LOOP('',(#70120,#70121,#70122,#70123));
#15650=EDGE_LOOP('',(#70124,#70125,#70126,#70127));
#15651=EDGE_LOOP('',(#70128,#70129,#70130,#70131));
#15652=EDGE_LOOP('',(#70132,#70133,#70134,#70135));
#15653=EDGE_LOOP('',(#70136,#70137,#70138,#70139));
#15654=EDGE_LOOP('',(#70140,#70141,#70142,#70143,#70144));
#15655=EDGE_LOOP('',(#70145,#70146,#70147,#70148));
#15656=EDGE_LOOP('',(#70149,#70150,#70151,#70152));
#15657=EDGE_LOOP('',(#70153,#70154,#70155,#70156,#70157));
#15658=EDGE_LOOP('',(#70158,#70159,#70160,#70161));
#15659=EDGE_LOOP('',(#70162,#70163,#70164,#70165));
#15660=EDGE_LOOP('',(#70166,#70167,#70168,#70169));
#15661=EDGE_LOOP('',(#70170,#70171,#70172,#70173));
#15662=EDGE_LOOP('',(#70174,#70175,#70176,#70177,#70178));
#15663=EDGE_LOOP('',(#70179,#70180,#70181,#70182));
#15664=EDGE_LOOP('',(#70183,#70184,#70185,#70186));
#15665=EDGE_LOOP('',(#70187,#70188,#70189,#70190));
#15666=EDGE_LOOP('',(#70191,#70192,#70193,#70194));
#15667=EDGE_LOOP('',(#70195,#70196,#70197,#70198));
#15668=EDGE_LOOP('',(#70199,#70200,#70201,#70202));
#15669=EDGE_LOOP('',(#70203,#70204,#70205,#70206));
#15670=EDGE_LOOP('',(#70207,#70208,#70209,#70210));
#15671=EDGE_LOOP('',(#70211,#70212,#70213,#70214));
#15672=EDGE_LOOP('',(#70215,#70216,#70217,#70218));
#15673=EDGE_LOOP('',(#70219,#70220,#70221,#70222,#70223));
#15674=EDGE_LOOP('',(#70224,#70225,#70226,#70227));
#15675=EDGE_LOOP('',(#70228,#70229,#70230,#70231));
#15676=EDGE_LOOP('',(#70232,#70233,#70234,#70235));
#15677=EDGE_LOOP('',(#70236,#70237,#70238,#70239));
#15678=EDGE_LOOP('',(#70240,#70241,#70242,#70243));
#15679=EDGE_LOOP('',(#70244,#70245,#70246,#70247));
#15680=EDGE_LOOP('',(#70248,#70249,#70250,#70251));
#15681=EDGE_LOOP('',(#70252,#70253,#70254,#70255));
#15682=EDGE_LOOP('',(#70256,#70257,#70258,#70259,#70260));
#15683=EDGE_LOOP('',(#70261,#70262,#70263,#70264));
#15684=EDGE_LOOP('',(#70265,#70266,#70267,#70268));
#15685=EDGE_LOOP('',(#70269,#70270,#70271,#70272,#70273));
#15686=EDGE_LOOP('',(#70274,#70275,#70276,#70277));
#15687=EDGE_LOOP('',(#70278,#70279,#70280,#70281));
#15688=EDGE_LOOP('',(#70282,#70283,#70284,#70285));
#15689=EDGE_LOOP('',(#70286,#70287,#70288,#70289));
#15690=EDGE_LOOP('',(#70290,#70291,#70292,#70293,#70294));
#15691=EDGE_LOOP('',(#70295,#70296,#70297,#70298));
#15692=EDGE_LOOP('',(#70299,#70300,#70301,#70302));
#15693=EDGE_LOOP('',(#70303,#70304,#70305,#70306));
#15694=EDGE_LOOP('',(#70307,#70308,#70309,#70310));
#15695=EDGE_LOOP('',(#70311,#70312,#70313,#70314));
#15696=EDGE_LOOP('',(#70315,#70316,#70317,#70318));
#15697=EDGE_LOOP('',(#70319,#70320,#70321,#70322));
#15698=EDGE_LOOP('',(#70323,#70324,#70325,#70326));
#15699=EDGE_LOOP('',(#70327,#70328,#70329,#70330));
#15700=EDGE_LOOP('',(#70331,#70332,#70333,#70334));
#15701=EDGE_LOOP('',(#70335,#70336,#70337,#70338,#70339));
#15702=EDGE_LOOP('',(#70340,#70341,#70342,#70343));
#15703=EDGE_LOOP('',(#70344,#70345,#70346,#70347));
#15704=EDGE_LOOP('',(#70348,#70349,#70350,#70351));
#15705=EDGE_LOOP('',(#70352,#70353,#70354,#70355));
#15706=EDGE_LOOP('',(#70356,#70357,#70358,#70359));
#15707=EDGE_LOOP('',(#70360,#70361,#70362,#70363));
#15708=EDGE_LOOP('',(#70364,#70365,#70366,#70367));
#15709=EDGE_LOOP('',(#70368,#70369,#70370,#70371));
#15710=EDGE_LOOP('',(#70372,#70373,#70374,#70375,#70376));
#15711=EDGE_LOOP('',(#70377,#70378,#70379,#70380));
#15712=EDGE_LOOP('',(#70381,#70382,#70383,#70384));
#15713=EDGE_LOOP('',(#70385,#70386,#70387,#70388,#70389));
#15714=EDGE_LOOP('',(#70390,#70391,#70392,#70393));
#15715=EDGE_LOOP('',(#70394,#70395,#70396,#70397));
#15716=EDGE_LOOP('',(#70398,#70399,#70400,#70401));
#15717=EDGE_LOOP('',(#70402,#70403,#70404,#70405));
#15718=EDGE_LOOP('',(#70406,#70407,#70408,#70409,#70410));
#15719=EDGE_LOOP('',(#70411,#70412,#70413,#70414));
#15720=EDGE_LOOP('',(#70415,#70416,#70417,#70418));
#15721=EDGE_LOOP('',(#70419,#70420,#70421,#70422));
#15722=EDGE_LOOP('',(#70423,#70424,#70425,#70426));
#15723=EDGE_LOOP('',(#70427,#70428,#70429,#70430));
#15724=EDGE_LOOP('',(#70431,#70432,#70433,#70434));
#15725=EDGE_LOOP('',(#70435,#70436,#70437,#70438));
#15726=EDGE_LOOP('',(#70439,#70440,#70441,#70442));
#15727=EDGE_LOOP('',(#70443,#70444,#70445,#70446));
#15728=EDGE_LOOP('',(#70447,#70448,#70449,#70450));
#15729=EDGE_LOOP('',(#70451,#70452,#70453,#70454,#70455));
#15730=EDGE_LOOP('',(#70456,#70457,#70458,#70459));
#15731=EDGE_LOOP('',(#70460,#70461,#70462,#70463));
#15732=EDGE_LOOP('',(#70464,#70465,#70466,#70467));
#15733=EDGE_LOOP('',(#70468,#70469,#70470,#70471));
#15734=EDGE_LOOP('',(#70472,#70473,#70474,#70475));
#15735=EDGE_LOOP('',(#70476,#70477,#70478,#70479));
#15736=EDGE_LOOP('',(#70480,#70481,#70482,#70483));
#15737=EDGE_LOOP('',(#70484,#70485,#70486,#70487));
#15738=EDGE_LOOP('',(#70488,#70489,#70490,#70491,#70492));
#15739=EDGE_LOOP('',(#70493,#70494,#70495,#70496));
#15740=EDGE_LOOP('',(#70497,#70498,#70499,#70500));
#15741=EDGE_LOOP('',(#70501,#70502,#70503,#70504,#70505));
#15742=EDGE_LOOP('',(#70506,#70507,#70508,#70509));
#15743=EDGE_LOOP('',(#70510,#70511,#70512,#70513));
#15744=EDGE_LOOP('',(#70514,#70515,#70516,#70517));
#15745=EDGE_LOOP('',(#70518,#70519,#70520,#70521));
#15746=EDGE_LOOP('',(#70522,#70523,#70524,#70525,#70526));
#15747=EDGE_LOOP('',(#70527,#70528,#70529,#70530));
#15748=EDGE_LOOP('',(#70531,#70532,#70533,#70534));
#15749=EDGE_LOOP('',(#70535,#70536,#70537,#70538));
#15750=EDGE_LOOP('',(#70539,#70540,#70541,#70542));
#15751=EDGE_LOOP('',(#70543,#70544,#70545,#70546));
#15752=EDGE_LOOP('',(#70547,#70548,#70549,#70550));
#15753=EDGE_LOOP('',(#70551,#70552,#70553,#70554));
#15754=EDGE_LOOP('',(#70555,#70556,#70557,#70558));
#15755=EDGE_LOOP('',(#70559,#70560,#70561,#70562));
#15756=EDGE_LOOP('',(#70563,#70564,#70565,#70566));
#15757=EDGE_LOOP('',(#70567,#70568,#70569,#70570,#70571));
#15758=EDGE_LOOP('',(#70572,#70573,#70574,#70575));
#15759=EDGE_LOOP('',(#70576,#70577,#70578,#70579));
#15760=EDGE_LOOP('',(#70580,#70581,#70582,#70583));
#15761=EDGE_LOOP('',(#70584,#70585,#70586,#70587));
#15762=EDGE_LOOP('',(#70588,#70589,#70590,#70591));
#15763=EDGE_LOOP('',(#70592,#70593,#70594,#70595));
#15764=EDGE_LOOP('',(#70596,#70597,#70598,#70599));
#15765=EDGE_LOOP('',(#70600,#70601,#70602,#70603));
#15766=EDGE_LOOP('',(#70604,#70605,#70606,#70607,#70608));
#15767=EDGE_LOOP('',(#70609,#70610,#70611,#70612));
#15768=EDGE_LOOP('',(#70613,#70614,#70615,#70616));
#15769=EDGE_LOOP('',(#70617,#70618,#70619,#70620,#70621));
#15770=EDGE_LOOP('',(#70622,#70623,#70624,#70625));
#15771=EDGE_LOOP('',(#70626,#70627,#70628,#70629));
#15772=EDGE_LOOP('',(#70630,#70631,#70632,#70633));
#15773=EDGE_LOOP('',(#70634,#70635,#70636,#70637));
#15774=EDGE_LOOP('',(#70638,#70639,#70640,#70641,#70642));
#15775=EDGE_LOOP('',(#70643,#70644,#70645,#70646));
#15776=EDGE_LOOP('',(#70647,#70648,#70649,#70650));
#15777=EDGE_LOOP('',(#70651,#70652,#70653,#70654));
#15778=EDGE_LOOP('',(#70655,#70656,#70657,#70658));
#15779=EDGE_LOOP('',(#70659,#70660,#70661,#70662));
#15780=EDGE_LOOP('',(#70663,#70664,#70665,#70666));
#15781=EDGE_LOOP('',(#70667,#70668,#70669,#70670));
#15782=EDGE_LOOP('',(#70671,#70672,#70673,#70674));
#15783=EDGE_LOOP('',(#70675,#70676,#70677,#70678));
#15784=EDGE_LOOP('',(#70679,#70680,#70681,#70682));
#15785=EDGE_LOOP('',(#70683,#70684,#70685,#70686,#70687));
#15786=EDGE_LOOP('',(#70688,#70689,#70690,#70691));
#15787=EDGE_LOOP('',(#70692,#70693,#70694,#70695));
#15788=EDGE_LOOP('',(#70696,#70697,#70698,#70699));
#15789=EDGE_LOOP('',(#70700,#70701,#70702,#70703));
#15790=EDGE_LOOP('',(#70704,#70705,#70706,#70707));
#15791=EDGE_LOOP('',(#70708,#70709,#70710,#70711));
#15792=EDGE_LOOP('',(#70712,#70713,#70714,#70715));
#15793=EDGE_LOOP('',(#70716,#70717,#70718,#70719));
#15794=EDGE_LOOP('',(#70720,#70721,#70722,#70723,#70724));
#15795=EDGE_LOOP('',(#70725,#70726,#70727,#70728));
#15796=EDGE_LOOP('',(#70729,#70730,#70731,#70732));
#15797=EDGE_LOOP('',(#70733,#70734,#70735,#70736,#70737));
#15798=EDGE_LOOP('',(#70738,#70739,#70740,#70741));
#15799=EDGE_LOOP('',(#70742,#70743,#70744,#70745));
#15800=EDGE_LOOP('',(#70746,#70747,#70748,#70749));
#15801=EDGE_LOOP('',(#70750,#70751,#70752,#70753));
#15802=EDGE_LOOP('',(#70754,#70755,#70756,#70757,#70758));
#15803=EDGE_LOOP('',(#70759,#70760,#70761,#70762));
#15804=EDGE_LOOP('',(#70763,#70764,#70765,#70766));
#15805=EDGE_LOOP('',(#70767,#70768,#70769,#70770));
#15806=EDGE_LOOP('',(#70771,#70772,#70773,#70774));
#15807=EDGE_LOOP('',(#70775,#70776,#70777,#70778));
#15808=EDGE_LOOP('',(#70779,#70780,#70781,#70782));
#15809=EDGE_LOOP('',(#70783,#70784,#70785,#70786));
#15810=EDGE_LOOP('',(#70787,#70788,#70789,#70790));
#15811=EDGE_LOOP('',(#70791,#70792,#70793,#70794));
#15812=EDGE_LOOP('',(#70795,#70796,#70797,#70798));
#15813=EDGE_LOOP('',(#70799,#70800,#70801,#70802,#70803));
#15814=EDGE_LOOP('',(#70804,#70805,#70806,#70807));
#15815=EDGE_LOOP('',(#70808,#70809,#70810,#70811));
#15816=EDGE_LOOP('',(#70812,#70813,#70814,#70815));
#15817=EDGE_LOOP('',(#70816,#70817,#70818,#70819));
#15818=EDGE_LOOP('',(#70820,#70821,#70822,#70823));
#15819=EDGE_LOOP('',(#70824,#70825,#70826,#70827));
#15820=EDGE_LOOP('',(#70828,#70829,#70830,#70831));
#15821=EDGE_LOOP('',(#70832,#70833,#70834,#70835));
#15822=EDGE_LOOP('',(#70836,#70837,#70838,#70839,#70840));
#15823=EDGE_LOOP('',(#70841,#70842,#70843,#70844));
#15824=EDGE_LOOP('',(#70845,#70846,#70847,#70848));
#15825=EDGE_LOOP('',(#70849,#70850,#70851,#70852,#70853));
#15826=EDGE_LOOP('',(#70854,#70855,#70856,#70857));
#15827=EDGE_LOOP('',(#70858,#70859,#70860,#70861));
#15828=EDGE_LOOP('',(#70862,#70863,#70864,#70865));
#15829=EDGE_LOOP('',(#70866,#70867,#70868,#70869));
#15830=EDGE_LOOP('',(#70870,#70871,#70872,#70873,#70874));
#15831=EDGE_LOOP('',(#70875,#70876,#70877,#70878));
#15832=EDGE_LOOP('',(#70879,#70880,#70881,#70882));
#15833=EDGE_LOOP('',(#70883,#70884,#70885,#70886));
#15834=EDGE_LOOP('',(#70887,#70888,#70889,#70890));
#15835=EDGE_LOOP('',(#70891,#70892,#70893,#70894));
#15836=EDGE_LOOP('',(#70895,#70896,#70897,#70898));
#15837=EDGE_LOOP('',(#70899,#70900,#70901,#70902));
#15838=EDGE_LOOP('',(#70903,#70904,#70905,#70906));
#15839=EDGE_LOOP('',(#70907,#70908,#70909,#70910));
#15840=EDGE_LOOP('',(#70911,#70912,#70913,#70914));
#15841=EDGE_LOOP('',(#70915,#70916,#70917,#70918,#70919));
#15842=EDGE_LOOP('',(#70920,#70921,#70922,#70923));
#15843=EDGE_LOOP('',(#70924,#70925,#70926,#70927));
#15844=EDGE_LOOP('',(#70928,#70929,#70930,#70931));
#15845=EDGE_LOOP('',(#70932,#70933,#70934,#70935));
#15846=EDGE_LOOP('',(#70936,#70937,#70938,#70939));
#15847=EDGE_LOOP('',(#70940,#70941,#70942,#70943));
#15848=EDGE_LOOP('',(#70944,#70945,#70946,#70947));
#15849=EDGE_LOOP('',(#70948,#70949,#70950,#70951));
#15850=EDGE_LOOP('',(#70952,#70953,#70954,#70955,#70956));
#15851=EDGE_LOOP('',(#70957,#70958,#70959,#70960));
#15852=EDGE_LOOP('',(#70961,#70962,#70963,#70964));
#15853=EDGE_LOOP('',(#70965,#70966,#70967,#70968,#70969));
#15854=EDGE_LOOP('',(#70970,#70971,#70972,#70973));
#15855=EDGE_LOOP('',(#70974,#70975,#70976,#70977));
#15856=EDGE_LOOP('',(#70978,#70979,#70980,#70981));
#15857=EDGE_LOOP('',(#70982,#70983,#70984,#70985));
#15858=EDGE_LOOP('',(#70986,#70987,#70988,#70989,#70990));
#15859=EDGE_LOOP('',(#70991,#70992,#70993,#70994));
#15860=EDGE_LOOP('',(#70995,#70996,#70997,#70998));
#15861=EDGE_LOOP('',(#70999,#71000,#71001,#71002));
#15862=EDGE_LOOP('',(#71003,#71004,#71005,#71006));
#15863=EDGE_LOOP('',(#71007,#71008,#71009,#71010));
#15864=EDGE_LOOP('',(#71011,#71012,#71013,#71014));
#15865=EDGE_LOOP('',(#71015,#71016,#71017,#71018));
#15866=EDGE_LOOP('',(#71019,#71020,#71021,#71022));
#15867=EDGE_LOOP('',(#71023,#71024,#71025,#71026));
#15868=EDGE_LOOP('',(#71027,#71028,#71029,#71030));
#15869=EDGE_LOOP('',(#71031,#71032,#71033,#71034,#71035));
#15870=EDGE_LOOP('',(#71036,#71037,#71038,#71039));
#15871=EDGE_LOOP('',(#71040,#71041,#71042,#71043));
#15872=EDGE_LOOP('',(#71044,#71045,#71046,#71047));
#15873=EDGE_LOOP('',(#71048,#71049,#71050,#71051));
#15874=EDGE_LOOP('',(#71052,#71053,#71054,#71055));
#15875=EDGE_LOOP('',(#71056,#71057,#71058,#71059));
#15876=EDGE_LOOP('',(#71060,#71061,#71062,#71063));
#15877=EDGE_LOOP('',(#71064,#71065,#71066,#71067));
#15878=EDGE_LOOP('',(#71068,#71069,#71070,#71071,#71072));
#15879=EDGE_LOOP('',(#71073,#71074,#71075,#71076));
#15880=EDGE_LOOP('',(#71077,#71078,#71079,#71080));
#15881=EDGE_LOOP('',(#71081,#71082,#71083,#71084,#71085));
#15882=EDGE_LOOP('',(#71086,#71087,#71088,#71089));
#15883=EDGE_LOOP('',(#71090,#71091,#71092,#71093));
#15884=EDGE_LOOP('',(#71094,#71095,#71096,#71097));
#15885=EDGE_LOOP('',(#71098,#71099,#71100,#71101));
#15886=EDGE_LOOP('',(#71102,#71103,#71104,#71105,#71106));
#15887=EDGE_LOOP('',(#71107,#71108,#71109,#71110));
#15888=EDGE_LOOP('',(#71111,#71112,#71113,#71114));
#15889=EDGE_LOOP('',(#71115,#71116,#71117,#71118));
#15890=EDGE_LOOP('',(#71119,#71120,#71121,#71122));
#15891=EDGE_LOOP('',(#71123,#71124,#71125,#71126));
#15892=EDGE_LOOP('',(#71127,#71128,#71129,#71130));
#15893=EDGE_LOOP('',(#71131,#71132,#71133,#71134));
#15894=EDGE_LOOP('',(#71135,#71136,#71137,#71138));
#15895=EDGE_LOOP('',(#71139,#71140,#71141,#71142));
#15896=EDGE_LOOP('',(#71143,#71144,#71145,#71146));
#15897=EDGE_LOOP('',(#71147,#71148,#71149,#71150,#71151));
#15898=EDGE_LOOP('',(#71152,#71153,#71154,#71155));
#15899=EDGE_LOOP('',(#71156,#71157,#71158,#71159));
#15900=EDGE_LOOP('',(#71160,#71161,#71162,#71163));
#15901=EDGE_LOOP('',(#71164,#71165,#71166,#71167));
#15902=EDGE_LOOP('',(#71168,#71169,#71170,#71171));
#15903=EDGE_LOOP('',(#71172,#71173,#71174,#71175));
#15904=EDGE_LOOP('',(#71176,#71177,#71178,#71179));
#15905=EDGE_LOOP('',(#71180,#71181,#71182,#71183));
#15906=EDGE_LOOP('',(#71184,#71185,#71186,#71187,#71188));
#15907=EDGE_LOOP('',(#71189,#71190,#71191,#71192));
#15908=EDGE_LOOP('',(#71193,#71194,#71195,#71196));
#15909=EDGE_LOOP('',(#71197,#71198,#71199,#71200,#71201));
#15910=EDGE_LOOP('',(#71202,#71203,#71204,#71205));
#15911=EDGE_LOOP('',(#71206,#71207,#71208,#71209));
#15912=EDGE_LOOP('',(#71210,#71211,#71212,#71213));
#15913=EDGE_LOOP('',(#71214,#71215,#71216,#71217));
#15914=EDGE_LOOP('',(#71218,#71219,#71220,#71221,#71222));
#15915=EDGE_LOOP('',(#71223,#71224,#71225,#71226));
#15916=EDGE_LOOP('',(#71227,#71228,#71229,#71230));
#15917=EDGE_LOOP('',(#71231,#71232,#71233,#71234));
#15918=EDGE_LOOP('',(#71235,#71236,#71237,#71238));
#15919=EDGE_LOOP('',(#71239,#71240,#71241,#71242));
#15920=EDGE_LOOP('',(#71243,#71244,#71245,#71246));
#15921=EDGE_LOOP('',(#71247,#71248,#71249,#71250));
#15922=EDGE_LOOP('',(#71251,#71252,#71253,#71254));
#15923=EDGE_LOOP('',(#71255,#71256,#71257,#71258));
#15924=EDGE_LOOP('',(#71259,#71260,#71261,#71262));
#15925=EDGE_LOOP('',(#71263,#71264,#71265,#71266,#71267));
#15926=EDGE_LOOP('',(#71268,#71269,#71270,#71271));
#15927=EDGE_LOOP('',(#71272,#71273,#71274,#71275));
#15928=EDGE_LOOP('',(#71276,#71277,#71278,#71279));
#15929=EDGE_LOOP('',(#71280,#71281,#71282,#71283));
#15930=EDGE_LOOP('',(#71284,#71285,#71286,#71287));
#15931=EDGE_LOOP('',(#71288,#71289,#71290,#71291));
#15932=EDGE_LOOP('',(#71292,#71293,#71294,#71295));
#15933=EDGE_LOOP('',(#71296,#71297,#71298,#71299));
#15934=EDGE_LOOP('',(#71300,#71301,#71302,#71303,#71304));
#15935=EDGE_LOOP('',(#71305,#71306,#71307,#71308));
#15936=EDGE_LOOP('',(#71309,#71310,#71311,#71312));
#15937=EDGE_LOOP('',(#71313,#71314,#71315,#71316,#71317));
#15938=EDGE_LOOP('',(#71318,#71319,#71320,#71321));
#15939=EDGE_LOOP('',(#71322,#71323,#71324,#71325));
#15940=EDGE_LOOP('',(#71326,#71327,#71328,#71329));
#15941=EDGE_LOOP('',(#71330,#71331,#71332,#71333));
#15942=EDGE_LOOP('',(#71334,#71335,#71336,#71337,#71338));
#15943=EDGE_LOOP('',(#71339,#71340,#71341,#71342));
#15944=EDGE_LOOP('',(#71343,#71344,#71345,#71346));
#15945=EDGE_LOOP('',(#71347,#71348,#71349,#71350));
#15946=EDGE_LOOP('',(#71351,#71352,#71353,#71354));
#15947=EDGE_LOOP('',(#71355,#71356,#71357,#71358));
#15948=EDGE_LOOP('',(#71359,#71360,#71361,#71362));
#15949=EDGE_LOOP('',(#71363,#71364,#71365,#71366));
#15950=EDGE_LOOP('',(#71367,#71368,#71369,#71370));
#15951=EDGE_LOOP('',(#71371,#71372,#71373,#71374));
#15952=EDGE_LOOP('',(#71375,#71376,#71377,#71378));
#15953=EDGE_LOOP('',(#71379,#71380,#71381,#71382,#71383));
#15954=EDGE_LOOP('',(#71384,#71385,#71386,#71387));
#15955=EDGE_LOOP('',(#71388,#71389,#71390,#71391));
#15956=EDGE_LOOP('',(#71392,#71393,#71394,#71395));
#15957=EDGE_LOOP('',(#71396,#71397,#71398,#71399));
#15958=EDGE_LOOP('',(#71400,#71401,#71402,#71403));
#15959=EDGE_LOOP('',(#71404,#71405,#71406,#71407));
#15960=EDGE_LOOP('',(#71408,#71409,#71410,#71411));
#15961=EDGE_LOOP('',(#71412,#71413,#71414,#71415));
#15962=EDGE_LOOP('',(#71416,#71417,#71418,#71419,#71420));
#15963=EDGE_LOOP('',(#71421,#71422,#71423,#71424));
#15964=EDGE_LOOP('',(#71425,#71426,#71427,#71428));
#15965=EDGE_LOOP('',(#71429,#71430,#71431,#71432,#71433));
#15966=EDGE_LOOP('',(#71434,#71435,#71436,#71437));
#15967=EDGE_LOOP('',(#71438,#71439,#71440,#71441));
#15968=EDGE_LOOP('',(#71442,#71443,#71444,#71445));
#15969=EDGE_LOOP('',(#71446,#71447,#71448,#71449));
#15970=EDGE_LOOP('',(#71450,#71451,#71452,#71453,#71454));
#15971=EDGE_LOOP('',(#71455,#71456,#71457,#71458));
#15972=EDGE_LOOP('',(#71459,#71460,#71461,#71462));
#15973=EDGE_LOOP('',(#71463,#71464,#71465,#71466));
#15974=EDGE_LOOP('',(#71467,#71468,#71469,#71470));
#15975=EDGE_LOOP('',(#71471,#71472,#71473,#71474));
#15976=EDGE_LOOP('',(#71475,#71476,#71477,#71478));
#15977=EDGE_LOOP('',(#71479,#71480,#71481,#71482));
#15978=EDGE_LOOP('',(#71483,#71484,#71485,#71486));
#15979=EDGE_LOOP('',(#71487,#71488,#71489,#71490));
#15980=EDGE_LOOP('',(#71491,#71492,#71493,#71494));
#15981=EDGE_LOOP('',(#71495,#71496,#71497,#71498,#71499));
#15982=EDGE_LOOP('',(#71500,#71501,#71502,#71503));
#15983=EDGE_LOOP('',(#71504,#71505,#71506,#71507));
#15984=EDGE_LOOP('',(#71508,#71509,#71510,#71511));
#15985=EDGE_LOOP('',(#71512,#71513,#71514,#71515));
#15986=EDGE_LOOP('',(#71516,#71517,#71518,#71519));
#15987=EDGE_LOOP('',(#71520,#71521,#71522,#71523));
#15988=EDGE_LOOP('',(#71524,#71525,#71526,#71527));
#15989=EDGE_LOOP('',(#71528,#71529,#71530,#71531));
#15990=EDGE_LOOP('',(#71532,#71533,#71534,#71535,#71536));
#15991=EDGE_LOOP('',(#71537,#71538,#71539,#71540));
#15992=EDGE_LOOP('',(#71541,#71542,#71543,#71544));
#15993=EDGE_LOOP('',(#71545,#71546,#71547,#71548,#71549));
#15994=EDGE_LOOP('',(#71550,#71551,#71552,#71553));
#15995=EDGE_LOOP('',(#71554,#71555,#71556,#71557));
#15996=EDGE_LOOP('',(#71558,#71559,#71560,#71561));
#15997=EDGE_LOOP('',(#71562,#71563,#71564,#71565));
#15998=EDGE_LOOP('',(#71566,#71567,#71568,#71569,#71570));
#15999=EDGE_LOOP('',(#71571,#71572,#71573,#71574));
#16000=EDGE_LOOP('',(#71575,#71576,#71577,#71578));
#16001=EDGE_LOOP('',(#71579,#71580,#71581,#71582));
#16002=EDGE_LOOP('',(#71583,#71584,#71585,#71586));
#16003=EDGE_LOOP('',(#71587,#71588,#71589,#71590));
#16004=EDGE_LOOP('',(#71591,#71592,#71593,#71594));
#16005=EDGE_LOOP('',(#71595,#71596,#71597,#71598));
#16006=EDGE_LOOP('',(#71599,#71600,#71601,#71602));
#16007=EDGE_LOOP('',(#71603,#71604,#71605,#71606));
#16008=EDGE_LOOP('',(#71607,#71608,#71609,#71610));
#16009=EDGE_LOOP('',(#71611,#71612,#71613,#71614,#71615));
#16010=EDGE_LOOP('',(#71616,#71617,#71618,#71619));
#16011=EDGE_LOOP('',(#71620,#71621,#71622,#71623));
#16012=EDGE_LOOP('',(#71624,#71625,#71626,#71627));
#16013=EDGE_LOOP('',(#71628,#71629,#71630,#71631));
#16014=EDGE_LOOP('',(#71632,#71633,#71634,#71635));
#16015=EDGE_LOOP('',(#71636,#71637,#71638,#71639));
#16016=EDGE_LOOP('',(#71640,#71641,#71642,#71643));
#16017=EDGE_LOOP('',(#71644,#71645,#71646,#71647));
#16018=EDGE_LOOP('',(#71648,#71649,#71650,#71651,#71652));
#16019=EDGE_LOOP('',(#71653,#71654,#71655,#71656));
#16020=EDGE_LOOP('',(#71657,#71658,#71659,#71660));
#16021=EDGE_LOOP('',(#71661,#71662,#71663,#71664,#71665));
#16022=EDGE_LOOP('',(#71666,#71667,#71668,#71669));
#16023=EDGE_LOOP('',(#71670,#71671,#71672,#71673));
#16024=EDGE_LOOP('',(#71674,#71675,#71676,#71677));
#16025=EDGE_LOOP('',(#71678,#71679,#71680,#71681));
#16026=EDGE_LOOP('',(#71682,#71683,#71684,#71685,#71686));
#16027=EDGE_LOOP('',(#71687,#71688,#71689,#71690));
#16028=EDGE_LOOP('',(#71691,#71692,#71693,#71694));
#16029=EDGE_LOOP('',(#71695,#71696,#71697,#71698));
#16030=EDGE_LOOP('',(#71699,#71700,#71701,#71702));
#16031=EDGE_LOOP('',(#71703,#71704,#71705,#71706));
#16032=EDGE_LOOP('',(#71707,#71708,#71709,#71710));
#16033=EDGE_LOOP('',(#71711,#71712,#71713,#71714));
#16034=EDGE_LOOP('',(#71715,#71716,#71717,#71718));
#16035=EDGE_LOOP('',(#71719,#71720,#71721,#71722));
#16036=EDGE_LOOP('',(#71723,#71724,#71725,#71726));
#16037=EDGE_LOOP('',(#71727,#71728,#71729,#71730,#71731));
#16038=EDGE_LOOP('',(#71732,#71733,#71734,#71735));
#16039=EDGE_LOOP('',(#71736,#71737,#71738,#71739));
#16040=EDGE_LOOP('',(#71740,#71741,#71742,#71743));
#16041=EDGE_LOOP('',(#71744,#71745,#71746,#71747));
#16042=EDGE_LOOP('',(#71748,#71749,#71750,#71751));
#16043=EDGE_LOOP('',(#71752,#71753,#71754,#71755));
#16044=EDGE_LOOP('',(#71756,#71757,#71758,#71759));
#16045=EDGE_LOOP('',(#71760,#71761,#71762,#71763));
#16046=EDGE_LOOP('',(#71764,#71765,#71766,#71767,#71768));
#16047=EDGE_LOOP('',(#71769,#71770,#71771,#71772));
#16048=EDGE_LOOP('',(#71773,#71774,#71775,#71776));
#16049=EDGE_LOOP('',(#71777,#71778,#71779,#71780,#71781));
#16050=EDGE_LOOP('',(#71782,#71783,#71784,#71785));
#16051=EDGE_LOOP('',(#71786,#71787,#71788,#71789));
#16052=EDGE_LOOP('',(#71790,#71791,#71792,#71793));
#16053=EDGE_LOOP('',(#71794,#71795,#71796,#71797));
#16054=EDGE_LOOP('',(#71798,#71799,#71800,#71801,#71802));
#16055=EDGE_LOOP('',(#71803,#71804,#71805,#71806));
#16056=EDGE_LOOP('',(#71807,#71808,#71809,#71810));
#16057=EDGE_LOOP('',(#71811,#71812,#71813,#71814));
#16058=EDGE_LOOP('',(#71815,#71816,#71817,#71818));
#16059=EDGE_LOOP('',(#71819,#71820,#71821,#71822));
#16060=EDGE_LOOP('',(#71823,#71824,#71825,#71826));
#16061=EDGE_LOOP('',(#71827,#71828,#71829,#71830));
#16062=EDGE_LOOP('',(#71831,#71832,#71833,#71834));
#16063=EDGE_LOOP('',(#71835,#71836,#71837,#71838,#71839));
#16064=EDGE_LOOP('',(#71840,#71841,#71842,#71843));
#16065=EDGE_LOOP('',(#71844,#71845,#71846,#71847));
#16066=EDGE_LOOP('',(#71848,#71849,#71850,#71851));
#16067=EDGE_LOOP('',(#71852,#71853,#71854,#71855));
#16068=EDGE_LOOP('',(#71856,#71857,#71858,#71859));
#16069=EDGE_LOOP('',(#71860,#71861,#71862,#71863));
#16070=EDGE_LOOP('',(#71864,#71865,#71866,#71867));
#16071=EDGE_LOOP('',(#71868,#71869,#71870,#71871));
#16072=EDGE_LOOP('',(#71872,#71873,#71874,#71875,#71876));
#16073=EDGE_LOOP('',(#71877,#71878,#71879,#71880));
#16074=EDGE_LOOP('',(#71881,#71882,#71883,#71884));
#16075=EDGE_LOOP('',(#71885,#71886,#71887,#71888,#71889));
#16076=EDGE_LOOP('',(#71890,#71891,#71892,#71893));
#16077=EDGE_LOOP('',(#71894,#71895,#71896,#71897));
#16078=EDGE_LOOP('',(#71898,#71899,#71900,#71901));
#16079=EDGE_LOOP('',(#71902,#71903,#71904,#71905));
#16080=EDGE_LOOP('',(#71906,#71907,#71908,#71909,#71910));
#16081=EDGE_LOOP('',(#71911,#71912,#71913,#71914));
#16082=EDGE_LOOP('',(#71915,#71916,#71917,#71918));
#16083=EDGE_LOOP('',(#71919,#71920,#71921,#71922));
#16084=EDGE_LOOP('',(#71923,#71924,#71925,#71926));
#16085=EDGE_LOOP('',(#71927,#71928,#71929,#71930));
#16086=EDGE_LOOP('',(#71931,#71932,#71933,#71934));
#16087=EDGE_LOOP('',(#71935,#71936,#71937,#71938));
#16088=EDGE_LOOP('',(#71939,#71940,#71941,#71942));
#16089=EDGE_LOOP('',(#71943,#71944,#71945,#71946));
#16090=EDGE_LOOP('',(#71947,#71948,#71949,#71950));
#16091=EDGE_LOOP('',(#71951,#71952,#71953,#71954,#71955));
#16092=EDGE_LOOP('',(#71956,#71957,#71958,#71959));
#16093=EDGE_LOOP('',(#71960,#71961,#71962,#71963));
#16094=EDGE_LOOP('',(#71964,#71965,#71966,#71967));
#16095=EDGE_LOOP('',(#71968,#71969,#71970,#71971));
#16096=EDGE_LOOP('',(#71972,#71973,#71974,#71975));
#16097=EDGE_LOOP('',(#71976,#71977,#71978,#71979));
#16098=EDGE_LOOP('',(#71980,#71981,#71982,#71983));
#16099=EDGE_LOOP('',(#71984,#71985,#71986,#71987));
#16100=EDGE_LOOP('',(#71988,#71989,#71990,#71991,#71992));
#16101=EDGE_LOOP('',(#71993,#71994,#71995,#71996));
#16102=EDGE_LOOP('',(#71997,#71998,#71999,#72000));
#16103=EDGE_LOOP('',(#72001,#72002,#72003,#72004,#72005));
#16104=EDGE_LOOP('',(#72006,#72007,#72008,#72009));
#16105=EDGE_LOOP('',(#72010,#72011,#72012,#72013));
#16106=EDGE_LOOP('',(#72014,#72015,#72016,#72017));
#16107=EDGE_LOOP('',(#72018,#72019,#72020,#72021));
#16108=EDGE_LOOP('',(#72022,#72023,#72024,#72025,#72026));
#16109=EDGE_LOOP('',(#72027,#72028,#72029,#72030));
#16110=EDGE_LOOP('',(#72031,#72032,#72033,#72034));
#16111=EDGE_LOOP('',(#72035,#72036,#72037,#72038));
#16112=EDGE_LOOP('',(#72039,#72040,#72041,#72042));
#16113=EDGE_LOOP('',(#72043,#72044,#72045,#72046));
#16114=EDGE_LOOP('',(#72047,#72048,#72049,#72050));
#16115=EDGE_LOOP('',(#72051,#72052,#72053,#72054));
#16116=EDGE_LOOP('',(#72055,#72056,#72057,#72058));
#16117=EDGE_LOOP('',(#72059,#72060,#72061,#72062));
#16118=EDGE_LOOP('',(#72063,#72064,#72065,#72066));
#16119=EDGE_LOOP('',(#72067,#72068,#72069,#72070,#72071));
#16120=EDGE_LOOP('',(#72072,#72073,#72074,#72075));
#16121=EDGE_LOOP('',(#72076,#72077,#72078,#72079));
#16122=EDGE_LOOP('',(#72080,#72081,#72082,#72083));
#16123=EDGE_LOOP('',(#72084,#72085,#72086,#72087));
#16124=EDGE_LOOP('',(#72088,#72089,#72090,#72091));
#16125=EDGE_LOOP('',(#72092,#72093,#72094,#72095));
#16126=EDGE_LOOP('',(#72096,#72097,#72098,#72099));
#16127=EDGE_LOOP('',(#72100,#72101,#72102,#72103));
#16128=EDGE_LOOP('',(#72104,#72105,#72106,#72107,#72108));
#16129=EDGE_LOOP('',(#72109,#72110,#72111,#72112));
#16130=EDGE_LOOP('',(#72113,#72114,#72115,#72116));
#16131=EDGE_LOOP('',(#72117,#72118,#72119,#72120,#72121));
#16132=EDGE_LOOP('',(#72122,#72123,#72124,#72125));
#16133=EDGE_LOOP('',(#72126,#72127,#72128,#72129));
#16134=EDGE_LOOP('',(#72130,#72131,#72132,#72133));
#16135=EDGE_LOOP('',(#72134,#72135,#72136,#72137));
#16136=EDGE_LOOP('',(#72138,#72139,#72140,#72141,#72142));
#16137=EDGE_LOOP('',(#72143,#72144,#72145,#72146));
#16138=EDGE_LOOP('',(#72147,#72148,#72149,#72150));
#16139=EDGE_LOOP('',(#72151,#72152,#72153,#72154));
#16140=EDGE_LOOP('',(#72155,#72156,#72157,#72158));
#16141=EDGE_LOOP('',(#72159,#72160,#72161,#72162));
#16142=EDGE_LOOP('',(#72163,#72164,#72165,#72166));
#16143=EDGE_LOOP('',(#72167,#72168,#72169,#72170));
#16144=EDGE_LOOP('',(#72171,#72172,#72173,#72174));
#16145=EDGE_LOOP('',(#72175,#72176,#72177,#72178));
#16146=EDGE_LOOP('',(#72179,#72180,#72181,#72182));
#16147=EDGE_LOOP('',(#72183,#72184,#72185,#72186,#72187));
#16148=EDGE_LOOP('',(#72188,#72189,#72190,#72191));
#16149=EDGE_LOOP('',(#72192,#72193,#72194,#72195));
#16150=EDGE_LOOP('',(#72196,#72197,#72198,#72199));
#16151=EDGE_LOOP('',(#72200,#72201,#72202,#72203));
#16152=EDGE_LOOP('',(#72204,#72205,#72206,#72207));
#16153=EDGE_LOOP('',(#72208,#72209,#72210,#72211));
#16154=EDGE_LOOP('',(#72212,#72213,#72214,#72215));
#16155=EDGE_LOOP('',(#72216,#72217,#72218,#72219));
#16156=EDGE_LOOP('',(#72220,#72221,#72222,#72223,#72224));
#16157=EDGE_LOOP('',(#72225,#72226,#72227,#72228));
#16158=EDGE_LOOP('',(#72229,#72230,#72231,#72232));
#16159=EDGE_LOOP('',(#72233,#72234,#72235,#72236,#72237));
#16160=EDGE_LOOP('',(#72238,#72239,#72240,#72241));
#16161=EDGE_LOOP('',(#72242,#72243,#72244,#72245));
#16162=EDGE_LOOP('',(#72246,#72247,#72248,#72249));
#16163=EDGE_LOOP('',(#72250,#72251,#72252,#72253));
#16164=EDGE_LOOP('',(#72254,#72255,#72256,#72257,#72258));
#16165=EDGE_LOOP('',(#72259,#72260,#72261,#72262));
#16166=EDGE_LOOP('',(#72263,#72264,#72265,#72266));
#16167=EDGE_LOOP('',(#72267,#72268,#72269,#72270));
#16168=EDGE_LOOP('',(#72271,#72272,#72273,#72274));
#16169=EDGE_LOOP('',(#72275,#72276,#72277,#72278));
#16170=EDGE_LOOP('',(#72279,#72280,#72281,#72282));
#16171=EDGE_LOOP('',(#72283,#72284,#72285,#72286));
#16172=EDGE_LOOP('',(#72287,#72288,#72289,#72290));
#16173=EDGE_LOOP('',(#72291,#72292,#72293,#72294));
#16174=EDGE_LOOP('',(#72295,#72296,#72297,#72298));
#16175=EDGE_LOOP('',(#72299,#72300,#72301,#72302,#72303));
#16176=EDGE_LOOP('',(#72304,#72305,#72306,#72307));
#16177=EDGE_LOOP('',(#72308,#72309,#72310,#72311));
#16178=EDGE_LOOP('',(#72312,#72313,#72314,#72315));
#16179=EDGE_LOOP('',(#72316,#72317,#72318,#72319));
#16180=EDGE_LOOP('',(#72320,#72321,#72322,#72323));
#16181=EDGE_LOOP('',(#72324,#72325,#72326,#72327));
#16182=EDGE_LOOP('',(#72328,#72329,#72330,#72331));
#16183=EDGE_LOOP('',(#72332,#72333,#72334,#72335));
#16184=EDGE_LOOP('',(#72336,#72337,#72338,#72339,#72340));
#16185=EDGE_LOOP('',(#72341,#72342,#72343,#72344));
#16186=EDGE_LOOP('',(#72345,#72346,#72347,#72348));
#16187=EDGE_LOOP('',(#72349,#72350,#72351,#72352,#72353));
#16188=EDGE_LOOP('',(#72354,#72355,#72356,#72357));
#16189=EDGE_LOOP('',(#72358,#72359,#72360,#72361));
#16190=EDGE_LOOP('',(#72362,#72363,#72364,#72365));
#16191=EDGE_LOOP('',(#72366,#72367,#72368,#72369));
#16192=EDGE_LOOP('',(#72370,#72371,#72372,#72373,#72374));
#16193=EDGE_LOOP('',(#72375,#72376,#72377,#72378));
#16194=EDGE_LOOP('',(#72379,#72380,#72381,#72382));
#16195=EDGE_LOOP('',(#72383,#72384,#72385,#72386));
#16196=EDGE_LOOP('',(#72387,#72388,#72389,#72390));
#16197=EDGE_LOOP('',(#72391,#72392,#72393,#72394));
#16198=EDGE_LOOP('',(#72395,#72396,#72397,#72398));
#16199=EDGE_LOOP('',(#72399,#72400,#72401,#72402));
#16200=EDGE_LOOP('',(#72403,#72404,#72405,#72406));
#16201=EDGE_LOOP('',(#72407,#72408,#72409,#72410));
#16202=EDGE_LOOP('',(#72411,#72412,#72413,#72414));
#16203=EDGE_LOOP('',(#72415,#72416,#72417,#72418,#72419));
#16204=EDGE_LOOP('',(#72420,#72421,#72422,#72423));
#16205=EDGE_LOOP('',(#72424,#72425,#72426,#72427));
#16206=EDGE_LOOP('',(#72428,#72429,#72430,#72431));
#16207=EDGE_LOOP('',(#72432,#72433,#72434,#72435));
#16208=EDGE_LOOP('',(#72436,#72437,#72438,#72439));
#16209=EDGE_LOOP('',(#72440,#72441,#72442,#72443));
#16210=EDGE_LOOP('',(#72444,#72445,#72446,#72447));
#16211=EDGE_LOOP('',(#72448,#72449,#72450,#72451));
#16212=EDGE_LOOP('',(#72452,#72453,#72454,#72455,#72456));
#16213=EDGE_LOOP('',(#72457,#72458,#72459,#72460));
#16214=EDGE_LOOP('',(#72461,#72462,#72463,#72464));
#16215=EDGE_LOOP('',(#72465,#72466,#72467,#72468,#72469));
#16216=EDGE_LOOP('',(#72470,#72471,#72472,#72473));
#16217=EDGE_LOOP('',(#72474,#72475,#72476,#72477));
#16218=EDGE_LOOP('',(#72478,#72479,#72480,#72481));
#16219=EDGE_LOOP('',(#72482,#72483,#72484,#72485));
#16220=EDGE_LOOP('',(#72486,#72487,#72488,#72489,#72490));
#16221=EDGE_LOOP('',(#72491,#72492,#72493,#72494));
#16222=EDGE_LOOP('',(#72495,#72496,#72497,#72498));
#16223=EDGE_LOOP('',(#72499,#72500,#72501,#72502));
#16224=EDGE_LOOP('',(#72503,#72504,#72505,#72506));
#16225=EDGE_LOOP('',(#72507,#72508,#72509,#72510));
#16226=EDGE_LOOP('',(#72511,#72512,#72513,#72514));
#16227=EDGE_LOOP('',(#72515,#72516,#72517,#72518));
#16228=EDGE_LOOP('',(#72519,#72520,#72521,#72522));
#16229=EDGE_LOOP('',(#72523,#72524,#72525,#72526));
#16230=EDGE_LOOP('',(#72527,#72528,#72529,#72530));
#16231=EDGE_LOOP('',(#72531,#72532,#72533,#72534,#72535));
#16232=EDGE_LOOP('',(#72536,#72537,#72538,#72539));
#16233=EDGE_LOOP('',(#72540,#72541,#72542,#72543));
#16234=EDGE_LOOP('',(#72544,#72545,#72546,#72547));
#16235=EDGE_LOOP('',(#72548,#72549,#72550,#72551));
#16236=EDGE_LOOP('',(#72552,#72553,#72554,#72555));
#16237=EDGE_LOOP('',(#72556,#72557,#72558,#72559));
#16238=EDGE_LOOP('',(#72560,#72561,#72562,#72563));
#16239=EDGE_LOOP('',(#72564,#72565,#72566,#72567));
#16240=EDGE_LOOP('',(#72568,#72569,#72570,#72571,#72572));
#16241=EDGE_LOOP('',(#72573,#72574,#72575,#72576));
#16242=EDGE_LOOP('',(#72577,#72578,#72579,#72580));
#16243=EDGE_LOOP('',(#72581,#72582,#72583,#72584,#72585));
#16244=EDGE_LOOP('',(#72586,#72587,#72588,#72589));
#16245=EDGE_LOOP('',(#72590,#72591,#72592,#72593));
#16246=EDGE_LOOP('',(#72594,#72595,#72596,#72597));
#16247=EDGE_LOOP('',(#72598,#72599,#72600,#72601));
#16248=EDGE_LOOP('',(#72602,#72603,#72604,#72605,#72606));
#16249=EDGE_LOOP('',(#72607,#72608,#72609,#72610));
#16250=EDGE_LOOP('',(#72611,#72612,#72613,#72614));
#16251=EDGE_LOOP('',(#72615,#72616,#72617,#72618));
#16252=EDGE_LOOP('',(#72619,#72620,#72621,#72622));
#16253=EDGE_LOOP('',(#72623,#72624,#72625,#72626));
#16254=EDGE_LOOP('',(#72627,#72628,#72629,#72630));
#16255=EDGE_LOOP('',(#72631,#72632,#72633,#72634));
#16256=EDGE_LOOP('',(#72635,#72636,#72637,#72638));
#16257=EDGE_LOOP('',(#72639,#72640,#72641,#72642));
#16258=EDGE_LOOP('',(#72643,#72644,#72645,#72646));
#16259=EDGE_LOOP('',(#72647,#72648,#72649,#72650,#72651));
#16260=EDGE_LOOP('',(#72652,#72653,#72654,#72655));
#16261=EDGE_LOOP('',(#72656,#72657,#72658,#72659));
#16262=EDGE_LOOP('',(#72660,#72661,#72662,#72663));
#16263=EDGE_LOOP('',(#72664,#72665,#72666,#72667));
#16264=EDGE_LOOP('',(#72668,#72669,#72670,#72671));
#16265=EDGE_LOOP('',(#72672,#72673,#72674,#72675));
#16266=EDGE_LOOP('',(#72676,#72677,#72678,#72679));
#16267=EDGE_LOOP('',(#72680,#72681,#72682,#72683));
#16268=EDGE_LOOP('',(#72684,#72685,#72686,#72687,#72688));
#16269=EDGE_LOOP('',(#72689,#72690,#72691,#72692));
#16270=EDGE_LOOP('',(#72693,#72694,#72695,#72696));
#16271=EDGE_LOOP('',(#72697,#72698,#72699,#72700,#72701));
#16272=EDGE_LOOP('',(#72702,#72703,#72704,#72705));
#16273=EDGE_LOOP('',(#72706,#72707,#72708,#72709));
#16274=EDGE_LOOP('',(#72710,#72711,#72712,#72713));
#16275=EDGE_LOOP('',(#72714,#72715,#72716,#72717));
#16276=EDGE_LOOP('',(#72718,#72719,#72720,#72721,#72722));
#16277=EDGE_LOOP('',(#72723,#72724,#72725,#72726));
#16278=EDGE_LOOP('',(#72727,#72728,#72729,#72730));
#16279=EDGE_LOOP('',(#72731,#72732,#72733,#72734));
#16280=EDGE_LOOP('',(#72735,#72736,#72737,#72738));
#16281=EDGE_LOOP('',(#72739,#72740,#72741,#72742));
#16282=EDGE_LOOP('',(#72743,#72744,#72745,#72746));
#16283=EDGE_LOOP('',(#72747,#72748,#72749,#72750));
#16284=EDGE_LOOP('',(#72751,#72752,#72753,#72754));
#16285=EDGE_LOOP('',(#72755,#72756,#72757,#72758));
#16286=EDGE_LOOP('',(#72759,#72760,#72761,#72762));
#16287=EDGE_LOOP('',(#72763,#72764,#72765,#72766,#72767));
#16288=EDGE_LOOP('',(#72768,#72769,#72770,#72771));
#16289=EDGE_LOOP('',(#72772,#72773,#72774,#72775));
#16290=EDGE_LOOP('',(#72776,#72777,#72778,#72779));
#16291=EDGE_LOOP('',(#72780,#72781,#72782,#72783));
#16292=EDGE_LOOP('',(#72784,#72785,#72786,#72787));
#16293=EDGE_LOOP('',(#72788,#72789,#72790,#72791));
#16294=EDGE_LOOP('',(#72792,#72793,#72794,#72795));
#16295=EDGE_LOOP('',(#72796,#72797,#72798,#72799));
#16296=EDGE_LOOP('',(#72800,#72801,#72802,#72803,#72804));
#16297=EDGE_LOOP('',(#72805,#72806,#72807,#72808));
#16298=EDGE_LOOP('',(#72809,#72810,#72811,#72812));
#16299=EDGE_LOOP('',(#72813,#72814,#72815,#72816,#72817));
#16300=EDGE_LOOP('',(#72818,#72819,#72820,#72821));
#16301=EDGE_LOOP('',(#72822,#72823,#72824,#72825));
#16302=EDGE_LOOP('',(#72826,#72827,#72828,#72829));
#16303=EDGE_LOOP('',(#72830,#72831,#72832,#72833));
#16304=EDGE_LOOP('',(#72834,#72835,#72836,#72837,#72838));
#16305=EDGE_LOOP('',(#72839,#72840,#72841,#72842));
#16306=EDGE_LOOP('',(#72843,#72844,#72845,#72846));
#16307=EDGE_LOOP('',(#72847,#72848,#72849,#72850));
#16308=EDGE_LOOP('',(#72851,#72852,#72853,#72854));
#16309=EDGE_LOOP('',(#72855,#72856,#72857,#72858));
#16310=EDGE_LOOP('',(#72859,#72860,#72861,#72862));
#16311=EDGE_LOOP('',(#72863,#72864,#72865,#72866));
#16312=EDGE_LOOP('',(#72867,#72868,#72869,#72870));
#16313=EDGE_LOOP('',(#72871,#72872,#72873,#72874));
#16314=EDGE_LOOP('',(#72875,#72876,#72877,#72878));
#16315=EDGE_LOOP('',(#72879,#72880,#72881,#72882,#72883));
#16316=EDGE_LOOP('',(#72884,#72885,#72886,#72887));
#16317=EDGE_LOOP('',(#72888,#72889,#72890,#72891));
#16318=EDGE_LOOP('',(#72892,#72893,#72894,#72895));
#16319=EDGE_LOOP('',(#72896,#72897,#72898,#72899));
#16320=EDGE_LOOP('',(#72900,#72901,#72902,#72903));
#16321=EDGE_LOOP('',(#72904,#72905,#72906,#72907));
#16322=EDGE_LOOP('',(#72908,#72909,#72910,#72911));
#16323=EDGE_LOOP('',(#72912,#72913,#72914,#72915));
#16324=EDGE_LOOP('',(#72916,#72917,#72918,#72919,#72920));
#16325=EDGE_LOOP('',(#72921,#72922,#72923,#72924));
#16326=EDGE_LOOP('',(#72925,#72926,#72927,#72928));
#16327=EDGE_LOOP('',(#72929,#72930,#72931,#72932,#72933));
#16328=EDGE_LOOP('',(#72934,#72935,#72936,#72937));
#16329=EDGE_LOOP('',(#72938,#72939,#72940,#72941));
#16330=EDGE_LOOP('',(#72942,#72943,#72944,#72945));
#16331=EDGE_LOOP('',(#72946,#72947,#72948,#72949));
#16332=EDGE_LOOP('',(#72950,#72951,#72952,#72953,#72954));
#16333=EDGE_LOOP('',(#72955,#72956,#72957,#72958));
#16334=EDGE_LOOP('',(#72959,#72960,#72961,#72962));
#16335=EDGE_LOOP('',(#72963,#72964,#72965,#72966));
#16336=EDGE_LOOP('',(#72967,#72968,#72969,#72970));
#16337=EDGE_LOOP('',(#72971,#72972,#72973,#72974));
#16338=EDGE_LOOP('',(#72975,#72976,#72977,#72978));
#16339=EDGE_LOOP('',(#72979,#72980,#72981,#72982));
#16340=EDGE_LOOP('',(#72983,#72984,#72985,#72986));
#16341=EDGE_LOOP('',(#72987,#72988,#72989,#72990));
#16342=EDGE_LOOP('',(#72991,#72992,#72993,#72994));
#16343=EDGE_LOOP('',(#72995,#72996,#72997,#72998,#72999));
#16344=EDGE_LOOP('',(#73000,#73001,#73002,#73003));
#16345=EDGE_LOOP('',(#73004,#73005,#73006,#73007));
#16346=EDGE_LOOP('',(#73008,#73009,#73010,#73011));
#16347=EDGE_LOOP('',(#73012,#73013,#73014,#73015));
#16348=EDGE_LOOP('',(#73016,#73017,#73018,#73019));
#16349=EDGE_LOOP('',(#73020,#73021,#73022,#73023));
#16350=EDGE_LOOP('',(#73024,#73025,#73026,#73027));
#16351=EDGE_LOOP('',(#73028,#73029,#73030,#73031));
#16352=EDGE_LOOP('',(#73032,#73033,#73034,#73035,#73036));
#16353=EDGE_LOOP('',(#73037,#73038,#73039,#73040));
#16354=EDGE_LOOP('',(#73041,#73042,#73043,#73044));
#16355=EDGE_LOOP('',(#73045,#73046,#73047,#73048,#73049));
#16356=EDGE_LOOP('',(#73050,#73051,#73052,#73053));
#16357=EDGE_LOOP('',(#73054,#73055,#73056,#73057));
#16358=EDGE_LOOP('',(#73058,#73059,#73060,#73061));
#16359=EDGE_LOOP('',(#73062,#73063,#73064,#73065));
#16360=EDGE_LOOP('',(#73066,#73067,#73068,#73069,#73070));
#16361=EDGE_LOOP('',(#73071,#73072,#73073,#73074));
#16362=EDGE_LOOP('',(#73075,#73076,#73077,#73078));
#16363=EDGE_LOOP('',(#73079,#73080,#73081,#73082));
#16364=EDGE_LOOP('',(#73083,#73084,#73085,#73086));
#16365=EDGE_LOOP('',(#73087,#73088,#73089,#73090));
#16366=EDGE_LOOP('',(#73091,#73092,#73093,#73094));
#16367=EDGE_LOOP('',(#73095,#73096,#73097,#73098));
#16368=EDGE_LOOP('',(#73099,#73100,#73101,#73102));
#16369=EDGE_LOOP('',(#73103,#73104,#73105,#73106));
#16370=EDGE_LOOP('',(#73107,#73108,#73109,#73110));
#16371=EDGE_LOOP('',(#73111,#73112,#73113,#73114,#73115));
#16372=EDGE_LOOP('',(#73116,#73117,#73118,#73119));
#16373=EDGE_LOOP('',(#73120,#73121,#73122,#73123));
#16374=EDGE_LOOP('',(#73124,#73125,#73126,#73127));
#16375=EDGE_LOOP('',(#73128,#73129,#73130,#73131));
#16376=EDGE_LOOP('',(#73132,#73133,#73134,#73135));
#16377=EDGE_LOOP('',(#73136,#73137,#73138,#73139));
#16378=EDGE_LOOP('',(#73140,#73141,#73142,#73143));
#16379=EDGE_LOOP('',(#73144,#73145,#73146,#73147));
#16380=EDGE_LOOP('',(#73148,#73149,#73150,#73151,#73152));
#16381=EDGE_LOOP('',(#73153,#73154,#73155,#73156));
#16382=EDGE_LOOP('',(#73157,#73158,#73159,#73160));
#16383=EDGE_LOOP('',(#73161,#73162,#73163,#73164,#73165));
#16384=EDGE_LOOP('',(#73166,#73167,#73168,#73169));
#16385=EDGE_LOOP('',(#73170,#73171,#73172,#73173));
#16386=EDGE_LOOP('',(#73174,#73175,#73176,#73177));
#16387=EDGE_LOOP('',(#73178,#73179,#73180,#73181));
#16388=EDGE_LOOP('',(#73182,#73183,#73184,#73185,#73186));
#16389=EDGE_LOOP('',(#73187,#73188,#73189,#73190));
#16390=EDGE_LOOP('',(#73191,#73192,#73193,#73194));
#16391=EDGE_LOOP('',(#73195,#73196,#73197,#73198));
#16392=EDGE_LOOP('',(#73199,#73200,#73201,#73202));
#16393=EDGE_LOOP('',(#73203,#73204,#73205,#73206));
#16394=EDGE_LOOP('',(#73207,#73208,#73209,#73210));
#16395=EDGE_LOOP('',(#73211,#73212,#73213,#73214));
#16396=EDGE_LOOP('',(#73215,#73216,#73217,#73218));
#16397=EDGE_LOOP('',(#73219,#73220,#73221,#73222));
#16398=EDGE_LOOP('',(#73223,#73224,#73225,#73226));
#16399=EDGE_LOOP('',(#73227,#73228,#73229,#73230,#73231));
#16400=EDGE_LOOP('',(#73232,#73233,#73234,#73235));
#16401=EDGE_LOOP('',(#73236,#73237,#73238,#73239));
#16402=EDGE_LOOP('',(#73240,#73241,#73242,#73243));
#16403=EDGE_LOOP('',(#73244,#73245,#73246,#73247));
#16404=EDGE_LOOP('',(#73248,#73249,#73250,#73251));
#16405=EDGE_LOOP('',(#73252,#73253,#73254,#73255));
#16406=EDGE_LOOP('',(#73256,#73257,#73258,#73259));
#16407=EDGE_LOOP('',(#73260,#73261,#73262,#73263));
#16408=EDGE_LOOP('',(#73264,#73265,#73266,#73267,#73268));
#16409=EDGE_LOOP('',(#73269,#73270,#73271,#73272));
#16410=EDGE_LOOP('',(#73273,#73274,#73275,#73276));
#16411=EDGE_LOOP('',(#73277,#73278,#73279,#73280,#73281));
#16412=EDGE_LOOP('',(#73282,#73283,#73284,#73285));
#16413=EDGE_LOOP('',(#73286,#73287,#73288,#73289));
#16414=EDGE_LOOP('',(#73290,#73291,#73292,#73293));
#16415=EDGE_LOOP('',(#73294,#73295,#73296,#73297));
#16416=EDGE_LOOP('',(#73298,#73299,#73300,#73301,#73302));
#16417=EDGE_LOOP('',(#73303,#73304,#73305,#73306));
#16418=EDGE_LOOP('',(#73307,#73308,#73309,#73310));
#16419=EDGE_LOOP('',(#73311,#73312,#73313,#73314));
#16420=EDGE_LOOP('',(#73315,#73316,#73317,#73318));
#16421=EDGE_LOOP('',(#73319,#73320,#73321,#73322));
#16422=EDGE_LOOP('',(#73323,#73324,#73325,#73326));
#16423=EDGE_LOOP('',(#73327,#73328,#73329,#73330));
#16424=EDGE_LOOP('',(#73331,#73332,#73333,#73334));
#16425=EDGE_LOOP('',(#73335,#73336,#73337,#73338));
#16426=EDGE_LOOP('',(#73339,#73340,#73341,#73342));
#16427=EDGE_LOOP('',(#73343,#73344,#73345,#73346,#73347));
#16428=EDGE_LOOP('',(#73348,#73349,#73350,#73351));
#16429=EDGE_LOOP('',(#73352,#73353,#73354,#73355));
#16430=EDGE_LOOP('',(#73356,#73357,#73358,#73359));
#16431=EDGE_LOOP('',(#73360,#73361,#73362,#73363));
#16432=EDGE_LOOP('',(#73364,#73365,#73366,#73367));
#16433=EDGE_LOOP('',(#73368,#73369,#73370,#73371));
#16434=EDGE_LOOP('',(#73372,#73373,#73374,#73375));
#16435=EDGE_LOOP('',(#73376,#73377,#73378,#73379));
#16436=EDGE_LOOP('',(#73380,#73381,#73382,#73383,#73384));
#16437=EDGE_LOOP('',(#73385,#73386,#73387,#73388));
#16438=EDGE_LOOP('',(#73389,#73390,#73391,#73392));
#16439=EDGE_LOOP('',(#73393,#73394,#73395,#73396,#73397));
#16440=EDGE_LOOP('',(#73398,#73399,#73400,#73401));
#16441=EDGE_LOOP('',(#73402,#73403,#73404,#73405));
#16442=EDGE_LOOP('',(#73406,#73407,#73408,#73409));
#16443=EDGE_LOOP('',(#73410,#73411,#73412,#73413));
#16444=EDGE_LOOP('',(#73414,#73415,#73416,#73417,#73418));
#16445=EDGE_LOOP('',(#73419,#73420,#73421,#73422));
#16446=EDGE_LOOP('',(#73423,#73424,#73425,#73426));
#16447=EDGE_LOOP('',(#73427,#73428,#73429,#73430));
#16448=EDGE_LOOP('',(#73431,#73432,#73433,#73434));
#16449=EDGE_LOOP('',(#73435,#73436,#73437,#73438));
#16450=EDGE_LOOP('',(#73439,#73440,#73441,#73442));
#16451=EDGE_LOOP('',(#73443,#73444,#73445,#73446));
#16452=EDGE_LOOP('',(#73447,#73448,#73449,#73450));
#16453=EDGE_LOOP('',(#73451,#73452,#73453,#73454));
#16454=EDGE_LOOP('',(#73455,#73456,#73457,#73458));
#16455=EDGE_LOOP('',(#73459,#73460,#73461,#73462,#73463));
#16456=EDGE_LOOP('',(#73464,#73465,#73466,#73467));
#16457=EDGE_LOOP('',(#73468,#73469,#73470,#73471));
#16458=EDGE_LOOP('',(#73472,#73473,#73474,#73475));
#16459=EDGE_LOOP('',(#73476,#73477,#73478,#73479));
#16460=EDGE_LOOP('',(#73480,#73481,#73482,#73483));
#16461=EDGE_LOOP('',(#73484,#73485,#73486,#73487));
#16462=EDGE_LOOP('',(#73488,#73489,#73490,#73491));
#16463=EDGE_LOOP('',(#73492,#73493,#73494,#73495));
#16464=EDGE_LOOP('',(#73496,#73497,#73498,#73499,#73500));
#16465=EDGE_LOOP('',(#73501,#73502,#73503,#73504));
#16466=EDGE_LOOP('',(#73505,#73506,#73507,#73508));
#16467=EDGE_LOOP('',(#73509,#73510,#73511,#73512));
#16468=EDGE_LOOP('',(#73513,#73514,#73515,#73516,#73517));
#16469=EDGE_LOOP('',(#73518,#73519,#73520,#73521,#73522));
#16470=EDGE_LOOP('',(#73523,#73524,#73525,#73526));
#16471=EDGE_LOOP('',(#73527,#73528,#73529,#73530,#73531));
#16472=EDGE_LOOP('',(#73532,#73533,#73534,#73535));
#16473=EDGE_LOOP('',(#73536,#73537,#73538,#73539));
#16474=EDGE_LOOP('',(#73540,#73541,#73542,#73543));
#16475=EDGE_LOOP('',(#73544,#73545,#73546,#73547,#73548,#73549,#73550,#73551,
#73552,#73553,#73554,#73555,#73556,#73557,#73558,#73559,#73560,#73561,#73562,
#73563,#73564,#73565,#73566,#73567,#73568,#73569,#73570,#73571,#73572,#73573,
#73574,#73575,#73576,#73577,#73578,#73579,#73580,#73581,#73582,#73583,#73584,
#73585,#73586,#73587,#73588,#73589,#73590,#73591,#73592,#73593,#73594,#73595,
#73596,#73597,#73598,#73599,#73600,#73601,#73602,#73603,#73604,#73605,#73606,
#73607,#73608,#73609,#73610,#73611,#73612,#73613,#73614,#73615,#73616,#73617,
#73618,#73619,#73620,#73621,#73622,#73623,#73624,#73625,#73626,#73627,#73628,
#73629,#73630,#73631,#73632,#73633,#73634,#73635,#73636,#73637,#73638,#73639,
#73640,#73641,#73642,#73643,#73644,#73645,#73646,#73647,#73648,#73649,#73650,
#73651,#73652,#73653,#73654,#73655,#73656,#73657,#73658,#73659,#73660,#73661,
#73662,#73663,#73664,#73665,#73666,#73667,#73668,#73669,#73670,#73671,#73672,
#73673,#73674,#73675,#73676,#73677,#73678,#73679,#73680,#73681,#73682,#73683,
#73684,#73685,#73686,#73687,#73688,#73689,#73690,#73691,#73692,#73693,#73694,
#73695,#73696,#73697,#73698,#73699,#73700,#73701,#73702,#73703,#73704,#73705,
#73706,#73707,#73708,#73709,#73710,#73711,#73712,#73713,#73714,#73715,#73716,
#73717,#73718,#73719,#73720,#73721,#73722,#73723,#73724,#73725,#73726,#73727,
#73728,#73729,#73730,#73731,#73732,#73733,#73734,#73735,#73736,#73737,#73738,
#73739,#73740,#73741,#73742,#73743,#73744,#73745,#73746,#73747,#73748,#73749,
#73750,#73751,#73752,#73753,#73754,#73755,#73756,#73757,#73758,#73759,#73760,
#73761,#73762,#73763,#73764,#73765,#73766,#73767,#73768,#73769,#73770,#73771,
#73772,#73773,#73774,#73775,#73776,#73777,#73778,#73779,#73780,#73781,#73782,
#73783,#73784,#73785,#73786,#73787,#73788,#73789,#73790,#73791,#73792,#73793,
#73794,#73795,#73796,#73797,#73798,#73799,#73800,#73801,#73802,#73803,#73804,
#73805,#73806,#73807,#73808,#73809,#73810,#73811,#73812,#73813,#73814,#73815,
#73816,#73817,#73818,#73819,#73820,#73821,#73822,#73823,#73824,#73825,#73826,
#73827,#73828,#73829,#73830,#73831,#73832,#73833,#73834,#73835,#73836,#73837,
#73838,#73839,#73840,#73841,#73842,#73843,#73844,#73845,#73846,#73847,#73848,
#73849,#73850,#73851,#73852,#73853,#73854,#73855,#73856,#73857,#73858,#73859,
#73860,#73861,#73862,#73863,#73864,#73865,#73866,#73867,#73868,#73869,#73870,
#73871,#73872,#73873,#73874,#73875,#73876,#73877,#73878,#73879,#73880,#73881,
#73882,#73883,#73884,#73885,#73886,#73887,#73888,#73889,#73890,#73891,#73892,
#73893,#73894,#73895,#73896,#73897,#73898,#73899,#73900,#73901,#73902,#73903,
#73904,#73905,#73906,#73907,#73908));
#16476=EDGE_LOOP('',(#73909,#73910,#73911,#73912,#73913,#73914,#73915,#73916,
#73917,#73918,#73919,#73920,#73921,#73922,#73923,#73924,#73925,#73926,#73927,
#73928,#73929,#73930,#73931,#73932,#73933,#73934,#73935,#73936,#73937,#73938,
#73939,#73940,#73941,#73942,#73943,#73944,#73945,#73946,#73947,#73948,#73949,
#73950,#73951,#73952,#73953,#73954,#73955,#73956,#73957,#73958,#73959,#73960,
#73961,#73962,#73963,#73964,#73965,#73966,#73967,#73968,#73969,#73970,#73971,
#73972,#73973,#73974,#73975,#73976,#73977,#73978,#73979,#73980,#73981,#73982,
#73983,#73984,#73985,#73986,#73987,#73988,#73989,#73990,#73991,#73992,#73993,
#73994,#73995,#73996,#73997,#73998,#73999,#74000,#74001,#74002,#74003,#74004,
#74005,#74006,#74007,#74008,#74009,#74010,#74011,#74012,#74013,#74014,#74015,
#74016,#74017,#74018,#74019,#74020,#74021,#74022,#74023,#74024,#74025,#74026,
#74027,#74028,#74029,#74030,#74031,#74032,#74033,#74034,#74035,#74036,#74037,
#74038,#74039,#74040,#74041,#74042,#74043,#74044,#74045,#74046,#74047,#74048,
#74049,#74050,#74051,#74052,#74053,#74054,#74055,#74056,#74057,#74058,#74059,
#74060,#74061,#74062,#74063,#74064,#74065,#74066,#74067,#74068,#74069,#74070,
#74071,#74072,#74073,#74074,#74075,#74076,#74077,#74078,#74079,#74080,#74081,
#74082,#74083,#74084,#74085,#74086,#74087,#74088,#74089,#74090,#74091,#74092,
#74093,#74094,#74095,#74096,#74097,#74098,#74099,#74100,#74101,#74102,#74103,
#74104,#74105,#74106,#74107,#74108,#74109,#74110,#74111,#74112,#74113,#74114,
#74115,#74116,#74117,#74118,#74119,#74120,#74121,#74122,#74123,#74124,#74125,
#74126,#74127,#74128,#74129,#74130,#74131,#74132,#74133,#74134,#74135,#74136,
#74137,#74138,#74139,#74140,#74141,#74142,#74143,#74144,#74145,#74146,#74147,
#74148,#74149,#74150,#74151,#74152,#74153,#74154,#74155,#74156,#74157,#74158,
#74159,#74160,#74161,#74162,#74163,#74164,#74165,#74166,#74167,#74168,#74169,
#74170,#74171,#74172,#74173,#74174,#74175,#74176,#74177,#74178,#74179,#74180,
#74181,#74182,#74183,#74184,#74185,#74186,#74187,#74188,#74189,#74190,#74191,
#74192,#74193,#74194,#74195,#74196,#74197,#74198,#74199,#74200,#74201,#74202,
#74203,#74204,#74205,#74206,#74207,#74208,#74209,#74210,#74211,#74212,#74213,
#74214,#74215,#74216,#74217,#74218,#74219,#74220,#74221,#74222,#74223,#74224,
#74225,#74226,#74227,#74228,#74229,#74230,#74231,#74232,#74233,#74234,#74235,
#74236,#74237,#74238,#74239,#74240,#74241,#74242,#74243,#74244,#74245,#74246,
#74247,#74248,#74249,#74250,#74251,#74252,#74253,#74254,#74255,#74256,#74257,
#74258,#74259,#74260,#74261,#74262,#74263,#74264,#74265,#74266,#74267,#74268,
#74269,#74270,#74271,#74272));
#16477=EDGE_LOOP('',(#74273,#74274,#74275,#74276,#74277,#74278));
#16478=EDGE_LOOP('',(#74279,#74280,#74281,#74282,#74283));
#16479=EDGE_LOOP('',(#74284,#74285,#74286,#74287,#74288,#74289));
#16480=EDGE_LOOP('',(#74290,#74291,#74292,#74293));
#16481=EDGE_LOOP('',(#74294,#74295,#74296,#74297));
#16482=EDGE_LOOP('',(#74298,#74299,#74300,#74301,#74302,#74303));
#16483=EDGE_LOOP('',(#74304,#74305,#74306,#74307));
#16484=EDGE_LOOP('',(#74308,#74309,#74310,#74311));
#16485=EDGE_LOOP('',(#74312,#74313,#74314,#74315));
#16486=EDGE_LOOP('',(#74316,#74317,#74318,#74319));
#16487=EDGE_LOOP('',(#74320,#74321,#74322,#74323));
#16488=EDGE_LOOP('',(#74324,#74325,#74326,#74327,#74328,#74329));
#16489=EDGE_LOOP('',(#74330,#74331,#74332,#74333));
#16490=EDGE_LOOP('',(#74334,#74335,#74336,#74337));
#16491=EDGE_LOOP('',(#74338,#74339,#74340,#74341,#74342,#74343));
#16492=EDGE_LOOP('',(#74344,#74345,#74346,#74347));
#16493=EDGE_LOOP('',(#74348,#74349,#74350,#74351));
#16494=EDGE_LOOP('',(#74352,#74353,#74354,#74355));
#16495=EDGE_LOOP('',(#74356,#74357,#74358,#74359));
#16496=EDGE_LOOP('',(#74360,#74361,#74362,#74363));
#16497=EDGE_LOOP('',(#74364,#74365,#74366,#74367,#74368,#74369));
#16498=EDGE_LOOP('',(#74370,#74371,#74372,#74373));
#16499=EDGE_LOOP('',(#74374,#74375,#74376,#74377));
#16500=EDGE_LOOP('',(#74378,#74379,#74380,#74381,#74382,#74383));
#16501=EDGE_LOOP('',(#74384,#74385,#74386,#74387));
#16502=EDGE_LOOP('',(#74388,#74389,#74390,#74391));
#16503=EDGE_LOOP('',(#74392,#74393,#74394,#74395));
#16504=EDGE_LOOP('',(#74396,#74397,#74398,#74399));
#16505=EDGE_LOOP('',(#74400,#74401,#74402,#74403));
#16506=EDGE_LOOP('',(#74404,#74405,#74406,#74407,#74408,#74409));
#16507=EDGE_LOOP('',(#74410,#74411,#74412,#74413));
#16508=EDGE_LOOP('',(#74414,#74415,#74416,#74417));
#16509=EDGE_LOOP('',(#74418,#74419,#74420,#74421,#74422,#74423));
#16510=EDGE_LOOP('',(#74424,#74425,#74426,#74427));
#16511=EDGE_LOOP('',(#74428,#74429,#74430,#74431));
#16512=EDGE_LOOP('',(#74432,#74433,#74434,#74435));
#16513=EDGE_LOOP('',(#74436,#74437,#74438,#74439));
#16514=EDGE_LOOP('',(#74440,#74441,#74442,#74443));
#16515=EDGE_LOOP('',(#74444,#74445,#74446,#74447,#74448,#74449));
#16516=EDGE_LOOP('',(#74450,#74451,#74452,#74453));
#16517=EDGE_LOOP('',(#74454,#74455,#74456,#74457));
#16518=EDGE_LOOP('',(#74458,#74459,#74460,#74461,#74462,#74463));
#16519=EDGE_LOOP('',(#74464,#74465,#74466,#74467));
#16520=EDGE_LOOP('',(#74468,#74469,#74470,#74471));
#16521=EDGE_LOOP('',(#74472,#74473,#74474,#74475));
#16522=EDGE_LOOP('',(#74476,#74477,#74478,#74479));
#16523=EDGE_LOOP('',(#74480,#74481,#74482,#74483));
#16524=EDGE_LOOP('',(#74484,#74485,#74486,#74487,#74488,#74489));
#16525=EDGE_LOOP('',(#74490,#74491,#74492,#74493));
#16526=EDGE_LOOP('',(#74494,#74495,#74496,#74497));
#16527=EDGE_LOOP('',(#74498,#74499,#74500,#74501,#74502,#74503));
#16528=EDGE_LOOP('',(#74504,#74505,#74506,#74507));
#16529=EDGE_LOOP('',(#74508,#74509,#74510,#74511));
#16530=EDGE_LOOP('',(#74512,#74513,#74514,#74515));
#16531=EDGE_LOOP('',(#74516,#74517,#74518,#74519));
#16532=EDGE_LOOP('',(#74520,#74521,#74522,#74523));
#16533=EDGE_LOOP('',(#74524,#74525,#74526,#74527,#74528,#74529));
#16534=EDGE_LOOP('',(#74530,#74531,#74532,#74533));
#16535=EDGE_LOOP('',(#74534,#74535,#74536,#74537));
#16536=EDGE_LOOP('',(#74538,#74539,#74540,#74541,#74542,#74543));
#16537=EDGE_LOOP('',(#74544,#74545,#74546,#74547));
#16538=EDGE_LOOP('',(#74548,#74549,#74550,#74551));
#16539=EDGE_LOOP('',(#74552,#74553,#74554,#74555));
#16540=EDGE_LOOP('',(#74556,#74557,#74558,#74559));
#16541=EDGE_LOOP('',(#74560,#74561,#74562,#74563));
#16542=EDGE_LOOP('',(#74564,#74565,#74566,#74567,#74568,#74569));
#16543=EDGE_LOOP('',(#74570,#74571,#74572,#74573));
#16544=EDGE_LOOP('',(#74574,#74575,#74576,#74577));
#16545=EDGE_LOOP('',(#74578,#74579,#74580,#74581,#74582,#74583));
#16546=EDGE_LOOP('',(#74584,#74585,#74586,#74587));
#16547=EDGE_LOOP('',(#74588,#74589,#74590,#74591));
#16548=EDGE_LOOP('',(#74592,#74593,#74594,#74595));
#16549=EDGE_LOOP('',(#74596,#74597,#74598,#74599));
#16550=EDGE_LOOP('',(#74600,#74601,#74602,#74603));
#16551=EDGE_LOOP('',(#74604,#74605,#74606,#74607,#74608,#74609));
#16552=EDGE_LOOP('',(#74610,#74611,#74612,#74613));
#16553=EDGE_LOOP('',(#74614,#74615,#74616,#74617));
#16554=EDGE_LOOP('',(#74618,#74619,#74620,#74621,#74622,#74623));
#16555=EDGE_LOOP('',(#74624,#74625,#74626,#74627));
#16556=EDGE_LOOP('',(#74628,#74629,#74630,#74631));
#16557=EDGE_LOOP('',(#74632,#74633,#74634,#74635));
#16558=EDGE_LOOP('',(#74636,#74637,#74638,#74639));
#16559=EDGE_LOOP('',(#74640,#74641,#74642,#74643));
#16560=EDGE_LOOP('',(#74644,#74645,#74646,#74647,#74648,#74649));
#16561=EDGE_LOOP('',(#74650,#74651,#74652,#74653));
#16562=EDGE_LOOP('',(#74654,#74655,#74656,#74657));
#16563=EDGE_LOOP('',(#74658,#74659,#74660,#74661,#74662,#74663));
#16564=EDGE_LOOP('',(#74664,#74665,#74666,#74667));
#16565=EDGE_LOOP('',(#74668,#74669,#74670,#74671));
#16566=EDGE_LOOP('',(#74672,#74673,#74674,#74675));
#16567=EDGE_LOOP('',(#74676,#74677,#74678,#74679));
#16568=EDGE_LOOP('',(#74680,#74681,#74682,#74683));
#16569=EDGE_LOOP('',(#74684,#74685,#74686,#74687,#74688,#74689));
#16570=EDGE_LOOP('',(#74690,#74691,#74692,#74693));
#16571=EDGE_LOOP('',(#74694,#74695,#74696,#74697));
#16572=EDGE_LOOP('',(#74698,#74699,#74700,#74701,#74702,#74703));
#16573=EDGE_LOOP('',(#74704,#74705,#74706,#74707));
#16574=EDGE_LOOP('',(#74708,#74709,#74710,#74711));
#16575=EDGE_LOOP('',(#74712,#74713,#74714,#74715));
#16576=EDGE_LOOP('',(#74716,#74717,#74718,#74719));
#16577=EDGE_LOOP('',(#74720,#74721,#74722,#74723));
#16578=EDGE_LOOP('',(#74724,#74725,#74726,#74727,#74728,#74729));
#16579=EDGE_LOOP('',(#74730,#74731,#74732,#74733));
#16580=EDGE_LOOP('',(#74734,#74735,#74736,#74737));
#16581=EDGE_LOOP('',(#74738,#74739,#74740,#74741,#74742,#74743));
#16582=EDGE_LOOP('',(#74744,#74745,#74746,#74747));
#16583=EDGE_LOOP('',(#74748,#74749,#74750,#74751));
#16584=EDGE_LOOP('',(#74752,#74753,#74754,#74755));
#16585=EDGE_LOOP('',(#74756,#74757,#74758,#74759));
#16586=EDGE_LOOP('',(#74760,#74761,#74762,#74763));
#16587=EDGE_LOOP('',(#74764,#74765,#74766,#74767,#74768,#74769));
#16588=EDGE_LOOP('',(#74770,#74771,#74772,#74773));
#16589=EDGE_LOOP('',(#74774,#74775,#74776,#74777));
#16590=EDGE_LOOP('',(#74778,#74779,#74780,#74781,#74782,#74783));
#16591=EDGE_LOOP('',(#74784,#74785,#74786,#74787));
#16592=EDGE_LOOP('',(#74788,#74789,#74790,#74791));
#16593=EDGE_LOOP('',(#74792,#74793,#74794,#74795));
#16594=EDGE_LOOP('',(#74796,#74797,#74798,#74799));
#16595=EDGE_LOOP('',(#74800,#74801,#74802,#74803));
#16596=EDGE_LOOP('',(#74804,#74805,#74806,#74807,#74808,#74809));
#16597=EDGE_LOOP('',(#74810,#74811,#74812,#74813));
#16598=EDGE_LOOP('',(#74814,#74815,#74816,#74817));
#16599=EDGE_LOOP('',(#74818,#74819,#74820,#74821,#74822,#74823));
#16600=EDGE_LOOP('',(#74824,#74825,#74826,#74827));
#16601=EDGE_LOOP('',(#74828,#74829,#74830,#74831));
#16602=EDGE_LOOP('',(#74832,#74833,#74834,#74835));
#16603=EDGE_LOOP('',(#74836,#74837,#74838,#74839));
#16604=EDGE_LOOP('',(#74840,#74841,#74842,#74843));
#16605=EDGE_LOOP('',(#74844,#74845,#74846,#74847,#74848,#74849));
#16606=EDGE_LOOP('',(#74850,#74851,#74852,#74853));
#16607=EDGE_LOOP('',(#74854,#74855,#74856,#74857));
#16608=EDGE_LOOP('',(#74858,#74859,#74860,#74861,#74862,#74863));
#16609=EDGE_LOOP('',(#74864,#74865,#74866,#74867));
#16610=EDGE_LOOP('',(#74868,#74869,#74870,#74871));
#16611=EDGE_LOOP('',(#74872,#74873,#74874,#74875));
#16612=EDGE_LOOP('',(#74876,#74877,#74878,#74879));
#16613=EDGE_LOOP('',(#74880,#74881,#74882,#74883));
#16614=EDGE_LOOP('',(#74884,#74885,#74886,#74887,#74888,#74889));
#16615=EDGE_LOOP('',(#74890,#74891,#74892,#74893));
#16616=EDGE_LOOP('',(#74894,#74895,#74896,#74897));
#16617=EDGE_LOOP('',(#74898,#74899,#74900,#74901,#74902,#74903));
#16618=EDGE_LOOP('',(#74904,#74905,#74906,#74907));
#16619=EDGE_LOOP('',(#74908,#74909,#74910,#74911));
#16620=EDGE_LOOP('',(#74912,#74913,#74914,#74915));
#16621=EDGE_LOOP('',(#74916,#74917,#74918,#74919));
#16622=EDGE_LOOP('',(#74920,#74921,#74922,#74923));
#16623=EDGE_LOOP('',(#74924,#74925,#74926,#74927,#74928,#74929));
#16624=EDGE_LOOP('',(#74930,#74931,#74932,#74933));
#16625=EDGE_LOOP('',(#74934,#74935,#74936,#74937));
#16626=EDGE_LOOP('',(#74938,#74939,#74940,#74941,#74942,#74943));
#16627=EDGE_LOOP('',(#74944,#74945,#74946,#74947));
#16628=EDGE_LOOP('',(#74948,#74949,#74950,#74951));
#16629=EDGE_LOOP('',(#74952,#74953,#74954,#74955));
#16630=EDGE_LOOP('',(#74956,#74957,#74958,#74959));
#16631=EDGE_LOOP('',(#74960,#74961,#74962,#74963));
#16632=EDGE_LOOP('',(#74964,#74965,#74966,#74967,#74968,#74969));
#16633=EDGE_LOOP('',(#74970,#74971,#74972,#74973));
#16634=EDGE_LOOP('',(#74974,#74975,#74976,#74977));
#16635=EDGE_LOOP('',(#74978,#74979,#74980,#74981,#74982,#74983));
#16636=EDGE_LOOP('',(#74984,#74985,#74986,#74987));
#16637=EDGE_LOOP('',(#74988,#74989,#74990,#74991));
#16638=EDGE_LOOP('',(#74992,#74993,#74994,#74995));
#16639=EDGE_LOOP('',(#74996,#74997,#74998,#74999));
#16640=EDGE_LOOP('',(#75000,#75001,#75002,#75003));
#16641=EDGE_LOOP('',(#75004,#75005,#75006,#75007,#75008,#75009));
#16642=EDGE_LOOP('',(#75010,#75011,#75012,#75013));
#16643=EDGE_LOOP('',(#75014,#75015,#75016,#75017));
#16644=EDGE_LOOP('',(#75018,#75019,#75020,#75021,#75022,#75023));
#16645=EDGE_LOOP('',(#75024,#75025,#75026,#75027));
#16646=EDGE_LOOP('',(#75028,#75029,#75030,#75031));
#16647=EDGE_LOOP('',(#75032,#75033,#75034,#75035));
#16648=EDGE_LOOP('',(#75036,#75037,#75038,#75039));
#16649=EDGE_LOOP('',(#75040,#75041,#75042,#75043));
#16650=EDGE_LOOP('',(#75044,#75045,#75046,#75047,#75048,#75049));
#16651=EDGE_LOOP('',(#75050,#75051,#75052,#75053));
#16652=EDGE_LOOP('',(#75054,#75055,#75056,#75057));
#16653=EDGE_LOOP('',(#75058,#75059,#75060,#75061,#75062,#75063));
#16654=EDGE_LOOP('',(#75064,#75065,#75066,#75067));
#16655=EDGE_LOOP('',(#75068,#75069,#75070,#75071));
#16656=EDGE_LOOP('',(#75072,#75073,#75074,#75075));
#16657=EDGE_LOOP('',(#75076,#75077,#75078,#75079));
#16658=EDGE_LOOP('',(#75080,#75081,#75082,#75083));
#16659=EDGE_LOOP('',(#75084,#75085,#75086,#75087,#75088,#75089));
#16660=EDGE_LOOP('',(#75090,#75091,#75092,#75093));
#16661=EDGE_LOOP('',(#75094,#75095,#75096,#75097));
#16662=EDGE_LOOP('',(#75098,#75099,#75100,#75101,#75102,#75103));
#16663=EDGE_LOOP('',(#75104,#75105,#75106,#75107));
#16664=EDGE_LOOP('',(#75108,#75109,#75110,#75111));
#16665=EDGE_LOOP('',(#75112,#75113,#75114,#75115));
#16666=EDGE_LOOP('',(#75116,#75117,#75118,#75119));
#16667=EDGE_LOOP('',(#75120,#75121,#75122,#75123));
#16668=EDGE_LOOP('',(#75124,#75125,#75126,#75127,#75128,#75129));
#16669=EDGE_LOOP('',(#75130,#75131,#75132,#75133));
#16670=EDGE_LOOP('',(#75134,#75135,#75136,#75137));
#16671=EDGE_LOOP('',(#75138,#75139,#75140,#75141,#75142,#75143));
#16672=EDGE_LOOP('',(#75144,#75145,#75146,#75147));
#16673=EDGE_LOOP('',(#75148,#75149,#75150,#75151));
#16674=EDGE_LOOP('',(#75152,#75153,#75154,#75155));
#16675=EDGE_LOOP('',(#75156,#75157,#75158,#75159));
#16676=EDGE_LOOP('',(#75160,#75161,#75162,#75163));
#16677=EDGE_LOOP('',(#75164,#75165,#75166,#75167,#75168,#75169));
#16678=EDGE_LOOP('',(#75170,#75171,#75172,#75173));
#16679=EDGE_LOOP('',(#75174,#75175,#75176,#75177));
#16680=EDGE_LOOP('',(#75178,#75179,#75180,#75181,#75182,#75183));
#16681=EDGE_LOOP('',(#75184,#75185,#75186,#75187));
#16682=EDGE_LOOP('',(#75188,#75189,#75190,#75191));
#16683=EDGE_LOOP('',(#75192,#75193,#75194,#75195));
#16684=EDGE_LOOP('',(#75196,#75197,#75198,#75199));
#16685=EDGE_LOOP('',(#75200,#75201,#75202,#75203));
#16686=EDGE_LOOP('',(#75204,#75205,#75206,#75207,#75208,#75209));
#16687=EDGE_LOOP('',(#75210,#75211,#75212,#75213));
#16688=EDGE_LOOP('',(#75214,#75215,#75216,#75217));
#16689=EDGE_LOOP('',(#75218,#75219,#75220,#75221,#75222,#75223));
#16690=EDGE_LOOP('',(#75224,#75225,#75226,#75227));
#16691=EDGE_LOOP('',(#75228,#75229,#75230,#75231));
#16692=EDGE_LOOP('',(#75232,#75233,#75234,#75235));
#16693=EDGE_LOOP('',(#75236,#75237,#75238,#75239));
#16694=EDGE_LOOP('',(#75240,#75241,#75242,#75243));
#16695=EDGE_LOOP('',(#75244,#75245,#75246,#75247,#75248,#75249));
#16696=EDGE_LOOP('',(#75250,#75251,#75252,#75253));
#16697=EDGE_LOOP('',(#75254,#75255,#75256,#75257));
#16698=EDGE_LOOP('',(#75258,#75259,#75260,#75261,#75262,#75263));
#16699=EDGE_LOOP('',(#75264,#75265,#75266,#75267));
#16700=EDGE_LOOP('',(#75268,#75269,#75270,#75271));
#16701=EDGE_LOOP('',(#75272,#75273,#75274,#75275));
#16702=EDGE_LOOP('',(#75276,#75277,#75278,#75279));
#16703=EDGE_LOOP('',(#75280,#75281,#75282,#75283));
#16704=EDGE_LOOP('',(#75284,#75285,#75286,#75287,#75288,#75289));
#16705=EDGE_LOOP('',(#75290,#75291,#75292,#75293));
#16706=EDGE_LOOP('',(#75294,#75295,#75296,#75297));
#16707=EDGE_LOOP('',(#75298,#75299,#75300,#75301,#75302,#75303));
#16708=EDGE_LOOP('',(#75304,#75305,#75306,#75307));
#16709=EDGE_LOOP('',(#75308,#75309,#75310,#75311));
#16710=EDGE_LOOP('',(#75312,#75313,#75314,#75315));
#16711=EDGE_LOOP('',(#75316,#75317,#75318,#75319));
#16712=EDGE_LOOP('',(#75320,#75321,#75322,#75323));
#16713=EDGE_LOOP('',(#75324,#75325,#75326,#75327,#75328,#75329));
#16714=EDGE_LOOP('',(#75330,#75331,#75332,#75333));
#16715=EDGE_LOOP('',(#75334,#75335,#75336,#75337));
#16716=EDGE_LOOP('',(#75338,#75339,#75340,#75341,#75342,#75343));
#16717=EDGE_LOOP('',(#75344,#75345,#75346,#75347));
#16718=EDGE_LOOP('',(#75348,#75349,#75350,#75351));
#16719=EDGE_LOOP('',(#75352,#75353,#75354,#75355));
#16720=EDGE_LOOP('',(#75356,#75357,#75358,#75359));
#16721=EDGE_LOOP('',(#75360,#75361,#75362,#75363));
#16722=EDGE_LOOP('',(#75364,#75365,#75366,#75367,#75368,#75369));
#16723=EDGE_LOOP('',(#75370,#75371,#75372,#75373));
#16724=EDGE_LOOP('',(#75374,#75375,#75376,#75377));
#16725=EDGE_LOOP('',(#75378,#75379,#75380,#75381,#75382,#75383));
#16726=EDGE_LOOP('',(#75384,#75385,#75386,#75387));
#16727=EDGE_LOOP('',(#75388,#75389,#75390,#75391));
#16728=EDGE_LOOP('',(#75392,#75393,#75394,#75395));
#16729=EDGE_LOOP('',(#75396,#75397,#75398,#75399));
#16730=EDGE_LOOP('',(#75400,#75401,#75402,#75403));
#16731=EDGE_LOOP('',(#75404,#75405,#75406,#75407,#75408,#75409));
#16732=EDGE_LOOP('',(#75410,#75411,#75412,#75413));
#16733=EDGE_LOOP('',(#75414,#75415,#75416,#75417));
#16734=EDGE_LOOP('',(#75418,#75419,#75420,#75421,#75422,#75423));
#16735=EDGE_LOOP('',(#75424,#75425,#75426,#75427));
#16736=EDGE_LOOP('',(#75428,#75429,#75430,#75431));
#16737=EDGE_LOOP('',(#75432,#75433,#75434,#75435));
#16738=EDGE_LOOP('',(#75436,#75437,#75438,#75439));
#16739=EDGE_LOOP('',(#75440,#75441,#75442,#75443));
#16740=EDGE_LOOP('',(#75444,#75445,#75446,#75447,#75448,#75449));
#16741=EDGE_LOOP('',(#75450,#75451,#75452,#75453));
#16742=EDGE_LOOP('',(#75454,#75455,#75456,#75457));
#16743=EDGE_LOOP('',(#75458,#75459,#75460,#75461,#75462,#75463));
#16744=EDGE_LOOP('',(#75464,#75465,#75466,#75467));
#16745=EDGE_LOOP('',(#75468,#75469,#75470,#75471));
#16746=EDGE_LOOP('',(#75472,#75473,#75474,#75475));
#16747=EDGE_LOOP('',(#75476,#75477,#75478,#75479));
#16748=EDGE_LOOP('',(#75480,#75481,#75482,#75483));
#16749=EDGE_LOOP('',(#75484,#75485,#75486,#75487,#75488,#75489));
#16750=EDGE_LOOP('',(#75490,#75491,#75492,#75493));
#16751=EDGE_LOOP('',(#75494,#75495,#75496,#75497));
#16752=EDGE_LOOP('',(#75498,#75499,#75500,#75501,#75502,#75503));
#16753=EDGE_LOOP('',(#75504,#75505,#75506,#75507));
#16754=EDGE_LOOP('',(#75508,#75509,#75510,#75511));
#16755=EDGE_LOOP('',(#75512,#75513,#75514,#75515));
#16756=EDGE_LOOP('',(#75516,#75517,#75518,#75519));
#16757=EDGE_LOOP('',(#75520,#75521,#75522,#75523));
#16758=EDGE_LOOP('',(#75524,#75525,#75526,#75527,#75528,#75529));
#16759=EDGE_LOOP('',(#75530,#75531,#75532,#75533));
#16760=EDGE_LOOP('',(#75534,#75535,#75536,#75537));
#16761=EDGE_LOOP('',(#75538,#75539,#75540,#75541,#75542,#75543));
#16762=EDGE_LOOP('',(#75544,#75545,#75546,#75547));
#16763=EDGE_LOOP('',(#75548,#75549,#75550,#75551));
#16764=EDGE_LOOP('',(#75552,#75553,#75554,#75555));
#16765=EDGE_LOOP('',(#75556,#75557,#75558,#75559));
#16766=EDGE_LOOP('',(#75560,#75561,#75562,#75563));
#16767=EDGE_LOOP('',(#75564,#75565,#75566,#75567,#75568,#75569));
#16768=EDGE_LOOP('',(#75570,#75571,#75572,#75573));
#16769=EDGE_LOOP('',(#75574,#75575,#75576,#75577));
#16770=EDGE_LOOP('',(#75578,#75579,#75580,#75581,#75582,#75583));
#16771=EDGE_LOOP('',(#75584,#75585,#75586,#75587));
#16772=EDGE_LOOP('',(#75588,#75589,#75590,#75591));
#16773=EDGE_LOOP('',(#75592,#75593,#75594,#75595));
#16774=EDGE_LOOP('',(#75596,#75597,#75598,#75599));
#16775=EDGE_LOOP('',(#75600,#75601,#75602,#75603));
#16776=EDGE_LOOP('',(#75604,#75605,#75606,#75607,#75608,#75609));
#16777=EDGE_LOOP('',(#75610,#75611,#75612,#75613));
#16778=EDGE_LOOP('',(#75614,#75615,#75616,#75617));
#16779=EDGE_LOOP('',(#75618,#75619,#75620,#75621,#75622,#75623));
#16780=EDGE_LOOP('',(#75624,#75625,#75626,#75627));
#16781=EDGE_LOOP('',(#75628,#75629,#75630,#75631));
#16782=EDGE_LOOP('',(#75632,#75633,#75634,#75635));
#16783=EDGE_LOOP('',(#75636,#75637,#75638,#75639));
#16784=EDGE_LOOP('',(#75640,#75641,#75642,#75643));
#16785=EDGE_LOOP('',(#75644,#75645,#75646,#75647,#75648,#75649));
#16786=EDGE_LOOP('',(#75650,#75651,#75652,#75653));
#16787=EDGE_LOOP('',(#75654,#75655,#75656,#75657));
#16788=EDGE_LOOP('',(#75658,#75659,#75660,#75661,#75662,#75663));
#16789=EDGE_LOOP('',(#75664,#75665,#75666,#75667));
#16790=EDGE_LOOP('',(#75668,#75669,#75670,#75671));
#16791=EDGE_LOOP('',(#75672,#75673,#75674,#75675));
#16792=EDGE_LOOP('',(#75676,#75677,#75678,#75679));
#16793=EDGE_LOOP('',(#75680,#75681,#75682,#75683));
#16794=EDGE_LOOP('',(#75684,#75685,#75686,#75687,#75688,#75689));
#16795=EDGE_LOOP('',(#75690,#75691,#75692,#75693));
#16796=EDGE_LOOP('',(#75694,#75695,#75696,#75697));
#16797=EDGE_LOOP('',(#75698,#75699,#75700,#75701,#75702,#75703));
#16798=EDGE_LOOP('',(#75704,#75705,#75706,#75707));
#16799=EDGE_LOOP('',(#75708,#75709,#75710,#75711));
#16800=EDGE_LOOP('',(#75712,#75713,#75714,#75715));
#16801=EDGE_LOOP('',(#75716,#75717,#75718,#75719));
#16802=EDGE_LOOP('',(#75720,#75721,#75722,#75723));
#16803=EDGE_LOOP('',(#75724,#75725,#75726,#75727,#75728,#75729));
#16804=EDGE_LOOP('',(#75730,#75731,#75732,#75733));
#16805=EDGE_LOOP('',(#75734,#75735,#75736,#75737));
#16806=EDGE_LOOP('',(#75738,#75739,#75740,#75741,#75742,#75743));
#16807=EDGE_LOOP('',(#75744,#75745,#75746,#75747));
#16808=EDGE_LOOP('',(#75748,#75749,#75750,#75751));
#16809=EDGE_LOOP('',(#75752,#75753,#75754,#75755));
#16810=EDGE_LOOP('',(#75756,#75757,#75758,#75759));
#16811=EDGE_LOOP('',(#75760,#75761,#75762,#75763));
#16812=EDGE_LOOP('',(#75764,#75765,#75766,#75767,#75768,#75769));
#16813=EDGE_LOOP('',(#75770,#75771,#75772,#75773));
#16814=EDGE_LOOP('',(#75774,#75775,#75776,#75777));
#16815=EDGE_LOOP('',(#75778,#75779,#75780,#75781,#75782,#75783));
#16816=EDGE_LOOP('',(#75784,#75785,#75786,#75787));
#16817=EDGE_LOOP('',(#75788,#75789,#75790,#75791));
#16818=EDGE_LOOP('',(#75792,#75793,#75794,#75795));
#16819=EDGE_LOOP('',(#75796,#75797,#75798,#75799));
#16820=EDGE_LOOP('',(#75800,#75801,#75802,#75803));
#16821=EDGE_LOOP('',(#75804,#75805,#75806,#75807,#75808,#75809));
#16822=EDGE_LOOP('',(#75810,#75811,#75812,#75813));
#16823=EDGE_LOOP('',(#75814,#75815,#75816,#75817));
#16824=EDGE_LOOP('',(#75818,#75819,#75820,#75821,#75822,#75823));
#16825=EDGE_LOOP('',(#75824,#75825,#75826,#75827));
#16826=EDGE_LOOP('',(#75828,#75829,#75830,#75831));
#16827=EDGE_LOOP('',(#75832,#75833,#75834,#75835));
#16828=EDGE_LOOP('',(#75836,#75837,#75838,#75839));
#16829=EDGE_LOOP('',(#75840,#75841,#75842,#75843));
#16830=EDGE_LOOP('',(#75844,#75845,#75846,#75847,#75848,#75849));
#16831=EDGE_LOOP('',(#75850,#75851,#75852,#75853));
#16832=EDGE_LOOP('',(#75854,#75855,#75856,#75857));
#16833=EDGE_LOOP('',(#75858,#75859,#75860,#75861,#75862,#75863));
#16834=EDGE_LOOP('',(#75864,#75865,#75866,#75867));
#16835=EDGE_LOOP('',(#75868,#75869,#75870,#75871));
#16836=EDGE_LOOP('',(#75872,#75873,#75874,#75875));
#16837=EDGE_LOOP('',(#75876,#75877,#75878,#75879));
#16838=EDGE_LOOP('',(#75880,#75881,#75882,#75883));
#16839=EDGE_LOOP('',(#75884,#75885,#75886,#75887,#75888,#75889));
#16840=EDGE_LOOP('',(#75890,#75891,#75892,#75893));
#16841=EDGE_LOOP('',(#75894,#75895,#75896,#75897));
#16842=EDGE_LOOP('',(#75898,#75899,#75900,#75901,#75902,#75903));
#16843=EDGE_LOOP('',(#75904,#75905,#75906,#75907));
#16844=EDGE_LOOP('',(#75908,#75909,#75910,#75911));
#16845=EDGE_LOOP('',(#75912,#75913,#75914,#75915));
#16846=EDGE_LOOP('',(#75916,#75917,#75918,#75919));
#16847=EDGE_LOOP('',(#75920,#75921,#75922,#75923));
#16848=EDGE_LOOP('',(#75924,#75925,#75926,#75927,#75928,#75929));
#16849=EDGE_LOOP('',(#75930,#75931,#75932,#75933));
#16850=EDGE_LOOP('',(#75934,#75935,#75936,#75937));
#16851=EDGE_LOOP('',(#75938,#75939,#75940,#75941,#75942,#75943));
#16852=EDGE_LOOP('',(#75944,#75945,#75946,#75947));
#16853=EDGE_LOOP('',(#75948,#75949,#75950,#75951));
#16854=EDGE_LOOP('',(#75952,#75953,#75954,#75955));
#16855=EDGE_LOOP('',(#75956,#75957,#75958,#75959));
#16856=EDGE_LOOP('',(#75960,#75961,#75962,#75963));
#16857=EDGE_LOOP('',(#75964,#75965,#75966,#75967,#75968,#75969));
#16858=EDGE_LOOP('',(#75970,#75971,#75972,#75973));
#16859=EDGE_LOOP('',(#75974,#75975,#75976,#75977));
#16860=EDGE_LOOP('',(#75978,#75979,#75980,#75981,#75982,#75983));
#16861=EDGE_LOOP('',(#75984,#75985,#75986,#75987));
#16862=EDGE_LOOP('',(#75988,#75989,#75990,#75991));
#16863=EDGE_LOOP('',(#75992,#75993,#75994,#75995));
#16864=EDGE_LOOP('',(#75996,#75997,#75998,#75999));
#16865=EDGE_LOOP('',(#76000,#76001,#76002,#76003));
#16866=EDGE_LOOP('',(#76004,#76005,#76006,#76007,#76008,#76009));
#16867=EDGE_LOOP('',(#76010,#76011,#76012,#76013));
#16868=EDGE_LOOP('',(#76014,#76015,#76016,#76017));
#16869=EDGE_LOOP('',(#76018,#76019,#76020,#76021,#76022,#76023));
#16870=EDGE_LOOP('',(#76024,#76025,#76026,#76027));
#16871=EDGE_LOOP('',(#76028,#76029,#76030,#76031));
#16872=EDGE_LOOP('',(#76032,#76033,#76034,#76035));
#16873=EDGE_LOOP('',(#76036,#76037,#76038,#76039));
#16874=EDGE_LOOP('',(#76040,#76041,#76042,#76043));
#16875=EDGE_LOOP('',(#76044,#76045,#76046,#76047,#76048,#76049));
#16876=EDGE_LOOP('',(#76050,#76051,#76052,#76053));
#16877=EDGE_LOOP('',(#76054,#76055,#76056,#76057));
#16878=EDGE_LOOP('',(#76058,#76059,#76060,#76061,#76062,#76063));
#16879=EDGE_LOOP('',(#76064,#76065,#76066,#76067));
#16880=EDGE_LOOP('',(#76068,#76069,#76070,#76071));
#16881=EDGE_LOOP('',(#76072,#76073,#76074,#76075));
#16882=EDGE_LOOP('',(#76076,#76077,#76078,#76079));
#16883=EDGE_LOOP('',(#76080,#76081,#76082,#76083));
#16884=EDGE_LOOP('',(#76084,#76085,#76086,#76087,#76088,#76089));
#16885=EDGE_LOOP('',(#76090,#76091,#76092,#76093));
#16886=EDGE_LOOP('',(#76094,#76095,#76096,#76097));
#16887=EDGE_LOOP('',(#76098,#76099,#76100,#76101,#76102,#76103));
#16888=EDGE_LOOP('',(#76104,#76105,#76106,#76107));
#16889=EDGE_LOOP('',(#76108,#76109,#76110,#76111));
#16890=EDGE_LOOP('',(#76112,#76113,#76114,#76115));
#16891=EDGE_LOOP('',(#76116,#76117,#76118,#76119));
#16892=EDGE_LOOP('',(#76120,#76121,#76122,#76123));
#16893=EDGE_LOOP('',(#76124,#76125,#76126,#76127,#76128,#76129));
#16894=EDGE_LOOP('',(#76130,#76131,#76132,#76133));
#16895=EDGE_LOOP('',(#76134,#76135,#76136,#76137));
#16896=EDGE_LOOP('',(#76138,#76139,#76140,#76141,#76142,#76143));
#16897=EDGE_LOOP('',(#76144,#76145,#76146,#76147));
#16898=EDGE_LOOP('',(#76148,#76149,#76150,#76151));
#16899=EDGE_LOOP('',(#76152,#76153,#76154,#76155));
#16900=EDGE_LOOP('',(#76156,#76157,#76158,#76159));
#16901=EDGE_LOOP('',(#76160,#76161,#76162,#76163));
#16902=EDGE_LOOP('',(#76164,#76165,#76166,#76167,#76168,#76169));
#16903=EDGE_LOOP('',(#76170,#76171,#76172,#76173));
#16904=EDGE_LOOP('',(#76174,#76175,#76176,#76177));
#16905=EDGE_LOOP('',(#76178,#76179,#76180,#76181,#76182,#76183));
#16906=EDGE_LOOP('',(#76184,#76185,#76186,#76187));
#16907=EDGE_LOOP('',(#76188,#76189,#76190,#76191));
#16908=EDGE_LOOP('',(#76192,#76193,#76194,#76195));
#16909=EDGE_LOOP('',(#76196,#76197,#76198,#76199));
#16910=EDGE_LOOP('',(#76200,#76201,#76202,#76203));
#16911=EDGE_LOOP('',(#76204,#76205,#76206,#76207,#76208,#76209));
#16912=EDGE_LOOP('',(#76210,#76211,#76212,#76213));
#16913=EDGE_LOOP('',(#76214,#76215,#76216,#76217));
#16914=EDGE_LOOP('',(#76218,#76219,#76220,#76221,#76222,#76223));
#16915=EDGE_LOOP('',(#76224,#76225,#76226,#76227));
#16916=EDGE_LOOP('',(#76228,#76229,#76230,#76231));
#16917=EDGE_LOOP('',(#76232,#76233,#76234,#76235));
#16918=EDGE_LOOP('',(#76236,#76237,#76238,#76239));
#16919=EDGE_LOOP('',(#76240,#76241,#76242,#76243));
#16920=EDGE_LOOP('',(#76244,#76245,#76246,#76247,#76248,#76249));
#16921=EDGE_LOOP('',(#76250,#76251,#76252,#76253));
#16922=EDGE_LOOP('',(#76254,#76255,#76256,#76257));
#16923=EDGE_LOOP('',(#76258,#76259,#76260,#76261,#76262,#76263));
#16924=EDGE_LOOP('',(#76264,#76265,#76266,#76267));
#16925=EDGE_LOOP('',(#76268,#76269,#76270,#76271));
#16926=EDGE_LOOP('',(#76272,#76273,#76274,#76275));
#16927=EDGE_LOOP('',(#76276,#76277,#76278,#76279));
#16928=EDGE_LOOP('',(#76280,#76281,#76282,#76283));
#16929=EDGE_LOOP('',(#76284,#76285,#76286,#76287,#76288,#76289));
#16930=EDGE_LOOP('',(#76290,#76291,#76292,#76293));
#16931=EDGE_LOOP('',(#76294,#76295,#76296,#76297));
#16932=EDGE_LOOP('',(#76298,#76299,#76300,#76301,#76302,#76303));
#16933=EDGE_LOOP('',(#76304,#76305,#76306,#76307));
#16934=EDGE_LOOP('',(#76308,#76309,#76310,#76311));
#16935=EDGE_LOOP('',(#76312,#76313,#76314,#76315));
#16936=EDGE_LOOP('',(#76316,#76317,#76318,#76319));
#16937=EDGE_LOOP('',(#76320,#76321,#76322,#76323));
#16938=EDGE_LOOP('',(#76324,#76325,#76326,#76327,#76328,#76329));
#16939=EDGE_LOOP('',(#76330,#76331,#76332,#76333));
#16940=EDGE_LOOP('',(#76334,#76335,#76336,#76337));
#16941=EDGE_LOOP('',(#76338,#76339,#76340,#76341,#76342,#76343));
#16942=EDGE_LOOP('',(#76344,#76345,#76346,#76347));
#16943=EDGE_LOOP('',(#76348,#76349,#76350,#76351));
#16944=EDGE_LOOP('',(#76352,#76353,#76354,#76355));
#16945=EDGE_LOOP('',(#76356,#76357,#76358,#76359));
#16946=EDGE_LOOP('',(#76360,#76361,#76362,#76363));
#16947=EDGE_LOOP('',(#76364,#76365,#76366,#76367,#76368,#76369));
#16948=EDGE_LOOP('',(#76370,#76371,#76372,#76373));
#16949=EDGE_LOOP('',(#76374,#76375,#76376,#76377));
#16950=EDGE_LOOP('',(#76378,#76379,#76380,#76381,#76382,#76383));
#16951=EDGE_LOOP('',(#76384,#76385,#76386,#76387));
#16952=EDGE_LOOP('',(#76388,#76389,#76390,#76391));
#16953=EDGE_LOOP('',(#76392,#76393,#76394,#76395));
#16954=EDGE_LOOP('',(#76396,#76397,#76398,#76399));
#16955=EDGE_LOOP('',(#76400,#76401,#76402,#76403));
#16956=EDGE_LOOP('',(#76404,#76405,#76406,#76407,#76408,#76409));
#16957=EDGE_LOOP('',(#76410,#76411,#76412,#76413));
#16958=EDGE_LOOP('',(#76414,#76415,#76416,#76417));
#16959=EDGE_LOOP('',(#76418,#76419,#76420,#76421,#76422,#76423));
#16960=EDGE_LOOP('',(#76424,#76425,#76426,#76427));
#16961=EDGE_LOOP('',(#76428,#76429,#76430,#76431));
#16962=EDGE_LOOP('',(#76432,#76433,#76434,#76435));
#16963=EDGE_LOOP('',(#76436,#76437,#76438,#76439));
#16964=EDGE_LOOP('',(#76440,#76441,#76442,#76443));
#16965=EDGE_LOOP('',(#76444,#76445,#76446,#76447,#76448,#76449));
#16966=EDGE_LOOP('',(#76450,#76451,#76452,#76453));
#16967=EDGE_LOOP('',(#76454,#76455,#76456,#76457));
#16968=EDGE_LOOP('',(#76458,#76459,#76460,#76461,#76462,#76463));
#16969=EDGE_LOOP('',(#76464,#76465,#76466,#76467));
#16970=EDGE_LOOP('',(#76468,#76469,#76470,#76471));
#16971=EDGE_LOOP('',(#76472,#76473,#76474,#76475));
#16972=EDGE_LOOP('',(#76476,#76477,#76478,#76479));
#16973=EDGE_LOOP('',(#76480,#76481,#76482,#76483));
#16974=EDGE_LOOP('',(#76484,#76485,#76486,#76487,#76488,#76489));
#16975=EDGE_LOOP('',(#76490,#76491,#76492,#76493));
#16976=EDGE_LOOP('',(#76494,#76495,#76496,#76497));
#16977=EDGE_LOOP('',(#76498,#76499,#76500,#76501,#76502,#76503));
#16978=EDGE_LOOP('',(#76504,#76505,#76506,#76507));
#16979=EDGE_LOOP('',(#76508,#76509,#76510,#76511));
#16980=EDGE_LOOP('',(#76512,#76513,#76514,#76515));
#16981=EDGE_LOOP('',(#76516,#76517,#76518,#76519));
#16982=EDGE_LOOP('',(#76520,#76521,#76522,#76523));
#16983=EDGE_LOOP('',(#76524,#76525,#76526,#76527,#76528,#76529));
#16984=EDGE_LOOP('',(#76530,#76531,#76532,#76533));
#16985=EDGE_LOOP('',(#76534,#76535,#76536,#76537));
#16986=EDGE_LOOP('',(#76538,#76539,#76540,#76541,#76542,#76543));
#16987=EDGE_LOOP('',(#76544,#76545,#76546,#76547));
#16988=EDGE_LOOP('',(#76548,#76549,#76550,#76551));
#16989=EDGE_LOOP('',(#76552,#76553,#76554,#76555));
#16990=EDGE_LOOP('',(#76556,#76557,#76558,#76559));
#16991=EDGE_LOOP('',(#76560,#76561,#76562,#76563));
#16992=EDGE_LOOP('',(#76564,#76565,#76566,#76567,#76568,#76569));
#16993=EDGE_LOOP('',(#76570,#76571,#76572,#76573));
#16994=EDGE_LOOP('',(#76574,#76575,#76576,#76577));
#16995=EDGE_LOOP('',(#76578,#76579,#76580,#76581,#76582,#76583));
#16996=EDGE_LOOP('',(#76584,#76585,#76586,#76587));
#16997=EDGE_LOOP('',(#76588,#76589,#76590,#76591));
#16998=EDGE_LOOP('',(#76592,#76593,#76594,#76595));
#16999=EDGE_LOOP('',(#76596,#76597,#76598,#76599));
#17000=EDGE_LOOP('',(#76600,#76601,#76602,#76603));
#17001=EDGE_LOOP('',(#76604,#76605,#76606,#76607,#76608,#76609));
#17002=EDGE_LOOP('',(#76610,#76611,#76612,#76613));
#17003=EDGE_LOOP('',(#76614,#76615,#76616,#76617));
#17004=EDGE_LOOP('',(#76618,#76619,#76620,#76621,#76622,#76623));
#17005=EDGE_LOOP('',(#76624,#76625,#76626,#76627));
#17006=EDGE_LOOP('',(#76628,#76629,#76630,#76631));
#17007=EDGE_LOOP('',(#76632,#76633,#76634,#76635));
#17008=EDGE_LOOP('',(#76636,#76637,#76638,#76639));
#17009=EDGE_LOOP('',(#76640,#76641,#76642,#76643));
#17010=EDGE_LOOP('',(#76644));
#17011=EDGE_LOOP('',(#76645));
#17012=EDGE_LOOP('',(#76646,#76647,#76648,#76649,#76650,#76651));
#17013=EDGE_LOOP('',(#76652,#76653,#76654,#76655));
#17014=EDGE_LOOP('',(#76656,#76657,#76658,#76659));
#17015=EDGE_LOOP('',(#76660,#76661,#76662,#76663,#76664,#76665));
#17016=EDGE_LOOP('',(#76666,#76667,#76668,#76669));
#17017=EDGE_LOOP('',(#76670));
#17018=EDGE_LOOP('',(#76671));
#17019=EDGE_LOOP('',(#76672));
#17020=EDGE_LOOP('',(#76673));
#17021=EDGE_LOOP('',(#76674,#76675,#76676,#76677));
#17022=EDGE_LOOP('',(#76678,#76679,#76680,#76681));
#17023=EDGE_LOOP('',(#76682,#76683,#76684,#76685));
#17024=EDGE_LOOP('',(#76686,#76687,#76688,#76689));
#17025=EDGE_LOOP('',(#76690,#76691,#76692,#76693));
#17026=EDGE_LOOP('',(#76694,#76695,#76696,#76697,#76698,#76699,#76700,#76701,
#76702,#76703,#76704,#76705));
#17027=EDGE_LOOP('',(#76706,#76707,#76708,#76709,#76710,#76711,#76712,#76713,
#76714,#76715,#76716,#76717));
#17028=EDGE_LOOP('',(#76718,#76719,#76720,#76721));
#17029=EDGE_LOOP('',(#76722,#76723,#76724,#76725));
#17030=EDGE_LOOP('',(#76726,#76727,#76728,#76729));
#17031=EDGE_LOOP('',(#76730,#76731,#76732,#76733));
#17032=EDGE_LOOP('',(#76734,#76735,#76736,#76737,#76738));
#17033=EDGE_LOOP('',(#76739,#76740,#76741,#76742));
#17034=EDGE_LOOP('',(#76743,#76744,#76745,#76746));
#17035=EDGE_LOOP('',(#76747,#76748,#76749,#76750));
#17036=EDGE_LOOP('',(#76751,#76752,#76753,#76754));
#17037=EDGE_LOOP('',(#76755,#76756,#76757,#76758,#76759));
#17038=EDGE_LOOP('',(#76760,#76761,#76762,#76763));
#17039=EDGE_LOOP('',(#76764,#76765,#76766,#76767));
#17040=EDGE_LOOP('',(#76768,#76769,#76770,#76771));
#17041=EDGE_LOOP('',(#76772,#76773,#76774,#76775));
#17042=EDGE_LOOP('',(#76776,#76777,#76778,#76779));
#17043=EDGE_LOOP('',(#76780,#76781,#76782,#76783));
#17044=EDGE_LOOP('',(#76784,#76785,#76786,#76787));
#17045=EDGE_LOOP('',(#76788,#76789,#76790,#76791));
#17046=EDGE_LOOP('',(#76792,#76793,#76794,#76795));
#17047=EDGE_LOOP('',(#76796,#76797,#76798,#76799,#76800));
#17048=EDGE_LOOP('',(#76801,#76802,#76803,#76804,#76805));
#17049=EDGE_LOOP('',(#76806,#76807,#76808,#76809));
#17050=EDGE_LOOP('',(#76810,#76811,#76812,#76813));
#17051=EDGE_LOOP('',(#76814,#76815,#76816,#76817));
#17052=EDGE_LOOP('',(#76818,#76819,#76820,#76821));
#17053=EDGE_LOOP('',(#76822,#76823,#76824,#76825));
#17054=EDGE_LOOP('',(#76826,#76827,#76828,#76829));
#17055=EDGE_LOOP('',(#76830,#76831,#76832,#76833));
#17056=EDGE_LOOP('',(#76834,#76835,#76836,#76837));
#17057=EDGE_LOOP('',(#76838,#76839,#76840,#76841,#76842));
#17058=EDGE_LOOP('',(#76843,#76844,#76845,#76846));
#17059=EDGE_LOOP('',(#76847,#76848,#76849,#76850,#76851,#76852,#76853,#76854,
#76855,#76856,#76857,#76858));
#17060=EDGE_LOOP('',(#76859,#76860,#76861,#76862,#76863,#76864,#76865,#76866,
#76867,#76868,#76869,#76870));
#17061=EDGE_LOOP('',(#76871,#76872,#76873,#76874));
#17062=EDGE_LOOP('',(#76875,#76876,#76877,#76878,#76879,#76880,#76881,#76882,
#76883,#76884,#76885,#76886));
#17063=EDGE_LOOP('',(#76887,#76888,#76889,#76890,#76891,#76892,#76893,#76894,
#76895,#76896,#76897,#76898));
#17064=EDGE_LOOP('',(#76899,#76900,#76901,#76902));
#17065=EDGE_LOOP('',(#76903,#76904,#76905,#76906,#76907,#76908,#76909,#76910,
#76911,#76912,#76913,#76914));
#17066=EDGE_LOOP('',(#76915,#76916,#76917,#76918,#76919,#76920,#76921,#76922,
#76923,#76924,#76925,#76926));
#17067=EDGE_LOOP('',(#76927,#76928,#76929,#76930));
#17068=EDGE_LOOP('',(#76931,#76932,#76933,#76934,#76935,#76936,#76937,#76938,
#76939,#76940,#76941,#76942));
#17069=EDGE_LOOP('',(#76943,#76944,#76945,#76946,#76947,#76948,#76949,#76950,
#76951,#76952,#76953,#76954));
#17070=EDGE_LOOP('',(#76955,#76956,#76957,#76958));
#17071=EDGE_LOOP('',(#76959,#76960,#76961,#76962,#76963,#76964,#76965,#76966,
#76967,#76968,#76969,#76970));
#17072=EDGE_LOOP('',(#76971,#76972,#76973,#76974,#76975,#76976,#76977,#76978,
#76979,#76980,#76981,#76982));
#17073=EDGE_LOOP('',(#76983,#76984,#76985,#76986));
#17074=EDGE_LOOP('',(#76987,#76988,#76989,#76990,#76991,#76992,#76993,#76994,
#76995,#76996,#76997,#76998));
#17075=EDGE_LOOP('',(#76999,#77000,#77001,#77002,#77003,#77004,#77005,#77006,
#77007,#77008,#77009,#77010));
#17076=EDGE_LOOP('',(#77011,#77012,#77013,#77014));
#17077=EDGE_LOOP('',(#77015,#77016,#77017,#77018,#77019,#77020,#77021,#77022,
#77023,#77024,#77025,#77026));
#17078=EDGE_LOOP('',(#77027,#77028,#77029,#77030,#77031,#77032,#77033,#77034,
#77035,#77036,#77037,#77038));
#17079=EDGE_LOOP('',(#77039,#77040,#77041,#77042));
#17080=EDGE_LOOP('',(#77043,#77044,#77045,#77046,#77047,#77048,#77049,#77050,
#77051,#77052,#77053,#77054));
#17081=EDGE_LOOP('',(#77055,#77056,#77057,#77058,#77059,#77060,#77061,#77062,
#77063,#77064,#77065,#77066));
#17082=EDGE_LOOP('',(#77067,#77068,#77069,#77070));
#17083=EDGE_LOOP('',(#77071,#77072,#77073,#77074,#77075,#77076,#77077,#77078,
#77079,#77080,#77081,#77082));
#17084=EDGE_LOOP('',(#77083,#77084,#77085,#77086,#77087,#77088,#77089,#77090,
#77091,#77092,#77093,#77094));
#17085=EDGE_LOOP('',(#77095,#77096,#77097,#77098));
#17086=EDGE_LOOP('',(#77099,#77100,#77101,#77102,#77103,#77104,#77105,#77106,
#77107,#77108,#77109,#77110));
#17087=EDGE_LOOP('',(#77111,#77112,#77113,#77114,#77115,#77116,#77117,#77118,
#77119,#77120,#77121,#77122));
#17088=EDGE_LOOP('',(#77123,#77124,#77125,#77126));
#17089=EDGE_LOOP('',(#77127,#77128,#77129,#77130,#77131,#77132,#77133,#77134,
#77135,#77136,#77137,#77138));
#17090=EDGE_LOOP('',(#77139,#77140,#77141,#77142,#77143,#77144,#77145,#77146,
#77147,#77148,#77149,#77150));
#17091=EDGE_LOOP('',(#77151,#77152,#77153,#77154));
#17092=EDGE_LOOP('',(#77155,#77156,#77157,#77158,#77159,#77160,#77161,#77162,
#77163,#77164,#77165,#77166));
#17093=EDGE_LOOP('',(#77167,#77168,#77169,#77170,#77171,#77172,#77173,#77174,
#77175,#77176,#77177,#77178));
#17094=EDGE_LOOP('',(#77179,#77180,#77181,#77182));
#17095=EDGE_LOOP('',(#77183,#77184,#77185,#77186,#77187,#77188,#77189,#77190,
#77191,#77192,#77193,#77194));
#17096=EDGE_LOOP('',(#77195,#77196,#77197,#77198,#77199,#77200,#77201,#77202,
#77203,#77204,#77205,#77206));
#17097=EDGE_LOOP('',(#77207,#77208,#77209,#77210));
#17098=EDGE_LOOP('',(#77211,#77212,#77213,#77214,#77215,#77216,#77217,#77218,
#77219,#77220,#77221,#77222));
#17099=EDGE_LOOP('',(#77223,#77224,#77225,#77226,#77227,#77228,#77229,#77230,
#77231,#77232,#77233,#77234));
#17100=EDGE_LOOP('',(#77235,#77236,#77237,#77238));
#17101=EDGE_LOOP('',(#77239,#77240,#77241,#77242,#77243,#77244,#77245,#77246,
#77247,#77248,#77249,#77250));
#17102=EDGE_LOOP('',(#77251,#77252,#77253,#77254,#77255,#77256,#77257,#77258,
#77259,#77260,#77261,#77262));
#17103=EDGE_LOOP('',(#77263,#77264,#77265,#77266));
#17104=EDGE_LOOP('',(#77267,#77268,#77269,#77270,#77271,#77272,#77273,#77274,
#77275,#77276,#77277,#77278));
#17105=EDGE_LOOP('',(#77279,#77280,#77281,#77282,#77283,#77284,#77285,#77286,
#77287,#77288,#77289,#77290));
#17106=EDGE_LOOP('',(#77291,#77292,#77293,#77294));
#17107=EDGE_LOOP('',(#77295,#77296,#77297,#77298,#77299,#77300,#77301,#77302,
#77303,#77304,#77305,#77306));
#17108=EDGE_LOOP('',(#77307,#77308,#77309,#77310,#77311,#77312,#77313,#77314,
#77315,#77316,#77317,#77318));
#17109=EDGE_LOOP('',(#77319,#77320,#77321,#77322));
#17110=EDGE_LOOP('',(#77323,#77324,#77325,#77326,#77327,#77328,#77329,#77330,
#77331,#77332,#77333,#77334));
#17111=EDGE_LOOP('',(#77335,#77336,#77337,#77338,#77339,#77340,#77341,#77342,
#77343,#77344,#77345,#77346));
#17112=EDGE_LOOP('',(#77347,#77348,#77349,#77350));
#17113=EDGE_LOOP('',(#77351,#77352,#77353,#77354,#77355,#77356,#77357,#77358,
#77359,#77360,#77361,#77362));
#17114=EDGE_LOOP('',(#77363,#77364,#77365,#77366,#77367,#77368,#77369,#77370,
#77371,#77372,#77373,#77374));
#17115=EDGE_LOOP('',(#77375,#77376,#77377,#77378));
#17116=EDGE_LOOP('',(#77379,#77380,#77381,#77382,#77383,#77384,#77385,#77386,
#77387,#77388,#77389,#77390));
#17117=EDGE_LOOP('',(#77391,#77392,#77393,#77394,#77395,#77396,#77397,#77398,
#77399,#77400,#77401,#77402));
#17118=EDGE_LOOP('',(#77403,#77404,#77405,#77406));
#17119=EDGE_LOOP('',(#77407,#77408,#77409,#77410,#77411,#77412,#77413,#77414,
#77415,#77416,#77417,#77418));
#17120=EDGE_LOOP('',(#77419,#77420,#77421,#77422,#77423,#77424,#77425,#77426,
#77427,#77428,#77429,#77430));
#17121=EDGE_LOOP('',(#77431,#77432,#77433,#77434));
#17122=EDGE_LOOP('',(#77435,#77436,#77437,#77438,#77439,#77440,#77441,#77442,
#77443,#77444,#77445,#77446));
#17123=EDGE_LOOP('',(#77447,#77448,#77449,#77450,#77451,#77452,#77453,#77454,
#77455,#77456,#77457,#77458));
#17124=EDGE_LOOP('',(#77459,#77460,#77461,#77462));
#17125=EDGE_LOOP('',(#77463,#77464,#77465,#77466,#77467,#77468,#77469,#77470,
#77471,#77472,#77473,#77474));
#17126=EDGE_LOOP('',(#77475,#77476,#77477,#77478,#77479,#77480,#77481,#77482,
#77483,#77484,#77485,#77486));
#17127=EDGE_LOOP('',(#77487,#77488,#77489,#77490));
#17128=EDGE_LOOP('',(#77491,#77492,#77493,#77494,#77495,#77496,#77497,#77498,
#77499,#77500,#77501,#77502));
#17129=EDGE_LOOP('',(#77503,#77504,#77505,#77506,#77507,#77508,#77509,#77510,
#77511,#77512,#77513,#77514));
#17130=EDGE_LOOP('',(#77515,#77516,#77517,#77518));
#17131=EDGE_LOOP('',(#77519,#77520,#77521,#77522,#77523,#77524,#77525,#77526,
#77527,#77528,#77529,#77530));
#17132=EDGE_LOOP('',(#77531,#77532,#77533,#77534,#77535,#77536,#77537,#77538,
#77539,#77540,#77541,#77542));
#17133=EDGE_LOOP('',(#77543,#77544,#77545,#77546));
#17134=EDGE_LOOP('',(#77547,#77548,#77549,#77550,#77551,#77552,#77553,#77554,
#77555,#77556,#77557,#77558));
#17135=EDGE_LOOP('',(#77559,#77560,#77561,#77562,#77563,#77564,#77565,#77566,
#77567,#77568,#77569,#77570));
#17136=EDGE_LOOP('',(#77571,#77572,#77573,#77574));
#17137=EDGE_LOOP('',(#77575,#77576,#77577,#77578,#77579,#77580,#77581,#77582,
#77583,#77584,#77585,#77586));
#17138=EDGE_LOOP('',(#77587,#77588,#77589,#77590,#77591,#77592,#77593,#77594,
#77595,#77596,#77597,#77598));
#17139=EDGE_LOOP('',(#77599,#77600,#77601,#77602));
#17140=EDGE_LOOP('',(#77603,#77604,#77605,#77606,#77607,#77608,#77609,#77610,
#77611,#77612,#77613,#77614));
#17141=EDGE_LOOP('',(#77615,#77616,#77617,#77618,#77619,#77620,#77621,#77622,
#77623,#77624,#77625,#77626));
#17142=EDGE_LOOP('',(#77627,#77628,#77629,#77630));
#17143=EDGE_LOOP('',(#77631,#77632,#77633,#77634,#77635,#77636,#77637,#77638,
#77639,#77640,#77641,#77642));
#17144=EDGE_LOOP('',(#77643,#77644,#77645,#77646,#77647,#77648,#77649,#77650,
#77651,#77652,#77653,#77654));
#17145=EDGE_LOOP('',(#77655,#77656,#77657,#77658));
#17146=EDGE_LOOP('',(#77659,#77660,#77661,#77662,#77663,#77664,#77665,#77666,
#77667,#77668,#77669,#77670));
#17147=EDGE_LOOP('',(#77671,#77672,#77673,#77674,#77675,#77676,#77677,#77678,
#77679,#77680,#77681,#77682));
#17148=EDGE_LOOP('',(#77683,#77684,#77685,#77686));
#17149=EDGE_LOOP('',(#77687,#77688,#77689,#77690,#77691,#77692,#77693,#77694,
#77695,#77696,#77697,#77698));
#17150=EDGE_LOOP('',(#77699,#77700,#77701,#77702,#77703,#77704,#77705,#77706,
#77707,#77708,#77709,#77710));
#17151=EDGE_LOOP('',(#77711,#77712,#77713,#77714));
#17152=EDGE_LOOP('',(#77715,#77716,#77717,#77718,#77719,#77720,#77721,#77722,
#77723,#77724,#77725,#77726));
#17153=EDGE_LOOP('',(#77727,#77728,#77729,#77730,#77731,#77732,#77733,#77734,
#77735,#77736,#77737,#77738));
#17154=EDGE_LOOP('',(#77739,#77740,#77741,#77742));
#17155=EDGE_LOOP('',(#77743,#77744,#77745,#77746,#77747,#77748,#77749,#77750,
#77751,#77752,#77753,#77754));
#17156=EDGE_LOOP('',(#77755,#77756,#77757,#77758,#77759,#77760,#77761,#77762,
#77763,#77764,#77765,#77766));
#17157=EDGE_LOOP('',(#77767,#77768,#77769,#77770));
#17158=EDGE_LOOP('',(#77771,#77772,#77773,#77774,#77775,#77776,#77777,#77778,
#77779,#77780,#77781,#77782));
#17159=EDGE_LOOP('',(#77783,#77784,#77785,#77786,#77787,#77788,#77789,#77790,
#77791,#77792,#77793,#77794));
#17160=EDGE_LOOP('',(#77795,#77796,#77797,#77798));
#17161=EDGE_LOOP('',(#77799,#77800,#77801,#77802,#77803,#77804,#77805,#77806,
#77807,#77808,#77809,#77810));
#17162=EDGE_LOOP('',(#77811,#77812,#77813,#77814,#77815,#77816,#77817,#77818,
#77819,#77820,#77821,#77822));
#17163=EDGE_LOOP('',(#77823,#77824,#77825,#77826));
#17164=EDGE_LOOP('',(#77827,#77828,#77829,#77830,#77831,#77832,#77833,#77834,
#77835,#77836,#77837,#77838));
#17165=EDGE_LOOP('',(#77839,#77840,#77841,#77842,#77843,#77844,#77845,#77846,
#77847,#77848,#77849,#77850));
#17166=EDGE_LOOP('',(#77851,#77852,#77853,#77854));
#17167=EDGE_LOOP('',(#77855,#77856,#77857,#77858,#77859,#77860,#77861,#77862,
#77863,#77864,#77865,#77866));
#17168=EDGE_LOOP('',(#77867,#77868,#77869,#77870,#77871,#77872,#77873,#77874,
#77875,#77876,#77877,#77878));
#17169=EDGE_LOOP('',(#77879,#77880,#77881,#77882));
#17170=EDGE_LOOP('',(#77883,#77884,#77885,#77886,#77887,#77888,#77889,#77890,
#77891,#77892,#77893,#77894));
#17171=EDGE_LOOP('',(#77895,#77896,#77897,#77898,#77899,#77900,#77901,#77902,
#77903,#77904,#77905,#77906));
#17172=EDGE_LOOP('',(#77907,#77908,#77909,#77910));
#17173=EDGE_LOOP('',(#77911,#77912,#77913,#77914,#77915,#77916,#77917,#77918,
#77919,#77920,#77921,#77922));
#17174=EDGE_LOOP('',(#77923,#77924,#77925,#77926,#77927,#77928,#77929,#77930,
#77931,#77932,#77933,#77934));
#17175=EDGE_LOOP('',(#77935,#77936,#77937,#77938));
#17176=EDGE_LOOP('',(#77939,#77940,#77941,#77942,#77943,#77944,#77945,#77946,
#77947,#77948,#77949,#77950));
#17177=EDGE_LOOP('',(#77951,#77952,#77953,#77954,#77955,#77956,#77957,#77958,
#77959,#77960,#77961,#77962));
#17178=EDGE_LOOP('',(#77963,#77964,#77965,#77966));
#17179=EDGE_LOOP('',(#77967,#77968,#77969,#77970,#77971,#77972,#77973,#77974,
#77975,#77976,#77977,#77978));
#17180=EDGE_LOOP('',(#77979,#77980,#77981,#77982,#77983,#77984,#77985,#77986,
#77987,#77988,#77989,#77990));
#17181=EDGE_LOOP('',(#77991,#77992,#77993,#77994));
#17182=EDGE_LOOP('',(#77995,#77996,#77997,#77998,#77999,#78000,#78001,#78002,
#78003,#78004,#78005,#78006));
#17183=EDGE_LOOP('',(#78007,#78008,#78009,#78010,#78011,#78012,#78013,#78014,
#78015,#78016,#78017,#78018));
#17184=EDGE_LOOP('',(#78019,#78020,#78021,#78022));
#17185=EDGE_LOOP('',(#78023,#78024,#78025,#78026,#78027,#78028,#78029,#78030,
#78031,#78032,#78033,#78034));
#17186=EDGE_LOOP('',(#78035,#78036,#78037,#78038,#78039,#78040,#78041,#78042,
#78043,#78044,#78045,#78046));
#17187=EDGE_LOOP('',(#78047,#78048,#78049,#78050));
#17188=EDGE_LOOP('',(#78051,#78052,#78053,#78054,#78055,#78056,#78057,#78058,
#78059,#78060,#78061,#78062));
#17189=EDGE_LOOP('',(#78063,#78064,#78065,#78066,#78067,#78068,#78069,#78070,
#78071,#78072,#78073,#78074));
#17190=EDGE_LOOP('',(#78075,#78076,#78077,#78078));
#17191=EDGE_LOOP('',(#78079,#78080,#78081,#78082,#78083,#78084,#78085,#78086,
#78087,#78088,#78089,#78090));
#17192=EDGE_LOOP('',(#78091,#78092,#78093,#78094,#78095,#78096,#78097,#78098,
#78099,#78100,#78101,#78102));
#17193=EDGE_LOOP('',(#78103,#78104,#78105,#78106));
#17194=EDGE_LOOP('',(#78107,#78108,#78109,#78110,#78111,#78112,#78113,#78114,
#78115,#78116,#78117,#78118));
#17195=EDGE_LOOP('',(#78119,#78120,#78121,#78122,#78123,#78124,#78125,#78126,
#78127,#78128,#78129,#78130));
#17196=EDGE_LOOP('',(#78131,#78132,#78133,#78134));
#17197=EDGE_LOOP('',(#78135,#78136,#78137,#78138,#78139,#78140,#78141,#78142,
#78143,#78144,#78145,#78146));
#17198=EDGE_LOOP('',(#78147,#78148,#78149,#78150,#78151,#78152,#78153,#78154,
#78155,#78156,#78157,#78158));
#17199=EDGE_LOOP('',(#78159,#78160,#78161,#78162));
#17200=EDGE_LOOP('',(#78163,#78164,#78165,#78166,#78167,#78168,#78169,#78170,
#78171,#78172,#78173,#78174));
#17201=EDGE_LOOP('',(#78175,#78176,#78177,#78178,#78179,#78180,#78181,#78182,
#78183,#78184,#78185,#78186));
#17202=EDGE_LOOP('',(#78187,#78188,#78189,#78190));
#17203=EDGE_LOOP('',(#78191,#78192,#78193,#78194,#78195,#78196,#78197,#78198,
#78199,#78200,#78201,#78202));
#17204=EDGE_LOOP('',(#78203,#78204,#78205,#78206,#78207,#78208,#78209,#78210,
#78211,#78212,#78213,#78214));
#17205=EDGE_LOOP('',(#78215,#78216,#78217,#78218));
#17206=EDGE_LOOP('',(#78219,#78220,#78221,#78222,#78223,#78224,#78225,#78226,
#78227,#78228,#78229,#78230));
#17207=EDGE_LOOP('',(#78231,#78232,#78233,#78234,#78235,#78236,#78237,#78238,
#78239,#78240,#78241,#78242));
#17208=EDGE_LOOP('',(#78243,#78244,#78245,#78246));
#17209=EDGE_LOOP('',(#78247,#78248,#78249,#78250,#78251,#78252,#78253,#78254,
#78255,#78256,#78257,#78258));
#17210=EDGE_LOOP('',(#78259,#78260,#78261,#78262,#78263,#78264,#78265,#78266,
#78267,#78268,#78269,#78270));
#17211=EDGE_LOOP('',(#78271,#78272,#78273,#78274));
#17212=EDGE_LOOP('',(#78275,#78276,#78277,#78278,#78279,#78280,#78281,#78282,
#78283,#78284,#78285,#78286));
#17213=EDGE_LOOP('',(#78287,#78288,#78289,#78290,#78291,#78292,#78293,#78294,
#78295,#78296,#78297,#78298));
#17214=EDGE_LOOP('',(#78299,#78300,#78301,#78302));
#17215=EDGE_LOOP('',(#78303,#78304,#78305,#78306,#78307,#78308,#78309,#78310,
#78311,#78312,#78313,#78314));
#17216=EDGE_LOOP('',(#78315,#78316,#78317,#78318,#78319,#78320,#78321,#78322,
#78323,#78324,#78325,#78326));
#17217=EDGE_LOOP('',(#78327,#78328,#78329,#78330));
#17218=EDGE_LOOP('',(#78331,#78332,#78333,#78334,#78335,#78336,#78337,#78338,
#78339,#78340,#78341,#78342));
#17219=EDGE_LOOP('',(#78343,#78344,#78345,#78346,#78347,#78348,#78349,#78350,
#78351,#78352,#78353,#78354));
#17220=EDGE_LOOP('',(#78355,#78356,#78357,#78358));
#17221=EDGE_LOOP('',(#78359,#78360,#78361,#78362,#78363,#78364,#78365,#78366,
#78367,#78368,#78369,#78370));
#17222=EDGE_LOOP('',(#78371,#78372,#78373,#78374,#78375,#78376,#78377,#78378,
#78379,#78380,#78381,#78382));
#17223=EDGE_LOOP('',(#78383,#78384,#78385,#78386));
#17224=EDGE_LOOP('',(#78387,#78388,#78389,#78390,#78391,#78392,#78393,#78394,
#78395,#78396,#78397,#78398));
#17225=EDGE_LOOP('',(#78399,#78400,#78401,#78402,#78403,#78404,#78405,#78406,
#78407,#78408,#78409,#78410));
#17226=EDGE_LOOP('',(#78411,#78412,#78413,#78414));
#17227=EDGE_LOOP('',(#78415,#78416,#78417,#78418,#78419,#78420,#78421,#78422,
#78423,#78424,#78425,#78426));
#17228=EDGE_LOOP('',(#78427,#78428,#78429,#78430,#78431,#78432,#78433,#78434,
#78435,#78436,#78437,#78438));
#17229=EDGE_LOOP('',(#78439,#78440,#78441,#78442));
#17230=EDGE_LOOP('',(#78443,#78444,#78445,#78446,#78447,#78448,#78449,#78450,
#78451,#78452,#78453,#78454));
#17231=EDGE_LOOP('',(#78455,#78456,#78457,#78458,#78459,#78460,#78461,#78462,
#78463,#78464,#78465,#78466));
#17232=EDGE_LOOP('',(#78467,#78468,#78469,#78470));
#17233=EDGE_LOOP('',(#78471,#78472,#78473,#78474,#78475,#78476,#78477,#78478,
#78479,#78480,#78481,#78482));
#17234=EDGE_LOOP('',(#78483,#78484,#78485,#78486,#78487,#78488,#78489,#78490,
#78491,#78492,#78493,#78494));
#17235=EDGE_LOOP('',(#78495,#78496,#78497,#78498));
#17236=EDGE_LOOP('',(#78499,#78500,#78501,#78502));
#17237=EDGE_LOOP('',(#78503,#78504,#78505,#78506));
#17238=EDGE_LOOP('',(#78507,#78508,#78509,#78510));
#17239=EDGE_LOOP('',(#78511,#78512,#78513,#78514));
#17240=EDGE_LOOP('',(#78515,#78516,#78517,#78518));
#17241=EDGE_LOOP('',(#78519,#78520,#78521,#78522));
#17242=EDGE_LOOP('',(#78523,#78524,#78525,#78526));
#17243=EDGE_LOOP('',(#78527,#78528,#78529,#78530));
#17244=EDGE_LOOP('',(#78531,#78532,#78533,#78534));
#17245=EDGE_LOOP('',(#78535,#78536,#78537,#78538));
#17246=EDGE_LOOP('',(#78539,#78540,#78541,#78542));
#17247=EDGE_LOOP('',(#78543,#78544,#78545,#78546));
#17248=EDGE_LOOP('',(#78547,#78548,#78549,#78550));
#17249=EDGE_LOOP('',(#78551,#78552,#78553,#78554));
#17250=EDGE_LOOP('',(#78555,#78556,#78557,#78558));
#17251=EDGE_LOOP('',(#78559,#78560,#78561,#78562));
#17252=EDGE_LOOP('',(#78563,#78564,#78565,#78566));
#17253=EDGE_LOOP('',(#78567,#78568,#78569,#78570));
#17254=EDGE_LOOP('',(#78571,#78572,#78573,#78574));
#17255=EDGE_LOOP('',(#78575,#78576,#78577,#78578));
#17256=EDGE_LOOP('',(#78579,#78580,#78581,#78582));
#17257=EDGE_LOOP('',(#78583,#78584,#78585,#78586));
#17258=EDGE_LOOP('',(#78587,#78588,#78589,#78590));
#17259=EDGE_LOOP('',(#78591,#78592,#78593,#78594));
#17260=EDGE_LOOP('',(#78595,#78596,#78597,#78598));
#17261=EDGE_LOOP('',(#78599,#78600,#78601,#78602));
#17262=EDGE_LOOP('',(#78603,#78604,#78605,#78606));
#17263=EDGE_LOOP('',(#78607,#78608,#78609,#78610));
#17264=EDGE_LOOP('',(#78611,#78612,#78613,#78614));
#17265=EDGE_LOOP('',(#78615,#78616,#78617,#78618));
#17266=EDGE_LOOP('',(#78619,#78620,#78621,#78622));
#17267=EDGE_LOOP('',(#78623,#78624,#78625,#78626));
#17268=EDGE_LOOP('',(#78627,#78628,#78629,#78630));
#17269=EDGE_LOOP('',(#78631,#78632,#78633,#78634));
#17270=EDGE_LOOP('',(#78635,#78636,#78637,#78638));
#17271=EDGE_LOOP('',(#78639,#78640,#78641,#78642));
#17272=EDGE_LOOP('',(#78643,#78644,#78645,#78646));
#17273=EDGE_LOOP('',(#78647,#78648,#78649,#78650));
#17274=EDGE_LOOP('',(#78651,#78652,#78653,#78654));
#17275=EDGE_LOOP('',(#78655,#78656,#78657,#78658));
#17276=EDGE_LOOP('',(#78659,#78660,#78661,#78662));
#17277=EDGE_LOOP('',(#78663,#78664,#78665,#78666));
#17278=EDGE_LOOP('',(#78667,#78668,#78669,#78670));
#17279=EDGE_LOOP('',(#78671,#78672,#78673,#78674));
#17280=EDGE_LOOP('',(#78675,#78676,#78677,#78678));
#17281=EDGE_LOOP('',(#78679,#78680,#78681,#78682));
#17282=EDGE_LOOP('',(#78683,#78684,#78685,#78686));
#17283=EDGE_LOOP('',(#78687,#78688,#78689,#78690));
#17284=EDGE_LOOP('',(#78691,#78692,#78693,#78694));
#17285=EDGE_LOOP('',(#78695,#78696,#78697,#78698));
#17286=EDGE_LOOP('',(#78699,#78700,#78701,#78702));
#17287=EDGE_LOOP('',(#78703,#78704,#78705,#78706));
#17288=EDGE_LOOP('',(#78707,#78708,#78709,#78710));
#17289=EDGE_LOOP('',(#78711,#78712,#78713,#78714));
#17290=EDGE_LOOP('',(#78715,#78716,#78717,#78718));
#17291=EDGE_LOOP('',(#78719,#78720,#78721,#78722));
#17292=EDGE_LOOP('',(#78723,#78724,#78725,#78726));
#17293=EDGE_LOOP('',(#78727,#78728,#78729,#78730));
#17294=EDGE_LOOP('',(#78731,#78732,#78733,#78734));
#17295=EDGE_LOOP('',(#78735,#78736,#78737,#78738));
#17296=EDGE_LOOP('',(#78739,#78740,#78741,#78742));
#17297=EDGE_LOOP('',(#78743,#78744,#78745,#78746));
#17298=EDGE_LOOP('',(#78747,#78748,#78749,#78750));
#17299=EDGE_LOOP('',(#78751,#78752,#78753,#78754));
#17300=EDGE_LOOP('',(#78755,#78756,#78757,#78758));
#17301=EDGE_LOOP('',(#78759,#78760,#78761,#78762));
#17302=EDGE_LOOP('',(#78763,#78764,#78765,#78766));
#17303=EDGE_LOOP('',(#78767,#78768,#78769,#78770));
#17304=EDGE_LOOP('',(#78771,#78772,#78773,#78774));
#17305=EDGE_LOOP('',(#78775,#78776,#78777,#78778));
#17306=EDGE_LOOP('',(#78779,#78780,#78781,#78782));
#17307=EDGE_LOOP('',(#78783,#78784,#78785,#78786));
#17308=EDGE_LOOP('',(#78787,#78788,#78789,#78790));
#17309=EDGE_LOOP('',(#78791,#78792,#78793,#78794));
#17310=EDGE_LOOP('',(#78795,#78796,#78797,#78798));
#17311=EDGE_LOOP('',(#78799,#78800,#78801,#78802));
#17312=EDGE_LOOP('',(#78803,#78804,#78805,#78806));
#17313=EDGE_LOOP('',(#78807,#78808,#78809,#78810));
#17314=EDGE_LOOP('',(#78811,#78812,#78813,#78814));
#17315=EDGE_LOOP('',(#78815,#78816,#78817,#78818));
#17316=EDGE_LOOP('',(#78819,#78820,#78821,#78822));
#17317=EDGE_LOOP('',(#78823,#78824,#78825,#78826));
#17318=EDGE_LOOP('',(#78827,#78828,#78829,#78830));
#17319=EDGE_LOOP('',(#78831,#78832,#78833,#78834));
#17320=EDGE_LOOP('',(#78835,#78836,#78837,#78838));
#17321=EDGE_LOOP('',(#78839,#78840,#78841,#78842));
#17322=EDGE_LOOP('',(#78843,#78844,#78845,#78846));
#17323=EDGE_LOOP('',(#78847,#78848,#78849,#78850));
#17324=EDGE_LOOP('',(#78851,#78852,#78853,#78854));
#17325=EDGE_LOOP('',(#78855,#78856,#78857,#78858));
#17326=EDGE_LOOP('',(#78859,#78860,#78861,#78862));
#17327=EDGE_LOOP('',(#78863,#78864,#78865,#78866));
#17328=EDGE_LOOP('',(#78867,#78868,#78869,#78870));
#17329=EDGE_LOOP('',(#78871,#78872,#78873,#78874));
#17330=EDGE_LOOP('',(#78875,#78876,#78877,#78878));
#17331=EDGE_LOOP('',(#78879,#78880,#78881,#78882));
#17332=EDGE_LOOP('',(#78883,#78884,#78885,#78886));
#17333=EDGE_LOOP('',(#78887,#78888,#78889,#78890));
#17334=EDGE_LOOP('',(#78891,#78892,#78893,#78894));
#17335=EDGE_LOOP('',(#78895,#78896,#78897,#78898));
#17336=EDGE_LOOP('',(#78899,#78900,#78901,#78902));
#17337=EDGE_LOOP('',(#78903,#78904,#78905,#78906));
#17338=EDGE_LOOP('',(#78907,#78908,#78909,#78910));
#17339=EDGE_LOOP('',(#78911,#78912,#78913,#78914));
#17340=EDGE_LOOP('',(#78915,#78916,#78917,#78918));
#17341=EDGE_LOOP('',(#78919,#78920,#78921,#78922));
#17342=EDGE_LOOP('',(#78923,#78924,#78925,#78926));
#17343=EDGE_LOOP('',(#78927,#78928,#78929,#78930));
#17344=EDGE_LOOP('',(#78931,#78932,#78933,#78934));
#17345=EDGE_LOOP('',(#78935,#78936,#78937,#78938));
#17346=EDGE_LOOP('',(#78939,#78940,#78941,#78942));
#17347=EDGE_LOOP('',(#78943,#78944,#78945,#78946));
#17348=EDGE_LOOP('',(#78947,#78948,#78949,#78950));
#17349=EDGE_LOOP('',(#78951,#78952,#78953,#78954));
#17350=EDGE_LOOP('',(#78955,#78956,#78957,#78958));
#17351=EDGE_LOOP('',(#78959,#78960,#78961,#78962));
#17352=EDGE_LOOP('',(#78963,#78964,#78965,#78966));
#17353=EDGE_LOOP('',(#78967,#78968,#78969,#78970));
#17354=EDGE_LOOP('',(#78971,#78972,#78973,#78974));
#17355=EDGE_LOOP('',(#78975,#78976,#78977,#78978,#78979));
#17356=EDGE_LOOP('',(#78980,#78981,#78982,#78983));
#17357=EDGE_LOOP('',(#78984,#78985,#78986,#78987));
#17358=EDGE_LOOP('',(#78988,#78989,#78990,#78991));
#17359=EDGE_LOOP('',(#78992,#78993,#78994,#78995));
#17360=EDGE_LOOP('',(#78996,#78997,#78998,#78999,#79000));
#17361=EDGE_LOOP('',(#79001,#79002,#79003,#79004));
#17362=EDGE_LOOP('',(#79005,#79006,#79007,#79008));
#17363=EDGE_LOOP('',(#79009,#79010,#79011,#79012));
#17364=EDGE_LOOP('',(#79013,#79014,#79015,#79016));
#17365=EDGE_LOOP('',(#79017,#79018,#79019,#79020));
#17366=EDGE_LOOP('',(#79021,#79022,#79023,#79024));
#17367=EDGE_LOOP('',(#79025,#79026,#79027,#79028));
#17368=EDGE_LOOP('',(#79029,#79030,#79031,#79032));
#17369=EDGE_LOOP('',(#79033,#79034,#79035,#79036));
#17370=EDGE_LOOP('',(#79037,#79038,#79039,#79040));
#17371=EDGE_LOOP('',(#79041,#79042,#79043,#79044,#79045));
#17372=EDGE_LOOP('',(#79046,#79047,#79048,#79049));
#17373=EDGE_LOOP('',(#79050,#79051,#79052,#79053));
#17374=EDGE_LOOP('',(#79054,#79055,#79056,#79057));
#17375=EDGE_LOOP('',(#79058,#79059,#79060,#79061));
#17376=EDGE_LOOP('',(#79062,#79063,#79064,#79065));
#17377=EDGE_LOOP('',(#79066,#79067,#79068,#79069));
#17378=EDGE_LOOP('',(#79070,#79071,#79072,#79073));
#17379=EDGE_LOOP('',(#79074,#79075,#79076,#79077));
#17380=EDGE_LOOP('',(#79078,#79079,#79080,#79081,#79082));
#17381=EDGE_LOOP('',(#79083,#79084,#79085,#79086));
#17382=EDGE_LOOP('',(#79087,#79088,#79089,#79090));
#17383=EDGE_LOOP('',(#79091,#79092,#79093,#79094,#79095));
#17384=EDGE_LOOP('',(#79096,#79097,#79098,#79099));
#17385=EDGE_LOOP('',(#79100,#79101,#79102,#79103));
#17386=EDGE_LOOP('',(#79104,#79105,#79106,#79107));
#17387=EDGE_LOOP('',(#79108,#79109,#79110,#79111));
#17388=EDGE_LOOP('',(#79112,#79113,#79114,#79115,#79116));
#17389=EDGE_LOOP('',(#79117,#79118,#79119,#79120));
#17390=EDGE_LOOP('',(#79121,#79122,#79123,#79124));
#17391=EDGE_LOOP('',(#79125,#79126,#79127,#79128));
#17392=EDGE_LOOP('',(#79129,#79130,#79131,#79132));
#17393=EDGE_LOOP('',(#79133,#79134,#79135,#79136));
#17394=EDGE_LOOP('',(#79137,#79138,#79139,#79140));
#17395=EDGE_LOOP('',(#79141,#79142,#79143,#79144));
#17396=EDGE_LOOP('',(#79145,#79146,#79147,#79148));
#17397=EDGE_LOOP('',(#79149,#79150,#79151,#79152));
#17398=EDGE_LOOP('',(#79153,#79154,#79155,#79156));
#17399=EDGE_LOOP('',(#79157,#79158,#79159,#79160,#79161));
#17400=EDGE_LOOP('',(#79162,#79163,#79164,#79165));
#17401=EDGE_LOOP('',(#79166,#79167,#79168,#79169));
#17402=EDGE_LOOP('',(#79170,#79171,#79172,#79173));
#17403=EDGE_LOOP('',(#79174,#79175,#79176,#79177));
#17404=EDGE_LOOP('',(#79178,#79179,#79180,#79181));
#17405=EDGE_LOOP('',(#79182,#79183,#79184,#79185));
#17406=EDGE_LOOP('',(#79186,#79187,#79188,#79189));
#17407=EDGE_LOOP('',(#79190,#79191,#79192,#79193));
#17408=EDGE_LOOP('',(#79194,#79195,#79196,#79197,#79198));
#17409=EDGE_LOOP('',(#79199,#79200,#79201,#79202));
#17410=EDGE_LOOP('',(#79203,#79204,#79205,#79206));
#17411=EDGE_LOOP('',(#79207,#79208,#79209,#79210,#79211));
#17412=EDGE_LOOP('',(#79212,#79213,#79214,#79215));
#17413=EDGE_LOOP('',(#79216,#79217,#79218,#79219));
#17414=EDGE_LOOP('',(#79220,#79221,#79222,#79223));
#17415=EDGE_LOOP('',(#79224,#79225,#79226,#79227));
#17416=EDGE_LOOP('',(#79228,#79229,#79230,#79231,#79232));
#17417=EDGE_LOOP('',(#79233,#79234,#79235,#79236));
#17418=EDGE_LOOP('',(#79237,#79238,#79239,#79240));
#17419=EDGE_LOOP('',(#79241,#79242,#79243,#79244));
#17420=EDGE_LOOP('',(#79245,#79246,#79247,#79248));
#17421=EDGE_LOOP('',(#79249,#79250,#79251,#79252));
#17422=EDGE_LOOP('',(#79253,#79254,#79255,#79256));
#17423=EDGE_LOOP('',(#79257,#79258,#79259,#79260));
#17424=EDGE_LOOP('',(#79261,#79262,#79263,#79264));
#17425=EDGE_LOOP('',(#79265,#79266,#79267,#79268));
#17426=EDGE_LOOP('',(#79269,#79270,#79271,#79272));
#17427=EDGE_LOOP('',(#79273,#79274,#79275,#79276,#79277));
#17428=EDGE_LOOP('',(#79278,#79279,#79280,#79281));
#17429=EDGE_LOOP('',(#79282,#79283,#79284,#79285));
#17430=EDGE_LOOP('',(#79286,#79287,#79288,#79289));
#17431=EDGE_LOOP('',(#79290,#79291,#79292,#79293));
#17432=EDGE_LOOP('',(#79294,#79295,#79296,#79297));
#17433=EDGE_LOOP('',(#79298,#79299,#79300,#79301));
#17434=EDGE_LOOP('',(#79302,#79303,#79304,#79305));
#17435=EDGE_LOOP('',(#79306,#79307,#79308,#79309));
#17436=EDGE_LOOP('',(#79310,#79311,#79312,#79313,#79314));
#17437=EDGE_LOOP('',(#79315,#79316,#79317,#79318));
#17438=EDGE_LOOP('',(#79319,#79320,#79321,#79322));
#17439=EDGE_LOOP('',(#79323,#79324,#79325,#79326,#79327));
#17440=EDGE_LOOP('',(#79328,#79329,#79330,#79331));
#17441=EDGE_LOOP('',(#79332,#79333,#79334,#79335));
#17442=EDGE_LOOP('',(#79336,#79337,#79338,#79339));
#17443=EDGE_LOOP('',(#79340,#79341,#79342,#79343));
#17444=EDGE_LOOP('',(#79344,#79345,#79346,#79347,#79348));
#17445=EDGE_LOOP('',(#79349,#79350,#79351,#79352));
#17446=EDGE_LOOP('',(#79353,#79354,#79355,#79356));
#17447=EDGE_LOOP('',(#79357,#79358,#79359,#79360));
#17448=EDGE_LOOP('',(#79361,#79362,#79363,#79364));
#17449=EDGE_LOOP('',(#79365,#79366,#79367,#79368));
#17450=EDGE_LOOP('',(#79369,#79370,#79371,#79372));
#17451=EDGE_LOOP('',(#79373,#79374,#79375,#79376));
#17452=EDGE_LOOP('',(#79377,#79378,#79379,#79380));
#17453=EDGE_LOOP('',(#79381,#79382,#79383,#79384));
#17454=EDGE_LOOP('',(#79385,#79386,#79387,#79388));
#17455=EDGE_LOOP('',(#79389,#79390,#79391,#79392,#79393));
#17456=EDGE_LOOP('',(#79394,#79395,#79396,#79397));
#17457=EDGE_LOOP('',(#79398,#79399,#79400,#79401));
#17458=EDGE_LOOP('',(#79402,#79403,#79404,#79405));
#17459=EDGE_LOOP('',(#79406,#79407,#79408,#79409));
#17460=EDGE_LOOP('',(#79410,#79411,#79412,#79413));
#17461=EDGE_LOOP('',(#79414,#79415,#79416,#79417));
#17462=EDGE_LOOP('',(#79418,#79419,#79420,#79421));
#17463=EDGE_LOOP('',(#79422,#79423,#79424,#79425));
#17464=EDGE_LOOP('',(#79426,#79427,#79428,#79429,#79430));
#17465=EDGE_LOOP('',(#79431,#79432,#79433,#79434));
#17466=EDGE_LOOP('',(#79435,#79436,#79437,#79438));
#17467=EDGE_LOOP('',(#79439,#79440,#79441,#79442,#79443));
#17468=EDGE_LOOP('',(#79444,#79445,#79446,#79447));
#17469=EDGE_LOOP('',(#79448,#79449,#79450,#79451));
#17470=EDGE_LOOP('',(#79452,#79453,#79454,#79455));
#17471=EDGE_LOOP('',(#79456,#79457,#79458,#79459));
#17472=EDGE_LOOP('',(#79460,#79461,#79462,#79463,#79464));
#17473=EDGE_LOOP('',(#79465,#79466,#79467,#79468));
#17474=EDGE_LOOP('',(#79469,#79470,#79471,#79472));
#17475=EDGE_LOOP('',(#79473,#79474,#79475,#79476));
#17476=EDGE_LOOP('',(#79477,#79478,#79479,#79480));
#17477=EDGE_LOOP('',(#79481,#79482,#79483,#79484));
#17478=EDGE_LOOP('',(#79485,#79486,#79487,#79488));
#17479=EDGE_LOOP('',(#79489,#79490,#79491,#79492));
#17480=EDGE_LOOP('',(#79493,#79494,#79495,#79496));
#17481=EDGE_LOOP('',(#79497,#79498,#79499,#79500));
#17482=EDGE_LOOP('',(#79501,#79502,#79503,#79504));
#17483=EDGE_LOOP('',(#79505,#79506,#79507,#79508,#79509));
#17484=EDGE_LOOP('',(#79510,#79511,#79512,#79513));
#17485=EDGE_LOOP('',(#79514,#79515,#79516,#79517));
#17486=EDGE_LOOP('',(#79518,#79519,#79520,#79521));
#17487=EDGE_LOOP('',(#79522,#79523,#79524,#79525));
#17488=EDGE_LOOP('',(#79526,#79527,#79528,#79529));
#17489=EDGE_LOOP('',(#79530,#79531,#79532,#79533));
#17490=EDGE_LOOP('',(#79534,#79535,#79536,#79537));
#17491=EDGE_LOOP('',(#79538,#79539,#79540,#79541));
#17492=EDGE_LOOP('',(#79542,#79543,#79544,#79545,#79546));
#17493=EDGE_LOOP('',(#79547,#79548,#79549,#79550));
#17494=EDGE_LOOP('',(#79551,#79552,#79553,#79554));
#17495=EDGE_LOOP('',(#79555,#79556,#79557,#79558,#79559));
#17496=EDGE_LOOP('',(#79560,#79561,#79562,#79563));
#17497=EDGE_LOOP('',(#79564,#79565,#79566,#79567));
#17498=EDGE_LOOP('',(#79568,#79569,#79570,#79571));
#17499=EDGE_LOOP('',(#79572,#79573,#79574,#79575));
#17500=EDGE_LOOP('',(#79576,#79577,#79578,#79579,#79580));
#17501=EDGE_LOOP('',(#79581,#79582,#79583,#79584));
#17502=EDGE_LOOP('',(#79585,#79586,#79587,#79588));
#17503=EDGE_LOOP('',(#79589,#79590,#79591,#79592));
#17504=EDGE_LOOP('',(#79593,#79594,#79595,#79596));
#17505=EDGE_LOOP('',(#79597,#79598,#79599,#79600));
#17506=EDGE_LOOP('',(#79601,#79602,#79603,#79604));
#17507=EDGE_LOOP('',(#79605,#79606,#79607,#79608));
#17508=EDGE_LOOP('',(#79609,#79610,#79611,#79612));
#17509=EDGE_LOOP('',(#79613,#79614,#79615,#79616));
#17510=EDGE_LOOP('',(#79617,#79618,#79619,#79620));
#17511=EDGE_LOOP('',(#79621,#79622,#79623,#79624,#79625));
#17512=EDGE_LOOP('',(#79626,#79627,#79628,#79629));
#17513=EDGE_LOOP('',(#79630,#79631,#79632,#79633));
#17514=EDGE_LOOP('',(#79634,#79635,#79636,#79637));
#17515=EDGE_LOOP('',(#79638,#79639,#79640,#79641));
#17516=EDGE_LOOP('',(#79642,#79643,#79644,#79645));
#17517=EDGE_LOOP('',(#79646,#79647,#79648,#79649));
#17518=EDGE_LOOP('',(#79650,#79651,#79652,#79653));
#17519=EDGE_LOOP('',(#79654,#79655,#79656,#79657));
#17520=EDGE_LOOP('',(#79658,#79659,#79660,#79661,#79662));
#17521=EDGE_LOOP('',(#79663,#79664,#79665,#79666));
#17522=EDGE_LOOP('',(#79667,#79668,#79669,#79670));
#17523=EDGE_LOOP('',(#79671,#79672,#79673,#79674,#79675));
#17524=EDGE_LOOP('',(#79676,#79677,#79678,#79679));
#17525=EDGE_LOOP('',(#79680,#79681,#79682,#79683));
#17526=EDGE_LOOP('',(#79684,#79685,#79686,#79687));
#17527=EDGE_LOOP('',(#79688,#79689,#79690,#79691));
#17528=EDGE_LOOP('',(#79692,#79693,#79694,#79695,#79696));
#17529=EDGE_LOOP('',(#79697,#79698,#79699,#79700));
#17530=EDGE_LOOP('',(#79701,#79702,#79703,#79704));
#17531=EDGE_LOOP('',(#79705,#79706,#79707,#79708));
#17532=EDGE_LOOP('',(#79709,#79710,#79711,#79712));
#17533=EDGE_LOOP('',(#79713,#79714,#79715,#79716));
#17534=EDGE_LOOP('',(#79717,#79718,#79719,#79720));
#17535=EDGE_LOOP('',(#79721,#79722,#79723,#79724));
#17536=EDGE_LOOP('',(#79725,#79726,#79727,#79728));
#17537=EDGE_LOOP('',(#79729,#79730,#79731,#79732));
#17538=EDGE_LOOP('',(#79733,#79734,#79735,#79736));
#17539=EDGE_LOOP('',(#79737,#79738,#79739,#79740,#79741));
#17540=EDGE_LOOP('',(#79742,#79743,#79744,#79745));
#17541=EDGE_LOOP('',(#79746,#79747,#79748,#79749));
#17542=EDGE_LOOP('',(#79750,#79751,#79752,#79753));
#17543=EDGE_LOOP('',(#79754,#79755,#79756,#79757));
#17544=EDGE_LOOP('',(#79758,#79759,#79760,#79761));
#17545=EDGE_LOOP('',(#79762,#79763,#79764,#79765));
#17546=EDGE_LOOP('',(#79766,#79767,#79768,#79769));
#17547=EDGE_LOOP('',(#79770,#79771,#79772,#79773));
#17548=EDGE_LOOP('',(#79774,#79775,#79776,#79777,#79778));
#17549=EDGE_LOOP('',(#79779,#79780,#79781,#79782));
#17550=EDGE_LOOP('',(#79783,#79784,#79785,#79786));
#17551=EDGE_LOOP('',(#79787,#79788,#79789,#79790,#79791));
#17552=EDGE_LOOP('',(#79792,#79793,#79794,#79795));
#17553=EDGE_LOOP('',(#79796,#79797,#79798,#79799));
#17554=EDGE_LOOP('',(#79800,#79801,#79802,#79803));
#17555=EDGE_LOOP('',(#79804,#79805,#79806,#79807));
#17556=EDGE_LOOP('',(#79808,#79809,#79810,#79811,#79812));
#17557=EDGE_LOOP('',(#79813,#79814,#79815,#79816));
#17558=EDGE_LOOP('',(#79817,#79818,#79819,#79820));
#17559=EDGE_LOOP('',(#79821,#79822,#79823,#79824));
#17560=EDGE_LOOP('',(#79825,#79826,#79827,#79828));
#17561=EDGE_LOOP('',(#79829,#79830,#79831,#79832));
#17562=EDGE_LOOP('',(#79833,#79834,#79835,#79836));
#17563=EDGE_LOOP('',(#79837,#79838,#79839,#79840));
#17564=EDGE_LOOP('',(#79841,#79842,#79843,#79844));
#17565=EDGE_LOOP('',(#79845,#79846,#79847,#79848));
#17566=EDGE_LOOP('',(#79849,#79850,#79851,#79852));
#17567=EDGE_LOOP('',(#79853,#79854,#79855,#79856,#79857));
#17568=EDGE_LOOP('',(#79858,#79859,#79860,#79861));
#17569=EDGE_LOOP('',(#79862,#79863,#79864,#79865));
#17570=EDGE_LOOP('',(#79866,#79867,#79868,#79869));
#17571=EDGE_LOOP('',(#79870,#79871,#79872,#79873));
#17572=EDGE_LOOP('',(#79874,#79875,#79876,#79877));
#17573=EDGE_LOOP('',(#79878,#79879,#79880,#79881));
#17574=EDGE_LOOP('',(#79882,#79883,#79884,#79885));
#17575=EDGE_LOOP('',(#79886,#79887,#79888,#79889));
#17576=EDGE_LOOP('',(#79890,#79891,#79892,#79893,#79894));
#17577=EDGE_LOOP('',(#79895,#79896,#79897,#79898));
#17578=EDGE_LOOP('',(#79899,#79900,#79901,#79902));
#17579=EDGE_LOOP('',(#79903,#79904,#79905,#79906,#79907));
#17580=EDGE_LOOP('',(#79908,#79909,#79910,#79911));
#17581=EDGE_LOOP('',(#79912,#79913,#79914,#79915));
#17582=EDGE_LOOP('',(#79916,#79917,#79918,#79919));
#17583=EDGE_LOOP('',(#79920,#79921,#79922,#79923));
#17584=EDGE_LOOP('',(#79924,#79925,#79926,#79927,#79928));
#17585=EDGE_LOOP('',(#79929,#79930,#79931,#79932));
#17586=EDGE_LOOP('',(#79933,#79934,#79935,#79936));
#17587=EDGE_LOOP('',(#79937,#79938,#79939,#79940));
#17588=EDGE_LOOP('',(#79941,#79942,#79943,#79944));
#17589=EDGE_LOOP('',(#79945,#79946,#79947,#79948));
#17590=EDGE_LOOP('',(#79949,#79950,#79951,#79952));
#17591=EDGE_LOOP('',(#79953,#79954,#79955,#79956));
#17592=EDGE_LOOP('',(#79957,#79958,#79959,#79960));
#17593=EDGE_LOOP('',(#79961,#79962,#79963,#79964));
#17594=EDGE_LOOP('',(#79965,#79966,#79967,#79968));
#17595=EDGE_LOOP('',(#79969,#79970,#79971,#79972,#79973));
#17596=EDGE_LOOP('',(#79974,#79975,#79976,#79977));
#17597=EDGE_LOOP('',(#79978,#79979,#79980,#79981));
#17598=EDGE_LOOP('',(#79982,#79983,#79984,#79985));
#17599=EDGE_LOOP('',(#79986,#79987,#79988,#79989));
#17600=EDGE_LOOP('',(#79990,#79991,#79992,#79993));
#17601=EDGE_LOOP('',(#79994,#79995,#79996,#79997));
#17602=EDGE_LOOP('',(#79998,#79999,#80000,#80001));
#17603=EDGE_LOOP('',(#80002,#80003,#80004,#80005));
#17604=EDGE_LOOP('',(#80006,#80007,#80008,#80009,#80010));
#17605=EDGE_LOOP('',(#80011,#80012,#80013,#80014));
#17606=EDGE_LOOP('',(#80015,#80016,#80017,#80018));
#17607=EDGE_LOOP('',(#80019,#80020,#80021,#80022,#80023));
#17608=EDGE_LOOP('',(#80024,#80025,#80026,#80027));
#17609=EDGE_LOOP('',(#80028,#80029,#80030,#80031));
#17610=EDGE_LOOP('',(#80032,#80033,#80034,#80035));
#17611=EDGE_LOOP('',(#80036,#80037,#80038,#80039));
#17612=EDGE_LOOP('',(#80040,#80041,#80042,#80043,#80044));
#17613=EDGE_LOOP('',(#80045,#80046,#80047,#80048));
#17614=EDGE_LOOP('',(#80049,#80050,#80051,#80052));
#17615=EDGE_LOOP('',(#80053,#80054,#80055,#80056));
#17616=EDGE_LOOP('',(#80057,#80058,#80059,#80060));
#17617=EDGE_LOOP('',(#80061,#80062,#80063,#80064));
#17618=EDGE_LOOP('',(#80065,#80066,#80067,#80068));
#17619=EDGE_LOOP('',(#80069,#80070,#80071,#80072));
#17620=EDGE_LOOP('',(#80073,#80074,#80075,#80076));
#17621=EDGE_LOOP('',(#80077,#80078,#80079,#80080));
#17622=EDGE_LOOP('',(#80081,#80082,#80083,#80084));
#17623=EDGE_LOOP('',(#80085,#80086,#80087,#80088,#80089));
#17624=EDGE_LOOP('',(#80090,#80091,#80092,#80093));
#17625=EDGE_LOOP('',(#80094,#80095,#80096,#80097));
#17626=EDGE_LOOP('',(#80098,#80099,#80100,#80101));
#17627=EDGE_LOOP('',(#80102,#80103,#80104,#80105));
#17628=EDGE_LOOP('',(#80106,#80107,#80108,#80109));
#17629=EDGE_LOOP('',(#80110,#80111,#80112,#80113));
#17630=EDGE_LOOP('',(#80114,#80115,#80116,#80117));
#17631=EDGE_LOOP('',(#80118,#80119,#80120,#80121));
#17632=EDGE_LOOP('',(#80122,#80123,#80124,#80125,#80126));
#17633=EDGE_LOOP('',(#80127,#80128,#80129,#80130));
#17634=EDGE_LOOP('',(#80131,#80132,#80133,#80134));
#17635=EDGE_LOOP('',(#80135,#80136,#80137,#80138,#80139));
#17636=EDGE_LOOP('',(#80140,#80141,#80142,#80143));
#17637=EDGE_LOOP('',(#80144,#80145,#80146,#80147));
#17638=EDGE_LOOP('',(#80148,#80149,#80150,#80151));
#17639=EDGE_LOOP('',(#80152,#80153,#80154,#80155));
#17640=EDGE_LOOP('',(#80156,#80157,#80158,#80159,#80160));
#17641=EDGE_LOOP('',(#80161,#80162,#80163,#80164));
#17642=EDGE_LOOP('',(#80165,#80166,#80167,#80168));
#17643=EDGE_LOOP('',(#80169,#80170,#80171,#80172));
#17644=EDGE_LOOP('',(#80173,#80174,#80175,#80176));
#17645=EDGE_LOOP('',(#80177,#80178,#80179,#80180));
#17646=EDGE_LOOP('',(#80181,#80182,#80183,#80184));
#17647=EDGE_LOOP('',(#80185,#80186,#80187,#80188));
#17648=EDGE_LOOP('',(#80189,#80190,#80191,#80192));
#17649=EDGE_LOOP('',(#80193,#80194,#80195,#80196));
#17650=EDGE_LOOP('',(#80197,#80198,#80199,#80200));
#17651=EDGE_LOOP('',(#80201,#80202,#80203,#80204,#80205));
#17652=EDGE_LOOP('',(#80206,#80207,#80208,#80209));
#17653=EDGE_LOOP('',(#80210,#80211,#80212,#80213));
#17654=EDGE_LOOP('',(#80214,#80215,#80216,#80217));
#17655=EDGE_LOOP('',(#80218,#80219,#80220,#80221));
#17656=EDGE_LOOP('',(#80222,#80223,#80224,#80225));
#17657=EDGE_LOOP('',(#80226,#80227,#80228,#80229));
#17658=EDGE_LOOP('',(#80230,#80231,#80232,#80233));
#17659=EDGE_LOOP('',(#80234,#80235,#80236,#80237));
#17660=EDGE_LOOP('',(#80238,#80239,#80240,#80241,#80242));
#17661=EDGE_LOOP('',(#80243,#80244,#80245,#80246));
#17662=EDGE_LOOP('',(#80247,#80248,#80249,#80250));
#17663=EDGE_LOOP('',(#80251,#80252,#80253,#80254,#80255));
#17664=EDGE_LOOP('',(#80256,#80257,#80258,#80259));
#17665=EDGE_LOOP('',(#80260,#80261,#80262,#80263));
#17666=EDGE_LOOP('',(#80264,#80265,#80266,#80267));
#17667=EDGE_LOOP('',(#80268,#80269,#80270,#80271));
#17668=EDGE_LOOP('',(#80272,#80273,#80274,#80275,#80276));
#17669=EDGE_LOOP('',(#80277,#80278,#80279,#80280));
#17670=EDGE_LOOP('',(#80281,#80282,#80283,#80284));
#17671=EDGE_LOOP('',(#80285,#80286,#80287,#80288));
#17672=EDGE_LOOP('',(#80289,#80290,#80291,#80292));
#17673=EDGE_LOOP('',(#80293,#80294,#80295,#80296));
#17674=EDGE_LOOP('',(#80297,#80298,#80299,#80300));
#17675=EDGE_LOOP('',(#80301,#80302,#80303,#80304));
#17676=EDGE_LOOP('',(#80305,#80306,#80307,#80308));
#17677=EDGE_LOOP('',(#80309,#80310,#80311,#80312));
#17678=EDGE_LOOP('',(#80313,#80314,#80315,#80316));
#17679=EDGE_LOOP('',(#80317,#80318,#80319,#80320,#80321));
#17680=EDGE_LOOP('',(#80322,#80323,#80324,#80325));
#17681=EDGE_LOOP('',(#80326,#80327,#80328,#80329));
#17682=EDGE_LOOP('',(#80330,#80331,#80332,#80333));
#17683=EDGE_LOOP('',(#80334,#80335,#80336,#80337));
#17684=EDGE_LOOP('',(#80338,#80339,#80340,#80341));
#17685=EDGE_LOOP('',(#80342,#80343,#80344,#80345));
#17686=EDGE_LOOP('',(#80346,#80347,#80348,#80349));
#17687=EDGE_LOOP('',(#80350,#80351,#80352,#80353));
#17688=EDGE_LOOP('',(#80354,#80355,#80356,#80357,#80358));
#17689=EDGE_LOOP('',(#80359,#80360,#80361,#80362));
#17690=EDGE_LOOP('',(#80363,#80364,#80365,#80366));
#17691=EDGE_LOOP('',(#80367,#80368,#80369,#80370,#80371));
#17692=EDGE_LOOP('',(#80372,#80373,#80374,#80375));
#17693=EDGE_LOOP('',(#80376,#80377,#80378,#80379));
#17694=EDGE_LOOP('',(#80380,#80381,#80382,#80383));
#17695=EDGE_LOOP('',(#80384,#80385,#80386,#80387));
#17696=EDGE_LOOP('',(#80388,#80389,#80390,#80391,#80392));
#17697=EDGE_LOOP('',(#80393,#80394,#80395,#80396));
#17698=EDGE_LOOP('',(#80397,#80398,#80399,#80400));
#17699=EDGE_LOOP('',(#80401,#80402,#80403,#80404));
#17700=EDGE_LOOP('',(#80405,#80406,#80407,#80408));
#17701=EDGE_LOOP('',(#80409,#80410,#80411,#80412));
#17702=EDGE_LOOP('',(#80413,#80414,#80415,#80416));
#17703=EDGE_LOOP('',(#80417,#80418,#80419,#80420));
#17704=EDGE_LOOP('',(#80421,#80422,#80423,#80424));
#17705=EDGE_LOOP('',(#80425,#80426,#80427,#80428));
#17706=EDGE_LOOP('',(#80429,#80430,#80431,#80432));
#17707=EDGE_LOOP('',(#80433,#80434,#80435,#80436,#80437));
#17708=EDGE_LOOP('',(#80438,#80439,#80440,#80441));
#17709=EDGE_LOOP('',(#80442,#80443,#80444,#80445));
#17710=EDGE_LOOP('',(#80446,#80447,#80448,#80449));
#17711=EDGE_LOOP('',(#80450,#80451,#80452,#80453));
#17712=EDGE_LOOP('',(#80454,#80455,#80456,#80457));
#17713=EDGE_LOOP('',(#80458,#80459,#80460,#80461));
#17714=EDGE_LOOP('',(#80462,#80463,#80464,#80465));
#17715=EDGE_LOOP('',(#80466,#80467,#80468,#80469));
#17716=EDGE_LOOP('',(#80470,#80471,#80472,#80473,#80474));
#17717=EDGE_LOOP('',(#80475,#80476,#80477,#80478));
#17718=EDGE_LOOP('',(#80479,#80480,#80481,#80482));
#17719=EDGE_LOOP('',(#80483,#80484,#80485,#80486,#80487));
#17720=EDGE_LOOP('',(#80488,#80489,#80490,#80491));
#17721=EDGE_LOOP('',(#80492,#80493,#80494,#80495));
#17722=EDGE_LOOP('',(#80496,#80497,#80498,#80499));
#17723=EDGE_LOOP('',(#80500,#80501,#80502,#80503));
#17724=EDGE_LOOP('',(#80504,#80505,#80506,#80507,#80508));
#17725=EDGE_LOOP('',(#80509,#80510,#80511,#80512));
#17726=EDGE_LOOP('',(#80513,#80514,#80515,#80516));
#17727=EDGE_LOOP('',(#80517,#80518,#80519,#80520));
#17728=EDGE_LOOP('',(#80521,#80522,#80523,#80524));
#17729=EDGE_LOOP('',(#80525,#80526,#80527,#80528));
#17730=EDGE_LOOP('',(#80529,#80530,#80531,#80532));
#17731=EDGE_LOOP('',(#80533,#80534,#80535,#80536));
#17732=EDGE_LOOP('',(#80537,#80538,#80539,#80540));
#17733=EDGE_LOOP('',(#80541,#80542,#80543,#80544));
#17734=EDGE_LOOP('',(#80545,#80546,#80547,#80548));
#17735=EDGE_LOOP('',(#80549,#80550,#80551,#80552,#80553));
#17736=EDGE_LOOP('',(#80554,#80555,#80556,#80557));
#17737=EDGE_LOOP('',(#80558,#80559,#80560,#80561));
#17738=EDGE_LOOP('',(#80562,#80563,#80564,#80565));
#17739=EDGE_LOOP('',(#80566,#80567,#80568,#80569));
#17740=EDGE_LOOP('',(#80570,#80571,#80572,#80573));
#17741=EDGE_LOOP('',(#80574,#80575,#80576,#80577));
#17742=EDGE_LOOP('',(#80578,#80579,#80580,#80581));
#17743=EDGE_LOOP('',(#80582,#80583,#80584,#80585));
#17744=EDGE_LOOP('',(#80586,#80587,#80588,#80589,#80590));
#17745=EDGE_LOOP('',(#80591,#80592,#80593,#80594));
#17746=EDGE_LOOP('',(#80595,#80596,#80597,#80598));
#17747=EDGE_LOOP('',(#80599,#80600,#80601,#80602,#80603));
#17748=EDGE_LOOP('',(#80604,#80605,#80606,#80607));
#17749=EDGE_LOOP('',(#80608,#80609,#80610,#80611));
#17750=EDGE_LOOP('',(#80612,#80613,#80614,#80615));
#17751=EDGE_LOOP('',(#80616,#80617,#80618,#80619));
#17752=EDGE_LOOP('',(#80620,#80621,#80622,#80623,#80624));
#17753=EDGE_LOOP('',(#80625,#80626,#80627,#80628));
#17754=EDGE_LOOP('',(#80629,#80630,#80631,#80632));
#17755=EDGE_LOOP('',(#80633,#80634,#80635,#80636));
#17756=EDGE_LOOP('',(#80637,#80638,#80639,#80640));
#17757=EDGE_LOOP('',(#80641,#80642,#80643,#80644));
#17758=EDGE_LOOP('',(#80645,#80646,#80647,#80648));
#17759=EDGE_LOOP('',(#80649,#80650,#80651,#80652));
#17760=EDGE_LOOP('',(#80653,#80654,#80655,#80656));
#17761=EDGE_LOOP('',(#80657,#80658,#80659,#80660));
#17762=EDGE_LOOP('',(#80661,#80662,#80663,#80664));
#17763=EDGE_LOOP('',(#80665,#80666,#80667,#80668,#80669));
#17764=EDGE_LOOP('',(#80670,#80671,#80672,#80673));
#17765=EDGE_LOOP('',(#80674,#80675,#80676,#80677));
#17766=EDGE_LOOP('',(#80678,#80679,#80680,#80681));
#17767=EDGE_LOOP('',(#80682,#80683,#80684,#80685));
#17768=EDGE_LOOP('',(#80686,#80687,#80688,#80689));
#17769=EDGE_LOOP('',(#80690,#80691,#80692,#80693));
#17770=EDGE_LOOP('',(#80694,#80695,#80696,#80697));
#17771=EDGE_LOOP('',(#80698,#80699,#80700,#80701));
#17772=EDGE_LOOP('',(#80702,#80703,#80704,#80705,#80706));
#17773=EDGE_LOOP('',(#80707,#80708,#80709,#80710));
#17774=EDGE_LOOP('',(#80711,#80712,#80713,#80714));
#17775=EDGE_LOOP('',(#80715,#80716,#80717,#80718,#80719));
#17776=EDGE_LOOP('',(#80720,#80721,#80722,#80723));
#17777=EDGE_LOOP('',(#80724,#80725,#80726,#80727));
#17778=EDGE_LOOP('',(#80728,#80729,#80730,#80731));
#17779=EDGE_LOOP('',(#80732,#80733,#80734,#80735));
#17780=EDGE_LOOP('',(#80736,#80737,#80738,#80739,#80740));
#17781=EDGE_LOOP('',(#80741,#80742,#80743,#80744));
#17782=EDGE_LOOP('',(#80745,#80746,#80747,#80748));
#17783=EDGE_LOOP('',(#80749,#80750,#80751,#80752));
#17784=EDGE_LOOP('',(#80753,#80754,#80755,#80756));
#17785=EDGE_LOOP('',(#80757,#80758,#80759,#80760));
#17786=EDGE_LOOP('',(#80761,#80762,#80763,#80764));
#17787=EDGE_LOOP('',(#80765,#80766,#80767,#80768));
#17788=EDGE_LOOP('',(#80769,#80770,#80771,#80772));
#17789=EDGE_LOOP('',(#80773,#80774,#80775,#80776));
#17790=EDGE_LOOP('',(#80777,#80778,#80779,#80780));
#17791=EDGE_LOOP('',(#80781,#80782,#80783,#80784,#80785));
#17792=EDGE_LOOP('',(#80786,#80787,#80788,#80789));
#17793=EDGE_LOOP('',(#80790,#80791,#80792,#80793));
#17794=EDGE_LOOP('',(#80794,#80795,#80796,#80797));
#17795=EDGE_LOOP('',(#80798,#80799,#80800,#80801));
#17796=EDGE_LOOP('',(#80802,#80803,#80804,#80805));
#17797=EDGE_LOOP('',(#80806,#80807,#80808,#80809));
#17798=EDGE_LOOP('',(#80810,#80811,#80812,#80813));
#17799=EDGE_LOOP('',(#80814,#80815,#80816,#80817));
#17800=EDGE_LOOP('',(#80818,#80819,#80820,#80821,#80822));
#17801=EDGE_LOOP('',(#80823,#80824,#80825,#80826));
#17802=EDGE_LOOP('',(#80827,#80828,#80829,#80830));
#17803=EDGE_LOOP('',(#80831,#80832,#80833,#80834,#80835));
#17804=EDGE_LOOP('',(#80836,#80837,#80838,#80839));
#17805=EDGE_LOOP('',(#80840,#80841,#80842,#80843));
#17806=EDGE_LOOP('',(#80844,#80845,#80846,#80847));
#17807=EDGE_LOOP('',(#80848,#80849,#80850,#80851));
#17808=EDGE_LOOP('',(#80852,#80853,#80854,#80855,#80856));
#17809=EDGE_LOOP('',(#80857,#80858,#80859,#80860));
#17810=EDGE_LOOP('',(#80861,#80862,#80863,#80864));
#17811=EDGE_LOOP('',(#80865,#80866,#80867,#80868));
#17812=EDGE_LOOP('',(#80869,#80870,#80871,#80872));
#17813=EDGE_LOOP('',(#80873,#80874,#80875,#80876));
#17814=EDGE_LOOP('',(#80877,#80878,#80879,#80880));
#17815=EDGE_LOOP('',(#80881,#80882,#80883,#80884));
#17816=EDGE_LOOP('',(#80885,#80886,#80887,#80888));
#17817=EDGE_LOOP('',(#80889,#80890,#80891,#80892));
#17818=EDGE_LOOP('',(#80893,#80894,#80895,#80896));
#17819=EDGE_LOOP('',(#80897,#80898,#80899,#80900,#80901));
#17820=EDGE_LOOP('',(#80902,#80903,#80904,#80905));
#17821=EDGE_LOOP('',(#80906,#80907,#80908,#80909));
#17822=EDGE_LOOP('',(#80910,#80911,#80912,#80913));
#17823=EDGE_LOOP('',(#80914,#80915,#80916,#80917));
#17824=EDGE_LOOP('',(#80918,#80919,#80920,#80921));
#17825=EDGE_LOOP('',(#80922,#80923,#80924,#80925));
#17826=EDGE_LOOP('',(#80926,#80927,#80928,#80929));
#17827=EDGE_LOOP('',(#80930,#80931,#80932,#80933));
#17828=EDGE_LOOP('',(#80934,#80935,#80936,#80937,#80938));
#17829=EDGE_LOOP('',(#80939,#80940,#80941,#80942));
#17830=EDGE_LOOP('',(#80943,#80944,#80945,#80946));
#17831=EDGE_LOOP('',(#80947,#80948,#80949,#80950,#80951));
#17832=EDGE_LOOP('',(#80952,#80953,#80954,#80955));
#17833=EDGE_LOOP('',(#80956,#80957,#80958,#80959));
#17834=EDGE_LOOP('',(#80960,#80961,#80962,#80963));
#17835=EDGE_LOOP('',(#80964,#80965,#80966,#80967));
#17836=EDGE_LOOP('',(#80968,#80969,#80970,#80971,#80972));
#17837=EDGE_LOOP('',(#80973,#80974,#80975,#80976));
#17838=EDGE_LOOP('',(#80977,#80978,#80979,#80980));
#17839=EDGE_LOOP('',(#80981,#80982,#80983,#80984));
#17840=EDGE_LOOP('',(#80985,#80986,#80987,#80988));
#17841=EDGE_LOOP('',(#80989,#80990,#80991,#80992));
#17842=EDGE_LOOP('',(#80993,#80994,#80995,#80996));
#17843=EDGE_LOOP('',(#80997,#80998,#80999,#81000));
#17844=EDGE_LOOP('',(#81001,#81002,#81003,#81004));
#17845=EDGE_LOOP('',(#81005,#81006,#81007,#81008));
#17846=EDGE_LOOP('',(#81009,#81010,#81011,#81012));
#17847=EDGE_LOOP('',(#81013,#81014,#81015,#81016,#81017));
#17848=EDGE_LOOP('',(#81018,#81019,#81020,#81021));
#17849=EDGE_LOOP('',(#81022,#81023,#81024,#81025));
#17850=EDGE_LOOP('',(#81026,#81027,#81028,#81029));
#17851=EDGE_LOOP('',(#81030,#81031,#81032,#81033));
#17852=EDGE_LOOP('',(#81034,#81035,#81036,#81037));
#17853=EDGE_LOOP('',(#81038,#81039,#81040,#81041));
#17854=EDGE_LOOP('',(#81042,#81043,#81044,#81045));
#17855=EDGE_LOOP('',(#81046,#81047,#81048,#81049));
#17856=EDGE_LOOP('',(#81050,#81051,#81052,#81053,#81054));
#17857=EDGE_LOOP('',(#81055,#81056,#81057,#81058));
#17858=EDGE_LOOP('',(#81059,#81060,#81061,#81062));
#17859=EDGE_LOOP('',(#81063,#81064,#81065,#81066,#81067));
#17860=EDGE_LOOP('',(#81068,#81069,#81070,#81071));
#17861=EDGE_LOOP('',(#81072,#81073,#81074,#81075));
#17862=EDGE_LOOP('',(#81076,#81077,#81078,#81079));
#17863=EDGE_LOOP('',(#81080,#81081,#81082,#81083));
#17864=EDGE_LOOP('',(#81084,#81085,#81086,#81087,#81088));
#17865=EDGE_LOOP('',(#81089,#81090,#81091,#81092));
#17866=EDGE_LOOP('',(#81093,#81094,#81095,#81096));
#17867=EDGE_LOOP('',(#81097,#81098,#81099,#81100));
#17868=EDGE_LOOP('',(#81101,#81102,#81103,#81104));
#17869=EDGE_LOOP('',(#81105,#81106,#81107,#81108));
#17870=EDGE_LOOP('',(#81109,#81110,#81111,#81112));
#17871=EDGE_LOOP('',(#81113,#81114,#81115,#81116));
#17872=EDGE_LOOP('',(#81117,#81118,#81119,#81120));
#17873=EDGE_LOOP('',(#81121,#81122,#81123,#81124));
#17874=EDGE_LOOP('',(#81125,#81126,#81127,#81128));
#17875=EDGE_LOOP('',(#81129,#81130,#81131,#81132,#81133));
#17876=EDGE_LOOP('',(#81134,#81135,#81136,#81137));
#17877=EDGE_LOOP('',(#81138,#81139,#81140,#81141));
#17878=EDGE_LOOP('',(#81142,#81143,#81144,#81145));
#17879=EDGE_LOOP('',(#81146,#81147,#81148,#81149));
#17880=EDGE_LOOP('',(#81150,#81151,#81152,#81153));
#17881=EDGE_LOOP('',(#81154,#81155,#81156,#81157));
#17882=EDGE_LOOP('',(#81158,#81159,#81160,#81161));
#17883=EDGE_LOOP('',(#81162,#81163,#81164,#81165));
#17884=EDGE_LOOP('',(#81166,#81167,#81168,#81169,#81170));
#17885=EDGE_LOOP('',(#81171,#81172,#81173,#81174));
#17886=EDGE_LOOP('',(#81175,#81176,#81177,#81178));
#17887=EDGE_LOOP('',(#81179,#81180,#81181,#81182,#81183));
#17888=EDGE_LOOP('',(#81184,#81185,#81186,#81187));
#17889=EDGE_LOOP('',(#81188,#81189,#81190,#81191));
#17890=EDGE_LOOP('',(#81192,#81193,#81194,#81195));
#17891=EDGE_LOOP('',(#81196,#81197,#81198,#81199));
#17892=EDGE_LOOP('',(#81200,#81201,#81202,#81203,#81204));
#17893=EDGE_LOOP('',(#81205,#81206,#81207,#81208));
#17894=EDGE_LOOP('',(#81209,#81210,#81211,#81212));
#17895=EDGE_LOOP('',(#81213,#81214,#81215,#81216));
#17896=EDGE_LOOP('',(#81217,#81218,#81219,#81220));
#17897=EDGE_LOOP('',(#81221,#81222,#81223,#81224));
#17898=EDGE_LOOP('',(#81225,#81226,#81227,#81228));
#17899=EDGE_LOOP('',(#81229,#81230,#81231,#81232));
#17900=EDGE_LOOP('',(#81233,#81234,#81235,#81236));
#17901=EDGE_LOOP('',(#81237,#81238,#81239,#81240));
#17902=EDGE_LOOP('',(#81241,#81242,#81243,#81244));
#17903=EDGE_LOOP('',(#81245,#81246,#81247,#81248,#81249));
#17904=EDGE_LOOP('',(#81250,#81251,#81252,#81253));
#17905=EDGE_LOOP('',(#81254,#81255,#81256,#81257));
#17906=EDGE_LOOP('',(#81258,#81259,#81260,#81261));
#17907=EDGE_LOOP('',(#81262,#81263,#81264,#81265));
#17908=EDGE_LOOP('',(#81266,#81267,#81268,#81269));
#17909=EDGE_LOOP('',(#81270,#81271,#81272,#81273));
#17910=EDGE_LOOP('',(#81274,#81275,#81276,#81277));
#17911=EDGE_LOOP('',(#81278,#81279,#81280,#81281));
#17912=EDGE_LOOP('',(#81282,#81283,#81284,#81285,#81286));
#17913=EDGE_LOOP('',(#81287,#81288,#81289,#81290));
#17914=EDGE_LOOP('',(#81291,#81292,#81293,#81294));
#17915=EDGE_LOOP('',(#81295,#81296,#81297,#81298,#81299));
#17916=EDGE_LOOP('',(#81300,#81301,#81302,#81303));
#17917=EDGE_LOOP('',(#81304,#81305,#81306,#81307));
#17918=EDGE_LOOP('',(#81308,#81309,#81310,#81311));
#17919=EDGE_LOOP('',(#81312,#81313,#81314,#81315));
#17920=EDGE_LOOP('',(#81316,#81317,#81318,#81319,#81320));
#17921=EDGE_LOOP('',(#81321,#81322,#81323,#81324));
#17922=EDGE_LOOP('',(#81325,#81326,#81327,#81328));
#17923=EDGE_LOOP('',(#81329,#81330,#81331,#81332));
#17924=EDGE_LOOP('',(#81333,#81334,#81335,#81336));
#17925=EDGE_LOOP('',(#81337,#81338,#81339,#81340));
#17926=EDGE_LOOP('',(#81341,#81342,#81343,#81344));
#17927=EDGE_LOOP('',(#81345,#81346,#81347,#81348));
#17928=EDGE_LOOP('',(#81349,#81350,#81351,#81352));
#17929=EDGE_LOOP('',(#81353,#81354,#81355,#81356));
#17930=EDGE_LOOP('',(#81357,#81358,#81359,#81360));
#17931=EDGE_LOOP('',(#81361,#81362,#81363,#81364,#81365));
#17932=EDGE_LOOP('',(#81366,#81367,#81368,#81369));
#17933=EDGE_LOOP('',(#81370,#81371,#81372,#81373));
#17934=EDGE_LOOP('',(#81374,#81375,#81376,#81377));
#17935=EDGE_LOOP('',(#81378,#81379,#81380,#81381));
#17936=EDGE_LOOP('',(#81382,#81383,#81384,#81385));
#17937=EDGE_LOOP('',(#81386,#81387,#81388,#81389));
#17938=EDGE_LOOP('',(#81390,#81391,#81392,#81393));
#17939=EDGE_LOOP('',(#81394,#81395,#81396,#81397));
#17940=EDGE_LOOP('',(#81398,#81399,#81400,#81401,#81402));
#17941=EDGE_LOOP('',(#81403,#81404,#81405,#81406));
#17942=EDGE_LOOP('',(#81407,#81408,#81409,#81410));
#17943=EDGE_LOOP('',(#81411,#81412,#81413,#81414,#81415));
#17944=EDGE_LOOP('',(#81416,#81417,#81418,#81419));
#17945=EDGE_LOOP('',(#81420,#81421,#81422,#81423));
#17946=EDGE_LOOP('',(#81424,#81425,#81426,#81427));
#17947=EDGE_LOOP('',(#81428,#81429,#81430,#81431));
#17948=EDGE_LOOP('',(#81432,#81433,#81434,#81435,#81436));
#17949=EDGE_LOOP('',(#81437,#81438,#81439,#81440));
#17950=EDGE_LOOP('',(#81441,#81442,#81443,#81444));
#17951=EDGE_LOOP('',(#81445,#81446,#81447,#81448));
#17952=EDGE_LOOP('',(#81449,#81450,#81451,#81452));
#17953=EDGE_LOOP('',(#81453,#81454,#81455,#81456));
#17954=EDGE_LOOP('',(#81457,#81458,#81459,#81460));
#17955=EDGE_LOOP('',(#81461,#81462,#81463,#81464));
#17956=EDGE_LOOP('',(#81465,#81466,#81467,#81468));
#17957=EDGE_LOOP('',(#81469,#81470,#81471,#81472));
#17958=EDGE_LOOP('',(#81473,#81474,#81475,#81476));
#17959=EDGE_LOOP('',(#81477,#81478,#81479,#81480,#81481));
#17960=EDGE_LOOP('',(#81482,#81483,#81484,#81485));
#17961=EDGE_LOOP('',(#81486,#81487,#81488,#81489));
#17962=EDGE_LOOP('',(#81490,#81491,#81492,#81493));
#17963=EDGE_LOOP('',(#81494,#81495,#81496,#81497));
#17964=EDGE_LOOP('',(#81498,#81499,#81500,#81501));
#17965=EDGE_LOOP('',(#81502,#81503,#81504,#81505));
#17966=EDGE_LOOP('',(#81506,#81507,#81508,#81509));
#17967=EDGE_LOOP('',(#81510,#81511,#81512,#81513));
#17968=EDGE_LOOP('',(#81514,#81515,#81516,#81517,#81518));
#17969=EDGE_LOOP('',(#81519,#81520,#81521,#81522));
#17970=EDGE_LOOP('',(#81523,#81524,#81525,#81526));
#17971=EDGE_LOOP('',(#81527,#81528,#81529,#81530,#81531));
#17972=EDGE_LOOP('',(#81532,#81533,#81534,#81535));
#17973=EDGE_LOOP('',(#81536,#81537,#81538,#81539));
#17974=EDGE_LOOP('',(#81540,#81541,#81542,#81543));
#17975=EDGE_LOOP('',(#81544,#81545,#81546,#81547));
#17976=EDGE_LOOP('',(#81548,#81549,#81550,#81551,#81552));
#17977=EDGE_LOOP('',(#81553,#81554,#81555,#81556));
#17978=EDGE_LOOP('',(#81557,#81558,#81559,#81560));
#17979=EDGE_LOOP('',(#81561,#81562,#81563,#81564));
#17980=EDGE_LOOP('',(#81565,#81566,#81567,#81568));
#17981=EDGE_LOOP('',(#81569,#81570,#81571,#81572));
#17982=EDGE_LOOP('',(#81573,#81574,#81575,#81576));
#17983=EDGE_LOOP('',(#81577,#81578,#81579,#81580));
#17984=EDGE_LOOP('',(#81581,#81582,#81583,#81584));
#17985=EDGE_LOOP('',(#81585,#81586,#81587,#81588));
#17986=EDGE_LOOP('',(#81589,#81590,#81591,#81592));
#17987=EDGE_LOOP('',(#81593,#81594,#81595,#81596,#81597));
#17988=EDGE_LOOP('',(#81598,#81599,#81600,#81601));
#17989=EDGE_LOOP('',(#81602,#81603,#81604,#81605));
#17990=EDGE_LOOP('',(#81606,#81607,#81608,#81609));
#17991=EDGE_LOOP('',(#81610,#81611,#81612,#81613));
#17992=EDGE_LOOP('',(#81614,#81615,#81616,#81617));
#17993=EDGE_LOOP('',(#81618,#81619,#81620,#81621));
#17994=EDGE_LOOP('',(#81622,#81623,#81624,#81625));
#17995=EDGE_LOOP('',(#81626,#81627,#81628,#81629));
#17996=EDGE_LOOP('',(#81630,#81631,#81632,#81633,#81634));
#17997=EDGE_LOOP('',(#81635,#81636,#81637,#81638));
#17998=EDGE_LOOP('',(#81639,#81640,#81641,#81642));
#17999=EDGE_LOOP('',(#81643,#81644,#81645,#81646,#81647));
#18000=EDGE_LOOP('',(#81648,#81649,#81650,#81651));
#18001=EDGE_LOOP('',(#81652,#81653,#81654,#81655));
#18002=EDGE_LOOP('',(#81656,#81657,#81658,#81659));
#18003=EDGE_LOOP('',(#81660,#81661,#81662,#81663));
#18004=EDGE_LOOP('',(#81664,#81665,#81666,#81667,#81668));
#18005=EDGE_LOOP('',(#81669,#81670,#81671,#81672));
#18006=EDGE_LOOP('',(#81673,#81674,#81675,#81676));
#18007=EDGE_LOOP('',(#81677,#81678,#81679,#81680));
#18008=EDGE_LOOP('',(#81681,#81682,#81683,#81684));
#18009=EDGE_LOOP('',(#81685,#81686,#81687,#81688));
#18010=EDGE_LOOP('',(#81689,#81690,#81691,#81692));
#18011=EDGE_LOOP('',(#81693,#81694,#81695,#81696));
#18012=EDGE_LOOP('',(#81697,#81698,#81699,#81700));
#18013=EDGE_LOOP('',(#81701,#81702,#81703,#81704));
#18014=EDGE_LOOP('',(#81705,#81706,#81707,#81708));
#18015=EDGE_LOOP('',(#81709,#81710,#81711,#81712,#81713));
#18016=EDGE_LOOP('',(#81714,#81715,#81716,#81717));
#18017=EDGE_LOOP('',(#81718,#81719,#81720,#81721));
#18018=EDGE_LOOP('',(#81722,#81723,#81724,#81725));
#18019=EDGE_LOOP('',(#81726,#81727,#81728,#81729));
#18020=EDGE_LOOP('',(#81730,#81731,#81732,#81733));
#18021=EDGE_LOOP('',(#81734,#81735,#81736,#81737));
#18022=EDGE_LOOP('',(#81738,#81739,#81740,#81741));
#18023=EDGE_LOOP('',(#81742,#81743,#81744,#81745));
#18024=EDGE_LOOP('',(#81746,#81747,#81748,#81749,#81750));
#18025=EDGE_LOOP('',(#81751,#81752,#81753,#81754));
#18026=EDGE_LOOP('',(#81755,#81756,#81757,#81758));
#18027=EDGE_LOOP('',(#81759,#81760,#81761,#81762,#81763));
#18028=EDGE_LOOP('',(#81764,#81765,#81766,#81767));
#18029=EDGE_LOOP('',(#81768,#81769,#81770,#81771));
#18030=EDGE_LOOP('',(#81772,#81773,#81774,#81775));
#18031=EDGE_LOOP('',(#81776,#81777,#81778,#81779));
#18032=EDGE_LOOP('',(#81780,#81781,#81782,#81783,#81784));
#18033=EDGE_LOOP('',(#81785,#81786,#81787,#81788));
#18034=EDGE_LOOP('',(#81789,#81790,#81791,#81792));
#18035=EDGE_LOOP('',(#81793,#81794,#81795,#81796));
#18036=EDGE_LOOP('',(#81797,#81798,#81799,#81800));
#18037=EDGE_LOOP('',(#81801,#81802,#81803,#81804));
#18038=EDGE_LOOP('',(#81805,#81806,#81807,#81808));
#18039=EDGE_LOOP('',(#81809,#81810,#81811,#81812));
#18040=EDGE_LOOP('',(#81813,#81814,#81815,#81816));
#18041=EDGE_LOOP('',(#81817,#81818,#81819,#81820));
#18042=EDGE_LOOP('',(#81821,#81822,#81823,#81824));
#18043=EDGE_LOOP('',(#81825,#81826,#81827,#81828,#81829));
#18044=EDGE_LOOP('',(#81830,#81831,#81832,#81833));
#18045=EDGE_LOOP('',(#81834,#81835,#81836,#81837));
#18046=EDGE_LOOP('',(#81838,#81839,#81840,#81841));
#18047=EDGE_LOOP('',(#81842,#81843,#81844,#81845));
#18048=EDGE_LOOP('',(#81846,#81847,#81848,#81849));
#18049=EDGE_LOOP('',(#81850,#81851,#81852,#81853));
#18050=EDGE_LOOP('',(#81854,#81855,#81856,#81857));
#18051=EDGE_LOOP('',(#81858,#81859,#81860,#81861));
#18052=EDGE_LOOP('',(#81862,#81863,#81864,#81865,#81866));
#18053=EDGE_LOOP('',(#81867,#81868,#81869,#81870));
#18054=EDGE_LOOP('',(#81871,#81872,#81873,#81874));
#18055=EDGE_LOOP('',(#81875,#81876,#81877,#81878,#81879));
#18056=EDGE_LOOP('',(#81880,#81881,#81882,#81883));
#18057=EDGE_LOOP('',(#81884,#81885,#81886,#81887));
#18058=EDGE_LOOP('',(#81888,#81889,#81890,#81891));
#18059=EDGE_LOOP('',(#81892,#81893,#81894,#81895));
#18060=EDGE_LOOP('',(#81896,#81897,#81898,#81899,#81900));
#18061=EDGE_LOOP('',(#81901,#81902,#81903,#81904));
#18062=EDGE_LOOP('',(#81905,#81906,#81907,#81908));
#18063=EDGE_LOOP('',(#81909,#81910,#81911,#81912));
#18064=EDGE_LOOP('',(#81913,#81914,#81915,#81916));
#18065=EDGE_LOOP('',(#81917,#81918,#81919,#81920));
#18066=EDGE_LOOP('',(#81921,#81922,#81923,#81924));
#18067=EDGE_LOOP('',(#81925,#81926,#81927,#81928));
#18068=EDGE_LOOP('',(#81929,#81930,#81931,#81932));
#18069=EDGE_LOOP('',(#81933,#81934,#81935,#81936));
#18070=EDGE_LOOP('',(#81937,#81938,#81939,#81940));
#18071=EDGE_LOOP('',(#81941,#81942,#81943,#81944,#81945));
#18072=EDGE_LOOP('',(#81946,#81947,#81948,#81949));
#18073=EDGE_LOOP('',(#81950,#81951,#81952,#81953));
#18074=EDGE_LOOP('',(#81954,#81955,#81956,#81957));
#18075=EDGE_LOOP('',(#81958,#81959,#81960,#81961));
#18076=EDGE_LOOP('',(#81962,#81963,#81964,#81965));
#18077=EDGE_LOOP('',(#81966,#81967,#81968,#81969));
#18078=EDGE_LOOP('',(#81970,#81971,#81972,#81973));
#18079=EDGE_LOOP('',(#81974,#81975,#81976,#81977));
#18080=EDGE_LOOP('',(#81978,#81979,#81980,#81981,#81982));
#18081=EDGE_LOOP('',(#81983,#81984,#81985,#81986));
#18082=EDGE_LOOP('',(#81987,#81988,#81989,#81990));
#18083=EDGE_LOOP('',(#81991,#81992,#81993,#81994,#81995));
#18084=EDGE_LOOP('',(#81996,#81997,#81998,#81999));
#18085=EDGE_LOOP('',(#82000,#82001,#82002,#82003));
#18086=EDGE_LOOP('',(#82004,#82005,#82006,#82007));
#18087=EDGE_LOOP('',(#82008,#82009,#82010,#82011));
#18088=EDGE_LOOP('',(#82012,#82013,#82014,#82015,#82016));
#18089=EDGE_LOOP('',(#82017,#82018,#82019,#82020));
#18090=EDGE_LOOP('',(#82021,#82022,#82023,#82024));
#18091=EDGE_LOOP('',(#82025,#82026,#82027,#82028));
#18092=EDGE_LOOP('',(#82029,#82030,#82031,#82032));
#18093=EDGE_LOOP('',(#82033,#82034,#82035,#82036));
#18094=EDGE_LOOP('',(#82037,#82038,#82039,#82040));
#18095=EDGE_LOOP('',(#82041,#82042,#82043,#82044));
#18096=EDGE_LOOP('',(#82045,#82046,#82047,#82048));
#18097=EDGE_LOOP('',(#82049,#82050,#82051,#82052));
#18098=EDGE_LOOP('',(#82053,#82054,#82055,#82056));
#18099=EDGE_LOOP('',(#82057,#82058,#82059,#82060,#82061));
#18100=EDGE_LOOP('',(#82062,#82063,#82064,#82065));
#18101=EDGE_LOOP('',(#82066,#82067,#82068,#82069));
#18102=EDGE_LOOP('',(#82070,#82071,#82072,#82073));
#18103=EDGE_LOOP('',(#82074,#82075,#82076,#82077));
#18104=EDGE_LOOP('',(#82078,#82079,#82080,#82081));
#18105=EDGE_LOOP('',(#82082,#82083,#82084,#82085));
#18106=EDGE_LOOP('',(#82086,#82087,#82088,#82089));
#18107=EDGE_LOOP('',(#82090,#82091,#82092,#82093));
#18108=EDGE_LOOP('',(#82094,#82095,#82096,#82097,#82098));
#18109=EDGE_LOOP('',(#82099,#82100,#82101,#82102));
#18110=EDGE_LOOP('',(#82103,#82104,#82105,#82106));
#18111=EDGE_LOOP('',(#82107,#82108,#82109,#82110,#82111));
#18112=EDGE_LOOP('',(#82112,#82113,#82114,#82115));
#18113=EDGE_LOOP('',(#82116,#82117,#82118,#82119));
#18114=EDGE_LOOP('',(#82120,#82121,#82122,#82123));
#18115=EDGE_LOOP('',(#82124,#82125,#82126,#82127));
#18116=EDGE_LOOP('',(#82128,#82129,#82130,#82131,#82132));
#18117=EDGE_LOOP('',(#82133,#82134,#82135,#82136));
#18118=EDGE_LOOP('',(#82137,#82138,#82139,#82140));
#18119=EDGE_LOOP('',(#82141,#82142,#82143,#82144));
#18120=EDGE_LOOP('',(#82145,#82146,#82147,#82148));
#18121=EDGE_LOOP('',(#82149,#82150,#82151,#82152));
#18122=EDGE_LOOP('',(#82153,#82154,#82155,#82156));
#18123=EDGE_LOOP('',(#82157,#82158,#82159,#82160));
#18124=EDGE_LOOP('',(#82161,#82162,#82163,#82164));
#18125=EDGE_LOOP('',(#82165,#82166,#82167,#82168));
#18126=EDGE_LOOP('',(#82169,#82170,#82171,#82172));
#18127=EDGE_LOOP('',(#82173,#82174,#82175,#82176,#82177));
#18128=EDGE_LOOP('',(#82178,#82179,#82180,#82181));
#18129=EDGE_LOOP('',(#82182,#82183,#82184,#82185));
#18130=EDGE_LOOP('',(#82186,#82187,#82188,#82189));
#18131=EDGE_LOOP('',(#82190,#82191,#82192,#82193));
#18132=EDGE_LOOP('',(#82194,#82195,#82196,#82197));
#18133=EDGE_LOOP('',(#82198,#82199,#82200,#82201));
#18134=EDGE_LOOP('',(#82202,#82203,#82204,#82205));
#18135=EDGE_LOOP('',(#82206,#82207,#82208,#82209));
#18136=EDGE_LOOP('',(#82210,#82211,#82212,#82213,#82214));
#18137=EDGE_LOOP('',(#82215,#82216,#82217,#82218));
#18138=EDGE_LOOP('',(#82219,#82220,#82221,#82222));
#18139=EDGE_LOOP('',(#82223,#82224,#82225,#82226,#82227));
#18140=EDGE_LOOP('',(#82228,#82229,#82230,#82231));
#18141=EDGE_LOOP('',(#82232,#82233,#82234,#82235));
#18142=EDGE_LOOP('',(#82236,#82237,#82238,#82239));
#18143=EDGE_LOOP('',(#82240,#82241,#82242,#82243));
#18144=EDGE_LOOP('',(#82244,#82245,#82246,#82247,#82248));
#18145=EDGE_LOOP('',(#82249,#82250,#82251,#82252));
#18146=EDGE_LOOP('',(#82253,#82254,#82255,#82256));
#18147=EDGE_LOOP('',(#82257,#82258,#82259,#82260));
#18148=EDGE_LOOP('',(#82261,#82262,#82263,#82264));
#18149=EDGE_LOOP('',(#82265,#82266,#82267,#82268));
#18150=EDGE_LOOP('',(#82269,#82270,#82271,#82272));
#18151=EDGE_LOOP('',(#82273,#82274,#82275,#82276));
#18152=EDGE_LOOP('',(#82277,#82278,#82279,#82280));
#18153=EDGE_LOOP('',(#82281,#82282,#82283,#82284));
#18154=EDGE_LOOP('',(#82285,#82286,#82287,#82288));
#18155=EDGE_LOOP('',(#82289,#82290,#82291,#82292,#82293));
#18156=EDGE_LOOP('',(#82294,#82295,#82296,#82297));
#18157=EDGE_LOOP('',(#82298,#82299,#82300,#82301));
#18158=EDGE_LOOP('',(#82302,#82303,#82304,#82305));
#18159=EDGE_LOOP('',(#82306,#82307,#82308,#82309));
#18160=EDGE_LOOP('',(#82310,#82311,#82312,#82313));
#18161=EDGE_LOOP('',(#82314,#82315,#82316,#82317));
#18162=EDGE_LOOP('',(#82318,#82319,#82320,#82321));
#18163=EDGE_LOOP('',(#82322,#82323,#82324,#82325));
#18164=EDGE_LOOP('',(#82326,#82327,#82328,#82329,#82330));
#18165=EDGE_LOOP('',(#82331,#82332,#82333,#82334));
#18166=EDGE_LOOP('',(#82335,#82336,#82337,#82338));
#18167=EDGE_LOOP('',(#82339,#82340,#82341,#82342,#82343));
#18168=EDGE_LOOP('',(#82344,#82345,#82346,#82347));
#18169=EDGE_LOOP('',(#82348,#82349,#82350,#82351));
#18170=EDGE_LOOP('',(#82352,#82353,#82354,#82355));
#18171=EDGE_LOOP('',(#82356,#82357,#82358,#82359));
#18172=EDGE_LOOP('',(#82360,#82361,#82362,#82363,#82364));
#18173=EDGE_LOOP('',(#82365,#82366,#82367,#82368));
#18174=EDGE_LOOP('',(#82369,#82370,#82371,#82372));
#18175=EDGE_LOOP('',(#82373,#82374,#82375,#82376));
#18176=EDGE_LOOP('',(#82377,#82378,#82379,#82380));
#18177=EDGE_LOOP('',(#82381,#82382,#82383,#82384));
#18178=EDGE_LOOP('',(#82385,#82386,#82387,#82388));
#18179=EDGE_LOOP('',(#82389,#82390,#82391,#82392));
#18180=EDGE_LOOP('',(#82393,#82394,#82395,#82396));
#18181=EDGE_LOOP('',(#82397,#82398,#82399,#82400,#82401));
#18182=EDGE_LOOP('',(#82402,#82403,#82404,#82405));
#18183=EDGE_LOOP('',(#82406,#82407,#82408,#82409));
#18184=EDGE_LOOP('',(#82410,#82411,#82412,#82413));
#18185=EDGE_LOOP('',(#82414,#82415,#82416,#82417));
#18186=EDGE_LOOP('',(#82418,#82419,#82420,#82421));
#18187=EDGE_LOOP('',(#82422,#82423,#82424,#82425));
#18188=EDGE_LOOP('',(#82426,#82427,#82428,#82429));
#18189=EDGE_LOOP('',(#82430,#82431,#82432,#82433));
#18190=EDGE_LOOP('',(#82434,#82435,#82436,#82437,#82438));
#18191=EDGE_LOOP('',(#82439,#82440,#82441,#82442));
#18192=EDGE_LOOP('',(#82443,#82444,#82445,#82446));
#18193=EDGE_LOOP('',(#82447,#82448,#82449,#82450,#82451));
#18194=EDGE_LOOP('',(#82452,#82453,#82454,#82455));
#18195=EDGE_LOOP('',(#82456,#82457,#82458,#82459));
#18196=EDGE_LOOP('',(#82460,#82461,#82462,#82463));
#18197=EDGE_LOOP('',(#82464,#82465,#82466,#82467));
#18198=EDGE_LOOP('',(#82468,#82469,#82470,#82471,#82472));
#18199=EDGE_LOOP('',(#82473,#82474,#82475,#82476));
#18200=EDGE_LOOP('',(#82477,#82478,#82479,#82480));
#18201=EDGE_LOOP('',(#82481,#82482,#82483,#82484));
#18202=EDGE_LOOP('',(#82485,#82486,#82487,#82488));
#18203=EDGE_LOOP('',(#82489,#82490,#82491,#82492));
#18204=EDGE_LOOP('',(#82493,#82494,#82495,#82496));
#18205=EDGE_LOOP('',(#82497,#82498,#82499,#82500));
#18206=EDGE_LOOP('',(#82501,#82502,#82503,#82504));
#18207=EDGE_LOOP('',(#82505,#82506,#82507,#82508));
#18208=EDGE_LOOP('',(#82509,#82510,#82511,#82512));
#18209=EDGE_LOOP('',(#82513,#82514,#82515,#82516,#82517));
#18210=EDGE_LOOP('',(#82518,#82519,#82520,#82521));
#18211=EDGE_LOOP('',(#82522,#82523,#82524,#82525));
#18212=EDGE_LOOP('',(#82526,#82527,#82528,#82529));
#18213=EDGE_LOOP('',(#82530,#82531,#82532,#82533));
#18214=EDGE_LOOP('',(#82534,#82535,#82536,#82537));
#18215=EDGE_LOOP('',(#82538,#82539,#82540,#82541));
#18216=EDGE_LOOP('',(#82542,#82543,#82544,#82545));
#18217=EDGE_LOOP('',(#82546,#82547,#82548,#82549));
#18218=EDGE_LOOP('',(#82550,#82551,#82552,#82553,#82554));
#18219=EDGE_LOOP('',(#82555,#82556,#82557,#82558));
#18220=EDGE_LOOP('',(#82559,#82560,#82561,#82562));
#18221=EDGE_LOOP('',(#82563,#82564,#82565,#82566,#82567));
#18222=EDGE_LOOP('',(#82568,#82569,#82570,#82571));
#18223=EDGE_LOOP('',(#82572,#82573,#82574,#82575));
#18224=EDGE_LOOP('',(#82576,#82577,#82578,#82579));
#18225=EDGE_LOOP('',(#82580,#82581,#82582,#82583));
#18226=EDGE_LOOP('',(#82584,#82585,#82586,#82587,#82588));
#18227=EDGE_LOOP('',(#82589,#82590,#82591,#82592));
#18228=EDGE_LOOP('',(#82593,#82594,#82595,#82596));
#18229=EDGE_LOOP('',(#82597,#82598,#82599,#82600));
#18230=EDGE_LOOP('',(#82601,#82602,#82603,#82604));
#18231=EDGE_LOOP('',(#82605,#82606,#82607,#82608));
#18232=EDGE_LOOP('',(#82609,#82610,#82611,#82612));
#18233=EDGE_LOOP('',(#82613,#82614,#82615,#82616));
#18234=EDGE_LOOP('',(#82617,#82618,#82619,#82620));
#18235=EDGE_LOOP('',(#82621,#82622,#82623,#82624));
#18236=EDGE_LOOP('',(#82625,#82626,#82627,#82628));
#18237=EDGE_LOOP('',(#82629,#82630,#82631,#82632,#82633));
#18238=EDGE_LOOP('',(#82634,#82635,#82636,#82637));
#18239=EDGE_LOOP('',(#82638,#82639,#82640,#82641));
#18240=EDGE_LOOP('',(#82642,#82643,#82644,#82645));
#18241=EDGE_LOOP('',(#82646,#82647,#82648,#82649));
#18242=EDGE_LOOP('',(#82650,#82651,#82652,#82653));
#18243=EDGE_LOOP('',(#82654,#82655,#82656,#82657));
#18244=EDGE_LOOP('',(#82658,#82659,#82660,#82661));
#18245=EDGE_LOOP('',(#82662,#82663,#82664,#82665));
#18246=EDGE_LOOP('',(#82666,#82667,#82668,#82669,#82670));
#18247=EDGE_LOOP('',(#82671,#82672,#82673,#82674));
#18248=EDGE_LOOP('',(#82675,#82676,#82677,#82678));
#18249=EDGE_LOOP('',(#82679,#82680,#82681,#82682,#82683));
#18250=EDGE_LOOP('',(#82684,#82685,#82686,#82687));
#18251=EDGE_LOOP('',(#82688,#82689,#82690,#82691));
#18252=EDGE_LOOP('',(#82692,#82693,#82694,#82695));
#18253=EDGE_LOOP('',(#82696,#82697,#82698,#82699));
#18254=EDGE_LOOP('',(#82700,#82701,#82702,#82703,#82704));
#18255=EDGE_LOOP('',(#82705,#82706,#82707,#82708));
#18256=EDGE_LOOP('',(#82709,#82710,#82711,#82712));
#18257=EDGE_LOOP('',(#82713,#82714,#82715,#82716));
#18258=EDGE_LOOP('',(#82717,#82718,#82719,#82720));
#18259=EDGE_LOOP('',(#82721,#82722,#82723,#82724));
#18260=EDGE_LOOP('',(#82725,#82726,#82727,#82728));
#18261=EDGE_LOOP('',(#82729,#82730,#82731,#82732));
#18262=EDGE_LOOP('',(#82733,#82734,#82735,#82736));
#18263=EDGE_LOOP('',(#82737,#82738,#82739,#82740));
#18264=EDGE_LOOP('',(#82741,#82742,#82743,#82744));
#18265=EDGE_LOOP('',(#82745,#82746,#82747,#82748,#82749));
#18266=EDGE_LOOP('',(#82750,#82751,#82752,#82753));
#18267=EDGE_LOOP('',(#82754,#82755,#82756,#82757));
#18268=EDGE_LOOP('',(#82758,#82759,#82760,#82761));
#18269=EDGE_LOOP('',(#82762,#82763,#82764,#82765));
#18270=EDGE_LOOP('',(#82766,#82767,#82768,#82769));
#18271=EDGE_LOOP('',(#82770,#82771,#82772,#82773));
#18272=EDGE_LOOP('',(#82774,#82775,#82776,#82777));
#18273=EDGE_LOOP('',(#82778,#82779,#82780,#82781));
#18274=EDGE_LOOP('',(#82782,#82783,#82784,#82785,#82786));
#18275=EDGE_LOOP('',(#82787,#82788,#82789,#82790));
#18276=EDGE_LOOP('',(#82791,#82792,#82793,#82794));
#18277=EDGE_LOOP('',(#82795,#82796,#82797,#82798,#82799));
#18278=EDGE_LOOP('',(#82800,#82801,#82802,#82803));
#18279=EDGE_LOOP('',(#82804,#82805,#82806,#82807));
#18280=EDGE_LOOP('',(#82808,#82809,#82810,#82811));
#18281=EDGE_LOOP('',(#82812,#82813,#82814,#82815));
#18282=EDGE_LOOP('',(#82816,#82817,#82818,#82819,#82820));
#18283=EDGE_LOOP('',(#82821,#82822,#82823,#82824));
#18284=EDGE_LOOP('',(#82825,#82826,#82827,#82828));
#18285=EDGE_LOOP('',(#82829,#82830,#82831,#82832));
#18286=EDGE_LOOP('',(#82833,#82834,#82835,#82836));
#18287=EDGE_LOOP('',(#82837,#82838,#82839,#82840));
#18288=EDGE_LOOP('',(#82841,#82842,#82843,#82844));
#18289=EDGE_LOOP('',(#82845,#82846,#82847,#82848));
#18290=EDGE_LOOP('',(#82849,#82850,#82851,#82852));
#18291=EDGE_LOOP('',(#82853,#82854,#82855,#82856));
#18292=EDGE_LOOP('',(#82857,#82858,#82859,#82860));
#18293=EDGE_LOOP('',(#82861,#82862,#82863,#82864,#82865));
#18294=EDGE_LOOP('',(#82866,#82867,#82868,#82869));
#18295=EDGE_LOOP('',(#82870,#82871,#82872,#82873));
#18296=EDGE_LOOP('',(#82874,#82875,#82876,#82877));
#18297=EDGE_LOOP('',(#82878,#82879,#82880,#82881));
#18298=EDGE_LOOP('',(#82882,#82883,#82884,#82885));
#18299=EDGE_LOOP('',(#82886,#82887,#82888,#82889));
#18300=EDGE_LOOP('',(#82890,#82891,#82892,#82893));
#18301=EDGE_LOOP('',(#82894,#82895,#82896,#82897));
#18302=EDGE_LOOP('',(#82898,#82899,#82900,#82901,#82902));
#18303=EDGE_LOOP('',(#82903,#82904,#82905,#82906));
#18304=EDGE_LOOP('',(#82907,#82908,#82909,#82910));
#18305=EDGE_LOOP('',(#82911,#82912,#82913,#82914,#82915));
#18306=EDGE_LOOP('',(#82916,#82917,#82918,#82919));
#18307=EDGE_LOOP('',(#82920,#82921,#82922,#82923));
#18308=EDGE_LOOP('',(#82924,#82925,#82926,#82927));
#18309=EDGE_LOOP('',(#82928,#82929,#82930,#82931));
#18310=EDGE_LOOP('',(#82932,#82933,#82934,#82935,#82936));
#18311=EDGE_LOOP('',(#82937,#82938,#82939,#82940));
#18312=EDGE_LOOP('',(#82941,#82942,#82943,#82944));
#18313=EDGE_LOOP('',(#82945,#82946,#82947,#82948));
#18314=EDGE_LOOP('',(#82949,#82950,#82951,#82952));
#18315=EDGE_LOOP('',(#82953,#82954,#82955,#82956));
#18316=EDGE_LOOP('',(#82957,#82958,#82959,#82960));
#18317=EDGE_LOOP('',(#82961,#82962,#82963,#82964));
#18318=EDGE_LOOP('',(#82965,#82966,#82967,#82968));
#18319=EDGE_LOOP('',(#82969,#82970,#82971,#82972));
#18320=EDGE_LOOP('',(#82973,#82974,#82975,#82976));
#18321=EDGE_LOOP('',(#82977,#82978,#82979,#82980,#82981));
#18322=EDGE_LOOP('',(#82982,#82983,#82984,#82985));
#18323=EDGE_LOOP('',(#82986,#82987,#82988,#82989));
#18324=EDGE_LOOP('',(#82990,#82991,#82992,#82993));
#18325=EDGE_LOOP('',(#82994,#82995,#82996,#82997));
#18326=EDGE_LOOP('',(#82998,#82999,#83000,#83001));
#18327=EDGE_LOOP('',(#83002,#83003,#83004,#83005));
#18328=EDGE_LOOP('',(#83006,#83007,#83008,#83009));
#18329=EDGE_LOOP('',(#83010,#83011,#83012,#83013));
#18330=EDGE_LOOP('',(#83014,#83015,#83016,#83017,#83018));
#18331=EDGE_LOOP('',(#83019,#83020,#83021,#83022));
#18332=EDGE_LOOP('',(#83023,#83024,#83025,#83026));
#18333=EDGE_LOOP('',(#83027,#83028,#83029,#83030,#83031));
#18334=EDGE_LOOP('',(#83032,#83033,#83034,#83035));
#18335=EDGE_LOOP('',(#83036,#83037,#83038,#83039));
#18336=EDGE_LOOP('',(#83040,#83041,#83042,#83043));
#18337=EDGE_LOOP('',(#83044,#83045,#83046,#83047));
#18338=EDGE_LOOP('',(#83048,#83049,#83050,#83051,#83052));
#18339=EDGE_LOOP('',(#83053,#83054,#83055,#83056));
#18340=EDGE_LOOP('',(#83057,#83058,#83059,#83060));
#18341=EDGE_LOOP('',(#83061,#83062,#83063,#83064));
#18342=EDGE_LOOP('',(#83065,#83066,#83067,#83068));
#18343=EDGE_LOOP('',(#83069,#83070,#83071,#83072));
#18344=EDGE_LOOP('',(#83073,#83074,#83075,#83076));
#18345=EDGE_LOOP('',(#83077,#83078,#83079,#83080));
#18346=EDGE_LOOP('',(#83081,#83082,#83083,#83084));
#18347=EDGE_LOOP('',(#83085,#83086,#83087,#83088));
#18348=EDGE_LOOP('',(#83089,#83090,#83091,#83092));
#18349=EDGE_LOOP('',(#83093,#83094,#83095,#83096,#83097));
#18350=EDGE_LOOP('',(#83098,#83099,#83100,#83101));
#18351=EDGE_LOOP('',(#83102,#83103,#83104,#83105));
#18352=EDGE_LOOP('',(#83106,#83107,#83108,#83109));
#18353=EDGE_LOOP('',(#83110,#83111,#83112,#83113));
#18354=EDGE_LOOP('',(#83114,#83115,#83116,#83117));
#18355=EDGE_LOOP('',(#83118,#83119,#83120,#83121));
#18356=EDGE_LOOP('',(#83122,#83123,#83124,#83125));
#18357=EDGE_LOOP('',(#83126,#83127,#83128,#83129));
#18358=EDGE_LOOP('',(#83130,#83131,#83132,#83133,#83134));
#18359=EDGE_LOOP('',(#83135,#83136,#83137,#83138));
#18360=EDGE_LOOP('',(#83139,#83140,#83141,#83142));
#18361=EDGE_LOOP('',(#83143,#83144,#83145,#83146,#83147));
#18362=EDGE_LOOP('',(#83148,#83149,#83150,#83151));
#18363=EDGE_LOOP('',(#83152,#83153,#83154,#83155));
#18364=EDGE_LOOP('',(#83156,#83157,#83158,#83159));
#18365=EDGE_LOOP('',(#83160,#83161,#83162,#83163));
#18366=EDGE_LOOP('',(#83164,#83165,#83166,#83167,#83168));
#18367=EDGE_LOOP('',(#83169,#83170,#83171,#83172));
#18368=EDGE_LOOP('',(#83173,#83174,#83175,#83176));
#18369=EDGE_LOOP('',(#83177,#83178,#83179,#83180));
#18370=EDGE_LOOP('',(#83181,#83182,#83183,#83184));
#18371=EDGE_LOOP('',(#83185,#83186,#83187,#83188));
#18372=EDGE_LOOP('',(#83189,#83190,#83191,#83192));
#18373=EDGE_LOOP('',(#83193,#83194,#83195,#83196));
#18374=EDGE_LOOP('',(#83197,#83198,#83199,#83200));
#18375=EDGE_LOOP('',(#83201,#83202,#83203,#83204));
#18376=EDGE_LOOP('',(#83205,#83206,#83207,#83208));
#18377=EDGE_LOOP('',(#83209,#83210,#83211,#83212,#83213));
#18378=EDGE_LOOP('',(#83214,#83215,#83216,#83217));
#18379=EDGE_LOOP('',(#83218,#83219,#83220,#83221));
#18380=EDGE_LOOP('',(#83222,#83223,#83224,#83225));
#18381=EDGE_LOOP('',(#83226,#83227,#83228,#83229));
#18382=EDGE_LOOP('',(#83230,#83231,#83232,#83233));
#18383=EDGE_LOOP('',(#83234,#83235,#83236,#83237));
#18384=EDGE_LOOP('',(#83238,#83239,#83240,#83241));
#18385=EDGE_LOOP('',(#83242,#83243,#83244,#83245));
#18386=EDGE_LOOP('',(#83246,#83247,#83248,#83249,#83250));
#18387=EDGE_LOOP('',(#83251,#83252,#83253,#83254));
#18388=EDGE_LOOP('',(#83255,#83256,#83257,#83258));
#18389=EDGE_LOOP('',(#83259,#83260,#83261,#83262,#83263));
#18390=EDGE_LOOP('',(#83264,#83265,#83266,#83267));
#18391=EDGE_LOOP('',(#83268,#83269,#83270,#83271));
#18392=EDGE_LOOP('',(#83272,#83273,#83274,#83275));
#18393=EDGE_LOOP('',(#83276,#83277,#83278,#83279));
#18394=EDGE_LOOP('',(#83280,#83281,#83282,#83283,#83284));
#18395=EDGE_LOOP('',(#83285,#83286,#83287,#83288));
#18396=EDGE_LOOP('',(#83289,#83290,#83291,#83292));
#18397=EDGE_LOOP('',(#83293,#83294,#83295,#83296));
#18398=EDGE_LOOP('',(#83297,#83298,#83299,#83300));
#18399=EDGE_LOOP('',(#83301,#83302,#83303,#83304));
#18400=EDGE_LOOP('',(#83305,#83306,#83307,#83308));
#18401=EDGE_LOOP('',(#83309,#83310,#83311,#83312));
#18402=EDGE_LOOP('',(#83313,#83314,#83315,#83316));
#18403=EDGE_LOOP('',(#83317,#83318,#83319,#83320));
#18404=EDGE_LOOP('',(#83321,#83322,#83323,#83324));
#18405=EDGE_LOOP('',(#83325,#83326,#83327,#83328,#83329));
#18406=EDGE_LOOP('',(#83330,#83331,#83332,#83333));
#18407=EDGE_LOOP('',(#83334,#83335,#83336,#83337));
#18408=EDGE_LOOP('',(#83338,#83339,#83340,#83341));
#18409=EDGE_LOOP('',(#83342,#83343,#83344,#83345));
#18410=EDGE_LOOP('',(#83346,#83347,#83348,#83349));
#18411=EDGE_LOOP('',(#83350,#83351,#83352,#83353));
#18412=EDGE_LOOP('',(#83354,#83355,#83356,#83357));
#18413=EDGE_LOOP('',(#83358,#83359,#83360,#83361));
#18414=EDGE_LOOP('',(#83362,#83363,#83364,#83365,#83366));
#18415=EDGE_LOOP('',(#83367,#83368,#83369,#83370));
#18416=EDGE_LOOP('',(#83371,#83372,#83373,#83374));
#18417=EDGE_LOOP('',(#83375,#83376,#83377,#83378,#83379));
#18418=EDGE_LOOP('',(#83380,#83381,#83382,#83383));
#18419=EDGE_LOOP('',(#83384,#83385,#83386,#83387));
#18420=EDGE_LOOP('',(#83388,#83389,#83390,#83391));
#18421=EDGE_LOOP('',(#83392,#83393,#83394,#83395));
#18422=EDGE_LOOP('',(#83396,#83397,#83398,#83399,#83400));
#18423=EDGE_LOOP('',(#83401,#83402,#83403,#83404));
#18424=EDGE_LOOP('',(#83405,#83406,#83407,#83408));
#18425=EDGE_LOOP('',(#83409,#83410,#83411,#83412));
#18426=EDGE_LOOP('',(#83413,#83414,#83415,#83416));
#18427=EDGE_LOOP('',(#83417,#83418,#83419,#83420));
#18428=EDGE_LOOP('',(#83421,#83422,#83423,#83424));
#18429=EDGE_LOOP('',(#83425,#83426,#83427,#83428));
#18430=EDGE_LOOP('',(#83429,#83430,#83431,#83432));
#18431=EDGE_LOOP('',(#83433,#83434,#83435,#83436));
#18432=EDGE_LOOP('',(#83437,#83438,#83439,#83440));
#18433=EDGE_LOOP('',(#83441,#83442,#83443,#83444,#83445));
#18434=EDGE_LOOP('',(#83446,#83447,#83448,#83449));
#18435=EDGE_LOOP('',(#83450,#83451,#83452,#83453));
#18436=EDGE_LOOP('',(#83454,#83455,#83456,#83457));
#18437=EDGE_LOOP('',(#83458,#83459,#83460,#83461));
#18438=EDGE_LOOP('',(#83462,#83463,#83464,#83465));
#18439=EDGE_LOOP('',(#83466,#83467,#83468,#83469));
#18440=EDGE_LOOP('',(#83470,#83471,#83472,#83473));
#18441=EDGE_LOOP('',(#83474,#83475,#83476,#83477));
#18442=EDGE_LOOP('',(#83478,#83479,#83480,#83481,#83482));
#18443=EDGE_LOOP('',(#83483,#83484,#83485,#83486));
#18444=EDGE_LOOP('',(#83487,#83488,#83489,#83490));
#18445=EDGE_LOOP('',(#83491,#83492,#83493,#83494,#83495));
#18446=EDGE_LOOP('',(#83496,#83497,#83498,#83499));
#18447=EDGE_LOOP('',(#83500,#83501,#83502,#83503));
#18448=EDGE_LOOP('',(#83504,#83505,#83506,#83507));
#18449=EDGE_LOOP('',(#83508,#83509,#83510,#83511));
#18450=EDGE_LOOP('',(#83512,#83513,#83514,#83515,#83516));
#18451=EDGE_LOOP('',(#83517,#83518,#83519,#83520));
#18452=EDGE_LOOP('',(#83521,#83522,#83523,#83524));
#18453=EDGE_LOOP('',(#83525,#83526,#83527,#83528));
#18454=EDGE_LOOP('',(#83529,#83530,#83531,#83532));
#18455=EDGE_LOOP('',(#83533,#83534,#83535,#83536));
#18456=EDGE_LOOP('',(#83537,#83538,#83539,#83540));
#18457=EDGE_LOOP('',(#83541,#83542,#83543,#83544));
#18458=EDGE_LOOP('',(#83545,#83546,#83547,#83548));
#18459=EDGE_LOOP('',(#83549,#83550,#83551,#83552));
#18460=EDGE_LOOP('',(#83553,#83554,#83555,#83556));
#18461=EDGE_LOOP('',(#83557,#83558,#83559,#83560,#83561));
#18462=EDGE_LOOP('',(#83562,#83563,#83564,#83565));
#18463=EDGE_LOOP('',(#83566,#83567,#83568,#83569));
#18464=EDGE_LOOP('',(#83570,#83571,#83572,#83573));
#18465=EDGE_LOOP('',(#83574,#83575,#83576,#83577));
#18466=EDGE_LOOP('',(#83578,#83579,#83580,#83581));
#18467=EDGE_LOOP('',(#83582,#83583,#83584,#83585));
#18468=EDGE_LOOP('',(#83586,#83587,#83588,#83589));
#18469=EDGE_LOOP('',(#83590,#83591,#83592,#83593));
#18470=EDGE_LOOP('',(#83594,#83595,#83596,#83597,#83598));
#18471=EDGE_LOOP('',(#83599,#83600,#83601,#83602));
#18472=EDGE_LOOP('',(#83603,#83604,#83605,#83606));
#18473=EDGE_LOOP('',(#83607,#83608,#83609,#83610,#83611));
#18474=EDGE_LOOP('',(#83612,#83613,#83614,#83615));
#18475=EDGE_LOOP('',(#83616,#83617,#83618,#83619));
#18476=EDGE_LOOP('',(#83620,#83621,#83622,#83623));
#18477=EDGE_LOOP('',(#83624,#83625,#83626,#83627));
#18478=EDGE_LOOP('',(#83628,#83629,#83630,#83631,#83632));
#18479=EDGE_LOOP('',(#83633,#83634,#83635,#83636));
#18480=EDGE_LOOP('',(#83637,#83638,#83639,#83640));
#18481=EDGE_LOOP('',(#83641,#83642,#83643,#83644));
#18482=EDGE_LOOP('',(#83645,#83646,#83647,#83648));
#18483=EDGE_LOOP('',(#83649,#83650,#83651,#83652));
#18484=EDGE_LOOP('',(#83653,#83654,#83655,#83656));
#18485=EDGE_LOOP('',(#83657,#83658,#83659,#83660));
#18486=EDGE_LOOP('',(#83661,#83662,#83663,#83664));
#18487=EDGE_LOOP('',(#83665,#83666,#83667,#83668));
#18488=EDGE_LOOP('',(#83669,#83670,#83671,#83672));
#18489=EDGE_LOOP('',(#83673,#83674,#83675,#83676,#83677));
#18490=EDGE_LOOP('',(#83678,#83679,#83680,#83681));
#18491=EDGE_LOOP('',(#83682,#83683,#83684,#83685));
#18492=EDGE_LOOP('',(#83686,#83687,#83688,#83689));
#18493=EDGE_LOOP('',(#83690,#83691,#83692,#83693));
#18494=EDGE_LOOP('',(#83694,#83695,#83696,#83697));
#18495=EDGE_LOOP('',(#83698,#83699,#83700,#83701));
#18496=EDGE_LOOP('',(#83702,#83703,#83704,#83705));
#18497=EDGE_LOOP('',(#83706,#83707,#83708,#83709));
#18498=EDGE_LOOP('',(#83710,#83711,#83712,#83713,#83714));
#18499=EDGE_LOOP('',(#83715,#83716,#83717,#83718));
#18500=EDGE_LOOP('',(#83719,#83720,#83721,#83722));
#18501=EDGE_LOOP('',(#83723,#83724,#83725,#83726,#83727));
#18502=EDGE_LOOP('',(#83728,#83729,#83730,#83731));
#18503=EDGE_LOOP('',(#83732,#83733,#83734,#83735));
#18504=EDGE_LOOP('',(#83736,#83737,#83738,#83739));
#18505=EDGE_LOOP('',(#83740,#83741,#83742,#83743));
#18506=EDGE_LOOP('',(#83744,#83745,#83746,#83747,#83748));
#18507=EDGE_LOOP('',(#83749,#83750,#83751,#83752));
#18508=EDGE_LOOP('',(#83753,#83754,#83755,#83756));
#18509=EDGE_LOOP('',(#83757,#83758,#83759,#83760));
#18510=EDGE_LOOP('',(#83761,#83762,#83763,#83764));
#18511=EDGE_LOOP('',(#83765,#83766,#83767,#83768));
#18512=EDGE_LOOP('',(#83769,#83770,#83771,#83772));
#18513=EDGE_LOOP('',(#83773,#83774,#83775,#83776));
#18514=EDGE_LOOP('',(#83777,#83778,#83779,#83780));
#18515=EDGE_LOOP('',(#83781,#83782,#83783,#83784));
#18516=EDGE_LOOP('',(#83785,#83786,#83787,#83788));
#18517=EDGE_LOOP('',(#83789,#83790,#83791,#83792,#83793));
#18518=EDGE_LOOP('',(#83794,#83795,#83796,#83797));
#18519=EDGE_LOOP('',(#83798,#83799,#83800,#83801));
#18520=EDGE_LOOP('',(#83802,#83803,#83804,#83805));
#18521=EDGE_LOOP('',(#83806,#83807,#83808,#83809));
#18522=EDGE_LOOP('',(#83810,#83811,#83812,#83813));
#18523=EDGE_LOOP('',(#83814,#83815,#83816,#83817));
#18524=EDGE_LOOP('',(#83818,#83819,#83820,#83821));
#18525=EDGE_LOOP('',(#83822,#83823,#83824,#83825));
#18526=EDGE_LOOP('',(#83826,#83827,#83828,#83829,#83830));
#18527=EDGE_LOOP('',(#83831,#83832,#83833,#83834));
#18528=EDGE_LOOP('',(#83835,#83836,#83837,#83838));
#18529=EDGE_LOOP('',(#83839,#83840,#83841,#83842,#83843));
#18530=EDGE_LOOP('',(#83844,#83845,#83846,#83847));
#18531=EDGE_LOOP('',(#83848,#83849,#83850,#83851));
#18532=EDGE_LOOP('',(#83852,#83853,#83854,#83855));
#18533=EDGE_LOOP('',(#83856,#83857,#83858,#83859));
#18534=EDGE_LOOP('',(#83860,#83861,#83862,#83863,#83864));
#18535=EDGE_LOOP('',(#83865,#83866,#83867,#83868));
#18536=EDGE_LOOP('',(#83869,#83870,#83871,#83872));
#18537=EDGE_LOOP('',(#83873,#83874,#83875,#83876));
#18538=EDGE_LOOP('',(#83877,#83878,#83879,#83880));
#18539=EDGE_LOOP('',(#83881,#83882,#83883,#83884));
#18540=EDGE_LOOP('',(#83885,#83886,#83887,#83888));
#18541=EDGE_LOOP('',(#83889,#83890,#83891,#83892));
#18542=EDGE_LOOP('',(#83893,#83894,#83895,#83896));
#18543=EDGE_LOOP('',(#83897,#83898,#83899,#83900));
#18544=EDGE_LOOP('',(#83901,#83902,#83903,#83904));
#18545=EDGE_LOOP('',(#83905,#83906,#83907,#83908,#83909));
#18546=EDGE_LOOP('',(#83910,#83911,#83912,#83913));
#18547=EDGE_LOOP('',(#83914,#83915,#83916,#83917));
#18548=EDGE_LOOP('',(#83918,#83919,#83920,#83921));
#18549=EDGE_LOOP('',(#83922,#83923,#83924,#83925));
#18550=EDGE_LOOP('',(#83926,#83927,#83928,#83929));
#18551=EDGE_LOOP('',(#83930,#83931,#83932,#83933));
#18552=EDGE_LOOP('',(#83934,#83935,#83936,#83937));
#18553=EDGE_LOOP('',(#83938,#83939,#83940,#83941));
#18554=EDGE_LOOP('',(#83942,#83943,#83944,#83945,#83946));
#18555=EDGE_LOOP('',(#83947,#83948,#83949,#83950));
#18556=EDGE_LOOP('',(#83951,#83952,#83953,#83954));
#18557=EDGE_LOOP('',(#83955,#83956,#83957,#83958,#83959));
#18558=EDGE_LOOP('',(#83960,#83961,#83962,#83963));
#18559=EDGE_LOOP('',(#83964,#83965,#83966,#83967));
#18560=EDGE_LOOP('',(#83968,#83969,#83970,#83971));
#18561=EDGE_LOOP('',(#83972,#83973,#83974,#83975));
#18562=EDGE_LOOP('',(#83976,#83977,#83978,#83979,#83980));
#18563=EDGE_LOOP('',(#83981,#83982,#83983,#83984));
#18564=EDGE_LOOP('',(#83985,#83986,#83987,#83988));
#18565=EDGE_LOOP('',(#83989,#83990,#83991,#83992));
#18566=EDGE_LOOP('',(#83993,#83994,#83995,#83996));
#18567=EDGE_LOOP('',(#83997,#83998,#83999,#84000));
#18568=EDGE_LOOP('',(#84001,#84002,#84003,#84004));
#18569=EDGE_LOOP('',(#84005,#84006,#84007,#84008));
#18570=EDGE_LOOP('',(#84009,#84010,#84011,#84012));
#18571=EDGE_LOOP('',(#84013,#84014,#84015,#84016));
#18572=EDGE_LOOP('',(#84017,#84018,#84019,#84020));
#18573=EDGE_LOOP('',(#84021,#84022,#84023,#84024,#84025));
#18574=EDGE_LOOP('',(#84026,#84027,#84028,#84029));
#18575=EDGE_LOOP('',(#84030,#84031,#84032,#84033));
#18576=EDGE_LOOP('',(#84034,#84035,#84036,#84037));
#18577=EDGE_LOOP('',(#84038,#84039,#84040,#84041));
#18578=EDGE_LOOP('',(#84042,#84043,#84044,#84045));
#18579=EDGE_LOOP('',(#84046,#84047,#84048,#84049));
#18580=EDGE_LOOP('',(#84050,#84051,#84052,#84053));
#18581=EDGE_LOOP('',(#84054,#84055,#84056,#84057));
#18582=EDGE_LOOP('',(#84058,#84059,#84060,#84061,#84062));
#18583=EDGE_LOOP('',(#84063,#84064,#84065,#84066));
#18584=EDGE_LOOP('',(#84067,#84068,#84069,#84070));
#18585=EDGE_LOOP('',(#84071,#84072,#84073,#84074,#84075));
#18586=EDGE_LOOP('',(#84076,#84077,#84078,#84079));
#18587=EDGE_LOOP('',(#84080,#84081,#84082,#84083));
#18588=EDGE_LOOP('',(#84084,#84085,#84086,#84087));
#18589=EDGE_LOOP('',(#84088,#84089,#84090,#84091));
#18590=EDGE_LOOP('',(#84092,#84093,#84094,#84095,#84096));
#18591=EDGE_LOOP('',(#84097,#84098,#84099,#84100));
#18592=EDGE_LOOP('',(#84101,#84102,#84103,#84104));
#18593=EDGE_LOOP('',(#84105,#84106,#84107,#84108));
#18594=EDGE_LOOP('',(#84109,#84110,#84111,#84112));
#18595=EDGE_LOOP('',(#84113,#84114,#84115,#84116));
#18596=EDGE_LOOP('',(#84117,#84118,#84119,#84120));
#18597=EDGE_LOOP('',(#84121,#84122,#84123,#84124));
#18598=EDGE_LOOP('',(#84125,#84126,#84127,#84128));
#18599=EDGE_LOOP('',(#84129,#84130,#84131,#84132,#84133));
#18600=EDGE_LOOP('',(#84134,#84135,#84136,#84137));
#18601=EDGE_LOOP('',(#84138,#84139,#84140,#84141));
#18602=EDGE_LOOP('',(#84142,#84143,#84144,#84145));
#18603=EDGE_LOOP('',(#84146,#84147,#84148,#84149));
#18604=EDGE_LOOP('',(#84150,#84151,#84152,#84153));
#18605=EDGE_LOOP('',(#84154,#84155,#84156,#84157));
#18606=EDGE_LOOP('',(#84158,#84159,#84160,#84161));
#18607=EDGE_LOOP('',(#84162,#84163,#84164,#84165));
#18608=EDGE_LOOP('',(#84166,#84167,#84168,#84169,#84170));
#18609=EDGE_LOOP('',(#84171,#84172,#84173,#84174));
#18610=EDGE_LOOP('',(#84175,#84176,#84177,#84178));
#18611=EDGE_LOOP('',(#84179,#84180,#84181,#84182,#84183));
#18612=EDGE_LOOP('',(#84184,#84185,#84186,#84187));
#18613=EDGE_LOOP('',(#84188,#84189,#84190,#84191));
#18614=EDGE_LOOP('',(#84192,#84193,#84194,#84195));
#18615=EDGE_LOOP('',(#84196,#84197,#84198,#84199));
#18616=EDGE_LOOP('',(#84200,#84201,#84202,#84203,#84204));
#18617=EDGE_LOOP('',(#84205,#84206,#84207,#84208));
#18618=EDGE_LOOP('',(#84209,#84210,#84211,#84212));
#18619=EDGE_LOOP('',(#84213,#84214,#84215,#84216));
#18620=EDGE_LOOP('',(#84217,#84218,#84219,#84220));
#18621=EDGE_LOOP('',(#84221,#84222,#84223,#84224));
#18622=EDGE_LOOP('',(#84225,#84226,#84227,#84228));
#18623=EDGE_LOOP('',(#84229,#84230,#84231,#84232));
#18624=EDGE_LOOP('',(#84233,#84234,#84235,#84236));
#18625=EDGE_LOOP('',(#84237,#84238,#84239,#84240));
#18626=EDGE_LOOP('',(#84241,#84242,#84243,#84244));
#18627=EDGE_LOOP('',(#84245,#84246,#84247,#84248,#84249));
#18628=EDGE_LOOP('',(#84250,#84251,#84252,#84253));
#18629=EDGE_LOOP('',(#84254,#84255,#84256,#84257));
#18630=EDGE_LOOP('',(#84258,#84259,#84260,#84261));
#18631=EDGE_LOOP('',(#84262,#84263,#84264,#84265));
#18632=EDGE_LOOP('',(#84266,#84267,#84268,#84269));
#18633=EDGE_LOOP('',(#84270,#84271,#84272,#84273));
#18634=EDGE_LOOP('',(#84274,#84275,#84276,#84277));
#18635=EDGE_LOOP('',(#84278,#84279,#84280,#84281));
#18636=EDGE_LOOP('',(#84282,#84283,#84284,#84285,#84286));
#18637=EDGE_LOOP('',(#84287,#84288,#84289,#84290));
#18638=EDGE_LOOP('',(#84291,#84292,#84293,#84294));
#18639=EDGE_LOOP('',(#84295,#84296,#84297,#84298,#84299));
#18640=EDGE_LOOP('',(#84300,#84301,#84302,#84303));
#18641=EDGE_LOOP('',(#84304,#84305,#84306,#84307));
#18642=EDGE_LOOP('',(#84308,#84309,#84310,#84311));
#18643=EDGE_LOOP('',(#84312,#84313,#84314,#84315));
#18644=EDGE_LOOP('',(#84316,#84317,#84318,#84319,#84320));
#18645=EDGE_LOOP('',(#84321,#84322,#84323,#84324));
#18646=EDGE_LOOP('',(#84325,#84326,#84327,#84328));
#18647=EDGE_LOOP('',(#84329,#84330,#84331,#84332));
#18648=EDGE_LOOP('',(#84333,#84334,#84335,#84336));
#18649=EDGE_LOOP('',(#84337,#84338,#84339,#84340));
#18650=EDGE_LOOP('',(#84341,#84342,#84343,#84344));
#18651=EDGE_LOOP('',(#84345,#84346,#84347,#84348));
#18652=EDGE_LOOP('',(#84349,#84350,#84351,#84352));
#18653=EDGE_LOOP('',(#84353,#84354,#84355,#84356));
#18654=EDGE_LOOP('',(#84357,#84358,#84359,#84360));
#18655=EDGE_LOOP('',(#84361,#84362,#84363,#84364,#84365));
#18656=EDGE_LOOP('',(#84366,#84367,#84368,#84369));
#18657=EDGE_LOOP('',(#84370,#84371,#84372,#84373));
#18658=EDGE_LOOP('',(#84374,#84375,#84376,#84377));
#18659=EDGE_LOOP('',(#84378,#84379,#84380,#84381));
#18660=EDGE_LOOP('',(#84382,#84383,#84384,#84385));
#18661=EDGE_LOOP('',(#84386,#84387,#84388,#84389));
#18662=EDGE_LOOP('',(#84390,#84391,#84392,#84393));
#18663=EDGE_LOOP('',(#84394,#84395,#84396,#84397));
#18664=EDGE_LOOP('',(#84398,#84399,#84400,#84401,#84402));
#18665=EDGE_LOOP('',(#84403,#84404,#84405,#84406));
#18666=EDGE_LOOP('',(#84407,#84408,#84409,#84410));
#18667=EDGE_LOOP('',(#84411,#84412,#84413,#84414,#84415));
#18668=EDGE_LOOP('',(#84416,#84417,#84418,#84419));
#18669=EDGE_LOOP('',(#84420,#84421,#84422,#84423));
#18670=EDGE_LOOP('',(#84424,#84425,#84426,#84427));
#18671=EDGE_LOOP('',(#84428,#84429,#84430,#84431));
#18672=EDGE_LOOP('',(#84432,#84433,#84434,#84435,#84436));
#18673=EDGE_LOOP('',(#84437,#84438,#84439,#84440));
#18674=EDGE_LOOP('',(#84441,#84442,#84443,#84444));
#18675=EDGE_LOOP('',(#84445,#84446,#84447,#84448));
#18676=EDGE_LOOP('',(#84449,#84450,#84451,#84452));
#18677=EDGE_LOOP('',(#84453,#84454,#84455,#84456));
#18678=EDGE_LOOP('',(#84457,#84458,#84459,#84460));
#18679=EDGE_LOOP('',(#84461,#84462,#84463,#84464));
#18680=EDGE_LOOP('',(#84465,#84466,#84467,#84468));
#18681=EDGE_LOOP('',(#84469,#84470,#84471,#84472));
#18682=EDGE_LOOP('',(#84473,#84474,#84475,#84476));
#18683=EDGE_LOOP('',(#84477,#84478,#84479,#84480,#84481));
#18684=EDGE_LOOP('',(#84482,#84483,#84484,#84485));
#18685=EDGE_LOOP('',(#84486,#84487,#84488,#84489));
#18686=EDGE_LOOP('',(#84490,#84491,#84492,#84493));
#18687=EDGE_LOOP('',(#84494,#84495,#84496,#84497));
#18688=EDGE_LOOP('',(#84498,#84499,#84500,#84501));
#18689=EDGE_LOOP('',(#84502,#84503,#84504,#84505));
#18690=EDGE_LOOP('',(#84506,#84507,#84508,#84509));
#18691=EDGE_LOOP('',(#84510,#84511,#84512,#84513));
#18692=EDGE_LOOP('',(#84514,#84515,#84516,#84517,#84518));
#18693=EDGE_LOOP('',(#84519,#84520,#84521,#84522));
#18694=EDGE_LOOP('',(#84523,#84524,#84525,#84526));
#18695=EDGE_LOOP('',(#84527,#84528,#84529,#84530,#84531));
#18696=EDGE_LOOP('',(#84532,#84533,#84534,#84535));
#18697=EDGE_LOOP('',(#84536,#84537,#84538,#84539));
#18698=EDGE_LOOP('',(#84540,#84541,#84542,#84543));
#18699=EDGE_LOOP('',(#84544,#84545,#84546,#84547));
#18700=EDGE_LOOP('',(#84548,#84549,#84550,#84551,#84552));
#18701=EDGE_LOOP('',(#84553,#84554,#84555,#84556));
#18702=EDGE_LOOP('',(#84557,#84558,#84559,#84560));
#18703=EDGE_LOOP('',(#84561,#84562,#84563,#84564));
#18704=EDGE_LOOP('',(#84565,#84566,#84567,#84568));
#18705=EDGE_LOOP('',(#84569,#84570,#84571,#84572));
#18706=EDGE_LOOP('',(#84573,#84574,#84575,#84576));
#18707=EDGE_LOOP('',(#84577,#84578,#84579,#84580));
#18708=EDGE_LOOP('',(#84581,#84582,#84583,#84584));
#18709=EDGE_LOOP('',(#84585,#84586,#84587,#84588));
#18710=EDGE_LOOP('',(#84589,#84590,#84591,#84592));
#18711=EDGE_LOOP('',(#84593,#84594,#84595,#84596,#84597));
#18712=EDGE_LOOP('',(#84598,#84599,#84600,#84601));
#18713=EDGE_LOOP('',(#84602,#84603,#84604,#84605));
#18714=EDGE_LOOP('',(#84606,#84607,#84608,#84609));
#18715=EDGE_LOOP('',(#84610,#84611,#84612,#84613));
#18716=EDGE_LOOP('',(#84614,#84615,#84616,#84617));
#18717=EDGE_LOOP('',(#84618,#84619,#84620,#84621));
#18718=EDGE_LOOP('',(#84622,#84623,#84624,#84625));
#18719=EDGE_LOOP('',(#84626,#84627,#84628,#84629));
#18720=EDGE_LOOP('',(#84630,#84631,#84632,#84633,#84634));
#18721=EDGE_LOOP('',(#84635,#84636,#84637,#84638));
#18722=EDGE_LOOP('',(#84639,#84640,#84641,#84642));
#18723=EDGE_LOOP('',(#84643,#84644,#84645,#84646,#84647));
#18724=EDGE_LOOP('',(#84648,#84649,#84650,#84651));
#18725=EDGE_LOOP('',(#84652,#84653,#84654,#84655));
#18726=EDGE_LOOP('',(#84656,#84657,#84658,#84659));
#18727=EDGE_LOOP('',(#84660,#84661,#84662,#84663));
#18728=EDGE_LOOP('',(#84664,#84665,#84666,#84667,#84668));
#18729=EDGE_LOOP('',(#84669,#84670,#84671,#84672));
#18730=EDGE_LOOP('',(#84673,#84674,#84675,#84676));
#18731=EDGE_LOOP('',(#84677,#84678,#84679,#84680));
#18732=EDGE_LOOP('',(#84681,#84682,#84683,#84684));
#18733=EDGE_LOOP('',(#84685,#84686,#84687,#84688));
#18734=EDGE_LOOP('',(#84689,#84690,#84691,#84692));
#18735=EDGE_LOOP('',(#84693,#84694,#84695,#84696));
#18736=EDGE_LOOP('',(#84697,#84698,#84699,#84700));
#18737=EDGE_LOOP('',(#84701,#84702,#84703,#84704));
#18738=EDGE_LOOP('',(#84705,#84706,#84707,#84708));
#18739=EDGE_LOOP('',(#84709,#84710,#84711,#84712,#84713));
#18740=EDGE_LOOP('',(#84714,#84715,#84716,#84717));
#18741=EDGE_LOOP('',(#84718,#84719,#84720,#84721));
#18742=EDGE_LOOP('',(#84722,#84723,#84724,#84725));
#18743=EDGE_LOOP('',(#84726,#84727,#84728,#84729));
#18744=EDGE_LOOP('',(#84730,#84731,#84732,#84733));
#18745=EDGE_LOOP('',(#84734,#84735,#84736,#84737));
#18746=EDGE_LOOP('',(#84738,#84739,#84740,#84741));
#18747=EDGE_LOOP('',(#84742,#84743,#84744,#84745));
#18748=EDGE_LOOP('',(#84746,#84747,#84748,#84749,#84750));
#18749=EDGE_LOOP('',(#84751,#84752,#84753,#84754));
#18750=EDGE_LOOP('',(#84755,#84756,#84757,#84758));
#18751=EDGE_LOOP('',(#84759,#84760,#84761,#84762,#84763));
#18752=EDGE_LOOP('',(#84764,#84765,#84766,#84767));
#18753=EDGE_LOOP('',(#84768,#84769,#84770,#84771));
#18754=EDGE_LOOP('',(#84772,#84773,#84774,#84775));
#18755=EDGE_LOOP('',(#84776,#84777,#84778,#84779));
#18756=EDGE_LOOP('',(#84780,#84781,#84782,#84783,#84784));
#18757=EDGE_LOOP('',(#84785,#84786,#84787,#84788));
#18758=EDGE_LOOP('',(#84789,#84790,#84791,#84792));
#18759=EDGE_LOOP('',(#84793,#84794,#84795,#84796));
#18760=EDGE_LOOP('',(#84797,#84798,#84799,#84800));
#18761=EDGE_LOOP('',(#84801,#84802,#84803,#84804));
#18762=EDGE_LOOP('',(#84805,#84806,#84807,#84808));
#18763=EDGE_LOOP('',(#84809,#84810,#84811,#84812));
#18764=EDGE_LOOP('',(#84813,#84814,#84815,#84816));
#18765=EDGE_LOOP('',(#84817,#84818,#84819,#84820));
#18766=EDGE_LOOP('',(#84821,#84822,#84823,#84824));
#18767=EDGE_LOOP('',(#84825,#84826,#84827,#84828,#84829));
#18768=EDGE_LOOP('',(#84830,#84831,#84832,#84833));
#18769=EDGE_LOOP('',(#84834,#84835,#84836,#84837));
#18770=EDGE_LOOP('',(#84838,#84839,#84840,#84841));
#18771=EDGE_LOOP('',(#84842,#84843,#84844,#84845));
#18772=EDGE_LOOP('',(#84846,#84847,#84848,#84849));
#18773=EDGE_LOOP('',(#84850,#84851,#84852,#84853));
#18774=EDGE_LOOP('',(#84854,#84855,#84856,#84857));
#18775=EDGE_LOOP('',(#84858,#84859,#84860,#84861));
#18776=EDGE_LOOP('',(#84862,#84863,#84864,#84865,#84866));
#18777=EDGE_LOOP('',(#84867,#84868,#84869,#84870));
#18778=EDGE_LOOP('',(#84871,#84872,#84873,#84874));
#18779=EDGE_LOOP('',(#84875,#84876,#84877,#84878,#84879));
#18780=EDGE_LOOP('',(#84880,#84881,#84882,#84883));
#18781=EDGE_LOOP('',(#84884,#84885,#84886,#84887));
#18782=EDGE_LOOP('',(#84888,#84889,#84890,#84891));
#18783=EDGE_LOOP('',(#84892,#84893,#84894,#84895));
#18784=EDGE_LOOP('',(#84896,#84897,#84898,#84899,#84900));
#18785=EDGE_LOOP('',(#84901,#84902,#84903,#84904));
#18786=EDGE_LOOP('',(#84905,#84906,#84907,#84908));
#18787=EDGE_LOOP('',(#84909,#84910,#84911,#84912));
#18788=EDGE_LOOP('',(#84913,#84914,#84915,#84916));
#18789=EDGE_LOOP('',(#84917,#84918,#84919,#84920));
#18790=EDGE_LOOP('',(#84921,#84922,#84923,#84924));
#18791=EDGE_LOOP('',(#84925,#84926,#84927,#84928));
#18792=EDGE_LOOP('',(#84929,#84930,#84931,#84932));
#18793=EDGE_LOOP('',(#84933,#84934,#84935,#84936));
#18794=EDGE_LOOP('',(#84937,#84938,#84939,#84940));
#18795=EDGE_LOOP('',(#84941,#84942,#84943,#84944,#84945));
#18796=EDGE_LOOP('',(#84946,#84947,#84948,#84949));
#18797=EDGE_LOOP('',(#84950,#84951,#84952,#84953));
#18798=EDGE_LOOP('',(#84954,#84955,#84956,#84957));
#18799=EDGE_LOOP('',(#84958,#84959,#84960,#84961));
#18800=EDGE_LOOP('',(#84962,#84963,#84964,#84965));
#18801=EDGE_LOOP('',(#84966,#84967,#84968,#84969));
#18802=EDGE_LOOP('',(#84970,#84971,#84972,#84973));
#18803=EDGE_LOOP('',(#84974,#84975,#84976,#84977));
#18804=EDGE_LOOP('',(#84978,#84979,#84980,#84981,#84982));
#18805=EDGE_LOOP('',(#84983,#84984,#84985,#84986));
#18806=EDGE_LOOP('',(#84987,#84988,#84989,#84990));
#18807=EDGE_LOOP('',(#84991,#84992,#84993,#84994,#84995));
#18808=EDGE_LOOP('',(#84996,#84997,#84998,#84999));
#18809=EDGE_LOOP('',(#85000,#85001,#85002,#85003));
#18810=EDGE_LOOP('',(#85004,#85005,#85006,#85007));
#18811=EDGE_LOOP('',(#85008,#85009,#85010,#85011));
#18812=EDGE_LOOP('',(#85012,#85013,#85014,#85015,#85016));
#18813=EDGE_LOOP('',(#85017,#85018,#85019,#85020));
#18814=EDGE_LOOP('',(#85021,#85022,#85023,#85024));
#18815=EDGE_LOOP('',(#85025,#85026,#85027,#85028));
#18816=EDGE_LOOP('',(#85029,#85030,#85031,#85032));
#18817=EDGE_LOOP('',(#85033,#85034,#85035,#85036));
#18818=EDGE_LOOP('',(#85037,#85038,#85039,#85040));
#18819=EDGE_LOOP('',(#85041,#85042,#85043,#85044));
#18820=EDGE_LOOP('',(#85045,#85046,#85047,#85048));
#18821=EDGE_LOOP('',(#85049,#85050,#85051,#85052));
#18822=EDGE_LOOP('',(#85053,#85054,#85055,#85056));
#18823=EDGE_LOOP('',(#85057,#85058,#85059,#85060,#85061));
#18824=EDGE_LOOP('',(#85062,#85063,#85064,#85065));
#18825=EDGE_LOOP('',(#85066,#85067,#85068,#85069));
#18826=EDGE_LOOP('',(#85070,#85071,#85072,#85073));
#18827=EDGE_LOOP('',(#85074,#85075,#85076,#85077));
#18828=EDGE_LOOP('',(#85078,#85079,#85080,#85081));
#18829=EDGE_LOOP('',(#85082,#85083,#85084,#85085));
#18830=EDGE_LOOP('',(#85086,#85087,#85088,#85089));
#18831=EDGE_LOOP('',(#85090,#85091,#85092,#85093));
#18832=EDGE_LOOP('',(#85094,#85095,#85096,#85097,#85098));
#18833=EDGE_LOOP('',(#85099,#85100,#85101,#85102));
#18834=EDGE_LOOP('',(#85103,#85104,#85105,#85106));
#18835=EDGE_LOOP('',(#85107,#85108,#85109,#85110,#85111));
#18836=EDGE_LOOP('',(#85112,#85113,#85114,#85115));
#18837=EDGE_LOOP('',(#85116,#85117,#85118,#85119));
#18838=EDGE_LOOP('',(#85120,#85121,#85122,#85123));
#18839=EDGE_LOOP('',(#85124,#85125,#85126,#85127));
#18840=EDGE_LOOP('',(#85128,#85129,#85130,#85131,#85132));
#18841=EDGE_LOOP('',(#85133,#85134,#85135,#85136));
#18842=EDGE_LOOP('',(#85137,#85138,#85139,#85140));
#18843=EDGE_LOOP('',(#85141,#85142,#85143,#85144));
#18844=EDGE_LOOP('',(#85145,#85146,#85147,#85148));
#18845=EDGE_LOOP('',(#85149,#85150,#85151,#85152));
#18846=EDGE_LOOP('',(#85153,#85154,#85155,#85156));
#18847=EDGE_LOOP('',(#85157,#85158,#85159,#85160));
#18848=EDGE_LOOP('',(#85161,#85162,#85163,#85164));
#18849=EDGE_LOOP('',(#85165,#85166,#85167,#85168));
#18850=EDGE_LOOP('',(#85169,#85170,#85171,#85172));
#18851=EDGE_LOOP('',(#85173,#85174,#85175,#85176,#85177));
#18852=EDGE_LOOP('',(#85178,#85179,#85180,#85181));
#18853=EDGE_LOOP('',(#85182,#85183,#85184,#85185));
#18854=EDGE_LOOP('',(#85186,#85187,#85188,#85189));
#18855=EDGE_LOOP('',(#85190,#85191,#85192,#85193));
#18856=EDGE_LOOP('',(#85194,#85195,#85196,#85197));
#18857=EDGE_LOOP('',(#85198,#85199,#85200,#85201));
#18858=EDGE_LOOP('',(#85202,#85203,#85204,#85205));
#18859=EDGE_LOOP('',(#85206,#85207,#85208,#85209));
#18860=EDGE_LOOP('',(#85210,#85211,#85212,#85213,#85214));
#18861=EDGE_LOOP('',(#85215,#85216,#85217,#85218));
#18862=EDGE_LOOP('',(#85219,#85220,#85221,#85222));
#18863=EDGE_LOOP('',(#85223,#85224,#85225,#85226,#85227));
#18864=EDGE_LOOP('',(#85228,#85229,#85230,#85231));
#18865=EDGE_LOOP('',(#85232,#85233,#85234,#85235));
#18866=EDGE_LOOP('',(#85236,#85237,#85238,#85239));
#18867=EDGE_LOOP('',(#85240,#85241,#85242,#85243));
#18868=EDGE_LOOP('',(#85244,#85245,#85246,#85247,#85248));
#18869=EDGE_LOOP('',(#85249,#85250,#85251,#85252));
#18870=EDGE_LOOP('',(#85253,#85254,#85255,#85256));
#18871=EDGE_LOOP('',(#85257,#85258,#85259,#85260));
#18872=EDGE_LOOP('',(#85261,#85262,#85263,#85264));
#18873=EDGE_LOOP('',(#85265,#85266,#85267,#85268));
#18874=EDGE_LOOP('',(#85269,#85270,#85271,#85272));
#18875=EDGE_LOOP('',(#85273,#85274,#85275,#85276));
#18876=EDGE_LOOP('',(#85277,#85278,#85279,#85280));
#18877=EDGE_LOOP('',(#85281,#85282,#85283,#85284));
#18878=EDGE_LOOP('',(#85285,#85286,#85287,#85288));
#18879=EDGE_LOOP('',(#85289,#85290,#85291,#85292,#85293));
#18880=EDGE_LOOP('',(#85294,#85295,#85296,#85297));
#18881=EDGE_LOOP('',(#85298,#85299,#85300,#85301));
#18882=EDGE_LOOP('',(#85302,#85303,#85304,#85305));
#18883=EDGE_LOOP('',(#85306,#85307,#85308,#85309));
#18884=EDGE_LOOP('',(#85310,#85311,#85312,#85313));
#18885=EDGE_LOOP('',(#85314,#85315,#85316,#85317));
#18886=EDGE_LOOP('',(#85318,#85319,#85320,#85321));
#18887=EDGE_LOOP('',(#85322,#85323,#85324,#85325));
#18888=EDGE_LOOP('',(#85326,#85327,#85328,#85329,#85330));
#18889=EDGE_LOOP('',(#85331,#85332,#85333,#85334));
#18890=EDGE_LOOP('',(#85335,#85336,#85337,#85338));
#18891=EDGE_LOOP('',(#85339,#85340,#85341,#85342,#85343));
#18892=EDGE_LOOP('',(#85344,#85345,#85346,#85347));
#18893=EDGE_LOOP('',(#85348,#85349,#85350,#85351));
#18894=EDGE_LOOP('',(#85352,#85353,#85354,#85355));
#18895=EDGE_LOOP('',(#85356,#85357,#85358,#85359));
#18896=EDGE_LOOP('',(#85360,#85361,#85362,#85363,#85364));
#18897=EDGE_LOOP('',(#85365,#85366,#85367,#85368));
#18898=EDGE_LOOP('',(#85369,#85370,#85371,#85372));
#18899=EDGE_LOOP('',(#85373,#85374,#85375,#85376));
#18900=EDGE_LOOP('',(#85377,#85378,#85379,#85380));
#18901=EDGE_LOOP('',(#85381,#85382,#85383,#85384));
#18902=EDGE_LOOP('',(#85385,#85386,#85387,#85388));
#18903=EDGE_LOOP('',(#85389,#85390,#85391,#85392));
#18904=EDGE_LOOP('',(#85393,#85394,#85395,#85396));
#18905=EDGE_LOOP('',(#85397,#85398,#85399,#85400));
#18906=EDGE_LOOP('',(#85401,#85402,#85403,#85404));
#18907=EDGE_LOOP('',(#85405,#85406,#85407,#85408,#85409));
#18908=EDGE_LOOP('',(#85410,#85411,#85412,#85413));
#18909=EDGE_LOOP('',(#85414,#85415,#85416,#85417));
#18910=EDGE_LOOP('',(#85418,#85419,#85420,#85421));
#18911=EDGE_LOOP('',(#85422,#85423,#85424,#85425));
#18912=EDGE_LOOP('',(#85426,#85427,#85428,#85429));
#18913=EDGE_LOOP('',(#85430,#85431,#85432,#85433));
#18914=EDGE_LOOP('',(#85434,#85435,#85436,#85437));
#18915=EDGE_LOOP('',(#85438,#85439,#85440,#85441));
#18916=EDGE_LOOP('',(#85442,#85443,#85444,#85445,#85446));
#18917=EDGE_LOOP('',(#85447,#85448,#85449,#85450));
#18918=EDGE_LOOP('',(#85451,#85452,#85453,#85454));
#18919=EDGE_LOOP('',(#85455,#85456,#85457,#85458,#85459));
#18920=EDGE_LOOP('',(#85460,#85461,#85462,#85463));
#18921=EDGE_LOOP('',(#85464,#85465,#85466,#85467));
#18922=EDGE_LOOP('',(#85468,#85469,#85470,#85471));
#18923=EDGE_LOOP('',(#85472,#85473,#85474,#85475));
#18924=EDGE_LOOP('',(#85476,#85477,#85478,#85479,#85480));
#18925=EDGE_LOOP('',(#85481,#85482,#85483,#85484));
#18926=EDGE_LOOP('',(#85485,#85486,#85487,#85488));
#18927=EDGE_LOOP('',(#85489,#85490,#85491,#85492));
#18928=EDGE_LOOP('',(#85493,#85494,#85495,#85496));
#18929=EDGE_LOOP('',(#85497,#85498,#85499,#85500));
#18930=EDGE_LOOP('',(#85501,#85502,#85503,#85504));
#18931=EDGE_LOOP('',(#85505,#85506,#85507,#85508));
#18932=EDGE_LOOP('',(#85509,#85510,#85511,#85512));
#18933=EDGE_LOOP('',(#85513,#85514,#85515,#85516));
#18934=EDGE_LOOP('',(#85517,#85518,#85519,#85520));
#18935=EDGE_LOOP('',(#85521,#85522,#85523,#85524,#85525));
#18936=EDGE_LOOP('',(#85526,#85527,#85528,#85529));
#18937=EDGE_LOOP('',(#85530,#85531,#85532,#85533));
#18938=EDGE_LOOP('',(#85534,#85535,#85536,#85537));
#18939=EDGE_LOOP('',(#85538,#85539,#85540,#85541));
#18940=EDGE_LOOP('',(#85542,#85543,#85544,#85545));
#18941=EDGE_LOOP('',(#85546,#85547,#85548,#85549));
#18942=EDGE_LOOP('',(#85550,#85551,#85552,#85553));
#18943=EDGE_LOOP('',(#85554,#85555,#85556,#85557));
#18944=EDGE_LOOP('',(#85558,#85559,#85560,#85561,#85562));
#18945=EDGE_LOOP('',(#85563,#85564,#85565,#85566));
#18946=EDGE_LOOP('',(#85567,#85568,#85569,#85570));
#18947=EDGE_LOOP('',(#85571,#85572,#85573,#85574,#85575));
#18948=EDGE_LOOP('',(#85576,#85577,#85578,#85579));
#18949=EDGE_LOOP('',(#85580,#85581,#85582,#85583));
#18950=EDGE_LOOP('',(#85584,#85585,#85586,#85587));
#18951=EDGE_LOOP('',(#85588,#85589,#85590,#85591));
#18952=EDGE_LOOP('',(#85592,#85593,#85594,#85595,#85596));
#18953=EDGE_LOOP('',(#85597,#85598,#85599,#85600));
#18954=EDGE_LOOP('',(#85601,#85602,#85603,#85604));
#18955=EDGE_LOOP('',(#85605,#85606,#85607,#85608));
#18956=EDGE_LOOP('',(#85609,#85610,#85611,#85612));
#18957=EDGE_LOOP('',(#85613,#85614,#85615,#85616));
#18958=EDGE_LOOP('',(#85617,#85618,#85619,#85620));
#18959=EDGE_LOOP('',(#85621,#85622,#85623,#85624));
#18960=EDGE_LOOP('',(#85625,#85626,#85627,#85628));
#18961=EDGE_LOOP('',(#85629,#85630,#85631,#85632));
#18962=EDGE_LOOP('',(#85633,#85634,#85635,#85636));
#18963=EDGE_LOOP('',(#85637,#85638,#85639,#85640,#85641));
#18964=EDGE_LOOP('',(#85642,#85643,#85644,#85645));
#18965=EDGE_LOOP('',(#85646,#85647,#85648,#85649));
#18966=EDGE_LOOP('',(#85650,#85651,#85652,#85653));
#18967=EDGE_LOOP('',(#85654,#85655,#85656,#85657));
#18968=EDGE_LOOP('',(#85658,#85659,#85660,#85661));
#18969=EDGE_LOOP('',(#85662,#85663,#85664,#85665));
#18970=EDGE_LOOP('',(#85666,#85667,#85668,#85669));
#18971=EDGE_LOOP('',(#85670,#85671,#85672,#85673));
#18972=EDGE_LOOP('',(#85674,#85675,#85676,#85677,#85678));
#18973=EDGE_LOOP('',(#85679,#85680,#85681,#85682));
#18974=EDGE_LOOP('',(#85683,#85684,#85685,#85686));
#18975=EDGE_LOOP('',(#85687,#85688,#85689,#85690,#85691));
#18976=EDGE_LOOP('',(#85692,#85693,#85694,#85695));
#18977=EDGE_LOOP('',(#85696,#85697,#85698,#85699));
#18978=EDGE_LOOP('',(#85700,#85701,#85702,#85703));
#18979=EDGE_LOOP('',(#85704,#85705,#85706,#85707));
#18980=EDGE_LOOP('',(#85708,#85709,#85710,#85711,#85712));
#18981=EDGE_LOOP('',(#85713,#85714,#85715,#85716));
#18982=EDGE_LOOP('',(#85717,#85718,#85719,#85720));
#18983=EDGE_LOOP('',(#85721,#85722,#85723,#85724));
#18984=EDGE_LOOP('',(#85725,#85726,#85727,#85728));
#18985=EDGE_LOOP('',(#85729,#85730,#85731,#85732));
#18986=EDGE_LOOP('',(#85733,#85734,#85735,#85736));
#18987=EDGE_LOOP('',(#85737,#85738,#85739,#85740));
#18988=EDGE_LOOP('',(#85741,#85742,#85743,#85744));
#18989=EDGE_LOOP('',(#85745,#85746,#85747,#85748));
#18990=EDGE_LOOP('',(#85749,#85750,#85751,#85752));
#18991=EDGE_LOOP('',(#85753,#85754,#85755,#85756,#85757));
#18992=EDGE_LOOP('',(#85758,#85759,#85760,#85761));
#18993=EDGE_LOOP('',(#85762,#85763,#85764,#85765));
#18994=EDGE_LOOP('',(#85766,#85767,#85768,#85769));
#18995=EDGE_LOOP('',(#85770,#85771,#85772,#85773));
#18996=EDGE_LOOP('',(#85774,#85775,#85776,#85777));
#18997=EDGE_LOOP('',(#85778,#85779,#85780,#85781));
#18998=EDGE_LOOP('',(#85782,#85783,#85784,#85785));
#18999=EDGE_LOOP('',(#85786,#85787,#85788,#85789));
#19000=EDGE_LOOP('',(#85790,#85791,#85792,#85793,#85794));
#19001=EDGE_LOOP('',(#85795,#85796,#85797,#85798));
#19002=EDGE_LOOP('',(#85799,#85800,#85801,#85802));
#19003=EDGE_LOOP('',(#85803,#85804,#85805,#85806,#85807));
#19004=EDGE_LOOP('',(#85808,#85809,#85810,#85811));
#19005=EDGE_LOOP('',(#85812,#85813,#85814,#85815,#85816));
#19006=EDGE_LOOP('',(#85817,#85818,#85819,#85820));
#19007=EDGE_LOOP('',(#85821));
#19008=EDGE_LOOP('',(#85822));
#19009=EDGE_LOOP('',(#85823));
#19010=EDGE_LOOP('',(#85824));
#19011=EDGE_LOOP('',(#85825));
#19012=EDGE_LOOP('',(#85826));
#19013=EDGE_LOOP('',(#85827,#85828,#85829,#85830));
#19014=EDGE_LOOP('',(#85831,#85832,#85833,#85834));
#19015=EDGE_LOOP('',(#85835,#85836,#85837,#85838));
#19016=EDGE_LOOP('',(#85839,#85840,#85841,#85842));
#19017=EDGE_LOOP('',(#85843));
#19018=EDGE_LOOP('',(#85844));
#19019=EDGE_LOOP('',(#85845));
#19020=EDGE_LOOP('',(#85846));
#19021=EDGE_LOOP('',(#85847,#85848,#85849,#85850));
#19022=EDGE_LOOP('',(#85851,#85852,#85853,#85854));
#19023=EDGE_LOOP('',(#85855,#85856,#85857,#85858));
#19024=EDGE_LOOP('',(#85859,#85860,#85861,#85862));
#19025=EDGE_LOOP('',(#85863,#85864,#85865,#85866));
#19026=EDGE_LOOP('',(#85867,#85868,#85869,#85870));
#19027=EDGE_LOOP('',(#85871,#85872,#85873,#85874));
#19028=EDGE_LOOP('',(#85875,#85876,#85877,#85878));
#19029=EDGE_LOOP('',(#85879,#85880,#85881,#85882));
#19030=EDGE_LOOP('',(#85883,#85884,#85885,#85886,#85887,#85888));
#19031=EDGE_LOOP('',(#85889,#85890,#85891,#85892,#85893,#85894));
#19032=EDGE_LOOP('',(#85895,#85896,#85897,#85898));
#19033=EDGE_LOOP('',(#85899,#85900,#85901,#85902));
#19034=EDGE_LOOP('',(#85903,#85904,#85905,#85906));
#19035=EDGE_LOOP('',(#85907,#85908,#85909,#85910));
#19036=EDGE_LOOP('',(#85911,#85912,#85913,#85914));
#19037=EDGE_LOOP('',(#85915,#85916,#85917,#85918));
#19038=EDGE_LOOP('',(#85919,#85920,#85921,#85922));
#19039=EDGE_LOOP('',(#85923,#85924,#85925,#85926,#85927,#85928,#85929,#85930,
#85931,#85932,#85933,#85934,#85935,#85936,#85937,#85938,#85939,#85940,#85941,
#85942,#85943,#85944,#85945,#85946,#85947,#85948,#85949,#85950));
#19040=EDGE_LOOP('',(#85951,#85952,#85953,#85954,#85955,#85956,#85957,#85958,
#85959,#85960));
#19041=EDGE_LOOP('',(#85961,#85962,#85963,#85964,#85965,#85966,#85967,#85968,
#85969,#85970));
#19042=EDGE_LOOP('',(#85971,#85972,#85973,#85974));
#19043=EDGE_LOOP('',(#85975,#85976,#85977,#85978));
#19044=EDGE_LOOP('',(#85979,#85980,#85981,#85982));
#19045=EDGE_LOOP('',(#85983,#85984,#85985,#85986,#85987,#85988,#85989,#85990,
#85991,#85992));
#19046=EDGE_LOOP('',(#85993,#85994,#85995,#85996,#85997,#85998,#85999,#86000,
#86001,#86002));
#19047=EDGE_LOOP('',(#86003,#86004,#86005,#86006,#86007,#86008));
#19048=EDGE_LOOP('',(#86009,#86010,#86011,#86012));
#19049=EDGE_LOOP('',(#86013,#86014,#86015,#86016));
#19050=EDGE_LOOP('',(#86017,#86018,#86019,#86020));
#19051=EDGE_LOOP('',(#86021,#86022,#86023,#86024));
#19052=EDGE_LOOP('',(#86025,#86026,#86027,#86028));
#19053=EDGE_LOOP('',(#86029,#86030,#86031,#86032));
#19054=EDGE_LOOP('',(#86033,#86034,#86035,#86036));
#19055=EDGE_LOOP('',(#86037,#86038,#86039,#86040));
#19056=EDGE_LOOP('',(#86041,#86042,#86043,#86044,#86045,#86046));
#19057=EDGE_LOOP('',(#86047));
#19058=EDGE_LOOP('',(#86048,#86049,#86050,#86051,#86052,#86053,#86054,#86055));
#19059=EDGE_LOOP('',(#86056,#86057,#86058,#86059,#86060,#86061,#86062,#86063));
#19060=EDGE_LOOP('',(#86064,#86065,#86066,#86067));
#19061=EDGE_LOOP('',(#86068,#86069,#86070,#86071,#86072,#86073));
#19062=EDGE_LOOP('',(#86074,#86075,#86076,#86077));
#19063=EDGE_LOOP('',(#86078,#86079,#86080,#86081,#86082,#86083,#86084));
#19064=EDGE_LOOP('',(#86085,#86086,#86087,#86088,#86089,#86090,#86091));
#19065=EDGE_LOOP('',(#86092,#86093,#86094,#86095));
#19066=EDGE_LOOP('',(#86096,#86097,#86098,#86099));
#19067=EDGE_LOOP('',(#86100));
#19068=EDGE_LOOP('',(#86101,#86102,#86103,#86104));
#19069=EDGE_LOOP('',(#86105,#86106,#86107,#86108));
#19070=EDGE_LOOP('',(#86109));
#19071=EDGE_LOOP('',(#86110,#86111,#86112,#86113));
#19072=EDGE_LOOP('',(#86114,#86115,#86116,#86117));
#19073=EDGE_LOOP('',(#86118));
#19074=EDGE_LOOP('',(#86119,#86120,#86121,#86122));
#19075=EDGE_LOOP('',(#86123));
#19076=EDGE_LOOP('',(#86124,#86125,#86126,#86127,#86128,#86129));
#19077=EDGE_LOOP('',(#86130,#86131,#86132,#86133,#86134,#86135));
#19078=EDGE_LOOP('',(#86136,#86137,#86138,#86139,#86140,#86141));
#19079=EDGE_LOOP('',(#86142,#86143,#86144,#86145,#86146,#86147,#86148,#86149));
#19080=EDGE_LOOP('',(#86150,#86151,#86152,#86153,#86154,#86155));
#19081=EDGE_LOOP('',(#86156,#86157,#86158,#86159,#86160,#86161));
#19082=EDGE_LOOP('',(#86162,#86163,#86164,#86165,#86166,#86167,#86168,#86169));
#19083=EDGE_LOOP('',(#86170,#86171,#86172,#86173,#86174,#86175));
#19084=EDGE_LOOP('',(#86176,#86177,#86178,#86179,#86180,#86181));
#19085=EDGE_LOOP('',(#86182,#86183,#86184,#86185,#86186,#86187,#86188,#86189));
#19086=EDGE_LOOP('',(#86190,#86191,#86192,#86193,#86194));
#19087=EDGE_LOOP('',(#86195,#86196,#86197,#86198,#86199,#86200,#86201,#86202));
#19088=EDGE_LOOP('',(#86203));
#19089=EDGE_LOOP('',(#86204));
#19090=EDGE_LOOP('',(#86205));
#19091=EDGE_LOOP('',(#86206));
#19092=EDGE_LOOP('',(#86207));
#19093=EDGE_LOOP('',(#86208));
#19094=EDGE_LOOP('',(#86209));
#19095=EDGE_LOOP('',(#86210,#86211,#86212,#86213,#86214,#86215,#86216,#86217));
#19096=EDGE_LOOP('',(#86218,#86219,#86220,#86221,#86222,#86223,#86224,#86225));
#19097=EDGE_LOOP('',(#86226,#86227,#86228,#86229));
#19098=EDGE_LOOP('',(#86230,#86231,#86232,#86233));
#19099=EDGE_LOOP('',(#86234,#86235,#86236,#86237));
#19100=EDGE_LOOP('',(#86238,#86239,#86240,#86241));
#19101=EDGE_LOOP('',(#86242,#86243,#86244,#86245,#86246));
#19102=EDGE_LOOP('',(#86247,#86248,#86249,#86250));
#19103=EDGE_LOOP('',(#86251,#86252,#86253,#86254,#86255));
#19104=EDGE_LOOP('',(#86256,#86257,#86258,#86259));
#19105=EDGE_LOOP('',(#86260,#86261,#86262,#86263,#86264));
#19106=EDGE_LOOP('',(#86265,#86266,#86267,#86268));
#19107=EDGE_LOOP('',(#86269,#86270,#86271,#86272,#86273,#86274));
#19108=EDGE_LOOP('',(#86275,#86276,#86277,#86278));
#19109=EDGE_LOOP('',(#86279,#86280,#86281,#86282,#86283));
#19110=EDGE_LOOP('',(#86284,#86285,#86286,#86287));
#19111=EDGE_LOOP('',(#86288,#86289,#86290,#86291,#86292));
#19112=EDGE_LOOP('',(#86293,#86294,#86295,#86296));
#19113=EDGE_LOOP('',(#86297,#86298,#86299,#86300));
#19114=EDGE_LOOP('',(#86301,#86302,#86303,#86304));
#19115=EDGE_LOOP('',(#86305,#86306,#86307,#86308));
#19116=EDGE_LOOP('',(#86309,#86310,#86311,#86312));
#19117=EDGE_LOOP('',(#86313,#86314,#86315,#86316));
#19118=EDGE_LOOP('',(#86317,#86318,#86319,#86320));
#19119=EDGE_LOOP('',(#86321,#86322,#86323,#86324));
#19120=EDGE_LOOP('',(#86325,#86326,#86327));
#19121=EDGE_LOOP('',(#86328,#86329,#86330,#86331));
#19122=EDGE_LOOP('',(#86332,#86333,#86334,#86335));
#19123=EDGE_LOOP('',(#86336,#86337,#86338,#86339));
#19124=EDGE_LOOP('',(#86340,#86341,#86342));
#19125=EDGE_LOOP('',(#86343,#86344,#86345,#86346));
#19126=EDGE_LOOP('',(#86347,#86348,#86349,#86350));
#19127=EDGE_LOOP('',(#86351,#86352,#86353));
#19128=EDGE_LOOP('',(#86354,#86355,#86356,#86357));
#19129=EDGE_LOOP('',(#86358,#86359,#86360,#86361));
#19130=EDGE_LOOP('',(#86362,#86363,#86364,#86365));
#19131=EDGE_LOOP('',(#86366,#86367,#86368));
#19132=EDGE_LOOP('',(#86369,#86370,#86371,#86372));
#19133=EDGE_LOOP('',(#86373,#86374,#86375,#86376));
#19134=EDGE_LOOP('',(#86377,#86378,#86379,#86380));
#19135=EDGE_LOOP('',(#86381,#86382,#86383));
#19136=EDGE_LOOP('',(#86384,#86385,#86386,#86387));
#19137=EDGE_LOOP('',(#86388,#86389,#86390,#86391));
#19138=EDGE_LOOP('',(#86392,#86393,#86394,#86395));
#19139=EDGE_LOOP('',(#86396,#86397,#86398));
#19140=EDGE_LOOP('',(#86399,#86400,#86401,#86402));
#19141=EDGE_LOOP('',(#86403,#86404,#86405,#86406));
#19142=EDGE_LOOP('',(#86407,#86408,#86409,#86410));
#19143=EDGE_LOOP('',(#86411,#86412,#86413,#86414));
#19144=EDGE_LOOP('',(#86415,#86416,#86417,#86418));
#19145=EDGE_LOOP('',(#86419,#86420,#86421,#86422));
#19146=EDGE_LOOP('',(#86423,#86424,#86425,#86426));
#19147=EDGE_LOOP('',(#86427,#86428,#86429,#86430));
#19148=EDGE_LOOP('',(#86431,#86432,#86433,#86434));
#19149=EDGE_LOOP('',(#86435,#86436,#86437,#86438));
#19150=EDGE_LOOP('',(#86439,#86440,#86441,#86442));
#19151=EDGE_LOOP('',(#86443,#86444,#86445,#86446));
#19152=EDGE_LOOP('',(#86447,#86448,#86449,#86450));
#19153=EDGE_LOOP('',(#86451,#86452,#86453,#86454,#86455,#86456));
#19154=EDGE_LOOP('',(#86457,#86458,#86459,#86460));
#19155=EDGE_LOOP('',(#86461,#86462,#86463,#86464,#86465,#86466));
#19156=EDGE_LOOP('',(#86467,#86468,#86469,#86470,#86471,#86472));
#19157=EDGE_LOOP('',(#86473,#86474,#86475,#86476));
#19158=EDGE_LOOP('',(#86477,#86478,#86479,#86480,#86481,#86482));
#19159=EDGE_LOOP('',(#86483,#86484,#86485,#86486,#86487,#86488));
#19160=EDGE_LOOP('',(#86489,#86490,#86491,#86492));
#19161=EDGE_LOOP('',(#86493,#86494,#86495,#86496,#86497,#86498));
#19162=EDGE_LOOP('',(#86499,#86500,#86501,#86502,#86503,#86504));
#19163=EDGE_LOOP('',(#86505,#86506,#86507,#86508));
#19164=EDGE_LOOP('',(#86509,#86510,#86511,#86512,#86513,#86514));
#19165=EDGE_LOOP('',(#86515,#86516,#86517,#86518));
#19166=EDGE_LOOP('',(#86519,#86520,#86521,#86522));
#19167=EDGE_LOOP('',(#86523,#86524,#86525,#86526,#86527));
#19168=EDGE_LOOP('',(#86528,#86529,#86530,#86531));
#19169=EDGE_LOOP('',(#86532,#86533,#86534,#86535));
#19170=EDGE_LOOP('',(#86536,#86537,#86538,#86539,#86540));
#19171=EDGE_LOOP('',(#86541,#86542,#86543,#86544,#86545));
#19172=EDGE_LOOP('',(#86546,#86547,#86548));
#19173=EDGE_LOOP('',(#86549,#86550,#86551,#86552,#86553));
#19174=EDGE_LOOP('',(#86554,#86555,#86556));
#19175=EDGE_LOOP('',(#86557,#86558,#86559,#86560));
#19176=EDGE_LOOP('',(#86561,#86562,#86563));
#19177=EDGE_LOOP('',(#86564,#86565,#86566));
#19178=EDGE_LOOP('',(#86567,#86568,#86569,#86570));
#19179=EDGE_LOOP('',(#86571,#86572,#86573,#86574));
#19180=EDGE_LOOP('',(#86575,#86576,#86577));
#19181=EDGE_LOOP('',(#86578,#86579,#86580,#86581));
#19182=EDGE_LOOP('',(#86582,#86583,#86584,#86585));
#19183=EDGE_LOOP('',(#86586,#86587,#86588));
#19184=EDGE_LOOP('',(#86589,#86590,#86591,#86592));
#19185=EDGE_LOOP('',(#86593,#86594,#86595,#86596));
#19186=EDGE_LOOP('',(#86597,#86598,#86599));
#19187=EDGE_LOOP('',(#86600,#86601,#86602,#86603,#86604));
#19188=EDGE_LOOP('',(#86605,#86606,#86607,#86608));
#19189=EDGE_LOOP('',(#86609,#86610,#86611));
#19190=EDGE_LOOP('',(#86612,#86613,#86614,#86615,#86616));
#19191=EDGE_LOOP('',(#86617,#86618,#86619,#86620));
#19192=EDGE_LOOP('',(#86621,#86622,#86623));
#19193=EDGE_LOOP('',(#86624,#86625,#86626,#86627));
#19194=EDGE_LOOP('',(#86628,#86629,#86630,#86631));
#19195=EDGE_LOOP('',(#86632,#86633,#86634));
#19196=EDGE_LOOP('',(#86635,#86636,#86637));
#19197=EDGE_LOOP('',(#86638,#86639,#86640,#86641));
#19198=EDGE_LOOP('',(#86642,#86643,#86644,#86645));
#19199=EDGE_LOOP('',(#86646,#86647,#86648,#86649));
#19200=EDGE_LOOP('',(#86650,#86651,#86652,#86653));
#19201=EDGE_LOOP('',(#86654,#86655,#86656));
#19202=EDGE_LOOP('',(#86657,#86658,#86659,#86660));
#19203=EDGE_LOOP('',(#86661,#86662,#86663,#86664));
#19204=EDGE_LOOP('',(#86665,#86666,#86667,#86668));
#19205=EDGE_LOOP('',(#86669,#86670,#86671,#86672));
#19206=EDGE_LOOP('',(#86673,#86674,#86675,#86676));
#19207=EDGE_LOOP('',(#86677,#86678));
#19208=EDGE_LOOP('',(#86679,#86680,#86681,#86682,#86683));
#19209=EDGE_LOOP('',(#86684,#86685,#86686,#86687,#86688));
#19210=EDGE_LOOP('',(#86689,#86690,#86691,#86692,#86693,#86694));
#19211=EDGE_LOOP('',(#86695,#86696,#86697,#86698));
#19212=EDGE_LOOP('',(#86699,#86700,#86701,#86702,#86703,#86704,#86705));
#19213=EDGE_LOOP('',(#86706,#86707,#86708,#86709,#86710,#86711));
#19214=EDGE_LOOP('',(#86712,#86713,#86714));
#19215=EDGE_LOOP('',(#86715));
#19216=EDGE_LOOP('',(#86716));
#19217=EDGE_LOOP('',(#86717,#86718,#86719,#86720,#86721,#86722));
#19218=EDGE_LOOP('',(#86723,#86724,#86725,#86726,#86727));
#19219=EDGE_LOOP('',(#86728,#86729,#86730,#86731,#86732));
#19220=EDGE_LOOP('',(#86733,#86734,#86735,#86736,#86737));
#19221=EDGE_LOOP('',(#86738,#86739,#86740,#86741,#86742));
#19222=EDGE_LOOP('',(#86743));
#19223=EDGE_LOOP('',(#86744,#86745,#86746,#86747,#86748));
#19224=EDGE_LOOP('',(#86749,#86750));
#19225=EDGE_LOOP('',(#86751));
#19226=EDGE_LOOP('',(#86752));
#19227=EDGE_LOOP('',(#86753));
#19228=EDGE_LOOP('',(#86754));
#19229=EDGE_LOOP('',(#86755,#86756,#86757,#86758));
#19230=EDGE_LOOP('',(#86759,#86760,#86761,#86762,#86763));
#19231=EDGE_LOOP('',(#86764,#86765,#86766,#86767,#86768));
#19232=EDGE_LOOP('',(#86769,#86770,#86771,#86772));
#19233=EDGE_LOOP('',(#86773,#86774,#86775,#86776));
#19234=EDGE_LOOP('',(#86777,#86778,#86779,#86780));
#19235=EDGE_LOOP('',(#86781,#86782,#86783,#86784));
#19236=EDGE_LOOP('',(#86785,#86786,#86787,#86788));
#19237=EDGE_LOOP('',(#86789,#86790,#86791,#86792,#86793));
#19238=EDGE_LOOP('',(#86794,#86795,#86796,#86797,#86798));
#19239=EDGE_LOOP('',(#86799,#86800,#86801,#86802));
#19240=EDGE_LOOP('',(#86803));
#19241=EDGE_LOOP('',(#86804));
#19242=EDGE_LOOP('',(#86805));
#19243=EDGE_LOOP('',(#86806));
#19244=EDGE_LOOP('',(#86807));
#19245=EDGE_LOOP('',(#86808));
#19246=EDGE_LOOP('',(#86809));
#19247=EDGE_LOOP('',(#86810));
#19248=EDGE_LOOP('',(#86811));
#19249=EDGE_LOOP('',(#86812));
#19250=EDGE_LOOP('',(#86813,#86814,#86815,#86816));
#19251=EDGE_LOOP('',(#86817,#86818,#86819,#86820));
#19252=EDGE_LOOP('',(#86821,#86822,#86823,#86824));
#19253=EDGE_LOOP('',(#86825,#86826,#86827,#86828));
#19254=EDGE_LOOP('',(#86829,#86830,#86831,#86832));
#19255=EDGE_LOOP('',(#86833,#86834,#86835,#86836));
#19256=EDGE_LOOP('',(#86837,#86838,#86839));
#19257=EDGE_LOOP('',(#86840,#86841,#86842,#86843,#86844));
#19258=EDGE_LOOP('',(#86845,#86846,#86847,#86848));
#19259=EDGE_LOOP('',(#86849,#86850,#86851,#86852));
#19260=EDGE_LOOP('',(#86853,#86854,#86855,#86856));
#19261=EDGE_LOOP('',(#86857,#86858,#86859,#86860));
#19262=EDGE_LOOP('',(#86861,#86862,#86863,#86864));
#19263=EDGE_LOOP('',(#86865,#86866,#86867,#86868,#86869));
#19264=EDGE_LOOP('',(#86870,#86871,#86872,#86873,#86874,#86875,#86876,#86877));
#19265=EDGE_LOOP('',(#86878,#86879,#86880,#86881,#86882,#86883,#86884,#86885,
#86886));
#19266=EDGE_LOOP('',(#86887,#86888,#86889,#86890));
#19267=EDGE_LOOP('',(#86891));
#19268=EDGE_LOOP('',(#86892));
#19269=EDGE_LOOP('',(#86893,#86894,#86895,#86896,#86897,#86898));
#19270=EDGE_LOOP('',(#86899,#86900));
#19271=EDGE_LOOP('',(#86901,#86902));
#19272=EDGE_LOOP('',(#86903,#86904));
#19273=EDGE_LOOP('',(#86905,#86906));
#19274=EDGE_LOOP('',(#86907,#86908));
#19275=EDGE_LOOP('',(#86909,#86910));
#19276=EDGE_LOOP('',(#86911,#86912,#86913,#86914,#86915,#86916));
#19277=EDGE_LOOP('',(#86917,#86918,#86919,#86920));
#19278=EDGE_LOOP('',(#86921,#86922,#86923,#86924));
#19279=EDGE_LOOP('',(#86925,#86926,#86927,#86928));
#19280=EDGE_LOOP('',(#86929,#86930,#86931,#86932));
#19281=EDGE_LOOP('',(#86933,#86934,#86935,#86936));
#19282=EDGE_LOOP('',(#86937,#86938,#86939,#86940));
#19283=EDGE_LOOP('',(#86941,#86942,#86943,#86944,#86945,#86946,#86947,#86948,
#86949,#86950,#86951,#86952,#86953,#86954,#86955,#86956,#86957));
#19284=EDGE_LOOP('',(#86958,#86959,#86960,#86961));
#19285=EDGE_LOOP('',(#86962,#86963,#86964,#86965,#86966,#86967,#86968,#86969,
#86970,#86971,#86972,#86973,#86974,#86975,#86976,#86977,#86978));
#19286=EDGE_LOOP('',(#86979,#86980,#86981,#86982));
#19287=EDGE_LOOP('',(#86983,#86984,#86985,#86986));
#19288=EDGE_LOOP('',(#86987,#86988,#86989,#86990));
#19289=EDGE_LOOP('',(#86991,#86992,#86993,#86994));
#19290=EDGE_LOOP('',(#86995,#86996,#86997,#86998));
#19291=EDGE_LOOP('',(#86999,#87000,#87001,#87002));
#19292=EDGE_LOOP('',(#87003,#87004,#87005));
#19293=EDGE_LOOP('',(#87006,#87007,#87008,#87009,#87010));
#19294=EDGE_LOOP('',(#87011,#87012,#87013,#87014));
#19295=EDGE_LOOP('',(#87015,#87016,#87017,#87018));
#19296=EDGE_LOOP('',(#87019,#87020,#87021,#87022));
#19297=EDGE_LOOP('',(#87023,#87024,#87025,#87026));
#19298=EDGE_LOOP('',(#87027,#87028,#87029,#87030));
#19299=EDGE_LOOP('',(#87031,#87032,#87033,#87034,#87035));
#19300=EDGE_LOOP('',(#87036,#87037,#87038,#87039,#87040,#87041,#87042,#87043));
#19301=EDGE_LOOP('',(#87044,#87045,#87046,#87047,#87048,#87049,#87050,#87051,
#87052));
#19302=EDGE_LOOP('',(#87053,#87054,#87055,#87056));
#19303=EDGE_LOOP('',(#87057));
#19304=EDGE_LOOP('',(#87058));
#19305=EDGE_LOOP('',(#87059,#87060,#87061,#87062,#87063,#87064));
#19306=EDGE_LOOP('',(#87065,#87066));
#19307=EDGE_LOOP('',(#87067,#87068));
#19308=EDGE_LOOP('',(#87069,#87070));
#19309=EDGE_LOOP('',(#87071,#87072));
#19310=EDGE_LOOP('',(#87073,#87074));
#19311=EDGE_LOOP('',(#87075,#87076));
#19312=EDGE_LOOP('',(#87077,#87078,#87079,#87080,#87081,#87082));
#19313=EDGE_LOOP('',(#87083,#87084,#87085,#87086));
#19314=EDGE_LOOP('',(#87087,#87088,#87089,#87090));
#19315=EDGE_LOOP('',(#87091,#87092,#87093,#87094));
#19316=EDGE_LOOP('',(#87095,#87096,#87097,#87098));
#19317=EDGE_LOOP('',(#87099,#87100,#87101,#87102));
#19318=EDGE_LOOP('',(#87103,#87104,#87105,#87106));
#19319=EDGE_LOOP('',(#87107,#87108,#87109,#87110,#87111,#87112,#87113,#87114,
#87115,#87116,#87117,#87118,#87119,#87120,#87121,#87122,#87123));
#19320=EDGE_LOOP('',(#87124,#87125,#87126,#87127));
#19321=EDGE_LOOP('',(#87128,#87129,#87130,#87131,#87132,#87133,#87134,#87135,
#87136,#87137,#87138,#87139,#87140,#87141,#87142,#87143,#87144));
#19322=EDGE_LOOP('',(#87145,#87146,#87147,#87148));
#19323=EDGE_LOOP('',(#87149,#87150,#87151,#87152,#87153));
#19324=EDGE_LOOP('',(#87154,#87155,#87156,#87157));
#19325=EDGE_LOOP('',(#87158,#87159,#87160,#87161,#87162));
#19326=EDGE_LOOP('',(#87163,#87164,#87165,#87166,#87167,#87168,#87169,#87170,
#87171));
#19327=EDGE_LOOP('',(#87172,#87173));
#19328=EDGE_LOOP('',(#87174,#87175,#87176,#87177,#87178));
#19329=EDGE_LOOP('',(#87179,#87180,#87181,#87182,#87183,#87184));
#19330=EDGE_LOOP('',(#87185,#87186,#87187,#87188,#87189,#87190,#87191,#87192,
#87193));
#19331=EDGE_LOOP('',(#87194));
#19332=EDGE_LOOP('',(#87195));
#19333=EDGE_LOOP('',(#87196));
#19334=EDGE_LOOP('',(#87197));
#19335=EDGE_LOOP('',(#87198));
#19336=EDGE_LOOP('',(#87199,#87200,#87201,#87202));
#19337=EDGE_LOOP('',(#87203,#87204,#87205,#87206));
#19338=EDGE_LOOP('',(#87207,#87208,#87209,#87210,#87211));
#19339=EDGE_LOOP('',(#87212,#87213,#87214,#87215,#87216));
#19340=EDGE_LOOP('',(#87217,#87218,#87219,#87220));
#19341=EDGE_LOOP('',(#87221,#87222,#87223,#87224));
#19342=EDGE_LOOP('',(#87225,#87226,#87227,#87228));
#19343=EDGE_LOOP('',(#87229,#87230,#87231,#87232));
#19344=EDGE_LOOP('',(#87233,#87234,#87235,#87236));
#19345=EDGE_LOOP('',(#87237,#87238,#87239,#87240));
#19346=EDGE_LOOP('',(#87241,#87242,#87243,#87244));
#19347=EDGE_LOOP('',(#87245,#87246,#87247,#87248));
#19348=EDGE_LOOP('',(#87249,#87250,#87251,#87252));
#19349=EDGE_LOOP('',(#87253,#87254,#87255,#87256));
#19350=EDGE_LOOP('',(#87257,#87258,#87259,#87260));
#19351=EDGE_LOOP('',(#87261,#87262,#87263,#87264));
#19352=EDGE_LOOP('',(#87265,#87266,#87267,#87268));
#19353=EDGE_LOOP('',(#87269,#87270,#87271,#87272));
#19354=EDGE_LOOP('',(#87273,#87274,#87275,#87276));
#19355=EDGE_LOOP('',(#87277,#87278,#87279,#87280));
#19356=EDGE_LOOP('',(#87281,#87282,#87283,#87284));
#19357=EDGE_LOOP('',(#87285,#87286,#87287,#87288));
#19358=EDGE_LOOP('',(#87289,#87290,#87291,#87292));
#19359=EDGE_LOOP('',(#87293,#87294,#87295,#87296,#87297,#87298,#87299,#87300));
#19360=EDGE_LOOP('',(#87301));
#19361=EDGE_LOOP('',(#87302));
#19362=EDGE_LOOP('',(#87303));
#19363=EDGE_LOOP('',(#87304));
#19364=EDGE_LOOP('',(#87305));
#19365=EDGE_LOOP('',(#87306));
#19366=EDGE_LOOP('',(#87307));
#19367=EDGE_LOOP('',(#87308));
#19368=EDGE_LOOP('',(#87309));
#19369=EDGE_LOOP('',(#87310));
#19370=EDGE_LOOP('',(#87311));
#19371=EDGE_LOOP('',(#87312));
#19372=EDGE_LOOP('',(#87313));
#19373=EDGE_LOOP('',(#87314,#87315,#87316,#87317,#87318,#87319,#87320,#87321));
#19374=EDGE_LOOP('',(#87322,#87323,#87324,#87325,#87326,#87327,#87328,#87329));
#19375=EDGE_LOOP('',(#87330,#87331,#87332,#87333));
#19376=EDGE_LOOP('',(#87334,#87335,#87336,#87337));
#19377=EDGE_LOOP('',(#87338,#87339,#87340,#87341));
#19378=EDGE_LOOP('',(#87342,#87343,#87344,#87345));
#19379=EDGE_LOOP('',(#87346,#87347,#87348,#87349));
#19380=EDGE_LOOP('',(#87350,#87351,#87352,#87353));
#19381=EDGE_LOOP('',(#87354,#87355,#87356,#87357));
#19382=EDGE_LOOP('',(#87358,#87359,#87360,#87361));
#19383=EDGE_LOOP('',(#87362,#87363,#87364,#87365));
#19384=EDGE_LOOP('',(#87366,#87367,#87368,#87369));
#19385=EDGE_LOOP('',(#87370,#87371,#87372,#87373));
#19386=EDGE_LOOP('',(#87374,#87375,#87376,#87377));
#19387=EDGE_LOOP('',(#87378,#87379,#87380,#87381));
#19388=EDGE_LOOP('',(#87382,#87383,#87384,#87385));
#19389=EDGE_LOOP('',(#87386,#87387,#87388,#87389));
#19390=EDGE_LOOP('',(#87390,#87391,#87392,#87393));
#19391=EDGE_LOOP('',(#87394,#87395,#87396,#87397,#87398,#87399,#87400,#87401));
#19392=EDGE_LOOP('',(#87402));
#19393=EDGE_LOOP('',(#87403));
#19394=EDGE_LOOP('',(#87404));
#19395=EDGE_LOOP('',(#87405));
#19396=EDGE_LOOP('',(#87406));
#19397=EDGE_LOOP('',(#87407,#87408,#87409,#87410));
#19398=EDGE_LOOP('',(#87411));
#19399=EDGE_LOOP('',(#87412,#87413,#87414,#87415,#87416,#87417,#87418,#87419));
#19400=EDGE_LOOP('',(#87420));
#19401=EDGE_LOOP('',(#87421));
#19402=EDGE_LOOP('',(#87422));
#19403=EDGE_LOOP('',(#87423));
#19404=EDGE_LOOP('',(#87424));
#19405=EDGE_LOOP('',(#87425));
#19406=EDGE_LOOP('',(#87426,#87427,#87428,#87429));
#19407=EDGE_LOOP('',(#87430,#87431,#87432,#87433));
#19408=EDGE_LOOP('',(#87434,#87435,#87436,#87437));
#19409=EDGE_LOOP('',(#87438,#87439,#87440,#87441,#87442,#87443,#87444,#87445));
#19410=EDGE_LOOP('',(#87446));
#19411=EDGE_LOOP('',(#87447,#87448,#87449,#87450));
#19412=EDGE_LOOP('',(#87451,#87452,#87453,#87454));
#19413=EDGE_LOOP('',(#87455,#87456,#87457,#87458));
#19414=EDGE_LOOP('',(#87459,#87460,#87461,#87462));
#19415=EDGE_LOOP('',(#87463,#87464,#87465,#87466));
#19416=EDGE_LOOP('',(#87467,#87468,#87469,#87470));
#19417=EDGE_LOOP('',(#87471,#87472,#87473,#87474));
#19418=EDGE_LOOP('',(#87475,#87476,#87477,#87478));
#19419=EDGE_LOOP('',(#87479,#87480,#87481,#87482));
#19420=EDGE_LOOP('',(#87483,#87484,#87485,#87486));
#19421=EDGE_LOOP('',(#87487,#87488,#87489,#87490));
#19422=EDGE_LOOP('',(#87491,#87492,#87493,#87494));
#19423=EDGE_LOOP('',(#87495,#87496,#87497,#87498));
#19424=EDGE_LOOP('',(#87499,#87500,#87501,#87502));
#19425=EDGE_LOOP('',(#87503,#87504,#87505,#87506));
#19426=EDGE_LOOP('',(#87507,#87508,#87509,#87510));
#19427=EDGE_LOOP('',(#87511,#87512,#87513));
#19428=EDGE_LOOP('',(#87514,#87515,#87516,#87517));
#19429=EDGE_LOOP('',(#87518,#87519,#87520,#87521));
#19430=EDGE_LOOP('',(#87522,#87523,#87524,#87525,#87526));
#19431=EDGE_LOOP('',(#87527,#87528,#87529,#87530));
#19432=EDGE_LOOP('',(#87531,#87532,#87533,#87534,#87535));
#19433=EDGE_LOOP('',(#87536,#87537,#87538,#87539));
#19434=EDGE_LOOP('',(#87540,#87541,#87542,#87543,#87544));
#19435=EDGE_LOOP('',(#87545,#87546,#87547,#87548));
#19436=EDGE_LOOP('',(#87549,#87550,#87551,#87552,#87553));
#19437=EDGE_LOOP('',(#87554,#87555,#87556,#87557));
#19438=EDGE_LOOP('',(#87558,#87559,#87560,#87561));
#19439=EDGE_LOOP('',(#87562,#87563,#87564,#87565,#87566));
#19440=EDGE_LOOP('',(#87567,#87568,#87569,#87570));
#19441=EDGE_LOOP('',(#87571,#87572,#87573,#87574));
#19442=EDGE_LOOP('',(#87575,#87576,#87577,#87578,#87579,#87580,#87581,#87582,
#87583,#87584,#87585,#87586,#87587,#87588,#87589,#87590,#87591));
#19443=EDGE_LOOP('',(#87592));
#19444=EDGE_LOOP('',(#87593,#87594));
#19445=EDGE_LOOP('',(#87595,#87596,#87597,#87598));
#19446=EDGE_LOOP('',(#87599,#87600,#87601,#87602));
#19447=EDGE_LOOP('',(#87603,#87604,#87605,#87606));
#19448=EDGE_LOOP('',(#87607,#87608,#87609,#87610));
#19449=EDGE_LOOP('',(#87611));
#19450=EDGE_LOOP('',(#87612,#87613,#87614,#87615,#87616,#87617));
#19451=EDGE_LOOP('',(#87618,#87619,#87620));
#19452=EDGE_LOOP('',(#87621,#87622));
#19453=EDGE_LOOP('',(#87623,#87624));
#19454=EDGE_LOOP('',(#87625,#87626,#87627));
#19455=EDGE_LOOP('',(#87628,#87629,#87630,#87631));
#19456=EDGE_LOOP('',(#87632,#87633,#87634,#87635));
#19457=EDGE_LOOP('',(#87636,#87637,#87638,#87639));
#19458=EDGE_LOOP('',(#87640,#87641,#87642,#87643));
#19459=EDGE_LOOP('',(#87644,#87645,#87646,#87647));
#19460=EDGE_LOOP('',(#87648,#87649,#87650,#87651));
#19461=EDGE_LOOP('',(#87652,#87653,#87654,#87655));
#19462=EDGE_LOOP('',(#87656,#87657,#87658,#87659));
#19463=EDGE_LOOP('',(#87660,#87661,#87662,#87663));
#19464=EDGE_LOOP('',(#87664,#87665,#87666,#87667));
#19465=EDGE_LOOP('',(#87668,#87669,#87670,#87671));
#19466=EDGE_LOOP('',(#87672,#87673,#87674,#87675));
#19467=EDGE_LOOP('',(#87676));
#19468=EDGE_LOOP('',(#87677,#87678,#87679,#87680,#87681,#87682));
#19469=EDGE_LOOP('',(#87683,#87684));
#19470=EDGE_LOOP('',(#87685,#87686,#87687));
#19471=EDGE_LOOP('',(#87688,#87689));
#19472=EDGE_LOOP('',(#87690,#87691,#87692));
#19473=EDGE_LOOP('',(#87693));
#19474=EDGE_LOOP('',(#87694,#87695,#87696));
#19475=EDGE_LOOP('',(#87697,#87698,#87699));
#19476=EDGE_LOOP('',(#87700,#87701));
#19477=EDGE_LOOP('',(#87702));
#19478=EDGE_LOOP('',(#87703,#87704,#87705));
#19479=EDGE_LOOP('',(#87706,#87707,#87708));
#19480=EDGE_LOOP('',(#87709,#87710));
#19481=EDGE_LOOP('',(#87711));
#19482=EDGE_LOOP('',(#87712,#87713,#87714));
#19483=EDGE_LOOP('',(#87715,#87716,#87717));
#19484=EDGE_LOOP('',(#87718,#87719));
#19485=EDGE_LOOP('',(#87720));
#19486=EDGE_LOOP('',(#87721,#87722,#87723));
#19487=EDGE_LOOP('',(#87724,#87725));
#19488=EDGE_LOOP('',(#87726,#87727,#87728));
#19489=EDGE_LOOP('',(#87729));
#19490=EDGE_LOOP('',(#87730));
#19491=EDGE_LOOP('',(#87731,#87732));
#19492=EDGE_LOOP('',(#87733,#87734,#87735,#87736));
#19493=EDGE_LOOP('',(#87737,#87738,#87739,#87740,#87741,#87742));
#19494=EDGE_LOOP('',(#87743,#87744,#87745,#87746,#87747,#87748,#87749,#87750));
#19495=EDGE_LOOP('',(#87751,#87752,#87753,#87754));
#19496=EDGE_LOOP('',(#87755,#87756,#87757,#87758,#87759,#87760,#87761,#87762));
#19497=EDGE_LOOP('',(#87763,#87764,#87765,#87766));
#19498=EDGE_LOOP('',(#87767,#87768,#87769,#87770,#87771,#87772,#87773,#87774));
#19499=EDGE_LOOP('',(#87775,#87776,#87777,#87778,#87779,#87780,#87781,#87782));
#19500=EDGE_LOOP('',(#87783,#87784,#87785,#87786));
#19501=EDGE_LOOP('',(#87787,#87788,#87789,#87790));
#19502=EDGE_LOOP('',(#87791,#87792,#87793,#87794));
#19503=EDGE_LOOP('',(#87795,#87796,#87797,#87798));
#19504=EDGE_LOOP('',(#87799,#87800,#87801,#87802));
#19505=EDGE_LOOP('',(#87803,#87804,#87805,#87806));
#19506=EDGE_LOOP('',(#87807,#87808,#87809,#87810));
#19507=EDGE_LOOP('',(#87811,#87812,#87813,#87814));
#19508=EDGE_LOOP('',(#87815,#87816,#87817,#87818));
#19509=EDGE_LOOP('',(#87819,#87820,#87821,#87822));
#19510=EDGE_LOOP('',(#87823,#87824,#87825,#87826));
#19511=EDGE_LOOP('',(#87827,#87828,#87829,#87830));
#19512=EDGE_LOOP('',(#87831,#87832,#87833,#87834));
#19513=EDGE_LOOP('',(#87835,#87836,#87837,#87838));
#19514=EDGE_LOOP('',(#87839,#87840,#87841,#87842));
#19515=EDGE_LOOP('',(#87843,#87844,#87845,#87846));
#19516=EDGE_LOOP('',(#87847,#87848,#87849,#87850,#87851));
#19517=EDGE_LOOP('',(#87852,#87853,#87854,#87855,#87856));
#19518=EDGE_LOOP('',(#87857,#87858,#87859,#87860,#87861));
#19519=EDGE_LOOP('',(#87862,#87863,#87864,#87865,#87866));
#19520=EDGE_LOOP('',(#87867,#87868,#87869,#87870));
#19521=EDGE_LOOP('',(#87871,#87872,#87873,#87874,#87875,#87876,#87877,#87878));
#19522=EDGE_LOOP('',(#87879,#87880,#87881,#87882));
#19523=EDGE_LOOP('',(#87883,#87884,#87885,#87886,#87887,#87888,#87889,#87890));
#19524=EDGE_LOOP('',(#87891,#87892,#87893,#87894,#87895,#87896));
#19525=EDGE_LOOP('',(#87897,#87898,#87899,#87900));
#19526=EDGE_LOOP('',(#87901,#87902,#87903,#87904));
#19527=EDGE_LOOP('',(#87905,#87906,#87907,#87908));
#19528=EDGE_LOOP('',(#87909,#87910,#87911,#87912));
#19529=EDGE_LOOP('',(#87913,#87914,#87915,#87916));
#19530=EDGE_LOOP('',(#87917,#87918,#87919,#87920));
#19531=EDGE_LOOP('',(#87921,#87922,#87923,#87924));
#19532=EDGE_LOOP('',(#87925,#87926,#87927,#87928));
#19533=EDGE_LOOP('',(#87929,#87930,#87931,#87932));
#19534=EDGE_LOOP('',(#87933,#87934,#87935,#87936));
#19535=EDGE_LOOP('',(#87937,#87938,#87939,#87940));
#19536=EDGE_LOOP('',(#87941,#87942,#87943,#87944));
#19537=EDGE_LOOP('',(#87945,#87946,#87947,#87948));
#19538=EDGE_LOOP('',(#87949,#87950,#87951,#87952));
#19539=EDGE_LOOP('',(#87953,#87954,#87955,#87956));
#19540=EDGE_LOOP('',(#87957,#87958,#87959,#87960));
#19541=EDGE_LOOP('',(#87961,#87962,#87963,#87964));
#19542=EDGE_LOOP('',(#87965,#87966,#87967,#87968));
#19543=EDGE_LOOP('',(#87969,#87970,#87971,#87972));
#19544=EDGE_LOOP('',(#87973,#87974,#87975,#87976));
#19545=EDGE_LOOP('',(#87977,#87978,#87979,#87980));
#19546=EDGE_LOOP('',(#87981,#87982,#87983,#87984));
#19547=EDGE_LOOP('',(#87985,#87986,#87987,#87988));
#19548=EDGE_LOOP('',(#87989,#87990,#87991,#87992));
#19549=EDGE_LOOP('',(#87993,#87994,#87995,#87996));
#19550=EDGE_LOOP('',(#87997,#87998,#87999,#88000));
#19551=EDGE_LOOP('',(#88001,#88002,#88003,#88004));
#19552=EDGE_LOOP('',(#88005,#88006,#88007,#88008));
#19553=EDGE_LOOP('',(#88009,#88010,#88011,#88012,#88013,#88014));
#19554=EDGE_LOOP('',(#88015,#88016,#88017,#88018));
#19555=EDGE_LOOP('',(#88019,#88020,#88021,#88022,#88023,#88024));
#19556=EDGE_LOOP('',(#88025,#88026,#88027,#88028));
#19557=EDGE_LOOP('',(#88029,#88030,#88031,#88032,#88033,#88034,#88035,#88036,
#88037,#88038,#88039,#88040,#88041,#88042,#88043,#88044));
#19558=EDGE_LOOP('',(#88045,#88046,#88047,#88048));
#19559=EDGE_LOOP('',(#88049,#88050,#88051,#88052));
#19560=EDGE_LOOP('',(#88053,#88054,#88055,#88056));
#19561=EDGE_LOOP('',(#88057,#88058,#88059,#88060));
#19562=EDGE_LOOP('',(#88061,#88062,#88063,#88064));
#19563=EDGE_LOOP('',(#88065,#88066,#88067,#88068));
#19564=EDGE_LOOP('',(#88069,#88070,#88071,#88072));
#19565=EDGE_LOOP('',(#88073,#88074,#88075,#88076));
#19566=EDGE_LOOP('',(#88077,#88078,#88079,#88080));
#19567=EDGE_LOOP('',(#88081,#88082,#88083,#88084));
#19568=EDGE_LOOP('',(#88085,#88086,#88087,#88088));
#19569=EDGE_LOOP('',(#88089,#88090,#88091,#88092));
#19570=EDGE_LOOP('',(#88093,#88094,#88095,#88096));
#19571=EDGE_LOOP('',(#88097,#88098,#88099,#88100));
#19572=EDGE_LOOP('',(#88101,#88102,#88103,#88104));
#19573=EDGE_LOOP('',(#88105,#88106,#88107,#88108,#88109,#88110,#88111,#88112,
#88113,#88114,#88115,#88116,#88117,#88118,#88119,#88120));
#19574=EDGE_LOOP('',(#88121,#88122,#88123,#88124,#88125,#88126,#88127,#88128));
#19575=EDGE_LOOP('',(#88129,#88130,#88131,#88132));
#19576=EDGE_LOOP('',(#88133,#88134,#88135,#88136));
#19577=EDGE_LOOP('',(#88137,#88138,#88139,#88140));
#19578=EDGE_LOOP('',(#88141,#88142,#88143,#88144));
#19579=EDGE_LOOP('',(#88145,#88146,#88147,#88148));
#19580=EDGE_LOOP('',(#88149,#88150,#88151,#88152));
#19581=EDGE_LOOP('',(#88153,#88154,#88155,#88156));
#19582=EDGE_LOOP('',(#88157,#88158,#88159,#88160));
#19583=EDGE_LOOP('',(#88161,#88162,#88163,#88164,#88165,#88166,#88167,#88168));
#19584=EDGE_LOOP('',(#88169,#88170,#88171,#88172,#88173,#88174,#88175,#88176,
#88177,#88178,#88179,#88180,#88181,#88182,#88183,#88184,#88185,#88186,#88187,
#88188,#88189,#88190,#88191,#88192,#88193,#88194,#88195,#88196,#88197,#88198,
#88199,#88200,#88201,#88202,#88203,#88204,#88205,#88206,#88207,#88208,#88209,
#88210,#88211,#88212,#88213,#88214,#88215,#88216,#88217,#88218,#88219,#88220,
#88221,#88222,#88223,#88224));
#19585=EDGE_LOOP('',(#88225,#88226,#88227,#88228,#88229,#88230,#88231,#88232,
#88233,#88234,#88235,#88236,#88237,#88238,#88239,#88240,#88241,#88242,#88243,
#88244,#88245,#88246,#88247,#88248,#88249,#88250,#88251,#88252,#88253,#88254,
#88255,#88256,#88257,#88258,#88259,#88260,#88261,#88262,#88263,#88264,#88265,
#88266,#88267,#88268,#88269,#88270,#88271,#88272,#88273,#88274,#88275,#88276,
#88277,#88278,#88279,#88280));
#19586=EDGE_LOOP('',(#88281,#88282,#88283,#88284));
#19587=EDGE_LOOP('',(#88285,#88286,#88287,#88288));
#19588=EDGE_LOOP('',(#88289,#88290,#88291,#88292));
#19589=EDGE_LOOP('',(#88293,#88294,#88295,#88296));
#19590=EDGE_LOOP('',(#88297,#88298,#88299,#88300));
#19591=EDGE_LOOP('',(#88301,#88302,#88303,#88304));
#19592=EDGE_LOOP('',(#88305,#88306,#88307,#88308));
#19593=EDGE_LOOP('',(#88309,#88310,#88311,#88312));
#19594=EDGE_LOOP('',(#88313,#88314,#88315,#88316));
#19595=EDGE_LOOP('',(#88317,#88318,#88319,#88320));
#19596=EDGE_LOOP('',(#88321,#88322,#88323,#88324));
#19597=EDGE_LOOP('',(#88325,#88326,#88327,#88328));
#19598=EDGE_LOOP('',(#88329,#88330,#88331,#88332));
#19599=EDGE_LOOP('',(#88333,#88334,#88335,#88336));
#19600=EDGE_LOOP('',(#88337,#88338,#88339,#88340));
#19601=EDGE_LOOP('',(#88341,#88342,#88343,#88344));
#19602=EDGE_LOOP('',(#88345,#88346,#88347,#88348));
#19603=EDGE_LOOP('',(#88349,#88350,#88351,#88352));
#19604=EDGE_LOOP('',(#88353,#88354,#88355,#88356));
#19605=EDGE_LOOP('',(#88357,#88358,#88359,#88360));
#19606=EDGE_LOOP('',(#88361,#88362,#88363,#88364));
#19607=EDGE_LOOP('',(#88365,#88366,#88367,#88368));
#19608=EDGE_LOOP('',(#88369,#88370,#88371,#88372));
#19609=EDGE_LOOP('',(#88373,#88374,#88375,#88376));
#19610=EDGE_LOOP('',(#88377,#88378,#88379,#88380));
#19611=EDGE_LOOP('',(#88381,#88382,#88383,#88384));
#19612=EDGE_LOOP('',(#88385,#88386,#88387,#88388));
#19613=EDGE_LOOP('',(#88389,#88390,#88391,#88392));
#19614=EDGE_LOOP('',(#88393,#88394,#88395,#88396));
#19615=EDGE_LOOP('',(#88397,#88398,#88399,#88400));
#19616=EDGE_LOOP('',(#88401,#88402,#88403,#88404));
#19617=EDGE_LOOP('',(#88405,#88406,#88407,#88408));
#19618=EDGE_LOOP('',(#88409,#88410,#88411,#88412));
#19619=EDGE_LOOP('',(#88413,#88414,#88415,#88416));
#19620=EDGE_LOOP('',(#88417,#88418,#88419,#88420));
#19621=EDGE_LOOP('',(#88421,#88422,#88423,#88424));
#19622=EDGE_LOOP('',(#88425,#88426,#88427,#88428));
#19623=EDGE_LOOP('',(#88429,#88430,#88431,#88432));
#19624=EDGE_LOOP('',(#88433,#88434,#88435,#88436));
#19625=EDGE_LOOP('',(#88437,#88438,#88439,#88440));
#19626=EDGE_LOOP('',(#88441,#88442,#88443,#88444));
#19627=EDGE_LOOP('',(#88445,#88446,#88447,#88448));
#19628=EDGE_LOOP('',(#88449,#88450,#88451,#88452));
#19629=EDGE_LOOP('',(#88453,#88454,#88455,#88456));
#19630=EDGE_LOOP('',(#88457,#88458,#88459,#88460));
#19631=EDGE_LOOP('',(#88461,#88462,#88463,#88464));
#19632=EDGE_LOOP('',(#88465,#88466,#88467,#88468));
#19633=EDGE_LOOP('',(#88469,#88470,#88471,#88472));
#19634=EDGE_LOOP('',(#88473,#88474,#88475,#88476));
#19635=EDGE_LOOP('',(#88477,#88478,#88479,#88480));
#19636=EDGE_LOOP('',(#88481,#88482,#88483,#88484));
#19637=EDGE_LOOP('',(#88485,#88486,#88487,#88488));
#19638=EDGE_LOOP('',(#88489,#88490,#88491,#88492));
#19639=EDGE_LOOP('',(#88493,#88494,#88495,#88496));
#19640=EDGE_LOOP('',(#88497,#88498,#88499,#88500));
#19641=EDGE_LOOP('',(#88501,#88502,#88503,#88504));
#19642=EDGE_LOOP('',(#88505,#88506,#88507,#88508));
#19643=EDGE_LOOP('',(#88509,#88510,#88511,#88512,#88513,#88514,#88515,#88516,
#88517,#88518,#88519,#88520,#88521,#88522,#88523,#88524));
#19644=EDGE_LOOP('',(#88525,#88526,#88527,#88528));
#19645=EDGE_LOOP('',(#88529,#88530,#88531,#88532));
#19646=EDGE_LOOP('',(#88533,#88534,#88535,#88536));
#19647=EDGE_LOOP('',(#88537,#88538,#88539,#88540));
#19648=EDGE_LOOP('',(#88541,#88542,#88543,#88544));
#19649=EDGE_LOOP('',(#88545,#88546,#88547,#88548));
#19650=EDGE_LOOP('',(#88549,#88550,#88551,#88552));
#19651=EDGE_LOOP('',(#88553,#88554,#88555,#88556));
#19652=EDGE_LOOP('',(#88557,#88558,#88559,#88560));
#19653=EDGE_LOOP('',(#88561,#88562,#88563,#88564));
#19654=EDGE_LOOP('',(#88565,#88566,#88567,#88568));
#19655=EDGE_LOOP('',(#88569,#88570,#88571,#88572));
#19656=EDGE_LOOP('',(#88573,#88574,#88575,#88576));
#19657=EDGE_LOOP('',(#88577,#88578,#88579,#88580));
#19658=EDGE_LOOP('',(#88581,#88582,#88583,#88584));
#19659=EDGE_LOOP('',(#88585,#88586,#88587,#88588,#88589,#88590,#88591,#88592,
#88593,#88594,#88595,#88596,#88597,#88598,#88599,#88600));
#19660=EDGE_LOOP('',(#88601,#88602,#88603,#88604,#88605,#88606,#88607,#88608));
#19661=EDGE_LOOP('',(#88609,#88610,#88611,#88612));
#19662=EDGE_LOOP('',(#88613,#88614,#88615,#88616));
#19663=EDGE_LOOP('',(#88617,#88618,#88619,#88620));
#19664=EDGE_LOOP('',(#88621,#88622,#88623,#88624));
#19665=EDGE_LOOP('',(#88625,#88626,#88627,#88628));
#19666=EDGE_LOOP('',(#88629,#88630,#88631,#88632));
#19667=EDGE_LOOP('',(#88633,#88634,#88635,#88636));
#19668=EDGE_LOOP('',(#88637,#88638,#88639,#88640));
#19669=EDGE_LOOP('',(#88641,#88642,#88643,#88644,#88645,#88646,#88647,#88648));
#19670=EDGE_LOOP('',(#88649,#88650,#88651,#88652));
#19671=EDGE_LOOP('',(#88653,#88654,#88655,#88656,#88657,#88658,#88659,#88660,
#88661,#88662,#88663,#88664,#88665,#88666,#88667,#88668));
#19672=EDGE_LOOP('',(#88669,#88670,#88671,#88672));
#19673=EDGE_LOOP('',(#88673,#88674,#88675,#88676));
#19674=EDGE_LOOP('',(#88677,#88678,#88679,#88680));
#19675=EDGE_LOOP('',(#88681,#88682,#88683,#88684));
#19676=EDGE_LOOP('',(#88685,#88686,#88687,#88688));
#19677=EDGE_LOOP('',(#88689,#88690,#88691,#88692));
#19678=EDGE_LOOP('',(#88693,#88694,#88695,#88696));
#19679=EDGE_LOOP('',(#88697,#88698,#88699,#88700));
#19680=EDGE_LOOP('',(#88701,#88702,#88703,#88704));
#19681=EDGE_LOOP('',(#88705,#88706,#88707,#88708));
#19682=EDGE_LOOP('',(#88709,#88710,#88711,#88712));
#19683=EDGE_LOOP('',(#88713,#88714,#88715,#88716));
#19684=EDGE_LOOP('',(#88717,#88718,#88719,#88720));
#19685=EDGE_LOOP('',(#88721,#88722,#88723,#88724));
#19686=EDGE_LOOP('',(#88725,#88726,#88727,#88728));
#19687=EDGE_LOOP('',(#88729,#88730,#88731,#88732,#88733,#88734,#88735,#88736,
#88737,#88738,#88739,#88740,#88741,#88742,#88743,#88744));
#19688=EDGE_LOOP('',(#88745,#88746,#88747,#88748,#88749,#88750,#88751,#88752));
#19689=EDGE_LOOP('',(#88753,#88754,#88755,#88756));
#19690=EDGE_LOOP('',(#88757,#88758,#88759,#88760));
#19691=EDGE_LOOP('',(#88761,#88762,#88763,#88764));
#19692=EDGE_LOOP('',(#88765,#88766,#88767,#88768));
#19693=EDGE_LOOP('',(#88769,#88770,#88771,#88772));
#19694=EDGE_LOOP('',(#88773,#88774,#88775,#88776));
#19695=EDGE_LOOP('',(#88777,#88778,#88779,#88780));
#19696=EDGE_LOOP('',(#88781,#88782,#88783,#88784));
#19697=EDGE_LOOP('',(#88785,#88786,#88787,#88788,#88789,#88790,#88791,#88792));
#19698=EDGE_LOOP('',(#88793,#88794,#88795,#88796));
#19699=EDGE_LOOP('',(#88797,#88798,#88799,#88800,#88801,#88802,#88803,#88804,
#88805,#88806,#88807,#88808,#88809,#88810,#88811,#88812));
#19700=EDGE_LOOP('',(#88813,#88814,#88815,#88816));
#19701=EDGE_LOOP('',(#88817,#88818,#88819,#88820));
#19702=EDGE_LOOP('',(#88821,#88822,#88823,#88824));
#19703=EDGE_LOOP('',(#88825,#88826,#88827,#88828));
#19704=EDGE_LOOP('',(#88829,#88830,#88831,#88832));
#19705=EDGE_LOOP('',(#88833,#88834,#88835,#88836));
#19706=EDGE_LOOP('',(#88837,#88838,#88839,#88840));
#19707=EDGE_LOOP('',(#88841,#88842,#88843,#88844));
#19708=EDGE_LOOP('',(#88845,#88846,#88847,#88848));
#19709=EDGE_LOOP('',(#88849,#88850,#88851,#88852));
#19710=EDGE_LOOP('',(#88853,#88854,#88855,#88856));
#19711=EDGE_LOOP('',(#88857,#88858,#88859,#88860));
#19712=EDGE_LOOP('',(#88861,#88862,#88863,#88864));
#19713=EDGE_LOOP('',(#88865,#88866,#88867,#88868));
#19714=EDGE_LOOP('',(#88869,#88870,#88871,#88872));
#19715=EDGE_LOOP('',(#88873,#88874,#88875,#88876,#88877,#88878,#88879,#88880,
#88881,#88882,#88883,#88884,#88885,#88886,#88887,#88888));
#19716=EDGE_LOOP('',(#88889,#88890,#88891,#88892,#88893,#88894,#88895,#88896));
#19717=EDGE_LOOP('',(#88897,#88898,#88899,#88900));
#19718=EDGE_LOOP('',(#88901,#88902,#88903,#88904));
#19719=EDGE_LOOP('',(#88905,#88906,#88907,#88908));
#19720=EDGE_LOOP('',(#88909,#88910,#88911,#88912));
#19721=EDGE_LOOP('',(#88913,#88914,#88915,#88916));
#19722=EDGE_LOOP('',(#88917,#88918,#88919,#88920));
#19723=EDGE_LOOP('',(#88921,#88922,#88923,#88924));
#19724=EDGE_LOOP('',(#88925,#88926,#88927,#88928));
#19725=EDGE_LOOP('',(#88929,#88930,#88931,#88932,#88933,#88934,#88935,#88936));
#19726=EDGE_LOOP('',(#88937,#88938,#88939,#88940));
#19727=EDGE_LOOP('',(#88941,#88942,#88943,#88944));
#19728=EDGE_LOOP('',(#88945,#88946,#88947,#88948));
#19729=EDGE_LOOP('',(#88949,#88950,#88951,#88952));
#19730=EDGE_LOOP('',(#88953,#88954,#88955,#88956));
#19731=EDGE_LOOP('',(#88957,#88958,#88959,#88960));
#19732=EDGE_LOOP('',(#88961,#88962,#88963,#88964));
#19733=EDGE_LOOP('',(#88965,#88966,#88967,#88968));
#19734=EDGE_LOOP('',(#88969,#88970,#88971,#88972));
#19735=EDGE_LOOP('',(#88973,#88974,#88975,#88976));
#19736=EDGE_LOOP('',(#88977,#88978,#88979,#88980));
#19737=EDGE_LOOP('',(#88981,#88982,#88983,#88984));
#19738=EDGE_LOOP('',(#88985,#88986,#88987,#88988));
#19739=EDGE_LOOP('',(#88989,#88990,#88991,#88992));
#19740=EDGE_LOOP('',(#88993,#88994,#88995,#88996));
#19741=EDGE_LOOP('',(#88997,#88998,#88999,#89000));
#19742=EDGE_LOOP('',(#89001,#89002,#89003,#89004));
#19743=EDGE_LOOP('',(#89005,#89006,#89007,#89008));
#19744=EDGE_LOOP('',(#89009,#89010,#89011,#89012));
#19745=EDGE_LOOP('',(#89013,#89014,#89015,#89016));
#19746=EDGE_LOOP('',(#89017,#89018,#89019,#89020));
#19747=EDGE_LOOP('',(#89021,#89022,#89023,#89024));
#19748=EDGE_LOOP('',(#89025,#89026,#89027,#89028));
#19749=EDGE_LOOP('',(#89029,#89030,#89031,#89032));
#19750=EDGE_LOOP('',(#89033,#89034,#89035,#89036));
#19751=EDGE_LOOP('',(#89037,#89038,#89039,#89040));
#19752=EDGE_LOOP('',(#89041,#89042,#89043,#89044));
#19753=EDGE_LOOP('',(#89045,#89046,#89047,#89048));
#19754=EDGE_LOOP('',(#89049,#89050,#89051,#89052));
#19755=EDGE_LOOP('',(#89053,#89054,#89055,#89056));
#19756=EDGE_LOOP('',(#89057,#89058,#89059,#89060));
#19757=EDGE_LOOP('',(#89061,#89062,#89063,#89064));
#19758=EDGE_LOOP('',(#89065,#89066,#89067,#89068));
#19759=EDGE_LOOP('',(#89069,#89070,#89071,#89072));
#19760=EDGE_LOOP('',(#89073,#89074,#89075,#89076));
#19761=EDGE_LOOP('',(#89077,#89078,#89079,#89080));
#19762=EDGE_LOOP('',(#89081,#89082,#89083,#89084));
#19763=EDGE_LOOP('',(#89085,#89086,#89087,#89088));
#19764=EDGE_LOOP('',(#89089,#89090,#89091,#89092));
#19765=EDGE_LOOP('',(#89093,#89094,#89095,#89096));
#19766=EDGE_LOOP('',(#89097,#89098,#89099,#89100));
#19767=EDGE_LOOP('',(#89101,#89102,#89103,#89104));
#19768=EDGE_LOOP('',(#89105,#89106,#89107,#89108));
#19769=EDGE_LOOP('',(#89109,#89110,#89111,#89112));
#19770=EDGE_LOOP('',(#89113,#89114,#89115,#89116));
#19771=EDGE_LOOP('',(#89117,#89118,#89119,#89120));
#19772=EDGE_LOOP('',(#89121,#89122,#89123,#89124));
#19773=EDGE_LOOP('',(#89125,#89126,#89127,#89128));
#19774=EDGE_LOOP('',(#89129,#89130,#89131,#89132));
#19775=EDGE_LOOP('',(#89133,#89134,#89135,#89136));
#19776=EDGE_LOOP('',(#89137,#89138,#89139,#89140));
#19777=EDGE_LOOP('',(#89141,#89142,#89143,#89144));
#19778=EDGE_LOOP('',(#89145,#89146,#89147,#89148));
#19779=EDGE_LOOP('',(#89149,#89150,#89151,#89152));
#19780=EDGE_LOOP('',(#89153,#89154,#89155,#89156));
#19781=EDGE_LOOP('',(#89157,#89158,#89159,#89160));
#19782=EDGE_LOOP('',(#89161,#89162,#89163,#89164));
#19783=EDGE_LOOP('',(#89165,#89166,#89167,#89168));
#19784=EDGE_LOOP('',(#89169,#89170,#89171,#89172));
#19785=EDGE_LOOP('',(#89173,#89174,#89175,#89176));
#19786=EDGE_LOOP('',(#89177,#89178,#89179,#89180));
#19787=EDGE_LOOP('',(#89181,#89182,#89183,#89184));
#19788=EDGE_LOOP('',(#89185,#89186,#89187,#89188));
#19789=EDGE_LOOP('',(#89189,#89190,#89191,#89192));
#19790=EDGE_LOOP('',(#89193,#89194,#89195,#89196));
#19791=EDGE_LOOP('',(#89197,#89198,#89199,#89200));
#19792=EDGE_LOOP('',(#89201,#89202,#89203,#89204));
#19793=EDGE_LOOP('',(#89205,#89206,#89207,#89208));
#19794=EDGE_LOOP('',(#89209,#89210,#89211,#89212));
#19795=EDGE_LOOP('',(#89213,#89214,#89215,#89216));
#19796=EDGE_LOOP('',(#89217,#89218,#89219,#89220));
#19797=EDGE_LOOP('',(#89221,#89222,#89223,#89224));
#19798=EDGE_LOOP('',(#89225,#89226,#89227,#89228));
#19799=EDGE_LOOP('',(#89229,#89230,#89231,#89232));
#19800=EDGE_LOOP('',(#89233,#89234,#89235,#89236));
#19801=EDGE_LOOP('',(#89237,#89238,#89239,#89240));
#19802=EDGE_LOOP('',(#89241,#89242,#89243,#89244));
#19803=EDGE_LOOP('',(#89245,#89246,#89247,#89248));
#19804=EDGE_LOOP('',(#89249,#89250,#89251,#89252));
#19805=EDGE_LOOP('',(#89253,#89254,#89255,#89256));
#19806=EDGE_LOOP('',(#89257,#89258,#89259,#89260));
#19807=EDGE_LOOP('',(#89261,#89262,#89263,#89264));
#19808=EDGE_LOOP('',(#89265,#89266,#89267,#89268));
#19809=EDGE_LOOP('',(#89269,#89270,#89271,#89272));
#19810=EDGE_LOOP('',(#89273,#89274,#89275,#89276));
#19811=EDGE_LOOP('',(#89277,#89278,#89279,#89280));
#19812=EDGE_LOOP('',(#89281,#89282,#89283,#89284));
#19813=EDGE_LOOP('',(#89285,#89286,#89287,#89288));
#19814=EDGE_LOOP('',(#89289,#89290,#89291,#89292));
#19815=EDGE_LOOP('',(#89293,#89294,#89295,#89296));
#19816=EDGE_LOOP('',(#89297,#89298,#89299,#89300));
#19817=EDGE_LOOP('',(#89301,#89302,#89303,#89304));
#19818=EDGE_LOOP('',(#89305,#89306,#89307,#89308));
#19819=EDGE_LOOP('',(#89309,#89310,#89311,#89312));
#19820=EDGE_LOOP('',(#89313,#89314,#89315,#89316));
#19821=EDGE_LOOP('',(#89317,#89318,#89319,#89320));
#19822=EDGE_LOOP('',(#89321,#89322,#89323,#89324));
#19823=EDGE_LOOP('',(#89325,#89326,#89327,#89328));
#19824=EDGE_LOOP('',(#89329,#89330,#89331,#89332));
#19825=EDGE_LOOP('',(#89333,#89334,#89335,#89336));
#19826=EDGE_LOOP('',(#89337,#89338,#89339,#89340));
#19827=EDGE_LOOP('',(#89341,#89342,#89343,#89344));
#19828=EDGE_LOOP('',(#89345,#89346,#89347,#89348));
#19829=EDGE_LOOP('',(#89349,#89350,#89351,#89352));
#19830=EDGE_LOOP('',(#89353,#89354,#89355,#89356));
#19831=EDGE_LOOP('',(#89357,#89358,#89359,#89360));
#19832=EDGE_LOOP('',(#89361,#89362,#89363,#89364));
#19833=EDGE_LOOP('',(#89365,#89366,#89367,#89368));
#19834=EDGE_LOOP('',(#89369,#89370,#89371,#89372));
#19835=EDGE_LOOP('',(#89373,#89374,#89375,#89376));
#19836=EDGE_LOOP('',(#89377,#89378,#89379,#89380));
#19837=EDGE_LOOP('',(#89381,#89382,#89383,#89384));
#19838=EDGE_LOOP('',(#89385,#89386,#89387,#89388));
#19839=EDGE_LOOP('',(#89389,#89390,#89391,#89392));
#19840=EDGE_LOOP('',(#89393,#89394,#89395,#89396));
#19841=EDGE_LOOP('',(#89397,#89398,#89399,#89400));
#19842=EDGE_LOOP('',(#89401,#89402,#89403,#89404));
#19843=EDGE_LOOP('',(#89405,#89406,#89407,#89408));
#19844=EDGE_LOOP('',(#89409,#89410,#89411,#89412));
#19845=EDGE_LOOP('',(#89413,#89414,#89415,#89416));
#19846=EDGE_LOOP('',(#89417,#89418,#89419,#89420));
#19847=EDGE_LOOP('',(#89421,#89422,#89423,#89424));
#19848=EDGE_LOOP('',(#89425,#89426,#89427,#89428));
#19849=EDGE_LOOP('',(#89429,#89430,#89431,#89432));
#19850=EDGE_LOOP('',(#89433,#89434,#89435,#89436));
#19851=EDGE_LOOP('',(#89437,#89438,#89439,#89440));
#19852=EDGE_LOOP('',(#89441,#89442,#89443,#89444));
#19853=EDGE_LOOP('',(#89445,#89446,#89447,#89448));
#19854=EDGE_LOOP('',(#89449,#89450,#89451,#89452));
#19855=EDGE_LOOP('',(#89453,#89454,#89455,#89456));
#19856=EDGE_LOOP('',(#89457,#89458,#89459,#89460));
#19857=EDGE_LOOP('',(#89461,#89462,#89463,#89464));
#19858=EDGE_LOOP('',(#89465,#89466,#89467,#89468));
#19859=EDGE_LOOP('',(#89469,#89470,#89471,#89472));
#19860=EDGE_LOOP('',(#89473,#89474,#89475,#89476));
#19861=EDGE_LOOP('',(#89477,#89478,#89479,#89480));
#19862=EDGE_LOOP('',(#89481,#89482,#89483,#89484));
#19863=EDGE_LOOP('',(#89485,#89486,#89487,#89488));
#19864=EDGE_LOOP('',(#89489,#89490,#89491,#89492));
#19865=EDGE_LOOP('',(#89493,#89494,#89495,#89496));
#19866=EDGE_LOOP('',(#89497,#89498,#89499,#89500));
#19867=EDGE_LOOP('',(#89501,#89502,#89503,#89504));
#19868=EDGE_LOOP('',(#89505,#89506,#89507,#89508));
#19869=EDGE_LOOP('',(#89509,#89510,#89511,#89512));
#19870=EDGE_LOOP('',(#89513,#89514,#89515,#89516));
#19871=EDGE_LOOP('',(#89517,#89518,#89519,#89520));
#19872=EDGE_LOOP('',(#89521,#89522,#89523,#89524));
#19873=EDGE_LOOP('',(#89525,#89526,#89527,#89528));
#19874=EDGE_LOOP('',(#89529,#89530,#89531,#89532));
#19875=EDGE_LOOP('',(#89533,#89534,#89535,#89536));
#19876=EDGE_LOOP('',(#89537,#89538,#89539,#89540));
#19877=EDGE_LOOP('',(#89541,#89542,#89543,#89544));
#19878=EDGE_LOOP('',(#89545,#89546,#89547,#89548));
#19879=EDGE_LOOP('',(#89549,#89550,#89551,#89552));
#19880=EDGE_LOOP('',(#89553,#89554,#89555,#89556));
#19881=EDGE_LOOP('',(#89557,#89558,#89559,#89560));
#19882=EDGE_LOOP('',(#89561,#89562,#89563,#89564));
#19883=EDGE_LOOP('',(#89565,#89566,#89567,#89568));
#19884=EDGE_LOOP('',(#89569,#89570,#89571,#89572));
#19885=EDGE_LOOP('',(#89573,#89574,#89575,#89576));
#19886=EDGE_LOOP('',(#89577,#89578,#89579,#89580));
#19887=EDGE_LOOP('',(#89581,#89582,#89583,#89584));
#19888=EDGE_LOOP('',(#89585,#89586,#89587,#89588));
#19889=EDGE_LOOP('',(#89589,#89590,#89591,#89592));
#19890=EDGE_LOOP('',(#89593,#89594,#89595,#89596));
#19891=EDGE_LOOP('',(#89597,#89598,#89599,#89600));
#19892=EDGE_LOOP('',(#89601,#89602,#89603,#89604));
#19893=EDGE_LOOP('',(#89605,#89606,#89607,#89608));
#19894=EDGE_LOOP('',(#89609,#89610,#89611,#89612));
#19895=EDGE_LOOP('',(#89613,#89614,#89615,#89616));
#19896=EDGE_LOOP('',(#89617,#89618,#89619,#89620));
#19897=EDGE_LOOP('',(#89621,#89622,#89623,#89624));
#19898=EDGE_LOOP('',(#89625,#89626,#89627,#89628));
#19899=EDGE_LOOP('',(#89629,#89630,#89631,#89632));
#19900=EDGE_LOOP('',(#89633,#89634,#89635,#89636));
#19901=EDGE_LOOP('',(#89637,#89638,#89639,#89640));
#19902=EDGE_LOOP('',(#89641,#89642,#89643,#89644));
#19903=EDGE_LOOP('',(#89645,#89646,#89647,#89648));
#19904=EDGE_LOOP('',(#89649,#89650,#89651,#89652));
#19905=EDGE_LOOP('',(#89653,#89654,#89655,#89656));
#19906=EDGE_LOOP('',(#89657,#89658,#89659,#89660));
#19907=EDGE_LOOP('',(#89661,#89662,#89663,#89664));
#19908=EDGE_LOOP('',(#89665,#89666,#89667,#89668));
#19909=EDGE_LOOP('',(#89669,#89670,#89671,#89672));
#19910=EDGE_LOOP('',(#89673,#89674,#89675,#89676));
#19911=EDGE_LOOP('',(#89677,#89678,#89679,#89680));
#19912=EDGE_LOOP('',(#89681,#89682,#89683,#89684));
#19913=EDGE_LOOP('',(#89685,#89686,#89687,#89688));
#19914=EDGE_LOOP('',(#89689,#89690,#89691,#89692));
#19915=EDGE_LOOP('',(#89693,#89694,#89695,#89696));
#19916=EDGE_LOOP('',(#89697,#89698,#89699,#89700));
#19917=EDGE_LOOP('',(#89701,#89702,#89703,#89704));
#19918=EDGE_LOOP('',(#89705,#89706,#89707,#89708));
#19919=EDGE_LOOP('',(#89709,#89710,#89711,#89712));
#19920=EDGE_LOOP('',(#89713,#89714,#89715,#89716));
#19921=EDGE_LOOP('',(#89717,#89718,#89719,#89720));
#19922=EDGE_LOOP('',(#89721,#89722,#89723,#89724));
#19923=EDGE_LOOP('',(#89725,#89726,#89727,#89728));
#19924=EDGE_LOOP('',(#89729,#89730,#89731,#89732));
#19925=EDGE_LOOP('',(#89733,#89734,#89735,#89736));
#19926=EDGE_LOOP('',(#89737,#89738,#89739,#89740));
#19927=EDGE_LOOP('',(#89741,#89742,#89743,#89744));
#19928=EDGE_LOOP('',(#89745,#89746,#89747,#89748));
#19929=EDGE_LOOP('',(#89749,#89750,#89751,#89752));
#19930=EDGE_LOOP('',(#89753,#89754,#89755,#89756));
#19931=EDGE_LOOP('',(#89757,#89758,#89759,#89760));
#19932=EDGE_LOOP('',(#89761,#89762,#89763,#89764));
#19933=EDGE_LOOP('',(#89765,#89766,#89767,#89768));
#19934=EDGE_LOOP('',(#89769,#89770,#89771,#89772));
#19935=EDGE_LOOP('',(#89773,#89774,#89775,#89776));
#19936=EDGE_LOOP('',(#89777,#89778,#89779,#89780));
#19937=EDGE_LOOP('',(#89781,#89782,#89783,#89784));
#19938=EDGE_LOOP('',(#89785,#89786,#89787,#89788));
#19939=EDGE_LOOP('',(#89789,#89790,#89791,#89792));
#19940=EDGE_LOOP('',(#89793,#89794,#89795,#89796,#89797,#89798,#89799,#89800));
#19941=EDGE_LOOP('',(#89801,#89802,#89803,#89804));
#19942=EDGE_LOOP('',(#89805,#89806,#89807,#89808));
#19943=EDGE_LOOP('',(#89809,#89810,#89811,#89812));
#19944=EDGE_LOOP('',(#89813,#89814,#89815,#89816));
#19945=EDGE_LOOP('',(#89817,#89818,#89819,#89820));
#19946=EDGE_LOOP('',(#89821,#89822,#89823,#89824));
#19947=EDGE_LOOP('',(#89825,#89826,#89827,#89828));
#19948=EDGE_LOOP('',(#89829,#89830,#89831,#89832));
#19949=EDGE_LOOP('',(#89833,#89834,#89835,#89836,#89837,#89838,#89839,#89840));
#19950=EDGE_LOOP('',(#89841,#89842,#89843,#89844,#89845,#89846,#89847,#89848,
#89849,#89850,#89851,#89852,#89853,#89854,#89855,#89856,#89857,#89858,#89859,
#89860,#89861,#89862,#89863,#89864,#89865,#89866,#89867,#89868,#89869,#89870,
#89871,#89872,#89873,#89874,#89875,#89876,#89877,#89878,#89879,#89880,#89881,
#89882,#89883,#89884,#89885,#89886,#89887,#89888,#89889,#89890,#89891,#89892,
#89893,#89894,#89895,#89896,#89897,#89898,#89899,#89900,#89901,#89902,#89903,
#89904,#89905,#89906,#89907,#89908,#89909,#89910,#89911,#89912,#89913,#89914,
#89915,#89916,#89917,#89918,#89919,#89920,#89921,#89922,#89923,#89924,#89925,
#89926,#89927,#89928,#89929,#89930,#89931,#89932,#89933,#89934,#89935,#89936,
#89937,#89938,#89939,#89940,#89941,#89942,#89943,#89944,#89945,#89946,#89947,
#89948,#89949,#89950,#89951,#89952,#89953,#89954,#89955,#89956,#89957,#89958,
#89959,#89960,#89961,#89962,#89963,#89964,#89965,#89966,#89967,#89968,#89969,
#89970,#89971,#89972,#89973,#89974,#89975,#89976,#89977,#89978,#89979,#89980,
#89981,#89982,#89983,#89984,#89985,#89986,#89987,#89988,#89989,#89990,#89991,
#89992,#89993,#89994,#89995,#89996,#89997,#89998,#89999,#90000,#90001,#90002,
#90003,#90004,#90005,#90006,#90007,#90008,#90009,#90010,#90011,#90012,#90013,
#90014,#90015,#90016,#90017,#90018,#90019,#90020,#90021,#90022,#90023,#90024,
#90025,#90026,#90027,#90028,#90029,#90030,#90031,#90032,#90033,#90034,#90035,
#90036,#90037,#90038,#90039,#90040,#90041,#90042,#90043,#90044,#90045,#90046,
#90047,#90048,#90049,#90050,#90051,#90052,#90053,#90054));
#19951=EDGE_LOOP('',(#90055,#90056,#90057,#90058));
#19952=EDGE_LOOP('',(#90059,#90060,#90061,#90062));
#19953=EDGE_LOOP('',(#90063,#90064,#90065,#90066));
#19954=EDGE_LOOP('',(#90067,#90068,#90069,#90070));
#19955=EDGE_LOOP('',(#90071,#90072,#90073,#90074));
#19956=EDGE_LOOP('',(#90075,#90076,#90077,#90078,#90079,#90080,#90081,#90082,
#90083,#90084,#90085,#90086,#90087,#90088,#90089,#90090,#90091,#90092,#90093,
#90094,#90095,#90096,#90097,#90098,#90099,#90100,#90101,#90102,#90103,#90104,
#90105,#90106,#90107,#90108,#90109,#90110,#90111,#90112,#90113,#90114,#90115,
#90116,#90117,#90118,#90119,#90120,#90121,#90122,#90123,#90124,#90125,#90126,
#90127,#90128,#90129,#90130,#90131,#90132,#90133,#90134,#90135,#90136,#90137,
#90138,#90139,#90140,#90141,#90142,#90143,#90144,#90145,#90146,#90147,#90148,
#90149,#90150,#90151,#90152,#90153,#90154,#90155,#90156,#90157,#90158,#90159,
#90160,#90161,#90162,#90163,#90164,#90165,#90166,#90167,#90168,#90169,#90170,
#90171,#90172,#90173,#90174,#90175,#90176,#90177,#90178,#90179,#90180,#90181,
#90182,#90183,#90184,#90185,#90186,#90187,#90188,#90189,#90190,#90191,#90192,
#90193,#90194,#90195,#90196,#90197,#90198,#90199,#90200,#90201,#90202,#90203,
#90204,#90205,#90206,#90207,#90208,#90209,#90210,#90211,#90212,#90213,#90214,
#90215,#90216,#90217,#90218,#90219,#90220,#90221,#90222,#90223,#90224,#90225,
#90226,#90227,#90228,#90229,#90230,#90231,#90232,#90233,#90234,#90235,#90236,
#90237,#90238,#90239,#90240,#90241,#90242,#90243,#90244,#90245,#90246,#90247,
#90248,#90249,#90250,#90251,#90252,#90253,#90254,#90255,#90256,#90257,#90258,
#90259,#90260,#90261,#90262,#90263,#90264,#90265,#90266,#90267,#90268,#90269,
#90270,#90271,#90272,#90273,#90274,#90275,#90276,#90277,#90278,#90279,#90280,
#90281,#90282,#90283,#90284,#90285,#90286,#90287,#90288));
#19957=EDGE_LOOP('',(#90289,#90290,#90291,#90292));
#19958=LINE('',#142648,#25185);
#19959=LINE('',#142654,#25186);
#19960=LINE('',#142660,#25187);
#19961=LINE('',#142666,#25188);
#19962=LINE('',#142671,#25189);
#19963=LINE('',#142673,#25190);
#19964=LINE('',#142675,#25191);
#19965=LINE('',#142676,#25192);
#19966=LINE('',#142679,#25193);
#19967=LINE('',#142681,#25194);
#19968=LINE('',#142682,#25195);
#19969=LINE('',#142685,#25196);
#19970=LINE('',#142687,#25197);
#19971=LINE('',#142688,#25198);
#19972=LINE('',#142690,#25199);
#19973=LINE('',#142691,#25200);
#19974=LINE('',#142695,#25201);
#19975=LINE('',#142697,#25202);
#19976=LINE('',#142699,#25203);
#19977=LINE('',#142700,#25204);
#19978=LINE('',#142703,#25205);
#19979=LINE('',#142705,#25206);
#19980=LINE('',#142706,#25207);
#19981=LINE('',#142709,#25208);
#19982=LINE('',#142710,#25209);
#19983=LINE('',#142713,#25210);
#19984=LINE('',#142714,#25211);
#19985=LINE('',#142716,#25212);
#19986=LINE('',#142719,#25213);
#19987=LINE('',#142721,#25214);
#19988=LINE('',#142722,#25215);
#19989=LINE('',#142725,#25216);
#19990=LINE('',#142726,#25217);
#19991=LINE('',#142729,#25218);
#19992=LINE('',#142730,#25219);
#19993=LINE('',#142732,#25220);
#19994=LINE('',#142735,#25221);
#19995=LINE('',#142737,#25222);
#19996=LINE('',#142738,#25223);
#19997=LINE('',#142741,#25224);
#19998=LINE('',#142742,#25225);
#19999=LINE('',#142745,#25226);
#20000=LINE('',#142746,#25227);
#20001=LINE('',#142748,#25228);
#20002=LINE('',#142751,#25229);
#20003=LINE('',#142753,#25230);
#20004=LINE('',#142754,#25231);
#20005=LINE('',#142757,#25232);
#20006=LINE('',#142758,#25233);
#20007=LINE('',#142761,#25234);
#20008=LINE('',#142762,#25235);
#20009=LINE('',#142764,#25236);
#20010=LINE('',#142768,#25237);
#20011=LINE('',#142772,#25238);
#20012=LINE('',#142776,#25239);
#20013=LINE('',#142780,#25240);
#20014=LINE('',#142785,#25241);
#20015=LINE('',#142789,#25242);
#20016=LINE('',#142793,#25243);
#20017=LINE('',#142797,#25244);
#20018=LINE('',#142801,#25245);
#20019=LINE('',#142803,#25246);
#20020=LINE('',#142804,#25247);
#20021=LINE('',#142807,#25248);
#20022=LINE('',#142809,#25249);
#20023=LINE('',#142810,#25250);
#20024=LINE('',#142813,#25251);
#20025=LINE('',#142815,#25252);
#20026=LINE('',#142816,#25253);
#20027=LINE('',#142819,#25254);
#20028=LINE('',#142821,#25255);
#20029=LINE('',#142822,#25256);
#20030=LINE('',#142886,#25257);
#20031=LINE('',#142964,#25258);
#20032=LINE('',#143043,#25259);
#20033=LINE('',#143123,#25260);
#20034=LINE('',#143183,#25261);
#20035=LINE('',#143184,#25262);
#20036=LINE('',#143186,#25263);
#20037=LINE('',#143188,#25264);
#20038=LINE('',#143195,#25265);
#20039=LINE('',#143233,#25266);
#20040=LINE('',#143272,#25267);
#20041=LINE('',#143414,#25268);
#20042=LINE('',#143556,#25269);
#20043=LINE('',#143698,#25270);
#20044=LINE('',#143840,#25271);
#20045=LINE('',#143982,#25272);
#20046=LINE('',#144124,#25273);
#20047=LINE('',#144266,#25274);
#20048=LINE('',#144296,#25275);
#20049=LINE('',#144298,#25276);
#20050=LINE('',#144396,#25277);
#20051=LINE('',#144510,#25278);
#20052=LINE('',#144566,#25279);
#20053=LINE('',#144622,#25280);
#20054=LINE('',#144678,#25281);
#20055=LINE('',#144734,#25282);
#20056=LINE('',#144790,#25283);
#20057=LINE('',#144846,#25284);
#20058=LINE('',#144903,#25285);
#20059=LINE('',#144973,#25286);
#20060=LINE('',#145045,#25287);
#20061=LINE('',#145117,#25288);
#20062=LINE('',#145189,#25289);
#20063=LINE('',#145261,#25290);
#20064=LINE('',#145333,#25291);
#20065=LINE('',#145404,#25292);
#20066=LINE('',#145463,#25293);
#20067=LINE('',#145484,#25294);
#20068=LINE('',#145545,#25295);
#20069=LINE('',#145577,#25296);
#20070=LINE('',#145811,#25297);
#20071=LINE('',#145813,#25298);
#20072=LINE('',#150387,#25299);
#20073=LINE('',#154421,#25300);
#20074=LINE('',#158490,#25301);
#20075=LINE('',#158528,#25302);
#20076=LINE('',#162563,#25303);
#20077=LINE('',#167138,#25304);
#20078=LINE('',#167167,#25305);
#20079=LINE('',#167179,#25306);
#20080=LINE('',#167194,#25307);
#20081=LINE('',#167227,#25308);
#20082=LINE('',#167242,#25309);
#20083=LINE('',#167254,#25310);
#20084=LINE('',#167448,#25311);
#20085=LINE('',#167450,#25312);
#20086=LINE('',#167451,#25313);
#20087=LINE('',#167453,#25314);
#20088=LINE('',#167454,#25315);
#20089=LINE('',#167456,#25316);
#20090=LINE('',#167457,#25317);
#20091=LINE('',#167459,#25318);
#20092=LINE('',#167460,#25319);
#20093=LINE('',#167462,#25320);
#20094=LINE('',#167472,#25321);
#20095=LINE('',#167478,#25322);
#20096=LINE('',#167486,#25323);
#20097=LINE('',#167492,#25324);
#20098=LINE('',#167500,#25325);
#20099=LINE('',#167506,#25326);
#20100=LINE('',#167514,#25327);
#20101=LINE('',#167520,#25328);
#20102=LINE('',#167543,#25329);
#20103=LINE('',#167546,#25330);
#20104=LINE('',#167569,#25331);
#20105=LINE('',#167572,#25332);
#20106=LINE('',#167580,#25333);
#20107=LINE('',#167586,#25334);
#20108=LINE('',#167660,#25335);
#20109=LINE('',#167663,#25336);
#20110=LINE('',#167713,#25337);
#20111=LINE('',#167717,#25338);
#20112=LINE('',#167806,#25339);
#20113=LINE('',#167810,#25340);
#20114=LINE('',#167899,#25341);
#20115=LINE('',#167903,#25342);
#20116=LINE('',#167992,#25343);
#20117=LINE('',#167996,#25344);
#20118=LINE('',#168085,#25345);
#20119=LINE('',#168089,#25346);
#20120=LINE('',#168178,#25347);
#20121=LINE('',#168182,#25348);
#20122=LINE('',#168271,#25349);
#20123=LINE('',#168275,#25350);
#20124=LINE('',#168364,#25351);
#20125=LINE('',#168368,#25352);
#20126=LINE('',#168457,#25353);
#20127=LINE('',#168461,#25354);
#20128=LINE('',#168550,#25355);
#20129=LINE('',#168554,#25356);
#20130=LINE('',#168643,#25357);
#20131=LINE('',#168647,#25358);
#20132=LINE('',#168736,#25359);
#20133=LINE('',#168740,#25360);
#20134=LINE('',#168829,#25361);
#20135=LINE('',#168833,#25362);
#20136=LINE('',#168922,#25363);
#20137=LINE('',#168926,#25364);
#20138=LINE('',#169015,#25365);
#20139=LINE('',#169019,#25366);
#20140=LINE('',#169108,#25367);
#20141=LINE('',#169112,#25368);
#20142=LINE('',#169201,#25369);
#20143=LINE('',#169205,#25370);
#20144=LINE('',#169294,#25371);
#20145=LINE('',#169298,#25372);
#20146=LINE('',#169387,#25373);
#20147=LINE('',#169391,#25374);
#20148=LINE('',#169480,#25375);
#20149=LINE('',#169484,#25376);
#20150=LINE('',#169573,#25377);
#20151=LINE('',#169577,#25378);
#20152=LINE('',#169666,#25379);
#20153=LINE('',#169670,#25380);
#20154=LINE('',#169759,#25381);
#20155=LINE('',#169763,#25382);
#20156=LINE('',#169852,#25383);
#20157=LINE('',#169856,#25384);
#20158=LINE('',#169945,#25385);
#20159=LINE('',#169949,#25386);
#20160=LINE('',#170038,#25387);
#20161=LINE('',#170042,#25388);
#20162=LINE('',#170131,#25389);
#20163=LINE('',#170135,#25390);
#20164=LINE('',#170224,#25391);
#20165=LINE('',#170228,#25392);
#20166=LINE('',#170317,#25393);
#20167=LINE('',#170321,#25394);
#20168=LINE('',#170410,#25395);
#20169=LINE('',#170414,#25396);
#20170=LINE('',#170455,#25397);
#20171=LINE('',#170501,#25398);
#20172=LINE('',#170505,#25399);
#20173=LINE('',#170594,#25400);
#20174=LINE('',#170598,#25401);
#20175=LINE('',#170687,#25402);
#20176=LINE('',#170691,#25403);
#20177=LINE('',#170780,#25404);
#20178=LINE('',#170784,#25405);
#20179=LINE('',#170873,#25406);
#20180=LINE('',#170877,#25407);
#20181=LINE('',#170966,#25408);
#20182=LINE('',#170970,#25409);
#20183=LINE('',#171059,#25410);
#20184=LINE('',#171063,#25411);
#20185=LINE('',#171152,#25412);
#20186=LINE('',#171156,#25413);
#20187=LINE('',#171245,#25414);
#20188=LINE('',#171249,#25415);
#20189=LINE('',#171338,#25416);
#20190=LINE('',#171342,#25417);
#20191=LINE('',#171431,#25418);
#20192=LINE('',#171435,#25419);
#20193=LINE('',#171524,#25420);
#20194=LINE('',#171528,#25421);
#20195=LINE('',#171617,#25422);
#20196=LINE('',#171621,#25423);
#20197=LINE('',#171710,#25424);
#20198=LINE('',#171714,#25425);
#20199=LINE('',#171803,#25426);
#20200=LINE('',#171807,#25427);
#20201=LINE('',#171893,#25428);
#20202=LINE('',#171897,#25429);
#20203=LINE('',#171986,#25430);
#20204=LINE('',#171990,#25431);
#20205=LINE('',#172079,#25432);
#20206=LINE('',#172083,#25433);
#20207=LINE('',#172172,#25434);
#20208=LINE('',#172176,#25435);
#20209=LINE('',#172265,#25436);
#20210=LINE('',#172269,#25437);
#20211=LINE('',#172358,#25438);
#20212=LINE('',#172362,#25439);
#20213=LINE('',#172451,#25440);
#20214=LINE('',#172455,#25441);
#20215=LINE('',#172544,#25442);
#20216=LINE('',#172548,#25443);
#20217=LINE('',#172637,#25444);
#20218=LINE('',#172641,#25445);
#20219=LINE('',#172730,#25446);
#20220=LINE('',#172734,#25447);
#20221=LINE('',#172823,#25448);
#20222=LINE('',#172827,#25449);
#20223=LINE('',#172916,#25450);
#20224=LINE('',#172920,#25451);
#20225=LINE('',#173009,#25452);
#20226=LINE('',#173013,#25453);
#20227=LINE('',#173102,#25454);
#20228=LINE('',#173106,#25455);
#20229=LINE('',#173195,#25456);
#20230=LINE('',#173199,#25457);
#20231=LINE('',#173280,#25458);
#20232=LINE('',#173284,#25459);
#20233=LINE('',#173367,#25460);
#20234=LINE('',#173371,#25461);
#20235=LINE('',#173454,#25462);
#20236=LINE('',#173458,#25463);
#20237=LINE('',#173541,#25464);
#20238=LINE('',#173545,#25465);
#20239=LINE('',#173628,#25466);
#20240=LINE('',#173632,#25467);
#20241=LINE('',#173715,#25468);
#20242=LINE('',#173719,#25469);
#20243=LINE('',#173802,#25470);
#20244=LINE('',#173806,#25471);
#20245=LINE('',#173889,#25472);
#20246=LINE('',#173893,#25473);
#20247=LINE('',#173976,#25474);
#20248=LINE('',#173980,#25475);
#20249=LINE('',#174063,#25476);
#20250=LINE('',#174067,#25477);
#20251=LINE('',#174150,#25478);
#20252=LINE('',#174154,#25479);
#20253=LINE('',#174237,#25480);
#20254=LINE('',#174241,#25481);
#20255=LINE('',#174324,#25482);
#20256=LINE('',#174328,#25483);
#20257=LINE('',#174411,#25484);
#20258=LINE('',#174415,#25485);
#20259=LINE('',#174498,#25486);
#20260=LINE('',#174502,#25487);
#20261=LINE('',#174585,#25488);
#20262=LINE('',#174589,#25489);
#20263=LINE('',#174672,#25490);
#20264=LINE('',#174676,#25491);
#20265=LINE('',#174759,#25492);
#20266=LINE('',#174763,#25493);
#20267=LINE('',#174846,#25494);
#20268=LINE('',#174850,#25495);
#20269=LINE('',#174933,#25496);
#20270=LINE('',#174937,#25497);
#20271=LINE('',#175020,#25498);
#20272=LINE('',#175024,#25499);
#20273=LINE('',#175107,#25500);
#20274=LINE('',#175111,#25501);
#20275=LINE('',#175194,#25502);
#20276=LINE('',#175198,#25503);
#20277=LINE('',#175281,#25504);
#20278=LINE('',#175285,#25505);
#20279=LINE('',#175368,#25506);
#20280=LINE('',#175372,#25507);
#20281=LINE('',#175455,#25508);
#20282=LINE('',#175459,#25509);
#20283=LINE('',#175542,#25510);
#20284=LINE('',#175546,#25511);
#20285=LINE('',#175629,#25512);
#20286=LINE('',#175633,#25513);
#20287=LINE('',#175716,#25514);
#20288=LINE('',#175720,#25515);
#20289=LINE('',#175803,#25516);
#20290=LINE('',#175807,#25517);
#20291=LINE('',#175851,#25518);
#20292=LINE('',#175893,#25519);
#20293=LINE('',#175897,#25520);
#20294=LINE('',#175980,#25521);
#20295=LINE('',#175984,#25522);
#20296=LINE('',#176067,#25523);
#20297=LINE('',#176071,#25524);
#20298=LINE('',#176154,#25525);
#20299=LINE('',#176158,#25526);
#20300=LINE('',#176241,#25527);
#20301=LINE('',#176245,#25528);
#20302=LINE('',#176328,#25529);
#20303=LINE('',#176332,#25530);
#20304=LINE('',#176415,#25531);
#20305=LINE('',#176419,#25532);
#20306=LINE('',#176502,#25533);
#20307=LINE('',#176506,#25534);
#20308=LINE('',#176589,#25535);
#20309=LINE('',#176593,#25536);
#20310=LINE('',#176676,#25537);
#20311=LINE('',#176680,#25538);
#20312=LINE('',#176763,#25539);
#20313=LINE('',#176767,#25540);
#20314=LINE('',#176850,#25541);
#20315=LINE('',#176854,#25542);
#20316=LINE('',#176937,#25543);
#20317=LINE('',#176941,#25544);
#20318=LINE('',#177024,#25545);
#20319=LINE('',#177028,#25546);
#20320=LINE('',#177111,#25547);
#20321=LINE('',#177115,#25548);
#20322=LINE('',#177195,#25549);
#20323=LINE('',#177199,#25550);
#20324=LINE('',#177282,#25551);
#20325=LINE('',#177286,#25552);
#20326=LINE('',#177369,#25553);
#20327=LINE('',#177373,#25554);
#20328=LINE('',#177456,#25555);
#20329=LINE('',#177460,#25556);
#20330=LINE('',#177543,#25557);
#20331=LINE('',#177547,#25558);
#20332=LINE('',#177630,#25559);
#20333=LINE('',#177634,#25560);
#20334=LINE('',#177717,#25561);
#20335=LINE('',#177721,#25562);
#20336=LINE('',#177804,#25563);
#20337=LINE('',#177808,#25564);
#20338=LINE('',#177891,#25565);
#20339=LINE('',#177895,#25566);
#20340=LINE('',#177978,#25567);
#20341=LINE('',#177982,#25568);
#20342=LINE('',#178065,#25569);
#20343=LINE('',#178069,#25570);
#20344=LINE('',#178152,#25571);
#20345=LINE('',#178156,#25572);
#20346=LINE('',#178239,#25573);
#20347=LINE('',#178243,#25574);
#20348=LINE('',#178326,#25575);
#20349=LINE('',#178330,#25576);
#20350=LINE('',#178413,#25577);
#20351=LINE('',#178417,#25578);
#20352=LINE('',#178462,#25579);
#20353=LINE('',#178466,#25580);
#20354=LINE('',#178473,#25581);
#20355=LINE('',#178477,#25582);
#20356=LINE('',#178485,#25583);
#20357=LINE('',#178486,#25584);
#20358=LINE('',#178492,#25585);
#20359=LINE('',#178495,#25586);
#20360=LINE('',#178501,#25587);
#20361=LINE('',#178505,#25588);
#20362=LINE('',#178513,#25589);
#20363=LINE('',#178514,#25590);
#20364=LINE('',#178532,#25591);
#20365=LINE('',#178539,#25592);
#20366=LINE('',#178542,#25593);
#20367=LINE('',#178545,#25594);
#20368=LINE('',#178551,#25595);
#20369=LINE('',#178554,#25596);
#20370=LINE('',#178560,#25597);
#20371=LINE('',#178567,#25598);
#20372=LINE('',#178570,#25599);
#20373=LINE('',#178573,#25600);
#20374=LINE('',#178591,#25601);
#20375=LINE('',#178598,#25602);
#20376=LINE('',#178601,#25603);
#20377=LINE('',#178604,#25604);
#20378=LINE('',#178610,#25605);
#20379=LINE('',#178613,#25606);
#20380=LINE('',#178619,#25607);
#20381=LINE('',#178626,#25608);
#20382=LINE('',#178629,#25609);
#20383=LINE('',#178632,#25610);
#20384=LINE('',#178650,#25611);
#20385=LINE('',#178657,#25612);
#20386=LINE('',#178660,#25613);
#20387=LINE('',#178663,#25614);
#20388=LINE('',#178669,#25615);
#20389=LINE('',#178672,#25616);
#20390=LINE('',#178678,#25617);
#20391=LINE('',#178685,#25618);
#20392=LINE('',#178688,#25619);
#20393=LINE('',#178691,#25620);
#20394=LINE('',#178709,#25621);
#20395=LINE('',#178716,#25622);
#20396=LINE('',#178719,#25623);
#20397=LINE('',#178722,#25624);
#20398=LINE('',#178728,#25625);
#20399=LINE('',#178731,#25626);
#20400=LINE('',#178737,#25627);
#20401=LINE('',#178744,#25628);
#20402=LINE('',#178747,#25629);
#20403=LINE('',#178750,#25630);
#20404=LINE('',#178768,#25631);
#20405=LINE('',#178775,#25632);
#20406=LINE('',#178778,#25633);
#20407=LINE('',#178781,#25634);
#20408=LINE('',#178787,#25635);
#20409=LINE('',#178790,#25636);
#20410=LINE('',#178796,#25637);
#20411=LINE('',#178803,#25638);
#20412=LINE('',#178806,#25639);
#20413=LINE('',#178809,#25640);
#20414=LINE('',#178827,#25641);
#20415=LINE('',#178834,#25642);
#20416=LINE('',#178837,#25643);
#20417=LINE('',#178840,#25644);
#20418=LINE('',#178846,#25645);
#20419=LINE('',#178849,#25646);
#20420=LINE('',#178855,#25647);
#20421=LINE('',#178862,#25648);
#20422=LINE('',#178865,#25649);
#20423=LINE('',#178868,#25650);
#20424=LINE('',#178886,#25651);
#20425=LINE('',#178893,#25652);
#20426=LINE('',#178896,#25653);
#20427=LINE('',#178899,#25654);
#20428=LINE('',#178905,#25655);
#20429=LINE('',#178908,#25656);
#20430=LINE('',#178914,#25657);
#20431=LINE('',#178921,#25658);
#20432=LINE('',#178924,#25659);
#20433=LINE('',#178927,#25660);
#20434=LINE('',#178945,#25661);
#20435=LINE('',#178952,#25662);
#20436=LINE('',#178955,#25663);
#20437=LINE('',#178958,#25664);
#20438=LINE('',#178964,#25665);
#20439=LINE('',#178967,#25666);
#20440=LINE('',#178973,#25667);
#20441=LINE('',#178980,#25668);
#20442=LINE('',#178983,#25669);
#20443=LINE('',#178986,#25670);
#20444=LINE('',#179004,#25671);
#20445=LINE('',#179011,#25672);
#20446=LINE('',#179014,#25673);
#20447=LINE('',#179017,#25674);
#20448=LINE('',#179023,#25675);
#20449=LINE('',#179026,#25676);
#20450=LINE('',#179032,#25677);
#20451=LINE('',#179039,#25678);
#20452=LINE('',#179042,#25679);
#20453=LINE('',#179045,#25680);
#20454=LINE('',#179063,#25681);
#20455=LINE('',#179070,#25682);
#20456=LINE('',#179073,#25683);
#20457=LINE('',#179076,#25684);
#20458=LINE('',#179082,#25685);
#20459=LINE('',#179085,#25686);
#20460=LINE('',#179091,#25687);
#20461=LINE('',#179098,#25688);
#20462=LINE('',#179101,#25689);
#20463=LINE('',#179104,#25690);
#20464=LINE('',#179122,#25691);
#20465=LINE('',#179129,#25692);
#20466=LINE('',#179132,#25693);
#20467=LINE('',#179135,#25694);
#20468=LINE('',#179141,#25695);
#20469=LINE('',#179144,#25696);
#20470=LINE('',#179150,#25697);
#20471=LINE('',#179157,#25698);
#20472=LINE('',#179160,#25699);
#20473=LINE('',#179163,#25700);
#20474=LINE('',#179181,#25701);
#20475=LINE('',#179188,#25702);
#20476=LINE('',#179191,#25703);
#20477=LINE('',#179194,#25704);
#20478=LINE('',#179200,#25705);
#20479=LINE('',#179203,#25706);
#20480=LINE('',#179209,#25707);
#20481=LINE('',#179216,#25708);
#20482=LINE('',#179219,#25709);
#20483=LINE('',#179222,#25710);
#20484=LINE('',#179240,#25711);
#20485=LINE('',#179247,#25712);
#20486=LINE('',#179250,#25713);
#20487=LINE('',#179253,#25714);
#20488=LINE('',#179259,#25715);
#20489=LINE('',#179262,#25716);
#20490=LINE('',#179268,#25717);
#20491=LINE('',#179275,#25718);
#20492=LINE('',#179278,#25719);
#20493=LINE('',#179281,#25720);
#20494=LINE('',#179299,#25721);
#20495=LINE('',#179306,#25722);
#20496=LINE('',#179309,#25723);
#20497=LINE('',#179312,#25724);
#20498=LINE('',#179318,#25725);
#20499=LINE('',#179321,#25726);
#20500=LINE('',#179327,#25727);
#20501=LINE('',#179334,#25728);
#20502=LINE('',#179337,#25729);
#20503=LINE('',#179340,#25730);
#20504=LINE('',#179358,#25731);
#20505=LINE('',#179365,#25732);
#20506=LINE('',#179368,#25733);
#20507=LINE('',#179371,#25734);
#20508=LINE('',#179377,#25735);
#20509=LINE('',#179380,#25736);
#20510=LINE('',#179386,#25737);
#20511=LINE('',#179393,#25738);
#20512=LINE('',#179396,#25739);
#20513=LINE('',#179399,#25740);
#20514=LINE('',#179417,#25741);
#20515=LINE('',#179424,#25742);
#20516=LINE('',#179427,#25743);
#20517=LINE('',#179430,#25744);
#20518=LINE('',#179436,#25745);
#20519=LINE('',#179439,#25746);
#20520=LINE('',#179445,#25747);
#20521=LINE('',#179452,#25748);
#20522=LINE('',#179455,#25749);
#20523=LINE('',#179458,#25750);
#20524=LINE('',#179476,#25751);
#20525=LINE('',#179483,#25752);
#20526=LINE('',#179486,#25753);
#20527=LINE('',#179489,#25754);
#20528=LINE('',#179495,#25755);
#20529=LINE('',#179498,#25756);
#20530=LINE('',#179504,#25757);
#20531=LINE('',#179511,#25758);
#20532=LINE('',#179514,#25759);
#20533=LINE('',#179517,#25760);
#20534=LINE('',#179535,#25761);
#20535=LINE('',#179542,#25762);
#20536=LINE('',#179545,#25763);
#20537=LINE('',#179548,#25764);
#20538=LINE('',#179554,#25765);
#20539=LINE('',#179557,#25766);
#20540=LINE('',#179563,#25767);
#20541=LINE('',#179570,#25768);
#20542=LINE('',#179573,#25769);
#20543=LINE('',#179576,#25770);
#20544=LINE('',#179594,#25771);
#20545=LINE('',#179601,#25772);
#20546=LINE('',#179604,#25773);
#20547=LINE('',#179607,#25774);
#20548=LINE('',#179613,#25775);
#20549=LINE('',#179616,#25776);
#20550=LINE('',#179622,#25777);
#20551=LINE('',#179629,#25778);
#20552=LINE('',#179632,#25779);
#20553=LINE('',#179635,#25780);
#20554=LINE('',#179653,#25781);
#20555=LINE('',#179660,#25782);
#20556=LINE('',#179663,#25783);
#20557=LINE('',#179666,#25784);
#20558=LINE('',#179672,#25785);
#20559=LINE('',#179675,#25786);
#20560=LINE('',#179681,#25787);
#20561=LINE('',#179688,#25788);
#20562=LINE('',#179691,#25789);
#20563=LINE('',#179694,#25790);
#20564=LINE('',#179712,#25791);
#20565=LINE('',#179719,#25792);
#20566=LINE('',#179722,#25793);
#20567=LINE('',#179725,#25794);
#20568=LINE('',#179731,#25795);
#20569=LINE('',#179734,#25796);
#20570=LINE('',#179740,#25797);
#20571=LINE('',#179747,#25798);
#20572=LINE('',#179750,#25799);
#20573=LINE('',#179753,#25800);
#20574=LINE('',#179771,#25801);
#20575=LINE('',#179778,#25802);
#20576=LINE('',#179781,#25803);
#20577=LINE('',#179784,#25804);
#20578=LINE('',#179790,#25805);
#20579=LINE('',#179793,#25806);
#20580=LINE('',#179799,#25807);
#20581=LINE('',#179806,#25808);
#20582=LINE('',#179809,#25809);
#20583=LINE('',#179812,#25810);
#20584=LINE('',#179830,#25811);
#20585=LINE('',#179837,#25812);
#20586=LINE('',#179840,#25813);
#20587=LINE('',#179843,#25814);
#20588=LINE('',#179849,#25815);
#20589=LINE('',#179852,#25816);
#20590=LINE('',#179858,#25817);
#20591=LINE('',#179865,#25818);
#20592=LINE('',#179868,#25819);
#20593=LINE('',#179871,#25820);
#20594=LINE('',#179889,#25821);
#20595=LINE('',#179896,#25822);
#20596=LINE('',#179899,#25823);
#20597=LINE('',#179902,#25824);
#20598=LINE('',#179908,#25825);
#20599=LINE('',#179911,#25826);
#20600=LINE('',#179917,#25827);
#20601=LINE('',#179924,#25828);
#20602=LINE('',#179927,#25829);
#20603=LINE('',#179930,#25830);
#20604=LINE('',#179948,#25831);
#20605=LINE('',#179955,#25832);
#20606=LINE('',#179958,#25833);
#20607=LINE('',#179961,#25834);
#20608=LINE('',#179967,#25835);
#20609=LINE('',#179970,#25836);
#20610=LINE('',#179976,#25837);
#20611=LINE('',#179983,#25838);
#20612=LINE('',#179986,#25839);
#20613=LINE('',#179989,#25840);
#20614=LINE('',#180007,#25841);
#20615=LINE('',#180014,#25842);
#20616=LINE('',#180017,#25843);
#20617=LINE('',#180020,#25844);
#20618=LINE('',#180026,#25845);
#20619=LINE('',#180029,#25846);
#20620=LINE('',#180035,#25847);
#20621=LINE('',#180042,#25848);
#20622=LINE('',#180045,#25849);
#20623=LINE('',#180048,#25850);
#20624=LINE('',#180066,#25851);
#20625=LINE('',#180073,#25852);
#20626=LINE('',#180076,#25853);
#20627=LINE('',#180079,#25854);
#20628=LINE('',#180085,#25855);
#20629=LINE('',#180088,#25856);
#20630=LINE('',#180094,#25857);
#20631=LINE('',#180101,#25858);
#20632=LINE('',#180104,#25859);
#20633=LINE('',#180107,#25860);
#20634=LINE('',#180125,#25861);
#20635=LINE('',#180132,#25862);
#20636=LINE('',#180135,#25863);
#20637=LINE('',#180138,#25864);
#20638=LINE('',#180144,#25865);
#20639=LINE('',#180147,#25866);
#20640=LINE('',#180153,#25867);
#20641=LINE('',#180160,#25868);
#20642=LINE('',#180163,#25869);
#20643=LINE('',#180166,#25870);
#20644=LINE('',#180184,#25871);
#20645=LINE('',#180191,#25872);
#20646=LINE('',#180194,#25873);
#20647=LINE('',#180197,#25874);
#20648=LINE('',#180203,#25875);
#20649=LINE('',#180206,#25876);
#20650=LINE('',#180212,#25877);
#20651=LINE('',#180219,#25878);
#20652=LINE('',#180222,#25879);
#20653=LINE('',#180225,#25880);
#20654=LINE('',#180243,#25881);
#20655=LINE('',#180250,#25882);
#20656=LINE('',#180253,#25883);
#20657=LINE('',#180256,#25884);
#20658=LINE('',#180262,#25885);
#20659=LINE('',#180265,#25886);
#20660=LINE('',#180271,#25887);
#20661=LINE('',#180278,#25888);
#20662=LINE('',#180281,#25889);
#20663=LINE('',#180284,#25890);
#20664=LINE('',#180302,#25891);
#20665=LINE('',#180309,#25892);
#20666=LINE('',#180312,#25893);
#20667=LINE('',#180315,#25894);
#20668=LINE('',#180321,#25895);
#20669=LINE('',#180324,#25896);
#20670=LINE('',#180330,#25897);
#20671=LINE('',#180337,#25898);
#20672=LINE('',#180340,#25899);
#20673=LINE('',#180343,#25900);
#20674=LINE('',#180361,#25901);
#20675=LINE('',#180368,#25902);
#20676=LINE('',#180371,#25903);
#20677=LINE('',#180374,#25904);
#20678=LINE('',#180380,#25905);
#20679=LINE('',#180383,#25906);
#20680=LINE('',#180389,#25907);
#20681=LINE('',#180396,#25908);
#20682=LINE('',#180399,#25909);
#20683=LINE('',#180402,#25910);
#20684=LINE('',#180420,#25911);
#20685=LINE('',#180427,#25912);
#20686=LINE('',#180430,#25913);
#20687=LINE('',#180433,#25914);
#20688=LINE('',#180439,#25915);
#20689=LINE('',#180442,#25916);
#20690=LINE('',#180448,#25917);
#20691=LINE('',#180455,#25918);
#20692=LINE('',#180458,#25919);
#20693=LINE('',#180461,#25920);
#20694=LINE('',#180479,#25921);
#20695=LINE('',#180486,#25922);
#20696=LINE('',#180489,#25923);
#20697=LINE('',#180492,#25924);
#20698=LINE('',#180498,#25925);
#20699=LINE('',#180501,#25926);
#20700=LINE('',#180507,#25927);
#20701=LINE('',#180514,#25928);
#20702=LINE('',#180517,#25929);
#20703=LINE('',#180520,#25930);
#20704=LINE('',#180538,#25931);
#20705=LINE('',#180545,#25932);
#20706=LINE('',#180548,#25933);
#20707=LINE('',#180551,#25934);
#20708=LINE('',#180557,#25935);
#20709=LINE('',#180560,#25936);
#20710=LINE('',#180566,#25937);
#20711=LINE('',#180573,#25938);
#20712=LINE('',#180576,#25939);
#20713=LINE('',#180579,#25940);
#20714=LINE('',#180597,#25941);
#20715=LINE('',#180604,#25942);
#20716=LINE('',#180607,#25943);
#20717=LINE('',#180610,#25944);
#20718=LINE('',#180616,#25945);
#20719=LINE('',#180619,#25946);
#20720=LINE('',#180625,#25947);
#20721=LINE('',#180632,#25948);
#20722=LINE('',#180635,#25949);
#20723=LINE('',#180638,#25950);
#20724=LINE('',#180656,#25951);
#20725=LINE('',#180663,#25952);
#20726=LINE('',#180666,#25953);
#20727=LINE('',#180669,#25954);
#20728=LINE('',#180675,#25955);
#20729=LINE('',#180678,#25956);
#20730=LINE('',#180684,#25957);
#20731=LINE('',#180691,#25958);
#20732=LINE('',#180694,#25959);
#20733=LINE('',#180697,#25960);
#20734=LINE('',#180715,#25961);
#20735=LINE('',#180722,#25962);
#20736=LINE('',#180725,#25963);
#20737=LINE('',#180728,#25964);
#20738=LINE('',#180734,#25965);
#20739=LINE('',#180737,#25966);
#20740=LINE('',#180743,#25967);
#20741=LINE('',#180750,#25968);
#20742=LINE('',#180753,#25969);
#20743=LINE('',#180756,#25970);
#20744=LINE('',#180774,#25971);
#20745=LINE('',#180781,#25972);
#20746=LINE('',#180784,#25973);
#20747=LINE('',#180787,#25974);
#20748=LINE('',#180793,#25975);
#20749=LINE('',#180796,#25976);
#20750=LINE('',#180802,#25977);
#20751=LINE('',#180809,#25978);
#20752=LINE('',#180812,#25979);
#20753=LINE('',#180815,#25980);
#20754=LINE('',#180833,#25981);
#20755=LINE('',#180840,#25982);
#20756=LINE('',#180843,#25983);
#20757=LINE('',#180846,#25984);
#20758=LINE('',#180852,#25985);
#20759=LINE('',#180855,#25986);
#20760=LINE('',#180861,#25987);
#20761=LINE('',#180868,#25988);
#20762=LINE('',#180871,#25989);
#20763=LINE('',#180874,#25990);
#20764=LINE('',#180892,#25991);
#20765=LINE('',#180899,#25992);
#20766=LINE('',#180902,#25993);
#20767=LINE('',#180905,#25994);
#20768=LINE('',#180911,#25995);
#20769=LINE('',#180914,#25996);
#20770=LINE('',#180920,#25997);
#20771=LINE('',#180927,#25998);
#20772=LINE('',#180930,#25999);
#20773=LINE('',#180933,#26000);
#20774=LINE('',#180951,#26001);
#20775=LINE('',#180958,#26002);
#20776=LINE('',#180961,#26003);
#20777=LINE('',#180964,#26004);
#20778=LINE('',#180970,#26005);
#20779=LINE('',#180973,#26006);
#20780=LINE('',#180979,#26007);
#20781=LINE('',#180986,#26008);
#20782=LINE('',#180989,#26009);
#20783=LINE('',#180992,#26010);
#20784=LINE('',#181010,#26011);
#20785=LINE('',#181017,#26012);
#20786=LINE('',#181020,#26013);
#20787=LINE('',#181023,#26014);
#20788=LINE('',#181029,#26015);
#20789=LINE('',#181032,#26016);
#20790=LINE('',#181038,#26017);
#20791=LINE('',#181045,#26018);
#20792=LINE('',#181048,#26019);
#20793=LINE('',#181051,#26020);
#20794=LINE('',#181069,#26021);
#20795=LINE('',#181076,#26022);
#20796=LINE('',#181079,#26023);
#20797=LINE('',#181082,#26024);
#20798=LINE('',#181088,#26025);
#20799=LINE('',#181091,#26026);
#20800=LINE('',#181097,#26027);
#20801=LINE('',#181104,#26028);
#20802=LINE('',#181107,#26029);
#20803=LINE('',#181110,#26030);
#20804=LINE('',#181128,#26031);
#20805=LINE('',#181135,#26032);
#20806=LINE('',#181138,#26033);
#20807=LINE('',#181141,#26034);
#20808=LINE('',#181147,#26035);
#20809=LINE('',#181150,#26036);
#20810=LINE('',#181156,#26037);
#20811=LINE('',#181163,#26038);
#20812=LINE('',#181166,#26039);
#20813=LINE('',#181169,#26040);
#20814=LINE('',#181187,#26041);
#20815=LINE('',#181194,#26042);
#20816=LINE('',#181197,#26043);
#20817=LINE('',#181200,#26044);
#20818=LINE('',#181206,#26045);
#20819=LINE('',#181209,#26046);
#20820=LINE('',#181215,#26047);
#20821=LINE('',#181222,#26048);
#20822=LINE('',#181225,#26049);
#20823=LINE('',#181228,#26050);
#20824=LINE('',#181246,#26051);
#20825=LINE('',#181253,#26052);
#20826=LINE('',#181256,#26053);
#20827=LINE('',#181259,#26054);
#20828=LINE('',#181265,#26055);
#20829=LINE('',#181268,#26056);
#20830=LINE('',#181274,#26057);
#20831=LINE('',#181281,#26058);
#20832=LINE('',#181284,#26059);
#20833=LINE('',#181287,#26060);
#20834=LINE('',#181305,#26061);
#20835=LINE('',#181312,#26062);
#20836=LINE('',#181315,#26063);
#20837=LINE('',#181318,#26064);
#20838=LINE('',#181324,#26065);
#20839=LINE('',#181327,#26066);
#20840=LINE('',#181333,#26067);
#20841=LINE('',#181340,#26068);
#20842=LINE('',#181343,#26069);
#20843=LINE('',#181346,#26070);
#20844=LINE('',#181364,#26071);
#20845=LINE('',#181371,#26072);
#20846=LINE('',#181374,#26073);
#20847=LINE('',#181377,#26074);
#20848=LINE('',#181383,#26075);
#20849=LINE('',#181386,#26076);
#20850=LINE('',#181392,#26077);
#20851=LINE('',#181399,#26078);
#20852=LINE('',#181402,#26079);
#20853=LINE('',#181405,#26080);
#20854=LINE('',#181423,#26081);
#20855=LINE('',#181430,#26082);
#20856=LINE('',#181433,#26083);
#20857=LINE('',#181436,#26084);
#20858=LINE('',#181442,#26085);
#20859=LINE('',#181445,#26086);
#20860=LINE('',#181451,#26087);
#20861=LINE('',#181458,#26088);
#20862=LINE('',#181461,#26089);
#20863=LINE('',#181464,#26090);
#20864=LINE('',#181482,#26091);
#20865=LINE('',#181489,#26092);
#20866=LINE('',#181492,#26093);
#20867=LINE('',#181495,#26094);
#20868=LINE('',#181501,#26095);
#20869=LINE('',#181504,#26096);
#20870=LINE('',#181510,#26097);
#20871=LINE('',#181517,#26098);
#20872=LINE('',#181520,#26099);
#20873=LINE('',#181523,#26100);
#20874=LINE('',#181541,#26101);
#20875=LINE('',#181548,#26102);
#20876=LINE('',#181551,#26103);
#20877=LINE('',#181554,#26104);
#20878=LINE('',#181560,#26105);
#20879=LINE('',#181563,#26106);
#20880=LINE('',#181569,#26107);
#20881=LINE('',#181576,#26108);
#20882=LINE('',#181579,#26109);
#20883=LINE('',#181582,#26110);
#20884=LINE('',#181600,#26111);
#20885=LINE('',#181607,#26112);
#20886=LINE('',#181610,#26113);
#20887=LINE('',#181613,#26114);
#20888=LINE('',#181619,#26115);
#20889=LINE('',#181622,#26116);
#20890=LINE('',#181628,#26117);
#20891=LINE('',#181635,#26118);
#20892=LINE('',#181638,#26119);
#20893=LINE('',#181641,#26120);
#20894=LINE('',#181659,#26121);
#20895=LINE('',#181666,#26122);
#20896=LINE('',#181669,#26123);
#20897=LINE('',#181672,#26124);
#20898=LINE('',#181678,#26125);
#20899=LINE('',#181681,#26126);
#20900=LINE('',#181687,#26127);
#20901=LINE('',#181694,#26128);
#20902=LINE('',#181697,#26129);
#20903=LINE('',#181700,#26130);
#20904=LINE('',#181718,#26131);
#20905=LINE('',#181725,#26132);
#20906=LINE('',#181728,#26133);
#20907=LINE('',#181731,#26134);
#20908=LINE('',#181737,#26135);
#20909=LINE('',#181740,#26136);
#20910=LINE('',#181746,#26137);
#20911=LINE('',#181753,#26138);
#20912=LINE('',#181756,#26139);
#20913=LINE('',#181759,#26140);
#20914=LINE('',#181777,#26141);
#20915=LINE('',#181784,#26142);
#20916=LINE('',#181787,#26143);
#20917=LINE('',#181790,#26144);
#20918=LINE('',#181796,#26145);
#20919=LINE('',#181799,#26146);
#20920=LINE('',#181805,#26147);
#20921=LINE('',#181812,#26148);
#20922=LINE('',#181815,#26149);
#20923=LINE('',#181818,#26150);
#20924=LINE('',#181836,#26151);
#20925=LINE('',#181843,#26152);
#20926=LINE('',#181846,#26153);
#20927=LINE('',#181849,#26154);
#20928=LINE('',#181855,#26155);
#20929=LINE('',#181858,#26156);
#20930=LINE('',#181864,#26157);
#20931=LINE('',#181871,#26158);
#20932=LINE('',#181874,#26159);
#20933=LINE('',#181877,#26160);
#20934=LINE('',#181895,#26161);
#20935=LINE('',#181902,#26162);
#20936=LINE('',#181905,#26163);
#20937=LINE('',#181908,#26164);
#20938=LINE('',#181914,#26165);
#20939=LINE('',#181917,#26166);
#20940=LINE('',#181923,#26167);
#20941=LINE('',#181930,#26168);
#20942=LINE('',#181933,#26169);
#20943=LINE('',#181936,#26170);
#20944=LINE('',#181955,#26171);
#20945=LINE('',#181962,#26172);
#20946=LINE('',#181965,#26173);
#20947=LINE('',#181968,#26174);
#20948=LINE('',#181974,#26175);
#20949=LINE('',#181977,#26176);
#20950=LINE('',#181983,#26177);
#20951=LINE('',#181990,#26178);
#20952=LINE('',#181993,#26179);
#20953=LINE('',#181996,#26180);
#20954=LINE('',#182014,#26181);
#20955=LINE('',#182018,#26182);
#20956=LINE('',#182025,#26183);
#20957=LINE('',#182027,#26184);
#20958=LINE('',#182029,#26185);
#20959=LINE('',#182033,#26186);
#20960=LINE('',#182035,#26187);
#20961=LINE('',#182039,#26188);
#20962=LINE('',#182043,#26189);
#20963=LINE('',#182044,#26190);
#20964=LINE('',#182050,#26191);
#20965=LINE('',#182052,#26192);
#20966=LINE('',#182054,#26193);
#20967=LINE('',#182058,#26194);
#20968=LINE('',#182060,#26195);
#20969=LINE('',#182064,#26196);
#20970=LINE('',#182068,#26197);
#20971=LINE('',#182069,#26198);
#20972=LINE('',#182489,#26199);
#20973=LINE('',#182493,#26200);
#20974=LINE('',#182500,#26201);
#20975=LINE('',#182502,#26202);
#20976=LINE('',#182504,#26203);
#20977=LINE('',#182508,#26204);
#20978=LINE('',#182510,#26205);
#20979=LINE('',#182514,#26206);
#20980=LINE('',#182518,#26207);
#20981=LINE('',#182519,#26208);
#20982=LINE('',#182525,#26209);
#20983=LINE('',#182527,#26210);
#20984=LINE('',#182529,#26211);
#20985=LINE('',#182533,#26212);
#20986=LINE('',#182535,#26213);
#20987=LINE('',#182539,#26214);
#20988=LINE('',#182543,#26215);
#20989=LINE('',#182544,#26216);
#20990=LINE('',#182548,#26217);
#20991=LINE('',#182552,#26218);
#20992=LINE('',#182559,#26219);
#20993=LINE('',#182561,#26220);
#20994=LINE('',#182563,#26221);
#20995=LINE('',#182567,#26222);
#20996=LINE('',#182569,#26223);
#20997=LINE('',#182573,#26224);
#20998=LINE('',#182577,#26225);
#20999=LINE('',#182578,#26226);
#21000=LINE('',#182584,#26227);
#21001=LINE('',#182586,#26228);
#21002=LINE('',#182588,#26229);
#21003=LINE('',#182592,#26230);
#21004=LINE('',#182594,#26231);
#21005=LINE('',#182598,#26232);
#21006=LINE('',#182602,#26233);
#21007=LINE('',#182603,#26234);
#21008=LINE('',#182607,#26235);
#21009=LINE('',#182611,#26236);
#21010=LINE('',#182618,#26237);
#21011=LINE('',#182620,#26238);
#21012=LINE('',#182622,#26239);
#21013=LINE('',#182626,#26240);
#21014=LINE('',#182628,#26241);
#21015=LINE('',#182632,#26242);
#21016=LINE('',#182636,#26243);
#21017=LINE('',#182637,#26244);
#21018=LINE('',#182643,#26245);
#21019=LINE('',#182645,#26246);
#21020=LINE('',#182647,#26247);
#21021=LINE('',#182651,#26248);
#21022=LINE('',#182653,#26249);
#21023=LINE('',#182657,#26250);
#21024=LINE('',#182661,#26251);
#21025=LINE('',#182662,#26252);
#21026=LINE('',#182666,#26253);
#21027=LINE('',#182670,#26254);
#21028=LINE('',#182677,#26255);
#21029=LINE('',#182679,#26256);
#21030=LINE('',#182681,#26257);
#21031=LINE('',#182685,#26258);
#21032=LINE('',#182687,#26259);
#21033=LINE('',#182691,#26260);
#21034=LINE('',#182695,#26261);
#21035=LINE('',#182696,#26262);
#21036=LINE('',#182702,#26263);
#21037=LINE('',#182704,#26264);
#21038=LINE('',#182706,#26265);
#21039=LINE('',#182710,#26266);
#21040=LINE('',#182712,#26267);
#21041=LINE('',#182716,#26268);
#21042=LINE('',#182720,#26269);
#21043=LINE('',#182721,#26270);
#21044=LINE('',#182725,#26271);
#21045=LINE('',#182729,#26272);
#21046=LINE('',#182736,#26273);
#21047=LINE('',#182738,#26274);
#21048=LINE('',#182740,#26275);
#21049=LINE('',#182744,#26276);
#21050=LINE('',#182746,#26277);
#21051=LINE('',#182750,#26278);
#21052=LINE('',#182754,#26279);
#21053=LINE('',#182755,#26280);
#21054=LINE('',#182761,#26281);
#21055=LINE('',#182763,#26282);
#21056=LINE('',#182765,#26283);
#21057=LINE('',#182769,#26284);
#21058=LINE('',#182771,#26285);
#21059=LINE('',#182775,#26286);
#21060=LINE('',#182779,#26287);
#21061=LINE('',#182780,#26288);
#21062=LINE('',#182784,#26289);
#21063=LINE('',#182788,#26290);
#21064=LINE('',#182795,#26291);
#21065=LINE('',#182797,#26292);
#21066=LINE('',#182799,#26293);
#21067=LINE('',#182803,#26294);
#21068=LINE('',#182805,#26295);
#21069=LINE('',#182809,#26296);
#21070=LINE('',#182813,#26297);
#21071=LINE('',#182814,#26298);
#21072=LINE('',#182820,#26299);
#21073=LINE('',#182822,#26300);
#21074=LINE('',#182824,#26301);
#21075=LINE('',#182828,#26302);
#21076=LINE('',#182830,#26303);
#21077=LINE('',#182834,#26304);
#21078=LINE('',#182838,#26305);
#21079=LINE('',#182839,#26306);
#21080=LINE('',#182843,#26307);
#21081=LINE('',#182847,#26308);
#21082=LINE('',#182854,#26309);
#21083=LINE('',#182856,#26310);
#21084=LINE('',#182858,#26311);
#21085=LINE('',#182862,#26312);
#21086=LINE('',#182864,#26313);
#21087=LINE('',#182868,#26314);
#21088=LINE('',#182872,#26315);
#21089=LINE('',#182873,#26316);
#21090=LINE('',#182879,#26317);
#21091=LINE('',#182881,#26318);
#21092=LINE('',#182883,#26319);
#21093=LINE('',#182887,#26320);
#21094=LINE('',#182889,#26321);
#21095=LINE('',#182893,#26322);
#21096=LINE('',#182897,#26323);
#21097=LINE('',#182898,#26324);
#21098=LINE('',#182902,#26325);
#21099=LINE('',#182906,#26326);
#21100=LINE('',#182913,#26327);
#21101=LINE('',#182915,#26328);
#21102=LINE('',#182917,#26329);
#21103=LINE('',#182921,#26330);
#21104=LINE('',#182923,#26331);
#21105=LINE('',#182927,#26332);
#21106=LINE('',#182931,#26333);
#21107=LINE('',#182932,#26334);
#21108=LINE('',#182938,#26335);
#21109=LINE('',#182940,#26336);
#21110=LINE('',#182942,#26337);
#21111=LINE('',#182946,#26338);
#21112=LINE('',#182948,#26339);
#21113=LINE('',#182952,#26340);
#21114=LINE('',#182956,#26341);
#21115=LINE('',#182957,#26342);
#21116=LINE('',#182961,#26343);
#21117=LINE('',#182965,#26344);
#21118=LINE('',#182972,#26345);
#21119=LINE('',#182974,#26346);
#21120=LINE('',#182976,#26347);
#21121=LINE('',#182980,#26348);
#21122=LINE('',#182982,#26349);
#21123=LINE('',#182986,#26350);
#21124=LINE('',#182990,#26351);
#21125=LINE('',#182991,#26352);
#21126=LINE('',#182997,#26353);
#21127=LINE('',#182999,#26354);
#21128=LINE('',#183001,#26355);
#21129=LINE('',#183005,#26356);
#21130=LINE('',#183007,#26357);
#21131=LINE('',#183011,#26358);
#21132=LINE('',#183015,#26359);
#21133=LINE('',#183016,#26360);
#21134=LINE('',#183020,#26361);
#21135=LINE('',#183024,#26362);
#21136=LINE('',#183031,#26363);
#21137=LINE('',#183033,#26364);
#21138=LINE('',#183035,#26365);
#21139=LINE('',#183039,#26366);
#21140=LINE('',#183041,#26367);
#21141=LINE('',#183045,#26368);
#21142=LINE('',#183049,#26369);
#21143=LINE('',#183050,#26370);
#21144=LINE('',#183056,#26371);
#21145=LINE('',#183058,#26372);
#21146=LINE('',#183060,#26373);
#21147=LINE('',#183064,#26374);
#21148=LINE('',#183066,#26375);
#21149=LINE('',#183070,#26376);
#21150=LINE('',#183074,#26377);
#21151=LINE('',#183075,#26378);
#21152=LINE('',#183079,#26379);
#21153=LINE('',#183083,#26380);
#21154=LINE('',#183090,#26381);
#21155=LINE('',#183092,#26382);
#21156=LINE('',#183094,#26383);
#21157=LINE('',#183098,#26384);
#21158=LINE('',#183100,#26385);
#21159=LINE('',#183104,#26386);
#21160=LINE('',#183108,#26387);
#21161=LINE('',#183109,#26388);
#21162=LINE('',#183115,#26389);
#21163=LINE('',#183117,#26390);
#21164=LINE('',#183119,#26391);
#21165=LINE('',#183123,#26392);
#21166=LINE('',#183125,#26393);
#21167=LINE('',#183129,#26394);
#21168=LINE('',#183133,#26395);
#21169=LINE('',#183134,#26396);
#21170=LINE('',#183138,#26397);
#21171=LINE('',#183142,#26398);
#21172=LINE('',#183149,#26399);
#21173=LINE('',#183151,#26400);
#21174=LINE('',#183153,#26401);
#21175=LINE('',#183157,#26402);
#21176=LINE('',#183159,#26403);
#21177=LINE('',#183163,#26404);
#21178=LINE('',#183167,#26405);
#21179=LINE('',#183168,#26406);
#21180=LINE('',#183174,#26407);
#21181=LINE('',#183176,#26408);
#21182=LINE('',#183178,#26409);
#21183=LINE('',#183182,#26410);
#21184=LINE('',#183184,#26411);
#21185=LINE('',#183188,#26412);
#21186=LINE('',#183192,#26413);
#21187=LINE('',#183193,#26414);
#21188=LINE('',#183197,#26415);
#21189=LINE('',#183201,#26416);
#21190=LINE('',#183208,#26417);
#21191=LINE('',#183210,#26418);
#21192=LINE('',#183212,#26419);
#21193=LINE('',#183216,#26420);
#21194=LINE('',#183218,#26421);
#21195=LINE('',#183222,#26422);
#21196=LINE('',#183226,#26423);
#21197=LINE('',#183227,#26424);
#21198=LINE('',#183233,#26425);
#21199=LINE('',#183235,#26426);
#21200=LINE('',#183237,#26427);
#21201=LINE('',#183241,#26428);
#21202=LINE('',#183243,#26429);
#21203=LINE('',#183247,#26430);
#21204=LINE('',#183251,#26431);
#21205=LINE('',#183252,#26432);
#21206=LINE('',#183256,#26433);
#21207=LINE('',#183260,#26434);
#21208=LINE('',#183267,#26435);
#21209=LINE('',#183269,#26436);
#21210=LINE('',#183271,#26437);
#21211=LINE('',#183275,#26438);
#21212=LINE('',#183277,#26439);
#21213=LINE('',#183281,#26440);
#21214=LINE('',#183285,#26441);
#21215=LINE('',#183286,#26442);
#21216=LINE('',#183292,#26443);
#21217=LINE('',#183294,#26444);
#21218=LINE('',#183296,#26445);
#21219=LINE('',#183300,#26446);
#21220=LINE('',#183302,#26447);
#21221=LINE('',#183306,#26448);
#21222=LINE('',#183310,#26449);
#21223=LINE('',#183311,#26450);
#21224=LINE('',#183315,#26451);
#21225=LINE('',#183319,#26452);
#21226=LINE('',#183326,#26453);
#21227=LINE('',#183328,#26454);
#21228=LINE('',#183330,#26455);
#21229=LINE('',#183334,#26456);
#21230=LINE('',#183336,#26457);
#21231=LINE('',#183340,#26458);
#21232=LINE('',#183344,#26459);
#21233=LINE('',#183345,#26460);
#21234=LINE('',#183351,#26461);
#21235=LINE('',#183353,#26462);
#21236=LINE('',#183355,#26463);
#21237=LINE('',#183359,#26464);
#21238=LINE('',#183361,#26465);
#21239=LINE('',#183365,#26466);
#21240=LINE('',#183369,#26467);
#21241=LINE('',#183370,#26468);
#21242=LINE('',#183374,#26469);
#21243=LINE('',#183378,#26470);
#21244=LINE('',#183385,#26471);
#21245=LINE('',#183387,#26472);
#21246=LINE('',#183389,#26473);
#21247=LINE('',#183393,#26474);
#21248=LINE('',#183395,#26475);
#21249=LINE('',#183399,#26476);
#21250=LINE('',#183403,#26477);
#21251=LINE('',#183404,#26478);
#21252=LINE('',#183410,#26479);
#21253=LINE('',#183412,#26480);
#21254=LINE('',#183414,#26481);
#21255=LINE('',#183418,#26482);
#21256=LINE('',#183420,#26483);
#21257=LINE('',#183424,#26484);
#21258=LINE('',#183428,#26485);
#21259=LINE('',#183429,#26486);
#21260=LINE('',#183433,#26487);
#21261=LINE('',#183437,#26488);
#21262=LINE('',#183444,#26489);
#21263=LINE('',#183446,#26490);
#21264=LINE('',#183448,#26491);
#21265=LINE('',#183452,#26492);
#21266=LINE('',#183454,#26493);
#21267=LINE('',#183458,#26494);
#21268=LINE('',#183462,#26495);
#21269=LINE('',#183463,#26496);
#21270=LINE('',#183469,#26497);
#21271=LINE('',#183471,#26498);
#21272=LINE('',#183473,#26499);
#21273=LINE('',#183477,#26500);
#21274=LINE('',#183479,#26501);
#21275=LINE('',#183483,#26502);
#21276=LINE('',#183487,#26503);
#21277=LINE('',#183488,#26504);
#21278=LINE('',#183492,#26505);
#21279=LINE('',#183496,#26506);
#21280=LINE('',#183503,#26507);
#21281=LINE('',#183505,#26508);
#21282=LINE('',#183507,#26509);
#21283=LINE('',#183511,#26510);
#21284=LINE('',#183513,#26511);
#21285=LINE('',#183517,#26512);
#21286=LINE('',#183521,#26513);
#21287=LINE('',#183522,#26514);
#21288=LINE('',#183528,#26515);
#21289=LINE('',#183530,#26516);
#21290=LINE('',#183532,#26517);
#21291=LINE('',#183536,#26518);
#21292=LINE('',#183538,#26519);
#21293=LINE('',#183542,#26520);
#21294=LINE('',#183546,#26521);
#21295=LINE('',#183547,#26522);
#21296=LINE('',#183551,#26523);
#21297=LINE('',#183555,#26524);
#21298=LINE('',#183562,#26525);
#21299=LINE('',#183564,#26526);
#21300=LINE('',#183566,#26527);
#21301=LINE('',#183570,#26528);
#21302=LINE('',#183572,#26529);
#21303=LINE('',#183576,#26530);
#21304=LINE('',#183580,#26531);
#21305=LINE('',#183581,#26532);
#21306=LINE('',#183587,#26533);
#21307=LINE('',#183589,#26534);
#21308=LINE('',#183591,#26535);
#21309=LINE('',#183595,#26536);
#21310=LINE('',#183597,#26537);
#21311=LINE('',#183601,#26538);
#21312=LINE('',#183605,#26539);
#21313=LINE('',#183606,#26540);
#21314=LINE('',#183610,#26541);
#21315=LINE('',#183614,#26542);
#21316=LINE('',#183621,#26543);
#21317=LINE('',#183623,#26544);
#21318=LINE('',#183625,#26545);
#21319=LINE('',#183629,#26546);
#21320=LINE('',#183631,#26547);
#21321=LINE('',#183635,#26548);
#21322=LINE('',#183639,#26549);
#21323=LINE('',#183640,#26550);
#21324=LINE('',#183646,#26551);
#21325=LINE('',#183648,#26552);
#21326=LINE('',#183650,#26553);
#21327=LINE('',#183654,#26554);
#21328=LINE('',#183656,#26555);
#21329=LINE('',#183660,#26556);
#21330=LINE('',#183664,#26557);
#21331=LINE('',#183665,#26558);
#21332=LINE('',#183669,#26559);
#21333=LINE('',#183673,#26560);
#21334=LINE('',#183680,#26561);
#21335=LINE('',#183682,#26562);
#21336=LINE('',#183684,#26563);
#21337=LINE('',#183688,#26564);
#21338=LINE('',#183690,#26565);
#21339=LINE('',#183694,#26566);
#21340=LINE('',#183698,#26567);
#21341=LINE('',#183699,#26568);
#21342=LINE('',#183705,#26569);
#21343=LINE('',#183707,#26570);
#21344=LINE('',#183709,#26571);
#21345=LINE('',#183713,#26572);
#21346=LINE('',#183715,#26573);
#21347=LINE('',#183719,#26574);
#21348=LINE('',#183723,#26575);
#21349=LINE('',#183724,#26576);
#21350=LINE('',#183728,#26577);
#21351=LINE('',#183732,#26578);
#21352=LINE('',#183739,#26579);
#21353=LINE('',#183741,#26580);
#21354=LINE('',#183743,#26581);
#21355=LINE('',#183747,#26582);
#21356=LINE('',#183749,#26583);
#21357=LINE('',#183753,#26584);
#21358=LINE('',#183757,#26585);
#21359=LINE('',#183758,#26586);
#21360=LINE('',#183764,#26587);
#21361=LINE('',#183766,#26588);
#21362=LINE('',#183768,#26589);
#21363=LINE('',#183772,#26590);
#21364=LINE('',#183774,#26591);
#21365=LINE('',#183778,#26592);
#21366=LINE('',#183782,#26593);
#21367=LINE('',#183783,#26594);
#21368=LINE('',#183787,#26595);
#21369=LINE('',#183791,#26596);
#21370=LINE('',#183798,#26597);
#21371=LINE('',#183800,#26598);
#21372=LINE('',#183802,#26599);
#21373=LINE('',#183806,#26600);
#21374=LINE('',#183808,#26601);
#21375=LINE('',#183812,#26602);
#21376=LINE('',#183816,#26603);
#21377=LINE('',#183817,#26604);
#21378=LINE('',#183823,#26605);
#21379=LINE('',#183825,#26606);
#21380=LINE('',#183827,#26607);
#21381=LINE('',#183831,#26608);
#21382=LINE('',#183833,#26609);
#21383=LINE('',#183837,#26610);
#21384=LINE('',#183841,#26611);
#21385=LINE('',#183842,#26612);
#21386=LINE('',#183846,#26613);
#21387=LINE('',#183850,#26614);
#21388=LINE('',#183857,#26615);
#21389=LINE('',#183859,#26616);
#21390=LINE('',#183861,#26617);
#21391=LINE('',#183865,#26618);
#21392=LINE('',#183867,#26619);
#21393=LINE('',#183871,#26620);
#21394=LINE('',#183875,#26621);
#21395=LINE('',#183876,#26622);
#21396=LINE('',#183882,#26623);
#21397=LINE('',#183884,#26624);
#21398=LINE('',#183886,#26625);
#21399=LINE('',#183890,#26626);
#21400=LINE('',#183892,#26627);
#21401=LINE('',#183896,#26628);
#21402=LINE('',#183900,#26629);
#21403=LINE('',#183901,#26630);
#21404=LINE('',#183905,#26631);
#21405=LINE('',#183909,#26632);
#21406=LINE('',#183916,#26633);
#21407=LINE('',#183918,#26634);
#21408=LINE('',#183920,#26635);
#21409=LINE('',#183924,#26636);
#21410=LINE('',#183926,#26637);
#21411=LINE('',#183930,#26638);
#21412=LINE('',#183934,#26639);
#21413=LINE('',#183935,#26640);
#21414=LINE('',#183941,#26641);
#21415=LINE('',#183943,#26642);
#21416=LINE('',#183945,#26643);
#21417=LINE('',#183949,#26644);
#21418=LINE('',#183951,#26645);
#21419=LINE('',#183955,#26646);
#21420=LINE('',#183959,#26647);
#21421=LINE('',#183960,#26648);
#21422=LINE('',#183964,#26649);
#21423=LINE('',#183968,#26650);
#21424=LINE('',#183975,#26651);
#21425=LINE('',#183977,#26652);
#21426=LINE('',#183979,#26653);
#21427=LINE('',#183983,#26654);
#21428=LINE('',#183985,#26655);
#21429=LINE('',#183989,#26656);
#21430=LINE('',#183993,#26657);
#21431=LINE('',#183994,#26658);
#21432=LINE('',#184000,#26659);
#21433=LINE('',#184002,#26660);
#21434=LINE('',#184004,#26661);
#21435=LINE('',#184008,#26662);
#21436=LINE('',#184010,#26663);
#21437=LINE('',#184014,#26664);
#21438=LINE('',#184018,#26665);
#21439=LINE('',#184019,#26666);
#21440=LINE('',#184023,#26667);
#21441=LINE('',#184027,#26668);
#21442=LINE('',#184034,#26669);
#21443=LINE('',#184036,#26670);
#21444=LINE('',#184038,#26671);
#21445=LINE('',#184042,#26672);
#21446=LINE('',#184044,#26673);
#21447=LINE('',#184048,#26674);
#21448=LINE('',#184052,#26675);
#21449=LINE('',#184053,#26676);
#21450=LINE('',#184059,#26677);
#21451=LINE('',#184061,#26678);
#21452=LINE('',#184063,#26679);
#21453=LINE('',#184067,#26680);
#21454=LINE('',#184069,#26681);
#21455=LINE('',#184073,#26682);
#21456=LINE('',#184077,#26683);
#21457=LINE('',#184078,#26684);
#21458=LINE('',#184082,#26685);
#21459=LINE('',#184086,#26686);
#21460=LINE('',#184093,#26687);
#21461=LINE('',#184095,#26688);
#21462=LINE('',#184097,#26689);
#21463=LINE('',#184101,#26690);
#21464=LINE('',#184103,#26691);
#21465=LINE('',#184107,#26692);
#21466=LINE('',#184111,#26693);
#21467=LINE('',#184112,#26694);
#21468=LINE('',#184118,#26695);
#21469=LINE('',#184120,#26696);
#21470=LINE('',#184122,#26697);
#21471=LINE('',#184126,#26698);
#21472=LINE('',#184128,#26699);
#21473=LINE('',#184132,#26700);
#21474=LINE('',#184136,#26701);
#21475=LINE('',#184137,#26702);
#21476=LINE('',#184141,#26703);
#21477=LINE('',#184145,#26704);
#21478=LINE('',#184152,#26705);
#21479=LINE('',#184154,#26706);
#21480=LINE('',#184156,#26707);
#21481=LINE('',#184160,#26708);
#21482=LINE('',#184162,#26709);
#21483=LINE('',#184166,#26710);
#21484=LINE('',#184170,#26711);
#21485=LINE('',#184171,#26712);
#21486=LINE('',#184177,#26713);
#21487=LINE('',#184179,#26714);
#21488=LINE('',#184181,#26715);
#21489=LINE('',#184185,#26716);
#21490=LINE('',#184187,#26717);
#21491=LINE('',#184191,#26718);
#21492=LINE('',#184195,#26719);
#21493=LINE('',#184196,#26720);
#21494=LINE('',#184198,#26721);
#21495=LINE('',#184199,#26722);
#21496=LINE('',#184205,#26723);
#21497=LINE('',#184207,#26724);
#21498=LINE('',#184209,#26725);
#21499=LINE('',#184213,#26726);
#21500=LINE('',#184215,#26727);
#21501=LINE('',#184219,#26728);
#21502=LINE('',#184223,#26729);
#21503=LINE('',#184224,#26730);
#21504=LINE('',#184230,#26731);
#21505=LINE('',#184232,#26732);
#21506=LINE('',#184234,#26733);
#21507=LINE('',#184238,#26734);
#21508=LINE('',#184240,#26735);
#21509=LINE('',#184244,#26736);
#21510=LINE('',#184248,#26737);
#21511=LINE('',#184249,#26738);
#21512=LINE('',#184253,#26739);
#21513=LINE('',#184257,#26740);
#21514=LINE('',#184264,#26741);
#21515=LINE('',#184266,#26742);
#21516=LINE('',#184268,#26743);
#21517=LINE('',#184272,#26744);
#21518=LINE('',#184274,#26745);
#21519=LINE('',#184278,#26746);
#21520=LINE('',#184282,#26747);
#21521=LINE('',#184283,#26748);
#21522=LINE('',#184289,#26749);
#21523=LINE('',#184291,#26750);
#21524=LINE('',#184293,#26751);
#21525=LINE('',#184297,#26752);
#21526=LINE('',#184299,#26753);
#21527=LINE('',#184303,#26754);
#21528=LINE('',#184307,#26755);
#21529=LINE('',#184308,#26756);
#21530=LINE('',#184312,#26757);
#21531=LINE('',#184316,#26758);
#21532=LINE('',#184323,#26759);
#21533=LINE('',#184325,#26760);
#21534=LINE('',#184327,#26761);
#21535=LINE('',#184331,#26762);
#21536=LINE('',#184333,#26763);
#21537=LINE('',#184337,#26764);
#21538=LINE('',#184341,#26765);
#21539=LINE('',#184342,#26766);
#21540=LINE('',#184348,#26767);
#21541=LINE('',#184350,#26768);
#21542=LINE('',#184352,#26769);
#21543=LINE('',#184356,#26770);
#21544=LINE('',#184358,#26771);
#21545=LINE('',#184362,#26772);
#21546=LINE('',#184366,#26773);
#21547=LINE('',#184367,#26774);
#21548=LINE('',#184371,#26775);
#21549=LINE('',#184375,#26776);
#21550=LINE('',#184382,#26777);
#21551=LINE('',#184384,#26778);
#21552=LINE('',#184386,#26779);
#21553=LINE('',#184390,#26780);
#21554=LINE('',#184392,#26781);
#21555=LINE('',#184396,#26782);
#21556=LINE('',#184400,#26783);
#21557=LINE('',#184401,#26784);
#21558=LINE('',#184407,#26785);
#21559=LINE('',#184409,#26786);
#21560=LINE('',#184411,#26787);
#21561=LINE('',#184415,#26788);
#21562=LINE('',#184417,#26789);
#21563=LINE('',#184421,#26790);
#21564=LINE('',#184425,#26791);
#21565=LINE('',#184426,#26792);
#21566=LINE('',#184430,#26793);
#21567=LINE('',#184434,#26794);
#21568=LINE('',#184441,#26795);
#21569=LINE('',#184443,#26796);
#21570=LINE('',#184445,#26797);
#21571=LINE('',#184449,#26798);
#21572=LINE('',#184451,#26799);
#21573=LINE('',#184455,#26800);
#21574=LINE('',#184459,#26801);
#21575=LINE('',#184460,#26802);
#21576=LINE('',#184466,#26803);
#21577=LINE('',#184468,#26804);
#21578=LINE('',#184470,#26805);
#21579=LINE('',#184474,#26806);
#21580=LINE('',#184476,#26807);
#21581=LINE('',#184480,#26808);
#21582=LINE('',#184484,#26809);
#21583=LINE('',#184485,#26810);
#21584=LINE('',#184489,#26811);
#21585=LINE('',#184493,#26812);
#21586=LINE('',#184500,#26813);
#21587=LINE('',#184502,#26814);
#21588=LINE('',#184504,#26815);
#21589=LINE('',#184508,#26816);
#21590=LINE('',#184510,#26817);
#21591=LINE('',#184514,#26818);
#21592=LINE('',#184518,#26819);
#21593=LINE('',#184519,#26820);
#21594=LINE('',#184525,#26821);
#21595=LINE('',#184527,#26822);
#21596=LINE('',#184529,#26823);
#21597=LINE('',#184533,#26824);
#21598=LINE('',#184535,#26825);
#21599=LINE('',#184539,#26826);
#21600=LINE('',#184543,#26827);
#21601=LINE('',#184544,#26828);
#21602=LINE('',#184548,#26829);
#21603=LINE('',#184552,#26830);
#21604=LINE('',#184559,#26831);
#21605=LINE('',#184561,#26832);
#21606=LINE('',#184563,#26833);
#21607=LINE('',#184567,#26834);
#21608=LINE('',#184569,#26835);
#21609=LINE('',#184573,#26836);
#21610=LINE('',#184577,#26837);
#21611=LINE('',#184578,#26838);
#21612=LINE('',#184584,#26839);
#21613=LINE('',#184586,#26840);
#21614=LINE('',#184588,#26841);
#21615=LINE('',#184592,#26842);
#21616=LINE('',#184594,#26843);
#21617=LINE('',#184598,#26844);
#21618=LINE('',#184602,#26845);
#21619=LINE('',#184603,#26846);
#21620=LINE('',#184607,#26847);
#21621=LINE('',#184611,#26848);
#21622=LINE('',#184618,#26849);
#21623=LINE('',#184620,#26850);
#21624=LINE('',#184622,#26851);
#21625=LINE('',#184626,#26852);
#21626=LINE('',#184628,#26853);
#21627=LINE('',#184632,#26854);
#21628=LINE('',#184636,#26855);
#21629=LINE('',#184637,#26856);
#21630=LINE('',#184643,#26857);
#21631=LINE('',#184645,#26858);
#21632=LINE('',#184647,#26859);
#21633=LINE('',#184651,#26860);
#21634=LINE('',#184653,#26861);
#21635=LINE('',#184657,#26862);
#21636=LINE('',#184661,#26863);
#21637=LINE('',#184662,#26864);
#21638=LINE('',#184666,#26865);
#21639=LINE('',#184670,#26866);
#21640=LINE('',#184677,#26867);
#21641=LINE('',#184679,#26868);
#21642=LINE('',#184681,#26869);
#21643=LINE('',#184685,#26870);
#21644=LINE('',#184687,#26871);
#21645=LINE('',#184691,#26872);
#21646=LINE('',#184695,#26873);
#21647=LINE('',#184696,#26874);
#21648=LINE('',#184702,#26875);
#21649=LINE('',#184704,#26876);
#21650=LINE('',#184706,#26877);
#21651=LINE('',#184710,#26878);
#21652=LINE('',#184712,#26879);
#21653=LINE('',#184716,#26880);
#21654=LINE('',#184720,#26881);
#21655=LINE('',#184721,#26882);
#21656=LINE('',#184725,#26883);
#21657=LINE('',#184729,#26884);
#21658=LINE('',#184736,#26885);
#21659=LINE('',#184738,#26886);
#21660=LINE('',#184740,#26887);
#21661=LINE('',#184744,#26888);
#21662=LINE('',#184746,#26889);
#21663=LINE('',#184750,#26890);
#21664=LINE('',#184754,#26891);
#21665=LINE('',#184755,#26892);
#21666=LINE('',#184761,#26893);
#21667=LINE('',#184763,#26894);
#21668=LINE('',#184765,#26895);
#21669=LINE('',#184769,#26896);
#21670=LINE('',#184771,#26897);
#21671=LINE('',#184775,#26898);
#21672=LINE('',#184779,#26899);
#21673=LINE('',#184780,#26900);
#21674=LINE('',#184784,#26901);
#21675=LINE('',#184788,#26902);
#21676=LINE('',#184795,#26903);
#21677=LINE('',#184797,#26904);
#21678=LINE('',#184799,#26905);
#21679=LINE('',#184803,#26906);
#21680=LINE('',#184805,#26907);
#21681=LINE('',#184809,#26908);
#21682=LINE('',#184813,#26909);
#21683=LINE('',#184814,#26910);
#21684=LINE('',#184820,#26911);
#21685=LINE('',#184822,#26912);
#21686=LINE('',#184824,#26913);
#21687=LINE('',#184828,#26914);
#21688=LINE('',#184830,#26915);
#21689=LINE('',#184834,#26916);
#21690=LINE('',#184838,#26917);
#21691=LINE('',#184839,#26918);
#21692=LINE('',#184843,#26919);
#21693=LINE('',#184847,#26920);
#21694=LINE('',#184854,#26921);
#21695=LINE('',#184856,#26922);
#21696=LINE('',#184858,#26923);
#21697=LINE('',#184862,#26924);
#21698=LINE('',#184864,#26925);
#21699=LINE('',#184868,#26926);
#21700=LINE('',#184872,#26927);
#21701=LINE('',#184873,#26928);
#21702=LINE('',#184879,#26929);
#21703=LINE('',#184881,#26930);
#21704=LINE('',#184883,#26931);
#21705=LINE('',#184887,#26932);
#21706=LINE('',#184889,#26933);
#21707=LINE('',#184893,#26934);
#21708=LINE('',#184897,#26935);
#21709=LINE('',#184898,#26936);
#21710=LINE('',#184902,#26937);
#21711=LINE('',#184906,#26938);
#21712=LINE('',#184913,#26939);
#21713=LINE('',#184915,#26940);
#21714=LINE('',#184917,#26941);
#21715=LINE('',#184921,#26942);
#21716=LINE('',#184923,#26943);
#21717=LINE('',#184927,#26944);
#21718=LINE('',#184931,#26945);
#21719=LINE('',#184932,#26946);
#21720=LINE('',#184938,#26947);
#21721=LINE('',#184940,#26948);
#21722=LINE('',#184942,#26949);
#21723=LINE('',#184946,#26950);
#21724=LINE('',#184948,#26951);
#21725=LINE('',#184952,#26952);
#21726=LINE('',#184956,#26953);
#21727=LINE('',#184957,#26954);
#21728=LINE('',#184961,#26955);
#21729=LINE('',#184965,#26956);
#21730=LINE('',#184972,#26957);
#21731=LINE('',#184974,#26958);
#21732=LINE('',#184976,#26959);
#21733=LINE('',#184980,#26960);
#21734=LINE('',#184982,#26961);
#21735=LINE('',#184986,#26962);
#21736=LINE('',#184990,#26963);
#21737=LINE('',#184991,#26964);
#21738=LINE('',#184997,#26965);
#21739=LINE('',#184999,#26966);
#21740=LINE('',#185001,#26967);
#21741=LINE('',#185005,#26968);
#21742=LINE('',#185007,#26969);
#21743=LINE('',#185011,#26970);
#21744=LINE('',#185015,#26971);
#21745=LINE('',#185016,#26972);
#21746=LINE('',#185020,#26973);
#21747=LINE('',#185024,#26974);
#21748=LINE('',#185031,#26975);
#21749=LINE('',#185033,#26976);
#21750=LINE('',#185035,#26977);
#21751=LINE('',#185039,#26978);
#21752=LINE('',#185041,#26979);
#21753=LINE('',#185045,#26980);
#21754=LINE('',#185049,#26981);
#21755=LINE('',#185050,#26982);
#21756=LINE('',#185056,#26983);
#21757=LINE('',#185058,#26984);
#21758=LINE('',#185060,#26985);
#21759=LINE('',#185064,#26986);
#21760=LINE('',#185066,#26987);
#21761=LINE('',#185070,#26988);
#21762=LINE('',#185074,#26989);
#21763=LINE('',#185075,#26990);
#21764=LINE('',#185077,#26991);
#21765=LINE('',#185078,#26992);
#21766=LINE('',#185084,#26993);
#21767=LINE('',#185086,#26994);
#21768=LINE('',#185088,#26995);
#21769=LINE('',#185092,#26996);
#21770=LINE('',#185094,#26997);
#21771=LINE('',#185098,#26998);
#21772=LINE('',#185102,#26999);
#21773=LINE('',#185103,#27000);
#21774=LINE('',#185109,#27001);
#21775=LINE('',#185111,#27002);
#21776=LINE('',#185113,#27003);
#21777=LINE('',#185117,#27004);
#21778=LINE('',#185119,#27005);
#21779=LINE('',#185123,#27006);
#21780=LINE('',#185127,#27007);
#21781=LINE('',#185128,#27008);
#21782=LINE('',#185132,#27009);
#21783=LINE('',#185136,#27010);
#21784=LINE('',#185143,#27011);
#21785=LINE('',#185145,#27012);
#21786=LINE('',#185147,#27013);
#21787=LINE('',#185151,#27014);
#21788=LINE('',#185153,#27015);
#21789=LINE('',#185157,#27016);
#21790=LINE('',#185161,#27017);
#21791=LINE('',#185162,#27018);
#21792=LINE('',#185168,#27019);
#21793=LINE('',#185170,#27020);
#21794=LINE('',#185172,#27021);
#21795=LINE('',#185176,#27022);
#21796=LINE('',#185178,#27023);
#21797=LINE('',#185182,#27024);
#21798=LINE('',#185186,#27025);
#21799=LINE('',#185187,#27026);
#21800=LINE('',#185191,#27027);
#21801=LINE('',#185195,#27028);
#21802=LINE('',#185202,#27029);
#21803=LINE('',#185204,#27030);
#21804=LINE('',#185206,#27031);
#21805=LINE('',#185210,#27032);
#21806=LINE('',#185212,#27033);
#21807=LINE('',#185216,#27034);
#21808=LINE('',#185220,#27035);
#21809=LINE('',#185221,#27036);
#21810=LINE('',#185227,#27037);
#21811=LINE('',#185229,#27038);
#21812=LINE('',#185231,#27039);
#21813=LINE('',#185235,#27040);
#21814=LINE('',#185237,#27041);
#21815=LINE('',#185241,#27042);
#21816=LINE('',#185245,#27043);
#21817=LINE('',#185246,#27044);
#21818=LINE('',#185250,#27045);
#21819=LINE('',#185254,#27046);
#21820=LINE('',#185261,#27047);
#21821=LINE('',#185263,#27048);
#21822=LINE('',#185265,#27049);
#21823=LINE('',#185269,#27050);
#21824=LINE('',#185271,#27051);
#21825=LINE('',#185275,#27052);
#21826=LINE('',#185279,#27053);
#21827=LINE('',#185280,#27054);
#21828=LINE('',#185286,#27055);
#21829=LINE('',#185288,#27056);
#21830=LINE('',#185290,#27057);
#21831=LINE('',#185294,#27058);
#21832=LINE('',#185296,#27059);
#21833=LINE('',#185300,#27060);
#21834=LINE('',#185304,#27061);
#21835=LINE('',#185305,#27062);
#21836=LINE('',#185309,#27063);
#21837=LINE('',#185313,#27064);
#21838=LINE('',#185320,#27065);
#21839=LINE('',#185322,#27066);
#21840=LINE('',#185324,#27067);
#21841=LINE('',#185328,#27068);
#21842=LINE('',#185330,#27069);
#21843=LINE('',#185334,#27070);
#21844=LINE('',#185338,#27071);
#21845=LINE('',#185339,#27072);
#21846=LINE('',#185345,#27073);
#21847=LINE('',#185347,#27074);
#21848=LINE('',#185349,#27075);
#21849=LINE('',#185353,#27076);
#21850=LINE('',#185355,#27077);
#21851=LINE('',#185359,#27078);
#21852=LINE('',#185363,#27079);
#21853=LINE('',#185364,#27080);
#21854=LINE('',#185368,#27081);
#21855=LINE('',#185372,#27082);
#21856=LINE('',#185379,#27083);
#21857=LINE('',#185381,#27084);
#21858=LINE('',#185383,#27085);
#21859=LINE('',#185387,#27086);
#21860=LINE('',#185389,#27087);
#21861=LINE('',#185393,#27088);
#21862=LINE('',#185397,#27089);
#21863=LINE('',#185398,#27090);
#21864=LINE('',#185404,#27091);
#21865=LINE('',#185406,#27092);
#21866=LINE('',#185408,#27093);
#21867=LINE('',#185412,#27094);
#21868=LINE('',#185414,#27095);
#21869=LINE('',#185418,#27096);
#21870=LINE('',#185422,#27097);
#21871=LINE('',#185423,#27098);
#21872=LINE('',#185427,#27099);
#21873=LINE('',#185431,#27100);
#21874=LINE('',#185438,#27101);
#21875=LINE('',#185440,#27102);
#21876=LINE('',#185442,#27103);
#21877=LINE('',#185446,#27104);
#21878=LINE('',#185448,#27105);
#21879=LINE('',#185452,#27106);
#21880=LINE('',#185456,#27107);
#21881=LINE('',#185457,#27108);
#21882=LINE('',#185463,#27109);
#21883=LINE('',#185465,#27110);
#21884=LINE('',#185467,#27111);
#21885=LINE('',#185471,#27112);
#21886=LINE('',#185473,#27113);
#21887=LINE('',#185477,#27114);
#21888=LINE('',#185481,#27115);
#21889=LINE('',#185482,#27116);
#21890=LINE('',#185486,#27117);
#21891=LINE('',#185490,#27118);
#21892=LINE('',#185497,#27119);
#21893=LINE('',#185499,#27120);
#21894=LINE('',#185501,#27121);
#21895=LINE('',#185505,#27122);
#21896=LINE('',#185507,#27123);
#21897=LINE('',#185511,#27124);
#21898=LINE('',#185515,#27125);
#21899=LINE('',#185516,#27126);
#21900=LINE('',#185522,#27127);
#21901=LINE('',#185524,#27128);
#21902=LINE('',#185526,#27129);
#21903=LINE('',#185530,#27130);
#21904=LINE('',#185532,#27131);
#21905=LINE('',#185536,#27132);
#21906=LINE('',#185540,#27133);
#21907=LINE('',#185541,#27134);
#21908=LINE('',#185545,#27135);
#21909=LINE('',#185549,#27136);
#21910=LINE('',#185556,#27137);
#21911=LINE('',#185558,#27138);
#21912=LINE('',#185560,#27139);
#21913=LINE('',#185564,#27140);
#21914=LINE('',#185566,#27141);
#21915=LINE('',#185570,#27142);
#21916=LINE('',#185574,#27143);
#21917=LINE('',#185575,#27144);
#21918=LINE('',#185581,#27145);
#21919=LINE('',#185583,#27146);
#21920=LINE('',#185585,#27147);
#21921=LINE('',#185589,#27148);
#21922=LINE('',#185591,#27149);
#21923=LINE('',#185595,#27150);
#21924=LINE('',#185599,#27151);
#21925=LINE('',#185600,#27152);
#21926=LINE('',#185604,#27153);
#21927=LINE('',#185608,#27154);
#21928=LINE('',#185615,#27155);
#21929=LINE('',#185617,#27156);
#21930=LINE('',#185619,#27157);
#21931=LINE('',#185623,#27158);
#21932=LINE('',#185625,#27159);
#21933=LINE('',#185629,#27160);
#21934=LINE('',#185633,#27161);
#21935=LINE('',#185634,#27162);
#21936=LINE('',#185640,#27163);
#21937=LINE('',#185642,#27164);
#21938=LINE('',#185644,#27165);
#21939=LINE('',#185648,#27166);
#21940=LINE('',#185650,#27167);
#21941=LINE('',#185654,#27168);
#21942=LINE('',#185658,#27169);
#21943=LINE('',#185659,#27170);
#21944=LINE('',#185663,#27171);
#21945=LINE('',#185667,#27172);
#21946=LINE('',#185674,#27173);
#21947=LINE('',#185676,#27174);
#21948=LINE('',#185678,#27175);
#21949=LINE('',#185682,#27176);
#21950=LINE('',#185684,#27177);
#21951=LINE('',#185688,#27178);
#21952=LINE('',#185692,#27179);
#21953=LINE('',#185693,#27180);
#21954=LINE('',#185699,#27181);
#21955=LINE('',#185701,#27182);
#21956=LINE('',#185703,#27183);
#21957=LINE('',#185707,#27184);
#21958=LINE('',#185709,#27185);
#21959=LINE('',#185713,#27186);
#21960=LINE('',#185717,#27187);
#21961=LINE('',#185718,#27188);
#21962=LINE('',#185722,#27189);
#21963=LINE('',#185726,#27190);
#21964=LINE('',#185733,#27191);
#21965=LINE('',#185735,#27192);
#21966=LINE('',#185737,#27193);
#21967=LINE('',#185741,#27194);
#21968=LINE('',#185743,#27195);
#21969=LINE('',#185747,#27196);
#21970=LINE('',#185751,#27197);
#21971=LINE('',#185752,#27198);
#21972=LINE('',#185758,#27199);
#21973=LINE('',#185760,#27200);
#21974=LINE('',#185762,#27201);
#21975=LINE('',#185766,#27202);
#21976=LINE('',#185768,#27203);
#21977=LINE('',#185772,#27204);
#21978=LINE('',#185776,#27205);
#21979=LINE('',#185777,#27206);
#21980=LINE('',#185781,#27207);
#21981=LINE('',#185785,#27208);
#21982=LINE('',#185792,#27209);
#21983=LINE('',#185794,#27210);
#21984=LINE('',#185796,#27211);
#21985=LINE('',#185800,#27212);
#21986=LINE('',#185802,#27213);
#21987=LINE('',#185806,#27214);
#21988=LINE('',#185810,#27215);
#21989=LINE('',#185811,#27216);
#21990=LINE('',#185817,#27217);
#21991=LINE('',#185819,#27218);
#21992=LINE('',#185821,#27219);
#21993=LINE('',#185825,#27220);
#21994=LINE('',#185827,#27221);
#21995=LINE('',#185831,#27222);
#21996=LINE('',#185835,#27223);
#21997=LINE('',#185836,#27224);
#21998=LINE('',#185840,#27225);
#21999=LINE('',#185844,#27226);
#22000=LINE('',#185851,#27227);
#22001=LINE('',#185853,#27228);
#22002=LINE('',#185855,#27229);
#22003=LINE('',#185859,#27230);
#22004=LINE('',#185861,#27231);
#22005=LINE('',#185865,#27232);
#22006=LINE('',#185869,#27233);
#22007=LINE('',#185870,#27234);
#22008=LINE('',#185876,#27235);
#22009=LINE('',#185878,#27236);
#22010=LINE('',#185880,#27237);
#22011=LINE('',#185884,#27238);
#22012=LINE('',#185886,#27239);
#22013=LINE('',#185890,#27240);
#22014=LINE('',#185894,#27241);
#22015=LINE('',#185895,#27242);
#22016=LINE('',#185899,#27243);
#22017=LINE('',#185903,#27244);
#22018=LINE('',#185910,#27245);
#22019=LINE('',#185912,#27246);
#22020=LINE('',#185914,#27247);
#22021=LINE('',#185918,#27248);
#22022=LINE('',#185920,#27249);
#22023=LINE('',#185924,#27250);
#22024=LINE('',#185928,#27251);
#22025=LINE('',#185929,#27252);
#22026=LINE('',#185935,#27253);
#22027=LINE('',#185937,#27254);
#22028=LINE('',#185939,#27255);
#22029=LINE('',#185943,#27256);
#22030=LINE('',#185945,#27257);
#22031=LINE('',#185949,#27258);
#22032=LINE('',#185953,#27259);
#22033=LINE('',#185954,#27260);
#22034=LINE('',#210557,#27261);
#22035=LINE('',#210560,#27262);
#22036=LINE('',#210610,#27263);
#22037=LINE('',#210614,#27264);
#22038=LINE('',#210703,#27265);
#22039=LINE('',#210707,#27266);
#22040=LINE('',#210796,#27267);
#22041=LINE('',#210800,#27268);
#22042=LINE('',#210889,#27269);
#22043=LINE('',#210893,#27270);
#22044=LINE('',#210982,#27271);
#22045=LINE('',#210986,#27272);
#22046=LINE('',#211075,#27273);
#22047=LINE('',#211079,#27274);
#22048=LINE('',#211168,#27275);
#22049=LINE('',#211172,#27276);
#22050=LINE('',#211261,#27277);
#22051=LINE('',#211265,#27278);
#22052=LINE('',#211354,#27279);
#22053=LINE('',#211358,#27280);
#22054=LINE('',#211447,#27281);
#22055=LINE('',#211451,#27282);
#22056=LINE('',#211540,#27283);
#22057=LINE('',#211544,#27284);
#22058=LINE('',#211633,#27285);
#22059=LINE('',#211637,#27286);
#22060=LINE('',#211726,#27287);
#22061=LINE('',#211730,#27288);
#22062=LINE('',#211819,#27289);
#22063=LINE('',#211823,#27290);
#22064=LINE('',#211912,#27291);
#22065=LINE('',#211916,#27292);
#22066=LINE('',#212005,#27293);
#22067=LINE('',#212009,#27294);
#22068=LINE('',#212098,#27295);
#22069=LINE('',#212102,#27296);
#22070=LINE('',#212191,#27297);
#22071=LINE('',#212195,#27298);
#22072=LINE('',#212284,#27299);
#22073=LINE('',#212288,#27300);
#22074=LINE('',#212377,#27301);
#22075=LINE('',#212381,#27302);
#22076=LINE('',#212470,#27303);
#22077=LINE('',#212474,#27304);
#22078=LINE('',#212563,#27305);
#22079=LINE('',#212567,#27306);
#22080=LINE('',#212656,#27307);
#22081=LINE('',#212660,#27308);
#22082=LINE('',#212749,#27309);
#22083=LINE('',#212753,#27310);
#22084=LINE('',#212842,#27311);
#22085=LINE('',#212846,#27312);
#22086=LINE('',#212935,#27313);
#22087=LINE('',#212939,#27314);
#22088=LINE('',#213028,#27315);
#22089=LINE('',#213032,#27316);
#22090=LINE('',#213121,#27317);
#22091=LINE('',#213125,#27318);
#22092=LINE('',#213214,#27319);
#22093=LINE('',#213218,#27320);
#22094=LINE('',#213307,#27321);
#22095=LINE('',#213311,#27322);
#22096=LINE('',#213352,#27323);
#22097=LINE('',#213398,#27324);
#22098=LINE('',#213402,#27325);
#22099=LINE('',#213491,#27326);
#22100=LINE('',#213495,#27327);
#22101=LINE('',#213584,#27328);
#22102=LINE('',#213588,#27329);
#22103=LINE('',#213677,#27330);
#22104=LINE('',#213681,#27331);
#22105=LINE('',#213770,#27332);
#22106=LINE('',#213774,#27333);
#22107=LINE('',#213863,#27334);
#22108=LINE('',#213867,#27335);
#22109=LINE('',#213956,#27336);
#22110=LINE('',#213960,#27337);
#22111=LINE('',#214049,#27338);
#22112=LINE('',#214053,#27339);
#22113=LINE('',#214142,#27340);
#22114=LINE('',#214146,#27341);
#22115=LINE('',#214235,#27342);
#22116=LINE('',#214239,#27343);
#22117=LINE('',#214328,#27344);
#22118=LINE('',#214332,#27345);
#22119=LINE('',#214421,#27346);
#22120=LINE('',#214425,#27347);
#22121=LINE('',#214514,#27348);
#22122=LINE('',#214518,#27349);
#22123=LINE('',#214607,#27350);
#22124=LINE('',#214611,#27351);
#22125=LINE('',#214700,#27352);
#22126=LINE('',#214704,#27353);
#22127=LINE('',#214790,#27354);
#22128=LINE('',#214794,#27355);
#22129=LINE('',#214883,#27356);
#22130=LINE('',#214887,#27357);
#22131=LINE('',#214976,#27358);
#22132=LINE('',#214980,#27359);
#22133=LINE('',#215069,#27360);
#22134=LINE('',#215073,#27361);
#22135=LINE('',#215162,#27362);
#22136=LINE('',#215166,#27363);
#22137=LINE('',#215255,#27364);
#22138=LINE('',#215259,#27365);
#22139=LINE('',#215348,#27366);
#22140=LINE('',#215352,#27367);
#22141=LINE('',#215441,#27368);
#22142=LINE('',#215445,#27369);
#22143=LINE('',#215534,#27370);
#22144=LINE('',#215538,#27371);
#22145=LINE('',#215627,#27372);
#22146=LINE('',#215631,#27373);
#22147=LINE('',#215720,#27374);
#22148=LINE('',#215724,#27375);
#22149=LINE('',#215813,#27376);
#22150=LINE('',#215817,#27377);
#22151=LINE('',#215906,#27378);
#22152=LINE('',#215910,#27379);
#22153=LINE('',#215999,#27380);
#22154=LINE('',#216003,#27381);
#22155=LINE('',#216092,#27382);
#22156=LINE('',#216096,#27383);
#22157=LINE('',#216177,#27384);
#22158=LINE('',#216181,#27385);
#22159=LINE('',#216264,#27386);
#22160=LINE('',#216268,#27387);
#22161=LINE('',#216351,#27388);
#22162=LINE('',#216355,#27389);
#22163=LINE('',#216438,#27390);
#22164=LINE('',#216442,#27391);
#22165=LINE('',#216525,#27392);
#22166=LINE('',#216529,#27393);
#22167=LINE('',#216612,#27394);
#22168=LINE('',#216616,#27395);
#22169=LINE('',#216699,#27396);
#22170=LINE('',#216703,#27397);
#22171=LINE('',#216786,#27398);
#22172=LINE('',#216790,#27399);
#22173=LINE('',#216873,#27400);
#22174=LINE('',#216877,#27401);
#22175=LINE('',#216960,#27402);
#22176=LINE('',#216964,#27403);
#22177=LINE('',#217047,#27404);
#22178=LINE('',#217051,#27405);
#22179=LINE('',#217134,#27406);
#22180=LINE('',#217138,#27407);
#22181=LINE('',#217221,#27408);
#22182=LINE('',#217225,#27409);
#22183=LINE('',#217308,#27410);
#22184=LINE('',#217312,#27411);
#22185=LINE('',#217395,#27412);
#22186=LINE('',#217399,#27413);
#22187=LINE('',#217482,#27414);
#22188=LINE('',#217486,#27415);
#22189=LINE('',#217569,#27416);
#22190=LINE('',#217573,#27417);
#22191=LINE('',#217656,#27418);
#22192=LINE('',#217660,#27419);
#22193=LINE('',#217743,#27420);
#22194=LINE('',#217747,#27421);
#22195=LINE('',#217830,#27422);
#22196=LINE('',#217834,#27423);
#22197=LINE('',#217917,#27424);
#22198=LINE('',#217921,#27425);
#22199=LINE('',#218004,#27426);
#22200=LINE('',#218008,#27427);
#22201=LINE('',#218091,#27428);
#22202=LINE('',#218095,#27429);
#22203=LINE('',#218178,#27430);
#22204=LINE('',#218182,#27431);
#22205=LINE('',#218265,#27432);
#22206=LINE('',#218269,#27433);
#22207=LINE('',#218352,#27434);
#22208=LINE('',#218356,#27435);
#22209=LINE('',#218439,#27436);
#22210=LINE('',#218443,#27437);
#22211=LINE('',#218526,#27438);
#22212=LINE('',#218530,#27439);
#22213=LINE('',#218613,#27440);
#22214=LINE('',#218617,#27441);
#22215=LINE('',#218700,#27442);
#22216=LINE('',#218704,#27443);
#22217=LINE('',#218748,#27444);
#22218=LINE('',#218790,#27445);
#22219=LINE('',#218794,#27446);
#22220=LINE('',#218877,#27447);
#22221=LINE('',#218881,#27448);
#22222=LINE('',#218964,#27449);
#22223=LINE('',#218968,#27450);
#22224=LINE('',#219051,#27451);
#22225=LINE('',#219055,#27452);
#22226=LINE('',#219138,#27453);
#22227=LINE('',#219142,#27454);
#22228=LINE('',#219225,#27455);
#22229=LINE('',#219229,#27456);
#22230=LINE('',#219312,#27457);
#22231=LINE('',#219316,#27458);
#22232=LINE('',#219399,#27459);
#22233=LINE('',#219403,#27460);
#22234=LINE('',#219486,#27461);
#22235=LINE('',#219490,#27462);
#22236=LINE('',#219573,#27463);
#22237=LINE('',#219577,#27464);
#22238=LINE('',#219660,#27465);
#22239=LINE('',#219664,#27466);
#22240=LINE('',#219747,#27467);
#22241=LINE('',#219751,#27468);
#22242=LINE('',#219834,#27469);
#22243=LINE('',#219838,#27470);
#22244=LINE('',#219921,#27471);
#22245=LINE('',#219925,#27472);
#22246=LINE('',#220008,#27473);
#22247=LINE('',#220012,#27474);
#22248=LINE('',#220092,#27475);
#22249=LINE('',#220096,#27476);
#22250=LINE('',#220179,#27477);
#22251=LINE('',#220183,#27478);
#22252=LINE('',#220266,#27479);
#22253=LINE('',#220270,#27480);
#22254=LINE('',#220353,#27481);
#22255=LINE('',#220357,#27482);
#22256=LINE('',#220440,#27483);
#22257=LINE('',#220444,#27484);
#22258=LINE('',#220527,#27485);
#22259=LINE('',#220531,#27486);
#22260=LINE('',#220614,#27487);
#22261=LINE('',#220618,#27488);
#22262=LINE('',#220701,#27489);
#22263=LINE('',#220705,#27490);
#22264=LINE('',#220788,#27491);
#22265=LINE('',#220792,#27492);
#22266=LINE('',#220875,#27493);
#22267=LINE('',#220879,#27494);
#22268=LINE('',#220962,#27495);
#22269=LINE('',#220966,#27496);
#22270=LINE('',#221049,#27497);
#22271=LINE('',#221053,#27498);
#22272=LINE('',#221136,#27499);
#22273=LINE('',#221140,#27500);
#22274=LINE('',#221223,#27501);
#22275=LINE('',#221227,#27502);
#22276=LINE('',#221310,#27503);
#22277=LINE('',#221314,#27504);
#22278=LINE('',#221359,#27505);
#22279=LINE('',#221363,#27506);
#22280=LINE('',#221370,#27507);
#22281=LINE('',#221374,#27508);
#22282=LINE('',#221382,#27509);
#22283=LINE('',#221383,#27510);
#22284=LINE('',#221389,#27511);
#22285=LINE('',#221392,#27512);
#22286=LINE('',#221398,#27513);
#22287=LINE('',#221402,#27514);
#22288=LINE('',#221410,#27515);
#22289=LINE('',#221411,#27516);
#22290=LINE('',#221429,#27517);
#22291=LINE('',#221436,#27518);
#22292=LINE('',#221439,#27519);
#22293=LINE('',#221442,#27520);
#22294=LINE('',#221448,#27521);
#22295=LINE('',#221451,#27522);
#22296=LINE('',#221457,#27523);
#22297=LINE('',#221464,#27524);
#22298=LINE('',#221467,#27525);
#22299=LINE('',#221470,#27526);
#22300=LINE('',#221488,#27527);
#22301=LINE('',#221495,#27528);
#22302=LINE('',#221498,#27529);
#22303=LINE('',#221501,#27530);
#22304=LINE('',#221507,#27531);
#22305=LINE('',#221510,#27532);
#22306=LINE('',#221516,#27533);
#22307=LINE('',#221523,#27534);
#22308=LINE('',#221526,#27535);
#22309=LINE('',#221529,#27536);
#22310=LINE('',#221547,#27537);
#22311=LINE('',#221554,#27538);
#22312=LINE('',#221557,#27539);
#22313=LINE('',#221560,#27540);
#22314=LINE('',#221566,#27541);
#22315=LINE('',#221569,#27542);
#22316=LINE('',#221575,#27543);
#22317=LINE('',#221582,#27544);
#22318=LINE('',#221585,#27545);
#22319=LINE('',#221588,#27546);
#22320=LINE('',#221606,#27547);
#22321=LINE('',#221613,#27548);
#22322=LINE('',#221616,#27549);
#22323=LINE('',#221619,#27550);
#22324=LINE('',#221625,#27551);
#22325=LINE('',#221628,#27552);
#22326=LINE('',#221634,#27553);
#22327=LINE('',#221641,#27554);
#22328=LINE('',#221644,#27555);
#22329=LINE('',#221647,#27556);
#22330=LINE('',#221665,#27557);
#22331=LINE('',#221672,#27558);
#22332=LINE('',#221675,#27559);
#22333=LINE('',#221678,#27560);
#22334=LINE('',#221684,#27561);
#22335=LINE('',#221687,#27562);
#22336=LINE('',#221693,#27563);
#22337=LINE('',#221700,#27564);
#22338=LINE('',#221703,#27565);
#22339=LINE('',#221706,#27566);
#22340=LINE('',#221724,#27567);
#22341=LINE('',#221731,#27568);
#22342=LINE('',#221734,#27569);
#22343=LINE('',#221737,#27570);
#22344=LINE('',#221743,#27571);
#22345=LINE('',#221746,#27572);
#22346=LINE('',#221752,#27573);
#22347=LINE('',#221759,#27574);
#22348=LINE('',#221762,#27575);
#22349=LINE('',#221765,#27576);
#22350=LINE('',#221783,#27577);
#22351=LINE('',#221790,#27578);
#22352=LINE('',#221793,#27579);
#22353=LINE('',#221796,#27580);
#22354=LINE('',#221802,#27581);
#22355=LINE('',#221805,#27582);
#22356=LINE('',#221811,#27583);
#22357=LINE('',#221818,#27584);
#22358=LINE('',#221821,#27585);
#22359=LINE('',#221824,#27586);
#22360=LINE('',#221842,#27587);
#22361=LINE('',#221849,#27588);
#22362=LINE('',#221852,#27589);
#22363=LINE('',#221855,#27590);
#22364=LINE('',#221861,#27591);
#22365=LINE('',#221864,#27592);
#22366=LINE('',#221870,#27593);
#22367=LINE('',#221877,#27594);
#22368=LINE('',#221880,#27595);
#22369=LINE('',#221883,#27596);
#22370=LINE('',#221901,#27597);
#22371=LINE('',#221908,#27598);
#22372=LINE('',#221911,#27599);
#22373=LINE('',#221914,#27600);
#22374=LINE('',#221920,#27601);
#22375=LINE('',#221923,#27602);
#22376=LINE('',#221929,#27603);
#22377=LINE('',#221936,#27604);
#22378=LINE('',#221939,#27605);
#22379=LINE('',#221942,#27606);
#22380=LINE('',#221960,#27607);
#22381=LINE('',#221967,#27608);
#22382=LINE('',#221970,#27609);
#22383=LINE('',#221973,#27610);
#22384=LINE('',#221979,#27611);
#22385=LINE('',#221982,#27612);
#22386=LINE('',#221988,#27613);
#22387=LINE('',#221995,#27614);
#22388=LINE('',#221998,#27615);
#22389=LINE('',#222001,#27616);
#22390=LINE('',#222019,#27617);
#22391=LINE('',#222026,#27618);
#22392=LINE('',#222029,#27619);
#22393=LINE('',#222032,#27620);
#22394=LINE('',#222038,#27621);
#22395=LINE('',#222041,#27622);
#22396=LINE('',#222047,#27623);
#22397=LINE('',#222054,#27624);
#22398=LINE('',#222057,#27625);
#22399=LINE('',#222060,#27626);
#22400=LINE('',#222078,#27627);
#22401=LINE('',#222085,#27628);
#22402=LINE('',#222088,#27629);
#22403=LINE('',#222091,#27630);
#22404=LINE('',#222097,#27631);
#22405=LINE('',#222100,#27632);
#22406=LINE('',#222106,#27633);
#22407=LINE('',#222113,#27634);
#22408=LINE('',#222116,#27635);
#22409=LINE('',#222119,#27636);
#22410=LINE('',#222137,#27637);
#22411=LINE('',#222144,#27638);
#22412=LINE('',#222147,#27639);
#22413=LINE('',#222150,#27640);
#22414=LINE('',#222156,#27641);
#22415=LINE('',#222159,#27642);
#22416=LINE('',#222165,#27643);
#22417=LINE('',#222172,#27644);
#22418=LINE('',#222175,#27645);
#22419=LINE('',#222178,#27646);
#22420=LINE('',#222196,#27647);
#22421=LINE('',#222203,#27648);
#22422=LINE('',#222206,#27649);
#22423=LINE('',#222209,#27650);
#22424=LINE('',#222215,#27651);
#22425=LINE('',#222218,#27652);
#22426=LINE('',#222224,#27653);
#22427=LINE('',#222231,#27654);
#22428=LINE('',#222234,#27655);
#22429=LINE('',#222237,#27656);
#22430=LINE('',#222255,#27657);
#22431=LINE('',#222262,#27658);
#22432=LINE('',#222265,#27659);
#22433=LINE('',#222268,#27660);
#22434=LINE('',#222274,#27661);
#22435=LINE('',#222277,#27662);
#22436=LINE('',#222283,#27663);
#22437=LINE('',#222290,#27664);
#22438=LINE('',#222293,#27665);
#22439=LINE('',#222296,#27666);
#22440=LINE('',#222314,#27667);
#22441=LINE('',#222321,#27668);
#22442=LINE('',#222324,#27669);
#22443=LINE('',#222327,#27670);
#22444=LINE('',#222333,#27671);
#22445=LINE('',#222336,#27672);
#22446=LINE('',#222342,#27673);
#22447=LINE('',#222349,#27674);
#22448=LINE('',#222352,#27675);
#22449=LINE('',#222355,#27676);
#22450=LINE('',#222373,#27677);
#22451=LINE('',#222380,#27678);
#22452=LINE('',#222383,#27679);
#22453=LINE('',#222386,#27680);
#22454=LINE('',#222392,#27681);
#22455=LINE('',#222395,#27682);
#22456=LINE('',#222401,#27683);
#22457=LINE('',#222408,#27684);
#22458=LINE('',#222411,#27685);
#22459=LINE('',#222414,#27686);
#22460=LINE('',#222432,#27687);
#22461=LINE('',#222439,#27688);
#22462=LINE('',#222442,#27689);
#22463=LINE('',#222445,#27690);
#22464=LINE('',#222451,#27691);
#22465=LINE('',#222454,#27692);
#22466=LINE('',#222460,#27693);
#22467=LINE('',#222467,#27694);
#22468=LINE('',#222470,#27695);
#22469=LINE('',#222473,#27696);
#22470=LINE('',#222491,#27697);
#22471=LINE('',#222498,#27698);
#22472=LINE('',#222501,#27699);
#22473=LINE('',#222504,#27700);
#22474=LINE('',#222510,#27701);
#22475=LINE('',#222513,#27702);
#22476=LINE('',#222519,#27703);
#22477=LINE('',#222526,#27704);
#22478=LINE('',#222529,#27705);
#22479=LINE('',#222532,#27706);
#22480=LINE('',#222550,#27707);
#22481=LINE('',#222557,#27708);
#22482=LINE('',#222560,#27709);
#22483=LINE('',#222563,#27710);
#22484=LINE('',#222569,#27711);
#22485=LINE('',#222572,#27712);
#22486=LINE('',#222578,#27713);
#22487=LINE('',#222585,#27714);
#22488=LINE('',#222588,#27715);
#22489=LINE('',#222591,#27716);
#22490=LINE('',#222609,#27717);
#22491=LINE('',#222616,#27718);
#22492=LINE('',#222619,#27719);
#22493=LINE('',#222622,#27720);
#22494=LINE('',#222628,#27721);
#22495=LINE('',#222631,#27722);
#22496=LINE('',#222637,#27723);
#22497=LINE('',#222644,#27724);
#22498=LINE('',#222647,#27725);
#22499=LINE('',#222650,#27726);
#22500=LINE('',#222668,#27727);
#22501=LINE('',#222675,#27728);
#22502=LINE('',#222678,#27729);
#22503=LINE('',#222681,#27730);
#22504=LINE('',#222687,#27731);
#22505=LINE('',#222690,#27732);
#22506=LINE('',#222696,#27733);
#22507=LINE('',#222703,#27734);
#22508=LINE('',#222706,#27735);
#22509=LINE('',#222709,#27736);
#22510=LINE('',#222727,#27737);
#22511=LINE('',#222734,#27738);
#22512=LINE('',#222737,#27739);
#22513=LINE('',#222740,#27740);
#22514=LINE('',#222746,#27741);
#22515=LINE('',#222749,#27742);
#22516=LINE('',#222755,#27743);
#22517=LINE('',#222762,#27744);
#22518=LINE('',#222765,#27745);
#22519=LINE('',#222768,#27746);
#22520=LINE('',#222786,#27747);
#22521=LINE('',#222793,#27748);
#22522=LINE('',#222796,#27749);
#22523=LINE('',#222799,#27750);
#22524=LINE('',#222805,#27751);
#22525=LINE('',#222808,#27752);
#22526=LINE('',#222814,#27753);
#22527=LINE('',#222821,#27754);
#22528=LINE('',#222824,#27755);
#22529=LINE('',#222827,#27756);
#22530=LINE('',#222845,#27757);
#22531=LINE('',#222852,#27758);
#22532=LINE('',#222855,#27759);
#22533=LINE('',#222858,#27760);
#22534=LINE('',#222864,#27761);
#22535=LINE('',#222867,#27762);
#22536=LINE('',#222873,#27763);
#22537=LINE('',#222880,#27764);
#22538=LINE('',#222883,#27765);
#22539=LINE('',#222886,#27766);
#22540=LINE('',#222904,#27767);
#22541=LINE('',#222911,#27768);
#22542=LINE('',#222914,#27769);
#22543=LINE('',#222917,#27770);
#22544=LINE('',#222923,#27771);
#22545=LINE('',#222926,#27772);
#22546=LINE('',#222932,#27773);
#22547=LINE('',#222939,#27774);
#22548=LINE('',#222942,#27775);
#22549=LINE('',#222945,#27776);
#22550=LINE('',#222963,#27777);
#22551=LINE('',#222970,#27778);
#22552=LINE('',#222973,#27779);
#22553=LINE('',#222976,#27780);
#22554=LINE('',#222982,#27781);
#22555=LINE('',#222985,#27782);
#22556=LINE('',#222991,#27783);
#22557=LINE('',#222998,#27784);
#22558=LINE('',#223001,#27785);
#22559=LINE('',#223004,#27786);
#22560=LINE('',#223022,#27787);
#22561=LINE('',#223029,#27788);
#22562=LINE('',#223032,#27789);
#22563=LINE('',#223035,#27790);
#22564=LINE('',#223041,#27791);
#22565=LINE('',#223044,#27792);
#22566=LINE('',#223050,#27793);
#22567=LINE('',#223057,#27794);
#22568=LINE('',#223060,#27795);
#22569=LINE('',#223063,#27796);
#22570=LINE('',#223081,#27797);
#22571=LINE('',#223088,#27798);
#22572=LINE('',#223091,#27799);
#22573=LINE('',#223094,#27800);
#22574=LINE('',#223100,#27801);
#22575=LINE('',#223103,#27802);
#22576=LINE('',#223109,#27803);
#22577=LINE('',#223116,#27804);
#22578=LINE('',#223119,#27805);
#22579=LINE('',#223122,#27806);
#22580=LINE('',#223140,#27807);
#22581=LINE('',#223147,#27808);
#22582=LINE('',#223150,#27809);
#22583=LINE('',#223153,#27810);
#22584=LINE('',#223159,#27811);
#22585=LINE('',#223162,#27812);
#22586=LINE('',#223168,#27813);
#22587=LINE('',#223175,#27814);
#22588=LINE('',#223178,#27815);
#22589=LINE('',#223181,#27816);
#22590=LINE('',#223199,#27817);
#22591=LINE('',#223206,#27818);
#22592=LINE('',#223209,#27819);
#22593=LINE('',#223212,#27820);
#22594=LINE('',#223218,#27821);
#22595=LINE('',#223221,#27822);
#22596=LINE('',#223227,#27823);
#22597=LINE('',#223234,#27824);
#22598=LINE('',#223237,#27825);
#22599=LINE('',#223240,#27826);
#22600=LINE('',#223258,#27827);
#22601=LINE('',#223265,#27828);
#22602=LINE('',#223268,#27829);
#22603=LINE('',#223271,#27830);
#22604=LINE('',#223277,#27831);
#22605=LINE('',#223280,#27832);
#22606=LINE('',#223286,#27833);
#22607=LINE('',#223293,#27834);
#22608=LINE('',#223296,#27835);
#22609=LINE('',#223299,#27836);
#22610=LINE('',#223317,#27837);
#22611=LINE('',#223324,#27838);
#22612=LINE('',#223327,#27839);
#22613=LINE('',#223330,#27840);
#22614=LINE('',#223336,#27841);
#22615=LINE('',#223339,#27842);
#22616=LINE('',#223345,#27843);
#22617=LINE('',#223352,#27844);
#22618=LINE('',#223355,#27845);
#22619=LINE('',#223358,#27846);
#22620=LINE('',#223376,#27847);
#22621=LINE('',#223383,#27848);
#22622=LINE('',#223386,#27849);
#22623=LINE('',#223389,#27850);
#22624=LINE('',#223395,#27851);
#22625=LINE('',#223398,#27852);
#22626=LINE('',#223404,#27853);
#22627=LINE('',#223411,#27854);
#22628=LINE('',#223414,#27855);
#22629=LINE('',#223417,#27856);
#22630=LINE('',#223435,#27857);
#22631=LINE('',#223442,#27858);
#22632=LINE('',#223445,#27859);
#22633=LINE('',#223448,#27860);
#22634=LINE('',#223454,#27861);
#22635=LINE('',#223457,#27862);
#22636=LINE('',#223463,#27863);
#22637=LINE('',#223470,#27864);
#22638=LINE('',#223473,#27865);
#22639=LINE('',#223476,#27866);
#22640=LINE('',#223494,#27867);
#22641=LINE('',#223501,#27868);
#22642=LINE('',#223504,#27869);
#22643=LINE('',#223507,#27870);
#22644=LINE('',#223513,#27871);
#22645=LINE('',#223516,#27872);
#22646=LINE('',#223522,#27873);
#22647=LINE('',#223529,#27874);
#22648=LINE('',#223532,#27875);
#22649=LINE('',#223535,#27876);
#22650=LINE('',#223553,#27877);
#22651=LINE('',#223560,#27878);
#22652=LINE('',#223563,#27879);
#22653=LINE('',#223566,#27880);
#22654=LINE('',#223572,#27881);
#22655=LINE('',#223575,#27882);
#22656=LINE('',#223581,#27883);
#22657=LINE('',#223588,#27884);
#22658=LINE('',#223591,#27885);
#22659=LINE('',#223594,#27886);
#22660=LINE('',#223612,#27887);
#22661=LINE('',#223619,#27888);
#22662=LINE('',#223622,#27889);
#22663=LINE('',#223625,#27890);
#22664=LINE('',#223631,#27891);
#22665=LINE('',#223634,#27892);
#22666=LINE('',#223640,#27893);
#22667=LINE('',#223647,#27894);
#22668=LINE('',#223650,#27895);
#22669=LINE('',#223653,#27896);
#22670=LINE('',#223671,#27897);
#22671=LINE('',#223678,#27898);
#22672=LINE('',#223681,#27899);
#22673=LINE('',#223684,#27900);
#22674=LINE('',#223690,#27901);
#22675=LINE('',#223693,#27902);
#22676=LINE('',#223699,#27903);
#22677=LINE('',#223706,#27904);
#22678=LINE('',#223709,#27905);
#22679=LINE('',#223712,#27906);
#22680=LINE('',#223730,#27907);
#22681=LINE('',#223737,#27908);
#22682=LINE('',#223740,#27909);
#22683=LINE('',#223743,#27910);
#22684=LINE('',#223749,#27911);
#22685=LINE('',#223752,#27912);
#22686=LINE('',#223758,#27913);
#22687=LINE('',#223765,#27914);
#22688=LINE('',#223768,#27915);
#22689=LINE('',#223771,#27916);
#22690=LINE('',#223789,#27917);
#22691=LINE('',#223796,#27918);
#22692=LINE('',#223799,#27919);
#22693=LINE('',#223802,#27920);
#22694=LINE('',#223808,#27921);
#22695=LINE('',#223811,#27922);
#22696=LINE('',#223817,#27923);
#22697=LINE('',#223824,#27924);
#22698=LINE('',#223827,#27925);
#22699=LINE('',#223830,#27926);
#22700=LINE('',#223848,#27927);
#22701=LINE('',#223855,#27928);
#22702=LINE('',#223858,#27929);
#22703=LINE('',#223861,#27930);
#22704=LINE('',#223867,#27931);
#22705=LINE('',#223870,#27932);
#22706=LINE('',#223876,#27933);
#22707=LINE('',#223883,#27934);
#22708=LINE('',#223886,#27935);
#22709=LINE('',#223889,#27936);
#22710=LINE('',#223907,#27937);
#22711=LINE('',#223914,#27938);
#22712=LINE('',#223917,#27939);
#22713=LINE('',#223920,#27940);
#22714=LINE('',#223926,#27941);
#22715=LINE('',#223929,#27942);
#22716=LINE('',#223935,#27943);
#22717=LINE('',#223942,#27944);
#22718=LINE('',#223945,#27945);
#22719=LINE('',#223948,#27946);
#22720=LINE('',#223966,#27947);
#22721=LINE('',#223973,#27948);
#22722=LINE('',#223976,#27949);
#22723=LINE('',#223979,#27950);
#22724=LINE('',#223985,#27951);
#22725=LINE('',#223988,#27952);
#22726=LINE('',#223994,#27953);
#22727=LINE('',#224001,#27954);
#22728=LINE('',#224004,#27955);
#22729=LINE('',#224007,#27956);
#22730=LINE('',#224025,#27957);
#22731=LINE('',#224032,#27958);
#22732=LINE('',#224035,#27959);
#22733=LINE('',#224038,#27960);
#22734=LINE('',#224044,#27961);
#22735=LINE('',#224047,#27962);
#22736=LINE('',#224053,#27963);
#22737=LINE('',#224060,#27964);
#22738=LINE('',#224063,#27965);
#22739=LINE('',#224066,#27966);
#22740=LINE('',#224084,#27967);
#22741=LINE('',#224091,#27968);
#22742=LINE('',#224094,#27969);
#22743=LINE('',#224097,#27970);
#22744=LINE('',#224103,#27971);
#22745=LINE('',#224106,#27972);
#22746=LINE('',#224112,#27973);
#22747=LINE('',#224119,#27974);
#22748=LINE('',#224122,#27975);
#22749=LINE('',#224125,#27976);
#22750=LINE('',#224143,#27977);
#22751=LINE('',#224150,#27978);
#22752=LINE('',#224153,#27979);
#22753=LINE('',#224156,#27980);
#22754=LINE('',#224162,#27981);
#22755=LINE('',#224165,#27982);
#22756=LINE('',#224171,#27983);
#22757=LINE('',#224178,#27984);
#22758=LINE('',#224181,#27985);
#22759=LINE('',#224184,#27986);
#22760=LINE('',#224202,#27987);
#22761=LINE('',#224209,#27988);
#22762=LINE('',#224212,#27989);
#22763=LINE('',#224215,#27990);
#22764=LINE('',#224221,#27991);
#22765=LINE('',#224224,#27992);
#22766=LINE('',#224230,#27993);
#22767=LINE('',#224237,#27994);
#22768=LINE('',#224240,#27995);
#22769=LINE('',#224243,#27996);
#22770=LINE('',#224261,#27997);
#22771=LINE('',#224268,#27998);
#22772=LINE('',#224271,#27999);
#22773=LINE('',#224274,#28000);
#22774=LINE('',#224280,#28001);
#22775=LINE('',#224283,#28002);
#22776=LINE('',#224289,#28003);
#22777=LINE('',#224296,#28004);
#22778=LINE('',#224299,#28005);
#22779=LINE('',#224302,#28006);
#22780=LINE('',#224320,#28007);
#22781=LINE('',#224327,#28008);
#22782=LINE('',#224330,#28009);
#22783=LINE('',#224333,#28010);
#22784=LINE('',#224339,#28011);
#22785=LINE('',#224342,#28012);
#22786=LINE('',#224348,#28013);
#22787=LINE('',#224355,#28014);
#22788=LINE('',#224358,#28015);
#22789=LINE('',#224361,#28016);
#22790=LINE('',#224379,#28017);
#22791=LINE('',#224386,#28018);
#22792=LINE('',#224389,#28019);
#22793=LINE('',#224392,#28020);
#22794=LINE('',#224398,#28021);
#22795=LINE('',#224401,#28022);
#22796=LINE('',#224407,#28023);
#22797=LINE('',#224414,#28024);
#22798=LINE('',#224417,#28025);
#22799=LINE('',#224420,#28026);
#22800=LINE('',#224438,#28027);
#22801=LINE('',#224445,#28028);
#22802=LINE('',#224448,#28029);
#22803=LINE('',#224451,#28030);
#22804=LINE('',#224457,#28031);
#22805=LINE('',#224460,#28032);
#22806=LINE('',#224466,#28033);
#22807=LINE('',#224473,#28034);
#22808=LINE('',#224476,#28035);
#22809=LINE('',#224479,#28036);
#22810=LINE('',#224497,#28037);
#22811=LINE('',#224504,#28038);
#22812=LINE('',#224507,#28039);
#22813=LINE('',#224510,#28040);
#22814=LINE('',#224516,#28041);
#22815=LINE('',#224519,#28042);
#22816=LINE('',#224525,#28043);
#22817=LINE('',#224532,#28044);
#22818=LINE('',#224535,#28045);
#22819=LINE('',#224538,#28046);
#22820=LINE('',#224556,#28047);
#22821=LINE('',#224563,#28048);
#22822=LINE('',#224566,#28049);
#22823=LINE('',#224569,#28050);
#22824=LINE('',#224575,#28051);
#22825=LINE('',#224578,#28052);
#22826=LINE('',#224584,#28053);
#22827=LINE('',#224591,#28054);
#22828=LINE('',#224594,#28055);
#22829=LINE('',#224597,#28056);
#22830=LINE('',#224615,#28057);
#22831=LINE('',#224622,#28058);
#22832=LINE('',#224625,#28059);
#22833=LINE('',#224628,#28060);
#22834=LINE('',#224634,#28061);
#22835=LINE('',#224637,#28062);
#22836=LINE('',#224643,#28063);
#22837=LINE('',#224650,#28064);
#22838=LINE('',#224653,#28065);
#22839=LINE('',#224656,#28066);
#22840=LINE('',#224674,#28067);
#22841=LINE('',#224681,#28068);
#22842=LINE('',#224684,#28069);
#22843=LINE('',#224687,#28070);
#22844=LINE('',#224693,#28071);
#22845=LINE('',#224696,#28072);
#22846=LINE('',#224702,#28073);
#22847=LINE('',#224709,#28074);
#22848=LINE('',#224712,#28075);
#22849=LINE('',#224715,#28076);
#22850=LINE('',#224733,#28077);
#22851=LINE('',#224740,#28078);
#22852=LINE('',#224743,#28079);
#22853=LINE('',#224746,#28080);
#22854=LINE('',#224752,#28081);
#22855=LINE('',#224755,#28082);
#22856=LINE('',#224761,#28083);
#22857=LINE('',#224768,#28084);
#22858=LINE('',#224771,#28085);
#22859=LINE('',#224774,#28086);
#22860=LINE('',#224792,#28087);
#22861=LINE('',#224799,#28088);
#22862=LINE('',#224802,#28089);
#22863=LINE('',#224805,#28090);
#22864=LINE('',#224811,#28091);
#22865=LINE('',#224814,#28092);
#22866=LINE('',#224820,#28093);
#22867=LINE('',#224827,#28094);
#22868=LINE('',#224830,#28095);
#22869=LINE('',#224833,#28096);
#22870=LINE('',#224852,#28097);
#22871=LINE('',#224859,#28098);
#22872=LINE('',#224862,#28099);
#22873=LINE('',#224865,#28100);
#22874=LINE('',#224871,#28101);
#22875=LINE('',#224874,#28102);
#22876=LINE('',#224880,#28103);
#22877=LINE('',#224887,#28104);
#22878=LINE('',#224890,#28105);
#22879=LINE('',#224893,#28106);
#22880=LINE('',#224911,#28107);
#22881=LINE('',#224915,#28108);
#22882=LINE('',#224922,#28109);
#22883=LINE('',#224924,#28110);
#22884=LINE('',#224926,#28111);
#22885=LINE('',#224930,#28112);
#22886=LINE('',#224932,#28113);
#22887=LINE('',#224936,#28114);
#22888=LINE('',#224940,#28115);
#22889=LINE('',#224941,#28116);
#22890=LINE('',#224947,#28117);
#22891=LINE('',#224949,#28118);
#22892=LINE('',#224951,#28119);
#22893=LINE('',#224955,#28120);
#22894=LINE('',#224957,#28121);
#22895=LINE('',#224961,#28122);
#22896=LINE('',#224965,#28123);
#22897=LINE('',#224966,#28124);
#22898=LINE('',#225386,#28125);
#22899=LINE('',#225390,#28126);
#22900=LINE('',#225397,#28127);
#22901=LINE('',#225399,#28128);
#22902=LINE('',#225401,#28129);
#22903=LINE('',#225405,#28130);
#22904=LINE('',#225407,#28131);
#22905=LINE('',#225411,#28132);
#22906=LINE('',#225415,#28133);
#22907=LINE('',#225416,#28134);
#22908=LINE('',#225422,#28135);
#22909=LINE('',#225424,#28136);
#22910=LINE('',#225426,#28137);
#22911=LINE('',#225430,#28138);
#22912=LINE('',#225432,#28139);
#22913=LINE('',#225436,#28140);
#22914=LINE('',#225440,#28141);
#22915=LINE('',#225441,#28142);
#22916=LINE('',#225445,#28143);
#22917=LINE('',#225449,#28144);
#22918=LINE('',#225456,#28145);
#22919=LINE('',#225458,#28146);
#22920=LINE('',#225460,#28147);
#22921=LINE('',#225464,#28148);
#22922=LINE('',#225466,#28149);
#22923=LINE('',#225470,#28150);
#22924=LINE('',#225474,#28151);
#22925=LINE('',#225475,#28152);
#22926=LINE('',#225481,#28153);
#22927=LINE('',#225483,#28154);
#22928=LINE('',#225485,#28155);
#22929=LINE('',#225489,#28156);
#22930=LINE('',#225491,#28157);
#22931=LINE('',#225495,#28158);
#22932=LINE('',#225499,#28159);
#22933=LINE('',#225500,#28160);
#22934=LINE('',#225504,#28161);
#22935=LINE('',#225508,#28162);
#22936=LINE('',#225515,#28163);
#22937=LINE('',#225517,#28164);
#22938=LINE('',#225519,#28165);
#22939=LINE('',#225523,#28166);
#22940=LINE('',#225525,#28167);
#22941=LINE('',#225529,#28168);
#22942=LINE('',#225533,#28169);
#22943=LINE('',#225534,#28170);
#22944=LINE('',#225540,#28171);
#22945=LINE('',#225542,#28172);
#22946=LINE('',#225544,#28173);
#22947=LINE('',#225548,#28174);
#22948=LINE('',#225550,#28175);
#22949=LINE('',#225554,#28176);
#22950=LINE('',#225558,#28177);
#22951=LINE('',#225559,#28178);
#22952=LINE('',#225563,#28179);
#22953=LINE('',#225567,#28180);
#22954=LINE('',#225574,#28181);
#22955=LINE('',#225576,#28182);
#22956=LINE('',#225578,#28183);
#22957=LINE('',#225582,#28184);
#22958=LINE('',#225584,#28185);
#22959=LINE('',#225588,#28186);
#22960=LINE('',#225592,#28187);
#22961=LINE('',#225593,#28188);
#22962=LINE('',#225599,#28189);
#22963=LINE('',#225601,#28190);
#22964=LINE('',#225603,#28191);
#22965=LINE('',#225607,#28192);
#22966=LINE('',#225609,#28193);
#22967=LINE('',#225613,#28194);
#22968=LINE('',#225617,#28195);
#22969=LINE('',#225618,#28196);
#22970=LINE('',#225622,#28197);
#22971=LINE('',#225626,#28198);
#22972=LINE('',#225633,#28199);
#22973=LINE('',#225635,#28200);
#22974=LINE('',#225637,#28201);
#22975=LINE('',#225641,#28202);
#22976=LINE('',#225643,#28203);
#22977=LINE('',#225647,#28204);
#22978=LINE('',#225651,#28205);
#22979=LINE('',#225652,#28206);
#22980=LINE('',#225658,#28207);
#22981=LINE('',#225660,#28208);
#22982=LINE('',#225662,#28209);
#22983=LINE('',#225666,#28210);
#22984=LINE('',#225668,#28211);
#22985=LINE('',#225672,#28212);
#22986=LINE('',#225676,#28213);
#22987=LINE('',#225677,#28214);
#22988=LINE('',#225681,#28215);
#22989=LINE('',#225685,#28216);
#22990=LINE('',#225692,#28217);
#22991=LINE('',#225694,#28218);
#22992=LINE('',#225696,#28219);
#22993=LINE('',#225700,#28220);
#22994=LINE('',#225702,#28221);
#22995=LINE('',#225706,#28222);
#22996=LINE('',#225710,#28223);
#22997=LINE('',#225711,#28224);
#22998=LINE('',#225717,#28225);
#22999=LINE('',#225719,#28226);
#23000=LINE('',#225721,#28227);
#23001=LINE('',#225725,#28228);
#23002=LINE('',#225727,#28229);
#23003=LINE('',#225731,#28230);
#23004=LINE('',#225735,#28231);
#23005=LINE('',#225736,#28232);
#23006=LINE('',#225740,#28233);
#23007=LINE('',#225744,#28234);
#23008=LINE('',#225751,#28235);
#23009=LINE('',#225753,#28236);
#23010=LINE('',#225755,#28237);
#23011=LINE('',#225759,#28238);
#23012=LINE('',#225761,#28239);
#23013=LINE('',#225765,#28240);
#23014=LINE('',#225769,#28241);
#23015=LINE('',#225770,#28242);
#23016=LINE('',#225776,#28243);
#23017=LINE('',#225778,#28244);
#23018=LINE('',#225780,#28245);
#23019=LINE('',#225784,#28246);
#23020=LINE('',#225786,#28247);
#23021=LINE('',#225790,#28248);
#23022=LINE('',#225794,#28249);
#23023=LINE('',#225795,#28250);
#23024=LINE('',#225799,#28251);
#23025=LINE('',#225803,#28252);
#23026=LINE('',#225810,#28253);
#23027=LINE('',#225812,#28254);
#23028=LINE('',#225814,#28255);
#23029=LINE('',#225818,#28256);
#23030=LINE('',#225820,#28257);
#23031=LINE('',#225824,#28258);
#23032=LINE('',#225828,#28259);
#23033=LINE('',#225829,#28260);
#23034=LINE('',#225835,#28261);
#23035=LINE('',#225837,#28262);
#23036=LINE('',#225839,#28263);
#23037=LINE('',#225843,#28264);
#23038=LINE('',#225845,#28265);
#23039=LINE('',#225849,#28266);
#23040=LINE('',#225853,#28267);
#23041=LINE('',#225854,#28268);
#23042=LINE('',#225858,#28269);
#23043=LINE('',#225862,#28270);
#23044=LINE('',#225869,#28271);
#23045=LINE('',#225871,#28272);
#23046=LINE('',#225873,#28273);
#23047=LINE('',#225877,#28274);
#23048=LINE('',#225879,#28275);
#23049=LINE('',#225883,#28276);
#23050=LINE('',#225887,#28277);
#23051=LINE('',#225888,#28278);
#23052=LINE('',#225894,#28279);
#23053=LINE('',#225896,#28280);
#23054=LINE('',#225898,#28281);
#23055=LINE('',#225902,#28282);
#23056=LINE('',#225904,#28283);
#23057=LINE('',#225908,#28284);
#23058=LINE('',#225912,#28285);
#23059=LINE('',#225913,#28286);
#23060=LINE('',#225917,#28287);
#23061=LINE('',#225921,#28288);
#23062=LINE('',#225928,#28289);
#23063=LINE('',#225930,#28290);
#23064=LINE('',#225932,#28291);
#23065=LINE('',#225936,#28292);
#23066=LINE('',#225938,#28293);
#23067=LINE('',#225942,#28294);
#23068=LINE('',#225946,#28295);
#23069=LINE('',#225947,#28296);
#23070=LINE('',#225953,#28297);
#23071=LINE('',#225955,#28298);
#23072=LINE('',#225957,#28299);
#23073=LINE('',#225961,#28300);
#23074=LINE('',#225963,#28301);
#23075=LINE('',#225967,#28302);
#23076=LINE('',#225971,#28303);
#23077=LINE('',#225972,#28304);
#23078=LINE('',#225976,#28305);
#23079=LINE('',#225980,#28306);
#23080=LINE('',#225987,#28307);
#23081=LINE('',#225989,#28308);
#23082=LINE('',#225991,#28309);
#23083=LINE('',#225995,#28310);
#23084=LINE('',#225997,#28311);
#23085=LINE('',#226001,#28312);
#23086=LINE('',#226005,#28313);
#23087=LINE('',#226006,#28314);
#23088=LINE('',#226012,#28315);
#23089=LINE('',#226014,#28316);
#23090=LINE('',#226016,#28317);
#23091=LINE('',#226020,#28318);
#23092=LINE('',#226022,#28319);
#23093=LINE('',#226026,#28320);
#23094=LINE('',#226030,#28321);
#23095=LINE('',#226031,#28322);
#23096=LINE('',#226035,#28323);
#23097=LINE('',#226039,#28324);
#23098=LINE('',#226046,#28325);
#23099=LINE('',#226048,#28326);
#23100=LINE('',#226050,#28327);
#23101=LINE('',#226054,#28328);
#23102=LINE('',#226056,#28329);
#23103=LINE('',#226060,#28330);
#23104=LINE('',#226064,#28331);
#23105=LINE('',#226065,#28332);
#23106=LINE('',#226071,#28333);
#23107=LINE('',#226073,#28334);
#23108=LINE('',#226075,#28335);
#23109=LINE('',#226079,#28336);
#23110=LINE('',#226081,#28337);
#23111=LINE('',#226085,#28338);
#23112=LINE('',#226089,#28339);
#23113=LINE('',#226090,#28340);
#23114=LINE('',#226094,#28341);
#23115=LINE('',#226098,#28342);
#23116=LINE('',#226105,#28343);
#23117=LINE('',#226107,#28344);
#23118=LINE('',#226109,#28345);
#23119=LINE('',#226113,#28346);
#23120=LINE('',#226115,#28347);
#23121=LINE('',#226119,#28348);
#23122=LINE('',#226123,#28349);
#23123=LINE('',#226124,#28350);
#23124=LINE('',#226130,#28351);
#23125=LINE('',#226132,#28352);
#23126=LINE('',#226134,#28353);
#23127=LINE('',#226138,#28354);
#23128=LINE('',#226140,#28355);
#23129=LINE('',#226144,#28356);
#23130=LINE('',#226148,#28357);
#23131=LINE('',#226149,#28358);
#23132=LINE('',#226153,#28359);
#23133=LINE('',#226157,#28360);
#23134=LINE('',#226164,#28361);
#23135=LINE('',#226166,#28362);
#23136=LINE('',#226168,#28363);
#23137=LINE('',#226172,#28364);
#23138=LINE('',#226174,#28365);
#23139=LINE('',#226178,#28366);
#23140=LINE('',#226182,#28367);
#23141=LINE('',#226183,#28368);
#23142=LINE('',#226189,#28369);
#23143=LINE('',#226191,#28370);
#23144=LINE('',#226193,#28371);
#23145=LINE('',#226197,#28372);
#23146=LINE('',#226199,#28373);
#23147=LINE('',#226203,#28374);
#23148=LINE('',#226207,#28375);
#23149=LINE('',#226208,#28376);
#23150=LINE('',#226212,#28377);
#23151=LINE('',#226216,#28378);
#23152=LINE('',#226223,#28379);
#23153=LINE('',#226225,#28380);
#23154=LINE('',#226227,#28381);
#23155=LINE('',#226231,#28382);
#23156=LINE('',#226233,#28383);
#23157=LINE('',#226237,#28384);
#23158=LINE('',#226241,#28385);
#23159=LINE('',#226242,#28386);
#23160=LINE('',#226248,#28387);
#23161=LINE('',#226250,#28388);
#23162=LINE('',#226252,#28389);
#23163=LINE('',#226256,#28390);
#23164=LINE('',#226258,#28391);
#23165=LINE('',#226262,#28392);
#23166=LINE('',#226266,#28393);
#23167=LINE('',#226267,#28394);
#23168=LINE('',#226271,#28395);
#23169=LINE('',#226275,#28396);
#23170=LINE('',#226282,#28397);
#23171=LINE('',#226284,#28398);
#23172=LINE('',#226286,#28399);
#23173=LINE('',#226290,#28400);
#23174=LINE('',#226292,#28401);
#23175=LINE('',#226296,#28402);
#23176=LINE('',#226300,#28403);
#23177=LINE('',#226301,#28404);
#23178=LINE('',#226307,#28405);
#23179=LINE('',#226309,#28406);
#23180=LINE('',#226311,#28407);
#23181=LINE('',#226315,#28408);
#23182=LINE('',#226317,#28409);
#23183=LINE('',#226321,#28410);
#23184=LINE('',#226325,#28411);
#23185=LINE('',#226326,#28412);
#23186=LINE('',#226330,#28413);
#23187=LINE('',#226334,#28414);
#23188=LINE('',#226341,#28415);
#23189=LINE('',#226343,#28416);
#23190=LINE('',#226345,#28417);
#23191=LINE('',#226349,#28418);
#23192=LINE('',#226351,#28419);
#23193=LINE('',#226355,#28420);
#23194=LINE('',#226359,#28421);
#23195=LINE('',#226360,#28422);
#23196=LINE('',#226366,#28423);
#23197=LINE('',#226368,#28424);
#23198=LINE('',#226370,#28425);
#23199=LINE('',#226374,#28426);
#23200=LINE('',#226376,#28427);
#23201=LINE('',#226380,#28428);
#23202=LINE('',#226384,#28429);
#23203=LINE('',#226385,#28430);
#23204=LINE('',#226389,#28431);
#23205=LINE('',#226393,#28432);
#23206=LINE('',#226400,#28433);
#23207=LINE('',#226402,#28434);
#23208=LINE('',#226404,#28435);
#23209=LINE('',#226408,#28436);
#23210=LINE('',#226410,#28437);
#23211=LINE('',#226414,#28438);
#23212=LINE('',#226418,#28439);
#23213=LINE('',#226419,#28440);
#23214=LINE('',#226425,#28441);
#23215=LINE('',#226427,#28442);
#23216=LINE('',#226429,#28443);
#23217=LINE('',#226433,#28444);
#23218=LINE('',#226435,#28445);
#23219=LINE('',#226439,#28446);
#23220=LINE('',#226443,#28447);
#23221=LINE('',#226444,#28448);
#23222=LINE('',#226448,#28449);
#23223=LINE('',#226452,#28450);
#23224=LINE('',#226459,#28451);
#23225=LINE('',#226461,#28452);
#23226=LINE('',#226463,#28453);
#23227=LINE('',#226467,#28454);
#23228=LINE('',#226469,#28455);
#23229=LINE('',#226473,#28456);
#23230=LINE('',#226477,#28457);
#23231=LINE('',#226478,#28458);
#23232=LINE('',#226484,#28459);
#23233=LINE('',#226486,#28460);
#23234=LINE('',#226488,#28461);
#23235=LINE('',#226492,#28462);
#23236=LINE('',#226494,#28463);
#23237=LINE('',#226498,#28464);
#23238=LINE('',#226502,#28465);
#23239=LINE('',#226503,#28466);
#23240=LINE('',#226507,#28467);
#23241=LINE('',#226511,#28468);
#23242=LINE('',#226518,#28469);
#23243=LINE('',#226520,#28470);
#23244=LINE('',#226522,#28471);
#23245=LINE('',#226526,#28472);
#23246=LINE('',#226528,#28473);
#23247=LINE('',#226532,#28474);
#23248=LINE('',#226536,#28475);
#23249=LINE('',#226537,#28476);
#23250=LINE('',#226543,#28477);
#23251=LINE('',#226545,#28478);
#23252=LINE('',#226547,#28479);
#23253=LINE('',#226551,#28480);
#23254=LINE('',#226553,#28481);
#23255=LINE('',#226557,#28482);
#23256=LINE('',#226561,#28483);
#23257=LINE('',#226562,#28484);
#23258=LINE('',#226566,#28485);
#23259=LINE('',#226570,#28486);
#23260=LINE('',#226577,#28487);
#23261=LINE('',#226579,#28488);
#23262=LINE('',#226581,#28489);
#23263=LINE('',#226585,#28490);
#23264=LINE('',#226587,#28491);
#23265=LINE('',#226591,#28492);
#23266=LINE('',#226595,#28493);
#23267=LINE('',#226596,#28494);
#23268=LINE('',#226602,#28495);
#23269=LINE('',#226604,#28496);
#23270=LINE('',#226606,#28497);
#23271=LINE('',#226610,#28498);
#23272=LINE('',#226612,#28499);
#23273=LINE('',#226616,#28500);
#23274=LINE('',#226620,#28501);
#23275=LINE('',#226621,#28502);
#23276=LINE('',#226625,#28503);
#23277=LINE('',#226629,#28504);
#23278=LINE('',#226636,#28505);
#23279=LINE('',#226638,#28506);
#23280=LINE('',#226640,#28507);
#23281=LINE('',#226644,#28508);
#23282=LINE('',#226646,#28509);
#23283=LINE('',#226650,#28510);
#23284=LINE('',#226654,#28511);
#23285=LINE('',#226655,#28512);
#23286=LINE('',#226661,#28513);
#23287=LINE('',#226663,#28514);
#23288=LINE('',#226665,#28515);
#23289=LINE('',#226669,#28516);
#23290=LINE('',#226671,#28517);
#23291=LINE('',#226675,#28518);
#23292=LINE('',#226679,#28519);
#23293=LINE('',#226680,#28520);
#23294=LINE('',#226684,#28521);
#23295=LINE('',#226688,#28522);
#23296=LINE('',#226695,#28523);
#23297=LINE('',#226697,#28524);
#23298=LINE('',#226699,#28525);
#23299=LINE('',#226703,#28526);
#23300=LINE('',#226705,#28527);
#23301=LINE('',#226709,#28528);
#23302=LINE('',#226713,#28529);
#23303=LINE('',#226714,#28530);
#23304=LINE('',#226720,#28531);
#23305=LINE('',#226722,#28532);
#23306=LINE('',#226724,#28533);
#23307=LINE('',#226728,#28534);
#23308=LINE('',#226730,#28535);
#23309=LINE('',#226734,#28536);
#23310=LINE('',#226738,#28537);
#23311=LINE('',#226739,#28538);
#23312=LINE('',#226743,#28539);
#23313=LINE('',#226747,#28540);
#23314=LINE('',#226754,#28541);
#23315=LINE('',#226756,#28542);
#23316=LINE('',#226758,#28543);
#23317=LINE('',#226762,#28544);
#23318=LINE('',#226764,#28545);
#23319=LINE('',#226768,#28546);
#23320=LINE('',#226772,#28547);
#23321=LINE('',#226773,#28548);
#23322=LINE('',#226779,#28549);
#23323=LINE('',#226781,#28550);
#23324=LINE('',#226783,#28551);
#23325=LINE('',#226787,#28552);
#23326=LINE('',#226789,#28553);
#23327=LINE('',#226793,#28554);
#23328=LINE('',#226797,#28555);
#23329=LINE('',#226798,#28556);
#23330=LINE('',#226802,#28557);
#23331=LINE('',#226806,#28558);
#23332=LINE('',#226813,#28559);
#23333=LINE('',#226815,#28560);
#23334=LINE('',#226817,#28561);
#23335=LINE('',#226821,#28562);
#23336=LINE('',#226823,#28563);
#23337=LINE('',#226827,#28564);
#23338=LINE('',#226831,#28565);
#23339=LINE('',#226832,#28566);
#23340=LINE('',#226838,#28567);
#23341=LINE('',#226840,#28568);
#23342=LINE('',#226842,#28569);
#23343=LINE('',#226846,#28570);
#23344=LINE('',#226848,#28571);
#23345=LINE('',#226852,#28572);
#23346=LINE('',#226856,#28573);
#23347=LINE('',#226857,#28574);
#23348=LINE('',#226861,#28575);
#23349=LINE('',#226865,#28576);
#23350=LINE('',#226872,#28577);
#23351=LINE('',#226874,#28578);
#23352=LINE('',#226876,#28579);
#23353=LINE('',#226880,#28580);
#23354=LINE('',#226882,#28581);
#23355=LINE('',#226886,#28582);
#23356=LINE('',#226890,#28583);
#23357=LINE('',#226891,#28584);
#23358=LINE('',#226897,#28585);
#23359=LINE('',#226899,#28586);
#23360=LINE('',#226901,#28587);
#23361=LINE('',#226905,#28588);
#23362=LINE('',#226907,#28589);
#23363=LINE('',#226911,#28590);
#23364=LINE('',#226915,#28591);
#23365=LINE('',#226916,#28592);
#23366=LINE('',#226920,#28593);
#23367=LINE('',#226924,#28594);
#23368=LINE('',#226931,#28595);
#23369=LINE('',#226933,#28596);
#23370=LINE('',#226935,#28597);
#23371=LINE('',#226939,#28598);
#23372=LINE('',#226941,#28599);
#23373=LINE('',#226945,#28600);
#23374=LINE('',#226949,#28601);
#23375=LINE('',#226950,#28602);
#23376=LINE('',#226956,#28603);
#23377=LINE('',#226958,#28604);
#23378=LINE('',#226960,#28605);
#23379=LINE('',#226964,#28606);
#23380=LINE('',#226966,#28607);
#23381=LINE('',#226970,#28608);
#23382=LINE('',#226974,#28609);
#23383=LINE('',#226975,#28610);
#23384=LINE('',#226979,#28611);
#23385=LINE('',#226983,#28612);
#23386=LINE('',#226990,#28613);
#23387=LINE('',#226992,#28614);
#23388=LINE('',#226994,#28615);
#23389=LINE('',#226998,#28616);
#23390=LINE('',#227000,#28617);
#23391=LINE('',#227004,#28618);
#23392=LINE('',#227008,#28619);
#23393=LINE('',#227009,#28620);
#23394=LINE('',#227015,#28621);
#23395=LINE('',#227017,#28622);
#23396=LINE('',#227019,#28623);
#23397=LINE('',#227023,#28624);
#23398=LINE('',#227025,#28625);
#23399=LINE('',#227029,#28626);
#23400=LINE('',#227033,#28627);
#23401=LINE('',#227034,#28628);
#23402=LINE('',#227038,#28629);
#23403=LINE('',#227042,#28630);
#23404=LINE('',#227049,#28631);
#23405=LINE('',#227051,#28632);
#23406=LINE('',#227053,#28633);
#23407=LINE('',#227057,#28634);
#23408=LINE('',#227059,#28635);
#23409=LINE('',#227063,#28636);
#23410=LINE('',#227067,#28637);
#23411=LINE('',#227068,#28638);
#23412=LINE('',#227074,#28639);
#23413=LINE('',#227076,#28640);
#23414=LINE('',#227078,#28641);
#23415=LINE('',#227082,#28642);
#23416=LINE('',#227084,#28643);
#23417=LINE('',#227088,#28644);
#23418=LINE('',#227092,#28645);
#23419=LINE('',#227093,#28646);
#23420=LINE('',#227095,#28647);
#23421=LINE('',#227096,#28648);
#23422=LINE('',#227102,#28649);
#23423=LINE('',#227104,#28650);
#23424=LINE('',#227106,#28651);
#23425=LINE('',#227110,#28652);
#23426=LINE('',#227112,#28653);
#23427=LINE('',#227116,#28654);
#23428=LINE('',#227120,#28655);
#23429=LINE('',#227121,#28656);
#23430=LINE('',#227127,#28657);
#23431=LINE('',#227129,#28658);
#23432=LINE('',#227131,#28659);
#23433=LINE('',#227135,#28660);
#23434=LINE('',#227137,#28661);
#23435=LINE('',#227141,#28662);
#23436=LINE('',#227145,#28663);
#23437=LINE('',#227146,#28664);
#23438=LINE('',#227150,#28665);
#23439=LINE('',#227154,#28666);
#23440=LINE('',#227161,#28667);
#23441=LINE('',#227163,#28668);
#23442=LINE('',#227165,#28669);
#23443=LINE('',#227169,#28670);
#23444=LINE('',#227171,#28671);
#23445=LINE('',#227175,#28672);
#23446=LINE('',#227179,#28673);
#23447=LINE('',#227180,#28674);
#23448=LINE('',#227186,#28675);
#23449=LINE('',#227188,#28676);
#23450=LINE('',#227190,#28677);
#23451=LINE('',#227194,#28678);
#23452=LINE('',#227196,#28679);
#23453=LINE('',#227200,#28680);
#23454=LINE('',#227204,#28681);
#23455=LINE('',#227205,#28682);
#23456=LINE('',#227209,#28683);
#23457=LINE('',#227213,#28684);
#23458=LINE('',#227220,#28685);
#23459=LINE('',#227222,#28686);
#23460=LINE('',#227224,#28687);
#23461=LINE('',#227228,#28688);
#23462=LINE('',#227230,#28689);
#23463=LINE('',#227234,#28690);
#23464=LINE('',#227238,#28691);
#23465=LINE('',#227239,#28692);
#23466=LINE('',#227245,#28693);
#23467=LINE('',#227247,#28694);
#23468=LINE('',#227249,#28695);
#23469=LINE('',#227253,#28696);
#23470=LINE('',#227255,#28697);
#23471=LINE('',#227259,#28698);
#23472=LINE('',#227263,#28699);
#23473=LINE('',#227264,#28700);
#23474=LINE('',#227268,#28701);
#23475=LINE('',#227272,#28702);
#23476=LINE('',#227279,#28703);
#23477=LINE('',#227281,#28704);
#23478=LINE('',#227283,#28705);
#23479=LINE('',#227287,#28706);
#23480=LINE('',#227289,#28707);
#23481=LINE('',#227293,#28708);
#23482=LINE('',#227297,#28709);
#23483=LINE('',#227298,#28710);
#23484=LINE('',#227304,#28711);
#23485=LINE('',#227306,#28712);
#23486=LINE('',#227308,#28713);
#23487=LINE('',#227312,#28714);
#23488=LINE('',#227314,#28715);
#23489=LINE('',#227318,#28716);
#23490=LINE('',#227322,#28717);
#23491=LINE('',#227323,#28718);
#23492=LINE('',#227327,#28719);
#23493=LINE('',#227331,#28720);
#23494=LINE('',#227338,#28721);
#23495=LINE('',#227340,#28722);
#23496=LINE('',#227342,#28723);
#23497=LINE('',#227346,#28724);
#23498=LINE('',#227348,#28725);
#23499=LINE('',#227352,#28726);
#23500=LINE('',#227356,#28727);
#23501=LINE('',#227357,#28728);
#23502=LINE('',#227363,#28729);
#23503=LINE('',#227365,#28730);
#23504=LINE('',#227367,#28731);
#23505=LINE('',#227371,#28732);
#23506=LINE('',#227373,#28733);
#23507=LINE('',#227377,#28734);
#23508=LINE('',#227381,#28735);
#23509=LINE('',#227382,#28736);
#23510=LINE('',#227386,#28737);
#23511=LINE('',#227390,#28738);
#23512=LINE('',#227397,#28739);
#23513=LINE('',#227399,#28740);
#23514=LINE('',#227401,#28741);
#23515=LINE('',#227405,#28742);
#23516=LINE('',#227407,#28743);
#23517=LINE('',#227411,#28744);
#23518=LINE('',#227415,#28745);
#23519=LINE('',#227416,#28746);
#23520=LINE('',#227422,#28747);
#23521=LINE('',#227424,#28748);
#23522=LINE('',#227426,#28749);
#23523=LINE('',#227430,#28750);
#23524=LINE('',#227432,#28751);
#23525=LINE('',#227436,#28752);
#23526=LINE('',#227440,#28753);
#23527=LINE('',#227441,#28754);
#23528=LINE('',#227445,#28755);
#23529=LINE('',#227449,#28756);
#23530=LINE('',#227456,#28757);
#23531=LINE('',#227458,#28758);
#23532=LINE('',#227460,#28759);
#23533=LINE('',#227464,#28760);
#23534=LINE('',#227466,#28761);
#23535=LINE('',#227470,#28762);
#23536=LINE('',#227474,#28763);
#23537=LINE('',#227475,#28764);
#23538=LINE('',#227481,#28765);
#23539=LINE('',#227483,#28766);
#23540=LINE('',#227485,#28767);
#23541=LINE('',#227489,#28768);
#23542=LINE('',#227491,#28769);
#23543=LINE('',#227495,#28770);
#23544=LINE('',#227499,#28771);
#23545=LINE('',#227500,#28772);
#23546=LINE('',#227504,#28773);
#23547=LINE('',#227508,#28774);
#23548=LINE('',#227515,#28775);
#23549=LINE('',#227517,#28776);
#23550=LINE('',#227519,#28777);
#23551=LINE('',#227523,#28778);
#23552=LINE('',#227525,#28779);
#23553=LINE('',#227529,#28780);
#23554=LINE('',#227533,#28781);
#23555=LINE('',#227534,#28782);
#23556=LINE('',#227540,#28783);
#23557=LINE('',#227542,#28784);
#23558=LINE('',#227544,#28785);
#23559=LINE('',#227548,#28786);
#23560=LINE('',#227550,#28787);
#23561=LINE('',#227554,#28788);
#23562=LINE('',#227558,#28789);
#23563=LINE('',#227559,#28790);
#23564=LINE('',#227563,#28791);
#23565=LINE('',#227567,#28792);
#23566=LINE('',#227574,#28793);
#23567=LINE('',#227576,#28794);
#23568=LINE('',#227578,#28795);
#23569=LINE('',#227582,#28796);
#23570=LINE('',#227584,#28797);
#23571=LINE('',#227588,#28798);
#23572=LINE('',#227592,#28799);
#23573=LINE('',#227593,#28800);
#23574=LINE('',#227599,#28801);
#23575=LINE('',#227601,#28802);
#23576=LINE('',#227603,#28803);
#23577=LINE('',#227607,#28804);
#23578=LINE('',#227609,#28805);
#23579=LINE('',#227613,#28806);
#23580=LINE('',#227617,#28807);
#23581=LINE('',#227618,#28808);
#23582=LINE('',#227622,#28809);
#23583=LINE('',#227626,#28810);
#23584=LINE('',#227633,#28811);
#23585=LINE('',#227635,#28812);
#23586=LINE('',#227637,#28813);
#23587=LINE('',#227641,#28814);
#23588=LINE('',#227643,#28815);
#23589=LINE('',#227647,#28816);
#23590=LINE('',#227651,#28817);
#23591=LINE('',#227652,#28818);
#23592=LINE('',#227658,#28819);
#23593=LINE('',#227660,#28820);
#23594=LINE('',#227662,#28821);
#23595=LINE('',#227666,#28822);
#23596=LINE('',#227668,#28823);
#23597=LINE('',#227672,#28824);
#23598=LINE('',#227676,#28825);
#23599=LINE('',#227677,#28826);
#23600=LINE('',#227681,#28827);
#23601=LINE('',#227685,#28828);
#23602=LINE('',#227692,#28829);
#23603=LINE('',#227694,#28830);
#23604=LINE('',#227696,#28831);
#23605=LINE('',#227700,#28832);
#23606=LINE('',#227702,#28833);
#23607=LINE('',#227706,#28834);
#23608=LINE('',#227710,#28835);
#23609=LINE('',#227711,#28836);
#23610=LINE('',#227717,#28837);
#23611=LINE('',#227719,#28838);
#23612=LINE('',#227721,#28839);
#23613=LINE('',#227725,#28840);
#23614=LINE('',#227727,#28841);
#23615=LINE('',#227731,#28842);
#23616=LINE('',#227735,#28843);
#23617=LINE('',#227736,#28844);
#23618=LINE('',#227740,#28845);
#23619=LINE('',#227744,#28846);
#23620=LINE('',#227751,#28847);
#23621=LINE('',#227753,#28848);
#23622=LINE('',#227755,#28849);
#23623=LINE('',#227759,#28850);
#23624=LINE('',#227761,#28851);
#23625=LINE('',#227765,#28852);
#23626=LINE('',#227769,#28853);
#23627=LINE('',#227770,#28854);
#23628=LINE('',#227776,#28855);
#23629=LINE('',#227778,#28856);
#23630=LINE('',#227780,#28857);
#23631=LINE('',#227784,#28858);
#23632=LINE('',#227786,#28859);
#23633=LINE('',#227790,#28860);
#23634=LINE('',#227794,#28861);
#23635=LINE('',#227795,#28862);
#23636=LINE('',#227799,#28863);
#23637=LINE('',#227803,#28864);
#23638=LINE('',#227810,#28865);
#23639=LINE('',#227812,#28866);
#23640=LINE('',#227814,#28867);
#23641=LINE('',#227818,#28868);
#23642=LINE('',#227820,#28869);
#23643=LINE('',#227824,#28870);
#23644=LINE('',#227828,#28871);
#23645=LINE('',#227829,#28872);
#23646=LINE('',#227835,#28873);
#23647=LINE('',#227837,#28874);
#23648=LINE('',#227839,#28875);
#23649=LINE('',#227843,#28876);
#23650=LINE('',#227845,#28877);
#23651=LINE('',#227849,#28878);
#23652=LINE('',#227853,#28879);
#23653=LINE('',#227854,#28880);
#23654=LINE('',#227858,#28881);
#23655=LINE('',#227862,#28882);
#23656=LINE('',#227869,#28883);
#23657=LINE('',#227871,#28884);
#23658=LINE('',#227873,#28885);
#23659=LINE('',#227877,#28886);
#23660=LINE('',#227879,#28887);
#23661=LINE('',#227883,#28888);
#23662=LINE('',#227887,#28889);
#23663=LINE('',#227888,#28890);
#23664=LINE('',#227894,#28891);
#23665=LINE('',#227896,#28892);
#23666=LINE('',#227898,#28893);
#23667=LINE('',#227902,#28894);
#23668=LINE('',#227904,#28895);
#23669=LINE('',#227908,#28896);
#23670=LINE('',#227912,#28897);
#23671=LINE('',#227913,#28898);
#23672=LINE('',#227917,#28899);
#23673=LINE('',#227921,#28900);
#23674=LINE('',#227928,#28901);
#23675=LINE('',#227930,#28902);
#23676=LINE('',#227932,#28903);
#23677=LINE('',#227936,#28904);
#23678=LINE('',#227938,#28905);
#23679=LINE('',#227942,#28906);
#23680=LINE('',#227946,#28907);
#23681=LINE('',#227947,#28908);
#23682=LINE('',#227953,#28909);
#23683=LINE('',#227955,#28910);
#23684=LINE('',#227957,#28911);
#23685=LINE('',#227961,#28912);
#23686=LINE('',#227963,#28913);
#23687=LINE('',#227967,#28914);
#23688=LINE('',#227971,#28915);
#23689=LINE('',#227972,#28916);
#23690=LINE('',#227974,#28917);
#23691=LINE('',#227975,#28918);
#23692=LINE('',#227981,#28919);
#23693=LINE('',#227983,#28920);
#23694=LINE('',#227985,#28921);
#23695=LINE('',#227989,#28922);
#23696=LINE('',#227991,#28923);
#23697=LINE('',#227995,#28924);
#23698=LINE('',#227999,#28925);
#23699=LINE('',#228000,#28926);
#23700=LINE('',#228006,#28927);
#23701=LINE('',#228008,#28928);
#23702=LINE('',#228010,#28929);
#23703=LINE('',#228014,#28930);
#23704=LINE('',#228016,#28931);
#23705=LINE('',#228020,#28932);
#23706=LINE('',#228024,#28933);
#23707=LINE('',#228025,#28934);
#23708=LINE('',#228029,#28935);
#23709=LINE('',#228033,#28936);
#23710=LINE('',#228040,#28937);
#23711=LINE('',#228042,#28938);
#23712=LINE('',#228044,#28939);
#23713=LINE('',#228048,#28940);
#23714=LINE('',#228050,#28941);
#23715=LINE('',#228054,#28942);
#23716=LINE('',#228058,#28943);
#23717=LINE('',#228059,#28944);
#23718=LINE('',#228065,#28945);
#23719=LINE('',#228067,#28946);
#23720=LINE('',#228069,#28947);
#23721=LINE('',#228073,#28948);
#23722=LINE('',#228075,#28949);
#23723=LINE('',#228079,#28950);
#23724=LINE('',#228083,#28951);
#23725=LINE('',#228084,#28952);
#23726=LINE('',#228088,#28953);
#23727=LINE('',#228092,#28954);
#23728=LINE('',#228099,#28955);
#23729=LINE('',#228101,#28956);
#23730=LINE('',#228103,#28957);
#23731=LINE('',#228107,#28958);
#23732=LINE('',#228109,#28959);
#23733=LINE('',#228113,#28960);
#23734=LINE('',#228117,#28961);
#23735=LINE('',#228118,#28962);
#23736=LINE('',#228124,#28963);
#23737=LINE('',#228126,#28964);
#23738=LINE('',#228128,#28965);
#23739=LINE('',#228132,#28966);
#23740=LINE('',#228134,#28967);
#23741=LINE('',#228138,#28968);
#23742=LINE('',#228142,#28969);
#23743=LINE('',#228143,#28970);
#23744=LINE('',#228147,#28971);
#23745=LINE('',#228151,#28972);
#23746=LINE('',#228158,#28973);
#23747=LINE('',#228160,#28974);
#23748=LINE('',#228162,#28975);
#23749=LINE('',#228166,#28976);
#23750=LINE('',#228168,#28977);
#23751=LINE('',#228172,#28978);
#23752=LINE('',#228176,#28979);
#23753=LINE('',#228177,#28980);
#23754=LINE('',#228183,#28981);
#23755=LINE('',#228185,#28982);
#23756=LINE('',#228187,#28983);
#23757=LINE('',#228191,#28984);
#23758=LINE('',#228193,#28985);
#23759=LINE('',#228197,#28986);
#23760=LINE('',#228201,#28987);
#23761=LINE('',#228202,#28988);
#23762=LINE('',#228206,#28989);
#23763=LINE('',#228210,#28990);
#23764=LINE('',#228217,#28991);
#23765=LINE('',#228219,#28992);
#23766=LINE('',#228221,#28993);
#23767=LINE('',#228225,#28994);
#23768=LINE('',#228227,#28995);
#23769=LINE('',#228231,#28996);
#23770=LINE('',#228235,#28997);
#23771=LINE('',#228236,#28998);
#23772=LINE('',#228242,#28999);
#23773=LINE('',#228244,#29000);
#23774=LINE('',#228246,#29001);
#23775=LINE('',#228250,#29002);
#23776=LINE('',#228252,#29003);
#23777=LINE('',#228256,#29004);
#23778=LINE('',#228260,#29005);
#23779=LINE('',#228261,#29006);
#23780=LINE('',#228265,#29007);
#23781=LINE('',#228269,#29008);
#23782=LINE('',#228276,#29009);
#23783=LINE('',#228278,#29010);
#23784=LINE('',#228280,#29011);
#23785=LINE('',#228284,#29012);
#23786=LINE('',#228286,#29013);
#23787=LINE('',#228290,#29014);
#23788=LINE('',#228294,#29015);
#23789=LINE('',#228295,#29016);
#23790=LINE('',#228301,#29017);
#23791=LINE('',#228303,#29018);
#23792=LINE('',#228305,#29019);
#23793=LINE('',#228309,#29020);
#23794=LINE('',#228311,#29021);
#23795=LINE('',#228315,#29022);
#23796=LINE('',#228319,#29023);
#23797=LINE('',#228320,#29024);
#23798=LINE('',#228324,#29025);
#23799=LINE('',#228328,#29026);
#23800=LINE('',#228335,#29027);
#23801=LINE('',#228337,#29028);
#23802=LINE('',#228339,#29029);
#23803=LINE('',#228343,#29030);
#23804=LINE('',#228345,#29031);
#23805=LINE('',#228349,#29032);
#23806=LINE('',#228353,#29033);
#23807=LINE('',#228354,#29034);
#23808=LINE('',#228360,#29035);
#23809=LINE('',#228362,#29036);
#23810=LINE('',#228364,#29037);
#23811=LINE('',#228368,#29038);
#23812=LINE('',#228370,#29039);
#23813=LINE('',#228374,#29040);
#23814=LINE('',#228378,#29041);
#23815=LINE('',#228379,#29042);
#23816=LINE('',#228383,#29043);
#23817=LINE('',#228387,#29044);
#23818=LINE('',#228394,#29045);
#23819=LINE('',#228396,#29046);
#23820=LINE('',#228398,#29047);
#23821=LINE('',#228402,#29048);
#23822=LINE('',#228404,#29049);
#23823=LINE('',#228408,#29050);
#23824=LINE('',#228412,#29051);
#23825=LINE('',#228413,#29052);
#23826=LINE('',#228419,#29053);
#23827=LINE('',#228421,#29054);
#23828=LINE('',#228423,#29055);
#23829=LINE('',#228427,#29056);
#23830=LINE('',#228429,#29057);
#23831=LINE('',#228433,#29058);
#23832=LINE('',#228437,#29059);
#23833=LINE('',#228438,#29060);
#23834=LINE('',#228442,#29061);
#23835=LINE('',#228446,#29062);
#23836=LINE('',#228453,#29063);
#23837=LINE('',#228455,#29064);
#23838=LINE('',#228457,#29065);
#23839=LINE('',#228461,#29066);
#23840=LINE('',#228463,#29067);
#23841=LINE('',#228467,#29068);
#23842=LINE('',#228471,#29069);
#23843=LINE('',#228472,#29070);
#23844=LINE('',#228478,#29071);
#23845=LINE('',#228480,#29072);
#23846=LINE('',#228482,#29073);
#23847=LINE('',#228486,#29074);
#23848=LINE('',#228488,#29075);
#23849=LINE('',#228492,#29076);
#23850=LINE('',#228496,#29077);
#23851=LINE('',#228497,#29078);
#23852=LINE('',#228501,#29079);
#23853=LINE('',#228505,#29080);
#23854=LINE('',#228512,#29081);
#23855=LINE('',#228514,#29082);
#23856=LINE('',#228516,#29083);
#23857=LINE('',#228520,#29084);
#23858=LINE('',#228522,#29085);
#23859=LINE('',#228526,#29086);
#23860=LINE('',#228530,#29087);
#23861=LINE('',#228531,#29088);
#23862=LINE('',#228537,#29089);
#23863=LINE('',#228539,#29090);
#23864=LINE('',#228541,#29091);
#23865=LINE('',#228545,#29092);
#23866=LINE('',#228547,#29093);
#23867=LINE('',#228551,#29094);
#23868=LINE('',#228555,#29095);
#23869=LINE('',#228556,#29096);
#23870=LINE('',#228560,#29097);
#23871=LINE('',#228564,#29098);
#23872=LINE('',#228571,#29099);
#23873=LINE('',#228573,#29100);
#23874=LINE('',#228575,#29101);
#23875=LINE('',#228579,#29102);
#23876=LINE('',#228581,#29103);
#23877=LINE('',#228585,#29104);
#23878=LINE('',#228589,#29105);
#23879=LINE('',#228590,#29106);
#23880=LINE('',#228596,#29107);
#23881=LINE('',#228598,#29108);
#23882=LINE('',#228600,#29109);
#23883=LINE('',#228604,#29110);
#23884=LINE('',#228606,#29111);
#23885=LINE('',#228610,#29112);
#23886=LINE('',#228614,#29113);
#23887=LINE('',#228615,#29114);
#23888=LINE('',#228619,#29115);
#23889=LINE('',#228623,#29116);
#23890=LINE('',#228630,#29117);
#23891=LINE('',#228632,#29118);
#23892=LINE('',#228634,#29119);
#23893=LINE('',#228638,#29120);
#23894=LINE('',#228640,#29121);
#23895=LINE('',#228644,#29122);
#23896=LINE('',#228648,#29123);
#23897=LINE('',#228649,#29124);
#23898=LINE('',#228655,#29125);
#23899=LINE('',#228657,#29126);
#23900=LINE('',#228659,#29127);
#23901=LINE('',#228663,#29128);
#23902=LINE('',#228665,#29129);
#23903=LINE('',#228669,#29130);
#23904=LINE('',#228673,#29131);
#23905=LINE('',#228674,#29132);
#23906=LINE('',#228678,#29133);
#23907=LINE('',#228682,#29134);
#23908=LINE('',#228689,#29135);
#23909=LINE('',#228691,#29136);
#23910=LINE('',#228693,#29137);
#23911=LINE('',#228697,#29138);
#23912=LINE('',#228699,#29139);
#23913=LINE('',#228703,#29140);
#23914=LINE('',#228707,#29141);
#23915=LINE('',#228708,#29142);
#23916=LINE('',#228714,#29143);
#23917=LINE('',#228716,#29144);
#23918=LINE('',#228718,#29145);
#23919=LINE('',#228722,#29146);
#23920=LINE('',#228724,#29147);
#23921=LINE('',#228728,#29148);
#23922=LINE('',#228732,#29149);
#23923=LINE('',#228733,#29150);
#23924=LINE('',#228737,#29151);
#23925=LINE('',#228741,#29152);
#23926=LINE('',#228748,#29153);
#23927=LINE('',#228750,#29154);
#23928=LINE('',#228752,#29155);
#23929=LINE('',#228756,#29156);
#23930=LINE('',#228758,#29157);
#23931=LINE('',#228762,#29158);
#23932=LINE('',#228766,#29159);
#23933=LINE('',#228767,#29160);
#23934=LINE('',#228773,#29161);
#23935=LINE('',#228775,#29162);
#23936=LINE('',#228777,#29163);
#23937=LINE('',#228781,#29164);
#23938=LINE('',#228783,#29165);
#23939=LINE('',#228787,#29166);
#23940=LINE('',#228791,#29167);
#23941=LINE('',#228792,#29168);
#23942=LINE('',#228796,#29169);
#23943=LINE('',#228800,#29170);
#23944=LINE('',#228807,#29171);
#23945=LINE('',#228809,#29172);
#23946=LINE('',#228811,#29173);
#23947=LINE('',#228815,#29174);
#23948=LINE('',#228817,#29175);
#23949=LINE('',#228821,#29176);
#23950=LINE('',#228825,#29177);
#23951=LINE('',#228826,#29178);
#23952=LINE('',#228832,#29179);
#23953=LINE('',#228834,#29180);
#23954=LINE('',#228836,#29181);
#23955=LINE('',#228840,#29182);
#23956=LINE('',#228842,#29183);
#23957=LINE('',#228846,#29184);
#23958=LINE('',#228850,#29185);
#23959=LINE('',#228851,#29186);
#23960=LINE('',#253407,#29187);
#23961=LINE('',#253409,#29188);
#23962=LINE('',#253414,#29189);
#23963=LINE('',#253434,#29190);
#23964=LINE('',#253437,#29191);
#23965=LINE('',#253547,#29192);
#23966=LINE('',#253578,#29193);
#23967=LINE('',#253581,#29194);
#23968=LINE('',#253630,#29195);
#23969=LINE('',#253648,#29196);
#23970=LINE('',#253654,#29197);
#23971=LINE('',#253660,#29198);
#23972=LINE('',#253666,#29199);
#23973=LINE('',#253672,#29200);
#23974=LINE('',#253676,#29201);
#23975=LINE('',#253679,#29202);
#23976=LINE('',#254180,#29203);
#23977=LINE('',#254191,#29204);
#23978=LINE('',#254195,#29205);
#23979=LINE('',#254251,#29206);
#23980=LINE('',#254257,#29207);
#23981=LINE('',#254320,#29208);
#23982=LINE('',#254324,#29209);
#23983=LINE('',#254380,#29210);
#23984=LINE('',#254384,#29211);
#23985=LINE('',#254385,#29212);
#23986=LINE('',#254386,#29213);
#23987=LINE('',#254388,#29214);
#23988=LINE('',#254389,#29215);
#23989=LINE('',#254393,#29216);
#23990=LINE('',#254395,#29217);
#23991=LINE('',#254397,#29218);
#23992=LINE('',#254398,#29219);
#23993=LINE('',#254401,#29220);
#23994=LINE('',#254403,#29221);
#23995=LINE('',#254521,#29222);
#23996=LINE('',#254523,#29223);
#23997=LINE('',#254587,#29224);
#23998=LINE('',#254657,#29225);
#23999=LINE('',#254658,#29226);
#24000=LINE('',#254659,#29227);
#24001=LINE('',#254663,#29228);
#24002=LINE('',#254667,#29229);
#24003=LINE('',#254671,#29230);
#24004=LINE('',#254673,#29231);
#24005=LINE('',#254674,#29232);
#24006=LINE('',#254679,#29233);
#24007=LINE('',#254683,#29234);
#24008=LINE('',#254685,#29235);
#24009=LINE('',#254686,#29236);
#24010=LINE('',#254691,#29237);
#24011=LINE('',#254695,#29238);
#24012=LINE('',#254697,#29239);
#24013=LINE('',#254698,#29240);
#24014=LINE('',#254703,#29241);
#24015=LINE('',#254706,#29242);
#24016=LINE('',#254707,#29243);
#24017=LINE('',#254757,#29244);
#24018=LINE('',#254761,#29245);
#24019=LINE('',#254816,#29246);
#24020=LINE('',#254818,#29247);
#24021=LINE('',#254846,#29248);
#24022=LINE('',#254851,#29249);
#24023=LINE('',#254853,#29250);
#24024=LINE('',#254862,#29251);
#24025=LINE('',#254998,#29252);
#24026=LINE('',#255001,#29253);
#24027=LINE('',#255004,#29254);
#24028=LINE('',#255025,#29255);
#24029=LINE('',#255044,#29256);
#24030=LINE('',#255046,#29257);
#24031=LINE('',#255054,#29258);
#24032=LINE('',#255055,#29259);
#24033=LINE('',#255059,#29260);
#24034=LINE('',#255063,#29261);
#24035=LINE('',#255070,#29262);
#24036=LINE('',#255074,#29263);
#24037=LINE('',#255079,#29264);
#24038=LINE('',#255083,#29265);
#24039=LINE('',#255087,#29266);
#24040=LINE('',#255090,#29267);
#24041=LINE('',#255093,#29268);
#24042=LINE('',#255096,#29269);
#24043=LINE('',#255099,#29270);
#24044=LINE('',#255161,#29271);
#24045=LINE('',#255164,#29272);
#24046=LINE('',#255223,#29273);
#24047=LINE('',#255286,#29274);
#24048=LINE('',#255287,#29275);
#24049=LINE('',#255293,#29276);
#24050=LINE('',#255296,#29277);
#24051=LINE('',#255298,#29278);
#24052=LINE('',#255301,#29279);
#24053=LINE('',#255359,#29280);
#24054=LINE('',#255363,#29281);
#24055=LINE('',#255425,#29282);
#24056=LINE('',#255426,#29283);
#24057=LINE('',#255432,#29284);
#24058=LINE('',#255436,#29285);
#24059=LINE('',#255443,#29286);
#24060=LINE('',#255446,#29287);
#24061=LINE('',#255506,#29288);
#24062=LINE('',#255507,#29289);
#24063=LINE('',#255510,#29290);
#24064=LINE('',#255572,#29291);
#24065=LINE('',#255573,#29292);
#24066=LINE('',#255579,#29293);
#24067=LINE('',#255582,#29294);
#24068=LINE('',#255583,#29295);
#24069=LINE('',#255586,#29296);
#24070=LINE('',#255589,#29297);
#24071=LINE('',#255590,#29298);
#24072=LINE('',#261328,#29299);
#24073=LINE('',#261411,#29300);
#24074=LINE('',#261529,#29301);
#24075=LINE('',#261571,#29302);
#24076=LINE('',#261574,#29303);
#24077=LINE('',#261616,#29304);
#24078=LINE('',#261619,#29305);
#24079=LINE('',#261621,#29306);
#24080=LINE('',#261625,#29307);
#24081=LINE('',#261628,#29308);
#24082=LINE('',#261634,#29309);
#24083=LINE('',#261644,#29310);
#24084=LINE('',#261681,#29311);
#24085=LINE('',#261719,#29312);
#24086=LINE('',#261757,#29313);
#24087=LINE('',#261795,#29314);
#24088=LINE('',#261833,#29315);
#24089=LINE('',#261871,#29316);
#24090=LINE('',#261887,#29317);
#24091=LINE('',#261941,#29318);
#24092=LINE('',#262017,#29319);
#24093=LINE('',#262093,#29320);
#24094=LINE('',#262169,#29321);
#24095=LINE('',#262245,#29322);
#24096=LINE('',#262323,#29323);
#24097=LINE('',#262393,#29324);
#24098=LINE('',#262403,#29325);
#24099=LINE('',#262467,#29326);
#24100=LINE('',#262469,#29327);
#24101=LINE('',#262471,#29328);
#24102=LINE('',#262473,#29329);
#24103=LINE('',#262475,#29330);
#24104=LINE('',#262476,#29331);
#24105=LINE('',#262478,#29332);
#24106=LINE('',#262479,#29333);
#24107=LINE('',#262481,#29334);
#24108=LINE('',#262483,#29335);
#24109=LINE('',#262485,#29336);
#24110=LINE('',#262487,#29337);
#24111=LINE('',#263171,#29338);
#24112=LINE('',#263208,#29339);
#24113=LINE('',#263246,#29340);
#24114=LINE('',#263284,#29341);
#24115=LINE('',#263322,#29342);
#24116=LINE('',#263360,#29343);
#24117=LINE('',#263398,#29344);
#24118=LINE('',#263414,#29345);
#24119=LINE('',#263468,#29346);
#24120=LINE('',#263544,#29347);
#24121=LINE('',#263620,#29348);
#24122=LINE('',#263696,#29349);
#24123=LINE('',#263772,#29350);
#24124=LINE('',#263850,#29351);
#24125=LINE('',#263920,#29352);
#24126=LINE('',#263930,#29353);
#24127=LINE('',#263994,#29354);
#24128=LINE('',#263996,#29355);
#24129=LINE('',#263998,#29356);
#24130=LINE('',#264000,#29357);
#24131=LINE('',#264002,#29358);
#24132=LINE('',#264003,#29359);
#24133=LINE('',#264005,#29360);
#24134=LINE('',#264006,#29361);
#24135=LINE('',#264008,#29362);
#24136=LINE('',#264010,#29363);
#24137=LINE('',#264012,#29364);
#24138=LINE('',#264014,#29365);
#24139=LINE('',#264699,#29366);
#24140=LINE('',#264707,#29367);
#24141=LINE('',#264713,#29368);
#24142=LINE('',#264721,#29369);
#24143=LINE('',#264725,#29370);
#24144=LINE('',#264745,#29371);
#24145=LINE('',#264806,#29372);
#24146=LINE('',#264843,#29373);
#24147=LINE('',#264883,#29374);
#24148=LINE('',#264884,#29375);
#24149=LINE('',#264891,#29376);
#24150=LINE('',#264897,#29377);
#24151=LINE('',#264910,#29378);
#24152=LINE('',#264916,#29379);
#24153=LINE('',#264919,#29380);
#24154=LINE('',#264924,#29381);
#24155=LINE('',#264930,#29382);
#24156=LINE('',#264936,#29383);
#24157=LINE('',#264942,#29384);
#24158=LINE('',#264948,#29385);
#24159=LINE('',#264954,#29386);
#24160=LINE('',#264960,#29387);
#24161=LINE('',#264966,#29388);
#24162=LINE('',#264972,#29389);
#24163=LINE('',#264978,#29390);
#24164=LINE('',#264983,#29391);
#24165=LINE('',#264987,#29392);
#24166=LINE('',#264991,#29393);
#24167=LINE('',#264993,#29394);
#24168=LINE('',#264994,#29395);
#24169=LINE('',#264999,#29396);
#24170=LINE('',#265003,#29397);
#24171=LINE('',#265005,#29398);
#24172=LINE('',#265006,#29399);
#24173=LINE('',#265011,#29400);
#24174=LINE('',#265015,#29401);
#24175=LINE('',#265017,#29402);
#24176=LINE('',#265018,#29403);
#24177=LINE('',#265023,#29404);
#24178=LINE('',#265026,#29405);
#24179=LINE('',#265027,#29406);
#24180=LINE('',#265031,#29407);
#24181=LINE('',#265035,#29408);
#24182=LINE('',#265039,#29409);
#24183=LINE('',#265043,#29410);
#24184=LINE('',#265054,#29411);
#24185=LINE('',#265058,#29412);
#24186=LINE('',#265062,#29413);
#24187=LINE('',#265065,#29414);
#24188=LINE('',#265068,#29415);
#24189=LINE('',#265071,#29416);
#24190=LINE('',#265074,#29417);
#24191=LINE('',#265075,#29418);
#24192=LINE('',#265078,#29419);
#24193=LINE('',#265082,#29420);
#24194=LINE('',#265083,#29421);
#24195=LINE('',#265086,#29422);
#24196=LINE('',#265090,#29423);
#24197=LINE('',#265091,#29424);
#24198=LINE('',#265094,#29425);
#24199=LINE('',#265097,#29426);
#24200=LINE('',#265118,#29427);
#24201=LINE('',#265122,#29428);
#24202=LINE('',#265126,#29429);
#24203=LINE('',#265129,#29430);
#24204=LINE('',#265131,#29431);
#24205=LINE('',#265134,#29432);
#24206=LINE('',#265140,#29433);
#24207=LINE('',#265143,#29434);
#24208=LINE('',#265145,#29435);
#24209=LINE('',#265147,#29436);
#24210=LINE('',#265150,#29437);
#24211=LINE('',#265153,#29438);
#24212=LINE('',#265155,#29439);
#24213=LINE('',#265156,#29440);
#24214=LINE('',#265339,#29441);
#24215=LINE('',#265510,#29442);
#24216=LINE('',#265517,#29443);
#24217=LINE('',#265697,#29444);
#24218=LINE('',#265860,#29445);
#24219=LINE('',#265861,#29446);
#24220=LINE('',#266045,#29447);
#24221=LINE('',#266214,#29448);
#24222=LINE('',#266223,#29449);
#24223=LINE('',#266401,#29450);
#24224=LINE('',#266564,#29451);
#24225=LINE('',#266565,#29452);
#24226=LINE('',#266572,#29453);
#24227=LINE('',#266576,#29454);
#24228=LINE('',#266614,#29455);
#24229=LINE('',#266675,#29456);
#24230=LINE('',#266753,#29457);
#24231=LINE('',#266832,#29458);
#24232=LINE('',#266911,#29459);
#24233=LINE('',#267027,#29460);
#24234=LINE('',#267121,#29461);
#24235=LINE('',#267122,#29462);
#24236=LINE('',#267124,#29463);
#24237=LINE('',#268110,#29464);
#24238=LINE('',#268124,#29465);
#24239=LINE('',#271698,#29466);
#24240=LINE('',#271712,#29467);
#24241=LINE('',#272378,#29468);
#24242=LINE('',#272731,#29469);
#24243=LINE('',#273068,#29470);
#24244=LINE('',#273409,#29471);
#24245=LINE('',#273745,#29472);
#24246=LINE('',#273747,#29473);
#24247=LINE('',#273749,#29474);
#24248=LINE('',#273750,#29475);
#24249=LINE('',#273754,#29476);
#24250=LINE('',#273758,#29477);
#24251=LINE('',#273760,#29478);
#24252=LINE('',#273762,#29479);
#24253=LINE('',#273767,#29480);
#24254=LINE('',#273769,#29481);
#24255=LINE('',#273771,#29482);
#24256=LINE('',#273773,#29483);
#24257=LINE('',#273774,#29484);
#24258=LINE('',#273776,#29485);
#24259=LINE('',#273777,#29486);
#24260=LINE('',#273781,#29487);
#24261=LINE('',#273783,#29488);
#24262=LINE('',#273785,#29489);
#24263=LINE('',#273786,#29490);
#24264=LINE('',#273790,#29491);
#24265=LINE('',#273792,#29492);
#24266=LINE('',#273794,#29493);
#24267=LINE('',#273796,#29494);
#24268=LINE('',#273797,#29495);
#24269=LINE('',#273799,#29496);
#24270=LINE('',#273800,#29497);
#24271=LINE('',#273804,#29498);
#24272=LINE('',#273806,#29499);
#24273=LINE('',#273808,#29500);
#24274=LINE('',#273809,#29501);
#24275=LINE('',#273813,#29502);
#24276=LINE('',#273817,#29503);
#24277=LINE('',#273821,#29504);
#24278=LINE('',#273825,#29505);
#24279=LINE('',#273829,#29506);
#24280=LINE('',#273833,#29507);
#24281=LINE('',#273837,#29508);
#24282=LINE('',#273841,#29509);
#24283=LINE('',#273846,#29510);
#24284=LINE('',#273848,#29511);
#24285=LINE('',#273850,#29512);
#24286=LINE('',#273851,#29513);
#24287=LINE('',#273855,#29514);
#24288=LINE('',#273857,#29515);
#24289=LINE('',#273859,#29516);
#24290=LINE('',#273860,#29517);
#24291=LINE('',#273864,#29518);
#24292=LINE('',#273866,#29519);
#24293=LINE('',#273868,#29520);
#24294=LINE('',#273869,#29521);
#24295=LINE('',#273873,#29522);
#24296=LINE('',#273875,#29523);
#24297=LINE('',#273877,#29524);
#24298=LINE('',#273878,#29525);
#24299=LINE('',#273997,#29526);
#24300=LINE('',#273999,#29527);
#24301=LINE('',#274000,#29528);
#24302=LINE('',#274003,#29529);
#24303=LINE('',#274005,#29530);
#24304=LINE('',#274007,#29531);
#24305=LINE('',#274009,#29532);
#24306=LINE('',#274011,#29533);
#24307=LINE('',#274012,#29534);
#24308=LINE('',#274015,#29535);
#24309=LINE('',#274017,#29536);
#24310=LINE('',#274018,#29537);
#24311=LINE('',#274021,#29538);
#24312=LINE('',#274023,#29539);
#24313=LINE('',#274025,#29540);
#24314=LINE('',#274026,#29541);
#24315=LINE('',#274027,#29542);
#24316=LINE('',#274031,#29543);
#24317=LINE('',#274121,#29544);
#24318=LINE('',#274123,#29545);
#24319=LINE('',#274125,#29546);
#24320=LINE('',#274126,#29547);
#24321=LINE('',#274129,#29548);
#24322=LINE('',#274131,#29549);
#24323=LINE('',#274132,#29550);
#24324=LINE('',#274135,#29551);
#24325=LINE('',#274136,#29552);
#24326=LINE('',#274139,#29553);
#24327=LINE('',#274140,#29554);
#24328=LINE('',#274142,#29555);
#24329=LINE('',#274145,#29556);
#24330=LINE('',#274148,#29557);
#24331=LINE('',#274156,#29558);
#24332=LINE('',#274159,#29559);
#24333=LINE('',#274165,#29560);
#24334=LINE('',#274169,#29561);
#24335=LINE('',#274173,#29562);
#24336=LINE('',#274177,#29563);
#24337=LINE('',#274181,#29564);
#24338=LINE('',#274185,#29565);
#24339=LINE('',#274188,#29566);
#24340=LINE('',#274189,#29567);
#24341=LINE('',#274192,#29568);
#24342=LINE('',#274193,#29569);
#24343=LINE('',#274196,#29570);
#24344=LINE('',#274197,#29571);
#24345=LINE('',#274200,#29572);
#24346=LINE('',#274204,#29573);
#24347=LINE('',#274205,#29574);
#24348=LINE('',#274208,#29575);
#24349=LINE('',#274212,#29576);
#24350=LINE('',#274213,#29577);
#24351=LINE('',#274216,#29578);
#24352=LINE('',#274220,#29579);
#24353=LINE('',#274221,#29580);
#24354=LINE('',#274224,#29581);
#24355=LINE('',#274228,#29582);
#24356=LINE('',#274229,#29583);
#24357=LINE('',#274232,#29584);
#24358=LINE('',#274236,#29585);
#24359=LINE('',#274237,#29586);
#24360=LINE('',#274240,#29587);
#24361=LINE('',#274244,#29588);
#24362=LINE('',#274245,#29589);
#24363=LINE('',#274254,#29590);
#24364=LINE('',#274258,#29591);
#24365=LINE('',#274262,#29592);
#24366=LINE('',#274265,#29593);
#24367=LINE('',#274268,#29594);
#24368=LINE('',#274270,#29595);
#24369=LINE('',#274271,#29596);
#24370=LINE('',#274274,#29597);
#24371=LINE('',#274278,#29598);
#24372=LINE('',#274279,#29599);
#24373=LINE('',#274282,#29600);
#24374=LINE('',#274286,#29601);
#24375=LINE('',#274287,#29602);
#24376=LINE('',#274290,#29603);
#24377=LINE('',#274294,#29604);
#24378=LINE('',#274295,#29605);
#24379=LINE('',#274304,#29606);
#24380=LINE('',#274308,#29607);
#24381=LINE('',#274312,#29608);
#24382=LINE('',#274316,#29609);
#24383=LINE('',#274318,#29610);
#24384=LINE('',#274320,#29611);
#24385=LINE('',#274324,#29612);
#24386=LINE('',#274328,#29613);
#24387=LINE('',#274332,#29614);
#24388=LINE('',#274336,#29615);
#24389=LINE('',#274340,#29616);
#24390=LINE('',#274344,#29617);
#24391=LINE('',#274346,#29618);
#24392=LINE('',#274348,#29619);
#24393=LINE('',#274352,#29620);
#24394=LINE('',#274356,#29621);
#24395=LINE('',#274360,#29622);
#24396=LINE('',#274364,#29623);
#24397=LINE('',#274368,#29624);
#24398=LINE('',#274372,#29625);
#24399=LINE('',#274374,#29626);
#24400=LINE('',#274376,#29627);
#24401=LINE('',#274380,#29628);
#24402=LINE('',#274384,#29629);
#24403=LINE('',#274388,#29630);
#24404=LINE('',#274392,#29631);
#24405=LINE('',#274396,#29632);
#24406=LINE('',#274400,#29633);
#24407=LINE('',#274402,#29634);
#24408=LINE('',#274404,#29635);
#24409=LINE('',#274408,#29636);
#24410=LINE('',#274411,#29637);
#24411=LINE('',#274417,#29638);
#24412=LINE('',#274421,#29639);
#24413=LINE('',#274425,#29640);
#24414=LINE('',#274429,#29641);
#24415=LINE('',#274431,#29642);
#24416=LINE('',#274433,#29643);
#24417=LINE('',#274437,#29644);
#24418=LINE('',#274441,#29645);
#24419=LINE('',#274445,#29646);
#24420=LINE('',#274449,#29647);
#24421=LINE('',#274453,#29648);
#24422=LINE('',#274457,#29649);
#24423=LINE('',#274459,#29650);
#24424=LINE('',#274461,#29651);
#24425=LINE('',#274465,#29652);
#24426=LINE('',#274469,#29653);
#24427=LINE('',#274473,#29654);
#24428=LINE('',#274477,#29655);
#24429=LINE('',#274481,#29656);
#24430=LINE('',#274485,#29657);
#24431=LINE('',#274487,#29658);
#24432=LINE('',#274489,#29659);
#24433=LINE('',#274493,#29660);
#24434=LINE('',#274497,#29661);
#24435=LINE('',#274501,#29662);
#24436=LINE('',#274505,#29663);
#24437=LINE('',#274509,#29664);
#24438=LINE('',#274513,#29665);
#24439=LINE('',#274515,#29666);
#24440=LINE('',#274517,#29667);
#24441=LINE('',#274521,#29668);
#24442=LINE('',#274524,#29669);
#24443=LINE('',#274526,#29670);
#24444=LINE('',#274527,#29671);
#24445=LINE('',#274529,#29672);
#24446=LINE('',#274531,#29673);
#24447=LINE('',#274533,#29674);
#24448=LINE('',#274535,#29675);
#24449=LINE('',#274537,#29676);
#24450=LINE('',#274539,#29677);
#24451=LINE('',#274541,#29678);
#24452=LINE('',#274543,#29679);
#24453=LINE('',#274545,#29680);
#24454=LINE('',#274547,#29681);
#24455=LINE('',#274549,#29682);
#24456=LINE('',#274551,#29683);
#24457=LINE('',#274553,#29684);
#24458=LINE('',#274555,#29685);
#24459=LINE('',#274557,#29686);
#24460=LINE('',#274559,#29687);
#24461=LINE('',#274561,#29688);
#24462=LINE('',#274563,#29689);
#24463=LINE('',#274565,#29690);
#24464=LINE('',#274567,#29691);
#24465=LINE('',#274569,#29692);
#24466=LINE('',#274571,#29693);
#24467=LINE('',#274573,#29694);
#24468=LINE('',#274575,#29695);
#24469=LINE('',#274577,#29696);
#24470=LINE('',#274579,#29697);
#24471=LINE('',#274581,#29698);
#24472=LINE('',#274583,#29699);
#24473=LINE('',#274585,#29700);
#24474=LINE('',#274587,#29701);
#24475=LINE('',#274589,#29702);
#24476=LINE('',#274591,#29703);
#24477=LINE('',#274593,#29704);
#24478=LINE('',#274595,#29705);
#24479=LINE('',#274597,#29706);
#24480=LINE('',#274599,#29707);
#24481=LINE('',#274601,#29708);
#24482=LINE('',#274603,#29709);
#24483=LINE('',#274605,#29710);
#24484=LINE('',#274607,#29711);
#24485=LINE('',#274609,#29712);
#24486=LINE('',#274611,#29713);
#24487=LINE('',#274613,#29714);
#24488=LINE('',#274615,#29715);
#24489=LINE('',#274617,#29716);
#24490=LINE('',#274619,#29717);
#24491=LINE('',#274621,#29718);
#24492=LINE('',#274623,#29719);
#24493=LINE('',#274625,#29720);
#24494=LINE('',#274627,#29721);
#24495=LINE('',#274629,#29722);
#24496=LINE('',#274631,#29723);
#24497=LINE('',#274633,#29724);
#24498=LINE('',#274635,#29725);
#24499=LINE('',#274642,#29726);
#24500=LINE('',#274645,#29727);
#24501=LINE('',#274651,#29728);
#24502=LINE('',#274655,#29729);
#24503=LINE('',#274658,#29730);
#24504=LINE('',#274660,#29731);
#24505=LINE('',#274664,#29732);
#24506=LINE('',#274668,#29733);
#24507=LINE('',#274672,#29734);
#24508=LINE('',#274675,#29735);
#24509=LINE('',#274678,#29736);
#24510=LINE('',#274680,#29737);
#24511=LINE('',#274681,#29738);
#24512=LINE('',#274684,#29739);
#24513=LINE('',#274688,#29740);
#24514=LINE('',#274689,#29741);
#24515=LINE('',#274692,#29742);
#24516=LINE('',#274696,#29743);
#24517=LINE('',#274697,#29744);
#24518=LINE('',#274700,#29745);
#24519=LINE('',#274704,#29746);
#24520=LINE('',#274705,#29747);
#24521=LINE('',#274708,#29748);
#24522=LINE('',#274711,#29749);
#24523=LINE('',#274714,#29750);
#24524=LINE('',#274715,#29751);
#24525=LINE('',#274718,#29752);
#24526=LINE('',#274722,#29753);
#24527=LINE('',#274723,#29754);
#24528=LINE('',#274726,#29755);
#24529=LINE('',#274730,#29756);
#24530=LINE('',#274731,#29757);
#24531=LINE('',#274740,#29758);
#24532=LINE('',#274744,#29759);
#24533=LINE('',#274748,#29760);
#24534=LINE('',#274751,#29761);
#24535=LINE('',#274754,#29762);
#24536=LINE('',#274756,#29763);
#24537=LINE('',#274757,#29764);
#24538=LINE('',#274760,#29765);
#24539=LINE('',#274764,#29766);
#24540=LINE('',#274765,#29767);
#24541=LINE('',#274768,#29768);
#24542=LINE('',#274772,#29769);
#24543=LINE('',#274773,#29770);
#24544=LINE('',#274776,#29771);
#24545=LINE('',#274780,#29772);
#24546=LINE('',#274781,#29773);
#24547=LINE('',#274790,#29774);
#24548=LINE('',#274793,#29775);
#24549=LINE('',#274798,#29776);
#24550=LINE('',#274800,#29777);
#24551=LINE('',#274804,#29778);
#24552=LINE('',#274808,#29779);
#24553=LINE('',#274812,#29780);
#24554=LINE('',#274816,#29781);
#24555=LINE('',#274820,#29782);
#24556=LINE('',#274823,#29783);
#24557=LINE('',#274826,#29784);
#24558=LINE('',#274828,#29785);
#24559=LINE('',#274829,#29786);
#24560=LINE('',#274832,#29787);
#24561=LINE('',#274836,#29788);
#24562=LINE('',#274837,#29789);
#24563=LINE('',#274840,#29790);
#24564=LINE('',#274844,#29791);
#24565=LINE('',#274845,#29792);
#24566=LINE('',#274848,#29793);
#24567=LINE('',#274852,#29794);
#24568=LINE('',#274853,#29795);
#24569=LINE('',#274856,#29796);
#24570=LINE('',#274860,#29797);
#24571=LINE('',#274861,#29798);
#24572=LINE('',#274864,#29799);
#24573=LINE('',#274868,#29800);
#24574=LINE('',#274869,#29801);
#24575=LINE('',#274872,#29802);
#24576=LINE('',#274875,#29803);
#24577=LINE('',#274878,#29804);
#24578=LINE('',#274879,#29805);
#24579=LINE('',#274888,#29806);
#24580=LINE('',#274892,#29807);
#24581=LINE('',#274896,#29808);
#24582=LINE('',#274899,#29809);
#24583=LINE('',#274902,#29810);
#24584=LINE('',#274904,#29811);
#24585=LINE('',#274905,#29812);
#24586=LINE('',#274908,#29813);
#24587=LINE('',#274912,#29814);
#24588=LINE('',#274913,#29815);
#24589=LINE('',#274916,#29816);
#24590=LINE('',#274920,#29817);
#24591=LINE('',#274921,#29818);
#24592=LINE('',#274924,#29819);
#24593=LINE('',#274928,#29820);
#24594=LINE('',#274929,#29821);
#24595=LINE('',#274938,#29822);
#24596=LINE('',#274941,#29823);
#24597=LINE('',#274946,#29824);
#24598=LINE('',#274948,#29825);
#24599=LINE('',#274952,#29826);
#24600=LINE('',#274956,#29827);
#24601=LINE('',#274960,#29828);
#24602=LINE('',#274964,#29829);
#24603=LINE('',#274968,#29830);
#24604=LINE('',#274971,#29831);
#24605=LINE('',#274974,#29832);
#24606=LINE('',#274976,#29833);
#24607=LINE('',#274977,#29834);
#24608=LINE('',#274980,#29835);
#24609=LINE('',#274984,#29836);
#24610=LINE('',#274985,#29837);
#24611=LINE('',#274988,#29838);
#24612=LINE('',#274992,#29839);
#24613=LINE('',#274993,#29840);
#24614=LINE('',#274996,#29841);
#24615=LINE('',#275000,#29842);
#24616=LINE('',#275001,#29843);
#24617=LINE('',#275004,#29844);
#24618=LINE('',#275008,#29845);
#24619=LINE('',#275009,#29846);
#24620=LINE('',#275012,#29847);
#24621=LINE('',#275016,#29848);
#24622=LINE('',#275017,#29849);
#24623=LINE('',#275020,#29850);
#24624=LINE('',#275023,#29851);
#24625=LINE('',#275026,#29852);
#24626=LINE('',#275027,#29853);
#24627=LINE('',#275036,#29854);
#24628=LINE('',#275040,#29855);
#24629=LINE('',#275044,#29856);
#24630=LINE('',#275047,#29857);
#24631=LINE('',#275050,#29858);
#24632=LINE('',#275052,#29859);
#24633=LINE('',#275053,#29860);
#24634=LINE('',#275056,#29861);
#24635=LINE('',#275060,#29862);
#24636=LINE('',#275061,#29863);
#24637=LINE('',#275064,#29864);
#24638=LINE('',#275068,#29865);
#24639=LINE('',#275069,#29866);
#24640=LINE('',#275072,#29867);
#24641=LINE('',#275076,#29868);
#24642=LINE('',#275077,#29869);
#24643=LINE('',#275084,#29870);
#24644=LINE('',#275086,#29871);
#24645=LINE('',#275088,#29872);
#24646=LINE('',#275089,#29873);
#24647=LINE('',#275093,#29874);
#24648=LINE('',#275095,#29875);
#24649=LINE('',#275097,#29876);
#24650=LINE('',#275098,#29877);
#24651=LINE('',#275102,#29878);
#24652=LINE('',#275104,#29879);
#24653=LINE('',#275106,#29880);
#24654=LINE('',#275107,#29881);
#24655=LINE('',#275110,#29882);
#24656=LINE('',#275112,#29883);
#24657=LINE('',#275113,#29884);
#24658=LINE('',#275116,#29885);
#24659=LINE('',#275118,#29886);
#24660=LINE('',#275119,#29887);
#24661=LINE('',#275125,#29888);
#24662=LINE('',#275128,#29889);
#24663=LINE('',#275130,#29890);
#24664=LINE('',#275131,#29891);
#24665=LINE('',#275137,#29892);
#24666=LINE('',#275140,#29893);
#24667=LINE('',#275142,#29894);
#24668=LINE('',#275143,#29895);
#24669=LINE('',#275149,#29896);
#24670=LINE('',#275152,#29897);
#24671=LINE('',#275154,#29898);
#24672=LINE('',#275155,#29899);
#24673=LINE('',#275161,#29900);
#24674=LINE('',#275164,#29901);
#24675=LINE('',#275166,#29902);
#24676=LINE('',#275167,#29903);
#24677=LINE('',#275170,#29904);
#24678=LINE('',#275172,#29905);
#24679=LINE('',#275173,#29906);
#24680=LINE('',#275176,#29907);
#24681=LINE('',#275178,#29908);
#24682=LINE('',#275179,#29909);
#24683=LINE('',#275182,#29910);
#24684=LINE('',#275184,#29911);
#24685=LINE('',#275185,#29912);
#24686=LINE('',#275189,#29913);
#24687=LINE('',#275191,#29914);
#24688=LINE('',#275193,#29915);
#24689=LINE('',#275194,#29916);
#24690=LINE('',#275197,#29917);
#24691=LINE('',#275199,#29918);
#24692=LINE('',#275200,#29919);
#24693=LINE('',#275203,#29920);
#24694=LINE('',#275205,#29921);
#24695=LINE('',#275206,#29922);
#24696=LINE('',#275209,#29923);
#24697=LINE('',#275211,#29924);
#24698=LINE('',#275212,#29925);
#24699=LINE('',#275218,#29926);
#24700=LINE('',#275221,#29927);
#24701=LINE('',#275223,#29928);
#24702=LINE('',#275224,#29929);
#24703=LINE('',#275230,#29930);
#24704=LINE('',#275233,#29931);
#24705=LINE('',#275235,#29932);
#24706=LINE('',#275236,#29933);
#24707=LINE('',#275242,#29934);
#24708=LINE('',#275245,#29935);
#24709=LINE('',#275247,#29936);
#24710=LINE('',#275248,#29937);
#24711=LINE('',#275254,#29938);
#24712=LINE('',#275257,#29939);
#24713=LINE('',#275259,#29940);
#24714=LINE('',#275260,#29941);
#24715=LINE('',#275263,#29942);
#24716=LINE('',#275265,#29943);
#24717=LINE('',#275266,#29944);
#24718=LINE('',#275269,#29945);
#24719=LINE('',#275271,#29946);
#24720=LINE('',#275272,#29947);
#24721=LINE('',#275275,#29948);
#24722=LINE('',#275277,#29949);
#24723=LINE('',#275278,#29950);
#24724=LINE('',#275284,#29951);
#24725=LINE('',#275287,#29952);
#24726=LINE('',#275289,#29953);
#24727=LINE('',#275290,#29954);
#24728=LINE('',#275296,#29955);
#24729=LINE('',#275299,#29956);
#24730=LINE('',#275301,#29957);
#24731=LINE('',#275302,#29958);
#24732=LINE('',#275309,#29959);
#24733=LINE('',#275311,#29960);
#24734=LINE('',#275313,#29961);
#24735=LINE('',#275314,#29962);
#24736=LINE('',#275320,#29963);
#24737=LINE('',#275323,#29964);
#24738=LINE('',#275325,#29965);
#24739=LINE('',#275326,#29966);
#24740=LINE('',#275329,#29967);
#24741=LINE('',#275331,#29968);
#24742=LINE('',#275332,#29969);
#24743=LINE('',#275335,#29970);
#24744=LINE('',#275337,#29971);
#24745=LINE('',#275338,#29972);
#24746=LINE('',#275341,#29973);
#24747=LINE('',#275343,#29974);
#24748=LINE('',#275344,#29975);
#24749=LINE('',#275350,#29976);
#24750=LINE('',#275353,#29977);
#24751=LINE('',#275355,#29978);
#24752=LINE('',#275356,#29979);
#24753=LINE('',#275359,#29980);
#24754=LINE('',#275361,#29981);
#24755=LINE('',#275362,#29982);
#24756=LINE('',#275365,#29983);
#24757=LINE('',#275367,#29984);
#24758=LINE('',#275368,#29985);
#24759=LINE('',#275371,#29986);
#24760=LINE('',#275373,#29987);
#24761=LINE('',#275374,#29988);
#24762=LINE('',#275380,#29989);
#24763=LINE('',#275383,#29990);
#24764=LINE('',#275385,#29991);
#24765=LINE('',#275386,#29992);
#24766=LINE('',#275392,#29993);
#24767=LINE('',#275395,#29994);
#24768=LINE('',#275397,#29995);
#24769=LINE('',#275398,#29996);
#24770=LINE('',#275404,#29997);
#24771=LINE('',#275407,#29998);
#24772=LINE('',#275409,#29999);
#24773=LINE('',#275410,#30000);
#24774=LINE('',#275416,#30001);
#24775=LINE('',#275418,#30002);
#24776=LINE('',#275419,#30003);
#24777=LINE('',#275423,#30004);
#24778=LINE('',#275425,#30005);
#24779=LINE('',#275427,#30006);
#24780=LINE('',#275428,#30007);
#24781=LINE('',#275431,#30008);
#24782=LINE('',#275433,#30009);
#24783=LINE('',#275434,#30010);
#24784=LINE('',#275437,#30011);
#24785=LINE('',#275439,#30012);
#24786=LINE('',#275440,#30013);
#24787=LINE('',#275446,#30014);
#24788=LINE('',#275449,#30015);
#24789=LINE('',#275451,#30016);
#24790=LINE('',#275452,#30017);
#24791=LINE('',#275458,#30018);
#24792=LINE('',#275461,#30019);
#24793=LINE('',#275463,#30020);
#24794=LINE('',#275464,#30021);
#24795=LINE('',#275470,#30022);
#24796=LINE('',#275473,#30023);
#24797=LINE('',#275475,#30024);
#24798=LINE('',#275476,#30025);
#24799=LINE('',#275482,#30026);
#24800=LINE('',#275485,#30027);
#24801=LINE('',#275487,#30028);
#24802=LINE('',#275488,#30029);
#24803=LINE('',#275491,#30030);
#24804=LINE('',#275493,#30031);
#24805=LINE('',#275494,#30032);
#24806=LINE('',#275496,#30033);
#24807=LINE('',#275497,#30034);
#24808=LINE('',#275501,#30035);
#24809=LINE('',#275503,#30036);
#24810=LINE('',#275505,#30037);
#24811=LINE('',#275506,#30038);
#24812=LINE('',#275509,#30039);
#24813=LINE('',#275511,#30040);
#24814=LINE('',#275512,#30041);
#24815=LINE('',#275515,#30042);
#24816=LINE('',#275517,#30043);
#24817=LINE('',#275518,#30044);
#24818=LINE('',#275521,#30045);
#24819=LINE('',#275523,#30046);
#24820=LINE('',#275524,#30047);
#24821=LINE('',#275530,#30048);
#24822=LINE('',#275533,#30049);
#24823=LINE('',#275535,#30050);
#24824=LINE('',#275536,#30051);
#24825=LINE('',#275542,#30052);
#24826=LINE('',#275545,#30053);
#24827=LINE('',#275547,#30054);
#24828=LINE('',#275548,#30055);
#24829=LINE('',#275554,#30056);
#24830=LINE('',#275557,#30057);
#24831=LINE('',#275559,#30058);
#24832=LINE('',#275560,#30059);
#24833=LINE('',#275566,#30060);
#24834=LINE('',#275569,#30061);
#24835=LINE('',#275571,#30062);
#24836=LINE('',#275572,#30063);
#24837=LINE('',#275575,#30064);
#24838=LINE('',#275577,#30065);
#24839=LINE('',#275578,#30066);
#24840=LINE('',#275581,#30067);
#24841=LINE('',#275583,#30068);
#24842=LINE('',#275584,#30069);
#24843=LINE('',#275587,#30070);
#24844=LINE('',#275589,#30071);
#24845=LINE('',#275590,#30072);
#24846=LINE('',#275596,#30073);
#24847=LINE('',#275599,#30074);
#24848=LINE('',#275601,#30075);
#24849=LINE('',#275602,#30076);
#24850=LINE('',#275608,#30077);
#24851=LINE('',#275611,#30078);
#24852=LINE('',#275613,#30079);
#24853=LINE('',#275614,#30080);
#24854=LINE('',#275620,#30081);
#24855=LINE('',#275623,#30082);
#24856=LINE('',#275625,#30083);
#24857=LINE('',#275626,#30084);
#24858=LINE('',#275632,#30085);
#24859=LINE('',#275635,#30086);
#24860=LINE('',#275637,#30087);
#24861=LINE('',#275638,#30088);
#24862=LINE('',#275641,#30089);
#24863=LINE('',#275643,#30090);
#24864=LINE('',#275644,#30091);
#24865=LINE('',#275647,#30092);
#24866=LINE('',#275649,#30093);
#24867=LINE('',#275650,#30094);
#24868=LINE('',#275653,#30095);
#24869=LINE('',#275655,#30096);
#24870=LINE('',#275656,#30097);
#24871=LINE('',#275662,#30098);
#24872=LINE('',#275665,#30099);
#24873=LINE('',#275667,#30100);
#24874=LINE('',#275668,#30101);
#24875=LINE('',#275671,#30102);
#24876=LINE('',#275673,#30103);
#24877=LINE('',#275674,#30104);
#24878=LINE('',#275677,#30105);
#24879=LINE('',#275679,#30106);
#24880=LINE('',#275680,#30107);
#24881=LINE('',#275683,#30108);
#24882=LINE('',#275685,#30109);
#24883=LINE('',#275686,#30110);
#24884=LINE('',#275692,#30111);
#24885=LINE('',#275695,#30112);
#24886=LINE('',#275697,#30113);
#24887=LINE('',#275698,#30114);
#24888=LINE('',#275704,#30115);
#24889=LINE('',#275707,#30116);
#24890=LINE('',#275709,#30117);
#24891=LINE('',#275710,#30118);
#24892=LINE('',#275716,#30119);
#24893=LINE('',#275719,#30120);
#24894=LINE('',#275721,#30121);
#24895=LINE('',#275722,#30122);
#24896=LINE('',#275728,#30123);
#24897=LINE('',#275730,#30124);
#24898=LINE('',#275731,#30125);
#24899=LINE('',#275735,#30126);
#24900=LINE('',#275737,#30127);
#24901=LINE('',#275739,#30128);
#24902=LINE('',#275740,#30129);
#24903=LINE('',#275743,#30130);
#24904=LINE('',#275745,#30131);
#24905=LINE('',#275746,#30132);
#24906=LINE('',#275749,#30133);
#24907=LINE('',#275751,#30134);
#24908=LINE('',#275752,#30135);
#24909=LINE('',#275758,#30136);
#24910=LINE('',#275761,#30137);
#24911=LINE('',#275763,#30138);
#24912=LINE('',#275764,#30139);
#24913=LINE('',#275770,#30140);
#24914=LINE('',#275773,#30141);
#24915=LINE('',#275775,#30142);
#24916=LINE('',#275776,#30143);
#24917=LINE('',#275782,#30144);
#24918=LINE('',#275785,#30145);
#24919=LINE('',#275787,#30146);
#24920=LINE('',#275788,#30147);
#24921=LINE('',#275794,#30148);
#24922=LINE('',#275797,#30149);
#24923=LINE('',#275799,#30150);
#24924=LINE('',#275800,#30151);
#24925=LINE('',#275803,#30152);
#24926=LINE('',#275805,#30153);
#24927=LINE('',#275806,#30154);
#24928=LINE('',#275808,#30155);
#24929=LINE('',#275809,#30156);
#24930=LINE('',#275813,#30157);
#24931=LINE('',#275815,#30158);
#24932=LINE('',#275817,#30159);
#24933=LINE('',#275818,#30160);
#24934=LINE('',#275821,#30161);
#24935=LINE('',#275823,#30162);
#24936=LINE('',#275824,#30163);
#24937=LINE('',#275827,#30164);
#24938=LINE('',#275829,#30165);
#24939=LINE('',#275830,#30166);
#24940=LINE('',#275833,#30167);
#24941=LINE('',#275835,#30168);
#24942=LINE('',#275836,#30169);
#24943=LINE('',#275842,#30170);
#24944=LINE('',#275845,#30171);
#24945=LINE('',#275847,#30172);
#24946=LINE('',#275848,#30173);
#24947=LINE('',#275854,#30174);
#24948=LINE('',#275857,#30175);
#24949=LINE('',#275859,#30176);
#24950=LINE('',#275860,#30177);
#24951=LINE('',#275866,#30178);
#24952=LINE('',#275869,#30179);
#24953=LINE('',#275871,#30180);
#24954=LINE('',#275872,#30181);
#24955=LINE('',#275878,#30182);
#24956=LINE('',#275881,#30183);
#24957=LINE('',#275883,#30184);
#24958=LINE('',#275884,#30185);
#24959=LINE('',#275887,#30186);
#24960=LINE('',#275889,#30187);
#24961=LINE('',#275890,#30188);
#24962=LINE('',#275893,#30189);
#24963=LINE('',#275895,#30190);
#24964=LINE('',#275896,#30191);
#24965=LINE('',#275899,#30192);
#24966=LINE('',#275901,#30193);
#24967=LINE('',#275902,#30194);
#24968=LINE('',#275908,#30195);
#24969=LINE('',#275911,#30196);
#24970=LINE('',#275913,#30197);
#24971=LINE('',#275914,#30198);
#24972=LINE('',#275920,#30199);
#24973=LINE('',#275923,#30200);
#24974=LINE('',#275925,#30201);
#24975=LINE('',#275926,#30202);
#24976=LINE('',#275932,#30203);
#24977=LINE('',#275935,#30204);
#24978=LINE('',#275937,#30205);
#24979=LINE('',#275938,#30206);
#24980=LINE('',#275944,#30207);
#24981=LINE('',#275947,#30208);
#24982=LINE('',#275949,#30209);
#24983=LINE('',#275950,#30210);
#24984=LINE('',#275953,#30211);
#24985=LINE('',#275955,#30212);
#24986=LINE('',#275956,#30213);
#24987=LINE('',#275959,#30214);
#24988=LINE('',#275961,#30215);
#24989=LINE('',#275962,#30216);
#24990=LINE('',#275965,#30217);
#24991=LINE('',#275967,#30218);
#24992=LINE('',#275968,#30219);
#24993=LINE('',#275974,#30220);
#24994=LINE('',#275977,#30221);
#24995=LINE('',#275979,#30222);
#24996=LINE('',#275980,#30223);
#24997=LINE('',#275983,#30224);
#24998=LINE('',#275985,#30225);
#24999=LINE('',#275986,#30226);
#25000=LINE('',#275989,#30227);
#25001=LINE('',#275991,#30228);
#25002=LINE('',#275992,#30229);
#25003=LINE('',#275995,#30230);
#25004=LINE('',#275997,#30231);
#25005=LINE('',#275998,#30232);
#25006=LINE('',#276004,#30233);
#25007=LINE('',#276007,#30234);
#25008=LINE('',#276009,#30235);
#25009=LINE('',#276010,#30236);
#25010=LINE('',#276016,#30237);
#25011=LINE('',#276019,#30238);
#25012=LINE('',#276021,#30239);
#25013=LINE('',#276022,#30240);
#25014=LINE('',#276028,#30241);
#25015=LINE('',#276031,#30242);
#25016=LINE('',#276033,#30243);
#25017=LINE('',#276034,#30244);
#25018=LINE('',#276040,#30245);
#25019=LINE('',#276042,#30246);
#25020=LINE('',#276043,#30247);
#25021=LINE('',#276047,#30248);
#25022=LINE('',#276049,#30249);
#25023=LINE('',#276051,#30250);
#25024=LINE('',#276052,#30251);
#25025=LINE('',#276055,#30252);
#25026=LINE('',#276057,#30253);
#25027=LINE('',#276058,#30254);
#25028=LINE('',#276061,#30255);
#25029=LINE('',#276063,#30256);
#25030=LINE('',#276064,#30257);
#25031=LINE('',#276070,#30258);
#25032=LINE('',#276073,#30259);
#25033=LINE('',#276075,#30260);
#25034=LINE('',#276076,#30261);
#25035=LINE('',#276082,#30262);
#25036=LINE('',#276085,#30263);
#25037=LINE('',#276087,#30264);
#25038=LINE('',#276088,#30265);
#25039=LINE('',#276094,#30266);
#25040=LINE('',#276097,#30267);
#25041=LINE('',#276099,#30268);
#25042=LINE('',#276100,#30269);
#25043=LINE('',#276106,#30270);
#25044=LINE('',#276109,#30271);
#25045=LINE('',#276111,#30272);
#25046=LINE('',#276112,#30273);
#25047=LINE('',#276115,#30274);
#25048=LINE('',#276117,#30275);
#25049=LINE('',#276118,#30276);
#25050=LINE('',#276120,#30277);
#25051=LINE('',#276121,#30278);
#25052=LINE('',#276124,#30279);
#25053=LINE('',#276126,#30280);
#25054=LINE('',#276127,#30281);
#25055=LINE('',#276130,#30282);
#25056=LINE('',#276132,#30283);
#25057=LINE('',#276133,#30284);
#25058=LINE('',#276136,#30285);
#25059=LINE('',#276138,#30286);
#25060=LINE('',#276139,#30287);
#25061=LINE('',#276145,#30288);
#25062=LINE('',#276148,#30289);
#25063=LINE('',#276150,#30290);
#25064=LINE('',#276151,#30291);
#25065=LINE('',#276157,#30292);
#25066=LINE('',#276160,#30293);
#25067=LINE('',#276162,#30294);
#25068=LINE('',#276163,#30295);
#25069=LINE('',#276169,#30296);
#25070=LINE('',#276172,#30297);
#25071=LINE('',#276174,#30298);
#25072=LINE('',#276175,#30299);
#25073=LINE('',#276181,#30300);
#25074=LINE('',#276184,#30301);
#25075=LINE('',#276186,#30302);
#25076=LINE('',#276187,#30303);
#25077=LINE('',#276190,#30304);
#25078=LINE('',#276192,#30305);
#25079=LINE('',#276193,#30306);
#25080=LINE('',#276196,#30307);
#25081=LINE('',#276198,#30308);
#25082=LINE('',#276199,#30309);
#25083=LINE('',#276202,#30310);
#25084=LINE('',#276204,#30311);
#25085=LINE('',#276205,#30312);
#25086=LINE('',#276211,#30313);
#25087=LINE('',#276214,#30314);
#25088=LINE('',#276216,#30315);
#25089=LINE('',#276217,#30316);
#25090=LINE('',#276223,#30317);
#25091=LINE('',#276226,#30318);
#25092=LINE('',#276228,#30319);
#25093=LINE('',#276229,#30320);
#25094=LINE('',#276235,#30321);
#25095=LINE('',#276238,#30322);
#25096=LINE('',#276240,#30323);
#25097=LINE('',#276241,#30324);
#25098=LINE('',#276247,#30325);
#25099=LINE('',#276250,#30326);
#25100=LINE('',#276252,#30327);
#25101=LINE('',#276253,#30328);
#25102=LINE('',#276256,#30329);
#25103=LINE('',#276258,#30330);
#25104=LINE('',#276259,#30331);
#25105=LINE('',#276262,#30332);
#25106=LINE('',#276264,#30333);
#25107=LINE('',#276265,#30334);
#25108=LINE('',#276268,#30335);
#25109=LINE('',#276270,#30336);
#25110=LINE('',#276271,#30337);
#25111=LINE('',#276277,#30338);
#25112=LINE('',#276280,#30339);
#25113=LINE('',#276282,#30340);
#25114=LINE('',#276283,#30341);
#25115=LINE('',#276286,#30342);
#25116=LINE('',#276288,#30343);
#25117=LINE('',#276289,#30344);
#25118=LINE('',#276292,#30345);
#25119=LINE('',#276294,#30346);
#25120=LINE('',#276295,#30347);
#25121=LINE('',#276298,#30348);
#25122=LINE('',#276300,#30349);
#25123=LINE('',#276301,#30350);
#25124=LINE('',#276307,#30351);
#25125=LINE('',#276310,#30352);
#25126=LINE('',#276312,#30353);
#25127=LINE('',#276313,#30354);
#25128=LINE('',#276319,#30355);
#25129=LINE('',#276322,#30356);
#25130=LINE('',#276324,#30357);
#25131=LINE('',#276325,#30358);
#25132=LINE('',#276331,#30359);
#25133=LINE('',#276334,#30360);
#25134=LINE('',#276336,#30361);
#25135=LINE('',#276337,#30362);
#25136=LINE('',#276343,#30363);
#25137=LINE('',#276345,#30364);
#25138=LINE('',#276346,#30365);
#25139=LINE('',#276349,#30366);
#25140=LINE('',#276351,#30367);
#25141=LINE('',#276352,#30368);
#25142=LINE('',#276354,#30369);
#25143=LINE('',#276355,#30370);
#25144=LINE('',#276358,#30371);
#25145=LINE('',#276360,#30372);
#25146=LINE('',#276361,#30373);
#25147=LINE('',#276363,#30374);
#25148=LINE('',#276364,#30375);
#25149=LINE('',#276368,#30376);
#25150=LINE('',#276370,#30377);
#25151=LINE('',#276372,#30378);
#25152=LINE('',#276374,#30379);
#25153=LINE('',#276376,#30380);
#25154=LINE('',#276378,#30381);
#25155=LINE('',#276380,#30382);
#25156=LINE('',#276381,#30383);
#25157=LINE('',#276385,#30384);
#25158=LINE('',#276386,#30385);
#25159=LINE('',#276387,#30386);
#25160=LINE('',#276390,#30387);
#25161=LINE('',#276391,#30388);
#25162=LINE('',#276394,#30389);
#25163=LINE('',#276395,#30390);
#25164=LINE('',#276398,#30391);
#25165=LINE('',#276399,#30392);
#25166=LINE('',#276402,#30393);
#25167=LINE('',#276403,#30394);
#25168=LINE('',#276406,#30395);
#25169=LINE('',#276407,#30396);
#25170=LINE('',#276410,#30397);
#25171=LINE('',#276411,#30398);
#25172=LINE('',#276413,#30399);
#25173=LINE('',#276418,#30400);
#25174=LINE('',#276420,#30401);
#25175=LINE('',#276422,#30402);
#25176=LINE('',#276423,#30403);
#25177=LINE('',#276426,#30404);
#25178=LINE('',#276428,#30405);
#25179=LINE('',#276429,#30406);
#25180=LINE('',#276432,#30407);
#25181=LINE('',#276434,#30408);
#25182=LINE('',#276435,#30409);
#25183=LINE('',#276437,#30410);
#25184=LINE('',#276438,#30411);
#25185=VECTOR('',#111681,8.4455);
#25186=VECTOR('',#111688,8.4455);
#25187=VECTOR('',#111695,8.4455);
#25188=VECTOR('',#111702,8.4455);
#25189=VECTOR('',#111707,1000.);
#25190=VECTOR('',#111708,1000.);
#25191=VECTOR('',#111709,1000.);
#25192=VECTOR('',#111710,1000.);
#25193=VECTOR('',#111713,1000.);
#25194=VECTOR('',#111714,1000.);
#25195=VECTOR('',#111715,1000.);
#25196=VECTOR('',#111718,1000.);
#25197=VECTOR('',#111719,1000.);
#25198=VECTOR('',#111720,1000.);
#25199=VECTOR('',#111723,1000.);
#25200=VECTOR('',#111724,1000.);
#25201=VECTOR('',#111727,1000.);
#25202=VECTOR('',#111728,1000.);
#25203=VECTOR('',#111729,1000.);
#25204=VECTOR('',#111730,1000.);
#25205=VECTOR('',#111733,1000.);
#25206=VECTOR('',#111734,1000.);
#25207=VECTOR('',#111735,1000.);
#25208=VECTOR('',#111738,1000.);
#25209=VECTOR('',#111739,1000.);
#25210=VECTOR('',#111742,1000.);
#25211=VECTOR('',#111743,1000.);
#25212=VECTOR('',#111746,1000.);
#25213=VECTOR('',#111749,1000.);
#25214=VECTOR('',#111750,1000.);
#25215=VECTOR('',#111751,1000.);
#25216=VECTOR('',#111754,1000.);
#25217=VECTOR('',#111755,1000.);
#25218=VECTOR('',#111758,1000.);
#25219=VECTOR('',#111759,1000.);
#25220=VECTOR('',#111762,1000.);
#25221=VECTOR('',#111765,1000.);
#25222=VECTOR('',#111766,1000.);
#25223=VECTOR('',#111767,1000.);
#25224=VECTOR('',#111770,1000.);
#25225=VECTOR('',#111771,1000.);
#25226=VECTOR('',#111774,1000.);
#25227=VECTOR('',#111775,1000.);
#25228=VECTOR('',#111778,1000.);
#25229=VECTOR('',#111781,1000.);
#25230=VECTOR('',#111782,1000.);
#25231=VECTOR('',#111783,1000.);
#25232=VECTOR('',#111786,1000.);
#25233=VECTOR('',#111787,1000.);
#25234=VECTOR('',#111790,1000.);
#25235=VECTOR('',#111791,1000.);
#25236=VECTOR('',#111794,1000.);
#25237=VECTOR('',#111797,1000.);
#25238=VECTOR('',#111800,1000.);
#25239=VECTOR('',#111803,1000.);
#25240=VECTOR('',#111806,1000.);
#25241=VECTOR('',#111811,1000.);
#25242=VECTOR('',#111814,1000.);
#25243=VECTOR('',#111817,1000.);
#25244=VECTOR('',#111820,1000.);
#25245=VECTOR('',#111825,1000.);
#25246=VECTOR('',#111826,1000.);
#25247=VECTOR('',#111827,1000.);
#25248=VECTOR('',#111830,1000.);
#25249=VECTOR('',#111831,1000.);
#25250=VECTOR('',#111832,1000.);
#25251=VECTOR('',#111835,1000.);
#25252=VECTOR('',#111836,1000.);
#25253=VECTOR('',#111837,1000.);
#25254=VECTOR('',#111840,1000.);
#25255=VECTOR('',#111841,1000.);
#25256=VECTOR('',#111842,1000.);
#25257=VECTOR('',#111915,5.15937500000002);
#25258=VECTOR('',#111918,5.15937500000002);
#25259=VECTOR('',#111921,5.15937500000008);
#25260=VECTOR('',#111924,5.15937500000008);
#25261=VECTOR('',#111929,11.3170000000002);
#25262=VECTOR('',#111930,11.3170000000002);
#25263=VECTOR('',#111933,9.00000000000018);
#25264=VECTOR('',#111934,9.00000000000018);
#25265=VECTOR('',#111943,18.0480000000001);
#25266=VECTOR('',#111944,10.);
#25267=VECTOR('',#111947,18.0480000000001);
#25268=VECTOR('',#111950,18.0480000000001);
#25269=VECTOR('',#111953,18.0480000000001);
#25270=VECTOR('',#111956,18.0480000000001);
#25271=VECTOR('',#111959,18.0480000000001);
#25272=VECTOR('',#111962,18.0480000000001);
#25273=VECTOR('',#111965,18.0480000000001);
#25274=VECTOR('',#111968,15.);
#25275=VECTOR('',#111971,10.);
#25276=VECTOR('',#111972,15.);
#25277=VECTOR('',#111975,15.);
#25278=VECTOR('',#111978,15.);
#25279=VECTOR('',#111981,15.);
#25280=VECTOR('',#111984,15.);
#25281=VECTOR('',#111987,15.);
#25282=VECTOR('',#111990,15.);
#25283=VECTOR('',#111993,15.);
#25284=VECTOR('',#111996,39.);
#25285=VECTOR('',#112001,39.);
#25286=VECTOR('',#112004,39.);
#25287=VECTOR('',#112007,39.);
#25288=VECTOR('',#112010,39.);
#25289=VECTOR('',#112013,39.);
#25290=VECTOR('',#112016,39.);
#25291=VECTOR('',#112019,39.);
#25292=VECTOR('',#112022,5.15937500000002);
#25293=VECTOR('',#112025,5.15937500000002);
#25294=VECTOR('',#112028,5.15937500000008);
#25295=VECTOR('',#112031,5.15937500000008);
#25296=VECTOR('',#112034,1000.);
#25297=VECTOR('',#112043,11.444);
#25298=VECTOR('',#112044,11.444);
#25299=VECTOR('',#112049,10.);
#25300=VECTOR('',#112050,10.);
#25301=VECTOR('',#112051,10.);
#25302=VECTOR('',#112052,10.);
#25303=VECTOR('',#112053,10.);
#25304=VECTOR('',#112056,10.);
#25305=VECTOR('',#112081,1000.);
#25306=VECTOR('',#112082,1000.);
#25307=VECTOR('',#112091,5.1435);
#25308=VECTOR('',#112108,3.78554799125932);
#25309=VECTOR('',#112127,2.40973730802039);
#25310=VECTOR('',#112142,0.952499999999998);
#25311=VECTOR('',#112185,1000.);
#25312=VECTOR('',#112188,1000.);
#25313=VECTOR('',#112189,1000.);
#25314=VECTOR('',#112192,1000.);
#25315=VECTOR('',#112193,1000.);
#25316=VECTOR('',#112196,1000.);
#25317=VECTOR('',#112197,1000.);
#25318=VECTOR('',#112200,1000.);
#25319=VECTOR('',#112201,1000.);
#25320=VECTOR('',#112204,1000.);
#25321=VECTOR('',#112219,7.9375);
#25322=VECTOR('',#112226,8.4455);
#25323=VECTOR('',#112237,7.9375);
#25324=VECTOR('',#112244,8.4455);
#25325=VECTOR('',#112255,7.9375);
#25326=VECTOR('',#112262,8.4455);
#25327=VECTOR('',#112273,7.9375);
#25328=VECTOR('',#112280,8.4455);
#25329=VECTOR('',#112311,51.27);
#25330=VECTOR('',#112314,50.);
#25331=VECTOR('',#112345,56.875);
#25332=VECTOR('',#112348,55.605);
#25333=VECTOR('',#112359,51.27);
#25334=VECTOR('',#112366,55.605);
#25335=VECTOR('',#112455,65.);
#25336=VECTOR('',#112460,64.008019903844);
#25337=VECTOR('',#112465,10.);
#25338=VECTOR('',#112468,10.);
#25339=VECTOR('',#112471,10.);
#25340=VECTOR('',#112474,10.);
#25341=VECTOR('',#112477,10.);
#25342=VECTOR('',#112480,10.);
#25343=VECTOR('',#112483,10.);
#25344=VECTOR('',#112486,10.);
#25345=VECTOR('',#112489,10.);
#25346=VECTOR('',#112492,10.);
#25347=VECTOR('',#112495,10.);
#25348=VECTOR('',#112498,10.);
#25349=VECTOR('',#112501,10.);
#25350=VECTOR('',#112504,10.);
#25351=VECTOR('',#112507,10.);
#25352=VECTOR('',#112510,10.);
#25353=VECTOR('',#112513,10.);
#25354=VECTOR('',#112516,10.);
#25355=VECTOR('',#112519,10.);
#25356=VECTOR('',#112522,10.);
#25357=VECTOR('',#112525,10.);
#25358=VECTOR('',#112528,10.);
#25359=VECTOR('',#112531,10.);
#25360=VECTOR('',#112534,10.);
#25361=VECTOR('',#112537,10.);
#25362=VECTOR('',#112540,10.);
#25363=VECTOR('',#112543,10.);
#25364=VECTOR('',#112546,10.);
#25365=VECTOR('',#112549,10.);
#25366=VECTOR('',#112552,10.);
#25367=VECTOR('',#112555,10.);
#25368=VECTOR('',#112558,10.);
#25369=VECTOR('',#112561,10.);
#25370=VECTOR('',#112564,10.);
#25371=VECTOR('',#112567,10.);
#25372=VECTOR('',#112570,10.);
#25373=VECTOR('',#112573,10.);
#25374=VECTOR('',#112576,10.);
#25375=VECTOR('',#112579,10.);
#25376=VECTOR('',#112582,10.);
#25377=VECTOR('',#112585,10.);
#25378=VECTOR('',#112588,10.);
#25379=VECTOR('',#112591,10.);
#25380=VECTOR('',#112594,10.);
#25381=VECTOR('',#112597,10.);
#25382=VECTOR('',#112600,10.);
#25383=VECTOR('',#112603,10.);
#25384=VECTOR('',#112606,10.);
#25385=VECTOR('',#112609,10.);
#25386=VECTOR('',#112612,10.);
#25387=VECTOR('',#112615,10.);
#25388=VECTOR('',#112618,10.);
#25389=VECTOR('',#112621,10.);
#25390=VECTOR('',#112624,10.);
#25391=VECTOR('',#112627,10.);
#25392=VECTOR('',#112630,10.);
#25393=VECTOR('',#112633,10.);
#25394=VECTOR('',#112636,10.);
#25395=VECTOR('',#112639,10.);
#25396=VECTOR('',#112642,10.);
#25397=VECTOR('',#112643,62.2224557307631);
#25398=VECTOR('',#112644,10.);
#25399=VECTOR('',#112647,10.);
#25400=VECTOR('',#112650,10.);
#25401=VECTOR('',#112653,10.);
#25402=VECTOR('',#112656,10.);
#25403=VECTOR('',#112659,10.);
#25404=VECTOR('',#112662,10.);
#25405=VECTOR('',#112665,10.);
#25406=VECTOR('',#112668,10.);
#25407=VECTOR('',#112671,10.);
#25408=VECTOR('',#112674,10.);
#25409=VECTOR('',#112677,10.);
#25410=VECTOR('',#112680,10.);
#25411=VECTOR('',#112683,10.);
#25412=VECTOR('',#112686,10.);
#25413=VECTOR('',#112689,10.);
#25414=VECTOR('',#112692,10.);
#25415=VECTOR('',#112695,10.);
#25416=VECTOR('',#112698,10.);
#25417=VECTOR('',#112701,10.);
#25418=VECTOR('',#112704,10.);
#25419=VECTOR('',#112707,10.);
#25420=VECTOR('',#112710,10.);
#25421=VECTOR('',#112713,10.);
#25422=VECTOR('',#112716,10.);
#25423=VECTOR('',#112719,10.);
#25424=VECTOR('',#112722,10.);
#25425=VECTOR('',#112725,10.);
#25426=VECTOR('',#112728,10.);
#25427=VECTOR('',#112731,10.);
#25428=VECTOR('',#112732,10.);
#25429=VECTOR('',#112735,10.);
#25430=VECTOR('',#112738,10.);
#25431=VECTOR('',#112741,10.);
#25432=VECTOR('',#112744,10.);
#25433=VECTOR('',#112747,10.);
#25434=VECTOR('',#112750,10.);
#25435=VECTOR('',#112753,10.);
#25436=VECTOR('',#112756,10.);
#25437=VECTOR('',#112759,10.);
#25438=VECTOR('',#112762,10.);
#25439=VECTOR('',#112765,10.);
#25440=VECTOR('',#112768,10.);
#25441=VECTOR('',#112771,10.);
#25442=VECTOR('',#112774,10.);
#25443=VECTOR('',#112777,10.);
#25444=VECTOR('',#112780,10.);
#25445=VECTOR('',#112783,10.);
#25446=VECTOR('',#112786,10.);
#25447=VECTOR('',#112789,10.);
#25448=VECTOR('',#112792,10.);
#25449=VECTOR('',#112795,10.);
#25450=VECTOR('',#112798,10.);
#25451=VECTOR('',#112801,10.);
#25452=VECTOR('',#112804,10.);
#25453=VECTOR('',#112807,10.);
#25454=VECTOR('',#112810,10.);
#25455=VECTOR('',#112813,10.);
#25456=VECTOR('',#112816,10.);
#25457=VECTOR('',#112819,10.);
#25458=VECTOR('',#112822,10.);
#25459=VECTOR('',#112825,10.);
#25460=VECTOR('',#112828,10.);
#25461=VECTOR('',#112831,10.);
#25462=VECTOR('',#112834,10.);
#25463=VECTOR('',#112837,10.);
#25464=VECTOR('',#112840,10.);
#25465=VECTOR('',#112843,10.);
#25466=VECTOR('',#112846,10.);
#25467=VECTOR('',#112849,10.);
#25468=VECTOR('',#112852,10.);
#25469=VECTOR('',#112855,10.);
#25470=VECTOR('',#112858,10.);
#25471=VECTOR('',#112861,10.);
#25472=VECTOR('',#112864,10.);
#25473=VECTOR('',#112867,10.);
#25474=VECTOR('',#112870,10.);
#25475=VECTOR('',#112873,10.);
#25476=VECTOR('',#112876,10.);
#25477=VECTOR('',#112879,10.);
#25478=VECTOR('',#112882,10.);
#25479=VECTOR('',#112885,10.);
#25480=VECTOR('',#112888,10.);
#25481=VECTOR('',#112891,10.);
#25482=VECTOR('',#112894,10.);
#25483=VECTOR('',#112897,10.);
#25484=VECTOR('',#112900,10.);
#25485=VECTOR('',#112903,10.);
#25486=VECTOR('',#112906,10.);
#25487=VECTOR('',#112909,10.);
#25488=VECTOR('',#112912,10.);
#25489=VECTOR('',#112915,10.);
#25490=VECTOR('',#112918,10.);
#25491=VECTOR('',#112921,10.);
#25492=VECTOR('',#112924,10.);
#25493=VECTOR('',#112927,10.);
#25494=VECTOR('',#112930,10.);
#25495=VECTOR('',#112933,10.);
#25496=VECTOR('',#112936,10.);
#25497=VECTOR('',#112939,10.);
#25498=VECTOR('',#112942,10.);
#25499=VECTOR('',#112945,10.);
#25500=VECTOR('',#112948,10.);
#25501=VECTOR('',#112951,10.);
#25502=VECTOR('',#112954,10.);
#25503=VECTOR('',#112957,10.);
#25504=VECTOR('',#112960,10.);
#25505=VECTOR('',#112963,10.);
#25506=VECTOR('',#112966,10.);
#25507=VECTOR('',#112969,10.);
#25508=VECTOR('',#112972,10.);
#25509=VECTOR('',#112975,10.);
#25510=VECTOR('',#112978,10.);
#25511=VECTOR('',#112981,10.);
#25512=VECTOR('',#112984,10.);
#25513=VECTOR('',#112987,10.);
#25514=VECTOR('',#112990,10.);
#25515=VECTOR('',#112993,10.);
#25516=VECTOR('',#112996,10.);
#25517=VECTOR('',#112999,10.);
#25518=VECTOR('',#113002,58.6605641730809);
#25519=VECTOR('',#113005,10.);
#25520=VECTOR('',#113008,10.);
#25521=VECTOR('',#113011,10.);
#25522=VECTOR('',#113014,10.);
#25523=VECTOR('',#113017,10.);
#25524=VECTOR('',#113020,10.);
#25525=VECTOR('',#113023,10.);
#25526=VECTOR('',#113026,10.);
#25527=VECTOR('',#113029,10.);
#25528=VECTOR('',#113032,10.);
#25529=VECTOR('',#113035,10.);
#25530=VECTOR('',#113038,10.);
#25531=VECTOR('',#113041,10.);
#25532=VECTOR('',#113044,10.);
#25533=VECTOR('',#113047,10.);
#25534=VECTOR('',#113050,10.);
#25535=VECTOR('',#113053,10.);
#25536=VECTOR('',#113056,10.);
#25537=VECTOR('',#113059,10.);
#25538=VECTOR('',#113062,10.);
#25539=VECTOR('',#113065,10.);
#25540=VECTOR('',#113068,10.);
#25541=VECTOR('',#113071,10.);
#25542=VECTOR('',#113074,10.);
#25543=VECTOR('',#113077,10.);
#25544=VECTOR('',#113080,10.);
#25545=VECTOR('',#113083,10.);
#25546=VECTOR('',#113086,10.);
#25547=VECTOR('',#113089,10.);
#25548=VECTOR('',#113092,10.);
#25549=VECTOR('',#113093,10.);
#25550=VECTOR('',#113096,10.);
#25551=VECTOR('',#113099,10.);
#25552=VECTOR('',#113102,10.);
#25553=VECTOR('',#113105,10.);
#25554=VECTOR('',#113108,10.);
#25555=VECTOR('',#113111,10.);
#25556=VECTOR('',#113114,10.);
#25557=VECTOR('',#113117,10.);
#25558=VECTOR('',#113120,10.);
#25559=VECTOR('',#113123,10.);
#25560=VECTOR('',#113126,10.);
#25561=VECTOR('',#113129,10.);
#25562=VECTOR('',#113132,10.);
#25563=VECTOR('',#113135,10.);
#25564=VECTOR('',#113138,10.);
#25565=VECTOR('',#113141,10.);
#25566=VECTOR('',#113144,10.);
#25567=VECTOR('',#113147,10.);
#25568=VECTOR('',#113150,10.);
#25569=VECTOR('',#113153,10.);
#25570=VECTOR('',#113156,10.);
#25571=VECTOR('',#113159,10.);
#25572=VECTOR('',#113162,10.);
#25573=VECTOR('',#113165,10.);
#25574=VECTOR('',#113168,10.);
#25575=VECTOR('',#113171,10.);
#25576=VECTOR('',#113174,10.);
#25577=VECTOR('',#113177,10.);
#25578=VECTOR('',#113180,10.);
#25579=VECTOR('',#113185,56.875);
#25580=VECTOR('',#113190,56.875);
#25581=VECTOR('',#113197,1000.);
#25582=VECTOR('',#113200,1000.);
#25583=VECTOR('',#113209,10.);
#25584=VECTOR('',#113210,10.);
#25585=VECTOR('',#113215,1000.);
#25586=VECTOR('',#113218,1000.);
#25587=VECTOR('',#113223,10.);
#25588=VECTOR('',#113226,10.);
#25589=VECTOR('',#113235,1000.);
#25590=VECTOR('',#113236,1000.);
#25591=VECTOR('',#113265,1000.);
#25592=VECTOR('',#113272,1000.);
#25593=VECTOR('',#113275,10.);
#25594=VECTOR('',#113278,10.);
#25595=VECTOR('',#113283,1000.);
#25596=VECTOR('',#113286,1000.);
#25597=VECTOR('',#113291,10.);
#25598=VECTOR('',#113298,10.);
#25599=VECTOR('',#113301,1000.);
#25600=VECTOR('',#113304,1000.);
#25601=VECTOR('',#113333,1000.);
#25602=VECTOR('',#113340,1000.);
#25603=VECTOR('',#113343,10.);
#25604=VECTOR('',#113346,10.);
#25605=VECTOR('',#113351,1000.);
#25606=VECTOR('',#113354,1000.);
#25607=VECTOR('',#113359,10.);
#25608=VECTOR('',#113366,10.);
#25609=VECTOR('',#113369,1000.);
#25610=VECTOR('',#113372,1000.);
#25611=VECTOR('',#113401,1000.);
#25612=VECTOR('',#113408,1000.);
#25613=VECTOR('',#113411,10.);
#25614=VECTOR('',#113414,10.);
#25615=VECTOR('',#113419,1000.);
#25616=VECTOR('',#113422,1000.);
#25617=VECTOR('',#113427,10.);
#25618=VECTOR('',#113434,10.);
#25619=VECTOR('',#113437,1000.);
#25620=VECTOR('',#113440,1000.);
#25621=VECTOR('',#113469,1000.);
#25622=VECTOR('',#113476,1000.);
#25623=VECTOR('',#113479,10.);
#25624=VECTOR('',#113482,10.);
#25625=VECTOR('',#113487,1000.);
#25626=VECTOR('',#113490,1000.);
#25627=VECTOR('',#113495,10.);
#25628=VECTOR('',#113502,10.);
#25629=VECTOR('',#113505,1000.);
#25630=VECTOR('',#113508,1000.);
#25631=VECTOR('',#113537,1000.);
#25632=VECTOR('',#113544,1000.);
#25633=VECTOR('',#113547,10.);
#25634=VECTOR('',#113550,10.);
#25635=VECTOR('',#113555,1000.);
#25636=VECTOR('',#113558,1000.);
#25637=VECTOR('',#113563,10.);
#25638=VECTOR('',#113570,10.);
#25639=VECTOR('',#113573,1000.);
#25640=VECTOR('',#113576,1000.);
#25641=VECTOR('',#113605,1000.);
#25642=VECTOR('',#113612,1000.);
#25643=VECTOR('',#113615,10.);
#25644=VECTOR('',#113618,10.);
#25645=VECTOR('',#113623,1000.);
#25646=VECTOR('',#113626,1000.);
#25647=VECTOR('',#113631,10.);
#25648=VECTOR('',#113638,10.);
#25649=VECTOR('',#113641,1000.);
#25650=VECTOR('',#113644,1000.);
#25651=VECTOR('',#113673,1000.);
#25652=VECTOR('',#113680,1000.);
#25653=VECTOR('',#113683,10.);
#25654=VECTOR('',#113686,10.);
#25655=VECTOR('',#113691,1000.);
#25656=VECTOR('',#113694,1000.);
#25657=VECTOR('',#113699,10.);
#25658=VECTOR('',#113706,10.);
#25659=VECTOR('',#113709,1000.);
#25660=VECTOR('',#113712,1000.);
#25661=VECTOR('',#113741,1000.);
#25662=VECTOR('',#113748,1000.);
#25663=VECTOR('',#113751,10.);
#25664=VECTOR('',#113754,10.);
#25665=VECTOR('',#113759,1000.);
#25666=VECTOR('',#113762,1000.);
#25667=VECTOR('',#113767,10.);
#25668=VECTOR('',#113774,10.);
#25669=VECTOR('',#113777,1000.);
#25670=VECTOR('',#113780,1000.);
#25671=VECTOR('',#113809,1000.);
#25672=VECTOR('',#113816,1000.);
#25673=VECTOR('',#113819,10.);
#25674=VECTOR('',#113822,10.);
#25675=VECTOR('',#113827,1000.);
#25676=VECTOR('',#113830,1000.);
#25677=VECTOR('',#113835,10.);
#25678=VECTOR('',#113842,10.);
#25679=VECTOR('',#113845,1000.);
#25680=VECTOR('',#113848,1000.);
#25681=VECTOR('',#113877,1000.);
#25682=VECTOR('',#113884,1000.);
#25683=VECTOR('',#113887,10.);
#25684=VECTOR('',#113890,10.);
#25685=VECTOR('',#113895,1000.);
#25686=VECTOR('',#113898,1000.);
#25687=VECTOR('',#113903,10.);
#25688=VECTOR('',#113910,10.);
#25689=VECTOR('',#113913,1000.);
#25690=VECTOR('',#113916,1000.);
#25691=VECTOR('',#113945,1000.);
#25692=VECTOR('',#113952,1000.);
#25693=VECTOR('',#113955,10.);
#25694=VECTOR('',#113958,10.);
#25695=VECTOR('',#113963,1000.);
#25696=VECTOR('',#113966,1000.);
#25697=VECTOR('',#113971,10.);
#25698=VECTOR('',#113978,10.);
#25699=VECTOR('',#113981,1000.);
#25700=VECTOR('',#113984,1000.);
#25701=VECTOR('',#114013,1000.);
#25702=VECTOR('',#114020,1000.);
#25703=VECTOR('',#114023,10.);
#25704=VECTOR('',#114026,10.);
#25705=VECTOR('',#114031,1000.);
#25706=VECTOR('',#114034,1000.);
#25707=VECTOR('',#114039,10.);
#25708=VECTOR('',#114046,10.);
#25709=VECTOR('',#114049,1000.);
#25710=VECTOR('',#114052,1000.);
#25711=VECTOR('',#114081,1000.);
#25712=VECTOR('',#114088,1000.);
#25713=VECTOR('',#114091,10.);
#25714=VECTOR('',#114094,10.);
#25715=VECTOR('',#114099,1000.);
#25716=VECTOR('',#114102,1000.);
#25717=VECTOR('',#114107,10.);
#25718=VECTOR('',#114114,10.);
#25719=VECTOR('',#114117,1000.);
#25720=VECTOR('',#114120,1000.);
#25721=VECTOR('',#114149,1000.);
#25722=VECTOR('',#114156,1000.);
#25723=VECTOR('',#114159,10.);
#25724=VECTOR('',#114162,10.);
#25725=VECTOR('',#114167,1000.);
#25726=VECTOR('',#114170,1000.);
#25727=VECTOR('',#114175,10.);
#25728=VECTOR('',#114182,10.);
#25729=VECTOR('',#114185,1000.);
#25730=VECTOR('',#114188,1000.);
#25731=VECTOR('',#114217,1000.);
#25732=VECTOR('',#114224,1000.);
#25733=VECTOR('',#114227,10.);
#25734=VECTOR('',#114230,10.);
#25735=VECTOR('',#114235,1000.);
#25736=VECTOR('',#114238,1000.);
#25737=VECTOR('',#114243,10.);
#25738=VECTOR('',#114250,10.);
#25739=VECTOR('',#114253,1000.);
#25740=VECTOR('',#114256,1000.);
#25741=VECTOR('',#114285,1000.);
#25742=VECTOR('',#114292,1000.);
#25743=VECTOR('',#114295,10.);
#25744=VECTOR('',#114298,10.);
#25745=VECTOR('',#114303,1000.);
#25746=VECTOR('',#114306,1000.);
#25747=VECTOR('',#114311,10.);
#25748=VECTOR('',#114318,10.);
#25749=VECTOR('',#114321,1000.);
#25750=VECTOR('',#114324,1000.);
#25751=VECTOR('',#114353,1000.);
#25752=VECTOR('',#114360,1000.);
#25753=VECTOR('',#114363,10.);
#25754=VECTOR('',#114366,10.);
#25755=VECTOR('',#114371,1000.);
#25756=VECTOR('',#114374,1000.);
#25757=VECTOR('',#114379,10.);
#25758=VECTOR('',#114386,10.);
#25759=VECTOR('',#114389,1000.);
#25760=VECTOR('',#114392,1000.);
#25761=VECTOR('',#114421,1000.);
#25762=VECTOR('',#114428,1000.);
#25763=VECTOR('',#114431,10.);
#25764=VECTOR('',#114434,10.);
#25765=VECTOR('',#114439,1000.);
#25766=VECTOR('',#114442,1000.);
#25767=VECTOR('',#114447,10.);
#25768=VECTOR('',#114454,10.);
#25769=VECTOR('',#114457,1000.);
#25770=VECTOR('',#114460,1000.);
#25771=VECTOR('',#114489,1000.);
#25772=VECTOR('',#114496,1000.);
#25773=VECTOR('',#114499,10.);
#25774=VECTOR('',#114502,10.);
#25775=VECTOR('',#114507,1000.);
#25776=VECTOR('',#114510,1000.);
#25777=VECTOR('',#114515,10.);
#25778=VECTOR('',#114522,10.);
#25779=VECTOR('',#114525,1000.);
#25780=VECTOR('',#114528,1000.);
#25781=VECTOR('',#114557,1000.);
#25782=VECTOR('',#114564,1000.);
#25783=VECTOR('',#114567,10.);
#25784=VECTOR('',#114570,10.);
#25785=VECTOR('',#114575,1000.);
#25786=VECTOR('',#114578,1000.);
#25787=VECTOR('',#114583,10.);
#25788=VECTOR('',#114590,10.);
#25789=VECTOR('',#114593,1000.);
#25790=VECTOR('',#114596,1000.);
#25791=VECTOR('',#114625,1000.);
#25792=VECTOR('',#114632,1000.);
#25793=VECTOR('',#114635,10.);
#25794=VECTOR('',#114638,10.);
#25795=VECTOR('',#114643,1000.);
#25796=VECTOR('',#114646,1000.);
#25797=VECTOR('',#114651,10.);
#25798=VECTOR('',#114658,10.);
#25799=VECTOR('',#114661,1000.);
#25800=VECTOR('',#114664,1000.);
#25801=VECTOR('',#114693,1000.);
#25802=VECTOR('',#114700,1000.);
#25803=VECTOR('',#114703,10.);
#25804=VECTOR('',#114706,10.);
#25805=VECTOR('',#114711,1000.);
#25806=VECTOR('',#114714,1000.);
#25807=VECTOR('',#114719,10.);
#25808=VECTOR('',#114726,10.);
#25809=VECTOR('',#114729,1000.);
#25810=VECTOR('',#114732,1000.);
#25811=VECTOR('',#114761,1000.);
#25812=VECTOR('',#114768,1000.);
#25813=VECTOR('',#114771,10.);
#25814=VECTOR('',#114774,10.);
#25815=VECTOR('',#114779,1000.);
#25816=VECTOR('',#114782,1000.);
#25817=VECTOR('',#114787,10.);
#25818=VECTOR('',#114794,10.);
#25819=VECTOR('',#114797,1000.);
#25820=VECTOR('',#114800,1000.);
#25821=VECTOR('',#114829,1000.);
#25822=VECTOR('',#114836,1000.);
#25823=VECTOR('',#114839,10.);
#25824=VECTOR('',#114842,10.);
#25825=VECTOR('',#114847,1000.);
#25826=VECTOR('',#114850,1000.);
#25827=VECTOR('',#114855,10.);
#25828=VECTOR('',#114862,10.);
#25829=VECTOR('',#114865,1000.);
#25830=VECTOR('',#114868,1000.);
#25831=VECTOR('',#114897,1000.);
#25832=VECTOR('',#114904,1000.);
#25833=VECTOR('',#114907,10.);
#25834=VECTOR('',#114910,10.);
#25835=VECTOR('',#114915,1000.);
#25836=VECTOR('',#114918,1000.);
#25837=VECTOR('',#114923,10.);
#25838=VECTOR('',#114930,10.);
#25839=VECTOR('',#114933,1000.);
#25840=VECTOR('',#114936,1000.);
#25841=VECTOR('',#114965,1000.);
#25842=VECTOR('',#114972,1000.);
#25843=VECTOR('',#114975,10.);
#25844=VECTOR('',#114978,10.);
#25845=VECTOR('',#114983,1000.);
#25846=VECTOR('',#114986,1000.);
#25847=VECTOR('',#114991,10.);
#25848=VECTOR('',#114998,10.);
#25849=VECTOR('',#115001,1000.);
#25850=VECTOR('',#115004,1000.);
#25851=VECTOR('',#115033,1000.);
#25852=VECTOR('',#115040,1000.);
#25853=VECTOR('',#115043,10.);
#25854=VECTOR('',#115046,10.);
#25855=VECTOR('',#115051,1000.);
#25856=VECTOR('',#115054,1000.);
#25857=VECTOR('',#115059,10.);
#25858=VECTOR('',#115066,10.);
#25859=VECTOR('',#115069,1000.);
#25860=VECTOR('',#115072,1000.);
#25861=VECTOR('',#115101,1000.);
#25862=VECTOR('',#115108,1000.);
#25863=VECTOR('',#115111,10.);
#25864=VECTOR('',#115114,10.);
#25865=VECTOR('',#115119,1000.);
#25866=VECTOR('',#115122,1000.);
#25867=VECTOR('',#115127,10.);
#25868=VECTOR('',#115134,10.);
#25869=VECTOR('',#115137,1000.);
#25870=VECTOR('',#115140,1000.);
#25871=VECTOR('',#115169,1000.);
#25872=VECTOR('',#115176,1000.);
#25873=VECTOR('',#115179,10.);
#25874=VECTOR('',#115182,10.);
#25875=VECTOR('',#115187,1000.);
#25876=VECTOR('',#115190,1000.);
#25877=VECTOR('',#115195,10.);
#25878=VECTOR('',#115202,10.);
#25879=VECTOR('',#115205,1000.);
#25880=VECTOR('',#115208,1000.);
#25881=VECTOR('',#115237,1000.);
#25882=VECTOR('',#115244,1000.);
#25883=VECTOR('',#115247,10.);
#25884=VECTOR('',#115250,10.);
#25885=VECTOR('',#115255,1000.);
#25886=VECTOR('',#115258,1000.);
#25887=VECTOR('',#115263,10.);
#25888=VECTOR('',#115270,10.);
#25889=VECTOR('',#115273,1000.);
#25890=VECTOR('',#115276,1000.);
#25891=VECTOR('',#115305,1000.);
#25892=VECTOR('',#115312,1000.);
#25893=VECTOR('',#115315,10.);
#25894=VECTOR('',#115318,10.);
#25895=VECTOR('',#115323,1000.);
#25896=VECTOR('',#115326,1000.);
#25897=VECTOR('',#115331,10.);
#25898=VECTOR('',#115338,10.);
#25899=VECTOR('',#115341,1000.);
#25900=VECTOR('',#115344,1000.);
#25901=VECTOR('',#115373,1000.);
#25902=VECTOR('',#115380,1000.);
#25903=VECTOR('',#115383,10.);
#25904=VECTOR('',#115386,10.);
#25905=VECTOR('',#115391,1000.);
#25906=VECTOR('',#115394,1000.);
#25907=VECTOR('',#115399,10.);
#25908=VECTOR('',#115406,10.);
#25909=VECTOR('',#115409,1000.);
#25910=VECTOR('',#115412,1000.);
#25911=VECTOR('',#115441,1000.);
#25912=VECTOR('',#115448,1000.);
#25913=VECTOR('',#115451,10.);
#25914=VECTOR('',#115454,10.);
#25915=VECTOR('',#115459,1000.);
#25916=VECTOR('',#115462,1000.);
#25917=VECTOR('',#115467,10.);
#25918=VECTOR('',#115474,10.);
#25919=VECTOR('',#115477,1000.);
#25920=VECTOR('',#115480,1000.);
#25921=VECTOR('',#115509,1000.);
#25922=VECTOR('',#115516,1000.);
#25923=VECTOR('',#115519,10.);
#25924=VECTOR('',#115522,10.);
#25925=VECTOR('',#115527,1000.);
#25926=VECTOR('',#115530,1000.);
#25927=VECTOR('',#115535,10.);
#25928=VECTOR('',#115542,10.);
#25929=VECTOR('',#115545,1000.);
#25930=VECTOR('',#115548,1000.);
#25931=VECTOR('',#115577,1000.);
#25932=VECTOR('',#115584,1000.);
#25933=VECTOR('',#115587,10.);
#25934=VECTOR('',#115590,10.);
#25935=VECTOR('',#115595,1000.);
#25936=VECTOR('',#115598,1000.);
#25937=VECTOR('',#115603,10.);
#25938=VECTOR('',#115610,10.);
#25939=VECTOR('',#115613,1000.);
#25940=VECTOR('',#115616,1000.);
#25941=VECTOR('',#115645,1000.);
#25942=VECTOR('',#115652,1000.);
#25943=VECTOR('',#115655,10.);
#25944=VECTOR('',#115658,10.);
#25945=VECTOR('',#115663,1000.);
#25946=VECTOR('',#115666,1000.);
#25947=VECTOR('',#115671,10.);
#25948=VECTOR('',#115678,10.);
#25949=VECTOR('',#115681,1000.);
#25950=VECTOR('',#115684,1000.);
#25951=VECTOR('',#115713,1000.);
#25952=VECTOR('',#115720,1000.);
#25953=VECTOR('',#115723,10.);
#25954=VECTOR('',#115726,10.);
#25955=VECTOR('',#115731,1000.);
#25956=VECTOR('',#115734,1000.);
#25957=VECTOR('',#115739,10.);
#25958=VECTOR('',#115746,10.);
#25959=VECTOR('',#115749,1000.);
#25960=VECTOR('',#115752,1000.);
#25961=VECTOR('',#115781,1000.);
#25962=VECTOR('',#115788,1000.);
#25963=VECTOR('',#115791,10.);
#25964=VECTOR('',#115794,10.);
#25965=VECTOR('',#115799,1000.);
#25966=VECTOR('',#115802,1000.);
#25967=VECTOR('',#115807,10.);
#25968=VECTOR('',#115814,10.);
#25969=VECTOR('',#115817,1000.);
#25970=VECTOR('',#115820,1000.);
#25971=VECTOR('',#115849,1000.);
#25972=VECTOR('',#115856,1000.);
#25973=VECTOR('',#115859,10.);
#25974=VECTOR('',#115862,10.);
#25975=VECTOR('',#115867,1000.);
#25976=VECTOR('',#115870,1000.);
#25977=VECTOR('',#115875,10.);
#25978=VECTOR('',#115882,10.);
#25979=VECTOR('',#115885,1000.);
#25980=VECTOR('',#115888,1000.);
#25981=VECTOR('',#115917,1000.);
#25982=VECTOR('',#115924,1000.);
#25983=VECTOR('',#115927,10.);
#25984=VECTOR('',#115930,10.);
#25985=VECTOR('',#115935,1000.);
#25986=VECTOR('',#115938,1000.);
#25987=VECTOR('',#115943,10.);
#25988=VECTOR('',#115950,10.);
#25989=VECTOR('',#115953,1000.);
#25990=VECTOR('',#115956,1000.);
#25991=VECTOR('',#115985,1000.);
#25992=VECTOR('',#115992,1000.);
#25993=VECTOR('',#115995,10.);
#25994=VECTOR('',#115998,10.);
#25995=VECTOR('',#116003,1000.);
#25996=VECTOR('',#116006,1000.);
#25997=VECTOR('',#116011,10.);
#25998=VECTOR('',#116018,10.);
#25999=VECTOR('',#116021,1000.);
#26000=VECTOR('',#116024,1000.);
#26001=VECTOR('',#116053,1000.);
#26002=VECTOR('',#116060,1000.);
#26003=VECTOR('',#116063,10.);
#26004=VECTOR('',#116066,10.);
#26005=VECTOR('',#116071,1000.);
#26006=VECTOR('',#116074,1000.);
#26007=VECTOR('',#116079,10.);
#26008=VECTOR('',#116086,10.);
#26009=VECTOR('',#116089,1000.);
#26010=VECTOR('',#116092,1000.);
#26011=VECTOR('',#116121,1000.);
#26012=VECTOR('',#116128,1000.);
#26013=VECTOR('',#116131,10.);
#26014=VECTOR('',#116134,10.);
#26015=VECTOR('',#116139,1000.);
#26016=VECTOR('',#116142,1000.);
#26017=VECTOR('',#116147,10.);
#26018=VECTOR('',#116154,10.);
#26019=VECTOR('',#116157,1000.);
#26020=VECTOR('',#116160,1000.);
#26021=VECTOR('',#116189,1000.);
#26022=VECTOR('',#116196,1000.);
#26023=VECTOR('',#116199,10.);
#26024=VECTOR('',#116202,10.);
#26025=VECTOR('',#116207,1000.);
#26026=VECTOR('',#116210,1000.);
#26027=VECTOR('',#116215,10.);
#26028=VECTOR('',#116222,10.);
#26029=VECTOR('',#116225,1000.);
#26030=VECTOR('',#116228,1000.);
#26031=VECTOR('',#116257,1000.);
#26032=VECTOR('',#116264,1000.);
#26033=VECTOR('',#116267,10.);
#26034=VECTOR('',#116270,10.);
#26035=VECTOR('',#116275,1000.);
#26036=VECTOR('',#116278,1000.);
#26037=VECTOR('',#116283,10.);
#26038=VECTOR('',#116290,10.);
#26039=VECTOR('',#116293,1000.);
#26040=VECTOR('',#116296,1000.);
#26041=VECTOR('',#116325,1000.);
#26042=VECTOR('',#116332,1000.);
#26043=VECTOR('',#116335,10.);
#26044=VECTOR('',#116338,10.);
#26045=VECTOR('',#116343,1000.);
#26046=VECTOR('',#116346,1000.);
#26047=VECTOR('',#116351,10.);
#26048=VECTOR('',#116358,10.);
#26049=VECTOR('',#116361,1000.);
#26050=VECTOR('',#116364,1000.);
#26051=VECTOR('',#116393,1000.);
#26052=VECTOR('',#116400,1000.);
#26053=VECTOR('',#116403,10.);
#26054=VECTOR('',#116406,10.);
#26055=VECTOR('',#116411,1000.);
#26056=VECTOR('',#116414,1000.);
#26057=VECTOR('',#116419,10.);
#26058=VECTOR('',#116426,10.);
#26059=VECTOR('',#116429,1000.);
#26060=VECTOR('',#116432,1000.);
#26061=VECTOR('',#116461,1000.);
#26062=VECTOR('',#116468,1000.);
#26063=VECTOR('',#116471,10.);
#26064=VECTOR('',#116474,10.);
#26065=VECTOR('',#116479,1000.);
#26066=VECTOR('',#116482,1000.);
#26067=VECTOR('',#116487,10.);
#26068=VECTOR('',#116494,10.);
#26069=VECTOR('',#116497,1000.);
#26070=VECTOR('',#116500,1000.);
#26071=VECTOR('',#116529,1000.);
#26072=VECTOR('',#116536,1000.);
#26073=VECTOR('',#116539,10.);
#26074=VECTOR('',#116542,10.);
#26075=VECTOR('',#116547,1000.);
#26076=VECTOR('',#116550,1000.);
#26077=VECTOR('',#116555,10.);
#26078=VECTOR('',#116562,10.);
#26079=VECTOR('',#116565,1000.);
#26080=VECTOR('',#116568,1000.);
#26081=VECTOR('',#116597,1000.);
#26082=VECTOR('',#116604,1000.);
#26083=VECTOR('',#116607,10.);
#26084=VECTOR('',#116610,10.);
#26085=VECTOR('',#116615,1000.);
#26086=VECTOR('',#116618,1000.);
#26087=VECTOR('',#116623,10.);
#26088=VECTOR('',#116630,10.);
#26089=VECTOR('',#116633,1000.);
#26090=VECTOR('',#116636,1000.);
#26091=VECTOR('',#116665,1000.);
#26092=VECTOR('',#116672,1000.);
#26093=VECTOR('',#116675,10.);
#26094=VECTOR('',#116678,10.);
#26095=VECTOR('',#116683,1000.);
#26096=VECTOR('',#116686,1000.);
#26097=VECTOR('',#116691,10.);
#26098=VECTOR('',#116698,10.);
#26099=VECTOR('',#116701,1000.);
#26100=VECTOR('',#116704,1000.);
#26101=VECTOR('',#116733,1000.);
#26102=VECTOR('',#116740,1000.);
#26103=VECTOR('',#116743,10.);
#26104=VECTOR('',#116746,10.);
#26105=VECTOR('',#116751,1000.);
#26106=VECTOR('',#116754,1000.);
#26107=VECTOR('',#116759,10.);
#26108=VECTOR('',#116766,10.);
#26109=VECTOR('',#116769,1000.);
#26110=VECTOR('',#116772,1000.);
#26111=VECTOR('',#116801,1000.);
#26112=VECTOR('',#116808,1000.);
#26113=VECTOR('',#116811,10.);
#26114=VECTOR('',#116814,10.);
#26115=VECTOR('',#116819,1000.);
#26116=VECTOR('',#116822,1000.);
#26117=VECTOR('',#116827,10.);
#26118=VECTOR('',#116834,10.);
#26119=VECTOR('',#116837,1000.);
#26120=VECTOR('',#116840,1000.);
#26121=VECTOR('',#116869,1000.);
#26122=VECTOR('',#116876,1000.);
#26123=VECTOR('',#116879,10.);
#26124=VECTOR('',#116882,10.);
#26125=VECTOR('',#116887,1000.);
#26126=VECTOR('',#116890,1000.);
#26127=VECTOR('',#116895,10.);
#26128=VECTOR('',#116902,10.);
#26129=VECTOR('',#116905,1000.);
#26130=VECTOR('',#116908,1000.);
#26131=VECTOR('',#116937,1000.);
#26132=VECTOR('',#116944,1000.);
#26133=VECTOR('',#116947,10.);
#26134=VECTOR('',#116950,10.);
#26135=VECTOR('',#116955,1000.);
#26136=VECTOR('',#116958,1000.);
#26137=VECTOR('',#116963,10.);
#26138=VECTOR('',#116970,10.);
#26139=VECTOR('',#116973,1000.);
#26140=VECTOR('',#116976,1000.);
#26141=VECTOR('',#117005,1000.);
#26142=VECTOR('',#117012,1000.);
#26143=VECTOR('',#117015,10.);
#26144=VECTOR('',#117018,10.);
#26145=VECTOR('',#117023,1000.);
#26146=VECTOR('',#117026,1000.);
#26147=VECTOR('',#117031,10.);
#26148=VECTOR('',#117038,10.);
#26149=VECTOR('',#117041,1000.);
#26150=VECTOR('',#117044,1000.);
#26151=VECTOR('',#117073,1000.);
#26152=VECTOR('',#117080,1000.);
#26153=VECTOR('',#117083,10.);
#26154=VECTOR('',#117086,10.);
#26155=VECTOR('',#117091,1000.);
#26156=VECTOR('',#117094,1000.);
#26157=VECTOR('',#117099,10.);
#26158=VECTOR('',#117106,10.);
#26159=VECTOR('',#117109,1000.);
#26160=VECTOR('',#117112,1000.);
#26161=VECTOR('',#117141,1000.);
#26162=VECTOR('',#117148,1000.);
#26163=VECTOR('',#117151,10.);
#26164=VECTOR('',#117154,10.);
#26165=VECTOR('',#117159,1000.);
#26166=VECTOR('',#117162,1000.);
#26167=VECTOR('',#117167,10.);
#26168=VECTOR('',#117174,10.);
#26169=VECTOR('',#117177,1000.);
#26170=VECTOR('',#117180,1000.);
#26171=VECTOR('',#117211,1000.);
#26172=VECTOR('',#117218,1000.);
#26173=VECTOR('',#117221,10.);
#26174=VECTOR('',#117224,10.);
#26175=VECTOR('',#117229,1000.);
#26176=VECTOR('',#117232,1000.);
#26177=VECTOR('',#117237,10.);
#26178=VECTOR('',#117244,10.);
#26179=VECTOR('',#117247,1000.);
#26180=VECTOR('',#117250,1000.);
#26181=VECTOR('',#117281,1000.);
#26182=VECTOR('',#117284,1000.);
#26183=VECTOR('',#117291,10.);
#26184=VECTOR('',#117292,1000.);
#26185=VECTOR('',#117293,10.);
#26186=VECTOR('',#117296,1000.);
#26187=VECTOR('',#117297,10.);
#26188=VECTOR('',#117300,1000.);
#26189=VECTOR('',#117303,10.);
#26190=VECTOR('',#117304,1000.);
#26191=VECTOR('',#117309,10.);
#26192=VECTOR('',#117310,1000.);
#26193=VECTOR('',#117311,10.);
#26194=VECTOR('',#117314,1000.);
#26195=VECTOR('',#117315,10.);
#26196=VECTOR('',#117318,1000.);
#26197=VECTOR('',#117321,10.);
#26198=VECTOR('',#117322,1000.);
#26199=VECTOR('',#117417,1000.);
#26200=VECTOR('',#117420,1000.);
#26201=VECTOR('',#117427,10.);
#26202=VECTOR('',#117428,1000.);
#26203=VECTOR('',#117429,10.);
#26204=VECTOR('',#117432,1000.);
#26205=VECTOR('',#117433,10.);
#26206=VECTOR('',#117436,1000.);
#26207=VECTOR('',#117439,10.);
#26208=VECTOR('',#117440,1000.);
#26209=VECTOR('',#117445,10.);
#26210=VECTOR('',#117446,1000.);
#26211=VECTOR('',#117447,10.);
#26212=VECTOR('',#117450,1000.);
#26213=VECTOR('',#117451,10.);
#26214=VECTOR('',#117454,1000.);
#26215=VECTOR('',#117457,10.);
#26216=VECTOR('',#117458,1000.);
#26217=VECTOR('',#117461,1000.);
#26218=VECTOR('',#117464,1000.);
#26219=VECTOR('',#117471,10.);
#26220=VECTOR('',#117472,1000.);
#26221=VECTOR('',#117473,10.);
#26222=VECTOR('',#117476,1000.);
#26223=VECTOR('',#117477,10.);
#26224=VECTOR('',#117480,1000.);
#26225=VECTOR('',#117483,10.);
#26226=VECTOR('',#117484,1000.);
#26227=VECTOR('',#117489,10.);
#26228=VECTOR('',#117490,1000.);
#26229=VECTOR('',#117491,10.);
#26230=VECTOR('',#117494,1000.);
#26231=VECTOR('',#117495,10.);
#26232=VECTOR('',#117498,1000.);
#26233=VECTOR('',#117501,10.);
#26234=VECTOR('',#117502,1000.);
#26235=VECTOR('',#117505,1000.);
#26236=VECTOR('',#117508,1000.);
#26237=VECTOR('',#117515,10.);
#26238=VECTOR('',#117516,1000.);
#26239=VECTOR('',#117517,10.);
#26240=VECTOR('',#117520,1000.);
#26241=VECTOR('',#117521,10.);
#26242=VECTOR('',#117524,1000.);
#26243=VECTOR('',#117527,10.);
#26244=VECTOR('',#117528,1000.);
#26245=VECTOR('',#117533,10.);
#26246=VECTOR('',#117534,1000.);
#26247=VECTOR('',#117535,10.);
#26248=VECTOR('',#117538,1000.);
#26249=VECTOR('',#117539,10.);
#26250=VECTOR('',#117542,1000.);
#26251=VECTOR('',#117545,10.);
#26252=VECTOR('',#117546,1000.);
#26253=VECTOR('',#117549,1000.);
#26254=VECTOR('',#117552,1000.);
#26255=VECTOR('',#117559,10.);
#26256=VECTOR('',#117560,1000.);
#26257=VECTOR('',#117561,10.);
#26258=VECTOR('',#117564,1000.);
#26259=VECTOR('',#117565,10.);
#26260=VECTOR('',#117568,1000.);
#26261=VECTOR('',#117571,10.);
#26262=VECTOR('',#117572,1000.);
#26263=VECTOR('',#117577,10.);
#26264=VECTOR('',#117578,1000.);
#26265=VECTOR('',#117579,10.);
#26266=VECTOR('',#117582,1000.);
#26267=VECTOR('',#117583,10.);
#26268=VECTOR('',#117586,1000.);
#26269=VECTOR('',#117589,10.);
#26270=VECTOR('',#117590,1000.);
#26271=VECTOR('',#117593,1000.);
#26272=VECTOR('',#117596,1000.);
#26273=VECTOR('',#117603,10.);
#26274=VECTOR('',#117604,1000.);
#26275=VECTOR('',#117605,10.);
#26276=VECTOR('',#117608,1000.);
#26277=VECTOR('',#117609,10.);
#26278=VECTOR('',#117612,1000.);
#26279=VECTOR('',#117615,10.);
#26280=VECTOR('',#117616,1000.);
#26281=VECTOR('',#117621,10.);
#26282=VECTOR('',#117622,1000.);
#26283=VECTOR('',#117623,10.);
#26284=VECTOR('',#117626,1000.);
#26285=VECTOR('',#117627,10.);
#26286=VECTOR('',#117630,1000.);
#26287=VECTOR('',#117633,10.);
#26288=VECTOR('',#117634,1000.);
#26289=VECTOR('',#117637,1000.);
#26290=VECTOR('',#117640,1000.);
#26291=VECTOR('',#117647,10.);
#26292=VECTOR('',#117648,1000.);
#26293=VECTOR('',#117649,10.);
#26294=VECTOR('',#117652,1000.);
#26295=VECTOR('',#117653,10.);
#26296=VECTOR('',#117656,1000.);
#26297=VECTOR('',#117659,10.);
#26298=VECTOR('',#117660,1000.);
#26299=VECTOR('',#117665,10.);
#26300=VECTOR('',#117666,1000.);
#26301=VECTOR('',#117667,10.);
#26302=VECTOR('',#117670,1000.);
#26303=VECTOR('',#117671,10.);
#26304=VECTOR('',#117674,1000.);
#26305=VECTOR('',#117677,10.);
#26306=VECTOR('',#117678,1000.);
#26307=VECTOR('',#117681,1000.);
#26308=VECTOR('',#117684,1000.);
#26309=VECTOR('',#117691,10.);
#26310=VECTOR('',#117692,1000.);
#26311=VECTOR('',#117693,10.);
#26312=VECTOR('',#117696,1000.);
#26313=VECTOR('',#117697,10.);
#26314=VECTOR('',#117700,1000.);
#26315=VECTOR('',#117703,10.);
#26316=VECTOR('',#117704,1000.);
#26317=VECTOR('',#117709,10.);
#26318=VECTOR('',#117710,1000.);
#26319=VECTOR('',#117711,10.);
#26320=VECTOR('',#117714,1000.);
#26321=VECTOR('',#117715,10.);
#26322=VECTOR('',#117718,1000.);
#26323=VECTOR('',#117721,10.);
#26324=VECTOR('',#117722,1000.);
#26325=VECTOR('',#117725,1000.);
#26326=VECTOR('',#117728,1000.);
#26327=VECTOR('',#117735,10.);
#26328=VECTOR('',#117736,1000.);
#26329=VECTOR('',#117737,10.);
#26330=VECTOR('',#117740,1000.);
#26331=VECTOR('',#117741,10.);
#26332=VECTOR('',#117744,1000.);
#26333=VECTOR('',#117747,10.);
#26334=VECTOR('',#117748,1000.);
#26335=VECTOR('',#117753,10.);
#26336=VECTOR('',#117754,1000.);
#26337=VECTOR('',#117755,10.);
#26338=VECTOR('',#117758,1000.);
#26339=VECTOR('',#117759,10.);
#26340=VECTOR('',#117762,1000.);
#26341=VECTOR('',#117765,10.);
#26342=VECTOR('',#117766,1000.);
#26343=VECTOR('',#117769,1000.);
#26344=VECTOR('',#117772,1000.);
#26345=VECTOR('',#117779,10.);
#26346=VECTOR('',#117780,1000.);
#26347=VECTOR('',#117781,10.);
#26348=VECTOR('',#117784,1000.);
#26349=VECTOR('',#117785,10.);
#26350=VECTOR('',#117788,1000.);
#26351=VECTOR('',#117791,10.);
#26352=VECTOR('',#117792,1000.);
#26353=VECTOR('',#117797,10.);
#26354=VECTOR('',#117798,1000.);
#26355=VECTOR('',#117799,10.);
#26356=VECTOR('',#117802,1000.);
#26357=VECTOR('',#117803,10.);
#26358=VECTOR('',#117806,1000.);
#26359=VECTOR('',#117809,10.);
#26360=VECTOR('',#117810,1000.);
#26361=VECTOR('',#117813,1000.);
#26362=VECTOR('',#117816,1000.);
#26363=VECTOR('',#117823,10.);
#26364=VECTOR('',#117824,1000.);
#26365=VECTOR('',#117825,10.);
#26366=VECTOR('',#117828,1000.);
#26367=VECTOR('',#117829,10.);
#26368=VECTOR('',#117832,1000.);
#26369=VECTOR('',#117835,10.);
#26370=VECTOR('',#117836,1000.);
#26371=VECTOR('',#117841,10.);
#26372=VECTOR('',#117842,1000.);
#26373=VECTOR('',#117843,10.);
#26374=VECTOR('',#117846,1000.);
#26375=VECTOR('',#117847,10.);
#26376=VECTOR('',#117850,1000.);
#26377=VECTOR('',#117853,10.);
#26378=VECTOR('',#117854,1000.);
#26379=VECTOR('',#117857,1000.);
#26380=VECTOR('',#117860,1000.);
#26381=VECTOR('',#117867,10.);
#26382=VECTOR('',#117868,1000.);
#26383=VECTOR('',#117869,10.);
#26384=VECTOR('',#117872,1000.);
#26385=VECTOR('',#117873,10.);
#26386=VECTOR('',#117876,1000.);
#26387=VECTOR('',#117879,10.);
#26388=VECTOR('',#117880,1000.);
#26389=VECTOR('',#117885,10.);
#26390=VECTOR('',#117886,1000.);
#26391=VECTOR('',#117887,10.);
#26392=VECTOR('',#117890,1000.);
#26393=VECTOR('',#117891,10.);
#26394=VECTOR('',#117894,1000.);
#26395=VECTOR('',#117897,10.);
#26396=VECTOR('',#117898,1000.);
#26397=VECTOR('',#117901,1000.);
#26398=VECTOR('',#117904,1000.);
#26399=VECTOR('',#117911,10.);
#26400=VECTOR('',#117912,1000.);
#26401=VECTOR('',#117913,10.);
#26402=VECTOR('',#117916,1000.);
#26403=VECTOR('',#117917,10.);
#26404=VECTOR('',#117920,1000.);
#26405=VECTOR('',#117923,10.);
#26406=VECTOR('',#117924,1000.);
#26407=VECTOR('',#117929,10.);
#26408=VECTOR('',#117930,1000.);
#26409=VECTOR('',#117931,10.);
#26410=VECTOR('',#117934,1000.);
#26411=VECTOR('',#117935,10.);
#26412=VECTOR('',#117938,1000.);
#26413=VECTOR('',#117941,10.);
#26414=VECTOR('',#117942,1000.);
#26415=VECTOR('',#117945,1000.);
#26416=VECTOR('',#117948,1000.);
#26417=VECTOR('',#117955,10.);
#26418=VECTOR('',#117956,1000.);
#26419=VECTOR('',#117957,10.);
#26420=VECTOR('',#117960,1000.);
#26421=VECTOR('',#117961,10.);
#26422=VECTOR('',#117964,1000.);
#26423=VECTOR('',#117967,10.);
#26424=VECTOR('',#117968,1000.);
#26425=VECTOR('',#117973,10.);
#26426=VECTOR('',#117974,1000.);
#26427=VECTOR('',#117975,10.);
#26428=VECTOR('',#117978,1000.);
#26429=VECTOR('',#117979,10.);
#26430=VECTOR('',#117982,1000.);
#26431=VECTOR('',#117985,10.);
#26432=VECTOR('',#117986,1000.);
#26433=VECTOR('',#117989,1000.);
#26434=VECTOR('',#117992,1000.);
#26435=VECTOR('',#117999,10.);
#26436=VECTOR('',#118000,1000.);
#26437=VECTOR('',#118001,10.);
#26438=VECTOR('',#118004,1000.);
#26439=VECTOR('',#118005,10.);
#26440=VECTOR('',#118008,1000.);
#26441=VECTOR('',#118011,10.);
#26442=VECTOR('',#118012,1000.);
#26443=VECTOR('',#118017,10.);
#26444=VECTOR('',#118018,1000.);
#26445=VECTOR('',#118019,10.);
#26446=VECTOR('',#118022,1000.);
#26447=VECTOR('',#118023,10.);
#26448=VECTOR('',#118026,1000.);
#26449=VECTOR('',#118029,10.);
#26450=VECTOR('',#118030,1000.);
#26451=VECTOR('',#118033,1000.);
#26452=VECTOR('',#118036,1000.);
#26453=VECTOR('',#118043,10.);
#26454=VECTOR('',#118044,1000.);
#26455=VECTOR('',#118045,10.);
#26456=VECTOR('',#118048,1000.);
#26457=VECTOR('',#118049,10.);
#26458=VECTOR('',#118052,1000.);
#26459=VECTOR('',#118055,10.);
#26460=VECTOR('',#118056,1000.);
#26461=VECTOR('',#118061,10.);
#26462=VECTOR('',#118062,1000.);
#26463=VECTOR('',#118063,10.);
#26464=VECTOR('',#118066,1000.);
#26465=VECTOR('',#118067,10.);
#26466=VECTOR('',#118070,1000.);
#26467=VECTOR('',#118073,10.);
#26468=VECTOR('',#118074,1000.);
#26469=VECTOR('',#118077,1000.);
#26470=VECTOR('',#118080,1000.);
#26471=VECTOR('',#118087,10.);
#26472=VECTOR('',#118088,1000.);
#26473=VECTOR('',#118089,10.);
#26474=VECTOR('',#118092,1000.);
#26475=VECTOR('',#118093,10.);
#26476=VECTOR('',#118096,1000.);
#26477=VECTOR('',#118099,10.);
#26478=VECTOR('',#118100,1000.);
#26479=VECTOR('',#118105,10.);
#26480=VECTOR('',#118106,1000.);
#26481=VECTOR('',#118107,10.);
#26482=VECTOR('',#118110,1000.);
#26483=VECTOR('',#118111,10.);
#26484=VECTOR('',#118114,1000.);
#26485=VECTOR('',#118117,10.);
#26486=VECTOR('',#118118,1000.);
#26487=VECTOR('',#118121,1000.);
#26488=VECTOR('',#118124,1000.);
#26489=VECTOR('',#118131,10.);
#26490=VECTOR('',#118132,1000.);
#26491=VECTOR('',#118133,10.);
#26492=VECTOR('',#118136,1000.);
#26493=VECTOR('',#118137,10.);
#26494=VECTOR('',#118140,1000.);
#26495=VECTOR('',#118143,10.);
#26496=VECTOR('',#118144,1000.);
#26497=VECTOR('',#118149,10.);
#26498=VECTOR('',#118150,1000.);
#26499=VECTOR('',#118151,10.);
#26500=VECTOR('',#118154,1000.);
#26501=VECTOR('',#118155,10.);
#26502=VECTOR('',#118158,1000.);
#26503=VECTOR('',#118161,10.);
#26504=VECTOR('',#118162,1000.);
#26505=VECTOR('',#118165,1000.);
#26506=VECTOR('',#118168,1000.);
#26507=VECTOR('',#118175,10.);
#26508=VECTOR('',#118176,1000.);
#26509=VECTOR('',#118177,10.);
#26510=VECTOR('',#118180,1000.);
#26511=VECTOR('',#118181,10.);
#26512=VECTOR('',#118184,1000.);
#26513=VECTOR('',#118187,10.);
#26514=VECTOR('',#118188,1000.);
#26515=VECTOR('',#118193,10.);
#26516=VECTOR('',#118194,1000.);
#26517=VECTOR('',#118195,10.);
#26518=VECTOR('',#118198,1000.);
#26519=VECTOR('',#118199,10.);
#26520=VECTOR('',#118202,1000.);
#26521=VECTOR('',#118205,10.);
#26522=VECTOR('',#118206,1000.);
#26523=VECTOR('',#118209,1000.);
#26524=VECTOR('',#118212,1000.);
#26525=VECTOR('',#118219,10.);
#26526=VECTOR('',#118220,1000.);
#26527=VECTOR('',#118221,10.);
#26528=VECTOR('',#118224,1000.);
#26529=VECTOR('',#118225,10.);
#26530=VECTOR('',#118228,1000.);
#26531=VECTOR('',#118231,10.);
#26532=VECTOR('',#118232,1000.);
#26533=VECTOR('',#118237,10.);
#26534=VECTOR('',#118238,1000.);
#26535=VECTOR('',#118239,10.);
#26536=VECTOR('',#118242,1000.);
#26537=VECTOR('',#118243,10.);
#26538=VECTOR('',#118246,1000.);
#26539=VECTOR('',#118249,10.);
#26540=VECTOR('',#118250,1000.);
#26541=VECTOR('',#118253,1000.);
#26542=VECTOR('',#118256,1000.);
#26543=VECTOR('',#118263,10.);
#26544=VECTOR('',#118264,1000.);
#26545=VECTOR('',#118265,10.);
#26546=VECTOR('',#118268,1000.);
#26547=VECTOR('',#118269,10.);
#26548=VECTOR('',#118272,1000.);
#26549=VECTOR('',#118275,10.);
#26550=VECTOR('',#118276,1000.);
#26551=VECTOR('',#118281,10.);
#26552=VECTOR('',#118282,1000.);
#26553=VECTOR('',#118283,10.);
#26554=VECTOR('',#118286,1000.);
#26555=VECTOR('',#118287,10.);
#26556=VECTOR('',#118290,1000.);
#26557=VECTOR('',#118293,10.);
#26558=VECTOR('',#118294,1000.);
#26559=VECTOR('',#118297,1000.);
#26560=VECTOR('',#118300,1000.);
#26561=VECTOR('',#118307,10.);
#26562=VECTOR('',#118308,1000.);
#26563=VECTOR('',#118309,10.);
#26564=VECTOR('',#118312,1000.);
#26565=VECTOR('',#118313,10.);
#26566=VECTOR('',#118316,1000.);
#26567=VECTOR('',#118319,10.);
#26568=VECTOR('',#118320,1000.);
#26569=VECTOR('',#118325,10.);
#26570=VECTOR('',#118326,1000.);
#26571=VECTOR('',#118327,10.);
#26572=VECTOR('',#118330,1000.);
#26573=VECTOR('',#118331,10.);
#26574=VECTOR('',#118334,1000.);
#26575=VECTOR('',#118337,10.);
#26576=VECTOR('',#118338,1000.);
#26577=VECTOR('',#118341,1000.);
#26578=VECTOR('',#118344,1000.);
#26579=VECTOR('',#118351,10.);
#26580=VECTOR('',#118352,1000.);
#26581=VECTOR('',#118353,10.);
#26582=VECTOR('',#118356,1000.);
#26583=VECTOR('',#118357,10.);
#26584=VECTOR('',#118360,1000.);
#26585=VECTOR('',#118363,10.);
#26586=VECTOR('',#118364,1000.);
#26587=VECTOR('',#118369,10.);
#26588=VECTOR('',#118370,1000.);
#26589=VECTOR('',#118371,10.);
#26590=VECTOR('',#118374,1000.);
#26591=VECTOR('',#118375,10.);
#26592=VECTOR('',#118378,1000.);
#26593=VECTOR('',#118381,10.);
#26594=VECTOR('',#118382,1000.);
#26595=VECTOR('',#118385,1000.);
#26596=VECTOR('',#118388,1000.);
#26597=VECTOR('',#118395,10.);
#26598=VECTOR('',#118396,1000.);
#26599=VECTOR('',#118397,10.);
#26600=VECTOR('',#118400,1000.);
#26601=VECTOR('',#118401,10.);
#26602=VECTOR('',#118404,1000.);
#26603=VECTOR('',#118407,10.);
#26604=VECTOR('',#118408,1000.);
#26605=VECTOR('',#118413,10.);
#26606=VECTOR('',#118414,1000.);
#26607=VECTOR('',#118415,10.);
#26608=VECTOR('',#118418,1000.);
#26609=VECTOR('',#118419,10.);
#26610=VECTOR('',#118422,1000.);
#26611=VECTOR('',#118425,10.);
#26612=VECTOR('',#118426,1000.);
#26613=VECTOR('',#118429,1000.);
#26614=VECTOR('',#118432,1000.);
#26615=VECTOR('',#118439,10.);
#26616=VECTOR('',#118440,1000.);
#26617=VECTOR('',#118441,10.);
#26618=VECTOR('',#118444,1000.);
#26619=VECTOR('',#118445,10.);
#26620=VECTOR('',#118448,1000.);
#26621=VECTOR('',#118451,10.);
#26622=VECTOR('',#118452,1000.);
#26623=VECTOR('',#118457,10.);
#26624=VECTOR('',#118458,1000.);
#26625=VECTOR('',#118459,10.);
#26626=VECTOR('',#118462,1000.);
#26627=VECTOR('',#118463,10.);
#26628=VECTOR('',#118466,1000.);
#26629=VECTOR('',#118469,10.);
#26630=VECTOR('',#118470,1000.);
#26631=VECTOR('',#118473,1000.);
#26632=VECTOR('',#118476,1000.);
#26633=VECTOR('',#118483,10.);
#26634=VECTOR('',#118484,1000.);
#26635=VECTOR('',#118485,10.);
#26636=VECTOR('',#118488,1000.);
#26637=VECTOR('',#118489,10.);
#26638=VECTOR('',#118492,1000.);
#26639=VECTOR('',#118495,10.);
#26640=VECTOR('',#118496,1000.);
#26641=VECTOR('',#118501,10.);
#26642=VECTOR('',#118502,1000.);
#26643=VECTOR('',#118503,10.);
#26644=VECTOR('',#118506,1000.);
#26645=VECTOR('',#118507,10.);
#26646=VECTOR('',#118510,1000.);
#26647=VECTOR('',#118513,10.);
#26648=VECTOR('',#118514,1000.);
#26649=VECTOR('',#118517,1000.);
#26650=VECTOR('',#118520,1000.);
#26651=VECTOR('',#118527,10.);
#26652=VECTOR('',#118528,1000.);
#26653=VECTOR('',#118529,10.);
#26654=VECTOR('',#118532,1000.);
#26655=VECTOR('',#118533,10.);
#26656=VECTOR('',#118536,1000.);
#26657=VECTOR('',#118539,10.);
#26658=VECTOR('',#118540,1000.);
#26659=VECTOR('',#118545,10.);
#26660=VECTOR('',#118546,1000.);
#26661=VECTOR('',#118547,10.);
#26662=VECTOR('',#118550,1000.);
#26663=VECTOR('',#118551,10.);
#26664=VECTOR('',#118554,1000.);
#26665=VECTOR('',#118557,10.);
#26666=VECTOR('',#118558,1000.);
#26667=VECTOR('',#118561,1000.);
#26668=VECTOR('',#118564,1000.);
#26669=VECTOR('',#118571,10.);
#26670=VECTOR('',#118572,1000.);
#26671=VECTOR('',#118573,10.);
#26672=VECTOR('',#118576,1000.);
#26673=VECTOR('',#118577,10.);
#26674=VECTOR('',#118580,1000.);
#26675=VECTOR('',#118583,10.);
#26676=VECTOR('',#118584,1000.);
#26677=VECTOR('',#118589,10.);
#26678=VECTOR('',#118590,1000.);
#26679=VECTOR('',#118591,10.);
#26680=VECTOR('',#118594,1000.);
#26681=VECTOR('',#118595,10.);
#26682=VECTOR('',#118598,1000.);
#26683=VECTOR('',#118601,10.);
#26684=VECTOR('',#118602,1000.);
#26685=VECTOR('',#118605,1000.);
#26686=VECTOR('',#118608,1000.);
#26687=VECTOR('',#118615,10.);
#26688=VECTOR('',#118616,1000.);
#26689=VECTOR('',#118617,10.);
#26690=VECTOR('',#118620,1000.);
#26691=VECTOR('',#118621,10.);
#26692=VECTOR('',#118624,1000.);
#26693=VECTOR('',#118627,10.);
#26694=VECTOR('',#118628,1000.);
#26695=VECTOR('',#118633,10.);
#26696=VECTOR('',#118634,1000.);
#26697=VECTOR('',#118635,10.);
#26698=VECTOR('',#118638,1000.);
#26699=VECTOR('',#118639,10.);
#26700=VECTOR('',#118642,1000.);
#26701=VECTOR('',#118645,10.);
#26702=VECTOR('',#118646,1000.);
#26703=VECTOR('',#118649,1000.);
#26704=VECTOR('',#118652,1000.);
#26705=VECTOR('',#118659,10.);
#26706=VECTOR('',#118660,1000.);
#26707=VECTOR('',#118661,10.);
#26708=VECTOR('',#118664,1000.);
#26709=VECTOR('',#118665,10.);
#26710=VECTOR('',#118668,1000.);
#26711=VECTOR('',#118671,10.);
#26712=VECTOR('',#118672,1000.);
#26713=VECTOR('',#118677,10.);
#26714=VECTOR('',#118678,1000.);
#26715=VECTOR('',#118679,10.);
#26716=VECTOR('',#118682,1000.);
#26717=VECTOR('',#118683,10.);
#26718=VECTOR('',#118686,1000.);
#26719=VECTOR('',#118689,10.);
#26720=VECTOR('',#118690,1000.);
#26721=VECTOR('',#118693,1000.);
#26722=VECTOR('',#118694,1000.);
#26723=VECTOR('',#118699,10.);
#26724=VECTOR('',#118700,1000.);
#26725=VECTOR('',#118701,10.);
#26726=VECTOR('',#118704,1000.);
#26727=VECTOR('',#118705,10.);
#26728=VECTOR('',#118708,1000.);
#26729=VECTOR('',#118711,10.);
#26730=VECTOR('',#118712,1000.);
#26731=VECTOR('',#118717,10.);
#26732=VECTOR('',#118718,1000.);
#26733=VECTOR('',#118719,10.);
#26734=VECTOR('',#118722,1000.);
#26735=VECTOR('',#118723,10.);
#26736=VECTOR('',#118726,1000.);
#26737=VECTOR('',#118729,10.);
#26738=VECTOR('',#118730,1000.);
#26739=VECTOR('',#118733,1000.);
#26740=VECTOR('',#118736,1000.);
#26741=VECTOR('',#118743,10.);
#26742=VECTOR('',#118744,1000.);
#26743=VECTOR('',#118745,10.);
#26744=VECTOR('',#118748,1000.);
#26745=VECTOR('',#118749,10.);
#26746=VECTOR('',#118752,1000.);
#26747=VECTOR('',#118755,10.);
#26748=VECTOR('',#118756,1000.);
#26749=VECTOR('',#118761,10.);
#26750=VECTOR('',#118762,1000.);
#26751=VECTOR('',#118763,10.);
#26752=VECTOR('',#118766,1000.);
#26753=VECTOR('',#118767,10.);
#26754=VECTOR('',#118770,1000.);
#26755=VECTOR('',#118773,10.);
#26756=VECTOR('',#118774,1000.);
#26757=VECTOR('',#118777,1000.);
#26758=VECTOR('',#118780,1000.);
#26759=VECTOR('',#118787,10.);
#26760=VECTOR('',#118788,1000.);
#26761=VECTOR('',#118789,10.);
#26762=VECTOR('',#118792,1000.);
#26763=VECTOR('',#118793,10.);
#26764=VECTOR('',#118796,1000.);
#26765=VECTOR('',#118799,10.);
#26766=VECTOR('',#118800,1000.);
#26767=VECTOR('',#118805,10.);
#26768=VECTOR('',#118806,1000.);
#26769=VECTOR('',#118807,10.);
#26770=VECTOR('',#118810,1000.);
#26771=VECTOR('',#118811,10.);
#26772=VECTOR('',#118814,1000.);
#26773=VECTOR('',#118817,10.);
#26774=VECTOR('',#118818,1000.);
#26775=VECTOR('',#118821,1000.);
#26776=VECTOR('',#118824,1000.);
#26777=VECTOR('',#118831,10.);
#26778=VECTOR('',#118832,1000.);
#26779=VECTOR('',#118833,10.);
#26780=VECTOR('',#118836,1000.);
#26781=VECTOR('',#118837,10.);
#26782=VECTOR('',#118840,1000.);
#26783=VECTOR('',#118843,10.);
#26784=VECTOR('',#118844,1000.);
#26785=VECTOR('',#118849,10.);
#26786=VECTOR('',#118850,1000.);
#26787=VECTOR('',#118851,10.);
#26788=VECTOR('',#118854,1000.);
#26789=VECTOR('',#118855,10.);
#26790=VECTOR('',#118858,1000.);
#26791=VECTOR('',#118861,10.);
#26792=VECTOR('',#118862,1000.);
#26793=VECTOR('',#118865,1000.);
#26794=VECTOR('',#118868,1000.);
#26795=VECTOR('',#118875,10.);
#26796=VECTOR('',#118876,1000.);
#26797=VECTOR('',#118877,10.);
#26798=VECTOR('',#118880,1000.);
#26799=VECTOR('',#118881,10.);
#26800=VECTOR('',#118884,1000.);
#26801=VECTOR('',#118887,10.);
#26802=VECTOR('',#118888,1000.);
#26803=VECTOR('',#118893,10.);
#26804=VECTOR('',#118894,1000.);
#26805=VECTOR('',#118895,10.);
#26806=VECTOR('',#118898,1000.);
#26807=VECTOR('',#118899,10.);
#26808=VECTOR('',#118902,1000.);
#26809=VECTOR('',#118905,10.);
#26810=VECTOR('',#118906,1000.);
#26811=VECTOR('',#118909,1000.);
#26812=VECTOR('',#118912,1000.);
#26813=VECTOR('',#118919,10.);
#26814=VECTOR('',#118920,1000.);
#26815=VECTOR('',#118921,10.);
#26816=VECTOR('',#118924,1000.);
#26817=VECTOR('',#118925,10.);
#26818=VECTOR('',#118928,1000.);
#26819=VECTOR('',#118931,10.);
#26820=VECTOR('',#118932,1000.);
#26821=VECTOR('',#118937,10.);
#26822=VECTOR('',#118938,1000.);
#26823=VECTOR('',#118939,10.);
#26824=VECTOR('',#118942,1000.);
#26825=VECTOR('',#118943,10.);
#26826=VECTOR('',#118946,1000.);
#26827=VECTOR('',#118949,10.);
#26828=VECTOR('',#118950,1000.);
#26829=VECTOR('',#118953,1000.);
#26830=VECTOR('',#118956,1000.);
#26831=VECTOR('',#118963,10.);
#26832=VECTOR('',#118964,1000.);
#26833=VECTOR('',#118965,10.);
#26834=VECTOR('',#118968,1000.);
#26835=VECTOR('',#118969,10.);
#26836=VECTOR('',#118972,1000.);
#26837=VECTOR('',#118975,10.);
#26838=VECTOR('',#118976,1000.);
#26839=VECTOR('',#118981,10.);
#26840=VECTOR('',#118982,1000.);
#26841=VECTOR('',#118983,10.);
#26842=VECTOR('',#118986,1000.);
#26843=VECTOR('',#118987,10.);
#26844=VECTOR('',#118990,1000.);
#26845=VECTOR('',#118993,10.);
#26846=VECTOR('',#118994,1000.);
#26847=VECTOR('',#118997,1000.);
#26848=VECTOR('',#119000,1000.);
#26849=VECTOR('',#119007,10.);
#26850=VECTOR('',#119008,1000.);
#26851=VECTOR('',#119009,10.);
#26852=VECTOR('',#119012,1000.);
#26853=VECTOR('',#119013,10.);
#26854=VECTOR('',#119016,1000.);
#26855=VECTOR('',#119019,10.);
#26856=VECTOR('',#119020,1000.);
#26857=VECTOR('',#119025,10.);
#26858=VECTOR('',#119026,1000.);
#26859=VECTOR('',#119027,10.);
#26860=VECTOR('',#119030,1000.);
#26861=VECTOR('',#119031,10.);
#26862=VECTOR('',#119034,1000.);
#26863=VECTOR('',#119037,10.);
#26864=VECTOR('',#119038,1000.);
#26865=VECTOR('',#119041,1000.);
#26866=VECTOR('',#119044,1000.);
#26867=VECTOR('',#119051,10.);
#26868=VECTOR('',#119052,1000.);
#26869=VECTOR('',#119053,10.);
#26870=VECTOR('',#119056,1000.);
#26871=VECTOR('',#119057,10.);
#26872=VECTOR('',#119060,1000.);
#26873=VECTOR('',#119063,10.);
#26874=VECTOR('',#119064,1000.);
#26875=VECTOR('',#119069,10.);
#26876=VECTOR('',#119070,1000.);
#26877=VECTOR('',#119071,10.);
#26878=VECTOR('',#119074,1000.);
#26879=VECTOR('',#119075,10.);
#26880=VECTOR('',#119078,1000.);
#26881=VECTOR('',#119081,10.);
#26882=VECTOR('',#119082,1000.);
#26883=VECTOR('',#119085,1000.);
#26884=VECTOR('',#119088,1000.);
#26885=VECTOR('',#119095,10.);
#26886=VECTOR('',#119096,1000.);
#26887=VECTOR('',#119097,10.);
#26888=VECTOR('',#119100,1000.);
#26889=VECTOR('',#119101,10.);
#26890=VECTOR('',#119104,1000.);
#26891=VECTOR('',#119107,10.);
#26892=VECTOR('',#119108,1000.);
#26893=VECTOR('',#119113,10.);
#26894=VECTOR('',#119114,1000.);
#26895=VECTOR('',#119115,10.);
#26896=VECTOR('',#119118,1000.);
#26897=VECTOR('',#119119,10.);
#26898=VECTOR('',#119122,1000.);
#26899=VECTOR('',#119125,10.);
#26900=VECTOR('',#119126,1000.);
#26901=VECTOR('',#119129,1000.);
#26902=VECTOR('',#119132,1000.);
#26903=VECTOR('',#119139,10.);
#26904=VECTOR('',#119140,1000.);
#26905=VECTOR('',#119141,10.);
#26906=VECTOR('',#119144,1000.);
#26907=VECTOR('',#119145,10.);
#26908=VECTOR('',#119148,1000.);
#26909=VECTOR('',#119151,10.);
#26910=VECTOR('',#119152,1000.);
#26911=VECTOR('',#119157,10.);
#26912=VECTOR('',#119158,1000.);
#26913=VECTOR('',#119159,10.);
#26914=VECTOR('',#119162,1000.);
#26915=VECTOR('',#119163,10.);
#26916=VECTOR('',#119166,1000.);
#26917=VECTOR('',#119169,10.);
#26918=VECTOR('',#119170,1000.);
#26919=VECTOR('',#119173,1000.);
#26920=VECTOR('',#119176,1000.);
#26921=VECTOR('',#119183,10.);
#26922=VECTOR('',#119184,1000.);
#26923=VECTOR('',#119185,10.);
#26924=VECTOR('',#119188,1000.);
#26925=VECTOR('',#119189,10.);
#26926=VECTOR('',#119192,1000.);
#26927=VECTOR('',#119195,10.);
#26928=VECTOR('',#119196,1000.);
#26929=VECTOR('',#119201,10.);
#26930=VECTOR('',#119202,1000.);
#26931=VECTOR('',#119203,10.);
#26932=VECTOR('',#119206,1000.);
#26933=VECTOR('',#119207,10.);
#26934=VECTOR('',#119210,1000.);
#26935=VECTOR('',#119213,10.);
#26936=VECTOR('',#119214,1000.);
#26937=VECTOR('',#119217,1000.);
#26938=VECTOR('',#119220,1000.);
#26939=VECTOR('',#119227,10.);
#26940=VECTOR('',#119228,1000.);
#26941=VECTOR('',#119229,10.);
#26942=VECTOR('',#119232,1000.);
#26943=VECTOR('',#119233,10.);
#26944=VECTOR('',#119236,1000.);
#26945=VECTOR('',#119239,10.);
#26946=VECTOR('',#119240,1000.);
#26947=VECTOR('',#119245,10.);
#26948=VECTOR('',#119246,1000.);
#26949=VECTOR('',#119247,10.);
#26950=VECTOR('',#119250,1000.);
#26951=VECTOR('',#119251,10.);
#26952=VECTOR('',#119254,1000.);
#26953=VECTOR('',#119257,10.);
#26954=VECTOR('',#119258,1000.);
#26955=VECTOR('',#119261,1000.);
#26956=VECTOR('',#119264,1000.);
#26957=VECTOR('',#119271,10.);
#26958=VECTOR('',#119272,1000.);
#26959=VECTOR('',#119273,10.);
#26960=VECTOR('',#119276,1000.);
#26961=VECTOR('',#119277,10.);
#26962=VECTOR('',#119280,1000.);
#26963=VECTOR('',#119283,10.);
#26964=VECTOR('',#119284,1000.);
#26965=VECTOR('',#119289,10.);
#26966=VECTOR('',#119290,1000.);
#26967=VECTOR('',#119291,10.);
#26968=VECTOR('',#119294,1000.);
#26969=VECTOR('',#119295,10.);
#26970=VECTOR('',#119298,1000.);
#26971=VECTOR('',#119301,10.);
#26972=VECTOR('',#119302,1000.);
#26973=VECTOR('',#119305,1000.);
#26974=VECTOR('',#119308,1000.);
#26975=VECTOR('',#119315,10.);
#26976=VECTOR('',#119316,1000.);
#26977=VECTOR('',#119317,10.);
#26978=VECTOR('',#119320,1000.);
#26979=VECTOR('',#119321,10.);
#26980=VECTOR('',#119324,1000.);
#26981=VECTOR('',#119327,10.);
#26982=VECTOR('',#119328,1000.);
#26983=VECTOR('',#119333,10.);
#26984=VECTOR('',#119334,1000.);
#26985=VECTOR('',#119335,10.);
#26986=VECTOR('',#119338,1000.);
#26987=VECTOR('',#119339,10.);
#26988=VECTOR('',#119342,1000.);
#26989=VECTOR('',#119345,10.);
#26990=VECTOR('',#119346,1000.);
#26991=VECTOR('',#119349,1000.);
#26992=VECTOR('',#119350,1000.);
#26993=VECTOR('',#119355,10.);
#26994=VECTOR('',#119356,1000.);
#26995=VECTOR('',#119357,10.);
#26996=VECTOR('',#119360,1000.);
#26997=VECTOR('',#119361,10.);
#26998=VECTOR('',#119364,1000.);
#26999=VECTOR('',#119367,10.);
#27000=VECTOR('',#119368,1000.);
#27001=VECTOR('',#119373,10.);
#27002=VECTOR('',#119374,1000.);
#27003=VECTOR('',#119375,10.);
#27004=VECTOR('',#119378,1000.);
#27005=VECTOR('',#119379,10.);
#27006=VECTOR('',#119382,1000.);
#27007=VECTOR('',#119385,10.);
#27008=VECTOR('',#119386,1000.);
#27009=VECTOR('',#119389,1000.);
#27010=VECTOR('',#119392,1000.);
#27011=VECTOR('',#119399,10.);
#27012=VECTOR('',#119400,1000.);
#27013=VECTOR('',#119401,10.);
#27014=VECTOR('',#119404,1000.);
#27015=VECTOR('',#119405,10.);
#27016=VECTOR('',#119408,1000.);
#27017=VECTOR('',#119411,10.);
#27018=VECTOR('',#119412,1000.);
#27019=VECTOR('',#119417,10.);
#27020=VECTOR('',#119418,1000.);
#27021=VECTOR('',#119419,10.);
#27022=VECTOR('',#119422,1000.);
#27023=VECTOR('',#119423,10.);
#27024=VECTOR('',#119426,1000.);
#27025=VECTOR('',#119429,10.);
#27026=VECTOR('',#119430,1000.);
#27027=VECTOR('',#119433,1000.);
#27028=VECTOR('',#119436,1000.);
#27029=VECTOR('',#119443,10.);
#27030=VECTOR('',#119444,1000.);
#27031=VECTOR('',#119445,10.);
#27032=VECTOR('',#119448,1000.);
#27033=VECTOR('',#119449,10.);
#27034=VECTOR('',#119452,1000.);
#27035=VECTOR('',#119455,10.);
#27036=VECTOR('',#119456,1000.);
#27037=VECTOR('',#119461,10.);
#27038=VECTOR('',#119462,1000.);
#27039=VECTOR('',#119463,10.);
#27040=VECTOR('',#119466,1000.);
#27041=VECTOR('',#119467,10.);
#27042=VECTOR('',#119470,1000.);
#27043=VECTOR('',#119473,10.);
#27044=VECTOR('',#119474,1000.);
#27045=VECTOR('',#119477,1000.);
#27046=VECTOR('',#119480,1000.);
#27047=VECTOR('',#119487,10.);
#27048=VECTOR('',#119488,1000.);
#27049=VECTOR('',#119489,10.);
#27050=VECTOR('',#119492,1000.);
#27051=VECTOR('',#119493,10.);
#27052=VECTOR('',#119496,1000.);
#27053=VECTOR('',#119499,10.);
#27054=VECTOR('',#119500,1000.);
#27055=VECTOR('',#119505,10.);
#27056=VECTOR('',#119506,1000.);
#27057=VECTOR('',#119507,10.);
#27058=VECTOR('',#119510,1000.);
#27059=VECTOR('',#119511,10.);
#27060=VECTOR('',#119514,1000.);
#27061=VECTOR('',#119517,10.);
#27062=VECTOR('',#119518,1000.);
#27063=VECTOR('',#119521,1000.);
#27064=VECTOR('',#119524,1000.);
#27065=VECTOR('',#119531,10.);
#27066=VECTOR('',#119532,1000.);
#27067=VECTOR('',#119533,10.);
#27068=VECTOR('',#119536,1000.);
#27069=VECTOR('',#119537,10.);
#27070=VECTOR('',#119540,1000.);
#27071=VECTOR('',#119543,10.);
#27072=VECTOR('',#119544,1000.);
#27073=VECTOR('',#119549,10.);
#27074=VECTOR('',#119550,1000.);
#27075=VECTOR('',#119551,10.);
#27076=VECTOR('',#119554,1000.);
#27077=VECTOR('',#119555,10.);
#27078=VECTOR('',#119558,1000.);
#27079=VECTOR('',#119561,10.);
#27080=VECTOR('',#119562,1000.);
#27081=VECTOR('',#119565,1000.);
#27082=VECTOR('',#119568,1000.);
#27083=VECTOR('',#119575,10.);
#27084=VECTOR('',#119576,1000.);
#27085=VECTOR('',#119577,10.);
#27086=VECTOR('',#119580,1000.);
#27087=VECTOR('',#119581,10.);
#27088=VECTOR('',#119584,1000.);
#27089=VECTOR('',#119587,10.);
#27090=VECTOR('',#119588,1000.);
#27091=VECTOR('',#119593,10.);
#27092=VECTOR('',#119594,1000.);
#27093=VECTOR('',#119595,10.);
#27094=VECTOR('',#119598,1000.);
#27095=VECTOR('',#119599,10.);
#27096=VECTOR('',#119602,1000.);
#27097=VECTOR('',#119605,10.);
#27098=VECTOR('',#119606,1000.);
#27099=VECTOR('',#119609,1000.);
#27100=VECTOR('',#119612,1000.);
#27101=VECTOR('',#119619,10.);
#27102=VECTOR('',#119620,1000.);
#27103=VECTOR('',#119621,10.);
#27104=VECTOR('',#119624,1000.);
#27105=VECTOR('',#119625,10.);
#27106=VECTOR('',#119628,1000.);
#27107=VECTOR('',#119631,10.);
#27108=VECTOR('',#119632,1000.);
#27109=VECTOR('',#119637,10.);
#27110=VECTOR('',#119638,1000.);
#27111=VECTOR('',#119639,10.);
#27112=VECTOR('',#119642,1000.);
#27113=VECTOR('',#119643,10.);
#27114=VECTOR('',#119646,1000.);
#27115=VECTOR('',#119649,10.);
#27116=VECTOR('',#119650,1000.);
#27117=VECTOR('',#119653,1000.);
#27118=VECTOR('',#119656,1000.);
#27119=VECTOR('',#119663,10.);
#27120=VECTOR('',#119664,1000.);
#27121=VECTOR('',#119665,10.);
#27122=VECTOR('',#119668,1000.);
#27123=VECTOR('',#119669,10.);
#27124=VECTOR('',#119672,1000.);
#27125=VECTOR('',#119675,10.);
#27126=VECTOR('',#119676,1000.);
#27127=VECTOR('',#119681,10.);
#27128=VECTOR('',#119682,1000.);
#27129=VECTOR('',#119683,10.);
#27130=VECTOR('',#119686,1000.);
#27131=VECTOR('',#119687,10.);
#27132=VECTOR('',#119690,1000.);
#27133=VECTOR('',#119693,10.);
#27134=VECTOR('',#119694,1000.);
#27135=VECTOR('',#119697,1000.);
#27136=VECTOR('',#119700,1000.);
#27137=VECTOR('',#119707,10.);
#27138=VECTOR('',#119708,1000.);
#27139=VECTOR('',#119709,10.);
#27140=VECTOR('',#119712,1000.);
#27141=VECTOR('',#119713,10.);
#27142=VECTOR('',#119716,1000.);
#27143=VECTOR('',#119719,10.);
#27144=VECTOR('',#119720,1000.);
#27145=VECTOR('',#119725,10.);
#27146=VECTOR('',#119726,1000.);
#27147=VECTOR('',#119727,10.);
#27148=VECTOR('',#119730,1000.);
#27149=VECTOR('',#119731,10.);
#27150=VECTOR('',#119734,1000.);
#27151=VECTOR('',#119737,10.);
#27152=VECTOR('',#119738,1000.);
#27153=VECTOR('',#119741,1000.);
#27154=VECTOR('',#119744,1000.);
#27155=VECTOR('',#119751,10.);
#27156=VECTOR('',#119752,1000.);
#27157=VECTOR('',#119753,10.);
#27158=VECTOR('',#119756,1000.);
#27159=VECTOR('',#119757,10.);
#27160=VECTOR('',#119760,1000.);
#27161=VECTOR('',#119763,10.);
#27162=VECTOR('',#119764,1000.);
#27163=VECTOR('',#119769,10.);
#27164=VECTOR('',#119770,1000.);
#27165=VECTOR('',#119771,10.);
#27166=VECTOR('',#119774,1000.);
#27167=VECTOR('',#119775,10.);
#27168=VECTOR('',#119778,1000.);
#27169=VECTOR('',#119781,10.);
#27170=VECTOR('',#119782,1000.);
#27171=VECTOR('',#119785,1000.);
#27172=VECTOR('',#119788,1000.);
#27173=VECTOR('',#119795,10.);
#27174=VECTOR('',#119796,1000.);
#27175=VECTOR('',#119797,10.);
#27176=VECTOR('',#119800,1000.);
#27177=VECTOR('',#119801,10.);
#27178=VECTOR('',#119804,1000.);
#27179=VECTOR('',#119807,10.);
#27180=VECTOR('',#119808,1000.);
#27181=VECTOR('',#119813,10.);
#27182=VECTOR('',#119814,1000.);
#27183=VECTOR('',#119815,10.);
#27184=VECTOR('',#119818,1000.);
#27185=VECTOR('',#119819,10.);
#27186=VECTOR('',#119822,1000.);
#27187=VECTOR('',#119825,10.);
#27188=VECTOR('',#119826,1000.);
#27189=VECTOR('',#119829,1000.);
#27190=VECTOR('',#119832,1000.);
#27191=VECTOR('',#119839,10.);
#27192=VECTOR('',#119840,1000.);
#27193=VECTOR('',#119841,10.);
#27194=VECTOR('',#119844,1000.);
#27195=VECTOR('',#119845,10.);
#27196=VECTOR('',#119848,1000.);
#27197=VECTOR('',#119851,10.);
#27198=VECTOR('',#119852,1000.);
#27199=VECTOR('',#119857,10.);
#27200=VECTOR('',#119858,1000.);
#27201=VECTOR('',#119859,10.);
#27202=VECTOR('',#119862,1000.);
#27203=VECTOR('',#119863,10.);
#27204=VECTOR('',#119866,1000.);
#27205=VECTOR('',#119869,10.);
#27206=VECTOR('',#119870,1000.);
#27207=VECTOR('',#119873,1000.);
#27208=VECTOR('',#119876,1000.);
#27209=VECTOR('',#119883,10.);
#27210=VECTOR('',#119884,1000.);
#27211=VECTOR('',#119885,10.);
#27212=VECTOR('',#119888,1000.);
#27213=VECTOR('',#119889,10.);
#27214=VECTOR('',#119892,1000.);
#27215=VECTOR('',#119895,10.);
#27216=VECTOR('',#119896,1000.);
#27217=VECTOR('',#119901,10.);
#27218=VECTOR('',#119902,1000.);
#27219=VECTOR('',#119903,10.);
#27220=VECTOR('',#119906,1000.);
#27221=VECTOR('',#119907,10.);
#27222=VECTOR('',#119910,1000.);
#27223=VECTOR('',#119913,10.);
#27224=VECTOR('',#119914,1000.);
#27225=VECTOR('',#119917,1000.);
#27226=VECTOR('',#119920,1000.);
#27227=VECTOR('',#119927,10.);
#27228=VECTOR('',#119928,1000.);
#27229=VECTOR('',#119929,10.);
#27230=VECTOR('',#119932,1000.);
#27231=VECTOR('',#119933,10.);
#27232=VECTOR('',#119936,1000.);
#27233=VECTOR('',#119939,10.);
#27234=VECTOR('',#119940,1000.);
#27235=VECTOR('',#119945,10.);
#27236=VECTOR('',#119946,1000.);
#27237=VECTOR('',#119947,10.);
#27238=VECTOR('',#119950,1000.);
#27239=VECTOR('',#119951,10.);
#27240=VECTOR('',#119954,1000.);
#27241=VECTOR('',#119957,10.);
#27242=VECTOR('',#119958,1000.);
#27243=VECTOR('',#119961,1000.);
#27244=VECTOR('',#119964,1000.);
#27245=VECTOR('',#119971,10.);
#27246=VECTOR('',#119972,1000.);
#27247=VECTOR('',#119973,10.);
#27248=VECTOR('',#119976,1000.);
#27249=VECTOR('',#119977,10.);
#27250=VECTOR('',#119980,1000.);
#27251=VECTOR('',#119983,10.);
#27252=VECTOR('',#119984,1000.);
#27253=VECTOR('',#119989,10.);
#27254=VECTOR('',#119990,1000.);
#27255=VECTOR('',#119991,10.);
#27256=VECTOR('',#119994,1000.);
#27257=VECTOR('',#119995,10.);
#27258=VECTOR('',#119998,1000.);
#27259=VECTOR('',#120001,10.);
#27260=VECTOR('',#120002,1000.);
#27261=VECTOR('',#125489,65.);
#27262=VECTOR('',#125494,64.008019903844);
#27263=VECTOR('',#125499,10.);
#27264=VECTOR('',#125502,10.);
#27265=VECTOR('',#125505,10.);
#27266=VECTOR('',#125508,10.);
#27267=VECTOR('',#125511,10.);
#27268=VECTOR('',#125514,10.);
#27269=VECTOR('',#125517,10.);
#27270=VECTOR('',#125520,10.);
#27271=VECTOR('',#125523,10.);
#27272=VECTOR('',#125526,10.);
#27273=VECTOR('',#125529,10.);
#27274=VECTOR('',#125532,10.);
#27275=VECTOR('',#125535,10.);
#27276=VECTOR('',#125538,10.);
#27277=VECTOR('',#125541,10.);
#27278=VECTOR('',#125544,10.);
#27279=VECTOR('',#125547,10.);
#27280=VECTOR('',#125550,10.);
#27281=VECTOR('',#125553,10.);
#27282=VECTOR('',#125556,10.);
#27283=VECTOR('',#125559,10.);
#27284=VECTOR('',#125562,10.);
#27285=VECTOR('',#125565,10.);
#27286=VECTOR('',#125568,10.);
#27287=VECTOR('',#125571,10.);
#27288=VECTOR('',#125574,10.);
#27289=VECTOR('',#125577,10.);
#27290=VECTOR('',#125580,10.);
#27291=VECTOR('',#125583,10.);
#27292=VECTOR('',#125586,10.);
#27293=VECTOR('',#125589,10.);
#27294=VECTOR('',#125592,10.);
#27295=VECTOR('',#125595,10.);
#27296=VECTOR('',#125598,10.);
#27297=VECTOR('',#125601,10.);
#27298=VECTOR('',#125604,10.);
#27299=VECTOR('',#125607,10.);
#27300=VECTOR('',#125610,10.);
#27301=VECTOR('',#125613,10.);
#27302=VECTOR('',#125616,10.);
#27303=VECTOR('',#125619,10.);
#27304=VECTOR('',#125622,10.);
#27305=VECTOR('',#125625,10.);
#27306=VECTOR('',#125628,10.);
#27307=VECTOR('',#125631,10.);
#27308=VECTOR('',#125634,10.);
#27309=VECTOR('',#125637,10.);
#27310=VECTOR('',#125640,10.);
#27311=VECTOR('',#125643,10.);
#27312=VECTOR('',#125646,10.);
#27313=VECTOR('',#125649,10.);
#27314=VECTOR('',#125652,10.);
#27315=VECTOR('',#125655,10.);
#27316=VECTOR('',#125658,10.);
#27317=VECTOR('',#125661,10.);
#27318=VECTOR('',#125664,10.);
#27319=VECTOR('',#125667,10.);
#27320=VECTOR('',#125670,10.);
#27321=VECTOR('',#125673,10.);
#27322=VECTOR('',#125676,10.);
#27323=VECTOR('',#125677,62.2224557307631);
#27324=VECTOR('',#125678,10.);
#27325=VECTOR('',#125681,10.);
#27326=VECTOR('',#125684,10.);
#27327=VECTOR('',#125687,10.);
#27328=VECTOR('',#125690,10.);
#27329=VECTOR('',#125693,10.);
#27330=VECTOR('',#125696,10.);
#27331=VECTOR('',#125699,10.);
#27332=VECTOR('',#125702,10.);
#27333=VECTOR('',#125705,10.);
#27334=VECTOR('',#125708,10.);
#27335=VECTOR('',#125711,10.);
#27336=VECTOR('',#125714,10.);
#27337=VECTOR('',#125717,10.);
#27338=VECTOR('',#125720,10.);
#27339=VECTOR('',#125723,10.);
#27340=VECTOR('',#125726,10.);
#27341=VECTOR('',#125729,10.);
#27342=VECTOR('',#125732,10.);
#27343=VECTOR('',#125735,10.);
#27344=VECTOR('',#125738,10.);
#27345=VECTOR('',#125741,10.);
#27346=VECTOR('',#125744,10.);
#27347=VECTOR('',#125747,10.);
#27348=VECTOR('',#125750,10.);
#27349=VECTOR('',#125753,10.);
#27350=VECTOR('',#125756,10.);
#27351=VECTOR('',#125759,10.);
#27352=VECTOR('',#125762,10.);
#27353=VECTOR('',#125765,10.);
#27354=VECTOR('',#125766,10.);
#27355=VECTOR('',#125769,10.);
#27356=VECTOR('',#125772,10.);
#27357=VECTOR('',#125775,10.);
#27358=VECTOR('',#125778,10.);
#27359=VECTOR('',#125781,10.);
#27360=VECTOR('',#125784,10.);
#27361=VECTOR('',#125787,10.);
#27362=VECTOR('',#125790,10.);
#27363=VECTOR('',#125793,10.);
#27364=VECTOR('',#125796,10.);
#27365=VECTOR('',#125799,10.);
#27366=VECTOR('',#125802,10.);
#27367=VECTOR('',#125805,10.);
#27368=VECTOR('',#125808,10.);
#27369=VECTOR('',#125811,10.);
#27370=VECTOR('',#125814,10.);
#27371=VECTOR('',#125817,10.);
#27372=VECTOR('',#125820,10.);
#27373=VECTOR('',#125823,10.);
#27374=VECTOR('',#125826,10.);
#27375=VECTOR('',#125829,10.);
#27376=VECTOR('',#125832,10.);
#27377=VECTOR('',#125835,10.);
#27378=VECTOR('',#125838,10.);
#27379=VECTOR('',#125841,10.);
#27380=VECTOR('',#125844,10.);
#27381=VECTOR('',#125847,10.);
#27382=VECTOR('',#125850,10.);
#27383=VECTOR('',#125853,10.);
#27384=VECTOR('',#125856,10.);
#27385=VECTOR('',#125859,10.);
#27386=VECTOR('',#125862,10.);
#27387=VECTOR('',#125865,10.);
#27388=VECTOR('',#125868,10.);
#27389=VECTOR('',#125871,10.);
#27390=VECTOR('',#125874,10.);
#27391=VECTOR('',#125877,10.);
#27392=VECTOR('',#125880,10.);
#27393=VECTOR('',#125883,10.);
#27394=VECTOR('',#125886,10.);
#27395=VECTOR('',#125889,10.);
#27396=VECTOR('',#125892,10.);
#27397=VECTOR('',#125895,10.);
#27398=VECTOR('',#125898,10.);
#27399=VECTOR('',#125901,10.);
#27400=VECTOR('',#125904,10.);
#27401=VECTOR('',#125907,10.);
#27402=VECTOR('',#125910,10.);
#27403=VECTOR('',#125913,10.);
#27404=VECTOR('',#125916,10.);
#27405=VECTOR('',#125919,10.);
#27406=VECTOR('',#125922,10.);
#27407=VECTOR('',#125925,10.);
#27408=VECTOR('',#125928,10.);
#27409=VECTOR('',#125931,10.);
#27410=VECTOR('',#125934,10.);
#27411=VECTOR('',#125937,10.);
#27412=VECTOR('',#125940,10.);
#27413=VECTOR('',#125943,10.);
#27414=VECTOR('',#125946,10.);
#27415=VECTOR('',#125949,10.);
#27416=VECTOR('',#125952,10.);
#27417=VECTOR('',#125955,10.);
#27418=VECTOR('',#125958,10.);
#27419=VECTOR('',#125961,10.);
#27420=VECTOR('',#125964,10.);
#27421=VECTOR('',#125967,10.);
#27422=VECTOR('',#125970,10.);
#27423=VECTOR('',#125973,10.);
#27424=VECTOR('',#125976,10.);
#27425=VECTOR('',#125979,10.);
#27426=VECTOR('',#125982,10.);
#27427=VECTOR('',#125985,10.);
#27428=VECTOR('',#125988,10.);
#27429=VECTOR('',#125991,10.);
#27430=VECTOR('',#125994,10.);
#27431=VECTOR('',#125997,10.);
#27432=VECTOR('',#126000,10.);
#27433=VECTOR('',#126003,10.);
#27434=VECTOR('',#126006,10.);
#27435=VECTOR('',#126009,10.);
#27436=VECTOR('',#126012,10.);
#27437=VECTOR('',#126015,10.);
#27438=VECTOR('',#126018,10.);
#27439=VECTOR('',#126021,10.);
#27440=VECTOR('',#126024,10.);
#27441=VECTOR('',#126027,10.);
#27442=VECTOR('',#126030,10.);
#27443=VECTOR('',#126033,10.);
#27444=VECTOR('',#126036,58.6605641730809);
#27445=VECTOR('',#126039,10.);
#27446=VECTOR('',#126042,10.);
#27447=VECTOR('',#126045,10.);
#27448=VECTOR('',#126048,10.);
#27449=VECTOR('',#126051,10.);
#27450=VECTOR('',#126054,10.);
#27451=VECTOR('',#126057,10.);
#27452=VECTOR('',#126060,10.);
#27453=VECTOR('',#126063,10.);
#27454=VECTOR('',#126066,10.);
#27455=VECTOR('',#126069,10.);
#27456=VECTOR('',#126072,10.);
#27457=VECTOR('',#126075,10.);
#27458=VECTOR('',#126078,10.);
#27459=VECTOR('',#126081,10.);
#27460=VECTOR('',#126084,10.);
#27461=VECTOR('',#126087,10.);
#27462=VECTOR('',#126090,10.);
#27463=VECTOR('',#126093,10.);
#27464=VECTOR('',#126096,10.);
#27465=VECTOR('',#126099,10.);
#27466=VECTOR('',#126102,10.);
#27467=VECTOR('',#126105,10.);
#27468=VECTOR('',#126108,10.);
#27469=VECTOR('',#126111,10.);
#27470=VECTOR('',#126114,10.);
#27471=VECTOR('',#126117,10.);
#27472=VECTOR('',#126120,10.);
#27473=VECTOR('',#126123,10.);
#27474=VECTOR('',#126126,10.);
#27475=VECTOR('',#126127,10.);
#27476=VECTOR('',#126130,10.);
#27477=VECTOR('',#126133,10.);
#27478=VECTOR('',#126136,10.);
#27479=VECTOR('',#126139,10.);
#27480=VECTOR('',#126142,10.);
#27481=VECTOR('',#126145,10.);
#27482=VECTOR('',#126148,10.);
#27483=VECTOR('',#126151,10.);
#27484=VECTOR('',#126154,10.);
#27485=VECTOR('',#126157,10.);
#27486=VECTOR('',#126160,10.);
#27487=VECTOR('',#126163,10.);
#27488=VECTOR('',#126166,10.);
#27489=VECTOR('',#126169,10.);
#27490=VECTOR('',#126172,10.);
#27491=VECTOR('',#126175,10.);
#27492=VECTOR('',#126178,10.);
#27493=VECTOR('',#126181,10.);
#27494=VECTOR('',#126184,10.);
#27495=VECTOR('',#126187,10.);
#27496=VECTOR('',#126190,10.);
#27497=VECTOR('',#126193,10.);
#27498=VECTOR('',#126196,10.);
#27499=VECTOR('',#126199,10.);
#27500=VECTOR('',#126202,10.);
#27501=VECTOR('',#126205,10.);
#27502=VECTOR('',#126208,10.);
#27503=VECTOR('',#126211,10.);
#27504=VECTOR('',#126214,10.);
#27505=VECTOR('',#126219,56.875);
#27506=VECTOR('',#126224,56.875);
#27507=VECTOR('',#126231,1000.);
#27508=VECTOR('',#126234,1000.);
#27509=VECTOR('',#126243,10.);
#27510=VECTOR('',#126244,10.);
#27511=VECTOR('',#126249,1000.);
#27512=VECTOR('',#126252,1000.);
#27513=VECTOR('',#126257,10.);
#27514=VECTOR('',#126260,10.);
#27515=VECTOR('',#126269,1000.);
#27516=VECTOR('',#126270,1000.);
#27517=VECTOR('',#126299,1000.);
#27518=VECTOR('',#126306,1000.);
#27519=VECTOR('',#126309,10.);
#27520=VECTOR('',#126312,10.);
#27521=VECTOR('',#126317,1000.);
#27522=VECTOR('',#126320,1000.);
#27523=VECTOR('',#126325,10.);
#27524=VECTOR('',#126332,10.);
#27525=VECTOR('',#126335,1000.);
#27526=VECTOR('',#126338,1000.);
#27527=VECTOR('',#126367,1000.);
#27528=VECTOR('',#126374,1000.);
#27529=VECTOR('',#126377,10.);
#27530=VECTOR('',#126380,10.);
#27531=VECTOR('',#126385,1000.);
#27532=VECTOR('',#126388,1000.);
#27533=VECTOR('',#126393,10.);
#27534=VECTOR('',#126400,10.);
#27535=VECTOR('',#126403,1000.);
#27536=VECTOR('',#126406,1000.);
#27537=VECTOR('',#126435,1000.);
#27538=VECTOR('',#126442,1000.);
#27539=VECTOR('',#126445,10.);
#27540=VECTOR('',#126448,10.);
#27541=VECTOR('',#126453,1000.);
#27542=VECTOR('',#126456,1000.);
#27543=VECTOR('',#126461,10.);
#27544=VECTOR('',#126468,10.);
#27545=VECTOR('',#126471,1000.);
#27546=VECTOR('',#126474,1000.);
#27547=VECTOR('',#126503,1000.);
#27548=VECTOR('',#126510,1000.);
#27549=VECTOR('',#126513,10.);
#27550=VECTOR('',#126516,10.);
#27551=VECTOR('',#126521,1000.);
#27552=VECTOR('',#126524,1000.);
#27553=VECTOR('',#126529,10.);
#27554=VECTOR('',#126536,10.);
#27555=VECTOR('',#126539,1000.);
#27556=VECTOR('',#126542,1000.);
#27557=VECTOR('',#126571,1000.);
#27558=VECTOR('',#126578,1000.);
#27559=VECTOR('',#126581,10.);
#27560=VECTOR('',#126584,10.);
#27561=VECTOR('',#126589,1000.);
#27562=VECTOR('',#126592,1000.);
#27563=VECTOR('',#126597,10.);
#27564=VECTOR('',#126604,10.);
#27565=VECTOR('',#126607,1000.);
#27566=VECTOR('',#126610,1000.);
#27567=VECTOR('',#126639,1000.);
#27568=VECTOR('',#126646,1000.);
#27569=VECTOR('',#126649,10.);
#27570=VECTOR('',#126652,10.);
#27571=VECTOR('',#126657,1000.);
#27572=VECTOR('',#126660,1000.);
#27573=VECTOR('',#126665,10.);
#27574=VECTOR('',#126672,10.);
#27575=VECTOR('',#126675,1000.);
#27576=VECTOR('',#126678,1000.);
#27577=VECTOR('',#126707,1000.);
#27578=VECTOR('',#126714,1000.);
#27579=VECTOR('',#126717,10.);
#27580=VECTOR('',#126720,10.);
#27581=VECTOR('',#126725,1000.);
#27582=VECTOR('',#126728,1000.);
#27583=VECTOR('',#126733,10.);
#27584=VECTOR('',#126740,10.);
#27585=VECTOR('',#126743,1000.);
#27586=VECTOR('',#126746,1000.);
#27587=VECTOR('',#126775,1000.);
#27588=VECTOR('',#126782,1000.);
#27589=VECTOR('',#126785,10.);
#27590=VECTOR('',#126788,10.);
#27591=VECTOR('',#126793,1000.);
#27592=VECTOR('',#126796,1000.);
#27593=VECTOR('',#126801,10.);
#27594=VECTOR('',#126808,10.);
#27595=VECTOR('',#126811,1000.);
#27596=VECTOR('',#126814,1000.);
#27597=VECTOR('',#126843,1000.);
#27598=VECTOR('',#126850,1000.);
#27599=VECTOR('',#126853,10.);
#27600=VECTOR('',#126856,10.);
#27601=VECTOR('',#126861,1000.);
#27602=VECTOR('',#126864,1000.);
#27603=VECTOR('',#126869,10.);
#27604=VECTOR('',#126876,10.);
#27605=VECTOR('',#126879,1000.);
#27606=VECTOR('',#126882,1000.);
#27607=VECTOR('',#126911,1000.);
#27608=VECTOR('',#126918,1000.);
#27609=VECTOR('',#126921,10.);
#27610=VECTOR('',#126924,10.);
#27611=VECTOR('',#126929,1000.);
#27612=VECTOR('',#126932,1000.);
#27613=VECTOR('',#126937,10.);
#27614=VECTOR('',#126944,10.);
#27615=VECTOR('',#126947,1000.);
#27616=VECTOR('',#126950,1000.);
#27617=VECTOR('',#126979,1000.);
#27618=VECTOR('',#126986,1000.);
#27619=VECTOR('',#126989,10.);
#27620=VECTOR('',#126992,10.);
#27621=VECTOR('',#126997,1000.);
#27622=VECTOR('',#127000,1000.);
#27623=VECTOR('',#127005,10.);
#27624=VECTOR('',#127012,10.);
#27625=VECTOR('',#127015,1000.);
#27626=VECTOR('',#127018,1000.);
#27627=VECTOR('',#127047,1000.);
#27628=VECTOR('',#127054,1000.);
#27629=VECTOR('',#127057,10.);
#27630=VECTOR('',#127060,10.);
#27631=VECTOR('',#127065,1000.);
#27632=VECTOR('',#127068,1000.);
#27633=VECTOR('',#127073,10.);
#27634=VECTOR('',#127080,10.);
#27635=VECTOR('',#127083,1000.);
#27636=VECTOR('',#127086,1000.);
#27637=VECTOR('',#127115,1000.);
#27638=VECTOR('',#127122,1000.);
#27639=VECTOR('',#127125,10.);
#27640=VECTOR('',#127128,10.);
#27641=VECTOR('',#127133,1000.);
#27642=VECTOR('',#127136,1000.);
#27643=VECTOR('',#127141,10.);
#27644=VECTOR('',#127148,10.);
#27645=VECTOR('',#127151,1000.);
#27646=VECTOR('',#127154,1000.);
#27647=VECTOR('',#127183,1000.);
#27648=VECTOR('',#127190,1000.);
#27649=VECTOR('',#127193,10.);
#27650=VECTOR('',#127196,10.);
#27651=VECTOR('',#127201,1000.);
#27652=VECTOR('',#127204,1000.);
#27653=VECTOR('',#127209,10.);
#27654=VECTOR('',#127216,10.);
#27655=VECTOR('',#127219,1000.);
#27656=VECTOR('',#127222,1000.);
#27657=VECTOR('',#127251,1000.);
#27658=VECTOR('',#127258,1000.);
#27659=VECTOR('',#127261,10.);
#27660=VECTOR('',#127264,10.);
#27661=VECTOR('',#127269,1000.);
#27662=VECTOR('',#127272,1000.);
#27663=VECTOR('',#127277,10.);
#27664=VECTOR('',#127284,10.);
#27665=VECTOR('',#127287,1000.);
#27666=VECTOR('',#127290,1000.);
#27667=VECTOR('',#127319,1000.);
#27668=VECTOR('',#127326,1000.);
#27669=VECTOR('',#127329,10.);
#27670=VECTOR('',#127332,10.);
#27671=VECTOR('',#127337,1000.);
#27672=VECTOR('',#127340,1000.);
#27673=VECTOR('',#127345,10.);
#27674=VECTOR('',#127352,10.);
#27675=VECTOR('',#127355,1000.);
#27676=VECTOR('',#127358,1000.);
#27677=VECTOR('',#127387,1000.);
#27678=VECTOR('',#127394,1000.);
#27679=VECTOR('',#127397,10.);
#27680=VECTOR('',#127400,10.);
#27681=VECTOR('',#127405,1000.);
#27682=VECTOR('',#127408,1000.);
#27683=VECTOR('',#127413,10.);
#27684=VECTOR('',#127420,10.);
#27685=VECTOR('',#127423,1000.);
#27686=VECTOR('',#127426,1000.);
#27687=VECTOR('',#127455,1000.);
#27688=VECTOR('',#127462,1000.);
#27689=VECTOR('',#127465,10.);
#27690=VECTOR('',#127468,10.);
#27691=VECTOR('',#127473,1000.);
#27692=VECTOR('',#127476,1000.);
#27693=VECTOR('',#127481,10.);
#27694=VECTOR('',#127488,10.);
#27695=VECTOR('',#127491,1000.);
#27696=VECTOR('',#127494,1000.);
#27697=VECTOR('',#127523,1000.);
#27698=VECTOR('',#127530,1000.);
#27699=VECTOR('',#127533,10.);
#27700=VECTOR('',#127536,10.);
#27701=VECTOR('',#127541,1000.);
#27702=VECTOR('',#127544,1000.);
#27703=VECTOR('',#127549,10.);
#27704=VECTOR('',#127556,10.);
#27705=VECTOR('',#127559,1000.);
#27706=VECTOR('',#127562,1000.);
#27707=VECTOR('',#127591,1000.);
#27708=VECTOR('',#127598,1000.);
#27709=VECTOR('',#127601,10.);
#27710=VECTOR('',#127604,10.);
#27711=VECTOR('',#127609,1000.);
#27712=VECTOR('',#127612,1000.);
#27713=VECTOR('',#127617,10.);
#27714=VECTOR('',#127624,10.);
#27715=VECTOR('',#127627,1000.);
#27716=VECTOR('',#127630,1000.);
#27717=VECTOR('',#127659,1000.);
#27718=VECTOR('',#127666,1000.);
#27719=VECTOR('',#127669,10.);
#27720=VECTOR('',#127672,10.);
#27721=VECTOR('',#127677,1000.);
#27722=VECTOR('',#127680,1000.);
#27723=VECTOR('',#127685,10.);
#27724=VECTOR('',#127692,10.);
#27725=VECTOR('',#127695,1000.);
#27726=VECTOR('',#127698,1000.);
#27727=VECTOR('',#127727,1000.);
#27728=VECTOR('',#127734,1000.);
#27729=VECTOR('',#127737,10.);
#27730=VECTOR('',#127740,10.);
#27731=VECTOR('',#127745,1000.);
#27732=VECTOR('',#127748,1000.);
#27733=VECTOR('',#127753,10.);
#27734=VECTOR('',#127760,10.);
#27735=VECTOR('',#127763,1000.);
#27736=VECTOR('',#127766,1000.);
#27737=VECTOR('',#127795,1000.);
#27738=VECTOR('',#127802,1000.);
#27739=VECTOR('',#127805,10.);
#27740=VECTOR('',#127808,10.);
#27741=VECTOR('',#127813,1000.);
#27742=VECTOR('',#127816,1000.);
#27743=VECTOR('',#127821,10.);
#27744=VECTOR('',#127828,10.);
#27745=VECTOR('',#127831,1000.);
#27746=VECTOR('',#127834,1000.);
#27747=VECTOR('',#127863,1000.);
#27748=VECTOR('',#127870,1000.);
#27749=VECTOR('',#127873,10.);
#27750=VECTOR('',#127876,10.);
#27751=VECTOR('',#127881,1000.);
#27752=VECTOR('',#127884,1000.);
#27753=VECTOR('',#127889,10.);
#27754=VECTOR('',#127896,10.);
#27755=VECTOR('',#127899,1000.);
#27756=VECTOR('',#127902,1000.);
#27757=VECTOR('',#127931,1000.);
#27758=VECTOR('',#127938,1000.);
#27759=VECTOR('',#127941,10.);
#27760=VECTOR('',#127944,10.);
#27761=VECTOR('',#127949,1000.);
#27762=VECTOR('',#127952,1000.);
#27763=VECTOR('',#127957,10.);
#27764=VECTOR('',#127964,10.);
#27765=VECTOR('',#127967,1000.);
#27766=VECTOR('',#127970,1000.);
#27767=VECTOR('',#127999,1000.);
#27768=VECTOR('',#128006,1000.);
#27769=VECTOR('',#128009,10.);
#27770=VECTOR('',#128012,10.);
#27771=VECTOR('',#128017,1000.);
#27772=VECTOR('',#128020,1000.);
#27773=VECTOR('',#128025,10.);
#27774=VECTOR('',#128032,10.);
#27775=VECTOR('',#128035,1000.);
#27776=VECTOR('',#128038,1000.);
#27777=VECTOR('',#128067,1000.);
#27778=VECTOR('',#128074,1000.);
#27779=VECTOR('',#128077,10.);
#27780=VECTOR('',#128080,10.);
#27781=VECTOR('',#128085,1000.);
#27782=VECTOR('',#128088,1000.);
#27783=VECTOR('',#128093,10.);
#27784=VECTOR('',#128100,10.);
#27785=VECTOR('',#128103,1000.);
#27786=VECTOR('',#128106,1000.);
#27787=VECTOR('',#128135,1000.);
#27788=VECTOR('',#128142,1000.);
#27789=VECTOR('',#128145,10.);
#27790=VECTOR('',#128148,10.);
#27791=VECTOR('',#128153,1000.);
#27792=VECTOR('',#128156,1000.);
#27793=VECTOR('',#128161,10.);
#27794=VECTOR('',#128168,10.);
#27795=VECTOR('',#128171,1000.);
#27796=VECTOR('',#128174,1000.);
#27797=VECTOR('',#128203,1000.);
#27798=VECTOR('',#128210,1000.);
#27799=VECTOR('',#128213,10.);
#27800=VECTOR('',#128216,10.);
#27801=VECTOR('',#128221,1000.);
#27802=VECTOR('',#128224,1000.);
#27803=VECTOR('',#128229,10.);
#27804=VECTOR('',#128236,10.);
#27805=VECTOR('',#128239,1000.);
#27806=VECTOR('',#128242,1000.);
#27807=VECTOR('',#128271,1000.);
#27808=VECTOR('',#128278,1000.);
#27809=VECTOR('',#128281,10.);
#27810=VECTOR('',#128284,10.);
#27811=VECTOR('',#128289,1000.);
#27812=VECTOR('',#128292,1000.);
#27813=VECTOR('',#128297,10.);
#27814=VECTOR('',#128304,10.);
#27815=VECTOR('',#128307,1000.);
#27816=VECTOR('',#128310,1000.);
#27817=VECTOR('',#128339,1000.);
#27818=VECTOR('',#128346,1000.);
#27819=VECTOR('',#128349,10.);
#27820=VECTOR('',#128352,10.);
#27821=VECTOR('',#128357,1000.);
#27822=VECTOR('',#128360,1000.);
#27823=VECTOR('',#128365,10.);
#27824=VECTOR('',#128372,10.);
#27825=VECTOR('',#128375,1000.);
#27826=VECTOR('',#128378,1000.);
#27827=VECTOR('',#128407,1000.);
#27828=VECTOR('',#128414,1000.);
#27829=VECTOR('',#128417,10.);
#27830=VECTOR('',#128420,10.);
#27831=VECTOR('',#128425,1000.);
#27832=VECTOR('',#128428,1000.);
#27833=VECTOR('',#128433,10.);
#27834=VECTOR('',#128440,10.);
#27835=VECTOR('',#128443,1000.);
#27836=VECTOR('',#128446,1000.);
#27837=VECTOR('',#128475,1000.);
#27838=VECTOR('',#128482,1000.);
#27839=VECTOR('',#128485,10.);
#27840=VECTOR('',#128488,10.);
#27841=VECTOR('',#128493,1000.);
#27842=VECTOR('',#128496,1000.);
#27843=VECTOR('',#128501,10.);
#27844=VECTOR('',#128508,10.);
#27845=VECTOR('',#128511,1000.);
#27846=VECTOR('',#128514,1000.);
#27847=VECTOR('',#128543,1000.);
#27848=VECTOR('',#128550,1000.);
#27849=VECTOR('',#128553,10.);
#27850=VECTOR('',#128556,10.);
#27851=VECTOR('',#128561,1000.);
#27852=VECTOR('',#128564,1000.);
#27853=VECTOR('',#128569,10.);
#27854=VECTOR('',#128576,10.);
#27855=VECTOR('',#128579,1000.);
#27856=VECTOR('',#128582,1000.);
#27857=VECTOR('',#128611,1000.);
#27858=VECTOR('',#128618,1000.);
#27859=VECTOR('',#128621,10.);
#27860=VECTOR('',#128624,10.);
#27861=VECTOR('',#128629,1000.);
#27862=VECTOR('',#128632,1000.);
#27863=VECTOR('',#128637,10.);
#27864=VECTOR('',#128644,10.);
#27865=VECTOR('',#128647,1000.);
#27866=VECTOR('',#128650,1000.);
#27867=VECTOR('',#128679,1000.);
#27868=VECTOR('',#128686,1000.);
#27869=VECTOR('',#128689,10.);
#27870=VECTOR('',#128692,10.);
#27871=VECTOR('',#128697,1000.);
#27872=VECTOR('',#128700,1000.);
#27873=VECTOR('',#128705,10.);
#27874=VECTOR('',#128712,10.);
#27875=VECTOR('',#128715,1000.);
#27876=VECTOR('',#128718,1000.);
#27877=VECTOR('',#128747,1000.);
#27878=VECTOR('',#128754,1000.);
#27879=VECTOR('',#128757,10.);
#27880=VECTOR('',#128760,10.);
#27881=VECTOR('',#128765,1000.);
#27882=VECTOR('',#128768,1000.);
#27883=VECTOR('',#128773,10.);
#27884=VECTOR('',#128780,10.);
#27885=VECTOR('',#128783,1000.);
#27886=VECTOR('',#128786,1000.);
#27887=VECTOR('',#128815,1000.);
#27888=VECTOR('',#128822,1000.);
#27889=VECTOR('',#128825,10.);
#27890=VECTOR('',#128828,10.);
#27891=VECTOR('',#128833,1000.);
#27892=VECTOR('',#128836,1000.);
#27893=VECTOR('',#128841,10.);
#27894=VECTOR('',#128848,10.);
#27895=VECTOR('',#128851,1000.);
#27896=VECTOR('',#128854,1000.);
#27897=VECTOR('',#128883,1000.);
#27898=VECTOR('',#128890,1000.);
#27899=VECTOR('',#128893,10.);
#27900=VECTOR('',#128896,10.);
#27901=VECTOR('',#128901,1000.);
#27902=VECTOR('',#128904,1000.);
#27903=VECTOR('',#128909,10.);
#27904=VECTOR('',#128916,10.);
#27905=VECTOR('',#128919,1000.);
#27906=VECTOR('',#128922,1000.);
#27907=VECTOR('',#128951,1000.);
#27908=VECTOR('',#128958,1000.);
#27909=VECTOR('',#128961,10.);
#27910=VECTOR('',#128964,10.);
#27911=VECTOR('',#128969,1000.);
#27912=VECTOR('',#128972,1000.);
#27913=VECTOR('',#128977,10.);
#27914=VECTOR('',#128984,10.);
#27915=VECTOR('',#128987,1000.);
#27916=VECTOR('',#128990,1000.);
#27917=VECTOR('',#129019,1000.);
#27918=VECTOR('',#129026,1000.);
#27919=VECTOR('',#129029,10.);
#27920=VECTOR('',#129032,10.);
#27921=VECTOR('',#129037,1000.);
#27922=VECTOR('',#129040,1000.);
#27923=VECTOR('',#129045,10.);
#27924=VECTOR('',#129052,10.);
#27925=VECTOR('',#129055,1000.);
#27926=VECTOR('',#129058,1000.);
#27927=VECTOR('',#129087,1000.);
#27928=VECTOR('',#129094,1000.);
#27929=VECTOR('',#129097,10.);
#27930=VECTOR('',#129100,10.);
#27931=VECTOR('',#129105,1000.);
#27932=VECTOR('',#129108,1000.);
#27933=VECTOR('',#129113,10.);
#27934=VECTOR('',#129120,10.);
#27935=VECTOR('',#129123,1000.);
#27936=VECTOR('',#129126,1000.);
#27937=VECTOR('',#129155,1000.);
#27938=VECTOR('',#129162,1000.);
#27939=VECTOR('',#129165,10.);
#27940=VECTOR('',#129168,10.);
#27941=VECTOR('',#129173,1000.);
#27942=VECTOR('',#129176,1000.);
#27943=VECTOR('',#129181,10.);
#27944=VECTOR('',#129188,10.);
#27945=VECTOR('',#129191,1000.);
#27946=VECTOR('',#129194,1000.);
#27947=VECTOR('',#129223,1000.);
#27948=VECTOR('',#129230,1000.);
#27949=VECTOR('',#129233,10.);
#27950=VECTOR('',#129236,10.);
#27951=VECTOR('',#129241,1000.);
#27952=VECTOR('',#129244,1000.);
#27953=VECTOR('',#129249,10.);
#27954=VECTOR('',#129256,10.);
#27955=VECTOR('',#129259,1000.);
#27956=VECTOR('',#129262,1000.);
#27957=VECTOR('',#129291,1000.);
#27958=VECTOR('',#129298,1000.);
#27959=VECTOR('',#129301,10.);
#27960=VECTOR('',#129304,10.);
#27961=VECTOR('',#129309,1000.);
#27962=VECTOR('',#129312,1000.);
#27963=VECTOR('',#129317,10.);
#27964=VECTOR('',#129324,10.);
#27965=VECTOR('',#129327,1000.);
#27966=VECTOR('',#129330,1000.);
#27967=VECTOR('',#129359,1000.);
#27968=VECTOR('',#129366,1000.);
#27969=VECTOR('',#129369,10.);
#27970=VECTOR('',#129372,10.);
#27971=VECTOR('',#129377,1000.);
#27972=VECTOR('',#129380,1000.);
#27973=VECTOR('',#129385,10.);
#27974=VECTOR('',#129392,10.);
#27975=VECTOR('',#129395,1000.);
#27976=VECTOR('',#129398,1000.);
#27977=VECTOR('',#129427,1000.);
#27978=VECTOR('',#129434,1000.);
#27979=VECTOR('',#129437,10.);
#27980=VECTOR('',#129440,10.);
#27981=VECTOR('',#129445,1000.);
#27982=VECTOR('',#129448,1000.);
#27983=VECTOR('',#129453,10.);
#27984=VECTOR('',#129460,10.);
#27985=VECTOR('',#129463,1000.);
#27986=VECTOR('',#129466,1000.);
#27987=VECTOR('',#129495,1000.);
#27988=VECTOR('',#129502,1000.);
#27989=VECTOR('',#129505,10.);
#27990=VECTOR('',#129508,10.);
#27991=VECTOR('',#129513,1000.);
#27992=VECTOR('',#129516,1000.);
#27993=VECTOR('',#129521,10.);
#27994=VECTOR('',#129528,10.);
#27995=VECTOR('',#129531,1000.);
#27996=VECTOR('',#129534,1000.);
#27997=VECTOR('',#129563,1000.);
#27998=VECTOR('',#129570,1000.);
#27999=VECTOR('',#129573,10.);
#28000=VECTOR('',#129576,10.);
#28001=VECTOR('',#129581,1000.);
#28002=VECTOR('',#129584,1000.);
#28003=VECTOR('',#129589,10.);
#28004=VECTOR('',#129596,10.);
#28005=VECTOR('',#129599,1000.);
#28006=VECTOR('',#129602,1000.);
#28007=VECTOR('',#129631,1000.);
#28008=VECTOR('',#129638,1000.);
#28009=VECTOR('',#129641,10.);
#28010=VECTOR('',#129644,10.);
#28011=VECTOR('',#129649,1000.);
#28012=VECTOR('',#129652,1000.);
#28013=VECTOR('',#129657,10.);
#28014=VECTOR('',#129664,10.);
#28015=VECTOR('',#129667,1000.);
#28016=VECTOR('',#129670,1000.);
#28017=VECTOR('',#129699,1000.);
#28018=VECTOR('',#129706,1000.);
#28019=VECTOR('',#129709,10.);
#28020=VECTOR('',#129712,10.);
#28021=VECTOR('',#129717,1000.);
#28022=VECTOR('',#129720,1000.);
#28023=VECTOR('',#129725,10.);
#28024=VECTOR('',#129732,10.);
#28025=VECTOR('',#129735,1000.);
#28026=VECTOR('',#129738,1000.);
#28027=VECTOR('',#129767,1000.);
#28028=VECTOR('',#129774,1000.);
#28029=VECTOR('',#129777,10.);
#28030=VECTOR('',#129780,10.);
#28031=VECTOR('',#129785,1000.);
#28032=VECTOR('',#129788,1000.);
#28033=VECTOR('',#129793,10.);
#28034=VECTOR('',#129800,10.);
#28035=VECTOR('',#129803,1000.);
#28036=VECTOR('',#129806,1000.);
#28037=VECTOR('',#129835,1000.);
#28038=VECTOR('',#129842,1000.);
#28039=VECTOR('',#129845,10.);
#28040=VECTOR('',#129848,10.);
#28041=VECTOR('',#129853,1000.);
#28042=VECTOR('',#129856,1000.);
#28043=VECTOR('',#129861,10.);
#28044=VECTOR('',#129868,10.);
#28045=VECTOR('',#129871,1000.);
#28046=VECTOR('',#129874,1000.);
#28047=VECTOR('',#129903,1000.);
#28048=VECTOR('',#129910,1000.);
#28049=VECTOR('',#129913,10.);
#28050=VECTOR('',#129916,10.);
#28051=VECTOR('',#129921,1000.);
#28052=VECTOR('',#129924,1000.);
#28053=VECTOR('',#129929,10.);
#28054=VECTOR('',#129936,10.);
#28055=VECTOR('',#129939,1000.);
#28056=VECTOR('',#129942,1000.);
#28057=VECTOR('',#129971,1000.);
#28058=VECTOR('',#129978,1000.);
#28059=VECTOR('',#129981,10.);
#28060=VECTOR('',#129984,10.);
#28061=VECTOR('',#129989,1000.);
#28062=VECTOR('',#129992,1000.);
#28063=VECTOR('',#129997,10.);
#28064=VECTOR('',#130004,10.);
#28065=VECTOR('',#130007,1000.);
#28066=VECTOR('',#130010,1000.);
#28067=VECTOR('',#130039,1000.);
#28068=VECTOR('',#130046,1000.);
#28069=VECTOR('',#130049,10.);
#28070=VECTOR('',#130052,10.);
#28071=VECTOR('',#130057,1000.);
#28072=VECTOR('',#130060,1000.);
#28073=VECTOR('',#130065,10.);
#28074=VECTOR('',#130072,10.);
#28075=VECTOR('',#130075,1000.);
#28076=VECTOR('',#130078,1000.);
#28077=VECTOR('',#130107,1000.);
#28078=VECTOR('',#130114,1000.);
#28079=VECTOR('',#130117,10.);
#28080=VECTOR('',#130120,10.);
#28081=VECTOR('',#130125,1000.);
#28082=VECTOR('',#130128,1000.);
#28083=VECTOR('',#130133,10.);
#28084=VECTOR('',#130140,10.);
#28085=VECTOR('',#130143,1000.);
#28086=VECTOR('',#130146,1000.);
#28087=VECTOR('',#130175,1000.);
#28088=VECTOR('',#130182,1000.);
#28089=VECTOR('',#130185,10.);
#28090=VECTOR('',#130188,10.);
#28091=VECTOR('',#130193,1000.);
#28092=VECTOR('',#130196,1000.);
#28093=VECTOR('',#130201,10.);
#28094=VECTOR('',#130208,10.);
#28095=VECTOR('',#130211,1000.);
#28096=VECTOR('',#130214,1000.);
#28097=VECTOR('',#130245,1000.);
#28098=VECTOR('',#130252,1000.);
#28099=VECTOR('',#130255,10.);
#28100=VECTOR('',#130258,10.);
#28101=VECTOR('',#130263,1000.);
#28102=VECTOR('',#130266,1000.);
#28103=VECTOR('',#130271,10.);
#28104=VECTOR('',#130278,10.);
#28105=VECTOR('',#130281,1000.);
#28106=VECTOR('',#130284,1000.);
#28107=VECTOR('',#130315,1000.);
#28108=VECTOR('',#130318,1000.);
#28109=VECTOR('',#130325,10.);
#28110=VECTOR('',#130326,1000.);
#28111=VECTOR('',#130327,10.);
#28112=VECTOR('',#130330,1000.);
#28113=VECTOR('',#130331,10.);
#28114=VECTOR('',#130334,1000.);
#28115=VECTOR('',#130337,10.);
#28116=VECTOR('',#130338,1000.);
#28117=VECTOR('',#130343,10.);
#28118=VECTOR('',#130344,1000.);
#28119=VECTOR('',#130345,10.);
#28120=VECTOR('',#130348,1000.);
#28121=VECTOR('',#130349,10.);
#28122=VECTOR('',#130352,1000.);
#28123=VECTOR('',#130355,10.);
#28124=VECTOR('',#130356,1000.);
#28125=VECTOR('',#130451,1000.);
#28126=VECTOR('',#130454,1000.);
#28127=VECTOR('',#130461,10.);
#28128=VECTOR('',#130462,1000.);
#28129=VECTOR('',#130463,10.);
#28130=VECTOR('',#130466,1000.);
#28131=VECTOR('',#130467,10.);
#28132=VECTOR('',#130470,1000.);
#28133=VECTOR('',#130473,10.);
#28134=VECTOR('',#130474,1000.);
#28135=VECTOR('',#130479,10.);
#28136=VECTOR('',#130480,1000.);
#28137=VECTOR('',#130481,10.);
#28138=VECTOR('',#130484,1000.);
#28139=VECTOR('',#130485,10.);
#28140=VECTOR('',#130488,1000.);
#28141=VECTOR('',#130491,10.);
#28142=VECTOR('',#130492,1000.);
#28143=VECTOR('',#130495,1000.);
#28144=VECTOR('',#130498,1000.);
#28145=VECTOR('',#130505,10.);
#28146=VECTOR('',#130506,1000.);
#28147=VECTOR('',#130507,10.);
#28148=VECTOR('',#130510,1000.);
#28149=VECTOR('',#130511,10.);
#28150=VECTOR('',#130514,1000.);
#28151=VECTOR('',#130517,10.);
#28152=VECTOR('',#130518,1000.);
#28153=VECTOR('',#130523,10.);
#28154=VECTOR('',#130524,1000.);
#28155=VECTOR('',#130525,10.);
#28156=VECTOR('',#130528,1000.);
#28157=VECTOR('',#130529,10.);
#28158=VECTOR('',#130532,1000.);
#28159=VECTOR('',#130535,10.);
#28160=VECTOR('',#130536,1000.);
#28161=VECTOR('',#130539,1000.);
#28162=VECTOR('',#130542,1000.);
#28163=VECTOR('',#130549,10.);
#28164=VECTOR('',#130550,1000.);
#28165=VECTOR('',#130551,10.);
#28166=VECTOR('',#130554,1000.);
#28167=VECTOR('',#130555,10.);
#28168=VECTOR('',#130558,1000.);
#28169=VECTOR('',#130561,10.);
#28170=VECTOR('',#130562,1000.);
#28171=VECTOR('',#130567,10.);
#28172=VECTOR('',#130568,1000.);
#28173=VECTOR('',#130569,10.);
#28174=VECTOR('',#130572,1000.);
#28175=VECTOR('',#130573,10.);
#28176=VECTOR('',#130576,1000.);
#28177=VECTOR('',#130579,10.);
#28178=VECTOR('',#130580,1000.);
#28179=VECTOR('',#130583,1000.);
#28180=VECTOR('',#130586,1000.);
#28181=VECTOR('',#130593,10.);
#28182=VECTOR('',#130594,1000.);
#28183=VECTOR('',#130595,10.);
#28184=VECTOR('',#130598,1000.);
#28185=VECTOR('',#130599,10.);
#28186=VECTOR('',#130602,1000.);
#28187=VECTOR('',#130605,10.);
#28188=VECTOR('',#130606,1000.);
#28189=VECTOR('',#130611,10.);
#28190=VECTOR('',#130612,1000.);
#28191=VECTOR('',#130613,10.);
#28192=VECTOR('',#130616,1000.);
#28193=VECTOR('',#130617,10.);
#28194=VECTOR('',#130620,1000.);
#28195=VECTOR('',#130623,10.);
#28196=VECTOR('',#130624,1000.);
#28197=VECTOR('',#130627,1000.);
#28198=VECTOR('',#130630,1000.);
#28199=VECTOR('',#130637,10.);
#28200=VECTOR('',#130638,1000.);
#28201=VECTOR('',#130639,10.);
#28202=VECTOR('',#130642,1000.);
#28203=VECTOR('',#130643,10.);
#28204=VECTOR('',#130646,1000.);
#28205=VECTOR('',#130649,10.);
#28206=VECTOR('',#130650,1000.);
#28207=VECTOR('',#130655,10.);
#28208=VECTOR('',#130656,1000.);
#28209=VECTOR('',#130657,10.);
#28210=VECTOR('',#130660,1000.);
#28211=VECTOR('',#130661,10.);
#28212=VECTOR('',#130664,1000.);
#28213=VECTOR('',#130667,10.);
#28214=VECTOR('',#130668,1000.);
#28215=VECTOR('',#130671,1000.);
#28216=VECTOR('',#130674,1000.);
#28217=VECTOR('',#130681,10.);
#28218=VECTOR('',#130682,1000.);
#28219=VECTOR('',#130683,10.);
#28220=VECTOR('',#130686,1000.);
#28221=VECTOR('',#130687,10.);
#28222=VECTOR('',#130690,1000.);
#28223=VECTOR('',#130693,10.);
#28224=VECTOR('',#130694,1000.);
#28225=VECTOR('',#130699,10.);
#28226=VECTOR('',#130700,1000.);
#28227=VECTOR('',#130701,10.);
#28228=VECTOR('',#130704,1000.);
#28229=VECTOR('',#130705,10.);
#28230=VECTOR('',#130708,1000.);
#28231=VECTOR('',#130711,10.);
#28232=VECTOR('',#130712,1000.);
#28233=VECTOR('',#130715,1000.);
#28234=VECTOR('',#130718,1000.);
#28235=VECTOR('',#130725,10.);
#28236=VECTOR('',#130726,1000.);
#28237=VECTOR('',#130727,10.);
#28238=VECTOR('',#130730,1000.);
#28239=VECTOR('',#130731,10.);
#28240=VECTOR('',#130734,1000.);
#28241=VECTOR('',#130737,10.);
#28242=VECTOR('',#130738,1000.);
#28243=VECTOR('',#130743,10.);
#28244=VECTOR('',#130744,1000.);
#28245=VECTOR('',#130745,10.);
#28246=VECTOR('',#130748,1000.);
#28247=VECTOR('',#130749,10.);
#28248=VECTOR('',#130752,1000.);
#28249=VECTOR('',#130755,10.);
#28250=VECTOR('',#130756,1000.);
#28251=VECTOR('',#130759,1000.);
#28252=VECTOR('',#130762,1000.);
#28253=VECTOR('',#130769,10.);
#28254=VECTOR('',#130770,1000.);
#28255=VECTOR('',#130771,10.);
#28256=VECTOR('',#130774,1000.);
#28257=VECTOR('',#130775,10.);
#28258=VECTOR('',#130778,1000.);
#28259=VECTOR('',#130781,10.);
#28260=VECTOR('',#130782,1000.);
#28261=VECTOR('',#130787,10.);
#28262=VECTOR('',#130788,1000.);
#28263=VECTOR('',#130789,10.);
#28264=VECTOR('',#130792,1000.);
#28265=VECTOR('',#130793,10.);
#28266=VECTOR('',#130796,1000.);
#28267=VECTOR('',#130799,10.);
#28268=VECTOR('',#130800,1000.);
#28269=VECTOR('',#130803,1000.);
#28270=VECTOR('',#130806,1000.);
#28271=VECTOR('',#130813,10.);
#28272=VECTOR('',#130814,1000.);
#28273=VECTOR('',#130815,10.);
#28274=VECTOR('',#130818,1000.);
#28275=VECTOR('',#130819,10.);
#28276=VECTOR('',#130822,1000.);
#28277=VECTOR('',#130825,10.);
#28278=VECTOR('',#130826,1000.);
#28279=VECTOR('',#130831,10.);
#28280=VECTOR('',#130832,1000.);
#28281=VECTOR('',#130833,10.);
#28282=VECTOR('',#130836,1000.);
#28283=VECTOR('',#130837,10.);
#28284=VECTOR('',#130840,1000.);
#28285=VECTOR('',#130843,10.);
#28286=VECTOR('',#130844,1000.);
#28287=VECTOR('',#130847,1000.);
#28288=VECTOR('',#130850,1000.);
#28289=VECTOR('',#130857,10.);
#28290=VECTOR('',#130858,1000.);
#28291=VECTOR('',#130859,10.);
#28292=VECTOR('',#130862,1000.);
#28293=VECTOR('',#130863,10.);
#28294=VECTOR('',#130866,1000.);
#28295=VECTOR('',#130869,10.);
#28296=VECTOR('',#130870,1000.);
#28297=VECTOR('',#130875,10.);
#28298=VECTOR('',#130876,1000.);
#28299=VECTOR('',#130877,10.);
#28300=VECTOR('',#130880,1000.);
#28301=VECTOR('',#130881,10.);
#28302=VECTOR('',#130884,1000.);
#28303=VECTOR('',#130887,10.);
#28304=VECTOR('',#130888,1000.);
#28305=VECTOR('',#130891,1000.);
#28306=VECTOR('',#130894,1000.);
#28307=VECTOR('',#130901,10.);
#28308=VECTOR('',#130902,1000.);
#28309=VECTOR('',#130903,10.);
#28310=VECTOR('',#130906,1000.);
#28311=VECTOR('',#130907,10.);
#28312=VECTOR('',#130910,1000.);
#28313=VECTOR('',#130913,10.);
#28314=VECTOR('',#130914,1000.);
#28315=VECTOR('',#130919,10.);
#28316=VECTOR('',#130920,1000.);
#28317=VECTOR('',#130921,10.);
#28318=VECTOR('',#130924,1000.);
#28319=VECTOR('',#130925,10.);
#28320=VECTOR('',#130928,1000.);
#28321=VECTOR('',#130931,10.);
#28322=VECTOR('',#130932,1000.);
#28323=VECTOR('',#130935,1000.);
#28324=VECTOR('',#130938,1000.);
#28325=VECTOR('',#130945,10.);
#28326=VECTOR('',#130946,1000.);
#28327=VECTOR('',#130947,10.);
#28328=VECTOR('',#130950,1000.);
#28329=VECTOR('',#130951,10.);
#28330=VECTOR('',#130954,1000.);
#28331=VECTOR('',#130957,10.);
#28332=VECTOR('',#130958,1000.);
#28333=VECTOR('',#130963,10.);
#28334=VECTOR('',#130964,1000.);
#28335=VECTOR('',#130965,10.);
#28336=VECTOR('',#130968,1000.);
#28337=VECTOR('',#130969,10.);
#28338=VECTOR('',#130972,1000.);
#28339=VECTOR('',#130975,10.);
#28340=VECTOR('',#130976,1000.);
#28341=VECTOR('',#130979,1000.);
#28342=VECTOR('',#130982,1000.);
#28343=VECTOR('',#130989,10.);
#28344=VECTOR('',#130990,1000.);
#28345=VECTOR('',#130991,10.);
#28346=VECTOR('',#130994,1000.);
#28347=VECTOR('',#130995,10.);
#28348=VECTOR('',#130998,1000.);
#28349=VECTOR('',#131001,10.);
#28350=VECTOR('',#131002,1000.);
#28351=VECTOR('',#131007,10.);
#28352=VECTOR('',#131008,1000.);
#28353=VECTOR('',#131009,10.);
#28354=VECTOR('',#131012,1000.);
#28355=VECTOR('',#131013,10.);
#28356=VECTOR('',#131016,1000.);
#28357=VECTOR('',#131019,10.);
#28358=VECTOR('',#131020,1000.);
#28359=VECTOR('',#131023,1000.);
#28360=VECTOR('',#131026,1000.);
#28361=VECTOR('',#131033,10.);
#28362=VECTOR('',#131034,1000.);
#28363=VECTOR('',#131035,10.);
#28364=VECTOR('',#131038,1000.);
#28365=VECTOR('',#131039,10.);
#28366=VECTOR('',#131042,1000.);
#28367=VECTOR('',#131045,10.);
#28368=VECTOR('',#131046,1000.);
#28369=VECTOR('',#131051,10.);
#28370=VECTOR('',#131052,1000.);
#28371=VECTOR('',#131053,10.);
#28372=VECTOR('',#131056,1000.);
#28373=VECTOR('',#131057,10.);
#28374=VECTOR('',#131060,1000.);
#28375=VECTOR('',#131063,10.);
#28376=VECTOR('',#131064,1000.);
#28377=VECTOR('',#131067,1000.);
#28378=VECTOR('',#131070,1000.);
#28379=VECTOR('',#131077,10.);
#28380=VECTOR('',#131078,1000.);
#28381=VECTOR('',#131079,10.);
#28382=VECTOR('',#131082,1000.);
#28383=VECTOR('',#131083,10.);
#28384=VECTOR('',#131086,1000.);
#28385=VECTOR('',#131089,10.);
#28386=VECTOR('',#131090,1000.);
#28387=VECTOR('',#131095,10.);
#28388=VECTOR('',#131096,1000.);
#28389=VECTOR('',#131097,10.);
#28390=VECTOR('',#131100,1000.);
#28391=VECTOR('',#131101,10.);
#28392=VECTOR('',#131104,1000.);
#28393=VECTOR('',#131107,10.);
#28394=VECTOR('',#131108,1000.);
#28395=VECTOR('',#131111,1000.);
#28396=VECTOR('',#131114,1000.);
#28397=VECTOR('',#131121,10.);
#28398=VECTOR('',#131122,1000.);
#28399=VECTOR('',#131123,10.);
#28400=VECTOR('',#131126,1000.);
#28401=VECTOR('',#131127,10.);
#28402=VECTOR('',#131130,1000.);
#28403=VECTOR('',#131133,10.);
#28404=VECTOR('',#131134,1000.);
#28405=VECTOR('',#131139,10.);
#28406=VECTOR('',#131140,1000.);
#28407=VECTOR('',#131141,10.);
#28408=VECTOR('',#131144,1000.);
#28409=VECTOR('',#131145,10.);
#28410=VECTOR('',#131148,1000.);
#28411=VECTOR('',#131151,10.);
#28412=VECTOR('',#131152,1000.);
#28413=VECTOR('',#131155,1000.);
#28414=VECTOR('',#131158,1000.);
#28415=VECTOR('',#131165,10.);
#28416=VECTOR('',#131166,1000.);
#28417=VECTOR('',#131167,10.);
#28418=VECTOR('',#131170,1000.);
#28419=VECTOR('',#131171,10.);
#28420=VECTOR('',#131174,1000.);
#28421=VECTOR('',#131177,10.);
#28422=VECTOR('',#131178,1000.);
#28423=VECTOR('',#131183,10.);
#28424=VECTOR('',#131184,1000.);
#28425=VECTOR('',#131185,10.);
#28426=VECTOR('',#131188,1000.);
#28427=VECTOR('',#131189,10.);
#28428=VECTOR('',#131192,1000.);
#28429=VECTOR('',#131195,10.);
#28430=VECTOR('',#131196,1000.);
#28431=VECTOR('',#131199,1000.);
#28432=VECTOR('',#131202,1000.);
#28433=VECTOR('',#131209,10.);
#28434=VECTOR('',#131210,1000.);
#28435=VECTOR('',#131211,10.);
#28436=VECTOR('',#131214,1000.);
#28437=VECTOR('',#131215,10.);
#28438=VECTOR('',#131218,1000.);
#28439=VECTOR('',#131221,10.);
#28440=VECTOR('',#131222,1000.);
#28441=VECTOR('',#131227,10.);
#28442=VECTOR('',#131228,1000.);
#28443=VECTOR('',#131229,10.);
#28444=VECTOR('',#131232,1000.);
#28445=VECTOR('',#131233,10.);
#28446=VECTOR('',#131236,1000.);
#28447=VECTOR('',#131239,10.);
#28448=VECTOR('',#131240,1000.);
#28449=VECTOR('',#131243,1000.);
#28450=VECTOR('',#131246,1000.);
#28451=VECTOR('',#131253,10.);
#28452=VECTOR('',#131254,1000.);
#28453=VECTOR('',#131255,10.);
#28454=VECTOR('',#131258,1000.);
#28455=VECTOR('',#131259,10.);
#28456=VECTOR('',#131262,1000.);
#28457=VECTOR('',#131265,10.);
#28458=VECTOR('',#131266,1000.);
#28459=VECTOR('',#131271,10.);
#28460=VECTOR('',#131272,1000.);
#28461=VECTOR('',#131273,10.);
#28462=VECTOR('',#131276,1000.);
#28463=VECTOR('',#131277,10.);
#28464=VECTOR('',#131280,1000.);
#28465=VECTOR('',#131283,10.);
#28466=VECTOR('',#131284,1000.);
#28467=VECTOR('',#131287,1000.);
#28468=VECTOR('',#131290,1000.);
#28469=VECTOR('',#131297,10.);
#28470=VECTOR('',#131298,1000.);
#28471=VECTOR('',#131299,10.);
#28472=VECTOR('',#131302,1000.);
#28473=VECTOR('',#131303,10.);
#28474=VECTOR('',#131306,1000.);
#28475=VECTOR('',#131309,10.);
#28476=VECTOR('',#131310,1000.);
#28477=VECTOR('',#131315,10.);
#28478=VECTOR('',#131316,1000.);
#28479=VECTOR('',#131317,10.);
#28480=VECTOR('',#131320,1000.);
#28481=VECTOR('',#131321,10.);
#28482=VECTOR('',#131324,1000.);
#28483=VECTOR('',#131327,10.);
#28484=VECTOR('',#131328,1000.);
#28485=VECTOR('',#131331,1000.);
#28486=VECTOR('',#131334,1000.);
#28487=VECTOR('',#131341,10.);
#28488=VECTOR('',#131342,1000.);
#28489=VECTOR('',#131343,10.);
#28490=VECTOR('',#131346,1000.);
#28491=VECTOR('',#131347,10.);
#28492=VECTOR('',#131350,1000.);
#28493=VECTOR('',#131353,10.);
#28494=VECTOR('',#131354,1000.);
#28495=VECTOR('',#131359,10.);
#28496=VECTOR('',#131360,1000.);
#28497=VECTOR('',#131361,10.);
#28498=VECTOR('',#131364,1000.);
#28499=VECTOR('',#131365,10.);
#28500=VECTOR('',#131368,1000.);
#28501=VECTOR('',#131371,10.);
#28502=VECTOR('',#131372,1000.);
#28503=VECTOR('',#131375,1000.);
#28504=VECTOR('',#131378,1000.);
#28505=VECTOR('',#131385,10.);
#28506=VECTOR('',#131386,1000.);
#28507=VECTOR('',#131387,10.);
#28508=VECTOR('',#131390,1000.);
#28509=VECTOR('',#131391,10.);
#28510=VECTOR('',#131394,1000.);
#28511=VECTOR('',#131397,10.);
#28512=VECTOR('',#131398,1000.);
#28513=VECTOR('',#131403,10.);
#28514=VECTOR('',#131404,1000.);
#28515=VECTOR('',#131405,10.);
#28516=VECTOR('',#131408,1000.);
#28517=VECTOR('',#131409,10.);
#28518=VECTOR('',#131412,1000.);
#28519=VECTOR('',#131415,10.);
#28520=VECTOR('',#131416,1000.);
#28521=VECTOR('',#131419,1000.);
#28522=VECTOR('',#131422,1000.);
#28523=VECTOR('',#131429,10.);
#28524=VECTOR('',#131430,1000.);
#28525=VECTOR('',#131431,10.);
#28526=VECTOR('',#131434,1000.);
#28527=VECTOR('',#131435,10.);
#28528=VECTOR('',#131438,1000.);
#28529=VECTOR('',#131441,10.);
#28530=VECTOR('',#131442,1000.);
#28531=VECTOR('',#131447,10.);
#28532=VECTOR('',#131448,1000.);
#28533=VECTOR('',#131449,10.);
#28534=VECTOR('',#131452,1000.);
#28535=VECTOR('',#131453,10.);
#28536=VECTOR('',#131456,1000.);
#28537=VECTOR('',#131459,10.);
#28538=VECTOR('',#131460,1000.);
#28539=VECTOR('',#131463,1000.);
#28540=VECTOR('',#131466,1000.);
#28541=VECTOR('',#131473,10.);
#28542=VECTOR('',#131474,1000.);
#28543=VECTOR('',#131475,10.);
#28544=VECTOR('',#131478,1000.);
#28545=VECTOR('',#131479,10.);
#28546=VECTOR('',#131482,1000.);
#28547=VECTOR('',#131485,10.);
#28548=VECTOR('',#131486,1000.);
#28549=VECTOR('',#131491,10.);
#28550=VECTOR('',#131492,1000.);
#28551=VECTOR('',#131493,10.);
#28552=VECTOR('',#131496,1000.);
#28553=VECTOR('',#131497,10.);
#28554=VECTOR('',#131500,1000.);
#28555=VECTOR('',#131503,10.);
#28556=VECTOR('',#131504,1000.);
#28557=VECTOR('',#131507,1000.);
#28558=VECTOR('',#131510,1000.);
#28559=VECTOR('',#131517,10.);
#28560=VECTOR('',#131518,1000.);
#28561=VECTOR('',#131519,10.);
#28562=VECTOR('',#131522,1000.);
#28563=VECTOR('',#131523,10.);
#28564=VECTOR('',#131526,1000.);
#28565=VECTOR('',#131529,10.);
#28566=VECTOR('',#131530,1000.);
#28567=VECTOR('',#131535,10.);
#28568=VECTOR('',#131536,1000.);
#28569=VECTOR('',#131537,10.);
#28570=VECTOR('',#131540,1000.);
#28571=VECTOR('',#131541,10.);
#28572=VECTOR('',#131544,1000.);
#28573=VECTOR('',#131547,10.);
#28574=VECTOR('',#131548,1000.);
#28575=VECTOR('',#131551,1000.);
#28576=VECTOR('',#131554,1000.);
#28577=VECTOR('',#131561,10.);
#28578=VECTOR('',#131562,1000.);
#28579=VECTOR('',#131563,10.);
#28580=VECTOR('',#131566,1000.);
#28581=VECTOR('',#131567,10.);
#28582=VECTOR('',#131570,1000.);
#28583=VECTOR('',#131573,10.);
#28584=VECTOR('',#131574,1000.);
#28585=VECTOR('',#131579,10.);
#28586=VECTOR('',#131580,1000.);
#28587=VECTOR('',#131581,10.);
#28588=VECTOR('',#131584,1000.);
#28589=VECTOR('',#131585,10.);
#28590=VECTOR('',#131588,1000.);
#28591=VECTOR('',#131591,10.);
#28592=VECTOR('',#131592,1000.);
#28593=VECTOR('',#131595,1000.);
#28594=VECTOR('',#131598,1000.);
#28595=VECTOR('',#131605,10.);
#28596=VECTOR('',#131606,1000.);
#28597=VECTOR('',#131607,10.);
#28598=VECTOR('',#131610,1000.);
#28599=VECTOR('',#131611,10.);
#28600=VECTOR('',#131614,1000.);
#28601=VECTOR('',#131617,10.);
#28602=VECTOR('',#131618,1000.);
#28603=VECTOR('',#131623,10.);
#28604=VECTOR('',#131624,1000.);
#28605=VECTOR('',#131625,10.);
#28606=VECTOR('',#131628,1000.);
#28607=VECTOR('',#131629,10.);
#28608=VECTOR('',#131632,1000.);
#28609=VECTOR('',#131635,10.);
#28610=VECTOR('',#131636,1000.);
#28611=VECTOR('',#131639,1000.);
#28612=VECTOR('',#131642,1000.);
#28613=VECTOR('',#131649,10.);
#28614=VECTOR('',#131650,1000.);
#28615=VECTOR('',#131651,10.);
#28616=VECTOR('',#131654,1000.);
#28617=VECTOR('',#131655,10.);
#28618=VECTOR('',#131658,1000.);
#28619=VECTOR('',#131661,10.);
#28620=VECTOR('',#131662,1000.);
#28621=VECTOR('',#131667,10.);
#28622=VECTOR('',#131668,1000.);
#28623=VECTOR('',#131669,10.);
#28624=VECTOR('',#131672,1000.);
#28625=VECTOR('',#131673,10.);
#28626=VECTOR('',#131676,1000.);
#28627=VECTOR('',#131679,10.);
#28628=VECTOR('',#131680,1000.);
#28629=VECTOR('',#131683,1000.);
#28630=VECTOR('',#131686,1000.);
#28631=VECTOR('',#131693,10.);
#28632=VECTOR('',#131694,1000.);
#28633=VECTOR('',#131695,10.);
#28634=VECTOR('',#131698,1000.);
#28635=VECTOR('',#131699,10.);
#28636=VECTOR('',#131702,1000.);
#28637=VECTOR('',#131705,10.);
#28638=VECTOR('',#131706,1000.);
#28639=VECTOR('',#131711,10.);
#28640=VECTOR('',#131712,1000.);
#28641=VECTOR('',#131713,10.);
#28642=VECTOR('',#131716,1000.);
#28643=VECTOR('',#131717,10.);
#28644=VECTOR('',#131720,1000.);
#28645=VECTOR('',#131723,10.);
#28646=VECTOR('',#131724,1000.);
#28647=VECTOR('',#131727,1000.);
#28648=VECTOR('',#131728,1000.);
#28649=VECTOR('',#131733,10.);
#28650=VECTOR('',#131734,1000.);
#28651=VECTOR('',#131735,10.);
#28652=VECTOR('',#131738,1000.);
#28653=VECTOR('',#131739,10.);
#28654=VECTOR('',#131742,1000.);
#28655=VECTOR('',#131745,10.);
#28656=VECTOR('',#131746,1000.);
#28657=VECTOR('',#131751,10.);
#28658=VECTOR('',#131752,1000.);
#28659=VECTOR('',#131753,10.);
#28660=VECTOR('',#131756,1000.);
#28661=VECTOR('',#131757,10.);
#28662=VECTOR('',#131760,1000.);
#28663=VECTOR('',#131763,10.);
#28664=VECTOR('',#131764,1000.);
#28665=VECTOR('',#131767,1000.);
#28666=VECTOR('',#131770,1000.);
#28667=VECTOR('',#131777,10.);
#28668=VECTOR('',#131778,1000.);
#28669=VECTOR('',#131779,10.);
#28670=VECTOR('',#131782,1000.);
#28671=VECTOR('',#131783,10.);
#28672=VECTOR('',#131786,1000.);
#28673=VECTOR('',#131789,10.);
#28674=VECTOR('',#131790,1000.);
#28675=VECTOR('',#131795,10.);
#28676=VECTOR('',#131796,1000.);
#28677=VECTOR('',#131797,10.);
#28678=VECTOR('',#131800,1000.);
#28679=VECTOR('',#131801,10.);
#28680=VECTOR('',#131804,1000.);
#28681=VECTOR('',#131807,10.);
#28682=VECTOR('',#131808,1000.);
#28683=VECTOR('',#131811,1000.);
#28684=VECTOR('',#131814,1000.);
#28685=VECTOR('',#131821,10.);
#28686=VECTOR('',#131822,1000.);
#28687=VECTOR('',#131823,10.);
#28688=VECTOR('',#131826,1000.);
#28689=VECTOR('',#131827,10.);
#28690=VECTOR('',#131830,1000.);
#28691=VECTOR('',#131833,10.);
#28692=VECTOR('',#131834,1000.);
#28693=VECTOR('',#131839,10.);
#28694=VECTOR('',#131840,1000.);
#28695=VECTOR('',#131841,10.);
#28696=VECTOR('',#131844,1000.);
#28697=VECTOR('',#131845,10.);
#28698=VECTOR('',#131848,1000.);
#28699=VECTOR('',#131851,10.);
#28700=VECTOR('',#131852,1000.);
#28701=VECTOR('',#131855,1000.);
#28702=VECTOR('',#131858,1000.);
#28703=VECTOR('',#131865,10.);
#28704=VECTOR('',#131866,1000.);
#28705=VECTOR('',#131867,10.);
#28706=VECTOR('',#131870,1000.);
#28707=VECTOR('',#131871,10.);
#28708=VECTOR('',#131874,1000.);
#28709=VECTOR('',#131877,10.);
#28710=VECTOR('',#131878,1000.);
#28711=VECTOR('',#131883,10.);
#28712=VECTOR('',#131884,1000.);
#28713=VECTOR('',#131885,10.);
#28714=VECTOR('',#131888,1000.);
#28715=VECTOR('',#131889,10.);
#28716=VECTOR('',#131892,1000.);
#28717=VECTOR('',#131895,10.);
#28718=VECTOR('',#131896,1000.);
#28719=VECTOR('',#131899,1000.);
#28720=VECTOR('',#131902,1000.);
#28721=VECTOR('',#131909,10.);
#28722=VECTOR('',#131910,1000.);
#28723=VECTOR('',#131911,10.);
#28724=VECTOR('',#131914,1000.);
#28725=VECTOR('',#131915,10.);
#28726=VECTOR('',#131918,1000.);
#28727=VECTOR('',#131921,10.);
#28728=VECTOR('',#131922,1000.);
#28729=VECTOR('',#131927,10.);
#28730=VECTOR('',#131928,1000.);
#28731=VECTOR('',#131929,10.);
#28732=VECTOR('',#131932,1000.);
#28733=VECTOR('',#131933,10.);
#28734=VECTOR('',#131936,1000.);
#28735=VECTOR('',#131939,10.);
#28736=VECTOR('',#131940,1000.);
#28737=VECTOR('',#131943,1000.);
#28738=VECTOR('',#131946,1000.);
#28739=VECTOR('',#131953,10.);
#28740=VECTOR('',#131954,1000.);
#28741=VECTOR('',#131955,10.);
#28742=VECTOR('',#131958,1000.);
#28743=VECTOR('',#131959,10.);
#28744=VECTOR('',#131962,1000.);
#28745=VECTOR('',#131965,10.);
#28746=VECTOR('',#131966,1000.);
#28747=VECTOR('',#131971,10.);
#28748=VECTOR('',#131972,1000.);
#28749=VECTOR('',#131973,10.);
#28750=VECTOR('',#131976,1000.);
#28751=VECTOR('',#131977,10.);
#28752=VECTOR('',#131980,1000.);
#28753=VECTOR('',#131983,10.);
#28754=VECTOR('',#131984,1000.);
#28755=VECTOR('',#131987,1000.);
#28756=VECTOR('',#131990,1000.);
#28757=VECTOR('',#131997,10.);
#28758=VECTOR('',#131998,1000.);
#28759=VECTOR('',#131999,10.);
#28760=VECTOR('',#132002,1000.);
#28761=VECTOR('',#132003,10.);
#28762=VECTOR('',#132006,1000.);
#28763=VECTOR('',#132009,10.);
#28764=VECTOR('',#132010,1000.);
#28765=VECTOR('',#132015,10.);
#28766=VECTOR('',#132016,1000.);
#28767=VECTOR('',#132017,10.);
#28768=VECTOR('',#132020,1000.);
#28769=VECTOR('',#132021,10.);
#28770=VECTOR('',#132024,1000.);
#28771=VECTOR('',#132027,10.);
#28772=VECTOR('',#132028,1000.);
#28773=VECTOR('',#132031,1000.);
#28774=VECTOR('',#132034,1000.);
#28775=VECTOR('',#132041,10.);
#28776=VECTOR('',#132042,1000.);
#28777=VECTOR('',#132043,10.);
#28778=VECTOR('',#132046,1000.);
#28779=VECTOR('',#132047,10.);
#28780=VECTOR('',#132050,1000.);
#28781=VECTOR('',#132053,10.);
#28782=VECTOR('',#132054,1000.);
#28783=VECTOR('',#132059,10.);
#28784=VECTOR('',#132060,1000.);
#28785=VECTOR('',#132061,10.);
#28786=VECTOR('',#132064,1000.);
#28787=VECTOR('',#132065,10.);
#28788=VECTOR('',#132068,1000.);
#28789=VECTOR('',#132071,10.);
#28790=VECTOR('',#132072,1000.);
#28791=VECTOR('',#132075,1000.);
#28792=VECTOR('',#132078,1000.);
#28793=VECTOR('',#132085,10.);
#28794=VECTOR('',#132086,1000.);
#28795=VECTOR('',#132087,10.);
#28796=VECTOR('',#132090,1000.);
#28797=VECTOR('',#132091,10.);
#28798=VECTOR('',#132094,1000.);
#28799=VECTOR('',#132097,10.);
#28800=VECTOR('',#132098,1000.);
#28801=VECTOR('',#132103,10.);
#28802=VECTOR('',#132104,1000.);
#28803=VECTOR('',#132105,10.);
#28804=VECTOR('',#132108,1000.);
#28805=VECTOR('',#132109,10.);
#28806=VECTOR('',#132112,1000.);
#28807=VECTOR('',#132115,10.);
#28808=VECTOR('',#132116,1000.);
#28809=VECTOR('',#132119,1000.);
#28810=VECTOR('',#132122,1000.);
#28811=VECTOR('',#132129,10.);
#28812=VECTOR('',#132130,1000.);
#28813=VECTOR('',#132131,10.);
#28814=VECTOR('',#132134,1000.);
#28815=VECTOR('',#132135,10.);
#28816=VECTOR('',#132138,1000.);
#28817=VECTOR('',#132141,10.);
#28818=VECTOR('',#132142,1000.);
#28819=VECTOR('',#132147,10.);
#28820=VECTOR('',#132148,1000.);
#28821=VECTOR('',#132149,10.);
#28822=VECTOR('',#132152,1000.);
#28823=VECTOR('',#132153,10.);
#28824=VECTOR('',#132156,1000.);
#28825=VECTOR('',#132159,10.);
#28826=VECTOR('',#132160,1000.);
#28827=VECTOR('',#132163,1000.);
#28828=VECTOR('',#132166,1000.);
#28829=VECTOR('',#132173,10.);
#28830=VECTOR('',#132174,1000.);
#28831=VECTOR('',#132175,10.);
#28832=VECTOR('',#132178,1000.);
#28833=VECTOR('',#132179,10.);
#28834=VECTOR('',#132182,1000.);
#28835=VECTOR('',#132185,10.);
#28836=VECTOR('',#132186,1000.);
#28837=VECTOR('',#132191,10.);
#28838=VECTOR('',#132192,1000.);
#28839=VECTOR('',#132193,10.);
#28840=VECTOR('',#132196,1000.);
#28841=VECTOR('',#132197,10.);
#28842=VECTOR('',#132200,1000.);
#28843=VECTOR('',#132203,10.);
#28844=VECTOR('',#132204,1000.);
#28845=VECTOR('',#132207,1000.);
#28846=VECTOR('',#132210,1000.);
#28847=VECTOR('',#132217,10.);
#28848=VECTOR('',#132218,1000.);
#28849=VECTOR('',#132219,10.);
#28850=VECTOR('',#132222,1000.);
#28851=VECTOR('',#132223,10.);
#28852=VECTOR('',#132226,1000.);
#28853=VECTOR('',#132229,10.);
#28854=VECTOR('',#132230,1000.);
#28855=VECTOR('',#132235,10.);
#28856=VECTOR('',#132236,1000.);
#28857=VECTOR('',#132237,10.);
#28858=VECTOR('',#132240,1000.);
#28859=VECTOR('',#132241,10.);
#28860=VECTOR('',#132244,1000.);
#28861=VECTOR('',#132247,10.);
#28862=VECTOR('',#132248,1000.);
#28863=VECTOR('',#132251,1000.);
#28864=VECTOR('',#132254,1000.);
#28865=VECTOR('',#132261,10.);
#28866=VECTOR('',#132262,1000.);
#28867=VECTOR('',#132263,10.);
#28868=VECTOR('',#132266,1000.);
#28869=VECTOR('',#132267,10.);
#28870=VECTOR('',#132270,1000.);
#28871=VECTOR('',#132273,10.);
#28872=VECTOR('',#132274,1000.);
#28873=VECTOR('',#132279,10.);
#28874=VECTOR('',#132280,1000.);
#28875=VECTOR('',#132281,10.);
#28876=VECTOR('',#132284,1000.);
#28877=VECTOR('',#132285,10.);
#28878=VECTOR('',#132288,1000.);
#28879=VECTOR('',#132291,10.);
#28880=VECTOR('',#132292,1000.);
#28881=VECTOR('',#132295,1000.);
#28882=VECTOR('',#132298,1000.);
#28883=VECTOR('',#132305,10.);
#28884=VECTOR('',#132306,1000.);
#28885=VECTOR('',#132307,10.);
#28886=VECTOR('',#132310,1000.);
#28887=VECTOR('',#132311,10.);
#28888=VECTOR('',#132314,1000.);
#28889=VECTOR('',#132317,10.);
#28890=VECTOR('',#132318,1000.);
#28891=VECTOR('',#132323,10.);
#28892=VECTOR('',#132324,1000.);
#28893=VECTOR('',#132325,10.);
#28894=VECTOR('',#132328,1000.);
#28895=VECTOR('',#132329,10.);
#28896=VECTOR('',#132332,1000.);
#28897=VECTOR('',#132335,10.);
#28898=VECTOR('',#132336,1000.);
#28899=VECTOR('',#132339,1000.);
#28900=VECTOR('',#132342,1000.);
#28901=VECTOR('',#132349,10.);
#28902=VECTOR('',#132350,1000.);
#28903=VECTOR('',#132351,10.);
#28904=VECTOR('',#132354,1000.);
#28905=VECTOR('',#132355,10.);
#28906=VECTOR('',#132358,1000.);
#28907=VECTOR('',#132361,10.);
#28908=VECTOR('',#132362,1000.);
#28909=VECTOR('',#132367,10.);
#28910=VECTOR('',#132368,1000.);
#28911=VECTOR('',#132369,10.);
#28912=VECTOR('',#132372,1000.);
#28913=VECTOR('',#132373,10.);
#28914=VECTOR('',#132376,1000.);
#28915=VECTOR('',#132379,10.);
#28916=VECTOR('',#132380,1000.);
#28917=VECTOR('',#132383,1000.);
#28918=VECTOR('',#132384,1000.);
#28919=VECTOR('',#132389,10.);
#28920=VECTOR('',#132390,1000.);
#28921=VECTOR('',#132391,10.);
#28922=VECTOR('',#132394,1000.);
#28923=VECTOR('',#132395,10.);
#28924=VECTOR('',#132398,1000.);
#28925=VECTOR('',#132401,10.);
#28926=VECTOR('',#132402,1000.);
#28927=VECTOR('',#132407,10.);
#28928=VECTOR('',#132408,1000.);
#28929=VECTOR('',#132409,10.);
#28930=VECTOR('',#132412,1000.);
#28931=VECTOR('',#132413,10.);
#28932=VECTOR('',#132416,1000.);
#28933=VECTOR('',#132419,10.);
#28934=VECTOR('',#132420,1000.);
#28935=VECTOR('',#132423,1000.);
#28936=VECTOR('',#132426,1000.);
#28937=VECTOR('',#132433,10.);
#28938=VECTOR('',#132434,1000.);
#28939=VECTOR('',#132435,10.);
#28940=VECTOR('',#132438,1000.);
#28941=VECTOR('',#132439,10.);
#28942=VECTOR('',#132442,1000.);
#28943=VECTOR('',#132445,10.);
#28944=VECTOR('',#132446,1000.);
#28945=VECTOR('',#132451,10.);
#28946=VECTOR('',#132452,1000.);
#28947=VECTOR('',#132453,10.);
#28948=VECTOR('',#132456,1000.);
#28949=VECTOR('',#132457,10.);
#28950=VECTOR('',#132460,1000.);
#28951=VECTOR('',#132463,10.);
#28952=VECTOR('',#132464,1000.);
#28953=VECTOR('',#132467,1000.);
#28954=VECTOR('',#132470,1000.);
#28955=VECTOR('',#132477,10.);
#28956=VECTOR('',#132478,1000.);
#28957=VECTOR('',#132479,10.);
#28958=VECTOR('',#132482,1000.);
#28959=VECTOR('',#132483,10.);
#28960=VECTOR('',#132486,1000.);
#28961=VECTOR('',#132489,10.);
#28962=VECTOR('',#132490,1000.);
#28963=VECTOR('',#132495,10.);
#28964=VECTOR('',#132496,1000.);
#28965=VECTOR('',#132497,10.);
#28966=VECTOR('',#132500,1000.);
#28967=VECTOR('',#132501,10.);
#28968=VECTOR('',#132504,1000.);
#28969=VECTOR('',#132507,10.);
#28970=VECTOR('',#132508,1000.);
#28971=VECTOR('',#132511,1000.);
#28972=VECTOR('',#132514,1000.);
#28973=VECTOR('',#132521,10.);
#28974=VECTOR('',#132522,1000.);
#28975=VECTOR('',#132523,10.);
#28976=VECTOR('',#132526,1000.);
#28977=VECTOR('',#132527,10.);
#28978=VECTOR('',#132530,1000.);
#28979=VECTOR('',#132533,10.);
#28980=VECTOR('',#132534,1000.);
#28981=VECTOR('',#132539,10.);
#28982=VECTOR('',#132540,1000.);
#28983=VECTOR('',#132541,10.);
#28984=VECTOR('',#132544,1000.);
#28985=VECTOR('',#132545,10.);
#28986=VECTOR('',#132548,1000.);
#28987=VECTOR('',#132551,10.);
#28988=VECTOR('',#132552,1000.);
#28989=VECTOR('',#132555,1000.);
#28990=VECTOR('',#132558,1000.);
#28991=VECTOR('',#132565,10.);
#28992=VECTOR('',#132566,1000.);
#28993=VECTOR('',#132567,10.);
#28994=VECTOR('',#132570,1000.);
#28995=VECTOR('',#132571,10.);
#28996=VECTOR('',#132574,1000.);
#28997=VECTOR('',#132577,10.);
#28998=VECTOR('',#132578,1000.);
#28999=VECTOR('',#132583,10.);
#29000=VECTOR('',#132584,1000.);
#29001=VECTOR('',#132585,10.);
#29002=VECTOR('',#132588,1000.);
#29003=VECTOR('',#132589,10.);
#29004=VECTOR('',#132592,1000.);
#29005=VECTOR('',#132595,10.);
#29006=VECTOR('',#132596,1000.);
#29007=VECTOR('',#132599,1000.);
#29008=VECTOR('',#132602,1000.);
#29009=VECTOR('',#132609,10.);
#29010=VECTOR('',#132610,1000.);
#29011=VECTOR('',#132611,10.);
#29012=VECTOR('',#132614,1000.);
#29013=VECTOR('',#132615,10.);
#29014=VECTOR('',#132618,1000.);
#29015=VECTOR('',#132621,10.);
#29016=VECTOR('',#132622,1000.);
#29017=VECTOR('',#132627,10.);
#29018=VECTOR('',#132628,1000.);
#29019=VECTOR('',#132629,10.);
#29020=VECTOR('',#132632,1000.);
#29021=VECTOR('',#132633,10.);
#29022=VECTOR('',#132636,1000.);
#29023=VECTOR('',#132639,10.);
#29024=VECTOR('',#132640,1000.);
#29025=VECTOR('',#132643,1000.);
#29026=VECTOR('',#132646,1000.);
#29027=VECTOR('',#132653,10.);
#29028=VECTOR('',#132654,1000.);
#29029=VECTOR('',#132655,10.);
#29030=VECTOR('',#132658,1000.);
#29031=VECTOR('',#132659,10.);
#29032=VECTOR('',#132662,1000.);
#29033=VECTOR('',#132665,10.);
#29034=VECTOR('',#132666,1000.);
#29035=VECTOR('',#132671,10.);
#29036=VECTOR('',#132672,1000.);
#29037=VECTOR('',#132673,10.);
#29038=VECTOR('',#132676,1000.);
#29039=VECTOR('',#132677,10.);
#29040=VECTOR('',#132680,1000.);
#29041=VECTOR('',#132683,10.);
#29042=VECTOR('',#132684,1000.);
#29043=VECTOR('',#132687,1000.);
#29044=VECTOR('',#132690,1000.);
#29045=VECTOR('',#132697,10.);
#29046=VECTOR('',#132698,1000.);
#29047=VECTOR('',#132699,10.);
#29048=VECTOR('',#132702,1000.);
#29049=VECTOR('',#132703,10.);
#29050=VECTOR('',#132706,1000.);
#29051=VECTOR('',#132709,10.);
#29052=VECTOR('',#132710,1000.);
#29053=VECTOR('',#132715,10.);
#29054=VECTOR('',#132716,1000.);
#29055=VECTOR('',#132717,10.);
#29056=VECTOR('',#132720,1000.);
#29057=VECTOR('',#132721,10.);
#29058=VECTOR('',#132724,1000.);
#29059=VECTOR('',#132727,10.);
#29060=VECTOR('',#132728,1000.);
#29061=VECTOR('',#132731,1000.);
#29062=VECTOR('',#132734,1000.);
#29063=VECTOR('',#132741,10.);
#29064=VECTOR('',#132742,1000.);
#29065=VECTOR('',#132743,10.);
#29066=VECTOR('',#132746,1000.);
#29067=VECTOR('',#132747,10.);
#29068=VECTOR('',#132750,1000.);
#29069=VECTOR('',#132753,10.);
#29070=VECTOR('',#132754,1000.);
#29071=VECTOR('',#132759,10.);
#29072=VECTOR('',#132760,1000.);
#29073=VECTOR('',#132761,10.);
#29074=VECTOR('',#132764,1000.);
#29075=VECTOR('',#132765,10.);
#29076=VECTOR('',#132768,1000.);
#29077=VECTOR('',#132771,10.);
#29078=VECTOR('',#132772,1000.);
#29079=VECTOR('',#132775,1000.);
#29080=VECTOR('',#132778,1000.);
#29081=VECTOR('',#132785,10.);
#29082=VECTOR('',#132786,1000.);
#29083=VECTOR('',#132787,10.);
#29084=VECTOR('',#132790,1000.);
#29085=VECTOR('',#132791,10.);
#29086=VECTOR('',#132794,1000.);
#29087=VECTOR('',#132797,10.);
#29088=VECTOR('',#132798,1000.);
#29089=VECTOR('',#132803,10.);
#29090=VECTOR('',#132804,1000.);
#29091=VECTOR('',#132805,10.);
#29092=VECTOR('',#132808,1000.);
#29093=VECTOR('',#132809,10.);
#29094=VECTOR('',#132812,1000.);
#29095=VECTOR('',#132815,10.);
#29096=VECTOR('',#132816,1000.);
#29097=VECTOR('',#132819,1000.);
#29098=VECTOR('',#132822,1000.);
#29099=VECTOR('',#132829,10.);
#29100=VECTOR('',#132830,1000.);
#29101=VECTOR('',#132831,10.);
#29102=VECTOR('',#132834,1000.);
#29103=VECTOR('',#132835,10.);
#29104=VECTOR('',#132838,1000.);
#29105=VECTOR('',#132841,10.);
#29106=VECTOR('',#132842,1000.);
#29107=VECTOR('',#132847,10.);
#29108=VECTOR('',#132848,1000.);
#29109=VECTOR('',#132849,10.);
#29110=VECTOR('',#132852,1000.);
#29111=VECTOR('',#132853,10.);
#29112=VECTOR('',#132856,1000.);
#29113=VECTOR('',#132859,10.);
#29114=VECTOR('',#132860,1000.);
#29115=VECTOR('',#132863,1000.);
#29116=VECTOR('',#132866,1000.);
#29117=VECTOR('',#132873,10.);
#29118=VECTOR('',#132874,1000.);
#29119=VECTOR('',#132875,10.);
#29120=VECTOR('',#132878,1000.);
#29121=VECTOR('',#132879,10.);
#29122=VECTOR('',#132882,1000.);
#29123=VECTOR('',#132885,10.);
#29124=VECTOR('',#132886,1000.);
#29125=VECTOR('',#132891,10.);
#29126=VECTOR('',#132892,1000.);
#29127=VECTOR('',#132893,10.);
#29128=VECTOR('',#132896,1000.);
#29129=VECTOR('',#132897,10.);
#29130=VECTOR('',#132900,1000.);
#29131=VECTOR('',#132903,10.);
#29132=VECTOR('',#132904,1000.);
#29133=VECTOR('',#132907,1000.);
#29134=VECTOR('',#132910,1000.);
#29135=VECTOR('',#132917,10.);
#29136=VECTOR('',#132918,1000.);
#29137=VECTOR('',#132919,10.);
#29138=VECTOR('',#132922,1000.);
#29139=VECTOR('',#132923,10.);
#29140=VECTOR('',#132926,1000.);
#29141=VECTOR('',#132929,10.);
#29142=VECTOR('',#132930,1000.);
#29143=VECTOR('',#132935,10.);
#29144=VECTOR('',#132936,1000.);
#29145=VECTOR('',#132937,10.);
#29146=VECTOR('',#132940,1000.);
#29147=VECTOR('',#132941,10.);
#29148=VECTOR('',#132944,1000.);
#29149=VECTOR('',#132947,10.);
#29150=VECTOR('',#132948,1000.);
#29151=VECTOR('',#132951,1000.);
#29152=VECTOR('',#132954,1000.);
#29153=VECTOR('',#132961,10.);
#29154=VECTOR('',#132962,1000.);
#29155=VECTOR('',#132963,10.);
#29156=VECTOR('',#132966,1000.);
#29157=VECTOR('',#132967,10.);
#29158=VECTOR('',#132970,1000.);
#29159=VECTOR('',#132973,10.);
#29160=VECTOR('',#132974,1000.);
#29161=VECTOR('',#132979,10.);
#29162=VECTOR('',#132980,1000.);
#29163=VECTOR('',#132981,10.);
#29164=VECTOR('',#132984,1000.);
#29165=VECTOR('',#132985,10.);
#29166=VECTOR('',#132988,1000.);
#29167=VECTOR('',#132991,10.);
#29168=VECTOR('',#132992,1000.);
#29169=VECTOR('',#132995,1000.);
#29170=VECTOR('',#132998,1000.);
#29171=VECTOR('',#133005,10.);
#29172=VECTOR('',#133006,1000.);
#29173=VECTOR('',#133007,10.);
#29174=VECTOR('',#133010,1000.);
#29175=VECTOR('',#133011,10.);
#29176=VECTOR('',#133014,1000.);
#29177=VECTOR('',#133017,10.);
#29178=VECTOR('',#133018,1000.);
#29179=VECTOR('',#133023,10.);
#29180=VECTOR('',#133024,1000.);
#29181=VECTOR('',#133025,10.);
#29182=VECTOR('',#133028,1000.);
#29183=VECTOR('',#133029,10.);
#29184=VECTOR('',#133032,1000.);
#29185=VECTOR('',#133035,10.);
#29186=VECTOR('',#133036,1000.);
#29187=VECTOR('',#138471,65.254);
#29188=VECTOR('',#138474,68.75);
#29189=VECTOR('',#138479,72.53);
#29190=VECTOR('',#138508,65.);
#29191=VECTOR('',#138511,65.254);
#29192=VECTOR('',#138596,1000.);
#29193=VECTOR('',#138599,1000.);
#29194=VECTOR('',#138602,1000.);
#29195=VECTOR('',#138605,1000.);
#29196=VECTOR('',#138616,72.53);
#29197=VECTOR('',#138623,8.4455);
#29198=VECTOR('',#138630,8.4455);
#29199=VECTOR('',#138637,8.4455);
#29200=VECTOR('',#138644,8.4455);
#29201=VECTOR('',#138649,1000.);
#29202=VECTOR('',#138652,1000.);
#29203=VECTOR('',#138675,1000.);
#29204=VECTOR('',#138678,1000.);
#29205=VECTOR('',#138681,1000.);
#29206=VECTOR('',#138684,1000.);
#29207=VECTOR('',#138689,1000.);
#29208=VECTOR('',#138692,1000.);
#29209=VECTOR('',#138695,1000.);
#29210=VECTOR('',#138698,1000.);
#29211=VECTOR('',#138701,1000.);
#29212=VECTOR('',#138702,1000.);
#29213=VECTOR('',#138703,1000.);
#29214=VECTOR('',#138706,1000.);
#29215=VECTOR('',#138707,1000.);
#29216=VECTOR('',#138710,1000.);
#29217=VECTOR('',#138711,1000.);
#29218=VECTOR('',#138712,1000.);
#29219=VECTOR('',#138713,1000.);
#29220=VECTOR('',#138716,1000.);
#29221=VECTOR('',#138717,1000.);
#29222=VECTOR('',#138726,1000.);
#29223=VECTOR('',#138727,1000.);
#29224=VECTOR('',#138732,1000.);
#29225=VECTOR('',#138737,1000.);
#29226=VECTOR('',#138738,1000.);
#29227=VECTOR('',#138739,1000.);
#29228=VECTOR('',#138742,1000.);
#29229=VECTOR('',#138745,1000.);
#29230=VECTOR('',#138750,1000.);
#29231=VECTOR('',#138751,1000.);
#29232=VECTOR('',#138752,1000.);
#29233=VECTOR('',#138757,1000.);
#29234=VECTOR('',#138762,1000.);
#29235=VECTOR('',#138763,1000.);
#29236=VECTOR('',#138764,1000.);
#29237=VECTOR('',#138769,1000.);
#29238=VECTOR('',#138774,1000.);
#29239=VECTOR('',#138775,1000.);
#29240=VECTOR('',#138776,1000.);
#29241=VECTOR('',#138781,1000.);
#29242=VECTOR('',#138786,1000.);
#29243=VECTOR('',#138787,1000.);
#29244=VECTOR('',#138790,1000.);
#29245=VECTOR('',#138793,1000.);
#29246=VECTOR('',#138796,1000.);
#29247=VECTOR('',#138797,1000.);
#29248=VECTOR('',#138798,1000.);
#29249=VECTOR('',#138803,1000.);
#29250=VECTOR('',#138804,1000.);
#29251=VECTOR('',#138807,1000.);
#29252=VECTOR('',#138816,1000.);
#29253=VECTOR('',#138819,1000.);
#29254=VECTOR('',#138822,1000.);
#29255=VECTOR('',#138827,1000.);
#29256=VECTOR('',#138832,1000.);
#29257=VECTOR('',#138833,1000.);
#29258=VECTOR('',#138842,1000.);
#29259=VECTOR('',#138843,1000.);
#29260=VECTOR('',#138846,1000.);
#29261=VECTOR('',#138849,1000.);
#29262=VECTOR('',#138858,1000.);
#29263=VECTOR('',#138861,1000.);
#29264=VECTOR('',#138866,1000.);
#29265=VECTOR('',#138869,1000.);
#29266=VECTOR('',#138874,1000.);
#29267=VECTOR('',#138877,1000.);
#29268=VECTOR('',#138880,1000.);
#29269=VECTOR('',#138883,1000.);
#29270=VECTOR('',#138886,1000.);
#29271=VECTOR('',#138887,1000.);
#29272=VECTOR('',#138890,1000.);
#29273=VECTOR('',#138891,1000.);
#29274=VECTOR('',#138894,1000.);
#29275=VECTOR('',#138895,1000.);
#29276=VECTOR('',#138900,1000.);
#29277=VECTOR('',#138903,1000.);
#29278=VECTOR('',#138906,1000.);
#29279=VECTOR('',#138909,1000.);
#29280=VECTOR('',#138910,1000.);
#29281=VECTOR('',#138913,1000.);
#29282=VECTOR('',#138914,1000.);
#29283=VECTOR('',#138915,1000.);
#29284=VECTOR('',#138920,1000.);
#29285=VECTOR('',#138923,1000.);
#29286=VECTOR('',#138930,1000.);
#29287=VECTOR('',#138933,1000.);
#29288=VECTOR('',#138934,1000.);
#29289=VECTOR('',#138935,1000.);
#29290=VECTOR('',#138938,1000.);
#29291=VECTOR('',#138939,1000.);
#29292=VECTOR('',#138940,1000.);
#29293=VECTOR('',#138945,1000.);
#29294=VECTOR('',#138948,1000.);
#29295=VECTOR('',#138949,1000.);
#29296=VECTOR('',#138952,1000.);
#29297=VECTOR('',#138955,1000.);
#29298=VECTOR('',#138956,1000.);
#29299=VECTOR('',#139235,1.27);
#29300=VECTOR('',#139240,1.905);
#29301=VECTOR('',#139269,1.27);
#29302=VECTOR('',#139274,66.0995441972308);
#29303=VECTOR('',#139277,66.4805441972308);
#29304=VECTOR('',#139332,56.875);
#29305=VECTOR('',#139337,56.2993860673093);
#29306=VECTOR('',#139340,57.8669800961561);
#29307=VECTOR('',#139345,51.27);
#29308=VECTOR('',#139348,50.);
#29309=VECTOR('',#139355,65.);
#29310=VECTOR('',#139370,4.7227367061318);
#29311=VECTOR('',#139375,4.7227367061318);
#29312=VECTOR('',#139378,4.7227367061318);
#29313=VECTOR('',#139381,4.7227367061318);
#29314=VECTOR('',#139384,4.7227367061318);
#29315=VECTOR('',#139387,4.7227367061318);
#29316=VECTOR('',#139390,4.74980000000001);
#29317=VECTOR('',#139395,4.74980000000001);
#29318=VECTOR('',#139400,4.74980000000001);
#29319=VECTOR('',#139403,4.74980000000001);
#29320=VECTOR('',#139406,4.74980000000001);
#29321=VECTOR('',#139409,4.74980000000001);
#29322=VECTOR('',#139412,4.74980000000001);
#29323=VECTOR('',#139415,4.74980000000001);
#29324=VECTOR('',#139426,4.74980000000001);
#29325=VECTOR('',#139439,3.98780000000001);
#29326=VECTOR('',#139474,1000.);
#29327=VECTOR('',#139475,1000.);
#29328=VECTOR('',#139476,1000.);
#29329=VECTOR('',#139477,1000.);
#29330=VECTOR('',#139478,1000.);
#29331=VECTOR('',#139479,1000.);
#29332=VECTOR('',#139482,1000.);
#29333=VECTOR('',#139483,1000.);
#29334=VECTOR('',#139486,1000.);
#29335=VECTOR('',#139489,1000.);
#29336=VECTOR('',#139492,1000.);
#29337=VECTOR('',#139495,1000.);
#29338=VECTOR('',#139502,4.72273670613179);
#29339=VECTOR('',#139507,4.72273670613179);
#29340=VECTOR('',#139510,4.72273670613179);
#29341=VECTOR('',#139513,4.72273670613179);
#29342=VECTOR('',#139516,4.72273670613179);
#29343=VECTOR('',#139519,4.72273670613179);
#29344=VECTOR('',#139522,4.74980000000001);
#29345=VECTOR('',#139527,4.74980000000001);
#29346=VECTOR('',#139532,4.74980000000001);
#29347=VECTOR('',#139535,4.7498);
#29348=VECTOR('',#139538,4.7498);
#29349=VECTOR('',#139541,4.74980000000001);
#29350=VECTOR('',#139544,4.74980000000001);
#29351=VECTOR('',#139547,4.74980000000001);
#29352=VECTOR('',#139558,4.74980000000001);
#29353=VECTOR('',#139571,3.98780000000001);
#29354=VECTOR('',#139606,1000.);
#29355=VECTOR('',#139607,1000.);
#29356=VECTOR('',#139608,1000.);
#29357=VECTOR('',#139609,1000.);
#29358=VECTOR('',#139610,1000.);
#29359=VECTOR('',#139611,1000.);
#29360=VECTOR('',#139614,1000.);
#29361=VECTOR('',#139615,1000.);
#29362=VECTOR('',#139618,1000.);
#29363=VECTOR('',#139621,1000.);
#29364=VECTOR('',#139624,1000.);
#29365=VECTOR('',#139627,1000.);
#29366=VECTOR('',#139636,40.);
#29367=VECTOR('',#139645,40.);
#29368=VECTOR('',#139652,48.4864729374055);
#29369=VECTOR('',#139661,48.4864729374054);
#29370=VECTOR('',#139666,50.);
#29371=VECTOR('',#139667,50.);
#29372=VECTOR('',#139670,4.7625);
#29373=VECTOR('',#139673,4.7625);
#29374=VECTOR('',#139676,40.);
#29375=VECTOR('',#139677,40.);
#29376=VECTOR('',#139686,65.0000000000002);
#29377=VECTOR('',#139693,56.875);
#29378=VECTOR('',#139710,76.4577478255888);
#29379=VECTOR('',#139715,1000.);
#29380=VECTOR('',#139718,1000.);
#29381=VECTOR('',#139723,70.625);
#29382=VECTOR('',#139730,76.5847478255888);
#29383=VECTOR('',#139737,8.4455);
#29384=VECTOR('',#139744,8.4455);
#29385=VECTOR('',#139751,8.4455);
#29386=VECTOR('',#139758,8.4455);
#29387=VECTOR('',#139765,7.9375);
#29388=VECTOR('',#139772,7.9375);
#29389=VECTOR('',#139779,7.9375);
#29390=VECTOR('',#139786,7.9375);
#29391=VECTOR('',#139791,1000.);
#29392=VECTOR('',#139794,1000.);
#29393=VECTOR('',#139799,1000.);
#29394=VECTOR('',#139800,1000.);
#29395=VECTOR('',#139801,1000.);
#29396=VECTOR('',#139806,1000.);
#29397=VECTOR('',#139811,1000.);
#29398=VECTOR('',#139812,1000.);
#29399=VECTOR('',#139813,1000.);
#29400=VECTOR('',#139818,1000.);
#29401=VECTOR('',#139823,1000.);
#29402=VECTOR('',#139824,1000.);
#29403=VECTOR('',#139825,1000.);
#29404=VECTOR('',#139830,1000.);
#29405=VECTOR('',#139835,1000.);
#29406=VECTOR('',#139836,1000.);
#29407=VECTOR('',#139839,1000.);
#29408=VECTOR('',#139842,1000.);
#29409=VECTOR('',#139845,1000.);
#29410=VECTOR('',#139848,1000.);
#29411=VECTOR('',#139863,1000.);
#29412=VECTOR('',#139866,1000.);
#29413=VECTOR('',#139869,1000.);
#29414=VECTOR('',#139872,1000.);
#29415=VECTOR('',#139875,1000.);
#29416=VECTOR('',#139878,1000.);
#29417=VECTOR('',#139881,1000.);
#29418=VECTOR('',#139882,1000.);
#29419=VECTOR('',#139885,1000.);
#29420=VECTOR('',#139890,1000.);
#29421=VECTOR('',#139891,1000.);
#29422=VECTOR('',#139894,1000.);
#29423=VECTOR('',#139899,1000.);
#29424=VECTOR('',#139900,1000.);
#29425=VECTOR('',#139903,1000.);
#29426=VECTOR('',#139908,1000.);
#29427=VECTOR('',#139945,1000.);
#29428=VECTOR('',#139948,1000.);
#29429=VECTOR('',#139953,1000.);
#29430=VECTOR('',#139956,1000.);
#29431=VECTOR('',#139957,1000.);
#29432=VECTOR('',#139960,1000.);
#29433=VECTOR('',#139969,1000.);
#29434=VECTOR('',#139972,1000.);
#29435=VECTOR('',#139975,1000.);
#29436=VECTOR('',#139978,1000.);
#29437=VECTOR('',#139981,1000.);
#29438=VECTOR('',#139984,1000.);
#29439=VECTOR('',#139987,1000.);
#29440=VECTOR('',#139988,1000.);
#29441=VECTOR('',#139995,1000.);
#29442=VECTOR('',#139996,10.);
#29443=VECTOR('',#139997,1000.);
#29444=VECTOR('',#139998,1000.);
#29445=VECTOR('',#139999,10.);
#29446=VECTOR('',#140000,1000.);
#29447=VECTOR('',#140005,1000.);
#29448=VECTOR('',#140006,10.);
#29449=VECTOR('',#140007,1000.);
#29450=VECTOR('',#140008,1000.);
#29451=VECTOR('',#140009,10.);
#29452=VECTOR('',#140010,1000.);
#29453=VECTOR('',#140019,3.4);
#29454=VECTOR('',#140024,3.4);
#29455=VECTOR('',#140027,7.49999999999995);
#29456=VECTOR('',#140032,7.49999999999995);
#29457=VECTOR('',#140037,7.49999999999995);
#29458=VECTOR('',#140042,7.49999999999995);
#29459=VECTOR('',#140047,7.49999999999995);
#29460=VECTOR('',#140052,7.49999999999995);
#29461=VECTOR('',#140059,15.);
#29462=VECTOR('',#140060,15.);
#29463=VECTOR('',#140061,15.);
#29464=VECTOR('',#140068,1000.);
#29465=VECTOR('',#140069,1000.);
#29466=VECTOR('',#140076,1000.);
#29467=VECTOR('',#140077,1000.);
#29468=VECTOR('',#140084,1000.);
#29469=VECTOR('',#140089,1000.);
#29470=VECTOR('',#140094,1000.);
#29471=VECTOR('',#140099,1000.);
#29472=VECTOR('',#140110,1000.);
#29473=VECTOR('',#140111,1000.);
#29474=VECTOR('',#140112,1000.);
#29475=VECTOR('',#140113,1000.);
#29476=VECTOR('',#140116,1000.);
#29477=VECTOR('',#140119,1000.);
#29478=VECTOR('',#140120,1000.);
#29479=VECTOR('',#140121,1000.);
#29480=VECTOR('',#140126,1000.);
#29481=VECTOR('',#140127,1000.);
#29482=VECTOR('',#140128,1000.);
#29483=VECTOR('',#140129,1000.);
#29484=VECTOR('',#140130,1000.);
#29485=VECTOR('',#140131,1000.);
#29486=VECTOR('',#140132,1000.);
#29487=VECTOR('',#140135,1000.);
#29488=VECTOR('',#140136,1000.);
#29489=VECTOR('',#140137,1000.);
#29490=VECTOR('',#140138,1000.);
#29491=VECTOR('',#140141,1000.);
#29492=VECTOR('',#140142,1000.);
#29493=VECTOR('',#140143,1000.);
#29494=VECTOR('',#140144,1000.);
#29495=VECTOR('',#140145,1000.);
#29496=VECTOR('',#140146,1000.);
#29497=VECTOR('',#140147,1000.);
#29498=VECTOR('',#140150,1000.);
#29499=VECTOR('',#140151,1000.);
#29500=VECTOR('',#140152,1000.);
#29501=VECTOR('',#140153,1000.);
#29502=VECTOR('',#140156,1000.);
#29503=VECTOR('',#140159,1000.);
#29504=VECTOR('',#140162,1000.);
#29505=VECTOR('',#140165,1000.);
#29506=VECTOR('',#140168,1000.);
#29507=VECTOR('',#140171,1000.);
#29508=VECTOR('',#140174,1000.);
#29509=VECTOR('',#140177,1000.);
#29510=VECTOR('',#140182,1000.);
#29511=VECTOR('',#140183,1000.);
#29512=VECTOR('',#140184,1000.);
#29513=VECTOR('',#140185,1000.);
#29514=VECTOR('',#140188,1000.);
#29515=VECTOR('',#140189,1000.);
#29516=VECTOR('',#140190,1000.);
#29517=VECTOR('',#140191,1000.);
#29518=VECTOR('',#140194,1000.);
#29519=VECTOR('',#140195,1000.);
#29520=VECTOR('',#140196,1000.);
#29521=VECTOR('',#140197,1000.);
#29522=VECTOR('',#140200,1000.);
#29523=VECTOR('',#140201,1000.);
#29524=VECTOR('',#140202,1000.);
#29525=VECTOR('',#140203,1000.);
#29526=VECTOR('',#140278,1000.);
#29527=VECTOR('',#140279,1000.);
#29528=VECTOR('',#140280,1000.);
#29529=VECTOR('',#140283,1000.);
#29530=VECTOR('',#140284,1000.);
#29531=VECTOR('',#140285,1000.);
#29532=VECTOR('',#140286,1000.);
#29533=VECTOR('',#140287,1000.);
#29534=VECTOR('',#140288,1000.);
#29535=VECTOR('',#140291,1000.);
#29536=VECTOR('',#140292,1000.);
#29537=VECTOR('',#140293,1000.);
#29538=VECTOR('',#140296,1000.);
#29539=VECTOR('',#140297,1000.);
#29540=VECTOR('',#140298,1000.);
#29541=VECTOR('',#140299,1000.);
#29542=VECTOR('',#140300,1000.);
#29543=VECTOR('',#140303,1000.);
#29544=VECTOR('',#140382,1000.);
#29545=VECTOR('',#140383,1000.);
#29546=VECTOR('',#140384,1000.);
#29547=VECTOR('',#140385,1000.);
#29548=VECTOR('',#140388,1000.);
#29549=VECTOR('',#140389,1000.);
#29550=VECTOR('',#140390,1000.);
#29551=VECTOR('',#140393,1000.);
#29552=VECTOR('',#140394,1000.);
#29553=VECTOR('',#140397,1000.);
#29554=VECTOR('',#140398,1000.);
#29555=VECTOR('',#140401,1000.);
#29556=VECTOR('',#140406,1000.);
#29557=VECTOR('',#140411,1000.);
#29558=VECTOR('',#140420,1000.);
#29559=VECTOR('',#140423,1000.);
#29560=VECTOR('',#140428,1000.);
#29561=VECTOR('',#140431,1000.);
#29562=VECTOR('',#140434,1000.);
#29563=VECTOR('',#140437,1000.);
#29564=VECTOR('',#140440,1000.);
#29565=VECTOR('',#140443,1000.);
#29566=VECTOR('',#140446,1000.);
#29567=VECTOR('',#140447,1000.);
#29568=VECTOR('',#140450,1000.);
#29569=VECTOR('',#140451,1000.);
#29570=VECTOR('',#140454,1000.);
#29571=VECTOR('',#140455,1000.);
#29572=VECTOR('',#140458,1000.);
#29573=VECTOR('',#140463,1000.);
#29574=VECTOR('',#140464,1000.);
#29575=VECTOR('',#140467,1000.);
#29576=VECTOR('',#140472,1000.);
#29577=VECTOR('',#140473,1000.);
#29578=VECTOR('',#140476,1000.);
#29579=VECTOR('',#140481,1000.);
#29580=VECTOR('',#140482,1000.);
#29581=VECTOR('',#140485,1000.);
#29582=VECTOR('',#140490,1000.);
#29583=VECTOR('',#140491,1000.);
#29584=VECTOR('',#140494,1000.);
#29585=VECTOR('',#140499,1000.);
#29586=VECTOR('',#140500,1000.);
#29587=VECTOR('',#140503,1000.);
#29588=VECTOR('',#140508,1000.);
#29589=VECTOR('',#140509,1000.);
#29590=VECTOR('',#140520,1000.);
#29591=VECTOR('',#140523,1000.);
#29592=VECTOR('',#140526,1000.);
#29593=VECTOR('',#140529,1000.);
#29594=VECTOR('',#140532,1000.);
#29595=VECTOR('',#140533,1000.);
#29596=VECTOR('',#140534,1000.);
#29597=VECTOR('',#140537,1000.);
#29598=VECTOR('',#140542,1000.);
#29599=VECTOR('',#140543,1000.);
#29600=VECTOR('',#140546,1000.);
#29601=VECTOR('',#140551,1000.);
#29602=VECTOR('',#140552,1000.);
#29603=VECTOR('',#140555,1000.);
#29604=VECTOR('',#140560,1000.);
#29605=VECTOR('',#140561,1000.);
#29606=VECTOR('',#140572,1000.);
#29607=VECTOR('',#140575,1000.);
#29608=VECTOR('',#140578,1000.);
#29609=VECTOR('',#140581,1000.);
#29610=VECTOR('',#140582,1000.);
#29611=VECTOR('',#140583,1000.);
#29612=VECTOR('',#140586,1000.);
#29613=VECTOR('',#140589,1000.);
#29614=VECTOR('',#140592,1000.);
#29615=VECTOR('',#140595,1000.);
#29616=VECTOR('',#140598,1000.);
#29617=VECTOR('',#140601,1000.);
#29618=VECTOR('',#140602,1000.);
#29619=VECTOR('',#140603,1000.);
#29620=VECTOR('',#140606,1000.);
#29621=VECTOR('',#140609,1000.);
#29622=VECTOR('',#140612,1000.);
#29623=VECTOR('',#140615,1000.);
#29624=VECTOR('',#140618,1000.);
#29625=VECTOR('',#140621,1000.);
#29626=VECTOR('',#140622,1000.);
#29627=VECTOR('',#140623,1000.);
#29628=VECTOR('',#140626,1000.);
#29629=VECTOR('',#140629,1000.);
#29630=VECTOR('',#140632,1000.);
#29631=VECTOR('',#140635,1000.);
#29632=VECTOR('',#140638,1000.);
#29633=VECTOR('',#140641,1000.);
#29634=VECTOR('',#140642,1000.);
#29635=VECTOR('',#140643,1000.);
#29636=VECTOR('',#140646,1000.);
#29637=VECTOR('',#140649,1000.);
#29638=VECTOR('',#140654,1000.);
#29639=VECTOR('',#140657,1000.);
#29640=VECTOR('',#140660,1000.);
#29641=VECTOR('',#140663,1000.);
#29642=VECTOR('',#140664,1000.);
#29643=VECTOR('',#140665,1000.);
#29644=VECTOR('',#140668,1000.);
#29645=VECTOR('',#140671,1000.);
#29646=VECTOR('',#140674,1000.);
#29647=VECTOR('',#140677,1000.);
#29648=VECTOR('',#140680,1000.);
#29649=VECTOR('',#140683,1000.);
#29650=VECTOR('',#140684,1000.);
#29651=VECTOR('',#140685,1000.);
#29652=VECTOR('',#140688,1000.);
#29653=VECTOR('',#140691,1000.);
#29654=VECTOR('',#140694,1000.);
#29655=VECTOR('',#140697,1000.);
#29656=VECTOR('',#140700,1000.);
#29657=VECTOR('',#140703,1000.);
#29658=VECTOR('',#140704,1000.);
#29659=VECTOR('',#140705,1000.);
#29660=VECTOR('',#140708,1000.);
#29661=VECTOR('',#140711,1000.);
#29662=VECTOR('',#140714,1000.);
#29663=VECTOR('',#140717,1000.);
#29664=VECTOR('',#140720,1000.);
#29665=VECTOR('',#140723,1000.);
#29666=VECTOR('',#140724,1000.);
#29667=VECTOR('',#140725,1000.);
#29668=VECTOR('',#140728,1000.);
#29669=VECTOR('',#140731,1000.);
#29670=VECTOR('',#140734,1000.);
#29671=VECTOR('',#140735,1000.);
#29672=VECTOR('',#140738,1000.);
#29673=VECTOR('',#140741,1000.);
#29674=VECTOR('',#140744,1000.);
#29675=VECTOR('',#140747,1000.);
#29676=VECTOR('',#140750,1000.);
#29677=VECTOR('',#140753,1000.);
#29678=VECTOR('',#140756,1000.);
#29679=VECTOR('',#140759,1000.);
#29680=VECTOR('',#140762,1000.);
#29681=VECTOR('',#140765,1000.);
#29682=VECTOR('',#140768,1000.);
#29683=VECTOR('',#140771,1000.);
#29684=VECTOR('',#140774,1000.);
#29685=VECTOR('',#140777,1000.);
#29686=VECTOR('',#140780,1000.);
#29687=VECTOR('',#140783,1000.);
#29688=VECTOR('',#140786,1000.);
#29689=VECTOR('',#140789,1000.);
#29690=VECTOR('',#140792,1000.);
#29691=VECTOR('',#140795,1000.);
#29692=VECTOR('',#140798,1000.);
#29693=VECTOR('',#140801,1000.);
#29694=VECTOR('',#140804,1000.);
#29695=VECTOR('',#140807,1000.);
#29696=VECTOR('',#140810,1000.);
#29697=VECTOR('',#140813,1000.);
#29698=VECTOR('',#140816,1000.);
#29699=VECTOR('',#140819,1000.);
#29700=VECTOR('',#140822,1000.);
#29701=VECTOR('',#140825,1000.);
#29702=VECTOR('',#140828,1000.);
#29703=VECTOR('',#140831,1000.);
#29704=VECTOR('',#140834,1000.);
#29705=VECTOR('',#140837,1000.);
#29706=VECTOR('',#140840,1000.);
#29707=VECTOR('',#140843,1000.);
#29708=VECTOR('',#140846,1000.);
#29709=VECTOR('',#140849,1000.);
#29710=VECTOR('',#140852,1000.);
#29711=VECTOR('',#140855,1000.);
#29712=VECTOR('',#140858,1000.);
#29713=VECTOR('',#140861,1000.);
#29714=VECTOR('',#140864,1000.);
#29715=VECTOR('',#140867,1000.);
#29716=VECTOR('',#140870,1000.);
#29717=VECTOR('',#140873,1000.);
#29718=VECTOR('',#140876,1000.);
#29719=VECTOR('',#140879,1000.);
#29720=VECTOR('',#140882,1000.);
#29721=VECTOR('',#140885,1000.);
#29722=VECTOR('',#140888,1000.);
#29723=VECTOR('',#140891,1000.);
#29724=VECTOR('',#140894,1000.);
#29725=VECTOR('',#140897,1000.);
#29726=VECTOR('',#140904,1000.);
#29727=VECTOR('',#140907,1000.);
#29728=VECTOR('',#140912,1000.);
#29729=VECTOR('',#140915,1000.);
#29730=VECTOR('',#140918,1000.);
#29731=VECTOR('',#140919,1000.);
#29732=VECTOR('',#140922,1000.);
#29733=VECTOR('',#140925,1000.);
#29734=VECTOR('',#140928,1000.);
#29735=VECTOR('',#140931,1000.);
#29736=VECTOR('',#140934,1000.);
#29737=VECTOR('',#140935,1000.);
#29738=VECTOR('',#140936,1000.);
#29739=VECTOR('',#140939,1000.);
#29740=VECTOR('',#140944,1000.);
#29741=VECTOR('',#140945,1000.);
#29742=VECTOR('',#140948,1000.);
#29743=VECTOR('',#140953,1000.);
#29744=VECTOR('',#140954,1000.);
#29745=VECTOR('',#140957,1000.);
#29746=VECTOR('',#140962,1000.);
#29747=VECTOR('',#140963,1000.);
#29748=VECTOR('',#140966,1000.);
#29749=VECTOR('',#140971,1000.);
#29750=VECTOR('',#140974,1000.);
#29751=VECTOR('',#140975,1000.);
#29752=VECTOR('',#140978,1000.);
#29753=VECTOR('',#140983,1000.);
#29754=VECTOR('',#140984,1000.);
#29755=VECTOR('',#140987,1000.);
#29756=VECTOR('',#140992,1000.);
#29757=VECTOR('',#140993,1000.);
#29758=VECTOR('',#141004,1000.);
#29759=VECTOR('',#141007,1000.);
#29760=VECTOR('',#141010,1000.);
#29761=VECTOR('',#141013,1000.);
#29762=VECTOR('',#141016,1000.);
#29763=VECTOR('',#141017,1000.);
#29764=VECTOR('',#141018,1000.);
#29765=VECTOR('',#141021,1000.);
#29766=VECTOR('',#141026,1000.);
#29767=VECTOR('',#141027,1000.);
#29768=VECTOR('',#141030,1000.);
#29769=VECTOR('',#141035,1000.);
#29770=VECTOR('',#141036,1000.);
#29771=VECTOR('',#141039,1000.);
#29772=VECTOR('',#141044,1000.);
#29773=VECTOR('',#141045,1000.);
#29774=VECTOR('',#141056,1000.);
#29775=VECTOR('',#141059,1000.);
#29776=VECTOR('',#141064,1000.);
#29777=VECTOR('',#141065,1000.);
#29778=VECTOR('',#141068,1000.);
#29779=VECTOR('',#141071,1000.);
#29780=VECTOR('',#141074,1000.);
#29781=VECTOR('',#141077,1000.);
#29782=VECTOR('',#141080,1000.);
#29783=VECTOR('',#141083,1000.);
#29784=VECTOR('',#141086,1000.);
#29785=VECTOR('',#141087,1000.);
#29786=VECTOR('',#141088,1000.);
#29787=VECTOR('',#141091,1000.);
#29788=VECTOR('',#141096,1000.);
#29789=VECTOR('',#141097,1000.);
#29790=VECTOR('',#141100,1000.);
#29791=VECTOR('',#141105,1000.);
#29792=VECTOR('',#141106,1000.);
#29793=VECTOR('',#141109,1000.);
#29794=VECTOR('',#141114,1000.);
#29795=VECTOR('',#141115,1000.);
#29796=VECTOR('',#141118,1000.);
#29797=VECTOR('',#141123,1000.);
#29798=VECTOR('',#141124,1000.);
#29799=VECTOR('',#141127,1000.);
#29800=VECTOR('',#141132,1000.);
#29801=VECTOR('',#141133,1000.);
#29802=VECTOR('',#141136,1000.);
#29803=VECTOR('',#141141,1000.);
#29804=VECTOR('',#141144,1000.);
#29805=VECTOR('',#141145,1000.);
#29806=VECTOR('',#141156,1000.);
#29807=VECTOR('',#141159,1000.);
#29808=VECTOR('',#141162,1000.);
#29809=VECTOR('',#141165,1000.);
#29810=VECTOR('',#141168,1000.);
#29811=VECTOR('',#141169,1000.);
#29812=VECTOR('',#141170,1000.);
#29813=VECTOR('',#141173,1000.);
#29814=VECTOR('',#141178,1000.);
#29815=VECTOR('',#141179,1000.);
#29816=VECTOR('',#141182,1000.);
#29817=VECTOR('',#141187,1000.);
#29818=VECTOR('',#141188,1000.);
#29819=VECTOR('',#141191,1000.);
#29820=VECTOR('',#141196,1000.);
#29821=VECTOR('',#141197,1000.);
#29822=VECTOR('',#141208,1000.);
#29823=VECTOR('',#141211,1000.);
#29824=VECTOR('',#141216,1000.);
#29825=VECTOR('',#141217,1000.);
#29826=VECTOR('',#141220,1000.);
#29827=VECTOR('',#141223,1000.);
#29828=VECTOR('',#141226,1000.);
#29829=VECTOR('',#141229,1000.);
#29830=VECTOR('',#141232,1000.);
#29831=VECTOR('',#141235,1000.);
#29832=VECTOR('',#141238,1000.);
#29833=VECTOR('',#141239,1000.);
#29834=VECTOR('',#141240,1000.);
#29835=VECTOR('',#141243,1000.);
#29836=VECTOR('',#141248,1000.);
#29837=VECTOR('',#141249,1000.);
#29838=VECTOR('',#141252,1000.);
#29839=VECTOR('',#141257,1000.);
#29840=VECTOR('',#141258,1000.);
#29841=VECTOR('',#141261,1000.);
#29842=VECTOR('',#141266,1000.);
#29843=VECTOR('',#141267,1000.);
#29844=VECTOR('',#141270,1000.);
#29845=VECTOR('',#141275,1000.);
#29846=VECTOR('',#141276,1000.);
#29847=VECTOR('',#141279,1000.);
#29848=VECTOR('',#141284,1000.);
#29849=VECTOR('',#141285,1000.);
#29850=VECTOR('',#141288,1000.);
#29851=VECTOR('',#141293,1000.);
#29852=VECTOR('',#141296,1000.);
#29853=VECTOR('',#141297,1000.);
#29854=VECTOR('',#141308,1000.);
#29855=VECTOR('',#141311,1000.);
#29856=VECTOR('',#141314,1000.);
#29857=VECTOR('',#141317,1000.);
#29858=VECTOR('',#141320,1000.);
#29859=VECTOR('',#141321,1000.);
#29860=VECTOR('',#141322,1000.);
#29861=VECTOR('',#141325,1000.);
#29862=VECTOR('',#141330,1000.);
#29863=VECTOR('',#141331,1000.);
#29864=VECTOR('',#141334,1000.);
#29865=VECTOR('',#141339,1000.);
#29866=VECTOR('',#141340,1000.);
#29867=VECTOR('',#141343,1000.);
#29868=VECTOR('',#141348,1000.);
#29869=VECTOR('',#141349,1000.);
#29870=VECTOR('',#141358,1000.);
#29871=VECTOR('',#141359,1000.);
#29872=VECTOR('',#141360,1000.);
#29873=VECTOR('',#141361,1000.);
#29874=VECTOR('',#141364,1000.);
#29875=VECTOR('',#141365,1000.);
#29876=VECTOR('',#141366,1000.);
#29877=VECTOR('',#141367,1000.);
#29878=VECTOR('',#141370,1000.);
#29879=VECTOR('',#141371,1000.);
#29880=VECTOR('',#141372,1000.);
#29881=VECTOR('',#141373,1000.);
#29882=VECTOR('',#141376,1000.);
#29883=VECTOR('',#141377,1000.);
#29884=VECTOR('',#141378,1000.);
#29885=VECTOR('',#141381,1000.);
#29886=VECTOR('',#141382,1000.);
#29887=VECTOR('',#141383,1000.);
#29888=VECTOR('',#141390,1000.);
#29889=VECTOR('',#141393,1000.);
#29890=VECTOR('',#141394,1000.);
#29891=VECTOR('',#141395,1000.);
#29892=VECTOR('',#141402,1000.);
#29893=VECTOR('',#141405,1000.);
#29894=VECTOR('',#141406,1000.);
#29895=VECTOR('',#141407,1000.);
#29896=VECTOR('',#141414,1000.);
#29897=VECTOR('',#141417,1000.);
#29898=VECTOR('',#141418,1000.);
#29899=VECTOR('',#141419,1000.);
#29900=VECTOR('',#141426,1000.);
#29901=VECTOR('',#141429,1000.);
#29902=VECTOR('',#141430,1000.);
#29903=VECTOR('',#141431,1000.);
#29904=VECTOR('',#141434,1000.);
#29905=VECTOR('',#141435,1000.);
#29906=VECTOR('',#141436,1000.);
#29907=VECTOR('',#141439,1000.);
#29908=VECTOR('',#141440,1000.);
#29909=VECTOR('',#141441,1000.);
#29910=VECTOR('',#141444,1000.);
#29911=VECTOR('',#141445,1000.);
#29912=VECTOR('',#141446,1000.);
#29913=VECTOR('',#141449,1000.);
#29914=VECTOR('',#141450,1000.);
#29915=VECTOR('',#141451,1000.);
#29916=VECTOR('',#141452,1000.);
#29917=VECTOR('',#141455,1000.);
#29918=VECTOR('',#141456,1000.);
#29919=VECTOR('',#141457,1000.);
#29920=VECTOR('',#141460,1000.);
#29921=VECTOR('',#141461,1000.);
#29922=VECTOR('',#141462,1000.);
#29923=VECTOR('',#141465,1000.);
#29924=VECTOR('',#141466,1000.);
#29925=VECTOR('',#141467,1000.);
#29926=VECTOR('',#141474,1000.);
#29927=VECTOR('',#141477,1000.);
#29928=VECTOR('',#141478,1000.);
#29929=VECTOR('',#141479,1000.);
#29930=VECTOR('',#141486,1000.);
#29931=VECTOR('',#141489,1000.);
#29932=VECTOR('',#141490,1000.);
#29933=VECTOR('',#141491,1000.);
#29934=VECTOR('',#141498,1000.);
#29935=VECTOR('',#141501,1000.);
#29936=VECTOR('',#141502,1000.);
#29937=VECTOR('',#141503,1000.);
#29938=VECTOR('',#141510,1000.);
#29939=VECTOR('',#141513,1000.);
#29940=VECTOR('',#141514,1000.);
#29941=VECTOR('',#141515,1000.);
#29942=VECTOR('',#141518,1000.);
#29943=VECTOR('',#141519,1000.);
#29944=VECTOR('',#141520,1000.);
#29945=VECTOR('',#141523,1000.);
#29946=VECTOR('',#141524,1000.);
#29947=VECTOR('',#141525,1000.);
#29948=VECTOR('',#141528,1000.);
#29949=VECTOR('',#141529,1000.);
#29950=VECTOR('',#141530,1000.);
#29951=VECTOR('',#141537,1000.);
#29952=VECTOR('',#141540,1000.);
#29953=VECTOR('',#141541,1000.);
#29954=VECTOR('',#141542,1000.);
#29955=VECTOR('',#141549,1000.);
#29956=VECTOR('',#141552,1000.);
#29957=VECTOR('',#141553,1000.);
#29958=VECTOR('',#141554,1000.);
#29959=VECTOR('',#141563,1000.);
#29960=VECTOR('',#141564,1000.);
#29961=VECTOR('',#141565,1000.);
#29962=VECTOR('',#141566,1000.);
#29963=VECTOR('',#141573,1000.);
#29964=VECTOR('',#141576,1000.);
#29965=VECTOR('',#141577,1000.);
#29966=VECTOR('',#141578,1000.);
#29967=VECTOR('',#141581,1000.);
#29968=VECTOR('',#141582,1000.);
#29969=VECTOR('',#141583,1000.);
#29970=VECTOR('',#141586,1000.);
#29971=VECTOR('',#141587,1000.);
#29972=VECTOR('',#141588,1000.);
#29973=VECTOR('',#141591,1000.);
#29974=VECTOR('',#141592,1000.);
#29975=VECTOR('',#141593,1000.);
#29976=VECTOR('',#141600,1000.);
#29977=VECTOR('',#141603,1000.);
#29978=VECTOR('',#141604,1000.);
#29979=VECTOR('',#141605,1000.);
#29980=VECTOR('',#141608,1000.);
#29981=VECTOR('',#141609,1000.);
#29982=VECTOR('',#141610,1000.);
#29983=VECTOR('',#141613,1000.);
#29984=VECTOR('',#141614,1000.);
#29985=VECTOR('',#141615,1000.);
#29986=VECTOR('',#141618,1000.);
#29987=VECTOR('',#141619,1000.);
#29988=VECTOR('',#141620,1000.);
#29989=VECTOR('',#141627,1000.);
#29990=VECTOR('',#141630,1000.);
#29991=VECTOR('',#141631,1000.);
#29992=VECTOR('',#141632,1000.);
#29993=VECTOR('',#141639,1000.);
#29994=VECTOR('',#141642,1000.);
#29995=VECTOR('',#141643,1000.);
#29996=VECTOR('',#141644,1000.);
#29997=VECTOR('',#141651,1000.);
#29998=VECTOR('',#141654,1000.);
#29999=VECTOR('',#141655,1000.);
#30000=VECTOR('',#141656,1000.);
#30001=VECTOR('',#141663,1000.);
#30002=VECTOR('',#141666,1000.);
#30003=VECTOR('',#141667,1000.);
#30004=VECTOR('',#141670,1000.);
#30005=VECTOR('',#141671,1000.);
#30006=VECTOR('',#141672,1000.);
#30007=VECTOR('',#141673,1000.);
#30008=VECTOR('',#141676,1000.);
#30009=VECTOR('',#141677,1000.);
#30010=VECTOR('',#141678,1000.);
#30011=VECTOR('',#141681,1000.);
#30012=VECTOR('',#141682,1000.);
#30013=VECTOR('',#141683,1000.);
#30014=VECTOR('',#141690,1000.);
#30015=VECTOR('',#141693,1000.);
#30016=VECTOR('',#141694,1000.);
#30017=VECTOR('',#141695,1000.);
#30018=VECTOR('',#141702,1000.);
#30019=VECTOR('',#141705,1000.);
#30020=VECTOR('',#141706,1000.);
#30021=VECTOR('',#141707,1000.);
#30022=VECTOR('',#141714,1000.);
#30023=VECTOR('',#141717,1000.);
#30024=VECTOR('',#141718,1000.);
#30025=VECTOR('',#141719,1000.);
#30026=VECTOR('',#141726,1000.);
#30027=VECTOR('',#141729,1000.);
#30028=VECTOR('',#141730,1000.);
#30029=VECTOR('',#141731,1000.);
#30030=VECTOR('',#141734,1000.);
#30031=VECTOR('',#141735,1000.);
#30032=VECTOR('',#141736,1000.);
#30033=VECTOR('',#141739,1000.);
#30034=VECTOR('',#141740,1000.);
#30035=VECTOR('',#141743,1000.);
#30036=VECTOR('',#141744,1000.);
#30037=VECTOR('',#141745,1000.);
#30038=VECTOR('',#141746,1000.);
#30039=VECTOR('',#141749,1000.);
#30040=VECTOR('',#141750,1000.);
#30041=VECTOR('',#141751,1000.);
#30042=VECTOR('',#141754,1000.);
#30043=VECTOR('',#141755,1000.);
#30044=VECTOR('',#141756,1000.);
#30045=VECTOR('',#141759,1000.);
#30046=VECTOR('',#141760,1000.);
#30047=VECTOR('',#141761,1000.);
#30048=VECTOR('',#141768,1000.);
#30049=VECTOR('',#141771,1000.);
#30050=VECTOR('',#141772,1000.);
#30051=VECTOR('',#141773,1000.);
#30052=VECTOR('',#141780,1000.);
#30053=VECTOR('',#141783,1000.);
#30054=VECTOR('',#141784,1000.);
#30055=VECTOR('',#141785,1000.);
#30056=VECTOR('',#141792,1000.);
#30057=VECTOR('',#141795,1000.);
#30058=VECTOR('',#141796,1000.);
#30059=VECTOR('',#141797,1000.);
#30060=VECTOR('',#141804,1000.);
#30061=VECTOR('',#141807,1000.);
#30062=VECTOR('',#141808,1000.);
#30063=VECTOR('',#141809,1000.);
#30064=VECTOR('',#141812,1000.);
#30065=VECTOR('',#141813,1000.);
#30066=VECTOR('',#141814,1000.);
#30067=VECTOR('',#141817,1000.);
#30068=VECTOR('',#141818,1000.);
#30069=VECTOR('',#141819,1000.);
#30070=VECTOR('',#141822,1000.);
#30071=VECTOR('',#141823,1000.);
#30072=VECTOR('',#141824,1000.);
#30073=VECTOR('',#141831,1000.);
#30074=VECTOR('',#141834,1000.);
#30075=VECTOR('',#141835,1000.);
#30076=VECTOR('',#141836,1000.);
#30077=VECTOR('',#141843,1000.);
#30078=VECTOR('',#141846,1000.);
#30079=VECTOR('',#141847,1000.);
#30080=VECTOR('',#141848,1000.);
#30081=VECTOR('',#141855,1000.);
#30082=VECTOR('',#141858,1000.);
#30083=VECTOR('',#141859,1000.);
#30084=VECTOR('',#141860,1000.);
#30085=VECTOR('',#141867,1000.);
#30086=VECTOR('',#141870,1000.);
#30087=VECTOR('',#141871,1000.);
#30088=VECTOR('',#141872,1000.);
#30089=VECTOR('',#141875,1000.);
#30090=VECTOR('',#141876,1000.);
#30091=VECTOR('',#141877,1000.);
#30092=VECTOR('',#141880,1000.);
#30093=VECTOR('',#141881,1000.);
#30094=VECTOR('',#141882,1000.);
#30095=VECTOR('',#141885,1000.);
#30096=VECTOR('',#141886,1000.);
#30097=VECTOR('',#141887,1000.);
#30098=VECTOR('',#141894,1000.);
#30099=VECTOR('',#141897,1000.);
#30100=VECTOR('',#141898,1000.);
#30101=VECTOR('',#141899,1000.);
#30102=VECTOR('',#141902,1000.);
#30103=VECTOR('',#141903,1000.);
#30104=VECTOR('',#141904,1000.);
#30105=VECTOR('',#141907,1000.);
#30106=VECTOR('',#141908,1000.);
#30107=VECTOR('',#141909,1000.);
#30108=VECTOR('',#141912,1000.);
#30109=VECTOR('',#141913,1000.);
#30110=VECTOR('',#141914,1000.);
#30111=VECTOR('',#141921,1000.);
#30112=VECTOR('',#141924,1000.);
#30113=VECTOR('',#141925,1000.);
#30114=VECTOR('',#141926,1000.);
#30115=VECTOR('',#141933,1000.);
#30116=VECTOR('',#141936,1000.);
#30117=VECTOR('',#141937,1000.);
#30118=VECTOR('',#141938,1000.);
#30119=VECTOR('',#141945,1000.);
#30120=VECTOR('',#141948,1000.);
#30121=VECTOR('',#141949,1000.);
#30122=VECTOR('',#141950,1000.);
#30123=VECTOR('',#141957,1000.);
#30124=VECTOR('',#141960,1000.);
#30125=VECTOR('',#141961,1000.);
#30126=VECTOR('',#141964,1000.);
#30127=VECTOR('',#141965,1000.);
#30128=VECTOR('',#141966,1000.);
#30129=VECTOR('',#141967,1000.);
#30130=VECTOR('',#141970,1000.);
#30131=VECTOR('',#141971,1000.);
#30132=VECTOR('',#141972,1000.);
#30133=VECTOR('',#141975,1000.);
#30134=VECTOR('',#141976,1000.);
#30135=VECTOR('',#141977,1000.);
#30136=VECTOR('',#141984,1000.);
#30137=VECTOR('',#141987,1000.);
#30138=VECTOR('',#141988,1000.);
#30139=VECTOR('',#141989,1000.);
#30140=VECTOR('',#141996,1000.);
#30141=VECTOR('',#141999,1000.);
#30142=VECTOR('',#142000,1000.);
#30143=VECTOR('',#142001,1000.);
#30144=VECTOR('',#142008,1000.);
#30145=VECTOR('',#142011,1000.);
#30146=VECTOR('',#142012,1000.);
#30147=VECTOR('',#142013,1000.);
#30148=VECTOR('',#142020,1000.);
#30149=VECTOR('',#142023,1000.);
#30150=VECTOR('',#142024,1000.);
#30151=VECTOR('',#142025,1000.);
#30152=VECTOR('',#142028,1000.);
#30153=VECTOR('',#142029,1000.);
#30154=VECTOR('',#142030,1000.);
#30155=VECTOR('',#142033,1000.);
#30156=VECTOR('',#142034,1000.);
#30157=VECTOR('',#142037,1000.);
#30158=VECTOR('',#142038,1000.);
#30159=VECTOR('',#142039,1000.);
#30160=VECTOR('',#142040,1000.);
#30161=VECTOR('',#142043,1000.);
#30162=VECTOR('',#142044,1000.);
#30163=VECTOR('',#142045,1000.);
#30164=VECTOR('',#142048,1000.);
#30165=VECTOR('',#142049,1000.);
#30166=VECTOR('',#142050,1000.);
#30167=VECTOR('',#142053,1000.);
#30168=VECTOR('',#142054,1000.);
#30169=VECTOR('',#142055,1000.);
#30170=VECTOR('',#142062,1000.);
#30171=VECTOR('',#142065,1000.);
#30172=VECTOR('',#142066,1000.);
#30173=VECTOR('',#142067,1000.);
#30174=VECTOR('',#142074,1000.);
#30175=VECTOR('',#142077,1000.);
#30176=VECTOR('',#142078,1000.);
#30177=VECTOR('',#142079,1000.);
#30178=VECTOR('',#142086,1000.);
#30179=VECTOR('',#142089,1000.);
#30180=VECTOR('',#142090,1000.);
#30181=VECTOR('',#142091,1000.);
#30182=VECTOR('',#142098,1000.);
#30183=VECTOR('',#142101,1000.);
#30184=VECTOR('',#142102,1000.);
#30185=VECTOR('',#142103,1000.);
#30186=VECTOR('',#142106,1000.);
#30187=VECTOR('',#142107,1000.);
#30188=VECTOR('',#142108,1000.);
#30189=VECTOR('',#142111,1000.);
#30190=VECTOR('',#142112,1000.);
#30191=VECTOR('',#142113,1000.);
#30192=VECTOR('',#142116,1000.);
#30193=VECTOR('',#142117,1000.);
#30194=VECTOR('',#142118,1000.);
#30195=VECTOR('',#142125,1000.);
#30196=VECTOR('',#142128,1000.);
#30197=VECTOR('',#142129,1000.);
#30198=VECTOR('',#142130,1000.);
#30199=VECTOR('',#142137,1000.);
#30200=VECTOR('',#142140,1000.);
#30201=VECTOR('',#142141,1000.);
#30202=VECTOR('',#142142,1000.);
#30203=VECTOR('',#142149,1000.);
#30204=VECTOR('',#142152,1000.);
#30205=VECTOR('',#142153,1000.);
#30206=VECTOR('',#142154,1000.);
#30207=VECTOR('',#142161,1000.);
#30208=VECTOR('',#142164,1000.);
#30209=VECTOR('',#142165,1000.);
#30210=VECTOR('',#142166,1000.);
#30211=VECTOR('',#142169,1000.);
#30212=VECTOR('',#142170,1000.);
#30213=VECTOR('',#142171,1000.);
#30214=VECTOR('',#142174,1000.);
#30215=VECTOR('',#142175,1000.);
#30216=VECTOR('',#142176,1000.);
#30217=VECTOR('',#142179,1000.);
#30218=VECTOR('',#142180,1000.);
#30219=VECTOR('',#142181,1000.);
#30220=VECTOR('',#142188,1000.);
#30221=VECTOR('',#142191,1000.);
#30222=VECTOR('',#142192,1000.);
#30223=VECTOR('',#142193,1000.);
#30224=VECTOR('',#142196,1000.);
#30225=VECTOR('',#142197,1000.);
#30226=VECTOR('',#142198,1000.);
#30227=VECTOR('',#142201,1000.);
#30228=VECTOR('',#142202,1000.);
#30229=VECTOR('',#142203,1000.);
#30230=VECTOR('',#142206,1000.);
#30231=VECTOR('',#142207,1000.);
#30232=VECTOR('',#142208,1000.);
#30233=VECTOR('',#142215,1000.);
#30234=VECTOR('',#142218,1000.);
#30235=VECTOR('',#142219,1000.);
#30236=VECTOR('',#142220,1000.);
#30237=VECTOR('',#142227,1000.);
#30238=VECTOR('',#142230,1000.);
#30239=VECTOR('',#142231,1000.);
#30240=VECTOR('',#142232,1000.);
#30241=VECTOR('',#142239,1000.);
#30242=VECTOR('',#142242,1000.);
#30243=VECTOR('',#142243,1000.);
#30244=VECTOR('',#142244,1000.);
#30245=VECTOR('',#142251,1000.);
#30246=VECTOR('',#142254,1000.);
#30247=VECTOR('',#142255,1000.);
#30248=VECTOR('',#142258,1000.);
#30249=VECTOR('',#142259,1000.);
#30250=VECTOR('',#142260,1000.);
#30251=VECTOR('',#142261,1000.);
#30252=VECTOR('',#142264,1000.);
#30253=VECTOR('',#142265,1000.);
#30254=VECTOR('',#142266,1000.);
#30255=VECTOR('',#142269,1000.);
#30256=VECTOR('',#142270,1000.);
#30257=VECTOR('',#142271,1000.);
#30258=VECTOR('',#142278,1000.);
#30259=VECTOR('',#142281,1000.);
#30260=VECTOR('',#142282,1000.);
#30261=VECTOR('',#142283,1000.);
#30262=VECTOR('',#142290,1000.);
#30263=VECTOR('',#142293,1000.);
#30264=VECTOR('',#142294,1000.);
#30265=VECTOR('',#142295,1000.);
#30266=VECTOR('',#142302,1000.);
#30267=VECTOR('',#142305,1000.);
#30268=VECTOR('',#142306,1000.);
#30269=VECTOR('',#142307,1000.);
#30270=VECTOR('',#142314,1000.);
#30271=VECTOR('',#142317,1000.);
#30272=VECTOR('',#142318,1000.);
#30273=VECTOR('',#142319,1000.);
#30274=VECTOR('',#142322,1000.);
#30275=VECTOR('',#142323,1000.);
#30276=VECTOR('',#142324,1000.);
#30277=VECTOR('',#142327,1000.);
#30278=VECTOR('',#142328,1000.);
#30279=VECTOR('',#142331,1000.);
#30280=VECTOR('',#142332,1000.);
#30281=VECTOR('',#142333,1000.);
#30282=VECTOR('',#142336,1000.);
#30283=VECTOR('',#142337,1000.);
#30284=VECTOR('',#142338,1000.);
#30285=VECTOR('',#142341,1000.);
#30286=VECTOR('',#142342,1000.);
#30287=VECTOR('',#142343,1000.);
#30288=VECTOR('',#142350,1000.);
#30289=VECTOR('',#142353,1000.);
#30290=VECTOR('',#142354,1000.);
#30291=VECTOR('',#142355,1000.);
#30292=VECTOR('',#142362,1000.);
#30293=VECTOR('',#142365,1000.);
#30294=VECTOR('',#142366,1000.);
#30295=VECTOR('',#142367,1000.);
#30296=VECTOR('',#142374,1000.);
#30297=VECTOR('',#142377,1000.);
#30298=VECTOR('',#142378,1000.);
#30299=VECTOR('',#142379,1000.);
#30300=VECTOR('',#142386,1000.);
#30301=VECTOR('',#142389,1000.);
#30302=VECTOR('',#142390,1000.);
#30303=VECTOR('',#142391,1000.);
#30304=VECTOR('',#142394,1000.);
#30305=VECTOR('',#142395,1000.);
#30306=VECTOR('',#142396,1000.);
#30307=VECTOR('',#142399,1000.);
#30308=VECTOR('',#142400,1000.);
#30309=VECTOR('',#142401,1000.);
#30310=VECTOR('',#142404,1000.);
#30311=VECTOR('',#142405,1000.);
#30312=VECTOR('',#142406,1000.);
#30313=VECTOR('',#142413,1000.);
#30314=VECTOR('',#142416,1000.);
#30315=VECTOR('',#142417,1000.);
#30316=VECTOR('',#142418,1000.);
#30317=VECTOR('',#142425,1000.);
#30318=VECTOR('',#142428,1000.);
#30319=VECTOR('',#142429,1000.);
#30320=VECTOR('',#142430,1000.);
#30321=VECTOR('',#142437,1000.);
#30322=VECTOR('',#142440,1000.);
#30323=VECTOR('',#142441,1000.);
#30324=VECTOR('',#142442,1000.);
#30325=VECTOR('',#142449,1000.);
#30326=VECTOR('',#142452,1000.);
#30327=VECTOR('',#142453,1000.);
#30328=VECTOR('',#142454,1000.);
#30329=VECTOR('',#142457,1000.);
#30330=VECTOR('',#142458,1000.);
#30331=VECTOR('',#142459,1000.);
#30332=VECTOR('',#142462,1000.);
#30333=VECTOR('',#142463,1000.);
#30334=VECTOR('',#142464,1000.);
#30335=VECTOR('',#142467,1000.);
#30336=VECTOR('',#142468,1000.);
#30337=VECTOR('',#142469,1000.);
#30338=VECTOR('',#142476,1000.);
#30339=VECTOR('',#142479,1000.);
#30340=VECTOR('',#142480,1000.);
#30341=VECTOR('',#142481,1000.);
#30342=VECTOR('',#142484,1000.);
#30343=VECTOR('',#142485,1000.);
#30344=VECTOR('',#142486,1000.);
#30345=VECTOR('',#142489,1000.);
#30346=VECTOR('',#142490,1000.);
#30347=VECTOR('',#142491,1000.);
#30348=VECTOR('',#142494,1000.);
#30349=VECTOR('',#142495,1000.);
#30350=VECTOR('',#142496,1000.);
#30351=VECTOR('',#142503,1000.);
#30352=VECTOR('',#142506,1000.);
#30353=VECTOR('',#142507,1000.);
#30354=VECTOR('',#142508,1000.);
#30355=VECTOR('',#142515,1000.);
#30356=VECTOR('',#142518,1000.);
#30357=VECTOR('',#142519,1000.);
#30358=VECTOR('',#142520,1000.);
#30359=VECTOR('',#142527,1000.);
#30360=VECTOR('',#142530,1000.);
#30361=VECTOR('',#142531,1000.);
#30362=VECTOR('',#142532,1000.);
#30363=VECTOR('',#142539,1000.);
#30364=VECTOR('',#142542,1000.);
#30365=VECTOR('',#142543,1000.);
#30366=VECTOR('',#142546,1000.);
#30367=VECTOR('',#142547,1000.);
#30368=VECTOR('',#142548,1000.);
#30369=VECTOR('',#142551,1000.);
#30370=VECTOR('',#142552,1000.);
#30371=VECTOR('',#142555,1000.);
#30372=VECTOR('',#142556,1000.);
#30373=VECTOR('',#142557,1000.);
#30374=VECTOR('',#142560,1000.);
#30375=VECTOR('',#142561,1000.);
#30376=VECTOR('',#142564,1000.);
#30377=VECTOR('',#142565,1000.);
#30378=VECTOR('',#142566,1000.);
#30379=VECTOR('',#142567,1000.);
#30380=VECTOR('',#142568,1000.);
#30381=VECTOR('',#142569,1000.);
#30382=VECTOR('',#142570,1000.);
#30383=VECTOR('',#142571,1000.);
#30384=VECTOR('',#142574,1000.);
#30385=VECTOR('',#142575,1000.);
#30386=VECTOR('',#142576,1000.);
#30387=VECTOR('',#142579,1000.);
#30388=VECTOR('',#142580,1000.);
#30389=VECTOR('',#142583,1000.);
#30390=VECTOR('',#142584,1000.);
#30391=VECTOR('',#142587,1000.);
#30392=VECTOR('',#142588,1000.);
#30393=VECTOR('',#142591,1000.);
#30394=VECTOR('',#142592,1000.);
#30395=VECTOR('',#142595,1000.);
#30396=VECTOR('',#142596,1000.);
#30397=VECTOR('',#142599,1000.);
#30398=VECTOR('',#142600,1000.);
#30399=VECTOR('',#142603,1000.);
#30400=VECTOR('',#142608,1000.);
#30401=VECTOR('',#142609,1000.);
#30402=VECTOR('',#142610,1000.);
#30403=VECTOR('',#142611,1000.);
#30404=VECTOR('',#142614,1000.);
#30405=VECTOR('',#142615,1000.);
#30406=VECTOR('',#142616,1000.);
#30407=VECTOR('',#142619,1000.);
#30408=VECTOR('',#142620,1000.);
#30409=VECTOR('',#142621,1000.);
#30410=VECTOR('',#142624,1000.);
#30411=VECTOR('',#142625,1000.);
#30412=CIRCLE('',#98805,8.4455);
#30413=CIRCLE('',#98806,8.4455);
#30414=CIRCLE('',#98808,8.4455);
#30415=CIRCLE('',#98809,8.4455);
#30416=CIRCLE('',#98811,8.4455);
#30417=CIRCLE('',#98812,8.4455);
#30418=CIRCLE('',#98814,8.4455);
#30419=CIRCLE('',#98815,8.4455);
#30420=CIRCLE('',#98838,23.);
#30421=CIRCLE('',#98839,23.);
#30422=CIRCLE('',#98840,23.);
#30423=CIRCLE('',#98841,23.);
#30424=CIRCLE('',#98843,25.);
#30425=CIRCLE('',#98844,25.);
#30426=CIRCLE('',#98845,25.);
#30427=CIRCLE('',#98846,25.);
#30428=CIRCLE('',#98852,25.);
#30429=CIRCLE('',#98854,25.);
#30430=CIRCLE('',#98856,25.);
#30431=CIRCLE('',#98858,25.);
#30432=CIRCLE('',#98860,2.);
#30433=CIRCLE('',#98861,2.);
#30434=CIRCLE('',#98863,2.);
#30435=CIRCLE('',#98865,2.);
#30436=CIRCLE('',#98867,2.);
#30437=CIRCLE('',#98869,2.);
#30438=CIRCLE('',#98871,2.);
#30439=CIRCLE('',#98873,2.);
#30440=CIRCLE('',#98877,9.00000000000018);
#30441=CIRCLE('',#98878,9.00000000000018);
#30442=CIRCLE('',#98879,0.254);
#30443=CIRCLE('',#98880,9.25400000000018);
#30444=CIRCLE('',#98882,11.0630000000002);
#30445=CIRCLE('',#98883,0.254);
#30446=CIRCLE('',#98884,11.3170000000002);
#30447=CIRCLE('',#98885,11.3170000000002);
#30448=CIRCLE('',#98891,11.3170000000002);
#30449=CIRCLE('',#98893,9.00000000000017);
#30450=CIRCLE('',#98905,15.0000000000002);
#30451=CIRCLE('',#98914,39.);
#30452=CIRCLE('',#98928,15.);
#30453=CIRCLE('',#98930,11.4440000000002);
#30454=CIRCLE('',#98931,11.444);
#30455=CIRCLE('',#98933,18.0480155876192);
#30456=CIRCLE('',#98941,2.94003217057229);
#30457=CIRCLE('',#98942,1.57226);
#30458=CIRCLE('',#98943,3.78554799125932);
#30459=CIRCLE('',#98944,3.78554799125932);
#30460=CIRCLE('',#98947,5.55625);
#30461=CIRCLE('',#98949,5.1435);
#30462=CIRCLE('',#98950,5.1435);
#30463=CIRCLE('',#98952,5.55625);
#30464=CIRCLE('',#98953,5.55625);
#30465=CIRCLE('',#98955,5.55625);
#30466=CIRCLE('',#98956,5.55625);
#30467=CIRCLE('',#98957,5.55625);
#30468=CIRCLE('',#98958,5.55625);
#30469=CIRCLE('',#98959,5.55625);
#30470=CIRCLE('',#98961,3.3479996643018);
#30471=CIRCLE('',#98963,3.31406494267269);
#30472=CIRCLE('',#98964,3.31406494267269);
#30473=CIRCLE('',#98965,0.635000000000008);
#30474=CIRCLE('',#98967,2.40973730802039);
#30475=CIRCLE('',#98968,2.40973730802039);
#30476=CIRCLE('',#98970,2.1119189867422);
#30477=CIRCLE('',#98971,0.317500000000003);
#30478=CIRCLE('',#98973,0.952499999999998);
#30479=CIRCLE('',#98974,0.952499999999998);
#30480=CIRCLE('',#98984,5.55625);
#30481=CIRCLE('',#98985,5.55625);
#30482=CIRCLE('',#98986,5.55625);
#30483=CIRCLE('',#98987,5.55625);
#30484=CIRCLE('',#98988,5.55625);
#30485=CIRCLE('',#99006,7.9375);
#30486=CIRCLE('',#99007,7.9375);
#30487=CIRCLE('',#99009,8.4455);
#30488=CIRCLE('',#99010,8.4455);
#30489=CIRCLE('',#99014,7.9375);
#30490=CIRCLE('',#99015,7.9375);
#30491=CIRCLE('',#99017,8.4455);
#30492=CIRCLE('',#99018,8.4455);
#30493=CIRCLE('',#99022,7.9375);
#30494=CIRCLE('',#99023,7.9375);
#30495=CIRCLE('',#99025,8.4455);
#30496=CIRCLE('',#99026,8.4455);
#30497=CIRCLE('',#99030,7.9375);
#30498=CIRCLE('',#99031,7.9375);
#30499=CIRCLE('',#99033,8.4455);
#30500=CIRCLE('',#99034,8.4455);
#30501=CIRCLE('',#99038,50.);
#30502=CIRCLE('',#99039,50.);
#30503=CIRCLE('',#99040,0.254);
#30504=CIRCLE('',#99041,50.254);
#30505=CIRCLE('',#99043,51.016);
#30506=CIRCLE('',#99044,0.254);
#30507=CIRCLE('',#99045,51.27);
#30508=CIRCLE('',#99046,51.27);
#30509=CIRCLE('',#99048,51.27);
#30510=CIRCLE('',#99050,50.);
#30511=CIRCLE('',#99054,56.621);
#30512=CIRCLE('',#99055,0.254);
#30513=CIRCLE('',#99056,56.875);
#30514=CIRCLE('',#99057,56.875);
#30515=CIRCLE('',#99059,55.605);
#30516=CIRCLE('',#99060,55.605);
#30517=CIRCLE('',#99061,0.254);
#30518=CIRCLE('',#99062,55.859);
#30519=CIRCLE('',#99064,56.875);
#30520=CIRCLE('',#99066,55.605);
#30521=CIRCLE('',#99070,51.27);
#30522=CIRCLE('',#99071,51.27);
#30523=CIRCLE('',#99073,55.605);
#30524=CIRCLE('',#99074,55.605);
#30525=CIRCLE('',#99078,59.0285554514622);
#30526=CIRCLE('',#99079,0.127000000000002);
#30527=CIRCLE('',#99080,58.9208533432504);
#30528=CIRCLE('',#99081,0.127000000000002);
#30529=CIRCLE('',#99083,62.9541466567496);
#30530=CIRCLE('',#99084,0.127000000000002);
#30531=CIRCLE('',#99085,62.8464445485378);
#30532=CIRCLE('',#99086,0.127000000000002);
#30533=CIRCLE('',#99088,59.0285554514622);
#30534=CIRCLE('',#99089,0.127000000000002);
#30535=CIRCLE('',#99090,58.9208533432504);
#30536=CIRCLE('',#99091,0.127000000000002);
#30537=CIRCLE('',#99093,62.9541466567496);
#30538=CIRCLE('',#99094,0.127000000000002);
#30539=CIRCLE('',#99095,62.8464445485378);
#30540=CIRCLE('',#99096,0.127000000000002);
#30541=CIRCLE('',#99097,62.9541466567496);
#30542=CIRCLE('',#99099,58.2189663438286);
#30543=CIRCLE('',#99100,0.635);
#30544=CIRCLE('',#99101,57.6804558027693);
#30545=CIRCLE('',#99102,57.6804558027693);
#30546=CIRCLE('',#99104,58.8470884664677);
#30547=CIRCLE('',#99105,0.635);
#30548=CIRCLE('',#99106,58.3085779254084);
#30549=CIRCLE('',#99108,63.5664220745916);
#30550=CIRCLE('',#99109,0.635);
#30551=CIRCLE('',#99110,63.0279115335323);
#30552=CIRCLE('',#99111,63.0279115335323);
#30553=CIRCLE('',#99113,64.1945441972308);
#30554=CIRCLE('',#99114,0.635);
#30555=CIRCLE('',#99115,63.6560336561714);
#30556=CIRCLE('',#99117,65.);
#30557=CIRCLE('',#99118,65.);
#30558=CIRCLE('',#99121,62.9541466567496);
#30559=CIRCLE('',#99122,62.4089800241499);
#30560=CIRCLE('',#99123,62.9541466567496);
#30561=CIRCLE('',#99124,62.4089800241499);
#30562=CIRCLE('',#99125,62.9541466567496);
#30563=CIRCLE('',#99126,62.4089800241499);
#30564=CIRCLE('',#99127,62.9541466567497);
#30565=CIRCLE('',#99128,62.4089800241499);
#30566=CIRCLE('',#99129,62.9541466567496);
#30567=CIRCLE('',#99130,62.4089800241499);
#30568=CIRCLE('',#99131,62.9541466567496);
#30569=CIRCLE('',#99132,62.4089800241499);
#30570=CIRCLE('',#99133,62.9541466567497);
#30571=CIRCLE('',#99134,62.4089800241499);
#30572=CIRCLE('',#99135,62.9541466567497);
#30573=CIRCLE('',#99136,62.4089800241499);
#30574=CIRCLE('',#99137,62.9541466567496);
#30575=CIRCLE('',#99138,62.4089800241499);
#30576=CIRCLE('',#99139,62.9541466567497);
#30577=CIRCLE('',#99140,62.4089800241499);
#30578=CIRCLE('',#99141,62.9541466567496);
#30579=CIRCLE('',#99142,62.4089800241499);
#30580=CIRCLE('',#99143,62.9541466567497);
#30581=CIRCLE('',#99144,62.4089800241499);
#30582=CIRCLE('',#99145,62.9541466567497);
#30583=CIRCLE('',#99146,62.4089800241499);
#30584=CIRCLE('',#99147,62.9541466567496);
#30585=CIRCLE('',#99148,62.4089800241499);
#30586=CIRCLE('',#99149,62.9541466567497);
#30587=CIRCLE('',#99150,62.4089800241499);
#30588=CIRCLE('',#99151,62.9541466567496);
#30589=CIRCLE('',#99152,62.4089800241499);
#30590=CIRCLE('',#99153,62.9541466567497);
#30591=CIRCLE('',#99154,62.4089800241499);
#30592=CIRCLE('',#99155,62.9541466567497);
#30593=CIRCLE('',#99156,62.4089800241499);
#30594=CIRCLE('',#99157,62.9541466567496);
#30595=CIRCLE('',#99158,62.4089800241499);
#30596=CIRCLE('',#99159,62.9541466567496);
#30597=CIRCLE('',#99160,62.4089800241499);
#30598=CIRCLE('',#99161,62.9541466567496);
#30599=CIRCLE('',#99162,62.4089800241499);
#30600=CIRCLE('',#99163,62.9541466567496);
#30601=CIRCLE('',#99164,62.4089800241499);
#30602=CIRCLE('',#99165,62.9541466567497);
#30603=CIRCLE('',#99166,62.4089800241499);
#30604=CIRCLE('',#99167,62.9541466567497);
#30605=CIRCLE('',#99168,62.4089800241499);
#30606=CIRCLE('',#99169,62.9541466567496);
#30607=CIRCLE('',#99170,62.4089800241499);
#30608=CIRCLE('',#99171,62.9541466567496);
#30609=CIRCLE('',#99172,62.4089800241499);
#30610=CIRCLE('',#99173,62.9541466567496);
#30611=CIRCLE('',#99174,62.4089800241499);
#30612=CIRCLE('',#99175,62.9541466567497);
#30613=CIRCLE('',#99176,62.4089800241499);
#30614=CIRCLE('',#99177,62.9541466567496);
#30615=CIRCLE('',#99178,62.4089800241499);
#30616=CIRCLE('',#99179,62.9541466567497);
#30617=CIRCLE('',#99180,62.4089800241499);
#30618=CIRCLE('',#99181,62.4089800241499);
#30619=CIRCLE('',#99182,62.9541466567497);
#30620=CIRCLE('',#99183,62.4089800241499);
#30621=CIRCLE('',#99184,62.9541466567496);
#30622=CIRCLE('',#99185,62.4089800241499);
#30623=CIRCLE('',#99186,62.9541466567496);
#30624=CIRCLE('',#99187,62.4089800241499);
#30625=CIRCLE('',#99188,62.9541466567496);
#30626=CIRCLE('',#99189,62.4089800241499);
#30627=CIRCLE('',#99190,62.9541466567497);
#30628=CIRCLE('',#99191,62.4089800241499);
#30629=CIRCLE('',#99192,62.9541466567496);
#30630=CIRCLE('',#99193,62.4089800241499);
#30631=CIRCLE('',#99194,62.9541466567497);
#30632=CIRCLE('',#99195,62.4089800241499);
#30633=CIRCLE('',#99196,62.9541466567497);
#30634=CIRCLE('',#99197,62.4089800241499);
#30635=CIRCLE('',#99198,62.9541466567497);
#30636=CIRCLE('',#99199,62.4089800241499);
#30637=CIRCLE('',#99200,62.9541466567496);
#30638=CIRCLE('',#99201,62.4089800241499);
#30639=CIRCLE('',#99202,62.9541466567496);
#30640=CIRCLE('',#99203,62.4089800241499);
#30641=CIRCLE('',#99204,62.9541466567496);
#30642=CIRCLE('',#99205,62.4089800241499);
#30643=CIRCLE('',#99206,62.9541466567497);
#30644=CIRCLE('',#99207,62.4089800241499);
#30645=CIRCLE('',#99208,62.9541466567496);
#30646=CIRCLE('',#99209,62.4089800241499);
#30647=CIRCLE('',#99210,62.4089800241499);
#30648=CIRCLE('',#99211,62.9541466567497);
#30649=CIRCLE('',#99212,62.4089800241499);
#30650=CIRCLE('',#99213,62.9541466567497);
#30651=CIRCLE('',#99214,62.4089800241499);
#30652=CIRCLE('',#99215,62.9541466567497);
#30653=CIRCLE('',#99216,62.4089800241499);
#30654=CIRCLE('',#99217,62.9541466567497);
#30655=CIRCLE('',#99218,62.4089800241499);
#30656=CIRCLE('',#99219,62.9541466567497);
#30657=CIRCLE('',#99220,62.4089800241499);
#30658=CIRCLE('',#99221,62.9541466567496);
#30659=CIRCLE('',#99222,62.4089800241499);
#30660=CIRCLE('',#99223,62.9541466567496);
#30661=CIRCLE('',#99224,62.4089800241499);
#30662=CIRCLE('',#99225,62.9541466567496);
#30663=CIRCLE('',#99226,62.4089800241499);
#30664=CIRCLE('',#99227,62.9541466567497);
#30665=CIRCLE('',#99228,62.4089800241499);
#30666=CIRCLE('',#99229,62.9541466567496);
#30667=CIRCLE('',#99230,62.4089800241499);
#30668=CIRCLE('',#99231,62.9541466567497);
#30669=CIRCLE('',#99232,62.4089800241499);
#30670=CIRCLE('',#99233,62.9541466567497);
#30671=CIRCLE('',#99234,62.4089800241499);
#30672=CIRCLE('',#99235,62.9541466567497);
#30673=CIRCLE('',#99236,62.4089800241499);
#30674=CIRCLE('',#99237,62.9541466567497);
#30675=CIRCLE('',#99238,62.4089800241499);
#30676=CIRCLE('',#99240,59.4660199758502);
#30677=CIRCLE('',#99241,58.9208533432504);
#30678=CIRCLE('',#99242,59.4660199758502);
#30679=CIRCLE('',#99243,58.9208533432504);
#30680=CIRCLE('',#99244,59.4660199758502);
#30681=CIRCLE('',#99245,58.9208533432504);
#30682=CIRCLE('',#99246,59.4660199758502);
#30683=CIRCLE('',#99247,58.9208533432504);
#30684=CIRCLE('',#99248,59.4660199758502);
#30685=CIRCLE('',#99249,58.9208533432504);
#30686=CIRCLE('',#99250,59.4660199758502);
#30687=CIRCLE('',#99251,58.9208533432504);
#30688=CIRCLE('',#99252,59.4660199758502);
#30689=CIRCLE('',#99253,58.9208533432504);
#30690=CIRCLE('',#99254,59.4660199758502);
#30691=CIRCLE('',#99255,58.9208533432504);
#30692=CIRCLE('',#99256,59.4660199758502);
#30693=CIRCLE('',#99257,58.9208533432504);
#30694=CIRCLE('',#99258,59.4660199758502);
#30695=CIRCLE('',#99259,58.9208533432504);
#30696=CIRCLE('',#99260,59.4660199758502);
#30697=CIRCLE('',#99261,58.9208533432504);
#30698=CIRCLE('',#99262,59.4660199758502);
#30699=CIRCLE('',#99263,58.9208533432504);
#30700=CIRCLE('',#99264,59.4660199758502);
#30701=CIRCLE('',#99265,58.9208533432504);
#30702=CIRCLE('',#99266,59.4660199758502);
#30703=CIRCLE('',#99267,58.9208533432504);
#30704=CIRCLE('',#99268,59.4660199758502);
#30705=CIRCLE('',#99269,58.9208533432504);
#30706=CIRCLE('',#99270,59.4660199758502);
#30707=CIRCLE('',#99271,58.9208533432504);
#30708=CIRCLE('',#99272,59.4660199758502);
#30709=CIRCLE('',#99273,58.9208533432504);
#30710=CIRCLE('',#99274,59.4660199758502);
#30711=CIRCLE('',#99275,58.9208533432504);
#30712=CIRCLE('',#99276,59.4660199758502);
#30713=CIRCLE('',#99277,58.9208533432504);
#30714=CIRCLE('',#99278,59.4660199758502);
#30715=CIRCLE('',#99279,58.9208533432504);
#30716=CIRCLE('',#99280,59.4660199758502);
#30717=CIRCLE('',#99281,58.9208533432504);
#30718=CIRCLE('',#99282,59.4660199758502);
#30719=CIRCLE('',#99283,58.9208533432504);
#30720=CIRCLE('',#99284,59.4660199758502);
#30721=CIRCLE('',#99285,58.9208533432504);
#30722=CIRCLE('',#99286,59.4660199758502);
#30723=CIRCLE('',#99287,58.9208533432504);
#30724=CIRCLE('',#99288,59.4660199758502);
#30725=CIRCLE('',#99289,58.9208533432504);
#30726=CIRCLE('',#99290,59.4660199758502);
#30727=CIRCLE('',#99291,58.9208533432504);
#30728=CIRCLE('',#99292,59.4660199758502);
#30729=CIRCLE('',#99293,58.9208533432504);
#30730=CIRCLE('',#99294,59.4660199758502);
#30731=CIRCLE('',#99295,58.9208533432504);
#30732=CIRCLE('',#99296,59.4660199758502);
#30733=CIRCLE('',#99297,58.9208533432504);
#30734=CIRCLE('',#99298,59.4660199758502);
#30735=CIRCLE('',#99299,58.9208533432504);
#30736=CIRCLE('',#99300,58.9208533432504);
#30737=CIRCLE('',#99301,59.4660199758502);
#30738=CIRCLE('',#99302,58.9208533432504);
#30739=CIRCLE('',#99303,59.4660199758502);
#30740=CIRCLE('',#99304,58.9208533432504);
#30741=CIRCLE('',#99305,59.4660199758502);
#30742=CIRCLE('',#99306,58.9208533432504);
#30743=CIRCLE('',#99307,59.4660199758502);
#30744=CIRCLE('',#99308,58.9208533432504);
#30745=CIRCLE('',#99309,59.4660199758502);
#30746=CIRCLE('',#99310,58.9208533432504);
#30747=CIRCLE('',#99311,59.4660199758502);
#30748=CIRCLE('',#99312,58.9208533432504);
#30749=CIRCLE('',#99313,59.4660199758502);
#30750=CIRCLE('',#99314,58.9208533432504);
#30751=CIRCLE('',#99315,59.4660199758502);
#30752=CIRCLE('',#99316,58.9208533432504);
#30753=CIRCLE('',#99317,59.4660199758502);
#30754=CIRCLE('',#99318,58.9208533432504);
#30755=CIRCLE('',#99319,59.4660199758502);
#30756=CIRCLE('',#99320,58.9208533432504);
#30757=CIRCLE('',#99321,59.4660199758502);
#30758=CIRCLE('',#99322,58.9208533432504);
#30759=CIRCLE('',#99323,59.4660199758502);
#30760=CIRCLE('',#99324,58.9208533432504);
#30761=CIRCLE('',#99325,59.4660199758502);
#30762=CIRCLE('',#99326,58.9208533432504);
#30763=CIRCLE('',#99327,59.4660199758502);
#30764=CIRCLE('',#99328,58.9208533432504);
#30765=CIRCLE('',#99329,59.4660199758502);
#30766=CIRCLE('',#99330,59.4660199758502);
#30767=CIRCLE('',#99331,58.9208533432504);
#30768=CIRCLE('',#99332,59.4660199758502);
#30769=CIRCLE('',#99333,58.9208533432504);
#30770=CIRCLE('',#99334,59.4660199758502);
#30771=CIRCLE('',#99335,58.9208533432504);
#30772=CIRCLE('',#99336,59.4660199758502);
#30773=CIRCLE('',#99337,58.9208533432504);
#30774=CIRCLE('',#99338,59.4660199758502);
#30775=CIRCLE('',#99339,58.9208533432504);
#30776=CIRCLE('',#99340,59.4660199758502);
#30777=CIRCLE('',#99341,58.9208533432504);
#30778=CIRCLE('',#99342,59.4660199758502);
#30779=CIRCLE('',#99343,58.9208533432504);
#30780=CIRCLE('',#99344,59.4660199758502);
#30781=CIRCLE('',#99345,58.9208533432504);
#30782=CIRCLE('',#99346,59.4660199758502);
#30783=CIRCLE('',#99347,58.9208533432504);
#30784=CIRCLE('',#99348,59.4660199758502);
#30785=CIRCLE('',#99349,58.9208533432504);
#30786=CIRCLE('',#99350,59.4660199758502);
#30787=CIRCLE('',#99351,58.9208533432504);
#30788=CIRCLE('',#99352,59.4660199758502);
#30789=CIRCLE('',#99353,58.9208533432504);
#30790=CIRCLE('',#99354,59.4660199758502);
#30791=CIRCLE('',#99355,58.9208533432504);
#30792=CIRCLE('',#99356,59.4660199758502);
#30793=CIRCLE('',#99357,58.9208533432504);
#30794=CIRCLE('',#99358,59.4660199758502);
#30795=CIRCLE('',#99360,56.875);
#30796=CIRCLE('',#99361,56.875);
#30797=CIRCLE('',#99363,56.875);
#30798=CIRCLE('',#99365,60.4792282238308);
#30799=CIRCLE('',#99366,60.0045305169095);
#30800=CIRCLE('',#99367,60.4792282238308);
#30801=CIRCLE('',#99368,60.4792282238308);
#30802=CIRCLE('',#99370,60.6419265158129);
#30803=CIRCLE('',#99372,61.0131030316259);
#30804=CIRCLE('',#99373,60.8618969683742);
#30805=CIRCLE('',#99375,61.3957717761693);
#30806=CIRCLE('',#99376,61.2330734841871);
#30807=CIRCLE('',#99377,61.3957717761693);
#30808=CIRCLE('',#99378,61.3957717761693);
#30809=CIRCLE('',#99380,61.8704694830905);
#30810=CIRCLE('',#99382,0.635007073208601);
#30811=CIRCLE('',#99383,0.635007073208629);
#30812=CIRCLE('',#99394,60.0045305169095);
#30813=CIRCLE('',#99395,60.4792282238308);
#30814=CIRCLE('',#99396,60.4792282238308);
#30815=CIRCLE('',#99397,60.4792282238308);
#30816=CIRCLE('',#99399,60.6419265158129);
#30817=CIRCLE('',#99401,60.8618969683742);
#30818=CIRCLE('',#99402,61.0131030316259);
#30819=CIRCLE('',#99404,61.2330734841871);
#30820=CIRCLE('',#99405,61.3957717761693);
#30821=CIRCLE('',#99406,61.3957717761693);
#30822=CIRCLE('',#99407,61.3957717761693);
#30823=CIRCLE('',#99409,61.8704694830905);
#30824=CIRCLE('',#99411,0.635007073208607);
#30825=CIRCLE('',#99412,0.635007073208605);
#30826=CIRCLE('',#99423,60.0045305169095);
#30827=CIRCLE('',#99424,60.4792282238308);
#30828=CIRCLE('',#99425,60.4792282238308);
#30829=CIRCLE('',#99426,60.4792282238308);
#30830=CIRCLE('',#99428,60.6419265158129);
#30831=CIRCLE('',#99430,60.8618969683742);
#30832=CIRCLE('',#99431,61.0131030316259);
#30833=CIRCLE('',#99433,61.2330734841871);
#30834=CIRCLE('',#99434,61.3957717761693);
#30835=CIRCLE('',#99435,61.3957717761693);
#30836=CIRCLE('',#99436,61.3957717761693);
#30837=CIRCLE('',#99438,61.8704694830905);
#30838=CIRCLE('',#99440,0.635007073208615);
#30839=CIRCLE('',#99441,0.635007073208627);
#30840=CIRCLE('',#99452,60.0045305169095);
#30841=CIRCLE('',#99453,60.4792282238308);
#30842=CIRCLE('',#99454,60.4792282238308);
#30843=CIRCLE('',#99455,60.4792282238308);
#30844=CIRCLE('',#99457,60.6419265158129);
#30845=CIRCLE('',#99459,60.8618969683742);
#30846=CIRCLE('',#99460,61.0131030316259);
#30847=CIRCLE('',#99462,61.2330734841871);
#30848=CIRCLE('',#99463,61.3957717761693);
#30849=CIRCLE('',#99464,61.3957717761693);
#30850=CIRCLE('',#99465,61.3957717761693);
#30851=CIRCLE('',#99467,61.8704694830905);
#30852=CIRCLE('',#99469,0.635007073208633);
#30853=CIRCLE('',#99470,0.635007073208601);
#30854=CIRCLE('',#99481,60.0045305169095);
#30855=CIRCLE('',#99482,60.4792282238308);
#30856=CIRCLE('',#99483,60.4792282238308);
#30857=CIRCLE('',#99484,60.4792282238308);
#30858=CIRCLE('',#99486,60.6419265158129);
#30859=CIRCLE('',#99488,60.8618969683742);
#30860=CIRCLE('',#99489,61.0131030316259);
#30861=CIRCLE('',#99491,61.2330734841871);
#30862=CIRCLE('',#99492,61.3957717761693);
#30863=CIRCLE('',#99493,61.3957717761693);
#30864=CIRCLE('',#99494,61.3957717761693);
#30865=CIRCLE('',#99496,61.8704694830905);
#30866=CIRCLE('',#99498,0.635007073208607);
#30867=CIRCLE('',#99499,0.635007073208594);
#30868=CIRCLE('',#99510,60.0045305169095);
#30869=CIRCLE('',#99511,60.4792282238308);
#30870=CIRCLE('',#99512,60.4792282238308);
#30871=CIRCLE('',#99513,60.4792282238308);
#30872=CIRCLE('',#99515,60.6419265158129);
#30873=CIRCLE('',#99517,60.8618969683742);
#30874=CIRCLE('',#99518,61.0131030316259);
#30875=CIRCLE('',#99520,61.2330734841871);
#30876=CIRCLE('',#99521,61.3957717761693);
#30877=CIRCLE('',#99522,61.3957717761693);
#30878=CIRCLE('',#99523,61.3957717761693);
#30879=CIRCLE('',#99525,61.8704694830905);
#30880=CIRCLE('',#99527,0.635007073208611);
#30881=CIRCLE('',#99528,0.635007073208602);
#30882=CIRCLE('',#99539,60.0045305169095);
#30883=CIRCLE('',#99540,60.4792282238308);
#30884=CIRCLE('',#99541,60.4792282238308);
#30885=CIRCLE('',#99542,60.4792282238308);
#30886=CIRCLE('',#99544,60.6419265158129);
#30887=CIRCLE('',#99546,60.8618969683742);
#30888=CIRCLE('',#99547,61.0131030316259);
#30889=CIRCLE('',#99549,61.2330734841871);
#30890=CIRCLE('',#99550,61.3957717761693);
#30891=CIRCLE('',#99551,61.3957717761693);
#30892=CIRCLE('',#99552,61.3957717761693);
#30893=CIRCLE('',#99554,61.8704694830905);
#30894=CIRCLE('',#99556,0.635007073208602);
#30895=CIRCLE('',#99557,0.635007073208613);
#30896=CIRCLE('',#99568,60.0045305169095);
#30897=CIRCLE('',#99569,60.4792282238308);
#30898=CIRCLE('',#99570,60.4792282238308);
#30899=CIRCLE('',#99571,60.4792282238308);
#30900=CIRCLE('',#99573,60.6419265158129);
#30901=CIRCLE('',#99575,60.8618969683742);
#30902=CIRCLE('',#99576,61.0131030316259);
#30903=CIRCLE('',#99578,61.2330734841871);
#30904=CIRCLE('',#99579,61.3957717761693);
#30905=CIRCLE('',#99580,61.3957717761693);
#30906=CIRCLE('',#99581,61.3957717761693);
#30907=CIRCLE('',#99583,61.8704694830905);
#30908=CIRCLE('',#99585,0.635007073208633);
#30909=CIRCLE('',#99586,0.635007073208603);
#30910=CIRCLE('',#99597,60.0045305169095);
#30911=CIRCLE('',#99598,60.4792282238308);
#30912=CIRCLE('',#99599,60.4792282238308);
#30913=CIRCLE('',#99600,60.4792282238308);
#30914=CIRCLE('',#99602,60.6419265158129);
#30915=CIRCLE('',#99604,60.8618969683742);
#30916=CIRCLE('',#99605,61.0131030316259);
#30917=CIRCLE('',#99607,61.2330734841871);
#30918=CIRCLE('',#99608,61.3957717761693);
#30919=CIRCLE('',#99609,61.3957717761693);
#30920=CIRCLE('',#99610,61.3957717761693);
#30921=CIRCLE('',#99612,61.8704694830905);
#30922=CIRCLE('',#99614,0.635007073208615);
#30923=CIRCLE('',#99615,0.635007073208628);
#30924=CIRCLE('',#99626,60.0045305169095);
#30925=CIRCLE('',#99627,60.4792282238308);
#30926=CIRCLE('',#99628,60.4792282238308);
#30927=CIRCLE('',#99629,60.4792282238308);
#30928=CIRCLE('',#99631,60.6419265158129);
#30929=CIRCLE('',#99633,60.8618969683742);
#30930=CIRCLE('',#99634,61.0131030316259);
#30931=CIRCLE('',#99636,61.2330734841871);
#30932=CIRCLE('',#99637,61.3957717761693);
#30933=CIRCLE('',#99638,61.3957717761693);
#30934=CIRCLE('',#99639,61.3957717761693);
#30935=CIRCLE('',#99641,61.8704694830905);
#30936=CIRCLE('',#99643,0.635007073208624);
#30937=CIRCLE('',#99644,0.635007073208631);
#30938=CIRCLE('',#99655,60.0045305169095);
#30939=CIRCLE('',#99656,60.4792282238308);
#30940=CIRCLE('',#99657,60.4792282238308);
#30941=CIRCLE('',#99658,60.4792282238308);
#30942=CIRCLE('',#99660,60.6419265158129);
#30943=CIRCLE('',#99662,60.8618969683742);
#30944=CIRCLE('',#99663,61.0131030316259);
#30945=CIRCLE('',#99665,61.2330734841871);
#30946=CIRCLE('',#99666,61.3957717761693);
#30947=CIRCLE('',#99667,61.3957717761693);
#30948=CIRCLE('',#99668,61.3957717761693);
#30949=CIRCLE('',#99670,61.8704694830905);
#30950=CIRCLE('',#99672,0.635007073208607);
#30951=CIRCLE('',#99673,0.635007073208634);
#30952=CIRCLE('',#99684,60.0045305169095);
#30953=CIRCLE('',#99685,60.4792282238308);
#30954=CIRCLE('',#99686,60.4792282238308);
#30955=CIRCLE('',#99687,60.4792282238308);
#30956=CIRCLE('',#99689,60.6419265158129);
#30957=CIRCLE('',#99691,60.8618969683742);
#30958=CIRCLE('',#99692,61.0131030316259);
#30959=CIRCLE('',#99694,61.2330734841871);
#30960=CIRCLE('',#99695,61.3957717761693);
#30961=CIRCLE('',#99696,61.3957717761693);
#30962=CIRCLE('',#99697,61.3957717761693);
#30963=CIRCLE('',#99699,61.8704694830905);
#30964=CIRCLE('',#99701,0.63500707320862);
#30965=CIRCLE('',#99702,0.635007073208639);
#30966=CIRCLE('',#99713,60.0045305169095);
#30967=CIRCLE('',#99714,60.4792282238308);
#30968=CIRCLE('',#99715,60.4792282238308);
#30969=CIRCLE('',#99716,60.4792282238308);
#30970=CIRCLE('',#99718,60.6419265158129);
#30971=CIRCLE('',#99720,60.8618969683742);
#30972=CIRCLE('',#99721,61.0131030316259);
#30973=CIRCLE('',#99723,61.2330734841871);
#30974=CIRCLE('',#99724,61.3957717761693);
#30975=CIRCLE('',#99725,61.3957717761693);
#30976=CIRCLE('',#99726,61.3957717761693);
#30977=CIRCLE('',#99728,61.8704694830905);
#30978=CIRCLE('',#99730,0.63500707320862);
#30979=CIRCLE('',#99731,0.635007073208627);
#30980=CIRCLE('',#99742,60.0045305169095);
#30981=CIRCLE('',#99743,60.4792282238308);
#30982=CIRCLE('',#99744,60.4792282238308);
#30983=CIRCLE('',#99745,60.4792282238308);
#30984=CIRCLE('',#99747,60.6419265158129);
#30985=CIRCLE('',#99749,60.8618969683742);
#30986=CIRCLE('',#99750,61.0131030316259);
#30987=CIRCLE('',#99752,61.2330734841871);
#30988=CIRCLE('',#99753,61.3957717761693);
#30989=CIRCLE('',#99754,61.3957717761693);
#30990=CIRCLE('',#99755,61.3957717761693);
#30991=CIRCLE('',#99757,61.8704694830905);
#30992=CIRCLE('',#99759,0.635007073208602);
#30993=CIRCLE('',#99760,0.635007073208611);
#30994=CIRCLE('',#99771,60.0045305169095);
#30995=CIRCLE('',#99772,60.4792282238308);
#30996=CIRCLE('',#99773,60.4792282238308);
#30997=CIRCLE('',#99774,60.4792282238308);
#30998=CIRCLE('',#99776,60.6419265158129);
#30999=CIRCLE('',#99778,60.8618969683742);
#31000=CIRCLE('',#99779,61.0131030316259);
#31001=CIRCLE('',#99781,61.2330734841871);
#31002=CIRCLE('',#99782,61.3957717761693);
#31003=CIRCLE('',#99783,61.3957717761693);
#31004=CIRCLE('',#99784,61.3957717761693);
#31005=CIRCLE('',#99786,61.8704694830905);
#31006=CIRCLE('',#99788,0.635007073208624);
#31007=CIRCLE('',#99789,0.635007073208605);
#31008=CIRCLE('',#99800,60.0045305169095);
#31009=CIRCLE('',#99801,60.4792282238308);
#31010=CIRCLE('',#99802,60.4792282238308);
#31011=CIRCLE('',#99803,60.4792282238308);
#31012=CIRCLE('',#99805,60.6419265158129);
#31013=CIRCLE('',#99807,60.8618969683742);
#31014=CIRCLE('',#99808,61.0131030316259);
#31015=CIRCLE('',#99810,61.2330734841871);
#31016=CIRCLE('',#99811,61.3957717761693);
#31017=CIRCLE('',#99812,61.3957717761693);
#31018=CIRCLE('',#99813,61.3957717761693);
#31019=CIRCLE('',#99815,61.8704694830905);
#31020=CIRCLE('',#99817,0.63500707320866);
#31021=CIRCLE('',#99818,0.635007073208591);
#31022=CIRCLE('',#99829,60.0045305169095);
#31023=CIRCLE('',#99830,60.4792282238308);
#31024=CIRCLE('',#99831,60.4792282238308);
#31025=CIRCLE('',#99832,60.4792282238308);
#31026=CIRCLE('',#99834,60.6419265158129);
#31027=CIRCLE('',#99836,60.8618969683742);
#31028=CIRCLE('',#99837,61.0131030316259);
#31029=CIRCLE('',#99839,61.2330734841871);
#31030=CIRCLE('',#99840,61.3957717761693);
#31031=CIRCLE('',#99841,61.3957717761693);
#31032=CIRCLE('',#99842,61.3957717761693);
#31033=CIRCLE('',#99844,61.8704694830905);
#31034=CIRCLE('',#99846,0.635007073208575);
#31035=CIRCLE('',#99847,0.635007073208613);
#31036=CIRCLE('',#99858,60.0045305169095);
#31037=CIRCLE('',#99859,60.4792282238308);
#31038=CIRCLE('',#99860,60.4792282238308);
#31039=CIRCLE('',#99861,60.4792282238308);
#31040=CIRCLE('',#99863,60.6419265158129);
#31041=CIRCLE('',#99865,60.8618969683742);
#31042=CIRCLE('',#99866,61.0131030316259);
#31043=CIRCLE('',#99868,61.2330734841871);
#31044=CIRCLE('',#99869,61.3957717761693);
#31045=CIRCLE('',#99870,61.3957717761693);
#31046=CIRCLE('',#99871,61.3957717761693);
#31047=CIRCLE('',#99873,61.8704694830905);
#31048=CIRCLE('',#99875,0.635007073208615);
#31049=CIRCLE('',#99876,0.635007073208595);
#31050=CIRCLE('',#99887,60.0045305169095);
#31051=CIRCLE('',#99888,60.4792282238308);
#31052=CIRCLE('',#99889,60.4792282238308);
#31053=CIRCLE('',#99890,60.4792282238308);
#31054=CIRCLE('',#99892,60.6419265158129);
#31055=CIRCLE('',#99894,60.8618969683742);
#31056=CIRCLE('',#99895,61.0131030316259);
#31057=CIRCLE('',#99897,61.2330734841871);
#31058=CIRCLE('',#99898,61.3957717761693);
#31059=CIRCLE('',#99899,61.3957717761693);
#31060=CIRCLE('',#99900,61.3957717761693);
#31061=CIRCLE('',#99902,61.8704694830905);
#31062=CIRCLE('',#99904,0.635007073208607);
#31063=CIRCLE('',#99905,0.635007073208594);
#31064=CIRCLE('',#99916,60.0045305169095);
#31065=CIRCLE('',#99917,60.4792282238308);
#31066=CIRCLE('',#99918,60.4792282238308);
#31067=CIRCLE('',#99919,60.4792282238308);
#31068=CIRCLE('',#99921,60.6419265158129);
#31069=CIRCLE('',#99923,60.8618969683742);
#31070=CIRCLE('',#99924,61.0131030316259);
#31071=CIRCLE('',#99926,61.2330734841871);
#31072=CIRCLE('',#99927,61.3957717761693);
#31073=CIRCLE('',#99928,61.3957717761693);
#31074=CIRCLE('',#99929,61.3957717761693);
#31075=CIRCLE('',#99931,61.8704694830905);
#31076=CIRCLE('',#99933,0.635007073208598);
#31077=CIRCLE('',#99934,0.635007073208625);
#31078=CIRCLE('',#99945,60.0045305169095);
#31079=CIRCLE('',#99946,60.4792282238308);
#31080=CIRCLE('',#99947,60.4792282238308);
#31081=CIRCLE('',#99948,60.4792282238308);
#31082=CIRCLE('',#99950,60.6419265158129);
#31083=CIRCLE('',#99952,60.8618969683742);
#31084=CIRCLE('',#99953,61.0131030316259);
#31085=CIRCLE('',#99955,61.2330734841871);
#31086=CIRCLE('',#99956,61.3957717761693);
#31087=CIRCLE('',#99957,61.3957717761693);
#31088=CIRCLE('',#99958,61.3957717761693);
#31089=CIRCLE('',#99960,61.8704694830905);
#31090=CIRCLE('',#99962,0.635007073208633);
#31091=CIRCLE('',#99963,0.635007073208599);
#31092=CIRCLE('',#99974,60.0045305169095);
#31093=CIRCLE('',#99975,60.4792282238308);
#31094=CIRCLE('',#99976,60.4792282238308);
#31095=CIRCLE('',#99977,60.4792282238308);
#31096=CIRCLE('',#99979,60.6419265158129);
#31097=CIRCLE('',#99981,60.8618969683742);
#31098=CIRCLE('',#99982,61.0131030316259);
#31099=CIRCLE('',#99984,61.2330734841871);
#31100=CIRCLE('',#99985,61.3957717761693);
#31101=CIRCLE('',#99986,61.3957717761693);
#31102=CIRCLE('',#99987,61.3957717761693);
#31103=CIRCLE('',#99989,61.8704694830905);
#31104=CIRCLE('',#99991,0.635007073208593);
#31105=CIRCLE('',#99992,0.635007073208574);
#31106=CIRCLE('',#100003,60.0045305169095);
#31107=CIRCLE('',#100004,60.4792282238308);
#31108=CIRCLE('',#100005,60.4792282238308);
#31109=CIRCLE('',#100006,60.4792282238308);
#31110=CIRCLE('',#100008,60.6419265158129);
#31111=CIRCLE('',#100010,60.8618969683742);
#31112=CIRCLE('',#100011,61.0131030316259);
#31113=CIRCLE('',#100013,61.2330734841871);
#31114=CIRCLE('',#100014,61.3957717761693);
#31115=CIRCLE('',#100015,61.3957717761693);
#31116=CIRCLE('',#100016,61.3957717761693);
#31117=CIRCLE('',#100018,61.8704694830905);
#31118=CIRCLE('',#100020,0.63500707320862);
#31119=CIRCLE('',#100021,0.63500707320863);
#31120=CIRCLE('',#100032,60.0045305169095);
#31121=CIRCLE('',#100033,60.4792282238308);
#31122=CIRCLE('',#100034,60.4792282238308);
#31123=CIRCLE('',#100035,60.4792282238308);
#31124=CIRCLE('',#100037,60.6419265158129);
#31125=CIRCLE('',#100039,60.8618969683742);
#31126=CIRCLE('',#100040,61.0131030316259);
#31127=CIRCLE('',#100042,61.2330734841871);
#31128=CIRCLE('',#100043,61.3957717761693);
#31129=CIRCLE('',#100044,61.3957717761693);
#31130=CIRCLE('',#100045,61.3957717761693);
#31131=CIRCLE('',#100047,61.8704694830905);
#31132=CIRCLE('',#100049,0.635007073208607);
#31133=CIRCLE('',#100050,0.635007073208609);
#31134=CIRCLE('',#100061,60.0045305169095);
#31135=CIRCLE('',#100062,60.4792282238308);
#31136=CIRCLE('',#100063,60.4792282238308);
#31137=CIRCLE('',#100064,60.4792282238308);
#31138=CIRCLE('',#100066,60.6419265158129);
#31139=CIRCLE('',#100068,60.8618969683742);
#31140=CIRCLE('',#100069,61.0131030316259);
#31141=CIRCLE('',#100071,61.2330734841871);
#31142=CIRCLE('',#100072,61.3957717761693);
#31143=CIRCLE('',#100073,61.3957717761693);
#31144=CIRCLE('',#100074,61.3957717761693);
#31145=CIRCLE('',#100076,61.8704694830905);
#31146=CIRCLE('',#100078,0.635007073208598);
#31147=CIRCLE('',#100079,0.635007073208644);
#31148=CIRCLE('',#100090,60.0045305169095);
#31149=CIRCLE('',#100091,60.4792282238308);
#31150=CIRCLE('',#100092,60.4792282238308);
#31151=CIRCLE('',#100093,60.4792282238308);
#31152=CIRCLE('',#100095,60.6419265158129);
#31153=CIRCLE('',#100097,60.8618969683742);
#31154=CIRCLE('',#100098,61.0131030316259);
#31155=CIRCLE('',#100100,61.2330734841871);
#31156=CIRCLE('',#100101,61.3957717761693);
#31157=CIRCLE('',#100102,61.3957717761693);
#31158=CIRCLE('',#100103,61.3957717761693);
#31159=CIRCLE('',#100105,61.8704694830905);
#31160=CIRCLE('',#100107,0.635007073208571);
#31161=CIRCLE('',#100108,0.635007073208592);
#31162=CIRCLE('',#100119,60.0045305169095);
#31163=CIRCLE('',#100120,60.4792282238308);
#31164=CIRCLE('',#100121,60.4792282238308);
#31165=CIRCLE('',#100122,60.4792282238308);
#31166=CIRCLE('',#100124,60.6419265158129);
#31167=CIRCLE('',#100126,60.8618969683742);
#31168=CIRCLE('',#100127,61.0131030316259);
#31169=CIRCLE('',#100129,61.2330734841871);
#31170=CIRCLE('',#100130,61.3957717761693);
#31171=CIRCLE('',#100131,61.3957717761693);
#31172=CIRCLE('',#100132,61.3957717761693);
#31173=CIRCLE('',#100134,61.8704694830905);
#31174=CIRCLE('',#100136,0.635007073208655);
#31175=CIRCLE('',#100137,0.635007073208618);
#31176=CIRCLE('',#100148,60.0045305169095);
#31177=CIRCLE('',#100149,60.4792282238308);
#31178=CIRCLE('',#100150,60.4792282238308);
#31179=CIRCLE('',#100151,60.4792282238308);
#31180=CIRCLE('',#100153,60.6419265158129);
#31181=CIRCLE('',#100155,60.8618969683742);
#31182=CIRCLE('',#100156,61.0131030316259);
#31183=CIRCLE('',#100158,61.2330734841871);
#31184=CIRCLE('',#100159,61.3957717761693);
#31185=CIRCLE('',#100160,61.3957717761693);
#31186=CIRCLE('',#100161,61.3957717761693);
#31187=CIRCLE('',#100163,61.8704694830905);
#31188=CIRCLE('',#100165,0.63500707320866);
#31189=CIRCLE('',#100166,0.635007073208662);
#31190=CIRCLE('',#100177,60.0045305169095);
#31191=CIRCLE('',#100178,60.4792282238308);
#31192=CIRCLE('',#100179,60.4792282238308);
#31193=CIRCLE('',#100180,60.4792282238308);
#31194=CIRCLE('',#100182,60.6419265158129);
#31195=CIRCLE('',#100184,60.8618969683742);
#31196=CIRCLE('',#100185,61.0131030316259);
#31197=CIRCLE('',#100187,61.2330734841871);
#31198=CIRCLE('',#100188,61.3957717761693);
#31199=CIRCLE('',#100189,61.3957717761693);
#31200=CIRCLE('',#100190,61.3957717761693);
#31201=CIRCLE('',#100192,61.8704694830905);
#31202=CIRCLE('',#100194,0.635007073208651);
#31203=CIRCLE('',#100195,0.635007073208644);
#31204=CIRCLE('',#100206,60.0045305169095);
#31205=CIRCLE('',#100207,60.4792282238308);
#31206=CIRCLE('',#100208,60.4792282238308);
#31207=CIRCLE('',#100209,60.4792282238308);
#31208=CIRCLE('',#100211,60.6419265158129);
#31209=CIRCLE('',#100213,60.8618969683742);
#31210=CIRCLE('',#100214,61.0131030316259);
#31211=CIRCLE('',#100216,61.2330734841871);
#31212=CIRCLE('',#100217,61.3957717761693);
#31213=CIRCLE('',#100218,61.3957717761693);
#31214=CIRCLE('',#100219,61.3957717761693);
#31215=CIRCLE('',#100221,61.8704694830905);
#31216=CIRCLE('',#100223,0.635007073208593);
#31217=CIRCLE('',#100224,0.635007073208605);
#31218=CIRCLE('',#100235,60.0045305169095);
#31219=CIRCLE('',#100236,60.4792282238308);
#31220=CIRCLE('',#100237,60.4792282238308);
#31221=CIRCLE('',#100238,60.4792282238308);
#31222=CIRCLE('',#100240,60.6419265158129);
#31223=CIRCLE('',#100242,60.8618969683742);
#31224=CIRCLE('',#100243,61.0131030316259);
#31225=CIRCLE('',#100245,61.2330734841871);
#31226=CIRCLE('',#100246,61.3957717761693);
#31227=CIRCLE('',#100247,61.3957717761693);
#31228=CIRCLE('',#100248,61.3957717761693);
#31229=CIRCLE('',#100250,61.8704694830905);
#31230=CIRCLE('',#100252,0.635007073208602);
#31231=CIRCLE('',#100253,0.63500707320862);
#31232=CIRCLE('',#100264,60.0045305169095);
#31233=CIRCLE('',#100265,60.4792282238308);
#31234=CIRCLE('',#100266,60.4792282238308);
#31235=CIRCLE('',#100267,60.4792282238308);
#31236=CIRCLE('',#100269,60.6419265158129);
#31237=CIRCLE('',#100271,60.8618969683742);
#31238=CIRCLE('',#100272,61.0131030316259);
#31239=CIRCLE('',#100274,61.2330734841871);
#31240=CIRCLE('',#100275,61.3957717761693);
#31241=CIRCLE('',#100276,61.3957717761693);
#31242=CIRCLE('',#100277,61.3957717761693);
#31243=CIRCLE('',#100279,61.8704694830905);
#31244=CIRCLE('',#100281,0.635007073208646);
#31245=CIRCLE('',#100282,0.635007073208569);
#31246=CIRCLE('',#100293,60.0045305169095);
#31247=CIRCLE('',#100294,60.4792282238308);
#31248=CIRCLE('',#100295,60.4792282238308);
#31249=CIRCLE('',#100296,60.4792282238308);
#31250=CIRCLE('',#100298,60.6419265158129);
#31251=CIRCLE('',#100300,60.8618969683742);
#31252=CIRCLE('',#100301,61.0131030316259);
#31253=CIRCLE('',#100303,61.2330734841871);
#31254=CIRCLE('',#100304,61.3957717761693);
#31255=CIRCLE('',#100305,61.3957717761693);
#31256=CIRCLE('',#100306,61.3957717761693);
#31257=CIRCLE('',#100308,61.8704694830905);
#31258=CIRCLE('',#100310,0.635007073208638);
#31259=CIRCLE('',#100311,0.63500707320862);
#31260=CIRCLE('',#100322,60.0045305169095);
#31261=CIRCLE('',#100323,60.4792282238308);
#31262=CIRCLE('',#100324,60.4792282238308);
#31263=CIRCLE('',#100325,60.4792282238308);
#31264=CIRCLE('',#100327,60.6419265158129);
#31265=CIRCLE('',#100329,60.8618969683742);
#31266=CIRCLE('',#100330,61.0131030316259);
#31267=CIRCLE('',#100332,61.2330734841871);
#31268=CIRCLE('',#100333,61.3957717761693);
#31269=CIRCLE('',#100334,61.3957717761693);
#31270=CIRCLE('',#100335,61.3957717761693);
#31271=CIRCLE('',#100337,61.8704694830905);
#31272=CIRCLE('',#100339,0.635007073208642);
#31273=CIRCLE('',#100340,0.635007073208594);
#31274=CIRCLE('',#100351,60.0045305169095);
#31275=CIRCLE('',#100352,60.4792282238308);
#31276=CIRCLE('',#100353,60.4792282238308);
#31277=CIRCLE('',#100354,60.4792282238308);
#31278=CIRCLE('',#100356,60.6419265158129);
#31279=CIRCLE('',#100358,60.8618969683742);
#31280=CIRCLE('',#100359,61.0131030316259);
#31281=CIRCLE('',#100361,61.2330734841871);
#31282=CIRCLE('',#100362,61.3957717761693);
#31283=CIRCLE('',#100363,61.3957717761693);
#31284=CIRCLE('',#100364,61.3957717761693);
#31285=CIRCLE('',#100366,61.8704694830905);
#31286=CIRCLE('',#100368,0.63500707320862);
#31287=CIRCLE('',#100369,0.635007073208609);
#31288=CIRCLE('',#100380,60.0045305169095);
#31289=CIRCLE('',#100381,60.4792282238308);
#31290=CIRCLE('',#100382,60.4792282238308);
#31291=CIRCLE('',#100383,60.4792282238308);
#31292=CIRCLE('',#100385,60.6419265158129);
#31293=CIRCLE('',#100387,60.8618969683742);
#31294=CIRCLE('',#100388,61.0131030316259);
#31295=CIRCLE('',#100390,61.2330734841871);
#31296=CIRCLE('',#100391,61.3957717761693);
#31297=CIRCLE('',#100392,61.3957717761693);
#31298=CIRCLE('',#100393,61.3957717761693);
#31299=CIRCLE('',#100395,61.8704694830905);
#31300=CIRCLE('',#100397,0.63500707320862);
#31301=CIRCLE('',#100398,0.635007073208601);
#31302=CIRCLE('',#100409,60.0045305169095);
#31303=CIRCLE('',#100410,60.4792282238308);
#31304=CIRCLE('',#100411,60.4792282238308);
#31305=CIRCLE('',#100412,60.4792282238308);
#31306=CIRCLE('',#100414,60.6419265158129);
#31307=CIRCLE('',#100416,60.8618969683742);
#31308=CIRCLE('',#100417,61.0131030316259);
#31309=CIRCLE('',#100419,61.2330734841871);
#31310=CIRCLE('',#100420,61.3957717761693);
#31311=CIRCLE('',#100421,61.3957717761693);
#31312=CIRCLE('',#100422,61.3957717761693);
#31313=CIRCLE('',#100424,61.8704694830905);
#31314=CIRCLE('',#100426,0.635007073208598);
#31315=CIRCLE('',#100427,0.63500707320861);
#31316=CIRCLE('',#100438,60.0045305169095);
#31317=CIRCLE('',#100439,60.4792282238308);
#31318=CIRCLE('',#100440,60.4792282238308);
#31319=CIRCLE('',#100441,60.4792282238308);
#31320=CIRCLE('',#100443,60.6419265158129);
#31321=CIRCLE('',#100445,60.8618969683742);
#31322=CIRCLE('',#100446,61.0131030316259);
#31323=CIRCLE('',#100448,61.2330734841871);
#31324=CIRCLE('',#100449,61.3957717761693);
#31325=CIRCLE('',#100450,61.3957717761693);
#31326=CIRCLE('',#100451,61.3957717761693);
#31327=CIRCLE('',#100453,61.8704694830905);
#31328=CIRCLE('',#100455,0.63500707320862);
#31329=CIRCLE('',#100456,0.635007073208583);
#31330=CIRCLE('',#100467,60.0045305169095);
#31331=CIRCLE('',#100468,60.4792282238308);
#31332=CIRCLE('',#100469,60.4792282238308);
#31333=CIRCLE('',#100470,60.4792282238308);
#31334=CIRCLE('',#100472,60.6419265158129);
#31335=CIRCLE('',#100474,60.8618969683742);
#31336=CIRCLE('',#100475,61.0131030316259);
#31337=CIRCLE('',#100477,61.2330734841871);
#31338=CIRCLE('',#100478,61.3957717761693);
#31339=CIRCLE('',#100479,61.3957717761693);
#31340=CIRCLE('',#100480,61.3957717761693);
#31341=CIRCLE('',#100482,61.8704694830905);
#31342=CIRCLE('',#100484,0.635007073208575);
#31343=CIRCLE('',#100485,0.635007073208584);
#31344=CIRCLE('',#100496,60.0045305169095);
#31345=CIRCLE('',#100497,60.4792282238308);
#31346=CIRCLE('',#100498,60.4792282238308);
#31347=CIRCLE('',#100499,60.4792282238308);
#31348=CIRCLE('',#100501,60.6419265158129);
#31349=CIRCLE('',#100503,60.8618969683742);
#31350=CIRCLE('',#100504,61.0131030316259);
#31351=CIRCLE('',#100506,61.2330734841871);
#31352=CIRCLE('',#100507,61.3957717761693);
#31353=CIRCLE('',#100508,61.3957717761693);
#31354=CIRCLE('',#100509,61.3957717761693);
#31355=CIRCLE('',#100511,61.8704694830905);
#31356=CIRCLE('',#100513,0.635007073208611);
#31357=CIRCLE('',#100514,0.635007073208621);
#31358=CIRCLE('',#100525,60.0045305169095);
#31359=CIRCLE('',#100526,60.4792282238308);
#31360=CIRCLE('',#100527,60.4792282238308);
#31361=CIRCLE('',#100528,60.4792282238308);
#31362=CIRCLE('',#100530,60.6419265158129);
#31363=CIRCLE('',#100532,60.8618969683742);
#31364=CIRCLE('',#100533,61.0131030316259);
#31365=CIRCLE('',#100535,61.2330734841871);
#31366=CIRCLE('',#100536,61.3957717761693);
#31367=CIRCLE('',#100537,61.3957717761693);
#31368=CIRCLE('',#100538,61.3957717761693);
#31369=CIRCLE('',#100540,61.8704694830905);
#31370=CIRCLE('',#100542,0.635007073208624);
#31371=CIRCLE('',#100543,0.63500707320863);
#31372=CIRCLE('',#100554,60.0045305169095);
#31373=CIRCLE('',#100555,60.4792282238308);
#31374=CIRCLE('',#100556,60.4792282238308);
#31375=CIRCLE('',#100557,60.4792282238308);
#31376=CIRCLE('',#100559,60.6419265158129);
#31377=CIRCLE('',#100561,60.8618969683742);
#31378=CIRCLE('',#100562,61.0131030316259);
#31379=CIRCLE('',#100564,61.2330734841871);
#31380=CIRCLE('',#100565,61.3957717761693);
#31381=CIRCLE('',#100566,61.3957717761693);
#31382=CIRCLE('',#100567,61.3957717761693);
#31383=CIRCLE('',#100569,61.8704694830905);
#31384=CIRCLE('',#100571,0.635007073208638);
#31385=CIRCLE('',#100572,0.635007073208613);
#31386=CIRCLE('',#100583,60.0045305169095);
#31387=CIRCLE('',#100584,60.4792282238308);
#31388=CIRCLE('',#100585,60.4792282238308);
#31389=CIRCLE('',#100586,60.4792282238308);
#31390=CIRCLE('',#100588,60.6419265158129);
#31391=CIRCLE('',#100590,60.8618969683742);
#31392=CIRCLE('',#100591,61.0131030316259);
#31393=CIRCLE('',#100593,61.2330734841871);
#31394=CIRCLE('',#100594,61.3957717761693);
#31395=CIRCLE('',#100595,61.3957717761693);
#31396=CIRCLE('',#100596,61.3957717761693);
#31397=CIRCLE('',#100598,61.8704694830905);
#31398=CIRCLE('',#100600,0.635007073208598);
#31399=CIRCLE('',#100601,0.635007073208607);
#31400=CIRCLE('',#100612,60.0045305169095);
#31401=CIRCLE('',#100613,60.4792282238308);
#31402=CIRCLE('',#100614,60.4792282238308);
#31403=CIRCLE('',#100615,60.4792282238308);
#31404=CIRCLE('',#100617,60.6419265158129);
#31405=CIRCLE('',#100619,60.8618969683742);
#31406=CIRCLE('',#100620,61.0131030316259);
#31407=CIRCLE('',#100622,61.2330734841871);
#31408=CIRCLE('',#100623,61.3957717761693);
#31409=CIRCLE('',#100624,61.3957717761693);
#31410=CIRCLE('',#100625,61.3957717761693);
#31411=CIRCLE('',#100627,61.8704694830905);
#31412=CIRCLE('',#100629,0.63500707320862);
#31413=CIRCLE('',#100630,0.635007073208593);
#31414=CIRCLE('',#100641,60.0045305169095);
#31415=CIRCLE('',#100642,60.4792282238308);
#31416=CIRCLE('',#100643,60.4792282238308);
#31417=CIRCLE('',#100644,60.4792282238308);
#31418=CIRCLE('',#100646,60.6419265158129);
#31419=CIRCLE('',#100648,60.8618969683742);
#31420=CIRCLE('',#100649,61.0131030316259);
#31421=CIRCLE('',#100651,61.2330734841871);
#31422=CIRCLE('',#100652,61.3957717761693);
#31423=CIRCLE('',#100653,61.3957717761693);
#31424=CIRCLE('',#100654,61.3957717761693);
#31425=CIRCLE('',#100656,61.8704694830905);
#31426=CIRCLE('',#100658,0.635007073208611);
#31427=CIRCLE('',#100659,0.635007073208634);
#31428=CIRCLE('',#100670,60.0045305169095);
#31429=CIRCLE('',#100671,60.4792282238308);
#31430=CIRCLE('',#100672,60.4792282238308);
#31431=CIRCLE('',#100673,60.4792282238308);
#31432=CIRCLE('',#100675,60.6419265158129);
#31433=CIRCLE('',#100677,60.8618969683742);
#31434=CIRCLE('',#100678,61.0131030316259);
#31435=CIRCLE('',#100680,61.2330734841871);
#31436=CIRCLE('',#100681,61.3957717761693);
#31437=CIRCLE('',#100682,61.3957717761693);
#31438=CIRCLE('',#100683,61.3957717761693);
#31439=CIRCLE('',#100685,61.8704694830905);
#31440=CIRCLE('',#100687,0.635007073208598);
#31441=CIRCLE('',#100688,0.635007073208591);
#31442=CIRCLE('',#100699,60.0045305169095);
#31443=CIRCLE('',#100700,60.4792282238308);
#31444=CIRCLE('',#100701,60.4792282238308);
#31445=CIRCLE('',#100702,60.4792282238308);
#31446=CIRCLE('',#100704,60.6419265158129);
#31447=CIRCLE('',#100706,60.8618969683742);
#31448=CIRCLE('',#100707,61.0131030316259);
#31449=CIRCLE('',#100709,61.2330734841871);
#31450=CIRCLE('',#100710,61.3957717761693);
#31451=CIRCLE('',#100711,61.3957717761693);
#31452=CIRCLE('',#100712,61.3957717761693);
#31453=CIRCLE('',#100714,61.8704694830905);
#31454=CIRCLE('',#100716,0.635007073208629);
#31455=CIRCLE('',#100717,0.635007073208631);
#31456=CIRCLE('',#100728,60.0045305169095);
#31457=CIRCLE('',#100729,60.4792282238308);
#31458=CIRCLE('',#100730,60.4792282238308);
#31459=CIRCLE('',#100731,60.4792282238308);
#31460=CIRCLE('',#100733,60.6419265158129);
#31461=CIRCLE('',#100735,60.8618969683742);
#31462=CIRCLE('',#100736,61.0131030316259);
#31463=CIRCLE('',#100738,61.2330734841871);
#31464=CIRCLE('',#100739,61.3957717761693);
#31465=CIRCLE('',#100740,61.3957717761693);
#31466=CIRCLE('',#100741,61.3957717761693);
#31467=CIRCLE('',#100743,61.8704694830905);
#31468=CIRCLE('',#100745,0.635007073208598);
#31469=CIRCLE('',#100746,0.635007073208607);
#31470=CIRCLE('',#100757,60.0045305169095);
#31471=CIRCLE('',#100758,60.4792282238308);
#31472=CIRCLE('',#100759,60.4792282238308);
#31473=CIRCLE('',#100760,60.4792282238308);
#31474=CIRCLE('',#100762,60.6419265158129);
#31475=CIRCLE('',#100764,60.8618969683742);
#31476=CIRCLE('',#100765,61.0131030316259);
#31477=CIRCLE('',#100767,61.2330734841871);
#31478=CIRCLE('',#100768,61.3957717761693);
#31479=CIRCLE('',#100769,61.3957717761693);
#31480=CIRCLE('',#100770,61.3957717761693);
#31481=CIRCLE('',#100772,61.8704694830905);
#31482=CIRCLE('',#100774,0.635007073208593);
#31483=CIRCLE('',#100775,0.63500707320864);
#31484=CIRCLE('',#100786,60.0045305169095);
#31485=CIRCLE('',#100787,60.4792282238308);
#31486=CIRCLE('',#100788,60.4792282238308);
#31487=CIRCLE('',#100789,60.4792282238308);
#31488=CIRCLE('',#100791,60.6419265158129);
#31489=CIRCLE('',#100793,60.8618969683742);
#31490=CIRCLE('',#100794,61.0131030316259);
#31491=CIRCLE('',#100796,61.2330734841871);
#31492=CIRCLE('',#100797,61.3957717761693);
#31493=CIRCLE('',#100798,61.3957717761693);
#31494=CIRCLE('',#100799,61.3957717761693);
#31495=CIRCLE('',#100801,61.8704694830905);
#31496=CIRCLE('',#100803,0.635007073208687);
#31497=CIRCLE('',#100804,0.635007073208632);
#31498=CIRCLE('',#100815,60.0045305169095);
#31499=CIRCLE('',#100816,60.4792282238308);
#31500=CIRCLE('',#100817,60.4792282238308);
#31501=CIRCLE('',#100818,60.4792282238308);
#31502=CIRCLE('',#100820,60.6419265158129);
#31503=CIRCLE('',#100822,60.8618969683742);
#31504=CIRCLE('',#100823,61.0131030316259);
#31505=CIRCLE('',#100825,61.2330734841871);
#31506=CIRCLE('',#100826,61.3957717761693);
#31507=CIRCLE('',#100827,61.3957717761693);
#31508=CIRCLE('',#100828,61.3957717761693);
#31509=CIRCLE('',#100830,61.8704694830905);
#31510=CIRCLE('',#100832,0.63500707320862);
#31511=CIRCLE('',#100833,0.635007073208634);
#31512=CIRCLE('',#100844,60.0045305169095);
#31513=CIRCLE('',#100845,60.4792282238308);
#31514=CIRCLE('',#100846,60.4792282238308);
#31515=CIRCLE('',#100847,60.4792282238308);
#31516=CIRCLE('',#100849,60.6419265158129);
#31517=CIRCLE('',#100851,60.8618969683742);
#31518=CIRCLE('',#100852,61.0131030316259);
#31519=CIRCLE('',#100854,61.2330734841871);
#31520=CIRCLE('',#100855,61.3957717761693);
#31521=CIRCLE('',#100856,61.3957717761693);
#31522=CIRCLE('',#100857,61.3957717761693);
#31523=CIRCLE('',#100859,61.8704694830905);
#31524=CIRCLE('',#100861,0.63500707320858);
#31525=CIRCLE('',#100862,0.635007073208591);
#31526=CIRCLE('',#100873,60.0045305169095);
#31527=CIRCLE('',#100874,60.4792282238308);
#31528=CIRCLE('',#100875,60.4792282238308);
#31529=CIRCLE('',#100876,60.4792282238308);
#31530=CIRCLE('',#100878,60.6419265158129);
#31531=CIRCLE('',#100880,60.8618969683742);
#31532=CIRCLE('',#100881,61.0131030316259);
#31533=CIRCLE('',#100883,61.2330734841871);
#31534=CIRCLE('',#100884,61.3957717761693);
#31535=CIRCLE('',#100885,61.3957717761693);
#31536=CIRCLE('',#100886,61.3957717761693);
#31537=CIRCLE('',#100888,61.8704694830905);
#31538=CIRCLE('',#100890,0.635007073208646);
#31539=CIRCLE('',#100891,0.635007073208626);
#31540=CIRCLE('',#100902,60.0045305169095);
#31541=CIRCLE('',#100903,60.4792282238308);
#31542=CIRCLE('',#100904,60.4792282238308);
#31543=CIRCLE('',#100905,60.4792282238308);
#31544=CIRCLE('',#100907,60.6419265158129);
#31545=CIRCLE('',#100909,60.8618969683742);
#31546=CIRCLE('',#100910,61.0131030316259);
#31547=CIRCLE('',#100912,61.2330734841871);
#31548=CIRCLE('',#100913,61.3957717761693);
#31549=CIRCLE('',#100914,61.3957717761693);
#31550=CIRCLE('',#100915,61.3957717761693);
#31551=CIRCLE('',#100917,61.8704694830905);
#31552=CIRCLE('',#100919,0.635007073208624);
#31553=CIRCLE('',#100920,0.635007073208612);
#31554=CIRCLE('',#100931,60.0045305169095);
#31555=CIRCLE('',#100932,60.4792282238308);
#31556=CIRCLE('',#100933,60.4792282238308);
#31557=CIRCLE('',#100934,60.4792282238308);
#31558=CIRCLE('',#100936,60.6419265158129);
#31559=CIRCLE('',#100938,60.8618969683742);
#31560=CIRCLE('',#100939,61.0131030316259);
#31561=CIRCLE('',#100941,61.2330734841871);
#31562=CIRCLE('',#100942,61.3957717761693);
#31563=CIRCLE('',#100943,61.3957717761693);
#31564=CIRCLE('',#100944,61.3957717761693);
#31565=CIRCLE('',#100946,61.8704694830905);
#31566=CIRCLE('',#100948,0.635007073208615);
#31567=CIRCLE('',#100949,0.63500707320861);
#31568=CIRCLE('',#100960,60.0045305169095);
#31569=CIRCLE('',#100961,60.4792282238308);
#31570=CIRCLE('',#100962,60.4792282238308);
#31571=CIRCLE('',#100963,60.4792282238308);
#31572=CIRCLE('',#100965,60.6419265158129);
#31573=CIRCLE('',#100967,60.8618969683742);
#31574=CIRCLE('',#100968,61.0131030316259);
#31575=CIRCLE('',#100970,61.2330734841871);
#31576=CIRCLE('',#100971,61.3957717761693);
#31577=CIRCLE('',#100972,61.3957717761693);
#31578=CIRCLE('',#100973,61.3957717761693);
#31579=CIRCLE('',#100975,61.8704694830905);
#31580=CIRCLE('',#100977,0.635007073208593);
#31581=CIRCLE('',#100978,0.635007073208623);
#31582=CIRCLE('',#100989,60.0045305169095);
#31583=CIRCLE('',#100990,60.4792282238308);
#31584=CIRCLE('',#100991,60.4792282238308);
#31585=CIRCLE('',#100992,60.4792282238308);
#31586=CIRCLE('',#100994,60.6419265158129);
#31587=CIRCLE('',#100996,60.8618969683742);
#31588=CIRCLE('',#100997,61.0131030316259);
#31589=CIRCLE('',#100999,61.2330734841871);
#31590=CIRCLE('',#101000,61.3957717761693);
#31591=CIRCLE('',#101001,61.3957717761693);
#31592=CIRCLE('',#101002,61.3957717761693);
#31593=CIRCLE('',#101004,61.8704694830905);
#31594=CIRCLE('',#101006,0.635007073208642);
#31595=CIRCLE('',#101007,0.635007073208646);
#31596=CIRCLE('',#101018,60.0045305169095);
#31597=CIRCLE('',#101019,60.4792282238308);
#31598=CIRCLE('',#101020,60.4792282238308);
#31599=CIRCLE('',#101021,60.4792282238308);
#31600=CIRCLE('',#101023,60.6419265158129);
#31601=CIRCLE('',#101025,60.8618969683742);
#31602=CIRCLE('',#101026,61.0131030316259);
#31603=CIRCLE('',#101028,61.2330734841871);
#31604=CIRCLE('',#101029,61.3957717761693);
#31605=CIRCLE('',#101030,61.3957717761693);
#31606=CIRCLE('',#101031,61.3957717761693);
#31607=CIRCLE('',#101033,61.8704694830905);
#31608=CIRCLE('',#101035,0.635007073208629);
#31609=CIRCLE('',#101036,0.635007073208629);
#31610=CIRCLE('',#101047,60.0045305169095);
#31611=CIRCLE('',#101048,60.4792282238308);
#31612=CIRCLE('',#101049,60.4792282238308);
#31613=CIRCLE('',#101050,60.4792282238308);
#31614=CIRCLE('',#101052,60.6419265158129);
#31615=CIRCLE('',#101054,60.8618969683742);
#31616=CIRCLE('',#101055,61.0131030316259);
#31617=CIRCLE('',#101057,61.2330734841871);
#31618=CIRCLE('',#101058,61.3957717761693);
#31619=CIRCLE('',#101059,61.3957717761693);
#31620=CIRCLE('',#101060,61.3957717761693);
#31621=CIRCLE('',#101062,61.8704694830905);
#31622=CIRCLE('',#101064,0.635007073208602);
#31623=CIRCLE('',#101065,0.635007073208621);
#31624=CIRCLE('',#101077,60.0045305169095);
#31625=CIRCLE('',#101078,60.4792282238308);
#31626=CIRCLE('',#101079,60.4792282238308);
#31627=CIRCLE('',#101080,60.4792282238308);
#31628=CIRCLE('',#101082,60.6419265158129);
#31629=CIRCLE('',#101084,60.8618969683742);
#31630=CIRCLE('',#101085,61.0131030316259);
#31631=CIRCLE('',#101087,61.2330734841871);
#31632=CIRCLE('',#101088,61.3957717761693);
#31633=CIRCLE('',#101089,61.3957717761693);
#31634=CIRCLE('',#101090,61.3957717761693);
#31635=CIRCLE('',#101092,61.8704694830905);
#31636=CIRCLE('',#101096,0.63500707320862);
#31637=CIRCLE('',#101097,0.635007073208634);
#31638=CIRCLE('',#101108,62.8464445485378);
#31639=CIRCLE('',#101109,59.0285554514622);
#31640=CIRCLE('',#101124,0.127);
#31641=CIRCLE('',#101125,0.127000000000002);
#31642=CIRCLE('',#101127,0.127000000000002);
#31643=CIRCLE('',#101129,0.127000000000002);
#31644=CIRCLE('',#101130,0.126999999999998);
#31645=CIRCLE('',#101131,0.127000000000001);
#31646=CIRCLE('',#101133,0.127000000000005);
#31647=CIRCLE('',#101136,0.127000000000002);
#31648=CIRCLE('',#101138,0.127000000000002);
#31649=CIRCLE('',#101140,0.127000000000002);
#31650=CIRCLE('',#101141,0.127000000000001);
#31651=CIRCLE('',#101142,0.127000000000005);
#31652=CIRCLE('',#101144,0.126999999999999);
#31653=CIRCLE('',#101146,0.126999999999998);
#31654=CIRCLE('',#101147,0.127000000000002);
#31655=CIRCLE('',#101148,0.127000000000002);
#31656=CIRCLE('',#101150,0.127000000000002);
#31657=CIRCLE('',#101153,0.126999999999999);
#31658=CIRCLE('',#101155,0.126999999999999);
#31659=CIRCLE('',#101157,0.127000000000001);
#31660=CIRCLE('',#101158,0.127000000000002);
#31661=CIRCLE('',#101159,0.127000000000002);
#31662=CIRCLE('',#101161,0.127000000000002);
#31663=CIRCLE('',#101164,0.127000000000001);
#31664=CIRCLE('',#101167,62.8464445485378);
#31665=CIRCLE('',#101168,59.0285554514622);
#31666=CIRCLE('',#101180,62.8464445485378);
#31667=CIRCLE('',#101181,59.0285554514622);
#31668=CIRCLE('',#101193,62.8464445485378);
#31669=CIRCLE('',#101194,59.0285554514622);
#31670=CIRCLE('',#101206,62.8464445485378);
#31671=CIRCLE('',#101207,59.0285554514622);
#31672=CIRCLE('',#101219,62.8464445485378);
#31673=CIRCLE('',#101220,59.0285554514622);
#31674=CIRCLE('',#101232,62.8464445485378);
#31675=CIRCLE('',#101233,59.0285554514622);
#31676=CIRCLE('',#101245,62.8464445485378);
#31677=CIRCLE('',#101246,59.0285554514622);
#31678=CIRCLE('',#101258,62.8464445485378);
#31679=CIRCLE('',#101259,59.0285554514622);
#31680=CIRCLE('',#101271,62.8464445485378);
#31681=CIRCLE('',#101272,59.0285554514622);
#31682=CIRCLE('',#101284,62.8464445485378);
#31683=CIRCLE('',#101285,59.0285554514622);
#31684=CIRCLE('',#101297,62.8464445485378);
#31685=CIRCLE('',#101298,59.0285554514622);
#31686=CIRCLE('',#101310,62.8464445485378);
#31687=CIRCLE('',#101311,59.0285554514622);
#31688=CIRCLE('',#101323,62.8464445485378);
#31689=CIRCLE('',#101324,59.0285554514622);
#31690=CIRCLE('',#101336,62.8464445485378);
#31691=CIRCLE('',#101337,59.0285554514622);
#31692=CIRCLE('',#101349,62.8464445485378);
#31693=CIRCLE('',#101350,59.0285554514622);
#31694=CIRCLE('',#101362,62.8464445485378);
#31695=CIRCLE('',#101363,59.0285554514622);
#31696=CIRCLE('',#101375,62.8464445485378);
#31697=CIRCLE('',#101376,59.0285554514622);
#31698=CIRCLE('',#101388,62.8464445485378);
#31699=CIRCLE('',#101389,59.0285554514622);
#31700=CIRCLE('',#101401,62.8464445485378);
#31701=CIRCLE('',#101402,59.0285554514622);
#31702=CIRCLE('',#101414,62.8464445485378);
#31703=CIRCLE('',#101415,59.0285554514622);
#31704=CIRCLE('',#101427,62.8464445485378);
#31705=CIRCLE('',#101428,59.0285554514622);
#31706=CIRCLE('',#101440,62.8464445485378);
#31707=CIRCLE('',#101441,59.0285554514622);
#31708=CIRCLE('',#101453,62.8464445485378);
#31709=CIRCLE('',#101454,59.0285554514622);
#31710=CIRCLE('',#101466,62.8464445485378);
#31711=CIRCLE('',#101467,59.0285554514622);
#31712=CIRCLE('',#101479,62.8464445485378);
#31713=CIRCLE('',#101480,59.0285554514622);
#31714=CIRCLE('',#101492,62.8464445485378);
#31715=CIRCLE('',#101493,59.0285554514622);
#31716=CIRCLE('',#101505,62.8464445485378);
#31717=CIRCLE('',#101506,59.0285554514622);
#31718=CIRCLE('',#101518,62.8464445485378);
#31719=CIRCLE('',#101519,59.0285554514622);
#31720=CIRCLE('',#101531,62.8464445485378);
#31721=CIRCLE('',#101532,59.0285554514622);
#31722=CIRCLE('',#101555,62.8464445485378);
#31723=CIRCLE('',#101556,59.0285554514622);
#31724=CIRCLE('',#101568,62.8464445485378);
#31725=CIRCLE('',#101569,59.0285554514622);
#31726=CIRCLE('',#101581,62.8464445485378);
#31727=CIRCLE('',#101582,59.0285554514622);
#31728=CIRCLE('',#101594,62.8464445485378);
#31729=CIRCLE('',#101595,59.0285554514622);
#31730=CIRCLE('',#101607,62.8464445485378);
#31731=CIRCLE('',#101608,59.0285554514622);
#31732=CIRCLE('',#101620,62.8464445485378);
#31733=CIRCLE('',#101621,59.0285554514622);
#31734=CIRCLE('',#101633,62.8464445485378);
#31735=CIRCLE('',#101634,59.0285554514622);
#31736=CIRCLE('',#101646,62.8464445485378);
#31737=CIRCLE('',#101647,59.0285554514622);
#31738=CIRCLE('',#101659,62.8464445485378);
#31739=CIRCLE('',#101660,59.0285554514622);
#31740=CIRCLE('',#101672,62.8464445485378);
#31741=CIRCLE('',#101673,59.0285554514622);
#31742=CIRCLE('',#101685,62.8464445485378);
#31743=CIRCLE('',#101686,59.0285554514622);
#31744=CIRCLE('',#101698,62.8464445485378);
#31745=CIRCLE('',#101699,59.0285554514622);
#31746=CIRCLE('',#101711,62.8464445485378);
#31747=CIRCLE('',#101712,59.0285554514622);
#31748=CIRCLE('',#101724,62.8464445485378);
#31749=CIRCLE('',#101725,59.0285554514622);
#31750=CIRCLE('',#101748,62.8464445485378);
#31751=CIRCLE('',#101749,59.0285554514622);
#31752=CIRCLE('',#101761,62.8464445485378);
#31753=CIRCLE('',#101762,59.0285554514622);
#31754=CIRCLE('',#101774,62.8464445485378);
#31755=CIRCLE('',#101775,59.0285554514622);
#31756=CIRCLE('',#101787,62.8464445485378);
#31757=CIRCLE('',#101788,59.0285554514622);
#31758=CIRCLE('',#101800,62.8464445485378);
#31759=CIRCLE('',#101801,59.0285554514622);
#31760=CIRCLE('',#101813,62.8464445485378);
#31761=CIRCLE('',#101814,59.0285554514622);
#31762=CIRCLE('',#101826,62.8464445485378);
#31763=CIRCLE('',#101827,59.0285554514622);
#31764=CIRCLE('',#101839,62.8464445485378);
#31765=CIRCLE('',#101840,59.0285554514622);
#31766=CIRCLE('',#101852,62.8464445485378);
#31767=CIRCLE('',#101853,59.0285554514622);
#31768=CIRCLE('',#101865,62.8464445485378);
#31769=CIRCLE('',#101866,59.0285554514622);
#31770=CIRCLE('',#101878,62.8464445485378);
#31771=CIRCLE('',#101879,59.0285554514622);
#31772=CIRCLE('',#101891,62.8464445485378);
#31773=CIRCLE('',#101892,59.0285554514622);
#31774=CIRCLE('',#101904,62.8464445485378);
#31775=CIRCLE('',#101905,59.0285554514622);
#31776=CIRCLE('',#101917,62.8464445485378);
#31777=CIRCLE('',#101918,59.0285554514622);
#31778=CIRCLE('',#102049,0.126999999999998);
#31779=CIRCLE('',#102050,0.127);
#31780=CIRCLE('',#102052,0.127);
#31781=CIRCLE('',#102054,0.127);
#31782=CIRCLE('',#102055,0.127);
#31783=CIRCLE('',#102056,0.127);
#31784=CIRCLE('',#102058,0.126999999999999);
#31785=CIRCLE('',#102061,0.127000000000004);
#31786=CIRCLE('',#102063,0.127);
#31787=CIRCLE('',#102065,0.127000000000002);
#31788=CIRCLE('',#102066,0.127000000000002);
#31789=CIRCLE('',#102067,0.126999999999997);
#31790=CIRCLE('',#102069,0.127000000000001);
#31791=CIRCLE('',#102071,0.127000000000004);
#31792=CIRCLE('',#102072,0.127);
#31793=CIRCLE('',#102073,0.127);
#31794=CIRCLE('',#102075,0.126999999999997);
#31795=CIRCLE('',#102078,0.127000000000001);
#31796=CIRCLE('',#102080,0.127000000000003);
#31797=CIRCLE('',#102082,0.127000000000004);
#31798=CIRCLE('',#102083,0.127);
#31799=CIRCLE('',#102084,0.127);
#31800=CIRCLE('',#102086,0.127);
#31801=CIRCLE('',#102089,0.127);
#31802=CIRCLE('',#102093,0.127000000000001);
#31803=CIRCLE('',#102094,0.126999999999999);
#31804=CIRCLE('',#102096,0.126999999999999);
#31805=CIRCLE('',#102098,0.126999999999999);
#31806=CIRCLE('',#102099,0.127000000000002);
#31807=CIRCLE('',#102100,0.127000000000003);
#31808=CIRCLE('',#102102,0.127000000000002);
#31809=CIRCLE('',#102105,0.127000000000003);
#31810=CIRCLE('',#102107,0.126999999999999);
#31811=CIRCLE('',#102109,0.126999999999997);
#31812=CIRCLE('',#102110,0.127);
#31813=CIRCLE('',#102111,0.127000000000002);
#31814=CIRCLE('',#102113,0.127000000000001);
#31815=CIRCLE('',#102115,0.126999999999999);
#31816=CIRCLE('',#102116,0.127000000000002);
#31817=CIRCLE('',#102117,0.126999999999999);
#31818=CIRCLE('',#102119,0.127000000000001);
#31819=CIRCLE('',#102122,0.127000000000001);
#31820=CIRCLE('',#102124,0.127000000000001);
#31821=CIRCLE('',#102126,0.127000000000002);
#31822=CIRCLE('',#102127,0.126999999999999);
#31823=CIRCLE('',#102128,0.126999999999999);
#31824=CIRCLE('',#102130,0.126999999999999);
#31825=CIRCLE('',#102133,0.127);
#31826=CIRCLE('',#102137,0.127000000000001);
#31827=CIRCLE('',#102138,0.126999999999999);
#31828=CIRCLE('',#102140,0.126999999999999);
#31829=CIRCLE('',#102142,0.127);
#31830=CIRCLE('',#102143,0.126999999999998);
#31831=CIRCLE('',#102144,0.126999999999997);
#31832=CIRCLE('',#102146,0.126999999999997);
#31833=CIRCLE('',#102149,0.126999999999997);
#31834=CIRCLE('',#102151,0.127);
#31835=CIRCLE('',#102153,0.127000000000001);
#31836=CIRCLE('',#102154,0.127000000000001);
#31837=CIRCLE('',#102155,0.127);
#31838=CIRCLE('',#102157,0.126999999999996);
#31839=CIRCLE('',#102159,0.127000000000002);
#31840=CIRCLE('',#102160,0.127000000000003);
#31841=CIRCLE('',#102161,0.126999999999999);
#31842=CIRCLE('',#102163,0.127);
#31843=CIRCLE('',#102166,0.126999999999996);
#31844=CIRCLE('',#102168,0.127000000000001);
#31845=CIRCLE('',#102170,0.127000000000001);
#31846=CIRCLE('',#102171,0.126999999999999);
#31847=CIRCLE('',#102172,0.126999999999999);
#31848=CIRCLE('',#102174,0.126999999999999);
#31849=CIRCLE('',#102177,0.127);
#31850=CIRCLE('',#102181,0.127);
#31851=CIRCLE('',#102182,0.127000000000001);
#31852=CIRCLE('',#102184,0.127000000000001);
#31853=CIRCLE('',#102186,0.127000000000001);
#31854=CIRCLE('',#102187,0.127000000000001);
#31855=CIRCLE('',#102188,0.127000000000001);
#31856=CIRCLE('',#102190,0.126999999999999);
#31857=CIRCLE('',#102193,0.127000000000002);
#31858=CIRCLE('',#102195,0.127000000000001);
#31859=CIRCLE('',#102197,0.127000000000001);
#31860=CIRCLE('',#102198,0.126999999999998);
#31861=CIRCLE('',#102199,0.126999999999999);
#31862=CIRCLE('',#102201,0.127);
#31863=CIRCLE('',#102203,0.127000000000004);
#31864=CIRCLE('',#102204,0.127000000000002);
#31865=CIRCLE('',#102205,0.127000000000001);
#31866=CIRCLE('',#102207,0.126999999999997);
#31867=CIRCLE('',#102210,0.127);
#31868=CIRCLE('',#102212,0.126999999999996);
#31869=CIRCLE('',#102214,0.126999999999998);
#31870=CIRCLE('',#102215,0.127000000000001);
#31871=CIRCLE('',#102216,0.127000000000001);
#31872=CIRCLE('',#102218,0.127000000000001);
#31873=CIRCLE('',#102221,0.127000000000001);
#31874=CIRCLE('',#102225,0.127000000000001);
#31875=CIRCLE('',#102226,0.127);
#31876=CIRCLE('',#102228,0.127);
#31877=CIRCLE('',#102230,0.127);
#31878=CIRCLE('',#102231,0.126999999999999);
#31879=CIRCLE('',#102232,0.126999999999998);
#31880=CIRCLE('',#102234,0.127);
#31881=CIRCLE('',#102237,0.127000000000002);
#31882=CIRCLE('',#102239,0.127);
#31883=CIRCLE('',#102241,0.127000000000002);
#31884=CIRCLE('',#102242,0.127000000000002);
#31885=CIRCLE('',#102243,0.127);
#31886=CIRCLE('',#102245,0.127000000000001);
#31887=CIRCLE('',#102247,0.126999999999999);
#31888=CIRCLE('',#102248,0.126999999999999);
#31889=CIRCLE('',#102249,0.127);
#31890=CIRCLE('',#102251,0.127000000000001);
#31891=CIRCLE('',#102254,0.127000000000001);
#31892=CIRCLE('',#102256,0.127000000000001);
#31893=CIRCLE('',#102258,0.126999999999999);
#31894=CIRCLE('',#102259,0.127);
#31895=CIRCLE('',#102260,0.127);
#31896=CIRCLE('',#102262,0.127);
#31897=CIRCLE('',#102265,0.126999999999998);
#31898=CIRCLE('',#102269,0.127000000000001);
#31899=CIRCLE('',#102270,0.126999999999999);
#31900=CIRCLE('',#102272,0.126999999999999);
#31901=CIRCLE('',#102274,0.127000000000004);
#31902=CIRCLE('',#102275,0.126999999999998);
#31903=CIRCLE('',#102276,0.126999999999997);
#31904=CIRCLE('',#102278,0.126999999999997);
#31905=CIRCLE('',#102281,0.126999999999999);
#31906=CIRCLE('',#102283,0.127);
#31907=CIRCLE('',#102285,0.127);
#31908=CIRCLE('',#102286,0.126999999999997);
#31909=CIRCLE('',#102287,0.126999999999997);
#31910=CIRCLE('',#102289,0.126999999999999);
#31911=CIRCLE('',#102291,0.126999999999998);
#31912=CIRCLE('',#102292,0.127000000000003);
#31913=CIRCLE('',#102293,0.126999999999999);
#31914=CIRCLE('',#102295,0.127);
#31915=CIRCLE('',#102298,0.127000000000003);
#31916=CIRCLE('',#102300,0.127000000000001);
#31917=CIRCLE('',#102302,0.127000000000004);
#31918=CIRCLE('',#102303,0.126999999999999);
#31919=CIRCLE('',#102304,0.127000000000004);
#31920=CIRCLE('',#102306,0.126999999999999);
#31921=CIRCLE('',#102309,0.126999999999997);
#31922=CIRCLE('',#102313,0.126999999999999);
#31923=CIRCLE('',#102314,0.127);
#31924=CIRCLE('',#102316,0.127);
#31925=CIRCLE('',#102318,0.127);
#31926=CIRCLE('',#102319,0.127000000000003);
#31927=CIRCLE('',#102320,0.127000000000001);
#31928=CIRCLE('',#102322,0.126999999999998);
#31929=CIRCLE('',#102325,0.127000000000003);
#31930=CIRCLE('',#102327,0.127);
#31931=CIRCLE('',#102329,0.126999999999999);
#31932=CIRCLE('',#102330,0.127000000000001);
#31933=CIRCLE('',#102331,0.126999999999998);
#31934=CIRCLE('',#102333,0.127000000000001);
#31935=CIRCLE('',#102335,0.126999999999997);
#31936=CIRCLE('',#102336,0.127000000000004);
#31937=CIRCLE('',#102337,0.127);
#31938=CIRCLE('',#102339,0.127000000000001);
#31939=CIRCLE('',#102342,0.126999999999998);
#31940=CIRCLE('',#102344,0.127000000000003);
#31941=CIRCLE('',#102346,0.127000000000001);
#31942=CIRCLE('',#102347,0.127);
#31943=CIRCLE('',#102348,0.127);
#31944=CIRCLE('',#102350,0.127);
#31945=CIRCLE('',#102353,0.127000000000001);
#31946=CIRCLE('',#102357,0.127000000000002);
#31947=CIRCLE('',#102358,0.127);
#31948=CIRCLE('',#102360,0.127);
#31949=CIRCLE('',#102362,0.127);
#31950=CIRCLE('',#102363,0.126999999999997);
#31951=CIRCLE('',#102364,0.127000000000001);
#31952=CIRCLE('',#102366,0.126999999999998);
#31953=CIRCLE('',#102369,0.126999999999999);
#31954=CIRCLE('',#102371,0.127);
#31955=CIRCLE('',#102373,0.127000000000003);
#31956=CIRCLE('',#102374,0.127000000000001);
#31957=CIRCLE('',#102375,0.126999999999998);
#31958=CIRCLE('',#102377,0.126999999999998);
#31959=CIRCLE('',#102379,0.126999999999997);
#31960=CIRCLE('',#102380,0.127000000000001);
#31961=CIRCLE('',#102381,0.127);
#31962=CIRCLE('',#102383,0.127);
#31963=CIRCLE('',#102386,0.127000000000001);
#31964=CIRCLE('',#102388,0.127000000000003);
#31965=CIRCLE('',#102390,0.126999999999998);
#31966=CIRCLE('',#102391,0.127);
#31967=CIRCLE('',#102392,0.127);
#31968=CIRCLE('',#102394,0.127);
#31969=CIRCLE('',#102397,0.127000000000001);
#31970=CIRCLE('',#102401,0.127000000000001);
#31971=CIRCLE('',#102402,0.127);
#31972=CIRCLE('',#102404,0.126999999999999);
#31973=CIRCLE('',#102406,0.127000000000004);
#31974=CIRCLE('',#102407,0.127000000000001);
#31975=CIRCLE('',#102408,0.127);
#31976=CIRCLE('',#102410,0.126999999999997);
#31977=CIRCLE('',#102413,0.126999999999995);
#31978=CIRCLE('',#102415,0.127);
#31979=CIRCLE('',#102417,0.126999999999998);
#31980=CIRCLE('',#102418,0.127000000000004);
#31981=CIRCLE('',#102419,0.126999999999997);
#31982=CIRCLE('',#102421,0.126999999999999);
#31983=CIRCLE('',#102423,0.127000000000001);
#31984=CIRCLE('',#102424,0.127000000000001);
#31985=CIRCLE('',#102425,0.126999999999999);
#31986=CIRCLE('',#102427,0.127000000000003);
#31987=CIRCLE('',#102430,0.126999999999999);
#31988=CIRCLE('',#102432,0.127000000000001);
#31989=CIRCLE('',#102434,0.127000000000004);
#31990=CIRCLE('',#102435,0.126999999999999);
#31991=CIRCLE('',#102436,0.126999999999999);
#31992=CIRCLE('',#102438,0.126999999999999);
#31993=CIRCLE('',#102441,0.126999999999997);
#31994=CIRCLE('',#102445,0.127000000000001);
#31995=CIRCLE('',#102446,0.127);
#31996=CIRCLE('',#102448,0.127);
#31997=CIRCLE('',#102450,0.127);
#31998=CIRCLE('',#102451,0.126999999999999);
#31999=CIRCLE('',#102452,0.126999999999998);
#32000=CIRCLE('',#102454,0.127);
#32001=CIRCLE('',#102457,0.127000000000002);
#32002=CIRCLE('',#102459,0.127);
#32003=CIRCLE('',#102461,0.126999999999999);
#32004=CIRCLE('',#102462,0.126999999999996);
#32005=CIRCLE('',#102463,0.127);
#32006=CIRCLE('',#102465,0.127000000000001);
#32007=CIRCLE('',#102467,0.126999999999999);
#32008=CIRCLE('',#102468,0.127);
#32009=CIRCLE('',#102469,0.127);
#32010=CIRCLE('',#102471,0.126999999999999);
#32011=CIRCLE('',#102474,0.127000000000001);
#32012=CIRCLE('',#102476,0.127000000000001);
#32013=CIRCLE('',#102478,0.126999999999996);
#32014=CIRCLE('',#102479,0.127);
#32015=CIRCLE('',#102480,0.127);
#32016=CIRCLE('',#102482,0.127);
#32017=CIRCLE('',#102485,0.126999999999998);
#32018=CIRCLE('',#102489,0.126999999999997);
#32019=CIRCLE('',#102490,0.127000000000001);
#32020=CIRCLE('',#102492,0.127000000000001);
#32021=CIRCLE('',#102494,0.127000000000001);
#32022=CIRCLE('',#102495,0.127000000000001);
#32023=CIRCLE('',#102496,0.127000000000001);
#32024=CIRCLE('',#102498,0.126999999999996);
#32025=CIRCLE('',#102501,0.127000000000001);
#32026=CIRCLE('',#102503,0.127000000000001);
#32027=CIRCLE('',#102505,0.127000000000001);
#32028=CIRCLE('',#102506,0.126999999999998);
#32029=CIRCLE('',#102507,0.126999999999999);
#32030=CIRCLE('',#102509,0.127);
#32031=CIRCLE('',#102511,0.127000000000001);
#32032=CIRCLE('',#102512,0.126999999999997);
#32033=CIRCLE('',#102513,0.127000000000001);
#32034=CIRCLE('',#102515,0.127000000000001);
#32035=CIRCLE('',#102518,0.126999999999997);
#32036=CIRCLE('',#102520,0.127);
#32037=CIRCLE('',#102522,0.126999999999998);
#32038=CIRCLE('',#102523,0.127000000000001);
#32039=CIRCLE('',#102524,0.127000000000001);
#32040=CIRCLE('',#102526,0.127000000000001);
#32041=CIRCLE('',#102529,0.127000000000004);
#32042=CIRCLE('',#102533,0.126999999999999);
#32043=CIRCLE('',#102534,0.127000000000002);
#32044=CIRCLE('',#102536,0.126999999999999);
#32045=CIRCLE('',#102538,0.126999999999999);
#32046=CIRCLE('',#102539,0.127000000000002);
#32047=CIRCLE('',#102540,0.127);
#32048=CIRCLE('',#102542,0.126999999999997);
#32049=CIRCLE('',#102545,0.127);
#32050=CIRCLE('',#102547,0.127);
#32051=CIRCLE('',#102549,0.126999999999998);
#32052=CIRCLE('',#102550,0.127000000000001);
#32053=CIRCLE('',#102551,0.126999999999997);
#32054=CIRCLE('',#102553,0.126999999999996);
#32055=CIRCLE('',#102555,0.126999999999998);
#32056=CIRCLE('',#102556,0.127);
#32057=CIRCLE('',#102557,0.126999999999999);
#32058=CIRCLE('',#102559,0.127000000000003);
#32059=CIRCLE('',#102562,0.126999999999996);
#32060=CIRCLE('',#102564,0.127000000000001);
#32061=CIRCLE('',#102566,0.127000000000001);
#32062=CIRCLE('',#102567,0.126999999999999);
#32063=CIRCLE('',#102568,0.126999999999999);
#32064=CIRCLE('',#102570,0.126999999999999);
#32065=CIRCLE('',#102573,0.127);
#32066=CIRCLE('',#102577,0.127000000000001);
#32067=CIRCLE('',#102578,0.126999999999999);
#32068=CIRCLE('',#102580,0.126999999999999);
#32069=CIRCLE('',#102582,0.126999999999999);
#32070=CIRCLE('',#102583,0.127000000000002);
#32071=CIRCLE('',#102584,0.127000000000003);
#32072=CIRCLE('',#102586,0.127000000000002);
#32073=CIRCLE('',#102589,0.126999999999997);
#32074=CIRCLE('',#102591,0.126999999999999);
#32075=CIRCLE('',#102593,0.126999999999996);
#32076=CIRCLE('',#102594,0.127000000000002);
#32077=CIRCLE('',#102595,0.127);
#32078=CIRCLE('',#102597,0.127000000000001);
#32079=CIRCLE('',#102599,0.127000000000002);
#32080=CIRCLE('',#102600,0.127);
#32081=CIRCLE('',#102601,0.126999999999999);
#32082=CIRCLE('',#102603,0.127000000000002);
#32083=CIRCLE('',#102606,0.127000000000001);
#32084=CIRCLE('',#102608,0.126999999999998);
#32085=CIRCLE('',#102610,0.126999999999996);
#32086=CIRCLE('',#102611,0.126999999999999);
#32087=CIRCLE('',#102612,0.126999999999999);
#32088=CIRCLE('',#102614,0.126999999999999);
#32089=CIRCLE('',#102617,0.127);
#32090=CIRCLE('',#102621,0.127000000000004);
#32091=CIRCLE('',#102622,0.127);
#32092=CIRCLE('',#102624,0.127);
#32093=CIRCLE('',#102626,0.127);
#32094=CIRCLE('',#102627,0.127);
#32095=CIRCLE('',#102628,0.127);
#32096=CIRCLE('',#102630,0.126999999999999);
#32097=CIRCLE('',#102633,0.127000000000002);
#32098=CIRCLE('',#102635,0.127);
#32099=CIRCLE('',#102637,0.127000000000004);
#32100=CIRCLE('',#102638,0.126999999999998);
#32101=CIRCLE('',#102639,0.126999999999999);
#32102=CIRCLE('',#102641,0.127000000000001);
#32103=CIRCLE('',#102643,0.126999999999998);
#32104=CIRCLE('',#102644,0.126999999999997);
#32105=CIRCLE('',#102645,0.127);
#32106=CIRCLE('',#102647,0.127);
#32107=CIRCLE('',#102650,0.127000000000001);
#32108=CIRCLE('',#102652,0.127000000000003);
#32109=CIRCLE('',#102654,0.126999999999998);
#32110=CIRCLE('',#102655,0.127);
#32111=CIRCLE('',#102656,0.127);
#32112=CIRCLE('',#102658,0.127);
#32113=CIRCLE('',#102661,0.127);
#32114=CIRCLE('',#102665,0.127);
#32115=CIRCLE('',#102666,0.127000000000002);
#32116=CIRCLE('',#102668,0.127000000000002);
#32117=CIRCLE('',#102670,0.127000000000002);
#32118=CIRCLE('',#102671,0.126999999999998);
#32119=CIRCLE('',#102672,0.127000000000001);
#32120=CIRCLE('',#102674,0.127000000000005);
#32121=CIRCLE('',#102677,0.127000000000002);
#32122=CIRCLE('',#102679,0.127000000000002);
#32123=CIRCLE('',#102681,0.127000000000002);
#32124=CIRCLE('',#102682,0.127000000000001);
#32125=CIRCLE('',#102683,0.126999999999997);
#32126=CIRCLE('',#102685,0.126999999999999);
#32127=CIRCLE('',#102687,0.126999999999998);
#32128=CIRCLE('',#102688,0.127000000000002);
#32129=CIRCLE('',#102689,0.127000000000002);
#32130=CIRCLE('',#102691,0.127000000000002);
#32131=CIRCLE('',#102694,0.126999999999999);
#32132=CIRCLE('',#102696,0.127000000000003);
#32133=CIRCLE('',#102698,0.127000000000001);
#32134=CIRCLE('',#102699,0.127000000000002);
#32135=CIRCLE('',#102700,0.127000000000002);
#32136=CIRCLE('',#102702,0.127000000000002);
#32137=CIRCLE('',#102705,0.127000000000001);
#32138=CIRCLE('',#102709,0.126999999999998);
#32139=CIRCLE('',#102710,0.127);
#32140=CIRCLE('',#102712,0.127);
#32141=CIRCLE('',#102714,0.127);
#32142=CIRCLE('',#102715,0.126999999999998);
#32143=CIRCLE('',#102716,0.127);
#32144=CIRCLE('',#102718,0.126999999999999);
#32145=CIRCLE('',#102721,0.127000000000004);
#32146=CIRCLE('',#102723,0.127);
#32147=CIRCLE('',#102725,0.127000000000002);
#32148=CIRCLE('',#102726,0.126999999999998);
#32149=CIRCLE('',#102727,0.126999999999999);
#32150=CIRCLE('',#102729,0.127000000000001);
#32151=CIRCLE('',#102731,0.127000000000004);
#32152=CIRCLE('',#102732,0.127);
#32153=CIRCLE('',#102733,0.127);
#32154=CIRCLE('',#102735,0.126999999999997);
#32155=CIRCLE('',#102738,0.127000000000001);
#32156=CIRCLE('',#102740,0.127000000000003);
#32157=CIRCLE('',#102742,0.127000000000004);
#32158=CIRCLE('',#102743,0.127);
#32159=CIRCLE('',#102744,0.127);
#32160=CIRCLE('',#102746,0.127);
#32161=CIRCLE('',#102749,0.127);
#32162=CIRCLE('',#102753,0.127000000000001);
#32163=CIRCLE('',#102754,0.126999999999999);
#32164=CIRCLE('',#102756,0.126999999999999);
#32165=CIRCLE('',#102758,0.126999999999999);
#32166=CIRCLE('',#102759,0.126999999999999);
#32167=CIRCLE('',#102760,0.127);
#32168=CIRCLE('',#102762,0.127000000000002);
#32169=CIRCLE('',#102765,0.126999999999997);
#32170=CIRCLE('',#102767,0.126999999999999);
#32171=CIRCLE('',#102769,0.126999999999997);
#32172=CIRCLE('',#102770,0.127);
#32173=CIRCLE('',#102771,0.127000000000002);
#32174=CIRCLE('',#102773,0.127000000000001);
#32175=CIRCLE('',#102775,0.126999999999999);
#32176=CIRCLE('',#102776,0.127000000000002);
#32177=CIRCLE('',#102777,0.126999999999999);
#32178=CIRCLE('',#102779,0.127000000000001);
#32179=CIRCLE('',#102782,0.127000000000001);
#32180=CIRCLE('',#102784,0.126999999999997);
#32181=CIRCLE('',#102786,0.127000000000002);
#32182=CIRCLE('',#102787,0.126999999999999);
#32183=CIRCLE('',#102788,0.126999999999999);
#32184=CIRCLE('',#102790,0.126999999999999);
#32185=CIRCLE('',#102793,0.127);
#32186=CIRCLE('',#102797,0.127000000000001);
#32187=CIRCLE('',#102798,0.126999999999999);
#32188=CIRCLE('',#102800,0.126999999999999);
#32189=CIRCLE('',#102802,0.127);
#32190=CIRCLE('',#102803,0.126999999999998);
#32191=CIRCLE('',#102804,0.127);
#32192=CIRCLE('',#102806,0.126999999999997);
#32193=CIRCLE('',#102809,0.126999999999998);
#32194=CIRCLE('',#102811,0.126999999999999);
#32195=CIRCLE('',#102813,0.127);
#32196=CIRCLE('',#102814,0.127000000000001);
#32197=CIRCLE('',#102815,0.127000000000003);
#32198=CIRCLE('',#102817,0.126999999999996);
#32199=CIRCLE('',#102819,0.127000000000002);
#32200=CIRCLE('',#102820,0.126999999999997);
#32201=CIRCLE('',#102821,0.126999999999999);
#32202=CIRCLE('',#102823,0.127);
#32203=CIRCLE('',#102826,0.126999999999999);
#32204=CIRCLE('',#102828,0.127000000000004);
#32205=CIRCLE('',#102830,0.127000000000001);
#32206=CIRCLE('',#102831,0.126999999999999);
#32207=CIRCLE('',#102832,0.126999999999999);
#32208=CIRCLE('',#102834,0.126999999999999);
#32209=CIRCLE('',#102837,0.127);
#32210=CIRCLE('',#102841,0.127);
#32211=CIRCLE('',#102842,0.127000000000001);
#32212=CIRCLE('',#102844,0.127000000000001);
#32213=CIRCLE('',#102846,0.127000000000001);
#32214=CIRCLE('',#102847,0.127000000000001);
#32215=CIRCLE('',#102848,0.127000000000001);
#32216=CIRCLE('',#102850,0.126999999999999);
#32217=CIRCLE('',#102853,0.127000000000002);
#32218=CIRCLE('',#102855,0.127000000000001);
#32219=CIRCLE('',#102857,0.127000000000001);
#32220=CIRCLE('',#102858,0.126999999999998);
#32221=CIRCLE('',#102859,0.126999999999996);
#32222=CIRCLE('',#102861,0.127);
#32223=CIRCLE('',#102863,0.127000000000001);
#32224=CIRCLE('',#102864,0.127000000000002);
#32225=CIRCLE('',#102865,0.127000000000001);
#32226=CIRCLE('',#102867,0.126999999999998);
#32227=CIRCLE('',#102870,0.127);
#32228=CIRCLE('',#102872,0.127);
#32229=CIRCLE('',#102874,0.127000000000004);
#32230=CIRCLE('',#102875,0.127000000000001);
#32231=CIRCLE('',#102876,0.127000000000001);
#32232=CIRCLE('',#102878,0.127000000000001);
#32233=CIRCLE('',#102881,0.126999999999998);
#32234=CIRCLE('',#102885,0.127000000000001);
#32235=CIRCLE('',#102886,0.127);
#32236=CIRCLE('',#102888,0.127000000000003);
#32237=CIRCLE('',#102890,0.127);
#32238=CIRCLE('',#102891,0.127000000000002);
#32239=CIRCLE('',#102892,0.127000000000001);
#32240=CIRCLE('',#102894,0.127);
#32241=CIRCLE('',#102897,0.126999999999998);
#32242=CIRCLE('',#102899,0.127);
#32243=CIRCLE('',#102901,0.127000000000002);
#32244=CIRCLE('',#102902,0.127000000000002);
#32245=CIRCLE('',#102903,0.127);
#32246=CIRCLE('',#102905,0.127000000000001);
#32247=CIRCLE('',#102907,0.127000000000002);
#32248=CIRCLE('',#102908,0.126999999999999);
#32249=CIRCLE('',#102909,0.127);
#32250=CIRCLE('',#102911,0.127);
#32251=CIRCLE('',#102914,0.127000000000001);
#32252=CIRCLE('',#102916,0.127000000000001);
#32253=CIRCLE('',#102918,0.127000000000002);
#32254=CIRCLE('',#102919,0.127);
#32255=CIRCLE('',#102920,0.127);
#32256=CIRCLE('',#102922,0.127);
#32257=CIRCLE('',#102925,0.126999999999998);
#32258=CIRCLE('',#102929,0.127000000000001);
#32259=CIRCLE('',#102930,0.127000000000004);
#32260=CIRCLE('',#102932,0.126999999999999);
#32261=CIRCLE('',#102934,0.127000000000004);
#32262=CIRCLE('',#102935,0.126999999999998);
#32263=CIRCLE('',#102936,0.126999999999997);
#32264=CIRCLE('',#102938,0.127);
#32265=CIRCLE('',#102941,0.126999999999998);
#32266=CIRCLE('',#102943,0.127000000000004);
#32267=CIRCLE('',#102945,0.126999999999995);
#32268=CIRCLE('',#102946,0.126999999999997);
#32269=CIRCLE('',#102947,0.127);
#32270=CIRCLE('',#102949,0.126999999999999);
#32271=CIRCLE('',#102951,0.126999999999998);
#32272=CIRCLE('',#102952,0.127000000000003);
#32273=CIRCLE('',#102953,0.126999999999999);
#32274=CIRCLE('',#102955,0.127);
#32275=CIRCLE('',#102958,0.127000000000002);
#32276=CIRCLE('',#102960,0.126999999999998);
#32277=CIRCLE('',#102962,0.127);
#32278=CIRCLE('',#102963,0.126999999999999);
#32279=CIRCLE('',#102964,0.126999999999999);
#32280=CIRCLE('',#102966,0.126999999999999);
#32281=CIRCLE('',#102969,0.126999999999997);
#32282=CIRCLE('',#102973,0.126999999999999);
#32283=CIRCLE('',#102974,0.127);
#32284=CIRCLE('',#102976,0.127);
#32285=CIRCLE('',#102978,0.127);
#32286=CIRCLE('',#102979,0.126999999999997);
#32287=CIRCLE('',#102980,0.127000000000001);
#32288=CIRCLE('',#102982,0.126999999999998);
#32289=CIRCLE('',#102985,0.126999999999998);
#32290=CIRCLE('',#102987,0.127);
#32291=CIRCLE('',#102989,0.126999999999998);
#32292=CIRCLE('',#102990,0.127000000000001);
#32293=CIRCLE('',#102991,0.126999999999998);
#32294=CIRCLE('',#102993,0.127000000000001);
#32295=CIRCLE('',#102995,0.127000000000003);
#32296=CIRCLE('',#102996,0.127);
#32297=CIRCLE('',#102997,0.127);
#32298=CIRCLE('',#102999,0.126999999999996);
#32299=CIRCLE('',#103002,0.126999999999998);
#32300=CIRCLE('',#103004,0.126999999999999);
#32301=CIRCLE('',#103006,0.127000000000001);
#32302=CIRCLE('',#103007,0.127);
#32303=CIRCLE('',#103008,0.127);
#32304=CIRCLE('',#103010,0.127);
#32305=CIRCLE('',#103013,0.127000000000001);
#32306=CIRCLE('',#103017,0.126999999999999);
#32307=CIRCLE('',#103018,0.127);
#32308=CIRCLE('',#103020,0.127);
#32309=CIRCLE('',#103022,0.127);
#32310=CIRCLE('',#103023,0.127000000000003);
#32311=CIRCLE('',#103024,0.127000000000001);
#32312=CIRCLE('',#103026,0.127000000000002);
#32313=CIRCLE('',#103029,0.126999999999999);
#32314=CIRCLE('',#103031,0.127);
#32315=CIRCLE('',#103033,0.127000000000003);
#32316=CIRCLE('',#103034,0.127000000000004);
#32317=CIRCLE('',#103035,0.127000000000001);
#32318=CIRCLE('',#103037,0.126999999999998);
#32319=CIRCLE('',#103039,0.126999999999997);
#32320=CIRCLE('',#103040,0.127000000000001);
#32321=CIRCLE('',#103041,0.127);
#32322=CIRCLE('',#103043,0.127);
#32323=CIRCLE('',#103046,0.127000000000001);
#32324=CIRCLE('',#103048,0.126999999999999);
#32325=CIRCLE('',#103050,0.127000000000001);
#32326=CIRCLE('',#103051,0.127);
#32327=CIRCLE('',#103052,0.127);
#32328=CIRCLE('',#103054,0.127);
#32329=CIRCLE('',#103057,0.127000000000001);
#32330=CIRCLE('',#103061,0.127000000000001);
#32331=CIRCLE('',#103062,0.127000000000004);
#32332=CIRCLE('',#103064,0.127000000000004);
#32333=CIRCLE('',#103066,0.127);
#32334=CIRCLE('',#103067,0.127000000000001);
#32335=CIRCLE('',#103068,0.126999999999997);
#32336=CIRCLE('',#103070,0.127);
#32337=CIRCLE('',#103073,0.126999999999995);
#32338=CIRCLE('',#103075,0.127000000000004);
#32339=CIRCLE('',#103077,0.126999999999998);
#32340=CIRCLE('',#103078,0.127000000000001);
#32341=CIRCLE('',#103079,0.127);
#32342=CIRCLE('',#103081,0.126999999999999);
#32343=CIRCLE('',#103083,0.127000000000001);
#32344=CIRCLE('',#103084,0.127);
#32345=CIRCLE('',#103085,0.127000000000004);
#32346=CIRCLE('',#103087,0.127000000000003);
#32347=CIRCLE('',#103090,0.126999999999999);
#32348=CIRCLE('',#103092,0.127000000000001);
#32349=CIRCLE('',#103094,0.127000000000004);
#32350=CIRCLE('',#103095,0.127000000000004);
#32351=CIRCLE('',#103096,0.127);
#32352=CIRCLE('',#103098,0.127000000000004);
#32353=CIRCLE('',#103101,0.127);
#32354=CIRCLE('',#103105,0.127000000000001);
#32355=CIRCLE('',#103106,0.127);
#32356=CIRCLE('',#103108,0.127);
#32357=CIRCLE('',#103110,0.127);
#32358=CIRCLE('',#103111,0.126999999999999);
#32359=CIRCLE('',#103112,0.127000000000001);
#32360=CIRCLE('',#103114,0.127);
#32361=CIRCLE('',#103117,0.127000000000002);
#32362=CIRCLE('',#103119,0.126999999999999);
#32363=CIRCLE('',#103121,0.127000000000002);
#32364=CIRCLE('',#103122,0.127000000000002);
#32365=CIRCLE('',#103123,0.127);
#32366=CIRCLE('',#103125,0.126999999999998);
#32367=CIRCLE('',#103127,0.126999999999999);
#32368=CIRCLE('',#103128,0.127);
#32369=CIRCLE('',#103129,0.127000000000003);
#32370=CIRCLE('',#103131,0.126999999999998);
#32371=CIRCLE('',#103134,0.127000000000001);
#32372=CIRCLE('',#103136,0.126999999999998);
#32373=CIRCLE('',#103138,0.127000000000002);
#32374=CIRCLE('',#103139,0.127);
#32375=CIRCLE('',#103140,0.127);
#32376=CIRCLE('',#103142,0.127);
#32377=CIRCLE('',#103145,0.126999999999998);
#32378=CIRCLE('',#103149,0.127);
#32379=CIRCLE('',#103150,0.127000000000001);
#32380=CIRCLE('',#103152,0.127000000000001);
#32381=CIRCLE('',#103154,0.127000000000001);
#32382=CIRCLE('',#103155,0.127000000000001);
#32383=CIRCLE('',#103156,0.127000000000004);
#32384=CIRCLE('',#103158,0.126999999999999);
#32385=CIRCLE('',#103161,0.127000000000002);
#32386=CIRCLE('',#103163,0.127000000000001);
#32387=CIRCLE('',#103165,0.127000000000001);
#32388=CIRCLE('',#103166,0.127000000000001);
#32389=CIRCLE('',#103167,0.126999999999999);
#32390=CIRCLE('',#103169,0.126999999999997);
#32391=CIRCLE('',#103171,0.126999999999997);
#32392=CIRCLE('',#103172,0.127000000000003);
#32393=CIRCLE('',#103173,0.127000000000001);
#32394=CIRCLE('',#103175,0.127000000000001);
#32395=CIRCLE('',#103178,0.127);
#32396=CIRCLE('',#103180,0.127);
#32397=CIRCLE('',#103182,0.126999999999998);
#32398=CIRCLE('',#103183,0.127000000000001);
#32399=CIRCLE('',#103184,0.127000000000001);
#32400=CIRCLE('',#103186,0.127000000000001);
#32401=CIRCLE('',#103189,0.127000000000001);
#32402=CIRCLE('',#103193,0.126999999999999);
#32403=CIRCLE('',#103194,0.126999999999999);
#32404=CIRCLE('',#103196,0.126999999999999);
#32405=CIRCLE('',#103198,0.126999999999999);
#32406=CIRCLE('',#103199,0.126999999999998);
#32407=CIRCLE('',#103200,0.127);
#32408=CIRCLE('',#103202,0.126999999999997);
#32409=CIRCLE('',#103205,0.127);
#32410=CIRCLE('',#103207,0.127);
#32411=CIRCLE('',#103209,0.126999999999998);
#32412=CIRCLE('',#103210,0.127000000000001);
#32413=CIRCLE('',#103211,0.126999999999997);
#32414=CIRCLE('',#103213,0.126999999999996);
#32415=CIRCLE('',#103215,0.127000000000002);
#32416=CIRCLE('',#103216,0.126999999999999);
#32417=CIRCLE('',#103217,0.126999999999999);
#32418=CIRCLE('',#103219,0.127000000000002);
#32419=CIRCLE('',#103222,0.126999999999996);
#32420=CIRCLE('',#103224,0.127000000000001);
#32421=CIRCLE('',#103226,0.127000000000001);
#32422=CIRCLE('',#103227,0.126999999999999);
#32423=CIRCLE('',#103228,0.127);
#32424=CIRCLE('',#103230,0.126999999999999);
#32425=CIRCLE('',#103233,0.127000000000003);
#32426=CIRCLE('',#103237,0.127000000000001);
#32427=CIRCLE('',#103238,0.127000000000001);
#32428=CIRCLE('',#103240,0.126999999999999);
#32429=CIRCLE('',#103242,0.127000000000001);
#32430=CIRCLE('',#103243,0.127000000000002);
#32431=CIRCLE('',#103244,0.127);
#32432=CIRCLE('',#103246,0.127000000000002);
#32433=CIRCLE('',#103249,0.126999999999997);
#32434=CIRCLE('',#103251,0.126999999999999);
#32435=CIRCLE('',#103253,0.126999999999997);
#32436=CIRCLE('',#103254,0.127);
#32437=CIRCLE('',#103255,0.126999999999999);
#32438=CIRCLE('',#103257,0.127000000000001);
#32439=CIRCLE('',#103259,0.126999999999999);
#32440=CIRCLE('',#103260,0.127);
#32441=CIRCLE('',#103261,0.126999999999999);
#32442=CIRCLE('',#103263,0.127000000000002);
#32443=CIRCLE('',#103266,0.127000000000001);
#32444=CIRCLE('',#103268,0.127000000000001);
#32445=CIRCLE('',#103270,0.126999999999996);
#32446=CIRCLE('',#103271,0.126999999999999);
#32447=CIRCLE('',#103272,0.126999999999999);
#32448=CIRCLE('',#103274,0.126999999999999);
#32449=CIRCLE('',#103277,0.127);
#32450=CIRCLE('',#103281,0.127000000000004);
#32451=CIRCLE('',#103282,0.127);
#32452=CIRCLE('',#103284,0.127);
#32453=CIRCLE('',#103286,0.127);
#32454=CIRCLE('',#103287,0.126999999999998);
#32455=CIRCLE('',#103288,0.127);
#32456=CIRCLE('',#103290,0.126999999999999);
#32457=CIRCLE('',#103293,0.127000000000002);
#32458=CIRCLE('',#103295,0.127);
#32459=CIRCLE('',#103297,0.127000000000004);
#32460=CIRCLE('',#103298,0.127000000000004);
#32461=CIRCLE('',#103299,0.126999999999999);
#32462=CIRCLE('',#103301,0.127000000000001);
#32463=CIRCLE('',#103303,0.126999999999998);
#32464=CIRCLE('',#103304,0.126999999999997);
#32465=CIRCLE('',#103305,0.127);
#32466=CIRCLE('',#103307,0.127);
#32467=CIRCLE('',#103310,0.127000000000001);
#32468=CIRCLE('',#103312,0.127000000000003);
#32469=CIRCLE('',#103314,0.126999999999998);
#32470=CIRCLE('',#103315,0.127);
#32471=CIRCLE('',#103316,0.127);
#32472=CIRCLE('',#103318,0.127);
#32473=CIRCLE('',#103321,0.127);
#32474=CIRCLE('',#103325,0.127);
#32475=CIRCLE('',#103326,0.127000000000002);
#32476=CIRCLE('',#103328,0.127000000000002);
#32477=CIRCLE('',#103330,0.127000000000002);
#32478=CIRCLE('',#103331,0.126999999999998);
#32479=CIRCLE('',#103332,0.127000000000001);
#32480=CIRCLE('',#103334,0.127000000000005);
#32481=CIRCLE('',#103338,0.127000000000002);
#32482=CIRCLE('',#103339,0.127000000000001);
#32483=CIRCLE('',#103340,0.127000000000005);
#32484=CIRCLE('',#103342,0.126999999999999);
#32485=CIRCLE('',#103344,0.126999999999998);
#32486=CIRCLE('',#103345,0.127000000000002);
#32487=CIRCLE('',#103348,0.126999999999999);
#32488=CIRCLE('',#103350,0.126999999999999);
#32489=CIRCLE('',#103352,0.127000000000001);
#32490=CIRCLE('',#103353,0.127000000000002);
#32491=CIRCLE('',#103354,0.127000000000002);
#32492=CIRCLE('',#103356,0.127000000000002);
#32493=CIRCLE('',#103359,0.127000000000001);
#32494=CIRCLE('',#103363,0.126999999999998);
#32495=CIRCLE('',#103364,0.127);
#32496=CIRCLE('',#103366,0.127);
#32497=CIRCLE('',#103368,0.127);
#32498=CIRCLE('',#103369,0.126999999999998);
#32499=CIRCLE('',#103370,0.127);
#32500=CIRCLE('',#103372,0.126999999999999);
#32501=CIRCLE('',#103375,0.127000000000004);
#32502=CIRCLE('',#103377,0.127);
#32503=CIRCLE('',#103379,0.127000000000002);
#32504=CIRCLE('',#103380,0.126999999999998);
#32505=CIRCLE('',#103381,0.126999999999999);
#32506=CIRCLE('',#103383,0.127000000000001);
#32507=CIRCLE('',#103385,0.126999999999996);
#32508=CIRCLE('',#103386,0.127);
#32509=CIRCLE('',#103387,0.127);
#32510=CIRCLE('',#103389,0.126999999999997);
#32511=CIRCLE('',#103392,0.127000000000001);
#32512=CIRCLE('',#103394,0.127000000000003);
#32513=CIRCLE('',#103396,0.127000000000004);
#32514=CIRCLE('',#103397,0.127);
#32515=CIRCLE('',#103398,0.127);
#32516=CIRCLE('',#103400,0.127);
#32517=CIRCLE('',#103403,0.127);
#32518=CIRCLE('',#103407,0.127000000000001);
#32519=CIRCLE('',#103408,0.126999999999999);
#32520=CIRCLE('',#103410,0.126999999999999);
#32521=CIRCLE('',#103412,0.126999999999999);
#32522=CIRCLE('',#103413,0.127000000000002);
#32523=CIRCLE('',#103414,0.127);
#32524=CIRCLE('',#103416,0.127000000000002);
#32525=CIRCLE('',#103419,0.126999999999997);
#32526=CIRCLE('',#103421,0.126999999999999);
#32527=CIRCLE('',#103423,0.126999999999997);
#32528=CIRCLE('',#103424,0.126999999999996);
#32529=CIRCLE('',#103425,0.127000000000002);
#32530=CIRCLE('',#103427,0.127000000000001);
#32531=CIRCLE('',#103429,0.127000000000002);
#32532=CIRCLE('',#103430,0.127000000000002);
#32533=CIRCLE('',#103431,0.126999999999999);
#32534=CIRCLE('',#103433,0.127000000000001);
#32535=CIRCLE('',#103436,0.127000000000001);
#32536=CIRCLE('',#103438,0.127000000000001);
#32537=CIRCLE('',#103440,0.127000000000002);
#32538=CIRCLE('',#103441,0.126999999999999);
#32539=CIRCLE('',#103442,0.126999999999999);
#32540=CIRCLE('',#103444,0.126999999999999);
#32541=CIRCLE('',#103447,0.127000000000003);
#32542=CIRCLE('',#103451,0.127000000000001);
#32543=CIRCLE('',#103452,0.126999999999999);
#32544=CIRCLE('',#103454,0.126999999999999);
#32545=CIRCLE('',#103456,0.127000000000002);
#32546=CIRCLE('',#103457,0.126999999999998);
#32547=CIRCLE('',#103458,0.127);
#32548=CIRCLE('',#103460,0.126999999999997);
#32549=CIRCLE('',#103463,0.126999999999999);
#32550=CIRCLE('',#103465,0.127000000000002);
#32551=CIRCLE('',#103467,0.127000000000001);
#32552=CIRCLE('',#103468,0.127000000000001);
#32553=CIRCLE('',#103469,0.127);
#32554=CIRCLE('',#103471,0.126999999999999);
#32555=CIRCLE('',#103473,0.126999999999998);
#32556=CIRCLE('',#103474,0.126999999999997);
#32557=CIRCLE('',#103475,0.126999999999999);
#32558=CIRCLE('',#103477,0.127);
#32559=CIRCLE('',#103480,0.127000000000002);
#32560=CIRCLE('',#103482,0.127000000000001);
#32561=CIRCLE('',#103484,0.126999999999997);
#32562=CIRCLE('',#103485,0.126999999999999);
#32563=CIRCLE('',#103486,0.126999999999999);
#32564=CIRCLE('',#103488,0.126999999999999);
#32565=CIRCLE('',#103491,0.127);
#32566=CIRCLE('',#103495,0.127);
#32567=CIRCLE('',#103496,0.127000000000001);
#32568=CIRCLE('',#103498,0.127000000000001);
#32569=CIRCLE('',#103500,0.127000000000001);
#32570=CIRCLE('',#103501,0.127000000000001);
#32571=CIRCLE('',#103502,0.127000000000004);
#32572=CIRCLE('',#103504,0.126999999999999);
#32573=CIRCLE('',#103507,0.127000000000002);
#32574=CIRCLE('',#103509,0.127000000000001);
#32575=CIRCLE('',#103511,0.127000000000001);
#32576=CIRCLE('',#103512,0.127000000000001);
#32577=CIRCLE('',#103513,0.127000000000002);
#32578=CIRCLE('',#103515,0.127);
#32579=CIRCLE('',#103517,0.127000000000001);
#32580=CIRCLE('',#103518,0.127000000000002);
#32581=CIRCLE('',#103519,0.127000000000001);
#32582=CIRCLE('',#103521,0.126999999999998);
#32583=CIRCLE('',#103524,0.126999999999997);
#32584=CIRCLE('',#103526,0.127);
#32585=CIRCLE('',#103528,0.127000000000004);
#32586=CIRCLE('',#103529,0.127000000000001);
#32587=CIRCLE('',#103530,0.127000000000001);
#32588=CIRCLE('',#103532,0.127000000000001);
#32589=CIRCLE('',#103535,0.127000000000001);
#32590=CIRCLE('',#103539,0.127000000000001);
#32591=CIRCLE('',#103540,0.127);
#32592=CIRCLE('',#103542,0.127);
#32593=CIRCLE('',#103544,0.127);
#32594=CIRCLE('',#103545,0.126999999999999);
#32595=CIRCLE('',#103546,0.126999999999998);
#32596=CIRCLE('',#103548,0.127);
#32597=CIRCLE('',#103551,0.127000000000002);
#32598=CIRCLE('',#103553,0.127);
#32599=CIRCLE('',#103555,0.127000000000002);
#32600=CIRCLE('',#103556,0.126999999999999);
#32601=CIRCLE('',#103557,0.127);
#32602=CIRCLE('',#103559,0.127000000000001);
#32603=CIRCLE('',#103561,0.126999999999999);
#32604=CIRCLE('',#103562,0.126999999999999);
#32605=CIRCLE('',#103563,0.127);
#32606=CIRCLE('',#103565,0.127000000000001);
#32607=CIRCLE('',#103568,0.127000000000001);
#32608=CIRCLE('',#103570,0.127000000000001);
#32609=CIRCLE('',#103572,0.126999999999999);
#32610=CIRCLE('',#103573,0.127);
#32611=CIRCLE('',#103574,0.127);
#32612=CIRCLE('',#103576,0.127);
#32613=CIRCLE('',#103579,0.126999999999998);
#32614=CIRCLE('',#103583,0.127000000000001);
#32615=CIRCLE('',#103584,0.127000000000004);
#32616=CIRCLE('',#103586,0.126999999999999);
#32617=CIRCLE('',#103588,0.127000000000004);
#32618=CIRCLE('',#103589,0.126999999999998);
#32619=CIRCLE('',#103590,0.126999999999997);
#32620=CIRCLE('',#103592,0.127);
#32621=CIRCLE('',#103595,0.126999999999998);
#32622=CIRCLE('',#103597,0.127000000000003);
#32623=CIRCLE('',#103599,0.126999999999995);
#32624=CIRCLE('',#103600,0.127000000000001);
#32625=CIRCLE('',#103601,0.127);
#32626=CIRCLE('',#103603,0.126999999999999);
#32627=CIRCLE('',#103605,0.127000000000001);
#32628=CIRCLE('',#103606,0.127000000000003);
#32629=CIRCLE('',#103607,0.126999999999999);
#32630=CIRCLE('',#103609,0.127);
#32631=CIRCLE('',#103612,0.126999999999999);
#32632=CIRCLE('',#103614,0.127000000000001);
#32633=CIRCLE('',#103616,0.126999999999997);
#32634=CIRCLE('',#103617,0.126999999999999);
#32635=CIRCLE('',#103618,0.126999999999999);
#32636=CIRCLE('',#103620,0.126999999999999);
#32637=CIRCLE('',#103623,0.126999999999997);
#32638=CIRCLE('',#103627,0.126999999999999);
#32639=CIRCLE('',#103628,0.127);
#32640=CIRCLE('',#103630,0.127);
#32641=CIRCLE('',#103632,0.127);
#32642=CIRCLE('',#103633,0.126999999999997);
#32643=CIRCLE('',#103634,0.127000000000001);
#32644=CIRCLE('',#103636,0.127000000000002);
#32645=CIRCLE('',#103639,0.127000000000003);
#32646=CIRCLE('',#103641,0.127);
#32647=CIRCLE('',#103643,0.126999999999998);
#32648=CIRCLE('',#103644,0.127000000000001);
#32649=CIRCLE('',#103645,0.126999999999998);
#32650=CIRCLE('',#103647,0.127000000000001);
#32651=CIRCLE('',#103649,0.127000000000003);
#32652=CIRCLE('',#103650,0.127);
#32653=CIRCLE('',#103651,0.127);
#32654=CIRCLE('',#103653,0.126999999999996);
#32655=CIRCLE('',#103656,0.126999999999998);
#32656=CIRCLE('',#103658,0.126999999999997);
#32657=CIRCLE('',#103660,0.127000000000001);
#32658=CIRCLE('',#103661,0.127);
#32659=CIRCLE('',#103662,0.127);
#32660=CIRCLE('',#103664,0.127);
#32661=CIRCLE('',#103667,0.127000000000001);
#32662=CIRCLE('',#103671,0.126999999999999);
#32663=CIRCLE('',#103672,0.127);
#32664=CIRCLE('',#103674,0.127);
#32665=CIRCLE('',#103676,0.127);
#32666=CIRCLE('',#103677,0.127000000000003);
#32667=CIRCLE('',#103678,0.126999999999998);
#32668=CIRCLE('',#103680,0.126999999999998);
#32669=CIRCLE('',#103683,0.126999999999999);
#32670=CIRCLE('',#103685,0.127);
#32671=CIRCLE('',#103687,0.127000000000003);
#32672=CIRCLE('',#103688,0.126999999999998);
#32673=CIRCLE('',#103689,0.126999999999998);
#32674=CIRCLE('',#103691,0.126999999999998);
#32675=CIRCLE('',#103693,0.126999999999997);
#32676=CIRCLE('',#103694,0.127000000000001);
#32677=CIRCLE('',#103695,0.127);
#32678=CIRCLE('',#103697,0.127);
#32679=CIRCLE('',#103700,0.127000000000001);
#32680=CIRCLE('',#103702,0.127000000000003);
#32681=CIRCLE('',#103704,0.126999999999998);
#32682=CIRCLE('',#103705,0.127);
#32683=CIRCLE('',#103706,0.127);
#32684=CIRCLE('',#103708,0.127);
#32685=CIRCLE('',#103711,0.127000000000004);
#32686=CIRCLE('',#103715,0.127000000000001);
#32687=CIRCLE('',#103716,0.127000000000004);
#32688=CIRCLE('',#103718,0.127000000000004);
#32689=CIRCLE('',#103720,0.127000000000004);
#32690=CIRCLE('',#103721,0.127000000000001);
#32691=CIRCLE('',#103722,0.127);
#32692=CIRCLE('',#103724,0.127);
#32693=CIRCLE('',#103727,0.126999999999995);
#32694=CIRCLE('',#103729,0.127000000000004);
#32695=CIRCLE('',#103731,0.126999999999998);
#32696=CIRCLE('',#103732,0.127);
#32697=CIRCLE('',#103733,0.126999999999997);
#32698=CIRCLE('',#103735,0.126999999999999);
#32699=CIRCLE('',#103737,0.127000000000001);
#32700=CIRCLE('',#103738,0.127);
#32701=CIRCLE('',#103739,0.127000000000004);
#32702=CIRCLE('',#103741,0.127000000000003);
#32703=CIRCLE('',#103744,0.127000000000003);
#32704=CIRCLE('',#103746,0.126999999999998);
#32705=CIRCLE('',#103748,0.126999999999997);
#32706=CIRCLE('',#103749,0.127000000000004);
#32707=CIRCLE('',#103750,0.126999999999999);
#32708=CIRCLE('',#103752,0.127000000000004);
#32709=CIRCLE('',#103755,0.126999999999997);
#32710=CIRCLE('',#103759,0.127000000000001);
#32711=CIRCLE('',#103760,0.127);
#32712=CIRCLE('',#103762,0.127);
#32713=CIRCLE('',#103764,0.127);
#32714=CIRCLE('',#103765,0.126999999999999);
#32715=CIRCLE('',#103766,0.127000000000001);
#32716=CIRCLE('',#103768,0.127);
#32717=CIRCLE('',#103771,0.127000000000002);
#32718=CIRCLE('',#103773,0.127);
#32719=CIRCLE('',#103775,0.127000000000002);
#32720=CIRCLE('',#103776,0.127000000000002);
#32721=CIRCLE('',#103777,0.127);
#32722=CIRCLE('',#103779,0.127000000000001);
#32723=CIRCLE('',#103781,0.127000000000002);
#32724=CIRCLE('',#103782,0.127);
#32725=CIRCLE('',#103783,0.127000000000003);
#32726=CIRCLE('',#103785,0.126999999999999);
#32727=CIRCLE('',#103788,0.127000000000001);
#32728=CIRCLE('',#103790,0.126999999999998);
#32729=CIRCLE('',#103792,0.127000000000002);
#32730=CIRCLE('',#103793,0.127);
#32731=CIRCLE('',#103794,0.127);
#32732=CIRCLE('',#103796,0.127);
#32733=CIRCLE('',#103799,0.127000000000001);
#32734=CIRCLE('',#103803,0.127);
#32735=CIRCLE('',#103804,0.127000000000001);
#32736=CIRCLE('',#103806,0.127000000000001);
#32737=CIRCLE('',#103808,0.127000000000001);
#32738=CIRCLE('',#103809,0.127000000000004);
#32739=CIRCLE('',#103810,0.127000000000004);
#32740=CIRCLE('',#103812,0.126999999999999);
#32741=CIRCLE('',#103815,0.126999999999999);
#32742=CIRCLE('',#103817,0.127000000000001);
#32743=CIRCLE('',#103819,0.127000000000002);
#32744=CIRCLE('',#103820,0.127000000000001);
#32745=CIRCLE('',#103821,0.126999999999999);
#32746=CIRCLE('',#103823,0.127);
#32747=CIRCLE('',#103825,0.127000000000001);
#32748=CIRCLE('',#103826,0.127000000000003);
#32749=CIRCLE('',#103827,0.127000000000001);
#32750=CIRCLE('',#103829,0.127000000000001);
#32751=CIRCLE('',#103832,0.127);
#32752=CIRCLE('',#103834,0.127000000000003);
#32753=CIRCLE('',#103836,0.126999999999998);
#32754=CIRCLE('',#103837,0.127000000000001);
#32755=CIRCLE('',#103838,0.127000000000001);
#32756=CIRCLE('',#103840,0.127000000000001);
#32757=CIRCLE('',#103843,0.127000000000001);
#32758=CIRCLE('',#103847,0.126999999999999);
#32759=CIRCLE('',#103848,0.127);
#32760=CIRCLE('',#103850,0.127);
#32761=CIRCLE('',#103852,0.126999999999999);
#32762=CIRCLE('',#103853,0.126999999999998);
#32763=CIRCLE('',#103854,0.127);
#32764=CIRCLE('',#103856,0.127);
#32765=CIRCLE('',#103859,0.127);
#32766=CIRCLE('',#103861,0.127);
#32767=CIRCLE('',#103863,0.126999999999998);
#32768=CIRCLE('',#103864,0.127000000000001);
#32769=CIRCLE('',#103865,0.126999999999997);
#32770=CIRCLE('',#103867,0.126999999999999);
#32771=CIRCLE('',#103869,0.127000000000002);
#32772=CIRCLE('',#103870,0.126999999999999);
#32773=CIRCLE('',#103871,0.127);
#32774=CIRCLE('',#103873,0.127000000000002);
#32775=CIRCLE('',#103876,0.126999999999999);
#32776=CIRCLE('',#103878,0.127000000000001);
#32777=CIRCLE('',#103880,0.127000000000001);
#32778=CIRCLE('',#103881,0.127);
#32779=CIRCLE('',#103882,0.127);
#32780=CIRCLE('',#103884,0.127);
#32781=CIRCLE('',#103887,0.127);
#32782=CIRCLE('',#103891,0.127000000000001);
#32783=CIRCLE('',#103892,0.126999999999999);
#32784=CIRCLE('',#103894,0.126999999999999);
#32785=CIRCLE('',#103896,0.126999999999999);
#32786=CIRCLE('',#103897,0.127000000000002);
#32787=CIRCLE('',#103898,0.127);
#32788=CIRCLE('',#103900,0.126999999999996);
#32789=CIRCLE('',#103903,0.127000000000003);
#32790=CIRCLE('',#103905,0.126999999999999);
#32791=CIRCLE('',#103907,0.127000000000003);
#32792=CIRCLE('',#103908,0.127);
#32793=CIRCLE('',#103909,0.127000000000002);
#32794=CIRCLE('',#103911,0.127000000000001);
#32795=CIRCLE('',#103913,0.127000000000002);
#32796=CIRCLE('',#103914,0.127);
#32797=CIRCLE('',#103915,0.126999999999999);
#32798=CIRCLE('',#103917,0.127000000000002);
#32799=CIRCLE('',#103920,0.126999999999999);
#32800=CIRCLE('',#103922,0.127000000000001);
#32801=CIRCLE('',#103924,0.127);
#32802=CIRCLE('',#103925,0.126999999999999);
#32803=CIRCLE('',#103926,0.126999999999999);
#32804=CIRCLE('',#103928,0.126999999999999);
#32805=CIRCLE('',#103931,0.127);
#32806=CIRCLE('',#103935,0.126999999999998);
#32807=CIRCLE('',#103936,0.127);
#32808=CIRCLE('',#103938,0.127);
#32809=CIRCLE('',#103940,0.127);
#32810=CIRCLE('',#103941,0.126999999999998);
#32811=CIRCLE('',#103942,0.127);
#32812=CIRCLE('',#103944,0.126999999999999);
#32813=CIRCLE('',#103947,0.127000000000002);
#32814=CIRCLE('',#103949,0.127);
#32815=CIRCLE('',#103951,0.127000000000004);
#32816=CIRCLE('',#103952,0.126999999999998);
#32817=CIRCLE('',#103953,0.126999999999999);
#32818=CIRCLE('',#103955,0.127000000000001);
#32819=CIRCLE('',#103957,0.127);
#32820=CIRCLE('',#103958,0.126999999999997);
#32821=CIRCLE('',#103959,0.127);
#32822=CIRCLE('',#103961,0.127);
#32823=CIRCLE('',#103964,0.127000000000001);
#32824=CIRCLE('',#103966,0.127000000000003);
#32825=CIRCLE('',#103968,0.126999999999998);
#32826=CIRCLE('',#103969,0.127);
#32827=CIRCLE('',#103970,0.127);
#32828=CIRCLE('',#103972,0.127);
#32829=CIRCLE('',#103975,0.126999999999997);
#32830=CIRCLE('',#103979,0.127);
#32831=CIRCLE('',#103980,0.127000000000002);
#32832=CIRCLE('',#103982,0.127000000000002);
#32833=CIRCLE('',#103984,0.127000000000002);
#32834=CIRCLE('',#103985,0.126999999999998);
#32835=CIRCLE('',#103986,0.127000000000001);
#32836=CIRCLE('',#103988,0.127000000000005);
#32837=CIRCLE('',#103992,0.127000000000002);
#32838=CIRCLE('',#103993,0.127000000000001);
#32839=CIRCLE('',#103994,0.127000000000005);
#32840=CIRCLE('',#103996,0.126999999999999);
#32841=CIRCLE('',#103998,0.126999999999998);
#32842=CIRCLE('',#103999,0.127000000000002);
#32843=CIRCLE('',#104002,0.126999999999999);
#32844=CIRCLE('',#104004,0.126999999999997);
#32845=CIRCLE('',#104006,0.127000000000001);
#32846=CIRCLE('',#104007,0.127000000000002);
#32847=CIRCLE('',#104008,0.127000000000002);
#32848=CIRCLE('',#104010,0.127000000000002);
#32849=CIRCLE('',#104013,0.127000000000001);
#32850=CIRCLE('',#104017,0.126999999999998);
#32851=CIRCLE('',#104018,0.127);
#32852=CIRCLE('',#104020,0.127);
#32853=CIRCLE('',#104022,0.127);
#32854=CIRCLE('',#104023,0.126999999999998);
#32855=CIRCLE('',#104024,0.127);
#32856=CIRCLE('',#104026,0.126999999999999);
#32857=CIRCLE('',#104029,0.127000000000004);
#32858=CIRCLE('',#104031,0.127);
#32859=CIRCLE('',#104033,0.127000000000002);
#32860=CIRCLE('',#104034,0.126999999999998);
#32861=CIRCLE('',#104035,0.126999999999999);
#32862=CIRCLE('',#104037,0.127000000000001);
#32863=CIRCLE('',#104039,0.127000000000004);
#32864=CIRCLE('',#104040,0.127);
#32865=CIRCLE('',#104041,0.127);
#32866=CIRCLE('',#104043,0.126999999999997);
#32867=CIRCLE('',#104046,0.127000000000001);
#32868=CIRCLE('',#104048,0.127000000000003);
#32869=CIRCLE('',#104050,0.127000000000004);
#32870=CIRCLE('',#104051,0.127);
#32871=CIRCLE('',#104052,0.127);
#32872=CIRCLE('',#104054,0.127);
#32873=CIRCLE('',#104057,0.126999999999997);
#32874=CIRCLE('',#104061,0.127000000000001);
#32875=CIRCLE('',#104062,0.126999999999999);
#32876=CIRCLE('',#104064,0.126999999999999);
#32877=CIRCLE('',#104066,0.126999999999999);
#32878=CIRCLE('',#104067,0.127000000000002);
#32879=CIRCLE('',#104068,0.127);
#32880=CIRCLE('',#104070,0.126999999999999);
#32881=CIRCLE('',#104073,0.126999999999997);
#32882=CIRCLE('',#104075,0.127000000000001);
#32883=CIRCLE('',#104077,0.126999999999997);
#32884=CIRCLE('',#104078,0.126999999999996);
#32885=CIRCLE('',#104079,0.126999999999999);
#32886=CIRCLE('',#104081,0.127000000000001);
#32887=CIRCLE('',#104083,0.127000000000002);
#32888=CIRCLE('',#104084,0.127000000000002);
#32889=CIRCLE('',#104085,0.126999999999999);
#32890=CIRCLE('',#104087,0.127000000000001);
#32891=CIRCLE('',#104090,0.127000000000001);
#32892=CIRCLE('',#104092,0.127000000000001);
#32893=CIRCLE('',#104094,0.126999999999996);
#32894=CIRCLE('',#104095,0.126999999999999);
#32895=CIRCLE('',#104096,0.126999999999999);
#32896=CIRCLE('',#104098,0.126999999999999);
#32897=CIRCLE('',#104101,0.127);
#32898=CIRCLE('',#104105,0.127000000000001);
#32899=CIRCLE('',#104106,0.126999999999999);
#32900=CIRCLE('',#104108,0.126999999999999);
#32901=CIRCLE('',#104110,0.127);
#32902=CIRCLE('',#104111,0.126999999999998);
#32903=CIRCLE('',#104112,0.126999999999997);
#32904=CIRCLE('',#104114,0.127000000000003);
#32905=CIRCLE('',#104117,0.126999999999998);
#32906=CIRCLE('',#104119,0.126999999999999);
#32907=CIRCLE('',#104121,0.127000000000001);
#32908=CIRCLE('',#104122,0.127000000000001);
#32909=CIRCLE('',#104123,0.126999999999999);
#32910=CIRCLE('',#104125,0.127000000000002);
#32911=CIRCLE('',#104127,0.126999999999998);
#32912=CIRCLE('',#104128,0.126999999999997);
#32913=CIRCLE('',#104129,0.126999999999999);
#32914=CIRCLE('',#104131,0.127);
#32915=CIRCLE('',#104134,0.126999999999999);
#32916=CIRCLE('',#104136,0.126999999999998);
#32917=CIRCLE('',#104138,0.127000000000001);
#32918=CIRCLE('',#104139,0.126999999999999);
#32919=CIRCLE('',#104140,0.126999999999999);
#32920=CIRCLE('',#104142,0.126999999999999);
#32921=CIRCLE('',#104145,0.127);
#32922=CIRCLE('',#104149,0.127);
#32923=CIRCLE('',#104150,0.127000000000001);
#32924=CIRCLE('',#104152,0.127000000000001);
#32925=CIRCLE('',#104154,0.127000000000001);
#32926=CIRCLE('',#104155,0.127000000000001);
#32927=CIRCLE('',#104156,0.127000000000004);
#32928=CIRCLE('',#104158,0.126999999999996);
#32929=CIRCLE('',#104161,0.127000000000002);
#32930=CIRCLE('',#104163,0.127000000000001);
#32931=CIRCLE('',#104165,0.127000000000001);
#32932=CIRCLE('',#104166,0.126999999999998);
#32933=CIRCLE('',#104167,0.126999999999999);
#32934=CIRCLE('',#104169,0.126999999999997);
#32935=CIRCLE('',#104171,0.127000000000001);
#32936=CIRCLE('',#104172,0.127000000000001);
#32937=CIRCLE('',#104173,0.127000000000001);
#32938=CIRCLE('',#104175,0.126999999999998);
#32939=CIRCLE('',#104178,0.127);
#32940=CIRCLE('',#104180,0.127000000000003);
#32941=CIRCLE('',#104182,0.127000000000004);
#32942=CIRCLE('',#104183,0.127000000000001);
#32943=CIRCLE('',#104184,0.127000000000001);
#32944=CIRCLE('',#104186,0.127000000000001);
#32945=CIRCLE('',#104189,0.127000000000001);
#32946=CIRCLE('',#104193,0.127000000000001);
#32947=CIRCLE('',#104194,0.127);
#32948=CIRCLE('',#104196,0.127000000000003);
#32949=CIRCLE('',#104198,0.127);
#32950=CIRCLE('',#104199,0.126999999999999);
#32951=CIRCLE('',#104200,0.126999999999998);
#32952=CIRCLE('',#104202,0.127);
#32953=CIRCLE('',#104205,0.126999999999998);
#32954=CIRCLE('',#104207,0.127);
#32955=CIRCLE('',#104209,0.126999999999996);
#32956=CIRCLE('',#104210,0.127000000000002);
#32957=CIRCLE('',#104211,0.126999999999996);
#32958=CIRCLE('',#104213,0.127000000000001);
#32959=CIRCLE('',#104215,0.127000000000002);
#32960=CIRCLE('',#104216,0.126999999999999);
#32961=CIRCLE('',#104217,0.127);
#32962=CIRCLE('',#104219,0.127000000000001);
#32963=CIRCLE('',#104222,0.126999999999998);
#32964=CIRCLE('',#104224,0.127000000000001);
#32965=CIRCLE('',#104226,0.126999999999999);
#32966=CIRCLE('',#104227,0.127);
#32967=CIRCLE('',#104228,0.127);
#32968=CIRCLE('',#104230,0.127);
#32969=CIRCLE('',#104233,0.126999999999998);
#32970=CIRCLE('',#104237,0.127000000000004);
#32971=CIRCLE('',#104238,0.126999999999999);
#32972=CIRCLE('',#104240,0.126999999999999);
#32973=CIRCLE('',#104242,0.127000000000004);
#32974=CIRCLE('',#104243,0.126999999999998);
#32975=CIRCLE('',#104244,0.126999999999997);
#32976=CIRCLE('',#104246,0.127);
#32977=CIRCLE('',#104249,0.126999999999998);
#32978=CIRCLE('',#104251,0.127000000000004);
#32979=CIRCLE('',#104253,0.127);
#32980=CIRCLE('',#104254,0.126999999999997);
#32981=CIRCLE('',#104255,0.126999999999997);
#32982=CIRCLE('',#104257,0.127000000000003);
#32983=CIRCLE('',#104259,0.126999999999998);
#32984=CIRCLE('',#104260,0.127000000000003);
#32985=CIRCLE('',#104261,0.126999999999999);
#32986=CIRCLE('',#104263,0.127);
#32987=CIRCLE('',#104266,0.126999999999999);
#32988=CIRCLE('',#104268,0.127000000000004);
#32989=CIRCLE('',#104270,0.127);
#32990=CIRCLE('',#104271,0.126999999999999);
#32991=CIRCLE('',#104272,0.126999999999999);
#32992=CIRCLE('',#104274,0.126999999999999);
#32993=CIRCLE('',#104277,0.126999999999997);
#32994=CIRCLE('',#104281,0.126999999999999);
#32995=CIRCLE('',#104282,0.127);
#32996=CIRCLE('',#104284,0.127);
#32997=CIRCLE('',#104286,0.127);
#32998=CIRCLE('',#104287,0.127000000000003);
#32999=CIRCLE('',#104288,0.127000000000001);
#33000=CIRCLE('',#104290,0.126999999999998);
#33001=CIRCLE('',#104293,0.126999999999998);
#33002=CIRCLE('',#104295,0.127);
#33003=CIRCLE('',#104297,0.126999999999998);
#33004=CIRCLE('',#104298,0.127000000000001);
#33005=CIRCLE('',#104299,0.126999999999998);
#33006=CIRCLE('',#104301,0.127000000000001);
#33007=CIRCLE('',#104303,0.127);
#33008=CIRCLE('',#104304,0.127);
#33009=CIRCLE('',#104305,0.127);
#33010=CIRCLE('',#104307,0.126999999999996);
#33011=CIRCLE('',#104310,0.126999999999998);
#33012=CIRCLE('',#104312,0.127000000000002);
#33013=CIRCLE('',#104314,0.127000000000001);
#33014=CIRCLE('',#104315,0.127);
#33015=CIRCLE('',#104316,0.127);
#33016=CIRCLE('',#104318,0.127);
#33017=CIRCLE('',#104321,0.127000000000001);
#33018=CIRCLE('',#104325,0.126999999999999);
#33019=CIRCLE('',#104326,0.127);
#33020=CIRCLE('',#104328,0.127);
#33021=CIRCLE('',#104330,0.127);
#33022=CIRCLE('',#104331,0.127000000000003);
#33023=CIRCLE('',#104332,0.127000000000001);
#33024=CIRCLE('',#104334,0.126999999999998);
#33025=CIRCLE('',#104337,0.126999999999999);
#33026=CIRCLE('',#104339,0.127);
#33027=CIRCLE('',#104341,0.127000000000003);
#33028=CIRCLE('',#104342,0.126999999999998);
#33029=CIRCLE('',#104343,0.126999999999998);
#33030=CIRCLE('',#104345,0.126999999999998);
#33031=CIRCLE('',#104347,0.127);
#33032=CIRCLE('',#104348,0.127000000000001);
#33033=CIRCLE('',#104349,0.127);
#33034=CIRCLE('',#104351,0.127);
#33035=CIRCLE('',#104354,0.127000000000001);
#33036=CIRCLE('',#104356,0.126999999999997);
#33037=CIRCLE('',#104358,0.126999999999998);
#33038=CIRCLE('',#104359,0.127);
#33039=CIRCLE('',#104360,0.127);
#33040=CIRCLE('',#104362,0.127);
#33041=CIRCLE('',#104365,0.127000000000001);
#33042=CIRCLE('',#104369,0.127000000000001);
#33043=CIRCLE('',#104370,0.127000000000004);
#33044=CIRCLE('',#104372,0.127000000000004);
#33045=CIRCLE('',#104374,0.127000000000004);
#33046=CIRCLE('',#104375,0.126999999999998);
#33047=CIRCLE('',#104376,0.126999999999997);
#33048=CIRCLE('',#104378,0.127);
#33049=CIRCLE('',#104381,0.127000000000001);
#33050=CIRCLE('',#104383,0.127000000000004);
#33051=CIRCLE('',#104385,0.126999999999998);
#33052=CIRCLE('',#104386,0.126999999999997);
#33053=CIRCLE('',#104387,0.127);
#33054=CIRCLE('',#104389,0.126999999999999);
#33055=CIRCLE('',#104391,0.127000000000001);
#33056=CIRCLE('',#104392,0.126999999999996);
#33057=CIRCLE('',#104393,0.127000000000004);
#33058=CIRCLE('',#104395,0.127000000000003);
#33059=CIRCLE('',#104398,0.126999999999999);
#33060=CIRCLE('',#104400,0.127000000000001);
#33061=CIRCLE('',#104402,0.127000000000001);
#33062=CIRCLE('',#104403,0.127000000000004);
#33063=CIRCLE('',#104404,0.127);
#33064=CIRCLE('',#104406,0.127000000000004);
#33065=CIRCLE('',#104409,0.126999999999997);
#33066=CIRCLE('',#104413,0.127000000000001);
#33067=CIRCLE('',#104414,0.127);
#33068=CIRCLE('',#104416,0.127);
#33069=CIRCLE('',#104418,0.126999999999999);
#33070=CIRCLE('',#104419,0.126999999999999);
#33071=CIRCLE('',#104420,0.126999999999998);
#33072=CIRCLE('',#104422,0.127);
#33073=CIRCLE('',#104425,0.127000000000002);
#33074=CIRCLE('',#104427,0.127);
#33075=CIRCLE('',#104429,0.127000000000002);
#33076=CIRCLE('',#104430,0.127000000000002);
#33077=CIRCLE('',#104431,0.127);
#33078=CIRCLE('',#104433,0.126999999999998);
#33079=CIRCLE('',#104435,0.126999999999999);
#33080=CIRCLE('',#104436,0.127);
#33081=CIRCLE('',#104437,0.127000000000003);
#33082=CIRCLE('',#104439,0.126999999999998);
#33083=CIRCLE('',#104442,0.127000000000001);
#33084=CIRCLE('',#104444,0.127000000000001);
#33085=CIRCLE('',#104446,0.127000000000002);
#33086=CIRCLE('',#104447,0.127);
#33087=CIRCLE('',#104448,0.127);
#33088=CIRCLE('',#104450,0.127);
#33089=CIRCLE('',#104453,0.127000000000001);
#33090=CIRCLE('',#104457,0.127);
#33091=CIRCLE('',#104458,0.127000000000001);
#33092=CIRCLE('',#104460,0.127000000000001);
#33093=CIRCLE('',#104462,0.127000000000001);
#33094=CIRCLE('',#104463,0.127000000000001);
#33095=CIRCLE('',#104464,0.127000000000004);
#33096=CIRCLE('',#104466,0.126999999999999);
#33097=CIRCLE('',#104469,0.127000000000001);
#33098=CIRCLE('',#104471,0.126999999999998);
#33099=CIRCLE('',#104473,0.127000000000001);
#33100=CIRCLE('',#104474,0.127000000000001);
#33101=CIRCLE('',#104475,0.127);
#33102=CIRCLE('',#104477,0.126999999999997);
#33103=CIRCLE('',#104479,0.126999999999997);
#33104=CIRCLE('',#104480,0.127000000000003);
#33105=CIRCLE('',#104481,0.127000000000001);
#33106=CIRCLE('',#104483,0.127000000000001);
#33107=CIRCLE('',#104486,0.127);
#33108=CIRCLE('',#104488,0.127);
#33109=CIRCLE('',#104490,0.126999999999998);
#33110=CIRCLE('',#104491,0.127000000000001);
#33111=CIRCLE('',#104492,0.127000000000001);
#33112=CIRCLE('',#104494,0.127000000000001);
#33113=CIRCLE('',#104497,0.127000000000001);
#33114=CIRCLE('',#104501,0.127000000000001);
#33115=CIRCLE('',#104502,0.127);
#33116=CIRCLE('',#104504,0.127);
#33117=CIRCLE('',#104506,0.127);
#33118=CIRCLE('',#104507,0.127000000000002);
#33119=CIRCLE('',#104508,0.126999999999997);
#33120=CIRCLE('',#104510,0.127);
#33121=CIRCLE('',#104513,0.127);
#33122=CIRCLE('',#104515,0.127);
#33123=CIRCLE('',#104517,0.126999999999998);
#33124=CIRCLE('',#104518,0.127000000000001);
#33125=CIRCLE('',#104519,0.126999999999997);
#33126=CIRCLE('',#104521,0.126999999999999);
#33127=CIRCLE('',#104523,0.126999999999998);
#33128=CIRCLE('',#104524,0.126999999999999);
#33129=CIRCLE('',#104525,0.127);
#33130=CIRCLE('',#104527,0.127000000000002);
#33131=CIRCLE('',#104530,0.126999999999999);
#33132=CIRCLE('',#104532,0.127000000000001);
#33133=CIRCLE('',#104534,0.127000000000001);
#33134=CIRCLE('',#104535,0.127);
#33135=CIRCLE('',#104536,0.127);
#33136=CIRCLE('',#104538,0.127);
#33137=CIRCLE('',#104541,0.127000000000003);
#33138=CIRCLE('',#104545,0.127000000000001);
#33139=CIRCLE('',#104546,0.126999999999999);
#33140=CIRCLE('',#104548,0.126999999999999);
#33141=CIRCLE('',#104550,0.126999999999999);
#33142=CIRCLE('',#104551,0.127000000000002);
#33143=CIRCLE('',#104552,0.127000000000003);
#33144=CIRCLE('',#104554,0.127000000000002);
#33145=CIRCLE('',#104557,0.127000000000003);
#33146=CIRCLE('',#104559,0.126999999999999);
#33147=CIRCLE('',#104561,0.126999999999996);
#33148=CIRCLE('',#104562,0.127000000000002);
#33149=CIRCLE('',#104563,0.126999999999999);
#33150=CIRCLE('',#104565,0.127000000000001);
#33151=CIRCLE('',#104567,0.127000000000002);
#33152=CIRCLE('',#104568,0.127);
#33153=CIRCLE('',#104569,0.126999999999999);
#33154=CIRCLE('',#104571,0.127000000000002);
#33155=CIRCLE('',#104574,0.127000000000001);
#33156=CIRCLE('',#104576,0.126999999999997);
#33157=CIRCLE('',#104578,0.127);
#33158=CIRCLE('',#104579,0.126999999999999);
#33159=CIRCLE('',#104580,0.126999999999999);
#33160=CIRCLE('',#104582,0.126999999999999);
#33161=CIRCLE('',#104585,0.127);
#33162=CIRCLE('',#104589,0.126999999999998);
#33163=CIRCLE('',#104590,0.127);
#33164=CIRCLE('',#104592,0.127);
#33165=CIRCLE('',#104594,0.127);
#33166=CIRCLE('',#104595,0.126999999999998);
#33167=CIRCLE('',#104596,0.127);
#33168=CIRCLE('',#104598,0.126999999999999);
#33169=CIRCLE('',#104601,0.127000000000002);
#33170=CIRCLE('',#104603,0.127);
#33171=CIRCLE('',#104605,0.127000000000004);
#33172=CIRCLE('',#104606,0.126999999999998);
#33173=CIRCLE('',#104607,0.127);
#33174=CIRCLE('',#104609,0.127000000000001);
#33175=CIRCLE('',#104611,0.126999999999998);
#33176=CIRCLE('',#104612,0.126999999999997);
#33177=CIRCLE('',#104613,0.127);
#33178=CIRCLE('',#104615,0.127);
#33179=CIRCLE('',#104618,0.127000000000001);
#33180=CIRCLE('',#104620,0.126999999999999);
#33181=CIRCLE('',#104622,0.126999999999998);
#33182=CIRCLE('',#104623,0.127);
#33183=CIRCLE('',#104624,0.127);
#33184=CIRCLE('',#104626,0.127);
#33185=CIRCLE('',#104629,0.127);
#33186=CIRCLE('',#104632,59.0285554514622);
#33187=CIRCLE('',#104633,0.127000000000002);
#33188=CIRCLE('',#104634,58.9208533432504);
#33189=CIRCLE('',#104635,0.127000000000002);
#33190=CIRCLE('',#104637,62.9541466567496);
#33191=CIRCLE('',#104638,0.127000000000002);
#33192=CIRCLE('',#104639,62.8464445485378);
#33193=CIRCLE('',#104640,0.127000000000002);
#33194=CIRCLE('',#104642,59.0285554514622);
#33195=CIRCLE('',#104643,0.127000000000002);
#33196=CIRCLE('',#104644,58.9208533432504);
#33197=CIRCLE('',#104645,0.127000000000002);
#33198=CIRCLE('',#104647,62.9541466567496);
#33199=CIRCLE('',#104648,0.127000000000002);
#33200=CIRCLE('',#104649,62.8464445485378);
#33201=CIRCLE('',#104650,0.127000000000002);
#33202=CIRCLE('',#104651,62.9541466567496);
#33203=CIRCLE('',#104653,58.2189663438286);
#33204=CIRCLE('',#104654,0.635);
#33205=CIRCLE('',#104655,57.6804558027693);
#33206=CIRCLE('',#104656,57.6804558027693);
#33207=CIRCLE('',#104658,58.8470884664677);
#33208=CIRCLE('',#104659,0.635);
#33209=CIRCLE('',#104660,58.3085779254084);
#33210=CIRCLE('',#104662,63.5664220745916);
#33211=CIRCLE('',#104663,0.635);
#33212=CIRCLE('',#104664,63.0279115335323);
#33213=CIRCLE('',#104665,63.0279115335323);
#33214=CIRCLE('',#104667,64.1945441972308);
#33215=CIRCLE('',#104668,0.635);
#33216=CIRCLE('',#104669,63.6560336561714);
#33217=CIRCLE('',#104671,65.);
#33218=CIRCLE('',#104672,65.);
#33219=CIRCLE('',#104675,62.9541466567496);
#33220=CIRCLE('',#104676,62.4089800241499);
#33221=CIRCLE('',#104677,62.9541466567496);
#33222=CIRCLE('',#104678,62.4089800241499);
#33223=CIRCLE('',#104679,62.9541466567496);
#33224=CIRCLE('',#104680,62.4089800241499);
#33225=CIRCLE('',#104681,62.9541466567497);
#33226=CIRCLE('',#104682,62.4089800241499);
#33227=CIRCLE('',#104683,62.9541466567496);
#33228=CIRCLE('',#104684,62.4089800241499);
#33229=CIRCLE('',#104685,62.9541466567496);
#33230=CIRCLE('',#104686,62.4089800241499);
#33231=CIRCLE('',#104687,62.9541466567497);
#33232=CIRCLE('',#104688,62.4089800241499);
#33233=CIRCLE('',#104689,62.9541466567497);
#33234=CIRCLE('',#104690,62.4089800241499);
#33235=CIRCLE('',#104691,62.9541466567496);
#33236=CIRCLE('',#104692,62.4089800241499);
#33237=CIRCLE('',#104693,62.9541466567497);
#33238=CIRCLE('',#104694,62.4089800241499);
#33239=CIRCLE('',#104695,62.9541466567496);
#33240=CIRCLE('',#104696,62.4089800241499);
#33241=CIRCLE('',#104697,62.9541466567497);
#33242=CIRCLE('',#104698,62.4089800241499);
#33243=CIRCLE('',#104699,62.9541466567497);
#33244=CIRCLE('',#104700,62.4089800241499);
#33245=CIRCLE('',#104701,62.9541466567496);
#33246=CIRCLE('',#104702,62.4089800241499);
#33247=CIRCLE('',#104703,62.9541466567497);
#33248=CIRCLE('',#104704,62.4089800241499);
#33249=CIRCLE('',#104705,62.9541466567496);
#33250=CIRCLE('',#104706,62.4089800241499);
#33251=CIRCLE('',#104707,62.9541466567497);
#33252=CIRCLE('',#104708,62.4089800241499);
#33253=CIRCLE('',#104709,62.9541466567497);
#33254=CIRCLE('',#104710,62.4089800241499);
#33255=CIRCLE('',#104711,62.9541466567496);
#33256=CIRCLE('',#104712,62.4089800241499);
#33257=CIRCLE('',#104713,62.9541466567496);
#33258=CIRCLE('',#104714,62.4089800241499);
#33259=CIRCLE('',#104715,62.9541466567496);
#33260=CIRCLE('',#104716,62.4089800241499);
#33261=CIRCLE('',#104717,62.9541466567496);
#33262=CIRCLE('',#104718,62.4089800241499);
#33263=CIRCLE('',#104719,62.9541466567497);
#33264=CIRCLE('',#104720,62.4089800241499);
#33265=CIRCLE('',#104721,62.9541466567497);
#33266=CIRCLE('',#104722,62.4089800241499);
#33267=CIRCLE('',#104723,62.9541466567496);
#33268=CIRCLE('',#104724,62.4089800241499);
#33269=CIRCLE('',#104725,62.9541466567496);
#33270=CIRCLE('',#104726,62.4089800241499);
#33271=CIRCLE('',#104727,62.9541466567496);
#33272=CIRCLE('',#104728,62.4089800241499);
#33273=CIRCLE('',#104729,62.9541466567497);
#33274=CIRCLE('',#104730,62.4089800241499);
#33275=CIRCLE('',#104731,62.9541466567496);
#33276=CIRCLE('',#104732,62.4089800241499);
#33277=CIRCLE('',#104733,62.9541466567497);
#33278=CIRCLE('',#104734,62.4089800241499);
#33279=CIRCLE('',#104735,62.4089800241499);
#33280=CIRCLE('',#104736,62.9541466567497);
#33281=CIRCLE('',#104737,62.4089800241499);
#33282=CIRCLE('',#104738,62.9541466567496);
#33283=CIRCLE('',#104739,62.4089800241499);
#33284=CIRCLE('',#104740,62.9541466567496);
#33285=CIRCLE('',#104741,62.4089800241499);
#33286=CIRCLE('',#104742,62.9541466567496);
#33287=CIRCLE('',#104743,62.4089800241499);
#33288=CIRCLE('',#104744,62.9541466567497);
#33289=CIRCLE('',#104745,62.4089800241499);
#33290=CIRCLE('',#104746,62.9541466567496);
#33291=CIRCLE('',#104747,62.4089800241499);
#33292=CIRCLE('',#104748,62.9541466567497);
#33293=CIRCLE('',#104749,62.4089800241499);
#33294=CIRCLE('',#104750,62.9541466567497);
#33295=CIRCLE('',#104751,62.4089800241499);
#33296=CIRCLE('',#104752,62.9541466567497);
#33297=CIRCLE('',#104753,62.4089800241499);
#33298=CIRCLE('',#104754,62.9541466567496);
#33299=CIRCLE('',#104755,62.4089800241499);
#33300=CIRCLE('',#104756,62.9541466567496);
#33301=CIRCLE('',#104757,62.4089800241499);
#33302=CIRCLE('',#104758,62.9541466567496);
#33303=CIRCLE('',#104759,62.4089800241499);
#33304=CIRCLE('',#104760,62.9541466567497);
#33305=CIRCLE('',#104761,62.4089800241499);
#33306=CIRCLE('',#104762,62.9541466567496);
#33307=CIRCLE('',#104763,62.4089800241499);
#33308=CIRCLE('',#104764,62.4089800241499);
#33309=CIRCLE('',#104765,62.9541466567497);
#33310=CIRCLE('',#104766,62.4089800241499);
#33311=CIRCLE('',#104767,62.9541466567497);
#33312=CIRCLE('',#104768,62.4089800241499);
#33313=CIRCLE('',#104769,62.9541466567497);
#33314=CIRCLE('',#104770,62.4089800241499);
#33315=CIRCLE('',#104771,62.9541466567497);
#33316=CIRCLE('',#104772,62.4089800241499);
#33317=CIRCLE('',#104773,62.9541466567497);
#33318=CIRCLE('',#104774,62.4089800241499);
#33319=CIRCLE('',#104775,62.9541466567496);
#33320=CIRCLE('',#104776,62.4089800241499);
#33321=CIRCLE('',#104777,62.9541466567496);
#33322=CIRCLE('',#104778,62.4089800241499);
#33323=CIRCLE('',#104779,62.9541466567496);
#33324=CIRCLE('',#104780,62.4089800241499);
#33325=CIRCLE('',#104781,62.9541466567497);
#33326=CIRCLE('',#104782,62.4089800241499);
#33327=CIRCLE('',#104783,62.9541466567496);
#33328=CIRCLE('',#104784,62.4089800241499);
#33329=CIRCLE('',#104785,62.9541466567497);
#33330=CIRCLE('',#104786,62.4089800241499);
#33331=CIRCLE('',#104787,62.9541466567497);
#33332=CIRCLE('',#104788,62.4089800241499);
#33333=CIRCLE('',#104789,62.9541466567497);
#33334=CIRCLE('',#104790,62.4089800241499);
#33335=CIRCLE('',#104791,62.9541466567497);
#33336=CIRCLE('',#104792,62.4089800241499);
#33337=CIRCLE('',#104794,59.4660199758502);
#33338=CIRCLE('',#104795,58.9208533432504);
#33339=CIRCLE('',#104796,59.4660199758502);
#33340=CIRCLE('',#104797,58.9208533432504);
#33341=CIRCLE('',#104798,59.4660199758502);
#33342=CIRCLE('',#104799,58.9208533432504);
#33343=CIRCLE('',#104800,59.4660199758502);
#33344=CIRCLE('',#104801,58.9208533432504);
#33345=CIRCLE('',#104802,59.4660199758502);
#33346=CIRCLE('',#104803,58.9208533432504);
#33347=CIRCLE('',#104804,59.4660199758502);
#33348=CIRCLE('',#104805,58.9208533432504);
#33349=CIRCLE('',#104806,59.4660199758502);
#33350=CIRCLE('',#104807,58.9208533432504);
#33351=CIRCLE('',#104808,59.4660199758502);
#33352=CIRCLE('',#104809,58.9208533432504);
#33353=CIRCLE('',#104810,59.4660199758502);
#33354=CIRCLE('',#104811,58.9208533432504);
#33355=CIRCLE('',#104812,59.4660199758502);
#33356=CIRCLE('',#104813,58.9208533432504);
#33357=CIRCLE('',#104814,59.4660199758502);
#33358=CIRCLE('',#104815,58.9208533432504);
#33359=CIRCLE('',#104816,59.4660199758502);
#33360=CIRCLE('',#104817,58.9208533432504);
#33361=CIRCLE('',#104818,59.4660199758502);
#33362=CIRCLE('',#104819,58.9208533432504);
#33363=CIRCLE('',#104820,59.4660199758502);
#33364=CIRCLE('',#104821,58.9208533432504);
#33365=CIRCLE('',#104822,59.4660199758502);
#33366=CIRCLE('',#104823,58.9208533432504);
#33367=CIRCLE('',#104824,59.4660199758502);
#33368=CIRCLE('',#104825,58.9208533432504);
#33369=CIRCLE('',#104826,59.4660199758502);
#33370=CIRCLE('',#104827,58.9208533432504);
#33371=CIRCLE('',#104828,59.4660199758502);
#33372=CIRCLE('',#104829,58.9208533432504);
#33373=CIRCLE('',#104830,59.4660199758502);
#33374=CIRCLE('',#104831,58.9208533432504);
#33375=CIRCLE('',#104832,59.4660199758502);
#33376=CIRCLE('',#104833,58.9208533432504);
#33377=CIRCLE('',#104834,59.4660199758502);
#33378=CIRCLE('',#104835,58.9208533432504);
#33379=CIRCLE('',#104836,59.4660199758502);
#33380=CIRCLE('',#104837,58.9208533432504);
#33381=CIRCLE('',#104838,59.4660199758502);
#33382=CIRCLE('',#104839,58.9208533432504);
#33383=CIRCLE('',#104840,59.4660199758502);
#33384=CIRCLE('',#104841,58.9208533432504);
#33385=CIRCLE('',#104842,59.4660199758502);
#33386=CIRCLE('',#104843,58.9208533432504);
#33387=CIRCLE('',#104844,59.4660199758502);
#33388=CIRCLE('',#104845,58.9208533432504);
#33389=CIRCLE('',#104846,59.4660199758502);
#33390=CIRCLE('',#104847,58.9208533432504);
#33391=CIRCLE('',#104848,59.4660199758502);
#33392=CIRCLE('',#104849,58.9208533432504);
#33393=CIRCLE('',#104850,59.4660199758502);
#33394=CIRCLE('',#104851,58.9208533432504);
#33395=CIRCLE('',#104852,59.4660199758502);
#33396=CIRCLE('',#104853,58.9208533432504);
#33397=CIRCLE('',#104854,58.9208533432504);
#33398=CIRCLE('',#104855,59.4660199758502);
#33399=CIRCLE('',#104856,58.9208533432504);
#33400=CIRCLE('',#104857,59.4660199758502);
#33401=CIRCLE('',#104858,58.9208533432504);
#33402=CIRCLE('',#104859,59.4660199758502);
#33403=CIRCLE('',#104860,58.9208533432504);
#33404=CIRCLE('',#104861,59.4660199758502);
#33405=CIRCLE('',#104862,58.9208533432504);
#33406=CIRCLE('',#104863,59.4660199758502);
#33407=CIRCLE('',#104864,58.9208533432504);
#33408=CIRCLE('',#104865,59.4660199758502);
#33409=CIRCLE('',#104866,58.9208533432504);
#33410=CIRCLE('',#104867,59.4660199758502);
#33411=CIRCLE('',#104868,58.9208533432504);
#33412=CIRCLE('',#104869,59.4660199758502);
#33413=CIRCLE('',#104870,58.9208533432504);
#33414=CIRCLE('',#104871,59.4660199758502);
#33415=CIRCLE('',#104872,58.9208533432504);
#33416=CIRCLE('',#104873,59.4660199758502);
#33417=CIRCLE('',#104874,58.9208533432504);
#33418=CIRCLE('',#104875,59.4660199758502);
#33419=CIRCLE('',#104876,58.9208533432504);
#33420=CIRCLE('',#104877,59.4660199758502);
#33421=CIRCLE('',#104878,58.9208533432504);
#33422=CIRCLE('',#104879,59.4660199758502);
#33423=CIRCLE('',#104880,58.9208533432504);
#33424=CIRCLE('',#104881,59.4660199758502);
#33425=CIRCLE('',#104882,58.9208533432504);
#33426=CIRCLE('',#104883,59.4660199758502);
#33427=CIRCLE('',#104884,59.4660199758502);
#33428=CIRCLE('',#104885,58.9208533432504);
#33429=CIRCLE('',#104886,59.4660199758502);
#33430=CIRCLE('',#104887,58.9208533432504);
#33431=CIRCLE('',#104888,59.4660199758502);
#33432=CIRCLE('',#104889,58.9208533432504);
#33433=CIRCLE('',#104890,59.4660199758502);
#33434=CIRCLE('',#104891,58.9208533432504);
#33435=CIRCLE('',#104892,59.4660199758502);
#33436=CIRCLE('',#104893,58.9208533432504);
#33437=CIRCLE('',#104894,59.4660199758502);
#33438=CIRCLE('',#104895,58.9208533432504);
#33439=CIRCLE('',#104896,59.4660199758502);
#33440=CIRCLE('',#104897,58.9208533432504);
#33441=CIRCLE('',#104898,59.4660199758502);
#33442=CIRCLE('',#104899,58.9208533432504);
#33443=CIRCLE('',#104900,59.4660199758502);
#33444=CIRCLE('',#104901,58.9208533432504);
#33445=CIRCLE('',#104902,59.4660199758502);
#33446=CIRCLE('',#104903,58.9208533432504);
#33447=CIRCLE('',#104904,59.4660199758502);
#33448=CIRCLE('',#104905,58.9208533432504);
#33449=CIRCLE('',#104906,59.4660199758502);
#33450=CIRCLE('',#104907,58.9208533432504);
#33451=CIRCLE('',#104908,59.4660199758502);
#33452=CIRCLE('',#104909,58.9208533432504);
#33453=CIRCLE('',#104910,59.4660199758502);
#33454=CIRCLE('',#104911,58.9208533432504);
#33455=CIRCLE('',#104912,59.4660199758502);
#33456=CIRCLE('',#104914,56.875);
#33457=CIRCLE('',#104915,56.875);
#33458=CIRCLE('',#104917,56.875);
#33459=CIRCLE('',#104919,60.4792282238308);
#33460=CIRCLE('',#104920,60.0045305169095);
#33461=CIRCLE('',#104921,60.4792282238308);
#33462=CIRCLE('',#104922,60.4792282238308);
#33463=CIRCLE('',#104924,60.6419265158129);
#33464=CIRCLE('',#104926,61.0131030316259);
#33465=CIRCLE('',#104927,60.8618969683742);
#33466=CIRCLE('',#104929,61.3957717761693);
#33467=CIRCLE('',#104930,61.2330734841871);
#33468=CIRCLE('',#104931,61.3957717761693);
#33469=CIRCLE('',#104932,61.3957717761693);
#33470=CIRCLE('',#104934,61.8704694830905);
#33471=CIRCLE('',#104936,0.635007073208622);
#33472=CIRCLE('',#104937,0.635007073208628);
#33473=CIRCLE('',#104948,60.0045305169095);
#33474=CIRCLE('',#104949,60.4792282238308);
#33475=CIRCLE('',#104950,60.4792282238308);
#33476=CIRCLE('',#104951,60.4792282238308);
#33477=CIRCLE('',#104953,60.6419265158129);
#33478=CIRCLE('',#104955,60.8618969683742);
#33479=CIRCLE('',#104956,61.0131030316259);
#33480=CIRCLE('',#104958,61.2330734841871);
#33481=CIRCLE('',#104959,61.3957717761693);
#33482=CIRCLE('',#104960,61.3957717761693);
#33483=CIRCLE('',#104961,61.3957717761693);
#33484=CIRCLE('',#104963,61.8704694830905);
#33485=CIRCLE('',#104965,0.635007073208604);
#33486=CIRCLE('',#104966,0.635007073208616);
#33487=CIRCLE('',#104977,60.0045305169095);
#33488=CIRCLE('',#104978,60.4792282238308);
#33489=CIRCLE('',#104979,60.4792282238308);
#33490=CIRCLE('',#104980,60.4792282238308);
#33491=CIRCLE('',#104982,60.6419265158129);
#33492=CIRCLE('',#104984,60.8618969683742);
#33493=CIRCLE('',#104985,61.0131030316259);
#33494=CIRCLE('',#104987,61.2330734841871);
#33495=CIRCLE('',#104988,61.3957717761693);
#33496=CIRCLE('',#104989,61.3957717761693);
#33497=CIRCLE('',#104990,61.3957717761693);
#33498=CIRCLE('',#104992,61.8704694830905);
#33499=CIRCLE('',#104994,0.635007073208621);
#33500=CIRCLE('',#104995,0.635007073208653);
#33501=CIRCLE('',#105006,60.0045305169095);
#33502=CIRCLE('',#105007,60.4792282238308);
#33503=CIRCLE('',#105008,60.4792282238308);
#33504=CIRCLE('',#105009,60.4792282238308);
#33505=CIRCLE('',#105011,60.6419265158129);
#33506=CIRCLE('',#105013,60.8618969683742);
#33507=CIRCLE('',#105014,61.0131030316259);
#33508=CIRCLE('',#105016,61.2330734841871);
#33509=CIRCLE('',#105017,61.3957717761693);
#33510=CIRCLE('',#105018,61.3957717761693);
#33511=CIRCLE('',#105019,61.3957717761693);
#33512=CIRCLE('',#105021,61.8704694830905);
#33513=CIRCLE('',#105023,0.635007073208651);
#33514=CIRCLE('',#105024,0.63500707320859);
#33515=CIRCLE('',#105035,60.0045305169095);
#33516=CIRCLE('',#105036,60.4792282238308);
#33517=CIRCLE('',#105037,60.4792282238308);
#33518=CIRCLE('',#105038,60.4792282238308);
#33519=CIRCLE('',#105040,60.6419265158129);
#33520=CIRCLE('',#105042,60.8618969683742);
#33521=CIRCLE('',#105043,61.0131030316259);
#33522=CIRCLE('',#105045,61.2330734841871);
#33523=CIRCLE('',#105046,61.3957717761693);
#33524=CIRCLE('',#105047,61.3957717761693);
#33525=CIRCLE('',#105048,61.3957717761693);
#33526=CIRCLE('',#105050,61.8704694830905);
#33527=CIRCLE('',#105052,0.63500707320864);
#33528=CIRCLE('',#105053,0.635007073208627);
#33529=CIRCLE('',#105064,60.0045305169095);
#33530=CIRCLE('',#105065,60.4792282238308);
#33531=CIRCLE('',#105066,60.4792282238308);
#33532=CIRCLE('',#105067,60.4792282238308);
#33533=CIRCLE('',#105069,60.6419265158129);
#33534=CIRCLE('',#105071,60.8618969683742);
#33535=CIRCLE('',#105072,61.0131030316259);
#33536=CIRCLE('',#105074,61.2330734841871);
#33537=CIRCLE('',#105075,61.3957717761693);
#33538=CIRCLE('',#105076,61.3957717761693);
#33539=CIRCLE('',#105077,61.3957717761693);
#33540=CIRCLE('',#105079,61.8704694830905);
#33541=CIRCLE('',#105081,0.635007073208625);
#33542=CIRCLE('',#105082,0.635007073208636);
#33543=CIRCLE('',#105093,60.0045305169095);
#33544=CIRCLE('',#105094,60.4792282238308);
#33545=CIRCLE('',#105095,60.4792282238308);
#33546=CIRCLE('',#105096,60.4792282238308);
#33547=CIRCLE('',#105098,60.6419265158129);
#33548=CIRCLE('',#105100,60.8618969683742);
#33549=CIRCLE('',#105101,61.0131030316259);
#33550=CIRCLE('',#105103,61.2330734841871);
#33551=CIRCLE('',#105104,61.3957717761693);
#33552=CIRCLE('',#105105,61.3957717761693);
#33553=CIRCLE('',#105106,61.3957717761693);
#33554=CIRCLE('',#105108,61.8704694830905);
#33555=CIRCLE('',#105110,0.635007073208613);
#33556=CIRCLE('',#105111,0.635007073208626);
#33557=CIRCLE('',#105122,60.0045305169095);
#33558=CIRCLE('',#105123,60.4792282238308);
#33559=CIRCLE('',#105124,60.4792282238308);
#33560=CIRCLE('',#105125,60.4792282238308);
#33561=CIRCLE('',#105127,60.6419265158129);
#33562=CIRCLE('',#105129,60.8618969683742);
#33563=CIRCLE('',#105130,61.0131030316259);
#33564=CIRCLE('',#105132,61.2330734841871);
#33565=CIRCLE('',#105133,61.3957717761693);
#33566=CIRCLE('',#105134,61.3957717761693);
#33567=CIRCLE('',#105135,61.3957717761693);
#33568=CIRCLE('',#105137,61.8704694830905);
#33569=CIRCLE('',#105139,0.635007073208636);
#33570=CIRCLE('',#105140,0.635007073208635);
#33571=CIRCLE('',#105151,60.0045305169095);
#33572=CIRCLE('',#105152,60.4792282238308);
#33573=CIRCLE('',#105153,60.4792282238308);
#33574=CIRCLE('',#105154,60.4792282238308);
#33575=CIRCLE('',#105156,60.6419265158129);
#33576=CIRCLE('',#105158,60.8618969683742);
#33577=CIRCLE('',#105159,61.0131030316259);
#33578=CIRCLE('',#105161,61.2330734841871);
#33579=CIRCLE('',#105162,61.3957717761693);
#33580=CIRCLE('',#105163,61.3957717761693);
#33581=CIRCLE('',#105164,61.3957717761693);
#33582=CIRCLE('',#105166,61.8704694830905);
#33583=CIRCLE('',#105168,0.635007073208616);
#33584=CIRCLE('',#105169,0.635007073208608);
#33585=CIRCLE('',#105180,60.0045305169095);
#33586=CIRCLE('',#105181,60.4792282238308);
#33587=CIRCLE('',#105182,60.4792282238308);
#33588=CIRCLE('',#105183,60.4792282238308);
#33589=CIRCLE('',#105185,60.6419265158129);
#33590=CIRCLE('',#105187,60.8618969683742);
#33591=CIRCLE('',#105188,61.0131030316259);
#33592=CIRCLE('',#105190,61.2330734841871);
#33593=CIRCLE('',#105191,61.3957717761693);
#33594=CIRCLE('',#105192,61.3957717761693);
#33595=CIRCLE('',#105193,61.3957717761693);
#33596=CIRCLE('',#105195,61.8704694830905);
#33597=CIRCLE('',#105197,0.635007073208567);
#33598=CIRCLE('',#105198,0.635007073208631);
#33599=CIRCLE('',#105209,60.0045305169095);
#33600=CIRCLE('',#105210,60.4792282238308);
#33601=CIRCLE('',#105211,60.4792282238308);
#33602=CIRCLE('',#105212,60.4792282238308);
#33603=CIRCLE('',#105214,60.6419265158129);
#33604=CIRCLE('',#105216,60.8618969683742);
#33605=CIRCLE('',#105217,61.0131030316259);
#33606=CIRCLE('',#105219,61.2330734841871);
#33607=CIRCLE('',#105220,61.3957717761693);
#33608=CIRCLE('',#105221,61.3957717761693);
#33609=CIRCLE('',#105222,61.3957717761693);
#33610=CIRCLE('',#105224,61.8704694830905);
#33611=CIRCLE('',#105226,0.635007073208609);
#33612=CIRCLE('',#105227,0.635007073208634);
#33613=CIRCLE('',#105238,60.0045305169095);
#33614=CIRCLE('',#105239,60.4792282238308);
#33615=CIRCLE('',#105240,60.4792282238308);
#33616=CIRCLE('',#105241,60.4792282238308);
#33617=CIRCLE('',#105243,60.6419265158129);
#33618=CIRCLE('',#105245,60.8618969683742);
#33619=CIRCLE('',#105246,61.0131030316259);
#33620=CIRCLE('',#105248,61.2330734841871);
#33621=CIRCLE('',#105249,61.3957717761693);
#33622=CIRCLE('',#105250,61.3957717761693);
#33623=CIRCLE('',#105251,61.3957717761693);
#33624=CIRCLE('',#105253,61.8704694830905);
#33625=CIRCLE('',#105255,0.63500707320864);
#33626=CIRCLE('',#105256,0.635007073208652);
#33627=CIRCLE('',#105267,60.0045305169095);
#33628=CIRCLE('',#105268,60.4792282238308);
#33629=CIRCLE('',#105269,60.4792282238308);
#33630=CIRCLE('',#105270,60.4792282238308);
#33631=CIRCLE('',#105272,60.6419265158129);
#33632=CIRCLE('',#105274,60.8618969683742);
#33633=CIRCLE('',#105275,61.0131030316259);
#33634=CIRCLE('',#105277,61.2330734841871);
#33635=CIRCLE('',#105278,61.3957717761693);
#33636=CIRCLE('',#105279,61.3957717761693);
#33637=CIRCLE('',#105280,61.3957717761693);
#33638=CIRCLE('',#105282,61.8704694830905);
#33639=CIRCLE('',#105284,0.635007073208623);
#33640=CIRCLE('',#105285,0.635007073208637);
#33641=CIRCLE('',#105296,60.0045305169095);
#33642=CIRCLE('',#105297,60.4792282238308);
#33643=CIRCLE('',#105298,60.4792282238308);
#33644=CIRCLE('',#105299,60.4792282238308);
#33645=CIRCLE('',#105301,60.6419265158129);
#33646=CIRCLE('',#105303,60.8618969683742);
#33647=CIRCLE('',#105304,61.0131030316259);
#33648=CIRCLE('',#105306,61.2330734841871);
#33649=CIRCLE('',#105307,61.3957717761693);
#33650=CIRCLE('',#105308,61.3957717761693);
#33651=CIRCLE('',#105309,61.3957717761693);
#33652=CIRCLE('',#105311,61.8704694830905);
#33653=CIRCLE('',#105313,0.635007073208589);
#33654=CIRCLE('',#105314,0.635007073208633);
#33655=CIRCLE('',#105325,60.0045305169095);
#33656=CIRCLE('',#105326,60.4792282238308);
#33657=CIRCLE('',#105327,60.4792282238308);
#33658=CIRCLE('',#105328,60.4792282238308);
#33659=CIRCLE('',#105330,60.6419265158129);
#33660=CIRCLE('',#105332,60.8618969683742);
#33661=CIRCLE('',#105333,61.0131030316259);
#33662=CIRCLE('',#105335,61.2330734841871);
#33663=CIRCLE('',#105336,61.3957717761693);
#33664=CIRCLE('',#105337,61.3957717761693);
#33665=CIRCLE('',#105338,61.3957717761693);
#33666=CIRCLE('',#105340,61.8704694830905);
#33667=CIRCLE('',#105342,0.635007073208619);
#33668=CIRCLE('',#105343,0.635007073208628);
#33669=CIRCLE('',#105354,60.0045305169095);
#33670=CIRCLE('',#105355,60.4792282238308);
#33671=CIRCLE('',#105356,60.4792282238308);
#33672=CIRCLE('',#105357,60.4792282238308);
#33673=CIRCLE('',#105359,60.6419265158129);
#33674=CIRCLE('',#105361,60.8618969683742);
#33675=CIRCLE('',#105362,61.0131030316259);
#33676=CIRCLE('',#105364,61.2330734841871);
#33677=CIRCLE('',#105365,61.3957717761693);
#33678=CIRCLE('',#105366,61.3957717761693);
#33679=CIRCLE('',#105367,61.3957717761693);
#33680=CIRCLE('',#105369,61.8704694830905);
#33681=CIRCLE('',#105371,0.635007073208656);
#33682=CIRCLE('',#105372,0.635007073208614);
#33683=CIRCLE('',#105383,60.0045305169095);
#33684=CIRCLE('',#105384,60.4792282238308);
#33685=CIRCLE('',#105385,60.4792282238308);
#33686=CIRCLE('',#105386,60.4792282238308);
#33687=CIRCLE('',#105388,60.6419265158129);
#33688=CIRCLE('',#105390,60.8618969683742);
#33689=CIRCLE('',#105391,61.0131030316259);
#33690=CIRCLE('',#105393,61.2330734841871);
#33691=CIRCLE('',#105394,61.3957717761693);
#33692=CIRCLE('',#105395,61.3957717761693);
#33693=CIRCLE('',#105396,61.3957717761693);
#33694=CIRCLE('',#105398,61.8704694830905);
#33695=CIRCLE('',#105400,0.635007073208594);
#33696=CIRCLE('',#105401,0.635007073208644);
#33697=CIRCLE('',#105412,60.0045305169095);
#33698=CIRCLE('',#105413,60.4792282238308);
#33699=CIRCLE('',#105414,60.4792282238308);
#33700=CIRCLE('',#105415,60.4792282238308);
#33701=CIRCLE('',#105417,60.6419265158129);
#33702=CIRCLE('',#105419,60.8618969683742);
#33703=CIRCLE('',#105420,61.0131030316259);
#33704=CIRCLE('',#105422,61.2330734841871);
#33705=CIRCLE('',#105423,61.3957717761693);
#33706=CIRCLE('',#105424,61.3957717761693);
#33707=CIRCLE('',#105425,61.3957717761693);
#33708=CIRCLE('',#105427,61.8704694830905);
#33709=CIRCLE('',#105429,0.635007073208621);
#33710=CIRCLE('',#105430,0.635007073208619);
#33711=CIRCLE('',#105441,60.0045305169095);
#33712=CIRCLE('',#105442,60.4792282238308);
#33713=CIRCLE('',#105443,60.4792282238308);
#33714=CIRCLE('',#105444,60.4792282238308);
#33715=CIRCLE('',#105446,60.6419265158129);
#33716=CIRCLE('',#105448,60.8618969683742);
#33717=CIRCLE('',#105449,61.0131030316259);
#33718=CIRCLE('',#105451,61.2330734841871);
#33719=CIRCLE('',#105452,61.3957717761693);
#33720=CIRCLE('',#105453,61.3957717761693);
#33721=CIRCLE('',#105454,61.3957717761693);
#33722=CIRCLE('',#105456,61.8704694830905);
#33723=CIRCLE('',#105458,0.635007073208605);
#33724=CIRCLE('',#105459,0.635007073208611);
#33725=CIRCLE('',#105470,60.0045305169095);
#33726=CIRCLE('',#105471,60.4792282238308);
#33727=CIRCLE('',#105472,60.4792282238308);
#33728=CIRCLE('',#105473,60.4792282238308);
#33729=CIRCLE('',#105475,60.6419265158129);
#33730=CIRCLE('',#105477,60.8618969683742);
#33731=CIRCLE('',#105478,61.0131030316259);
#33732=CIRCLE('',#105480,61.2330734841871);
#33733=CIRCLE('',#105481,61.3957717761693);
#33734=CIRCLE('',#105482,61.3957717761693);
#33735=CIRCLE('',#105483,61.3957717761693);
#33736=CIRCLE('',#105485,61.8704694830905);
#33737=CIRCLE('',#105487,0.635007073208634);
#33738=CIRCLE('',#105488,0.63500707320863);
#33739=CIRCLE('',#105499,60.0045305169095);
#33740=CIRCLE('',#105500,60.4792282238308);
#33741=CIRCLE('',#105501,60.4792282238308);
#33742=CIRCLE('',#105502,60.4792282238308);
#33743=CIRCLE('',#105504,60.6419265158129);
#33744=CIRCLE('',#105506,60.8618969683742);
#33745=CIRCLE('',#105507,61.0131030316259);
#33746=CIRCLE('',#105509,61.2330734841871);
#33747=CIRCLE('',#105510,61.3957717761693);
#33748=CIRCLE('',#105511,61.3957717761693);
#33749=CIRCLE('',#105512,61.3957717761693);
#33750=CIRCLE('',#105514,61.8704694830905);
#33751=CIRCLE('',#105516,0.635007073208654);
#33752=CIRCLE('',#105517,0.635007073208608);
#33753=CIRCLE('',#105528,60.0045305169095);
#33754=CIRCLE('',#105529,60.4792282238308);
#33755=CIRCLE('',#105530,60.4792282238308);
#33756=CIRCLE('',#105531,60.4792282238308);
#33757=CIRCLE('',#105533,60.6419265158129);
#33758=CIRCLE('',#105535,60.8618969683742);
#33759=CIRCLE('',#105536,61.0131030316259);
#33760=CIRCLE('',#105538,61.2330734841871);
#33761=CIRCLE('',#105539,61.3957717761693);
#33762=CIRCLE('',#105540,61.3957717761693);
#33763=CIRCLE('',#105541,61.3957717761693);
#33764=CIRCLE('',#105543,61.8704694830905);
#33765=CIRCLE('',#105545,0.6350070732086);
#33766=CIRCLE('',#105546,0.635007073208599);
#33767=CIRCLE('',#105557,60.0045305169095);
#33768=CIRCLE('',#105558,60.4792282238308);
#33769=CIRCLE('',#105559,60.4792282238308);
#33770=CIRCLE('',#105560,60.4792282238308);
#33771=CIRCLE('',#105562,60.6419265158129);
#33772=CIRCLE('',#105564,60.8618969683742);
#33773=CIRCLE('',#105565,61.0131030316259);
#33774=CIRCLE('',#105567,61.2330734841871);
#33775=CIRCLE('',#105568,61.3957717761693);
#33776=CIRCLE('',#105569,61.3957717761693);
#33777=CIRCLE('',#105570,61.3957717761693);
#33778=CIRCLE('',#105572,61.8704694830905);
#33779=CIRCLE('',#105574,0.635007073208643);
#33780=CIRCLE('',#105575,0.635007073208631);
#33781=CIRCLE('',#105586,60.0045305169095);
#33782=CIRCLE('',#105587,60.4792282238308);
#33783=CIRCLE('',#105588,60.4792282238308);
#33784=CIRCLE('',#105589,60.4792282238308);
#33785=CIRCLE('',#105591,60.6419265158129);
#33786=CIRCLE('',#105593,60.8618969683742);
#33787=CIRCLE('',#105594,61.0131030316259);
#33788=CIRCLE('',#105596,61.2330734841871);
#33789=CIRCLE('',#105597,61.3957717761693);
#33790=CIRCLE('',#105598,61.3957717761693);
#33791=CIRCLE('',#105599,61.3957717761693);
#33792=CIRCLE('',#105601,61.8704694830905);
#33793=CIRCLE('',#105603,0.635007073208614);
#33794=CIRCLE('',#105604,0.635007073208602);
#33795=CIRCLE('',#105615,60.0045305169095);
#33796=CIRCLE('',#105616,60.4792282238308);
#33797=CIRCLE('',#105617,60.4792282238308);
#33798=CIRCLE('',#105618,60.4792282238308);
#33799=CIRCLE('',#105620,60.6419265158129);
#33800=CIRCLE('',#105622,60.8618969683742);
#33801=CIRCLE('',#105623,61.0131030316259);
#33802=CIRCLE('',#105625,61.2330734841871);
#33803=CIRCLE('',#105626,61.3957717761693);
#33804=CIRCLE('',#105627,61.3957717761693);
#33805=CIRCLE('',#105628,61.3957717761693);
#33806=CIRCLE('',#105630,61.8704694830905);
#33807=CIRCLE('',#105632,0.635007073208624);
#33808=CIRCLE('',#105633,0.635007073208626);
#33809=CIRCLE('',#105644,60.0045305169095);
#33810=CIRCLE('',#105645,60.4792282238308);
#33811=CIRCLE('',#105646,60.4792282238308);
#33812=CIRCLE('',#105647,60.4792282238308);
#33813=CIRCLE('',#105649,60.6419265158129);
#33814=CIRCLE('',#105651,60.8618969683742);
#33815=CIRCLE('',#105652,61.0131030316259);
#33816=CIRCLE('',#105654,61.2330734841871);
#33817=CIRCLE('',#105655,61.3957717761693);
#33818=CIRCLE('',#105656,61.3957717761693);
#33819=CIRCLE('',#105657,61.3957717761693);
#33820=CIRCLE('',#105659,61.8704694830905);
#33821=CIRCLE('',#105661,0.635007073208606);
#33822=CIRCLE('',#105662,0.635007073208636);
#33823=CIRCLE('',#105673,60.0045305169095);
#33824=CIRCLE('',#105674,60.4792282238308);
#33825=CIRCLE('',#105675,60.4792282238308);
#33826=CIRCLE('',#105676,60.4792282238308);
#33827=CIRCLE('',#105678,60.6419265158129);
#33828=CIRCLE('',#105680,60.8618969683742);
#33829=CIRCLE('',#105681,61.0131030316259);
#33830=CIRCLE('',#105683,61.2330734841871);
#33831=CIRCLE('',#105684,61.3957717761693);
#33832=CIRCLE('',#105685,61.3957717761693);
#33833=CIRCLE('',#105686,61.3957717761693);
#33834=CIRCLE('',#105688,61.8704694830905);
#33835=CIRCLE('',#105690,0.635007073208653);
#33836=CIRCLE('',#105691,0.635007073208628);
#33837=CIRCLE('',#105702,60.0045305169095);
#33838=CIRCLE('',#105703,60.4792282238308);
#33839=CIRCLE('',#105704,60.4792282238308);
#33840=CIRCLE('',#105705,60.4792282238308);
#33841=CIRCLE('',#105707,60.6419265158129);
#33842=CIRCLE('',#105709,60.8618969683742);
#33843=CIRCLE('',#105710,61.0131030316259);
#33844=CIRCLE('',#105712,61.2330734841871);
#33845=CIRCLE('',#105713,61.3957717761693);
#33846=CIRCLE('',#105714,61.3957717761693);
#33847=CIRCLE('',#105715,61.3957717761693);
#33848=CIRCLE('',#105717,61.8704694830905);
#33849=CIRCLE('',#105719,0.635007073208654);
#33850=CIRCLE('',#105720,0.63500707320867);
#33851=CIRCLE('',#105731,60.0045305169095);
#33852=CIRCLE('',#105732,60.4792282238308);
#33853=CIRCLE('',#105733,60.4792282238308);
#33854=CIRCLE('',#105734,60.4792282238308);
#33855=CIRCLE('',#105736,60.6419265158129);
#33856=CIRCLE('',#105738,60.8618969683742);
#33857=CIRCLE('',#105739,61.0131030316259);
#33858=CIRCLE('',#105741,61.2330734841871);
#33859=CIRCLE('',#105742,61.3957717761693);
#33860=CIRCLE('',#105743,61.3957717761693);
#33861=CIRCLE('',#105744,61.3957717761693);
#33862=CIRCLE('',#105746,61.8704694830905);
#33863=CIRCLE('',#105748,0.635007073208616);
#33864=CIRCLE('',#105749,0.635007073208614);
#33865=CIRCLE('',#105760,60.0045305169095);
#33866=CIRCLE('',#105761,60.4792282238308);
#33867=CIRCLE('',#105762,60.4792282238308);
#33868=CIRCLE('',#105763,60.4792282238308);
#33869=CIRCLE('',#105765,60.6419265158129);
#33870=CIRCLE('',#105767,60.8618969683742);
#33871=CIRCLE('',#105768,61.0131030316259);
#33872=CIRCLE('',#105770,61.2330734841871);
#33873=CIRCLE('',#105771,61.3957717761693);
#33874=CIRCLE('',#105772,61.3957717761693);
#33875=CIRCLE('',#105773,61.3957717761693);
#33876=CIRCLE('',#105775,61.8704694830905);
#33877=CIRCLE('',#105777,0.635007073208599);
#33878=CIRCLE('',#105778,0.635007073208632);
#33879=CIRCLE('',#105789,60.0045305169095);
#33880=CIRCLE('',#105790,60.4792282238308);
#33881=CIRCLE('',#105791,60.4792282238308);
#33882=CIRCLE('',#105792,60.4792282238308);
#33883=CIRCLE('',#105794,60.6419265158129);
#33884=CIRCLE('',#105796,60.8618969683742);
#33885=CIRCLE('',#105797,61.0131030316259);
#33886=CIRCLE('',#105799,61.2330734841871);
#33887=CIRCLE('',#105800,61.3957717761693);
#33888=CIRCLE('',#105801,61.3957717761693);
#33889=CIRCLE('',#105802,61.3957717761693);
#33890=CIRCLE('',#105804,61.8704694830905);
#33891=CIRCLE('',#105806,0.635007073208614);
#33892=CIRCLE('',#105807,0.63500707320859);
#33893=CIRCLE('',#105818,60.0045305169095);
#33894=CIRCLE('',#105819,60.4792282238308);
#33895=CIRCLE('',#105820,60.4792282238308);
#33896=CIRCLE('',#105821,60.4792282238308);
#33897=CIRCLE('',#105823,60.6419265158129);
#33898=CIRCLE('',#105825,60.8618969683742);
#33899=CIRCLE('',#105826,61.0131030316259);
#33900=CIRCLE('',#105828,61.2330734841871);
#33901=CIRCLE('',#105829,61.3957717761693);
#33902=CIRCLE('',#105830,61.3957717761693);
#33903=CIRCLE('',#105831,61.3957717761693);
#33904=CIRCLE('',#105833,61.8704694830905);
#33905=CIRCLE('',#105835,0.635007073208637);
#33906=CIRCLE('',#105836,0.635007073208625);
#33907=CIRCLE('',#105847,60.0045305169095);
#33908=CIRCLE('',#105848,60.4792282238308);
#33909=CIRCLE('',#105849,60.4792282238308);
#33910=CIRCLE('',#105850,60.4792282238308);
#33911=CIRCLE('',#105852,60.6419265158129);
#33912=CIRCLE('',#105854,60.8618969683742);
#33913=CIRCLE('',#105855,61.0131030316259);
#33914=CIRCLE('',#105857,61.2330734841871);
#33915=CIRCLE('',#105858,61.3957717761693);
#33916=CIRCLE('',#105859,61.3957717761693);
#33917=CIRCLE('',#105860,61.3957717761693);
#33918=CIRCLE('',#105862,61.8704694830905);
#33919=CIRCLE('',#105864,0.635007073208638);
#33920=CIRCLE('',#105865,0.635007073208649);
#33921=CIRCLE('',#105876,60.0045305169095);
#33922=CIRCLE('',#105877,60.4792282238308);
#33923=CIRCLE('',#105878,60.4792282238308);
#33924=CIRCLE('',#105879,60.4792282238308);
#33925=CIRCLE('',#105881,60.6419265158129);
#33926=CIRCLE('',#105883,60.8618969683742);
#33927=CIRCLE('',#105884,61.0131030316259);
#33928=CIRCLE('',#105886,61.2330734841871);
#33929=CIRCLE('',#105887,61.3957717761693);
#33930=CIRCLE('',#105888,61.3957717761693);
#33931=CIRCLE('',#105889,61.3957717761693);
#33932=CIRCLE('',#105891,61.8704694830905);
#33933=CIRCLE('',#105893,0.635007073208641);
#33934=CIRCLE('',#105894,0.635007073208602);
#33935=CIRCLE('',#105905,60.0045305169095);
#33936=CIRCLE('',#105906,60.4792282238308);
#33937=CIRCLE('',#105907,60.4792282238308);
#33938=CIRCLE('',#105908,60.4792282238308);
#33939=CIRCLE('',#105910,60.6419265158129);
#33940=CIRCLE('',#105912,60.8618969683742);
#33941=CIRCLE('',#105913,61.0131030316259);
#33942=CIRCLE('',#105915,61.2330734841871);
#33943=CIRCLE('',#105916,61.3957717761693);
#33944=CIRCLE('',#105917,61.3957717761693);
#33945=CIRCLE('',#105918,61.3957717761693);
#33946=CIRCLE('',#105920,61.8704694830905);
#33947=CIRCLE('',#105922,0.635007073208628);
#33948=CIRCLE('',#105923,0.635007073208635);
#33949=CIRCLE('',#105934,60.0045305169095);
#33950=CIRCLE('',#105935,60.4792282238308);
#33951=CIRCLE('',#105936,60.4792282238308);
#33952=CIRCLE('',#105937,60.4792282238308);
#33953=CIRCLE('',#105939,60.6419265158129);
#33954=CIRCLE('',#105941,60.8618969683742);
#33955=CIRCLE('',#105942,61.0131030316259);
#33956=CIRCLE('',#105944,61.2330734841871);
#33957=CIRCLE('',#105945,61.3957717761693);
#33958=CIRCLE('',#105946,61.3957717761693);
#33959=CIRCLE('',#105947,61.3957717761693);
#33960=CIRCLE('',#105949,61.8704694830905);
#33961=CIRCLE('',#105951,0.63500707320863);
#33962=CIRCLE('',#105952,0.635007073208594);
#33963=CIRCLE('',#105963,60.0045305169095);
#33964=CIRCLE('',#105964,60.4792282238308);
#33965=CIRCLE('',#105965,60.4792282238308);
#33966=CIRCLE('',#105966,60.4792282238308);
#33967=CIRCLE('',#105968,60.6419265158129);
#33968=CIRCLE('',#105970,60.8618969683742);
#33969=CIRCLE('',#105971,61.0131030316259);
#33970=CIRCLE('',#105973,61.2330734841871);
#33971=CIRCLE('',#105974,61.3957717761693);
#33972=CIRCLE('',#105975,61.3957717761693);
#33973=CIRCLE('',#105976,61.3957717761693);
#33974=CIRCLE('',#105978,61.8704694830905);
#33975=CIRCLE('',#105980,0.635007073208599);
#33976=CIRCLE('',#105981,0.635007073208596);
#33977=CIRCLE('',#105992,60.0045305169095);
#33978=CIRCLE('',#105993,60.4792282238308);
#33979=CIRCLE('',#105994,60.4792282238308);
#33980=CIRCLE('',#105995,60.4792282238308);
#33981=CIRCLE('',#105997,60.6419265158129);
#33982=CIRCLE('',#105999,60.8618969683742);
#33983=CIRCLE('',#106000,61.0131030316259);
#33984=CIRCLE('',#106002,61.2330734841871);
#33985=CIRCLE('',#106003,61.3957717761693);
#33986=CIRCLE('',#106004,61.3957717761693);
#33987=CIRCLE('',#106005,61.3957717761693);
#33988=CIRCLE('',#106007,61.8704694830905);
#33989=CIRCLE('',#106009,0.635007073208624);
#33990=CIRCLE('',#106010,0.635007073208611);
#33991=CIRCLE('',#106021,60.0045305169095);
#33992=CIRCLE('',#106022,60.4792282238308);
#33993=CIRCLE('',#106023,60.4792282238308);
#33994=CIRCLE('',#106024,60.4792282238308);
#33995=CIRCLE('',#106026,60.6419265158129);
#33996=CIRCLE('',#106028,60.8618969683742);
#33997=CIRCLE('',#106029,61.0131030316259);
#33998=CIRCLE('',#106031,61.2330734841871);
#33999=CIRCLE('',#106032,61.3957717761693);
#34000=CIRCLE('',#106033,61.3957717761693);
#34001=CIRCLE('',#106034,61.3957717761693);
#34002=CIRCLE('',#106036,61.8704694830905);
#34003=CIRCLE('',#106038,0.635007073208621);
#34004=CIRCLE('',#106039,0.6350070732086);
#34005=CIRCLE('',#106050,60.0045305169095);
#34006=CIRCLE('',#106051,60.4792282238308);
#34007=CIRCLE('',#106052,60.4792282238308);
#34008=CIRCLE('',#106053,60.4792282238308);
#34009=CIRCLE('',#106055,60.6419265158129);
#34010=CIRCLE('',#106057,60.8618969683742);
#34011=CIRCLE('',#106058,61.0131030316259);
#34012=CIRCLE('',#106060,61.2330734841871);
#34013=CIRCLE('',#106061,61.3957717761693);
#34014=CIRCLE('',#106062,61.3957717761693);
#34015=CIRCLE('',#106063,61.3957717761693);
#34016=CIRCLE('',#106065,61.8704694830905);
#34017=CIRCLE('',#106067,0.635007073208618);
#34018=CIRCLE('',#106068,0.635007073208615);
#34019=CIRCLE('',#106079,60.0045305169095);
#34020=CIRCLE('',#106080,60.4792282238308);
#34021=CIRCLE('',#106081,60.4792282238308);
#34022=CIRCLE('',#106082,60.4792282238308);
#34023=CIRCLE('',#106084,60.6419265158129);
#34024=CIRCLE('',#106086,60.8618969683742);
#34025=CIRCLE('',#106087,61.0131030316259);
#34026=CIRCLE('',#106089,61.2330734841871);
#34027=CIRCLE('',#106090,61.3957717761693);
#34028=CIRCLE('',#106091,61.3957717761693);
#34029=CIRCLE('',#106092,61.3957717761693);
#34030=CIRCLE('',#106094,61.8704694830905);
#34031=CIRCLE('',#106096,0.635007073208615);
#34032=CIRCLE('',#106097,0.6350070732086);
#34033=CIRCLE('',#106108,60.0045305169095);
#34034=CIRCLE('',#106109,60.4792282238308);
#34035=CIRCLE('',#106110,60.4792282238308);
#34036=CIRCLE('',#106111,60.4792282238308);
#34037=CIRCLE('',#106113,60.6419265158129);
#34038=CIRCLE('',#106115,60.8618969683742);
#34039=CIRCLE('',#106116,61.0131030316259);
#34040=CIRCLE('',#106118,61.2330734841871);
#34041=CIRCLE('',#106119,61.3957717761693);
#34042=CIRCLE('',#106120,61.3957717761693);
#34043=CIRCLE('',#106121,61.3957717761693);
#34044=CIRCLE('',#106123,61.8704694830905);
#34045=CIRCLE('',#106125,0.635007073208631);
#34046=CIRCLE('',#106126,0.635007073208609);
#34047=CIRCLE('',#106137,60.0045305169095);
#34048=CIRCLE('',#106138,60.4792282238308);
#34049=CIRCLE('',#106139,60.4792282238308);
#34050=CIRCLE('',#106140,60.4792282238308);
#34051=CIRCLE('',#106142,60.6419265158129);
#34052=CIRCLE('',#106144,60.8618969683742);
#34053=CIRCLE('',#106145,61.0131030316259);
#34054=CIRCLE('',#106147,61.2330734841871);
#34055=CIRCLE('',#106148,61.3957717761693);
#34056=CIRCLE('',#106149,61.3957717761693);
#34057=CIRCLE('',#106150,61.3957717761693);
#34058=CIRCLE('',#106152,61.8704694830905);
#34059=CIRCLE('',#106154,0.635007073208616);
#34060=CIRCLE('',#106155,0.635007073208572);
#34061=CIRCLE('',#106166,60.0045305169095);
#34062=CIRCLE('',#106167,60.4792282238308);
#34063=CIRCLE('',#106168,60.4792282238308);
#34064=CIRCLE('',#106169,60.4792282238308);
#34065=CIRCLE('',#106171,60.6419265158129);
#34066=CIRCLE('',#106173,60.8618969683742);
#34067=CIRCLE('',#106174,61.0131030316259);
#34068=CIRCLE('',#106176,61.2330734841871);
#34069=CIRCLE('',#106177,61.3957717761693);
#34070=CIRCLE('',#106178,61.3957717761693);
#34071=CIRCLE('',#106179,61.3957717761693);
#34072=CIRCLE('',#106181,61.8704694830905);
#34073=CIRCLE('',#106183,0.635007073208599);
#34074=CIRCLE('',#106184,0.635007073208599);
#34075=CIRCLE('',#106195,60.0045305169095);
#34076=CIRCLE('',#106196,60.4792282238308);
#34077=CIRCLE('',#106197,60.4792282238308);
#34078=CIRCLE('',#106198,60.4792282238308);
#34079=CIRCLE('',#106200,60.6419265158129);
#34080=CIRCLE('',#106202,60.8618969683742);
#34081=CIRCLE('',#106203,61.0131030316259);
#34082=CIRCLE('',#106205,61.2330734841871);
#34083=CIRCLE('',#106206,61.3957717761693);
#34084=CIRCLE('',#106207,61.3957717761693);
#34085=CIRCLE('',#106208,61.3957717761693);
#34086=CIRCLE('',#106210,61.8704694830905);
#34087=CIRCLE('',#106212,0.635007073208628);
#34088=CIRCLE('',#106213,0.635007073208624);
#34089=CIRCLE('',#106224,60.0045305169095);
#34090=CIRCLE('',#106225,60.4792282238308);
#34091=CIRCLE('',#106226,60.4792282238308);
#34092=CIRCLE('',#106227,60.4792282238308);
#34093=CIRCLE('',#106229,60.6419265158129);
#34094=CIRCLE('',#106231,60.8618969683742);
#34095=CIRCLE('',#106232,61.0131030316259);
#34096=CIRCLE('',#106234,61.2330734841871);
#34097=CIRCLE('',#106235,61.3957717761693);
#34098=CIRCLE('',#106236,61.3957717761693);
#34099=CIRCLE('',#106237,61.3957717761693);
#34100=CIRCLE('',#106239,61.8704694830905);
#34101=CIRCLE('',#106241,0.635007073208624);
#34102=CIRCLE('',#106242,0.635007073208604);
#34103=CIRCLE('',#106253,60.0045305169095);
#34104=CIRCLE('',#106254,60.4792282238308);
#34105=CIRCLE('',#106255,60.4792282238308);
#34106=CIRCLE('',#106256,60.4792282238308);
#34107=CIRCLE('',#106258,60.6419265158129);
#34108=CIRCLE('',#106260,60.8618969683742);
#34109=CIRCLE('',#106261,61.0131030316259);
#34110=CIRCLE('',#106263,61.2330734841871);
#34111=CIRCLE('',#106264,61.3957717761693);
#34112=CIRCLE('',#106265,61.3957717761693);
#34113=CIRCLE('',#106266,61.3957717761693);
#34114=CIRCLE('',#106268,61.8704694830905);
#34115=CIRCLE('',#106270,0.635007073208647);
#34116=CIRCLE('',#106271,0.635007073208648);
#34117=CIRCLE('',#106282,60.0045305169095);
#34118=CIRCLE('',#106283,60.4792282238308);
#34119=CIRCLE('',#106284,60.4792282238308);
#34120=CIRCLE('',#106285,60.4792282238308);
#34121=CIRCLE('',#106287,60.6419265158129);
#34122=CIRCLE('',#106289,60.8618969683742);
#34123=CIRCLE('',#106290,61.0131030316259);
#34124=CIRCLE('',#106292,61.2330734841871);
#34125=CIRCLE('',#106293,61.3957717761693);
#34126=CIRCLE('',#106294,61.3957717761693);
#34127=CIRCLE('',#106295,61.3957717761693);
#34128=CIRCLE('',#106297,61.8704694830905);
#34129=CIRCLE('',#106299,0.63500707320862);
#34130=CIRCLE('',#106300,0.635007073208608);
#34131=CIRCLE('',#106311,60.0045305169095);
#34132=CIRCLE('',#106312,60.4792282238308);
#34133=CIRCLE('',#106313,60.4792282238308);
#34134=CIRCLE('',#106314,60.4792282238308);
#34135=CIRCLE('',#106316,60.6419265158129);
#34136=CIRCLE('',#106318,60.8618969683742);
#34137=CIRCLE('',#106319,61.0131030316259);
#34138=CIRCLE('',#106321,61.2330734841871);
#34139=CIRCLE('',#106322,61.3957717761693);
#34140=CIRCLE('',#106323,61.3957717761693);
#34141=CIRCLE('',#106324,61.3957717761693);
#34142=CIRCLE('',#106326,61.8704694830905);
#34143=CIRCLE('',#106328,0.635007073208603);
#34144=CIRCLE('',#106329,0.635007073208596);
#34145=CIRCLE('',#106340,60.0045305169095);
#34146=CIRCLE('',#106341,60.4792282238308);
#34147=CIRCLE('',#106342,60.4792282238308);
#34148=CIRCLE('',#106343,60.4792282238308);
#34149=CIRCLE('',#106345,60.6419265158129);
#34150=CIRCLE('',#106347,60.8618969683742);
#34151=CIRCLE('',#106348,61.0131030316259);
#34152=CIRCLE('',#106350,61.2330734841871);
#34153=CIRCLE('',#106351,61.3957717761693);
#34154=CIRCLE('',#106352,61.3957717761693);
#34155=CIRCLE('',#106353,61.3957717761693);
#34156=CIRCLE('',#106355,61.8704694830905);
#34157=CIRCLE('',#106357,0.635007073208654);
#34158=CIRCLE('',#106358,0.6350070732086);
#34159=CIRCLE('',#106369,60.0045305169095);
#34160=CIRCLE('',#106370,60.4792282238308);
#34161=CIRCLE('',#106371,60.4792282238308);
#34162=CIRCLE('',#106372,60.4792282238308);
#34163=CIRCLE('',#106374,60.6419265158129);
#34164=CIRCLE('',#106376,60.8618969683742);
#34165=CIRCLE('',#106377,61.0131030316259);
#34166=CIRCLE('',#106379,61.2330734841871);
#34167=CIRCLE('',#106380,61.3957717761693);
#34168=CIRCLE('',#106381,61.3957717761693);
#34169=CIRCLE('',#106382,61.3957717761693);
#34170=CIRCLE('',#106384,61.8704694830905);
#34171=CIRCLE('',#106386,0.635007073208615);
#34172=CIRCLE('',#106387,0.635007073208638);
#34173=CIRCLE('',#106398,60.0045305169095);
#34174=CIRCLE('',#106399,60.4792282238308);
#34175=CIRCLE('',#106400,60.4792282238308);
#34176=CIRCLE('',#106401,60.4792282238308);
#34177=CIRCLE('',#106403,60.6419265158129);
#34178=CIRCLE('',#106405,60.8618969683742);
#34179=CIRCLE('',#106406,61.0131030316259);
#34180=CIRCLE('',#106408,61.2330734841871);
#34181=CIRCLE('',#106409,61.3957717761693);
#34182=CIRCLE('',#106410,61.3957717761693);
#34183=CIRCLE('',#106411,61.3957717761693);
#34184=CIRCLE('',#106413,61.8704694830905);
#34185=CIRCLE('',#106415,0.635007073208598);
#34186=CIRCLE('',#106416,0.635007073208636);
#34187=CIRCLE('',#106427,60.0045305169095);
#34188=CIRCLE('',#106428,60.4792282238308);
#34189=CIRCLE('',#106429,60.4792282238308);
#34190=CIRCLE('',#106430,60.4792282238308);
#34191=CIRCLE('',#106432,60.6419265158129);
#34192=CIRCLE('',#106434,60.8618969683742);
#34193=CIRCLE('',#106435,61.0131030316259);
#34194=CIRCLE('',#106437,61.2330734841871);
#34195=CIRCLE('',#106438,61.3957717761693);
#34196=CIRCLE('',#106439,61.3957717761693);
#34197=CIRCLE('',#106440,61.3957717761693);
#34198=CIRCLE('',#106442,61.8704694830905);
#34199=CIRCLE('',#106444,0.635007073208679);
#34200=CIRCLE('',#106445,0.635007073208629);
#34201=CIRCLE('',#106456,60.0045305169095);
#34202=CIRCLE('',#106457,60.4792282238308);
#34203=CIRCLE('',#106458,60.4792282238308);
#34204=CIRCLE('',#106459,60.4792282238308);
#34205=CIRCLE('',#106461,60.6419265158129);
#34206=CIRCLE('',#106463,60.8618969683742);
#34207=CIRCLE('',#106464,61.0131030316259);
#34208=CIRCLE('',#106466,61.2330734841871);
#34209=CIRCLE('',#106467,61.3957717761693);
#34210=CIRCLE('',#106468,61.3957717761693);
#34211=CIRCLE('',#106469,61.3957717761693);
#34212=CIRCLE('',#106471,61.8704694830905);
#34213=CIRCLE('',#106473,0.63500707320862);
#34214=CIRCLE('',#106474,0.635007073208651);
#34215=CIRCLE('',#106485,60.0045305169095);
#34216=CIRCLE('',#106486,60.4792282238308);
#34217=CIRCLE('',#106487,60.4792282238308);
#34218=CIRCLE('',#106488,60.4792282238308);
#34219=CIRCLE('',#106490,60.6419265158129);
#34220=CIRCLE('',#106492,60.8618969683742);
#34221=CIRCLE('',#106493,61.0131030316259);
#34222=CIRCLE('',#106495,61.2330734841871);
#34223=CIRCLE('',#106496,61.3957717761693);
#34224=CIRCLE('',#106497,61.3957717761693);
#34225=CIRCLE('',#106498,61.3957717761693);
#34226=CIRCLE('',#106500,61.8704694830905);
#34227=CIRCLE('',#106502,0.635007073208615);
#34228=CIRCLE('',#106503,0.635007073208618);
#34229=CIRCLE('',#106514,60.0045305169095);
#34230=CIRCLE('',#106515,60.4792282238308);
#34231=CIRCLE('',#106516,60.4792282238308);
#34232=CIRCLE('',#106517,60.4792282238308);
#34233=CIRCLE('',#106519,60.6419265158129);
#34234=CIRCLE('',#106521,60.8618969683742);
#34235=CIRCLE('',#106522,61.0131030316259);
#34236=CIRCLE('',#106524,61.2330734841871);
#34237=CIRCLE('',#106525,61.3957717761693);
#34238=CIRCLE('',#106526,61.3957717761693);
#34239=CIRCLE('',#106527,61.3957717761693);
#34240=CIRCLE('',#106529,61.8704694830905);
#34241=CIRCLE('',#106531,0.635007073208631);
#34242=CIRCLE('',#106532,0.63500707320861);
#34243=CIRCLE('',#106543,60.0045305169095);
#34244=CIRCLE('',#106544,60.4792282238308);
#34245=CIRCLE('',#106545,60.4792282238308);
#34246=CIRCLE('',#106546,60.4792282238308);
#34247=CIRCLE('',#106548,60.6419265158129);
#34248=CIRCLE('',#106550,60.8618969683742);
#34249=CIRCLE('',#106551,61.0131030316259);
#34250=CIRCLE('',#106553,61.2330734841871);
#34251=CIRCLE('',#106554,61.3957717761693);
#34252=CIRCLE('',#106555,61.3957717761693);
#34253=CIRCLE('',#106556,61.3957717761693);
#34254=CIRCLE('',#106558,61.8704694830905);
#34255=CIRCLE('',#106560,0.635007073208622);
#34256=CIRCLE('',#106561,0.635007073208639);
#34257=CIRCLE('',#106572,60.0045305169095);
#34258=CIRCLE('',#106573,60.4792282238308);
#34259=CIRCLE('',#106574,60.4792282238308);
#34260=CIRCLE('',#106575,60.4792282238308);
#34261=CIRCLE('',#106577,60.6419265158129);
#34262=CIRCLE('',#106579,60.8618969683742);
#34263=CIRCLE('',#106580,61.0131030316259);
#34264=CIRCLE('',#106582,61.2330734841871);
#34265=CIRCLE('',#106583,61.3957717761693);
#34266=CIRCLE('',#106584,61.3957717761693);
#34267=CIRCLE('',#106585,61.3957717761693);
#34268=CIRCLE('',#106587,61.8704694830905);
#34269=CIRCLE('',#106589,0.635007073208608);
#34270=CIRCLE('',#106590,0.635007073208623);
#34271=CIRCLE('',#106601,60.0045305169095);
#34272=CIRCLE('',#106602,60.4792282238308);
#34273=CIRCLE('',#106603,60.4792282238308);
#34274=CIRCLE('',#106604,60.4792282238308);
#34275=CIRCLE('',#106606,60.6419265158129);
#34276=CIRCLE('',#106608,60.8618969683742);
#34277=CIRCLE('',#106609,61.0131030316259);
#34278=CIRCLE('',#106611,61.2330734841871);
#34279=CIRCLE('',#106612,61.3957717761693);
#34280=CIRCLE('',#106613,61.3957717761693);
#34281=CIRCLE('',#106614,61.3957717761693);
#34282=CIRCLE('',#106616,61.8704694830905);
#34283=CIRCLE('',#106618,0.635007073208607);
#34284=CIRCLE('',#106619,0.635007073208629);
#34285=CIRCLE('',#106631,60.0045305169095);
#34286=CIRCLE('',#106632,60.4792282238308);
#34287=CIRCLE('',#106633,60.4792282238308);
#34288=CIRCLE('',#106634,60.4792282238308);
#34289=CIRCLE('',#106636,60.6419265158129);
#34290=CIRCLE('',#106638,60.8618969683742);
#34291=CIRCLE('',#106639,61.0131030316259);
#34292=CIRCLE('',#106641,61.2330734841871);
#34293=CIRCLE('',#106642,61.3957717761693);
#34294=CIRCLE('',#106643,61.3957717761693);
#34295=CIRCLE('',#106644,61.3957717761693);
#34296=CIRCLE('',#106646,61.8704694830905);
#34297=CIRCLE('',#106650,0.635007073208622);
#34298=CIRCLE('',#106651,0.635007073208615);
#34299=CIRCLE('',#106662,62.8464445485378);
#34300=CIRCLE('',#106663,59.0285554514622);
#34301=CIRCLE('',#106678,0.127);
#34302=CIRCLE('',#106679,0.127);
#34303=CIRCLE('',#106681,0.127);
#34304=CIRCLE('',#106683,0.127);
#34305=CIRCLE('',#106684,0.126999999999997);
#34306=CIRCLE('',#106685,0.127000000000002);
#34307=CIRCLE('',#106687,0.127000000000005);
#34308=CIRCLE('',#106690,0.127000000000002);
#34309=CIRCLE('',#106692,0.127);
#34310=CIRCLE('',#106694,0.127000000000002);
#34311=CIRCLE('',#106695,0.127);
#34312=CIRCLE('',#106696,0.127000000000005);
#34313=CIRCLE('',#106698,0.126999999999998);
#34314=CIRCLE('',#106700,0.126999999999999);
#34315=CIRCLE('',#106701,0.127000000000002);
#34316=CIRCLE('',#106702,0.127);
#34317=CIRCLE('',#106704,0.127000000000002);
#34318=CIRCLE('',#106707,0.126999999999998);
#34319=CIRCLE('',#106709,0.127);
#34320=CIRCLE('',#106711,0.127);
#34321=CIRCLE('',#106712,0.127);
#34322=CIRCLE('',#106713,0.127);
#34323=CIRCLE('',#106715,0.127);
#34324=CIRCLE('',#106718,0.127);
#34325=CIRCLE('',#106721,62.8464445485378);
#34326=CIRCLE('',#106722,59.0285554514622);
#34327=CIRCLE('',#106734,62.8464445485378);
#34328=CIRCLE('',#106735,59.0285554514622);
#34329=CIRCLE('',#106747,62.8464445485378);
#34330=CIRCLE('',#106748,59.0285554514622);
#34331=CIRCLE('',#106760,62.8464445485378);
#34332=CIRCLE('',#106761,59.0285554514622);
#34333=CIRCLE('',#106773,62.8464445485378);
#34334=CIRCLE('',#106774,59.0285554514622);
#34335=CIRCLE('',#106786,62.8464445485378);
#34336=CIRCLE('',#106787,59.0285554514622);
#34337=CIRCLE('',#106799,62.8464445485378);
#34338=CIRCLE('',#106800,59.0285554514622);
#34339=CIRCLE('',#106812,62.8464445485378);
#34340=CIRCLE('',#106813,59.0285554514622);
#34341=CIRCLE('',#106825,62.8464445485378);
#34342=CIRCLE('',#106826,59.0285554514622);
#34343=CIRCLE('',#106838,62.8464445485378);
#34344=CIRCLE('',#106839,59.0285554514622);
#34345=CIRCLE('',#106851,62.8464445485378);
#34346=CIRCLE('',#106852,59.0285554514622);
#34347=CIRCLE('',#106864,62.8464445485378);
#34348=CIRCLE('',#106865,59.0285554514622);
#34349=CIRCLE('',#106877,62.8464445485378);
#34350=CIRCLE('',#106878,59.0285554514622);
#34351=CIRCLE('',#106890,62.8464445485378);
#34352=CIRCLE('',#106891,59.0285554514622);
#34353=CIRCLE('',#106903,62.8464445485378);
#34354=CIRCLE('',#106904,59.0285554514622);
#34355=CIRCLE('',#106916,62.8464445485378);
#34356=CIRCLE('',#106917,59.0285554514622);
#34357=CIRCLE('',#106929,62.8464445485378);
#34358=CIRCLE('',#106930,59.0285554514622);
#34359=CIRCLE('',#106942,62.8464445485378);
#34360=CIRCLE('',#106943,59.0285554514622);
#34361=CIRCLE('',#106955,62.8464445485378);
#34362=CIRCLE('',#106956,59.0285554514622);
#34363=CIRCLE('',#106968,62.8464445485378);
#34364=CIRCLE('',#106969,59.0285554514622);
#34365=CIRCLE('',#106981,62.8464445485378);
#34366=CIRCLE('',#106982,59.0285554514622);
#34367=CIRCLE('',#106994,62.8464445485378);
#34368=CIRCLE('',#106995,59.0285554514622);
#34369=CIRCLE('',#107007,62.8464445485378);
#34370=CIRCLE('',#107008,59.0285554514622);
#34371=CIRCLE('',#107020,62.8464445485378);
#34372=CIRCLE('',#107021,59.0285554514622);
#34373=CIRCLE('',#107033,62.8464445485378);
#34374=CIRCLE('',#107034,59.0285554514622);
#34375=CIRCLE('',#107046,62.8464445485378);
#34376=CIRCLE('',#107047,59.0285554514622);
#34377=CIRCLE('',#107059,62.8464445485378);
#34378=CIRCLE('',#107060,59.0285554514622);
#34379=CIRCLE('',#107072,62.8464445485378);
#34380=CIRCLE('',#107073,59.0285554514622);
#34381=CIRCLE('',#107085,62.8464445485378);
#34382=CIRCLE('',#107086,59.0285554514622);
#34383=CIRCLE('',#107109,62.8464445485378);
#34384=CIRCLE('',#107110,59.0285554514622);
#34385=CIRCLE('',#107122,62.8464445485378);
#34386=CIRCLE('',#107123,59.0285554514622);
#34387=CIRCLE('',#107135,62.8464445485378);
#34388=CIRCLE('',#107136,59.0285554514622);
#34389=CIRCLE('',#107148,62.8464445485378);
#34390=CIRCLE('',#107149,59.0285554514622);
#34391=CIRCLE('',#107161,62.8464445485378);
#34392=CIRCLE('',#107162,59.0285554514622);
#34393=CIRCLE('',#107174,62.8464445485378);
#34394=CIRCLE('',#107175,59.0285554514622);
#34395=CIRCLE('',#107187,62.8464445485378);
#34396=CIRCLE('',#107188,59.0285554514622);
#34397=CIRCLE('',#107200,62.8464445485378);
#34398=CIRCLE('',#107201,59.0285554514622);
#34399=CIRCLE('',#107213,62.8464445485378);
#34400=CIRCLE('',#107214,59.0285554514622);
#34401=CIRCLE('',#107226,62.8464445485378);
#34402=CIRCLE('',#107227,59.0285554514622);
#34403=CIRCLE('',#107239,62.8464445485378);
#34404=CIRCLE('',#107240,59.0285554514622);
#34405=CIRCLE('',#107252,62.8464445485378);
#34406=CIRCLE('',#107253,59.0285554514622);
#34407=CIRCLE('',#107265,62.8464445485378);
#34408=CIRCLE('',#107266,59.0285554514622);
#34409=CIRCLE('',#107278,62.8464445485378);
#34410=CIRCLE('',#107279,59.0285554514622);
#34411=CIRCLE('',#107302,62.8464445485378);
#34412=CIRCLE('',#107303,59.0285554514622);
#34413=CIRCLE('',#107315,62.8464445485378);
#34414=CIRCLE('',#107316,59.0285554514622);
#34415=CIRCLE('',#107328,62.8464445485378);
#34416=CIRCLE('',#107329,59.0285554514622);
#34417=CIRCLE('',#107341,62.8464445485378);
#34418=CIRCLE('',#107342,59.0285554514622);
#34419=CIRCLE('',#107354,62.8464445485378);
#34420=CIRCLE('',#107355,59.0285554514622);
#34421=CIRCLE('',#107367,62.8464445485378);
#34422=CIRCLE('',#107368,59.0285554514622);
#34423=CIRCLE('',#107380,62.8464445485378);
#34424=CIRCLE('',#107381,59.0285554514622);
#34425=CIRCLE('',#107393,62.8464445485378);
#34426=CIRCLE('',#107394,59.0285554514622);
#34427=CIRCLE('',#107406,62.8464445485378);
#34428=CIRCLE('',#107407,59.0285554514622);
#34429=CIRCLE('',#107419,62.8464445485378);
#34430=CIRCLE('',#107420,59.0285554514622);
#34431=CIRCLE('',#107432,62.8464445485378);
#34432=CIRCLE('',#107433,59.0285554514622);
#34433=CIRCLE('',#107445,62.8464445485378);
#34434=CIRCLE('',#107446,59.0285554514622);
#34435=CIRCLE('',#107458,62.8464445485378);
#34436=CIRCLE('',#107459,59.0285554514622);
#34437=CIRCLE('',#107471,62.8464445485378);
#34438=CIRCLE('',#107472,59.0285554514622);
#34439=CIRCLE('',#107603,0.126999999999997);
#34440=CIRCLE('',#107604,0.127);
#34441=CIRCLE('',#107606,0.127);
#34442=CIRCLE('',#107608,0.127);
#34443=CIRCLE('',#107609,0.127000000000001);
#34444=CIRCLE('',#107610,0.127000000000001);
#34445=CIRCLE('',#107612,0.127);
#34446=CIRCLE('',#107615,0.127000000000004);
#34447=CIRCLE('',#107617,0.127);
#34448=CIRCLE('',#107619,0.127000000000002);
#34449=CIRCLE('',#107620,0.127000000000001);
#34450=CIRCLE('',#107621,0.126999999999998);
#34451=CIRCLE('',#107623,0.127);
#34452=CIRCLE('',#107625,0.127000000000002);
#34453=CIRCLE('',#107626,0.127);
#34454=CIRCLE('',#107627,0.127);
#34455=CIRCLE('',#107629,0.126999999999997);
#34456=CIRCLE('',#107632,0.127);
#34457=CIRCLE('',#107634,0.127000000000002);
#34458=CIRCLE('',#107636,0.127000000000003);
#34459=CIRCLE('',#107637,0.127);
#34460=CIRCLE('',#107638,0.127);
#34461=CIRCLE('',#107640,0.127);
#34462=CIRCLE('',#107643,0.127);
#34463=CIRCLE('',#107647,0.127);
#34464=CIRCLE('',#107648,0.126999999999999);
#34465=CIRCLE('',#107650,0.126999999999999);
#34466=CIRCLE('',#107652,0.126999999999999);
#34467=CIRCLE('',#107653,0.127000000000002);
#34468=CIRCLE('',#107654,0.127000000000003);
#34469=CIRCLE('',#107656,0.127000000000001);
#34470=CIRCLE('',#107659,0.127000000000003);
#34471=CIRCLE('',#107661,0.126999999999999);
#34472=CIRCLE('',#107663,0.126999999999997);
#34473=CIRCLE('',#107664,0.127);
#34474=CIRCLE('',#107665,0.127000000000002);
#34475=CIRCLE('',#107667,0.127000000000003);
#34476=CIRCLE('',#107669,0.126999999999999);
#34477=CIRCLE('',#107670,0.127000000000002);
#34478=CIRCLE('',#107671,0.126999999999999);
#34479=CIRCLE('',#107673,0.127000000000001);
#34480=CIRCLE('',#107676,0.127000000000003);
#34481=CIRCLE('',#107678,0.126999999999999);
#34482=CIRCLE('',#107680,0.127000000000002);
#34483=CIRCLE('',#107681,0.126999999999999);
#34484=CIRCLE('',#107682,0.126999999999999);
#34485=CIRCLE('',#107684,0.126999999999999);
#34486=CIRCLE('',#107687,0.127000000000001);
#34487=CIRCLE('',#107691,0.127000000000003);
#34488=CIRCLE('',#107692,0.126999999999999);
#34489=CIRCLE('',#107694,0.126999999999999);
#34490=CIRCLE('',#107696,0.127);
#34491=CIRCLE('',#107697,0.127);
#34492=CIRCLE('',#107698,0.126999999999998);
#34493=CIRCLE('',#107700,0.126999999999998);
#34494=CIRCLE('',#107703,0.126999999999997);
#34495=CIRCLE('',#107705,0.127);
#34496=CIRCLE('',#107707,0.127000000000001);
#34497=CIRCLE('',#107708,0.127000000000002);
#34498=CIRCLE('',#107709,0.127000000000002);
#34499=CIRCLE('',#107711,0.126999999999997);
#34500=CIRCLE('',#107713,0.127000000000002);
#34501=CIRCLE('',#107714,0.127000000000003);
#34502=CIRCLE('',#107715,0.126999999999999);
#34503=CIRCLE('',#107717,0.127);
#34504=CIRCLE('',#107720,0.126999999999997);
#34505=CIRCLE('',#107722,0.127);
#34506=CIRCLE('',#107724,0.127);
#34507=CIRCLE('',#107725,0.126999999999999);
#34508=CIRCLE('',#107726,0.126999999999999);
#34509=CIRCLE('',#107728,0.126999999999999);
#34510=CIRCLE('',#107731,0.127000000000002);
#34511=CIRCLE('',#107735,0.126999999999998);
#34512=CIRCLE('',#107736,0.127000000000001);
#34513=CIRCLE('',#107738,0.127000000000001);
#34514=CIRCLE('',#107740,0.127000000000001);
#34515=CIRCLE('',#107741,0.127);
#34516=CIRCLE('',#107742,0.127000000000001);
#34517=CIRCLE('',#107744,0.127);
#34518=CIRCLE('',#107747,0.127000000000002);
#34519=CIRCLE('',#107749,0.127000000000001);
#34520=CIRCLE('',#107751,0.127000000000001);
#34521=CIRCLE('',#107752,0.126999999999998);
#34522=CIRCLE('',#107753,0.127);
#34523=CIRCLE('',#107755,0.126999999999999);
#34524=CIRCLE('',#107757,0.127000000000002);
#34525=CIRCLE('',#107758,0.127000000000002);
#34526=CIRCLE('',#107759,0.127000000000001);
#34527=CIRCLE('',#107761,0.126999999999997);
#34528=CIRCLE('',#107764,0.126999999999999);
#34529=CIRCLE('',#107766,0.126999999999998);
#34530=CIRCLE('',#107768,0.126999999999998);
#34531=CIRCLE('',#107769,0.127000000000001);
#34532=CIRCLE('',#107770,0.127000000000001);
#34533=CIRCLE('',#107772,0.127000000000001);
#34534=CIRCLE('',#107775,0.127000000000002);
#34535=CIRCLE('',#107779,0.127000000000001);
#34536=CIRCLE('',#107780,0.127);
#34537=CIRCLE('',#107782,0.127000000000003);
#34538=CIRCLE('',#107784,0.127);
#34539=CIRCLE('',#107785,0.126999999999998);
#34540=CIRCLE('',#107786,0.126999999999999);
#34541=CIRCLE('',#107788,0.127);
#34542=CIRCLE('',#107791,0.127000000000002);
#34543=CIRCLE('',#107793,0.127);
#34544=CIRCLE('',#107795,0.127000000000002);
#34545=CIRCLE('',#107796,0.127000000000002);
#34546=CIRCLE('',#107797,0.127);
#34547=CIRCLE('',#107799,0.127000000000001);
#34548=CIRCLE('',#107801,0.127);
#34549=CIRCLE('',#107802,0.126999999999999);
#34550=CIRCLE('',#107803,0.127);
#34551=CIRCLE('',#107805,0.127000000000001);
#34552=CIRCLE('',#107808,0.127000000000001);
#34553=CIRCLE('',#107810,0.127000000000002);
#34554=CIRCLE('',#107812,0.127);
#34555=CIRCLE('',#107813,0.127);
#34556=CIRCLE('',#107814,0.127);
#34557=CIRCLE('',#107816,0.127);
#34558=CIRCLE('',#107819,0.126999999999998);
#34559=CIRCLE('',#107823,0.127000000000001);
#34560=CIRCLE('',#107824,0.126999999999999);
#34561=CIRCLE('',#107826,0.126999999999999);
#34562=CIRCLE('',#107828,0.127000000000004);
#34563=CIRCLE('',#107829,0.127);
#34564=CIRCLE('',#107830,0.126999999999998);
#34565=CIRCLE('',#107832,0.126999999999999);
#34566=CIRCLE('',#107835,0.126999999999999);
#34567=CIRCLE('',#107837,0.127);
#34568=CIRCLE('',#107839,0.127);
#34569=CIRCLE('',#107840,0.126999999999997);
#34570=CIRCLE('',#107841,0.126999999999997);
#34571=CIRCLE('',#107843,0.127000000000001);
#34572=CIRCLE('',#107845,0.126999999999997);
#34573=CIRCLE('',#107846,0.127000000000003);
#34574=CIRCLE('',#107847,0.126999999999999);
#34575=CIRCLE('',#107849,0.127);
#34576=CIRCLE('',#107852,0.127000000000002);
#34577=CIRCLE('',#107854,0.127000000000002);
#34578=CIRCLE('',#107856,0.127000000000003);
#34579=CIRCLE('',#107857,0.126999999999999);
#34580=CIRCLE('',#107858,0.127000000000004);
#34581=CIRCLE('',#107860,0.126999999999999);
#34582=CIRCLE('',#107863,0.126999999999998);
#34583=CIRCLE('',#107867,0.127);
#34584=CIRCLE('',#107868,0.127);
#34585=CIRCLE('',#107870,0.127);
#34586=CIRCLE('',#107872,0.127);
#34587=CIRCLE('',#107873,0.127000000000003);
#34588=CIRCLE('',#107874,0.127000000000002);
#34589=CIRCLE('',#107876,0.126999999999998);
#34590=CIRCLE('',#107879,0.127000000000003);
#34591=CIRCLE('',#107881,0.127);
#34592=CIRCLE('',#107883,0.126999999999999);
#34593=CIRCLE('',#107884,0.127000000000001);
#34594=CIRCLE('',#107885,0.126999999999998);
#34595=CIRCLE('',#107887,0.127000000000002);
#34596=CIRCLE('',#107889,0.126999999999997);
#34597=CIRCLE('',#107890,0.127000000000004);
#34598=CIRCLE('',#107891,0.127);
#34599=CIRCLE('',#107893,0.127000000000001);
#34600=CIRCLE('',#107896,0.126999999999998);
#34601=CIRCLE('',#107898,0.127000000000002);
#34602=CIRCLE('',#107900,0.127);
#34603=CIRCLE('',#107901,0.127);
#34604=CIRCLE('',#107902,0.127);
#34605=CIRCLE('',#107904,0.127);
#34606=CIRCLE('',#107907,0.127000000000002);
#34607=CIRCLE('',#107911,0.127000000000002);
#34608=CIRCLE('',#107912,0.127);
#34609=CIRCLE('',#107914,0.127);
#34610=CIRCLE('',#107916,0.127);
#34611=CIRCLE('',#107917,0.126999999999998);
#34612=CIRCLE('',#107918,0.127000000000002);
#34613=CIRCLE('',#107920,0.126999999999999);
#34614=CIRCLE('',#107923,0.126999999999999);
#34615=CIRCLE('',#107925,0.127);
#34616=CIRCLE('',#107927,0.127000000000003);
#34617=CIRCLE('',#107928,0.127000000000002);
#34618=CIRCLE('',#107929,0.126999999999998);
#34619=CIRCLE('',#107931,0.126999999999999);
#34620=CIRCLE('',#107933,0.126999999999997);
#34621=CIRCLE('',#107934,0.127000000000001);
#34622=CIRCLE('',#107935,0.127);
#34623=CIRCLE('',#107937,0.127);
#34624=CIRCLE('',#107940,0.127000000000002);
#34625=CIRCLE('',#107942,0.127000000000001);
#34626=CIRCLE('',#107944,0.126999999999998);
#34627=CIRCLE('',#107945,0.127);
#34628=CIRCLE('',#107946,0.127);
#34629=CIRCLE('',#107948,0.127);
#34630=CIRCLE('',#107951,0.127000000000002);
#34631=CIRCLE('',#107955,0.127000000000001);
#34632=CIRCLE('',#107956,0.127);
#34633=CIRCLE('',#107958,0.126999999999999);
#34634=CIRCLE('',#107960,0.127000000000004);
#34635=CIRCLE('',#107961,0.127000000000001);
#34636=CIRCLE('',#107962,0.126999999999999);
#34637=CIRCLE('',#107964,0.126999999999999);
#34638=CIRCLE('',#107967,0.126999999999995);
#34639=CIRCLE('',#107969,0.127);
#34640=CIRCLE('',#107971,0.126999999999998);
#34641=CIRCLE('',#107972,0.127000000000002);
#34642=CIRCLE('',#107973,0.126999999999998);
#34643=CIRCLE('',#107975,0.126999999999999);
#34644=CIRCLE('',#107977,0.127000000000003);
#34645=CIRCLE('',#107978,0.127000000000001);
#34646=CIRCLE('',#107979,0.126999999999999);
#34647=CIRCLE('',#107981,0.127000000000003);
#34648=CIRCLE('',#107984,0.127);
#34649=CIRCLE('',#107986,0.127000000000001);
#34650=CIRCLE('',#107988,0.127000000000003);
#34651=CIRCLE('',#107989,0.126999999999999);
#34652=CIRCLE('',#107990,0.126999999999999);
#34653=CIRCLE('',#107992,0.126999999999999);
#34654=CIRCLE('',#107995,0.126999999999997);
#34655=CIRCLE('',#107999,0.127);
#34656=CIRCLE('',#108000,0.127);
#34657=CIRCLE('',#108002,0.127);
#34658=CIRCLE('',#108004,0.127);
#34659=CIRCLE('',#108005,0.127);
#34660=CIRCLE('',#108006,0.126999999999999);
#34661=CIRCLE('',#108008,0.126999999999999);
#34662=CIRCLE('',#108011,0.127000000000002);
#34663=CIRCLE('',#108013,0.127);
#34664=CIRCLE('',#108015,0.126999999999999);
#34665=CIRCLE('',#108016,0.126999999999997);
#34666=CIRCLE('',#108017,0.126999999999999);
#34667=CIRCLE('',#108019,0.126999999999999);
#34668=CIRCLE('',#108021,0.126999999999998);
#34669=CIRCLE('',#108022,0.127);
#34670=CIRCLE('',#108023,0.127);
#34671=CIRCLE('',#108025,0.126999999999999);
#34672=CIRCLE('',#108028,0.126999999999999);
#34673=CIRCLE('',#108030,0.127);
#34674=CIRCLE('',#108032,0.127000000000003);
#34675=CIRCLE('',#108033,0.127);
#34676=CIRCLE('',#108034,0.127);
#34677=CIRCLE('',#108036,0.127);
#34678=CIRCLE('',#108039,0.127);
#34679=CIRCLE('',#108043,0.126999999999998);
#34680=CIRCLE('',#108044,0.127000000000001);
#34681=CIRCLE('',#108046,0.127000000000001);
#34682=CIRCLE('',#108048,0.127000000000001);
#34683=CIRCLE('',#108049,0.127000000000002);
#34684=CIRCLE('',#108050,0.127000000000003);
#34685=CIRCLE('',#108052,0.126999999999998);
#34686=CIRCLE('',#108055,0.127000000000001);
#34687=CIRCLE('',#108057,0.127000000000001);
#34688=CIRCLE('',#108059,0.127000000000001);
#34689=CIRCLE('',#108060,0.126999999999999);
#34690=CIRCLE('',#108061,0.126999999999999);
#34691=CIRCLE('',#108063,0.126999999999999);
#34692=CIRCLE('',#108065,0.127000000000002);
#34693=CIRCLE('',#108066,0.126999999999997);
#34694=CIRCLE('',#108067,0.127000000000001);
#34695=CIRCLE('',#108069,0.127000000000001);
#34696=CIRCLE('',#108072,0.126999999999998);
#34697=CIRCLE('',#108074,0.126999999999999);
#34698=CIRCLE('',#108076,0.126999999999998);
#34699=CIRCLE('',#108077,0.127000000000001);
#34700=CIRCLE('',#108078,0.127000000000001);
#34701=CIRCLE('',#108080,0.127000000000001);
#34702=CIRCLE('',#108083,0.127000000000003);
#34703=CIRCLE('',#108087,0.127000000000003);
#34704=CIRCLE('',#108088,0.127000000000002);
#34705=CIRCLE('',#108090,0.126999999999999);
#34706=CIRCLE('',#108092,0.126999999999999);
#34707=CIRCLE('',#108093,0.127000000000002);
#34708=CIRCLE('',#108094,0.127000000000001);
#34709=CIRCLE('',#108096,0.126999999999998);
#34710=CIRCLE('',#108099,0.127);
#34711=CIRCLE('',#108101,0.127);
#34712=CIRCLE('',#108103,0.126999999999998);
#34713=CIRCLE('',#108104,0.127);
#34714=CIRCLE('',#108105,0.126999999999998);
#34715=CIRCLE('',#108107,0.126999999999997);
#34716=CIRCLE('',#108109,0.127);
#34717=CIRCLE('',#108110,0.127);
#34718=CIRCLE('',#108111,0.126999999999999);
#34719=CIRCLE('',#108113,0.127000000000003);
#34720=CIRCLE('',#108116,0.127000000000003);
#34721=CIRCLE('',#108118,0.126999999999999);
#34722=CIRCLE('',#108120,0.127);
#34723=CIRCLE('',#108121,0.126999999999999);
#34724=CIRCLE('',#108122,0.126999999999999);
#34725=CIRCLE('',#108124,0.126999999999999);
#34726=CIRCLE('',#108127,0.127000000000002);
#34727=CIRCLE('',#108131,0.127);
#34728=CIRCLE('',#108132,0.126999999999999);
#34729=CIRCLE('',#108134,0.126999999999999);
#34730=CIRCLE('',#108136,0.126999999999999);
#34731=CIRCLE('',#108137,0.126999999999997);
#34732=CIRCLE('',#108138,0.127000000000003);
#34733=CIRCLE('',#108140,0.127000000000002);
#34734=CIRCLE('',#108143,0.126999999999997);
#34735=CIRCLE('',#108145,0.126999999999999);
#34736=CIRCLE('',#108147,0.127000000000003);
#34737=CIRCLE('',#108148,0.127000000000002);
#34738=CIRCLE('',#108149,0.127000000000001);
#34739=CIRCLE('',#108151,0.127000000000003);
#34740=CIRCLE('',#108153,0.127000000000002);
#34741=CIRCLE('',#108154,0.127);
#34742=CIRCLE('',#108155,0.126999999999999);
#34743=CIRCLE('',#108157,0.127000000000002);
#34744=CIRCLE('',#108160,0.127000000000002);
#34745=CIRCLE('',#108162,0.126999999999997);
#34746=CIRCLE('',#108164,0.126999999999997);
#34747=CIRCLE('',#108165,0.126999999999999);
#34748=CIRCLE('',#108166,0.126999999999999);
#34749=CIRCLE('',#108168,0.126999999999999);
#34750=CIRCLE('',#108171,0.127);
#34751=CIRCLE('',#108175,0.127000000000003);
#34752=CIRCLE('',#108176,0.127);
#34753=CIRCLE('',#108178,0.127);
#34754=CIRCLE('',#108180,0.127);
#34755=CIRCLE('',#108181,0.127000000000001);
#34756=CIRCLE('',#108182,0.127);
#34757=CIRCLE('',#108184,0.126999999999999);
#34758=CIRCLE('',#108187,0.127000000000002);
#34759=CIRCLE('',#108189,0.127);
#34760=CIRCLE('',#108191,0.127000000000004);
#34761=CIRCLE('',#108192,0.127000000000002);
#34762=CIRCLE('',#108193,0.126999999999999);
#34763=CIRCLE('',#108195,0.126999999999999);
#34764=CIRCLE('',#108197,0.126999999999998);
#34765=CIRCLE('',#108198,0.126999999999997);
#34766=CIRCLE('',#108199,0.127);
#34767=CIRCLE('',#108201,0.127);
#34768=CIRCLE('',#108204,0.127);
#34769=CIRCLE('',#108206,0.127000000000001);
#34770=CIRCLE('',#108208,0.126999999999998);
#34771=CIRCLE('',#108209,0.127);
#34772=CIRCLE('',#108210,0.127);
#34773=CIRCLE('',#108212,0.127);
#34774=CIRCLE('',#108215,0.126999999999999);
#34775=CIRCLE('',#108219,0.126999999999999);
#34776=CIRCLE('',#108220,0.127);
#34777=CIRCLE('',#108222,0.127);
#34778=CIRCLE('',#108224,0.127);
#34779=CIRCLE('',#108225,0.126999999999999);
#34780=CIRCLE('',#108226,0.127);
#34781=CIRCLE('',#108228,0.127000000000005);
#34782=CIRCLE('',#108231,0.127000000000002);
#34783=CIRCLE('',#108233,0.127);
#34784=CIRCLE('',#108235,0.127000000000002);
#34785=CIRCLE('',#108236,0.127);
#34786=CIRCLE('',#108237,0.126999999999998);
#34787=CIRCLE('',#108239,0.126999999999998);
#34788=CIRCLE('',#108241,0.126999999999999);
#34789=CIRCLE('',#108242,0.127000000000002);
#34790=CIRCLE('',#108243,0.127);
#34791=CIRCLE('',#108245,0.127000000000002);
#34792=CIRCLE('',#108248,0.126999999999998);
#34793=CIRCLE('',#108250,0.127000000000003);
#34794=CIRCLE('',#108252,0.127);
#34795=CIRCLE('',#108253,0.127);
#34796=CIRCLE('',#108254,0.127);
#34797=CIRCLE('',#108256,0.127);
#34798=CIRCLE('',#108259,0.127);
#34799=CIRCLE('',#108263,0.127000000000003);
#34800=CIRCLE('',#108264,0.127);
#34801=CIRCLE('',#108266,0.127);
#34802=CIRCLE('',#108268,0.127);
#34803=CIRCLE('',#108269,0.127);
#34804=CIRCLE('',#108270,0.126999999999999);
#34805=CIRCLE('',#108272,0.126999999999998);
#34806=CIRCLE('',#108275,0.127000000000004);
#34807=CIRCLE('',#108277,0.127);
#34808=CIRCLE('',#108279,0.127000000000002);
#34809=CIRCLE('',#108280,0.126999999999998);
#34810=CIRCLE('',#108281,0.126999999999999);
#34811=CIRCLE('',#108283,0.127);
#34812=CIRCLE('',#108285,0.127000000000002);
#34813=CIRCLE('',#108286,0.127);
#34814=CIRCLE('',#108287,0.127);
#34815=CIRCLE('',#108289,0.126999999999997);
#34816=CIRCLE('',#108292,0.126999999999999);
#34817=CIRCLE('',#108294,0.127000000000002);
#34818=CIRCLE('',#108296,0.127000000000002);
#34819=CIRCLE('',#108297,0.127);
#34820=CIRCLE('',#108298,0.127);
#34821=CIRCLE('',#108300,0.127);
#34822=CIRCLE('',#108303,0.127000000000002);
#34823=CIRCLE('',#108307,0.127);
#34824=CIRCLE('',#108308,0.126999999999999);
#34825=CIRCLE('',#108310,0.126999999999999);
#34826=CIRCLE('',#108312,0.126999999999999);
#34827=CIRCLE('',#108313,0.127000000000001);
#34828=CIRCLE('',#108314,0.127);
#34829=CIRCLE('',#108316,0.127000000000002);
#34830=CIRCLE('',#108319,0.126999999999997);
#34831=CIRCLE('',#108321,0.126999999999999);
#34832=CIRCLE('',#108323,0.126999999999997);
#34833=CIRCLE('',#108324,0.127);
#34834=CIRCLE('',#108325,0.127000000000003);
#34835=CIRCLE('',#108327,0.127000000000002);
#34836=CIRCLE('',#108329,0.127);
#34837=CIRCLE('',#108330,0.127000000000002);
#34838=CIRCLE('',#108331,0.126999999999999);
#34839=CIRCLE('',#108333,0.127000000000001);
#34840=CIRCLE('',#108336,0.127000000000002);
#34841=CIRCLE('',#108338,0.126999999999998);
#34842=CIRCLE('',#108340,0.127000000000002);
#34843=CIRCLE('',#108341,0.126999999999999);
#34844=CIRCLE('',#108342,0.126999999999999);
#34845=CIRCLE('',#108344,0.126999999999999);
#34846=CIRCLE('',#108347,0.127000000000002);
#34847=CIRCLE('',#108351,0.127000000000002);
#34848=CIRCLE('',#108352,0.126999999999999);
#34849=CIRCLE('',#108354,0.126999999999999);
#34850=CIRCLE('',#108356,0.127);
#34851=CIRCLE('',#108357,0.127);
#34852=CIRCLE('',#108358,0.127000000000001);
#34853=CIRCLE('',#108360,0.126999999999998);
#34854=CIRCLE('',#108363,0.126999999999998);
#34855=CIRCLE('',#108365,0.126999999999999);
#34856=CIRCLE('',#108367,0.127);
#34857=CIRCLE('',#108368,0.127);
#34858=CIRCLE('',#108369,0.127000000000002);
#34859=CIRCLE('',#108371,0.127000000000003);
#34860=CIRCLE('',#108373,0.127000000000002);
#34861=CIRCLE('',#108374,0.126999999999997);
#34862=CIRCLE('',#108375,0.126999999999999);
#34863=CIRCLE('',#108377,0.127);
#34864=CIRCLE('',#108380,0.126999999999997);
#34865=CIRCLE('',#108382,0.127000000000002);
#34866=CIRCLE('',#108384,0.126999999999999);
#34867=CIRCLE('',#108385,0.126999999999999);
#34868=CIRCLE('',#108386,0.126999999999999);
#34869=CIRCLE('',#108388,0.126999999999999);
#34870=CIRCLE('',#108391,0.127000000000001);
#34871=CIRCLE('',#108395,0.126999999999998);
#34872=CIRCLE('',#108396,0.127000000000001);
#34873=CIRCLE('',#108398,0.127000000000001);
#34874=CIRCLE('',#108400,0.127000000000001);
#34875=CIRCLE('',#108401,0.127000000000001);
#34876=CIRCLE('',#108402,0.127);
#34877=CIRCLE('',#108404,0.126999999999999);
#34878=CIRCLE('',#108407,0.127000000000002);
#34879=CIRCLE('',#108409,0.127000000000001);
#34880=CIRCLE('',#108411,0.127000000000001);
#34881=CIRCLE('',#108412,0.126999999999998);
#34882=CIRCLE('',#108413,0.126999999999998);
#34883=CIRCLE('',#108415,0.126999999999999);
#34884=CIRCLE('',#108417,0.127);
#34885=CIRCLE('',#108418,0.127000000000002);
#34886=CIRCLE('',#108419,0.127000000000001);
#34887=CIRCLE('',#108421,0.126999999999998);
#34888=CIRCLE('',#108424,0.126999999999999);
#34889=CIRCLE('',#108426,0.126999999999998);
#34890=CIRCLE('',#108428,0.127000000000002);
#34891=CIRCLE('',#108429,0.127000000000001);
#34892=CIRCLE('',#108430,0.127000000000001);
#34893=CIRCLE('',#108432,0.127000000000001);
#34894=CIRCLE('',#108435,0.126999999999998);
#34895=CIRCLE('',#108439,0.127);
#34896=CIRCLE('',#108440,0.127);
#34897=CIRCLE('',#108442,0.127000000000003);
#34898=CIRCLE('',#108444,0.127);
#34899=CIRCLE('',#108445,0.127000000000001);
#34900=CIRCLE('',#108446,0.127);
#34901=CIRCLE('',#108448,0.127);
#34902=CIRCLE('',#108451,0.126999999999998);
#34903=CIRCLE('',#108453,0.127);
#34904=CIRCLE('',#108455,0.127000000000002);
#34905=CIRCLE('',#108456,0.127000000000001);
#34906=CIRCLE('',#108457,0.127);
#34907=CIRCLE('',#108459,0.127);
#34908=CIRCLE('',#108461,0.127000000000002);
#34909=CIRCLE('',#108462,0.126999999999999);
#34910=CIRCLE('',#108463,0.127);
#34911=CIRCLE('',#108465,0.127);
#34912=CIRCLE('',#108468,0.127);
#34913=CIRCLE('',#108470,0.127000000000001);
#34914=CIRCLE('',#108472,0.127);
#34915=CIRCLE('',#108473,0.127);
#34916=CIRCLE('',#108474,0.127);
#34917=CIRCLE('',#108476,0.127);
#34918=CIRCLE('',#108479,0.127);
#34919=CIRCLE('',#108483,0.127000000000001);
#34920=CIRCLE('',#108484,0.127000000000004);
#34921=CIRCLE('',#108486,0.126999999999999);
#34922=CIRCLE('',#108488,0.127000000000004);
#34923=CIRCLE('',#108489,0.127);
#34924=CIRCLE('',#108490,0.126999999999999);
#34925=CIRCLE('',#108492,0.126999999999999);
#34926=CIRCLE('',#108495,0.126999999999998);
#34927=CIRCLE('',#108497,0.127000000000004);
#34928=CIRCLE('',#108499,0.126999999999995);
#34929=CIRCLE('',#108500,0.127000000000003);
#34930=CIRCLE('',#108501,0.127000000000001);
#34931=CIRCLE('',#108503,0.127);
#34932=CIRCLE('',#108505,0.126999999999999);
#34933=CIRCLE('',#108506,0.127000000000003);
#34934=CIRCLE('',#108507,0.126999999999999);
#34935=CIRCLE('',#108509,0.127);
#34936=CIRCLE('',#108512,0.127000000000001);
#34937=CIRCLE('',#108514,0.126999999999998);
#34938=CIRCLE('',#108516,0.127000000000002);
#34939=CIRCLE('',#108517,0.126999999999999);
#34940=CIRCLE('',#108518,0.126999999999999);
#34941=CIRCLE('',#108520,0.126999999999999);
#34942=CIRCLE('',#108523,0.126999999999999);
#34943=CIRCLE('',#108527,0.127);
#34944=CIRCLE('',#108528,0.127);
#34945=CIRCLE('',#108530,0.127);
#34946=CIRCLE('',#108532,0.127);
#34947=CIRCLE('',#108533,0.126999999999998);
#34948=CIRCLE('',#108534,0.127000000000002);
#34949=CIRCLE('',#108536,0.126999999999999);
#34950=CIRCLE('',#108539,0.126999999999998);
#34951=CIRCLE('',#108541,0.127);
#34952=CIRCLE('',#108543,0.126999999999998);
#34953=CIRCLE('',#108544,0.127);
#34954=CIRCLE('',#108545,0.126999999999999);
#34955=CIRCLE('',#108547,0.127);
#34956=CIRCLE('',#108549,0.126999999999997);
#34957=CIRCLE('',#108550,0.127);
#34958=CIRCLE('',#108551,0.127);
#34959=CIRCLE('',#108553,0.126999999999996);
#34960=CIRCLE('',#108556,0.127000000000003);
#34961=CIRCLE('',#108558,0.126999999999998);
#34962=CIRCLE('',#108560,0.127000000000002);
#34963=CIRCLE('',#108561,0.127);
#34964=CIRCLE('',#108562,0.127);
#34965=CIRCLE('',#108564,0.127);
#34966=CIRCLE('',#108567,0.127000000000002);
#34967=CIRCLE('',#108571,0.127);
#34968=CIRCLE('',#108572,0.127);
#34969=CIRCLE('',#108574,0.127);
#34970=CIRCLE('',#108576,0.127);
#34971=CIRCLE('',#108577,0.127000000000003);
#34972=CIRCLE('',#108578,0.127000000000003);
#34973=CIRCLE('',#108580,0.127000000000003);
#34974=CIRCLE('',#108583,0.126999999999999);
#34975=CIRCLE('',#108585,0.127);
#34976=CIRCLE('',#108587,0.127000000000003);
#34977=CIRCLE('',#108588,0.127000000000003);
#34978=CIRCLE('',#108589,0.127000000000002);
#34979=CIRCLE('',#108591,0.126999999999998);
#34980=CIRCLE('',#108593,0.126999999999998);
#34981=CIRCLE('',#108594,0.127000000000001);
#34982=CIRCLE('',#108595,0.127);
#34983=CIRCLE('',#108597,0.127);
#34984=CIRCLE('',#108600,0.127000000000002);
#34985=CIRCLE('',#108602,0.126999999999999);
#34986=CIRCLE('',#108604,0.127000000000002);
#34987=CIRCLE('',#108605,0.127);
#34988=CIRCLE('',#108606,0.127);
#34989=CIRCLE('',#108608,0.127);
#34990=CIRCLE('',#108611,0.127000000000002);
#34991=CIRCLE('',#108615,0.127000000000002);
#34992=CIRCLE('',#108616,0.127000000000004);
#34993=CIRCLE('',#108618,0.127000000000004);
#34994=CIRCLE('',#108620,0.127);
#34995=CIRCLE('',#108621,0.127);
#34996=CIRCLE('',#108622,0.126999999999998);
#34997=CIRCLE('',#108624,0.127);
#34998=CIRCLE('',#108627,0.126999999999995);
#34999=CIRCLE('',#108629,0.127000000000004);
#35000=CIRCLE('',#108631,0.126999999999998);
#35001=CIRCLE('',#108632,0.126999999999999);
#35002=CIRCLE('',#108633,0.127);
#35003=CIRCLE('',#108635,0.126999999999999);
#35004=CIRCLE('',#108637,0.127000000000001);
#35005=CIRCLE('',#108638,0.127);
#35006=CIRCLE('',#108639,0.127000000000004);
#35007=CIRCLE('',#108641,0.127000000000003);
#35008=CIRCLE('',#108644,0.127000000000001);
#35009=CIRCLE('',#108646,0.127);
#35010=CIRCLE('',#108648,0.127000000000002);
#35011=CIRCLE('',#108649,0.127000000000004);
#35012=CIRCLE('',#108650,0.127);
#35013=CIRCLE('',#108652,0.127000000000004);
#35014=CIRCLE('',#108655,0.126999999999999);
#35015=CIRCLE('',#108659,0.127);
#35016=CIRCLE('',#108660,0.127);
#35017=CIRCLE('',#108662,0.127);
#35018=CIRCLE('',#108664,0.127);
#35019=CIRCLE('',#108665,0.126999999999999);
#35020=CIRCLE('',#108666,0.127);
#35021=CIRCLE('',#108668,0.126999999999999);
#35022=CIRCLE('',#108671,0.127000000000002);
#35023=CIRCLE('',#108673,0.126999999999999);
#35024=CIRCLE('',#108675,0.127000000000002);
#35025=CIRCLE('',#108676,0.127000000000001);
#35026=CIRCLE('',#108677,0.127);
#35027=CIRCLE('',#108679,0.126999999999998);
#35028=CIRCLE('',#108681,0.126999999999999);
#35029=CIRCLE('',#108682,0.127);
#35030=CIRCLE('',#108683,0.127);
#35031=CIRCLE('',#108685,0.126999999999998);
#35032=CIRCLE('',#108688,0.127000000000002);
#35033=CIRCLE('',#108690,0.126999999999997);
#35034=CIRCLE('',#108692,0.127000000000001);
#35035=CIRCLE('',#108693,0.127);
#35036=CIRCLE('',#108694,0.127);
#35037=CIRCLE('',#108696,0.127);
#35038=CIRCLE('',#108699,0.126999999999998);
#35039=CIRCLE('',#108703,0.127);
#35040=CIRCLE('',#108704,0.127000000000001);
#35041=CIRCLE('',#108706,0.127000000000001);
#35042=CIRCLE('',#108708,0.127000000000001);
#35043=CIRCLE('',#108709,0.127);
#35044=CIRCLE('',#108710,0.127000000000002);
#35045=CIRCLE('',#108712,0.126999999999999);
#35046=CIRCLE('',#108715,0.127000000000002);
#35047=CIRCLE('',#108717,0.127000000000001);
#35048=CIRCLE('',#108719,0.127000000000001);
#35049=CIRCLE('',#108720,0.127000000000001);
#35050=CIRCLE('',#108721,0.127);
#35051=CIRCLE('',#108723,0.126999999999998);
#35052=CIRCLE('',#108725,0.126999999999999);
#35053=CIRCLE('',#108726,0.127000000000003);
#35054=CIRCLE('',#108727,0.127000000000001);
#35055=CIRCLE('',#108729,0.127000000000001);
#35056=CIRCLE('',#108732,0.126999999999999);
#35057=CIRCLE('',#108734,0.126999999999998);
#35058=CIRCLE('',#108736,0.126999999999999);
#35059=CIRCLE('',#108737,0.127000000000001);
#35060=CIRCLE('',#108738,0.127000000000001);
#35061=CIRCLE('',#108740,0.127000000000001);
#35062=CIRCLE('',#108743,0.127000000000001);
#35063=CIRCLE('',#108747,0.126999999999998);
#35064=CIRCLE('',#108748,0.126999999999999);
#35065=CIRCLE('',#108750,0.126999999999999);
#35066=CIRCLE('',#108752,0.126999999999999);
#35067=CIRCLE('',#108753,0.127);
#35068=CIRCLE('',#108754,0.127000000000001);
#35069=CIRCLE('',#108756,0.126999999999997);
#35070=CIRCLE('',#108759,0.127);
#35071=CIRCLE('',#108761,0.127);
#35072=CIRCLE('',#108763,0.126999999999998);
#35073=CIRCLE('',#108764,0.127);
#35074=CIRCLE('',#108765,0.126999999999998);
#35075=CIRCLE('',#108767,0.126999999999998);
#35076=CIRCLE('',#108769,0.127000000000002);
#35077=CIRCLE('',#108770,0.126999999999999);
#35078=CIRCLE('',#108771,0.126999999999999);
#35079=CIRCLE('',#108773,0.127000000000002);
#35080=CIRCLE('',#108776,0.126999999999997);
#35081=CIRCLE('',#108778,0.127);
#35082=CIRCLE('',#108780,0.127);
#35083=CIRCLE('',#108781,0.126999999999999);
#35084=CIRCLE('',#108782,0.127);
#35085=CIRCLE('',#108784,0.126999999999999);
#35086=CIRCLE('',#108787,0.127000000000002);
#35087=CIRCLE('',#108791,0.127);
#35088=CIRCLE('',#108792,0.127000000000001);
#35089=CIRCLE('',#108794,0.126999999999999);
#35090=CIRCLE('',#108796,0.127000000000001);
#35091=CIRCLE('',#108797,0.127000000000003);
#35092=CIRCLE('',#108798,0.127);
#35093=CIRCLE('',#108800,0.127000000000001);
#35094=CIRCLE('',#108803,0.126999999999997);
#35095=CIRCLE('',#108805,0.126999999999999);
#35096=CIRCLE('',#108807,0.126999999999997);
#35097=CIRCLE('',#108808,0.126999999999999);
#35098=CIRCLE('',#108809,0.127);
#35099=CIRCLE('',#108811,0.127000000000002);
#35100=CIRCLE('',#108813,0.126999999999999);
#35101=CIRCLE('',#108814,0.127);
#35102=CIRCLE('',#108815,0.126999999999999);
#35103=CIRCLE('',#108817,0.127000000000002);
#35104=CIRCLE('',#108820,0.127000000000003);
#35105=CIRCLE('',#108822,0.127);
#35106=CIRCLE('',#108824,0.126999999999997);
#35107=CIRCLE('',#108825,0.126999999999999);
#35108=CIRCLE('',#108826,0.126999999999999);
#35109=CIRCLE('',#108828,0.126999999999999);
#35110=CIRCLE('',#108831,0.127);
#35111=CIRCLE('',#108835,0.127000000000003);
#35112=CIRCLE('',#108836,0.127);
#35113=CIRCLE('',#108838,0.127);
#35114=CIRCLE('',#108840,0.127);
#35115=CIRCLE('',#108841,0.126999999999997);
#35116=CIRCLE('',#108842,0.127);
#35117=CIRCLE('',#108844,0.126999999999999);
#35118=CIRCLE('',#108847,0.127000000000002);
#35119=CIRCLE('',#108849,0.127);
#35120=CIRCLE('',#108851,0.127000000000004);
#35121=CIRCLE('',#108852,0.127000000000003);
#35122=CIRCLE('',#108853,0.126999999999998);
#35123=CIRCLE('',#108855,0.126999999999999);
#35124=CIRCLE('',#108857,0.126999999999998);
#35125=CIRCLE('',#108858,0.126999999999997);
#35126=CIRCLE('',#108859,0.127);
#35127=CIRCLE('',#108861,0.127);
#35128=CIRCLE('',#108864,0.127);
#35129=CIRCLE('',#108866,0.127000000000002);
#35130=CIRCLE('',#108868,0.126999999999998);
#35131=CIRCLE('',#108869,0.127);
#35132=CIRCLE('',#108870,0.127);
#35133=CIRCLE('',#108872,0.127);
#35134=CIRCLE('',#108875,0.127000000000001);
#35135=CIRCLE('',#108879,0.127);
#35136=CIRCLE('',#108880,0.127);
#35137=CIRCLE('',#108882,0.127);
#35138=CIRCLE('',#108884,0.127);
#35139=CIRCLE('',#108885,0.126999999999999);
#35140=CIRCLE('',#108886,0.127);
#35141=CIRCLE('',#108888,0.127000000000005);
#35142=CIRCLE('',#108892,0.127);
#35143=CIRCLE('',#108893,0.127);
#35144=CIRCLE('',#108894,0.127000000000005);
#35145=CIRCLE('',#108896,0.126999999999998);
#35146=CIRCLE('',#108898,0.126999999999999);
#35147=CIRCLE('',#108899,0.127);
#35148=CIRCLE('',#108902,0.126999999999998);
#35149=CIRCLE('',#108904,0.127);
#35150=CIRCLE('',#108906,0.127);
#35151=CIRCLE('',#108907,0.127);
#35152=CIRCLE('',#108908,0.127);
#35153=CIRCLE('',#108910,0.127);
#35154=CIRCLE('',#108913,0.127000000000001);
#35155=CIRCLE('',#108917,0.126999999999997);
#35156=CIRCLE('',#108918,0.127);
#35157=CIRCLE('',#108920,0.127);
#35158=CIRCLE('',#108922,0.127);
#35159=CIRCLE('',#108923,0.126999999999998);
#35160=CIRCLE('',#108924,0.126999999999999);
#35161=CIRCLE('',#108926,0.126999999999998);
#35162=CIRCLE('',#108929,0.127000000000004);
#35163=CIRCLE('',#108931,0.127);
#35164=CIRCLE('',#108933,0.127000000000002);
#35165=CIRCLE('',#108934,0.126999999999998);
#35166=CIRCLE('',#108935,0.126999999999998);
#35167=CIRCLE('',#108937,0.127);
#35168=CIRCLE('',#108939,0.126999999999998);
#35169=CIRCLE('',#108940,0.127);
#35170=CIRCLE('',#108941,0.127);
#35171=CIRCLE('',#108943,0.126999999999997);
#35172=CIRCLE('',#108946,0.126999999999999);
#35173=CIRCLE('',#108948,0.127000000000002);
#35174=CIRCLE('',#108950,0.127000000000003);
#35175=CIRCLE('',#108951,0.127);
#35176=CIRCLE('',#108952,0.127);
#35177=CIRCLE('',#108954,0.127);
#35178=CIRCLE('',#108957,0.127000000000001);
#35179=CIRCLE('',#108961,0.127);
#35180=CIRCLE('',#108962,0.126999999999999);
#35181=CIRCLE('',#108964,0.126999999999999);
#35182=CIRCLE('',#108966,0.126999999999999);
#35183=CIRCLE('',#108967,0.127000000000003);
#35184=CIRCLE('',#108968,0.127);
#35185=CIRCLE('',#108970,0.127000000000001);
#35186=CIRCLE('',#108973,0.126999999999997);
#35187=CIRCLE('',#108975,0.126999999999999);
#35188=CIRCLE('',#108977,0.126999999999997);
#35189=CIRCLE('',#108978,0.126999999999998);
#35190=CIRCLE('',#108979,0.127000000000002);
#35191=CIRCLE('',#108981,0.127000000000003);
#35192=CIRCLE('',#108983,0.127000000000001);
#35193=CIRCLE('',#108984,0.127000000000002);
#35194=CIRCLE('',#108985,0.126999999999999);
#35195=CIRCLE('',#108987,0.127000000000001);
#35196=CIRCLE('',#108990,0.127000000000003);
#35197=CIRCLE('',#108992,0.127000000000002);
#35198=CIRCLE('',#108994,0.127000000000003);
#35199=CIRCLE('',#108995,0.126999999999999);
#35200=CIRCLE('',#108996,0.126999999999999);
#35201=CIRCLE('',#108998,0.126999999999999);
#35202=CIRCLE('',#109001,0.127000000000001);
#35203=CIRCLE('',#109005,0.127000000000002);
#35204=CIRCLE('',#109006,0.126999999999999);
#35205=CIRCLE('',#109008,0.126999999999999);
#35206=CIRCLE('',#109010,0.127000000000002);
#35207=CIRCLE('',#109011,0.126999999999999);
#35208=CIRCLE('',#109012,0.127);
#35209=CIRCLE('',#109014,0.126999999999997);
#35210=CIRCLE('',#109017,0.126999999999999);
#35211=CIRCLE('',#109019,0.127000000000002);
#35212=CIRCLE('',#109021,0.127000000000001);
#35213=CIRCLE('',#109022,0.127);
#35214=CIRCLE('',#109023,0.127);
#35215=CIRCLE('',#109025,0.126999999999998);
#35216=CIRCLE('',#109027,0.126999999999999);
#35217=CIRCLE('',#109028,0.126999999999997);
#35218=CIRCLE('',#109029,0.126999999999999);
#35219=CIRCLE('',#109031,0.127);
#35220=CIRCLE('',#109034,0.127000000000003);
#35221=CIRCLE('',#109036,0.127);
#35222=CIRCLE('',#109038,0.126999999999999);
#35223=CIRCLE('',#109039,0.126999999999999);
#35224=CIRCLE('',#109040,0.126999999999999);
#35225=CIRCLE('',#109042,0.126999999999999);
#35226=CIRCLE('',#109045,0.127000000000002);
#35227=CIRCLE('',#109049,0.126999999999998);
#35228=CIRCLE('',#109050,0.127000000000001);
#35229=CIRCLE('',#109052,0.127000000000001);
#35230=CIRCLE('',#109054,0.127000000000001);
#35231=CIRCLE('',#109055,0.126999999999999);
#35232=CIRCLE('',#109056,0.127000000000003);
#35233=CIRCLE('',#109058,0.127);
#35234=CIRCLE('',#109061,0.127000000000002);
#35235=CIRCLE('',#109063,0.127000000000001);
#35236=CIRCLE('',#109065,0.127000000000001);
#35237=CIRCLE('',#109066,0.127000000000001);
#35238=CIRCLE('',#109067,0.127000000000001);
#35239=CIRCLE('',#109069,0.127);
#35240=CIRCLE('',#109071,0.127);
#35241=CIRCLE('',#109072,0.127000000000002);
#35242=CIRCLE('',#109073,0.127000000000001);
#35243=CIRCLE('',#109075,0.126999999999998);
#35244=CIRCLE('',#109078,0.126999999999998);
#35245=CIRCLE('',#109080,0.127000000000001);
#35246=CIRCLE('',#109082,0.127000000000003);
#35247=CIRCLE('',#109083,0.127000000000001);
#35248=CIRCLE('',#109084,0.127000000000001);
#35249=CIRCLE('',#109086,0.127000000000001);
#35250=CIRCLE('',#109089,0.127000000000002);
#35251=CIRCLE('',#109093,0.127000000000001);
#35252=CIRCLE('',#109094,0.127);
#35253=CIRCLE('',#109096,0.127000000000003);
#35254=CIRCLE('',#109098,0.127);
#35255=CIRCLE('',#109099,0.126999999999998);
#35256=CIRCLE('',#109100,0.126999999999999);
#35257=CIRCLE('',#109102,0.127000000000001);
#35258=CIRCLE('',#109105,0.127000000000002);
#35259=CIRCLE('',#109107,0.127);
#35260=CIRCLE('',#109109,0.127000000000002);
#35261=CIRCLE('',#109110,0.126999999999999);
#35262=CIRCLE('',#109111,0.127000000000001);
#35263=CIRCLE('',#109113,0.127000000000001);
#35264=CIRCLE('',#109115,0.126999999999999);
#35265=CIRCLE('',#109116,0.126999999999999);
#35266=CIRCLE('',#109117,0.127);
#35267=CIRCLE('',#109119,0.127000000000001);
#35268=CIRCLE('',#109122,0.127);
#35269=CIRCLE('',#109124,0.127);
#35270=CIRCLE('',#109126,0.127);
#35271=CIRCLE('',#109127,0.127);
#35272=CIRCLE('',#109128,0.127);
#35273=CIRCLE('',#109130,0.127);
#35274=CIRCLE('',#109133,0.126999999999998);
#35275=CIRCLE('',#109137,0.127000000000001);
#35276=CIRCLE('',#109138,0.127000000000004);
#35277=CIRCLE('',#109140,0.126999999999999);
#35278=CIRCLE('',#109142,0.127000000000004);
#35279=CIRCLE('',#109143,0.126999999999999);
#35280=CIRCLE('',#109144,0.126999999999999);
#35281=CIRCLE('',#109146,0.126999999999999);
#35282=CIRCLE('',#109149,0.126999999999998);
#35283=CIRCLE('',#109151,0.127000000000003);
#35284=CIRCLE('',#109153,0.126999999999995);
#35285=CIRCLE('',#109154,0.127);
#35286=CIRCLE('',#109155,0.126999999999999);
#35287=CIRCLE('',#109157,0.127);
#35288=CIRCLE('',#109159,0.127000000000001);
#35289=CIRCLE('',#109160,0.127000000000003);
#35290=CIRCLE('',#109161,0.126999999999999);
#35291=CIRCLE('',#109163,0.127);
#35292=CIRCLE('',#109166,0.126999999999999);
#35293=CIRCLE('',#109168,0.127000000000001);
#35294=CIRCLE('',#109170,0.126999999999997);
#35295=CIRCLE('',#109171,0.126999999999999);
#35296=CIRCLE('',#109172,0.126999999999999);
#35297=CIRCLE('',#109174,0.126999999999999);
#35298=CIRCLE('',#109177,0.126999999999997);
#35299=CIRCLE('',#109181,0.126999999999999);
#35300=CIRCLE('',#109182,0.127);
#35301=CIRCLE('',#109184,0.127);
#35302=CIRCLE('',#109186,0.127);
#35303=CIRCLE('',#109187,0.126999999999997);
#35304=CIRCLE('',#109188,0.127000000000002);
#35305=CIRCLE('',#109190,0.127000000000003);
#35306=CIRCLE('',#109193,0.127000000000003);
#35307=CIRCLE('',#109195,0.127);
#35308=CIRCLE('',#109197,0.126999999999998);
#35309=CIRCLE('',#109198,0.127);
#35310=CIRCLE('',#109199,0.126999999999997);
#35311=CIRCLE('',#109201,0.127000000000002);
#35312=CIRCLE('',#109203,0.127000000000002);
#35313=CIRCLE('',#109204,0.127);
#35314=CIRCLE('',#109205,0.127);
#35315=CIRCLE('',#109207,0.126999999999996);
#35316=CIRCLE('',#109210,0.126999999999999);
#35317=CIRCLE('',#109212,0.126999999999997);
#35318=CIRCLE('',#109214,0.127000000000002);
#35319=CIRCLE('',#109215,0.127);
#35320=CIRCLE('',#109216,0.127);
#35321=CIRCLE('',#109218,0.127);
#35322=CIRCLE('',#109221,0.127000000000002);
#35323=CIRCLE('',#109225,0.127);
#35324=CIRCLE('',#109226,0.127);
#35325=CIRCLE('',#109228,0.127);
#35326=CIRCLE('',#109230,0.127);
#35327=CIRCLE('',#109231,0.127000000000002);
#35328=CIRCLE('',#109232,0.127000000000003);
#35329=CIRCLE('',#109234,0.126999999999998);
#35330=CIRCLE('',#109237,0.126999999999999);
#35331=CIRCLE('',#109239,0.127);
#35332=CIRCLE('',#109241,0.127000000000003);
#35333=CIRCLE('',#109242,0.126999999999998);
#35334=CIRCLE('',#109243,0.126999999999998);
#35335=CIRCLE('',#109245,0.126999999999999);
#35336=CIRCLE('',#109247,0.126999999999998);
#35337=CIRCLE('',#109248,0.127000000000001);
#35338=CIRCLE('',#109249,0.127);
#35339=CIRCLE('',#109251,0.127);
#35340=CIRCLE('',#109254,0.127000000000002);
#35341=CIRCLE('',#109256,0.126999999999997);
#35342=CIRCLE('',#109258,0.126999999999998);
#35343=CIRCLE('',#109259,0.127);
#35344=CIRCLE('',#109260,0.127);
#35345=CIRCLE('',#109262,0.127);
#35346=CIRCLE('',#109265,0.127000000000003);
#35347=CIRCLE('',#109269,0.127000000000002);
#35348=CIRCLE('',#109270,0.127000000000004);
#35349=CIRCLE('',#109272,0.127000000000004);
#35350=CIRCLE('',#109274,0.127000000000004);
#35351=CIRCLE('',#109275,0.127);
#35352=CIRCLE('',#109276,0.127000000000001);
#35353=CIRCLE('',#109278,0.126999999999999);
#35354=CIRCLE('',#109281,0.126999999999995);
#35355=CIRCLE('',#109283,0.127000000000004);
#35356=CIRCLE('',#109285,0.126999999999998);
#35357=CIRCLE('',#109286,0.127000000000002);
#35358=CIRCLE('',#109287,0.126999999999997);
#35359=CIRCLE('',#109289,0.127);
#35360=CIRCLE('',#109291,0.127);
#35361=CIRCLE('',#109292,0.127);
#35362=CIRCLE('',#109293,0.127000000000004);
#35363=CIRCLE('',#109295,0.127000000000003);
#35364=CIRCLE('',#109298,0.127000000000002);
#35365=CIRCLE('',#109300,0.126999999999999);
#35366=CIRCLE('',#109302,0.126999999999999);
#35367=CIRCLE('',#109303,0.127000000000004);
#35368=CIRCLE('',#109304,0.126999999999999);
#35369=CIRCLE('',#109306,0.127000000000004);
#35370=CIRCLE('',#109309,0.126999999999997);
#35371=CIRCLE('',#109313,0.127000000000002);
#35372=CIRCLE('',#109314,0.127);
#35373=CIRCLE('',#109316,0.127);
#35374=CIRCLE('',#109318,0.127);
#35375=CIRCLE('',#109319,0.126999999999998);
#35376=CIRCLE('',#109320,0.127000000000001);
#35377=CIRCLE('',#109322,0.126999999999999);
#35378=CIRCLE('',#109325,0.127000000000002);
#35379=CIRCLE('',#109327,0.127);
#35380=CIRCLE('',#109329,0.127000000000002);
#35381=CIRCLE('',#109330,0.127000000000002);
#35382=CIRCLE('',#109331,0.126999999999999);
#35383=CIRCLE('',#109333,0.127);
#35384=CIRCLE('',#109335,0.127000000000001);
#35385=CIRCLE('',#109336,0.127);
#35386=CIRCLE('',#109337,0.127000000000003);
#35387=CIRCLE('',#109339,0.126999999999999);
#35388=CIRCLE('',#109342,0.127000000000002);
#35389=CIRCLE('',#109344,0.126999999999998);
#35390=CIRCLE('',#109346,0.127000000000001);
#35391=CIRCLE('',#109347,0.127);
#35392=CIRCLE('',#109348,0.127);
#35393=CIRCLE('',#109350,0.127);
#35394=CIRCLE('',#109353,0.127000000000002);
#35395=CIRCLE('',#109357,0.126999999999999);
#35396=CIRCLE('',#109358,0.127000000000001);
#35397=CIRCLE('',#109360,0.127000000000001);
#35398=CIRCLE('',#109362,0.127000000000001);
#35399=CIRCLE('',#109363,0.127000000000002);
#35400=CIRCLE('',#109364,0.127000000000002);
#35401=CIRCLE('',#109366,0.126999999999999);
#35402=CIRCLE('',#109369,0.126999999999999);
#35403=CIRCLE('',#109371,0.127000000000001);
#35404=CIRCLE('',#109373,0.127000000000002);
#35405=CIRCLE('',#109374,0.127000000000001);
#35406=CIRCLE('',#109375,0.126999999999999);
#35407=CIRCLE('',#109377,0.126999999999999);
#35408=CIRCLE('',#109379,0.127);
#35409=CIRCLE('',#109380,0.127000000000003);
#35410=CIRCLE('',#109381,0.127000000000001);
#35411=CIRCLE('',#109383,0.127000000000001);
#35412=CIRCLE('',#109386,0.126999999999999);
#35413=CIRCLE('',#109388,0.127000000000002);
#35414=CIRCLE('',#109390,0.127);
#35415=CIRCLE('',#109391,0.127000000000001);
#35416=CIRCLE('',#109392,0.127000000000001);
#35417=CIRCLE('',#109394,0.127000000000001);
#35418=CIRCLE('',#109397,0.127000000000002);
#35419=CIRCLE('',#109401,0.126999999999998);
#35420=CIRCLE('',#109402,0.127);
#35421=CIRCLE('',#109404,0.127);
#35422=CIRCLE('',#109406,0.126999999999999);
#35423=CIRCLE('',#109407,0.127);
#35424=CIRCLE('',#109408,0.127000000000001);
#35425=CIRCLE('',#109410,0.126999999999998);
#35426=CIRCLE('',#109413,0.127);
#35427=CIRCLE('',#109415,0.127);
#35428=CIRCLE('',#109417,0.126999999999998);
#35429=CIRCLE('',#109418,0.126999999999997);
#35430=CIRCLE('',#109419,0.127000000000003);
#35431=CIRCLE('',#109421,0.126999999999999);
#35432=CIRCLE('',#109423,0.127000000000002);
#35433=CIRCLE('',#109424,0.126999999999999);
#35434=CIRCLE('',#109425,0.127);
#35435=CIRCLE('',#109427,0.127000000000002);
#35436=CIRCLE('',#109430,0.126999999999999);
#35437=CIRCLE('',#109432,0.127000000000003);
#35438=CIRCLE('',#109434,0.127);
#35439=CIRCLE('',#109435,0.127);
#35440=CIRCLE('',#109436,0.127);
#35441=CIRCLE('',#109438,0.127);
#35442=CIRCLE('',#109441,0.127);
#35443=CIRCLE('',#109445,0.127);
#35444=CIRCLE('',#109446,0.126999999999999);
#35445=CIRCLE('',#109448,0.126999999999999);
#35446=CIRCLE('',#109450,0.126999999999999);
#35447=CIRCLE('',#109451,0.127000000000001);
#35448=CIRCLE('',#109452,0.126999999999999);
#35449=CIRCLE('',#109454,0.126999999999997);
#35450=CIRCLE('',#109457,0.127000000000003);
#35451=CIRCLE('',#109459,0.126999999999999);
#35452=CIRCLE('',#109461,0.126999999999996);
#35453=CIRCLE('',#109462,0.127);
#35454=CIRCLE('',#109463,0.127000000000001);
#35455=CIRCLE('',#109465,0.126999999999997);
#35456=CIRCLE('',#109467,0.127000000000002);
#35457=CIRCLE('',#109468,0.127);
#35458=CIRCLE('',#109469,0.126999999999999);
#35459=CIRCLE('',#109471,0.127000000000002);
#35460=CIRCLE('',#109474,0.126999999999998);
#35461=CIRCLE('',#109476,0.127);
#35462=CIRCLE('',#109478,0.126999999999999);
#35463=CIRCLE('',#109479,0.126999999999999);
#35464=CIRCLE('',#109480,0.126999999999999);
#35465=CIRCLE('',#109482,0.126999999999999);
#35466=CIRCLE('',#109485,0.127);
#35467=CIRCLE('',#109489,0.126999999999998);
#35468=CIRCLE('',#109490,0.127);
#35469=CIRCLE('',#109492,0.127);
#35470=CIRCLE('',#109494,0.127);
#35471=CIRCLE('',#109495,0.127000000000003);
#35472=CIRCLE('',#109496,0.126999999999999);
#35473=CIRCLE('',#109498,0.127);
#35474=CIRCLE('',#109501,0.127000000000002);
#35475=CIRCLE('',#109503,0.127);
#35476=CIRCLE('',#109505,0.127000000000004);
#35477=CIRCLE('',#109506,0.127);
#35478=CIRCLE('',#109507,0.126999999999999);
#35479=CIRCLE('',#109509,0.127);
#35480=CIRCLE('',#109511,0.127000000000001);
#35481=CIRCLE('',#109512,0.126999999999997);
#35482=CIRCLE('',#109513,0.127);
#35483=CIRCLE('',#109515,0.127);
#35484=CIRCLE('',#109518,0.127000000000001);
#35485=CIRCLE('',#109520,0.127000000000003);
#35486=CIRCLE('',#109522,0.126999999999999);
#35487=CIRCLE('',#109523,0.127);
#35488=CIRCLE('',#109524,0.127);
#35489=CIRCLE('',#109526,0.127);
#35490=CIRCLE('',#109529,0.126999999999998);
#35491=CIRCLE('',#109533,0.127);
#35492=CIRCLE('',#109534,0.127);
#35493=CIRCLE('',#109536,0.127);
#35494=CIRCLE('',#109538,0.127);
#35495=CIRCLE('',#109539,0.126999999999999);
#35496=CIRCLE('',#109540,0.126999999999999);
#35497=CIRCLE('',#109542,0.127000000000004);
#35498=CIRCLE('',#109546,0.127);
#35499=CIRCLE('',#109547,0.127);
#35500=CIRCLE('',#109548,0.127000000000004);
#35501=CIRCLE('',#109550,0.126999999999999);
#35502=CIRCLE('',#109552,0.126999999999999);
#35503=CIRCLE('',#109553,0.127);
#35504=CIRCLE('',#109556,0.126999999999999);
#35505=CIRCLE('',#109558,0.126999999999999);
#35506=CIRCLE('',#109560,0.127);
#35507=CIRCLE('',#109561,0.127);
#35508=CIRCLE('',#109562,0.127);
#35509=CIRCLE('',#109564,0.127);
#35510=CIRCLE('',#109567,0.126999999999999);
#35511=CIRCLE('',#109571,0.126999999999998);
#35512=CIRCLE('',#109572,0.127);
#35513=CIRCLE('',#109574,0.127);
#35514=CIRCLE('',#109576,0.127);
#35515=CIRCLE('',#109577,0.126999999999997);
#35516=CIRCLE('',#109578,0.127);
#35517=CIRCLE('',#109580,0.126999999999998);
#35518=CIRCLE('',#109583,0.127000000000004);
#35519=CIRCLE('',#109585,0.127);
#35520=CIRCLE('',#109587,0.127000000000002);
#35521=CIRCLE('',#109588,0.126999999999998);
#35522=CIRCLE('',#109589,0.126999999999998);
#35523=CIRCLE('',#109591,0.127);
#35524=CIRCLE('',#109593,0.127000000000002);
#35525=CIRCLE('',#109594,0.127);
#35526=CIRCLE('',#109595,0.127);
#35527=CIRCLE('',#109597,0.126999999999997);
#35528=CIRCLE('',#109600,0.127);
#35529=CIRCLE('',#109602,0.127000000000002);
#35530=CIRCLE('',#109604,0.126999999999997);
#35531=CIRCLE('',#109605,0.127);
#35532=CIRCLE('',#109606,0.127);
#35533=CIRCLE('',#109608,0.127);
#35534=CIRCLE('',#109611,0.126999999999998);
#35535=CIRCLE('',#109615,0.127);
#35536=CIRCLE('',#109616,0.126999999999999);
#35537=CIRCLE('',#109618,0.126999999999999);
#35538=CIRCLE('',#109620,0.126999999999999);
#35539=CIRCLE('',#109621,0.127000000000002);
#35540=CIRCLE('',#109622,0.126999999999999);
#35541=CIRCLE('',#109624,0.127);
#35542=CIRCLE('',#109627,0.126999999999997);
#35543=CIRCLE('',#109629,0.127000000000001);
#35544=CIRCLE('',#109631,0.126999999999997);
#35545=CIRCLE('',#109632,0.126999999999998);
#35546=CIRCLE('',#109633,0.126999999999999);
#35547=CIRCLE('',#109635,0.127000000000003);
#35548=CIRCLE('',#109637,0.127000000000002);
#35549=CIRCLE('',#109638,0.127000000000002);
#35550=CIRCLE('',#109639,0.126999999999999);
#35551=CIRCLE('',#109641,0.127000000000001);
#35552=CIRCLE('',#109644,0.127000000000002);
#35553=CIRCLE('',#109646,0.127);
#35554=CIRCLE('',#109648,0.126999999999998);
#35555=CIRCLE('',#109649,0.126999999999999);
#35556=CIRCLE('',#109650,0.126999999999999);
#35557=CIRCLE('',#109652,0.126999999999999);
#35558=CIRCLE('',#109655,0.126999999999999);
#35559=CIRCLE('',#109659,0.126999999999997);
#35560=CIRCLE('',#109660,0.126999999999999);
#35561=CIRCLE('',#109662,0.126999999999999);
#35562=CIRCLE('',#109664,0.127);
#35563=CIRCLE('',#109665,0.126999999999998);
#35564=CIRCLE('',#109666,0.126999999999997);
#35565=CIRCLE('',#109668,0.127000000000002);
#35566=CIRCLE('',#109671,0.126999999999998);
#35567=CIRCLE('',#109673,0.126999999999999);
#35568=CIRCLE('',#109675,0.127000000000001);
#35569=CIRCLE('',#109676,0.127000000000002);
#35570=CIRCLE('',#109677,0.127000000000001);
#35571=CIRCLE('',#109679,0.126999999999997);
#35572=CIRCLE('',#109681,0.126999999999999);
#35573=CIRCLE('',#109682,0.126999999999997);
#35574=CIRCLE('',#109683,0.126999999999999);
#35575=CIRCLE('',#109685,0.127);
#35576=CIRCLE('',#109688,0.126999999999999);
#35577=CIRCLE('',#109690,0.126999999999999);
#35578=CIRCLE('',#109692,0.127);
#35579=CIRCLE('',#109693,0.126999999999999);
#35580=CIRCLE('',#109694,0.126999999999999);
#35581=CIRCLE('',#109696,0.126999999999999);
#35582=CIRCLE('',#109699,0.127000000000001);
#35583=CIRCLE('',#109703,0.126999999999999);
#35584=CIRCLE('',#109704,0.127000000000001);
#35585=CIRCLE('',#109706,0.127000000000001);
#35586=CIRCLE('',#109708,0.127000000000001);
#35587=CIRCLE('',#109709,0.127000000000001);
#35588=CIRCLE('',#109710,0.127000000000003);
#35589=CIRCLE('',#109712,0.127000000000003);
#35590=CIRCLE('',#109715,0.127000000000002);
#35591=CIRCLE('',#109717,0.127000000000001);
#35592=CIRCLE('',#109719,0.127000000000001);
#35593=CIRCLE('',#109720,0.126999999999998);
#35594=CIRCLE('',#109721,0.126999999999998);
#35595=CIRCLE('',#109723,0.126999999999999);
#35596=CIRCLE('',#109725,0.127000000000002);
#35597=CIRCLE('',#109726,0.127000000000001);
#35598=CIRCLE('',#109727,0.127000000000001);
#35599=CIRCLE('',#109729,0.126999999999998);
#35600=CIRCLE('',#109732,0.127);
#35601=CIRCLE('',#109734,0.127000000000003);
#35602=CIRCLE('',#109736,0.126999999999997);
#35603=CIRCLE('',#109737,0.127000000000001);
#35604=CIRCLE('',#109738,0.127000000000001);
#35605=CIRCLE('',#109740,0.127000000000001);
#35606=CIRCLE('',#109743,0.127000000000002);
#35607=CIRCLE('',#109747,0.127000000000001);
#35608=CIRCLE('',#109748,0.127);
#35609=CIRCLE('',#109750,0.127000000000003);
#35610=CIRCLE('',#109752,0.127);
#35611=CIRCLE('',#109753,0.127);
#35612=CIRCLE('',#109754,0.126999999999999);
#35613=CIRCLE('',#109756,0.126999999999999);
#35614=CIRCLE('',#109759,0.126999999999998);
#35615=CIRCLE('',#109761,0.127);
#35616=CIRCLE('',#109763,0.126999999999996);
#35617=CIRCLE('',#109764,0.127000000000001);
#35618=CIRCLE('',#109765,0.126999999999998);
#35619=CIRCLE('',#109767,0.127000000000001);
#35620=CIRCLE('',#109769,0.127000000000002);
#35621=CIRCLE('',#109770,0.126999999999999);
#35622=CIRCLE('',#109771,0.127);
#35623=CIRCLE('',#109773,0.127000000000001);
#35624=CIRCLE('',#109776,0.126999999999999);
#35625=CIRCLE('',#109778,0.127000000000002);
#35626=CIRCLE('',#109780,0.127000000000001);
#35627=CIRCLE('',#109781,0.127);
#35628=CIRCLE('',#109782,0.127);
#35629=CIRCLE('',#109784,0.127);
#35630=CIRCLE('',#109787,0.126999999999997);
#35631=CIRCLE('',#109791,0.127000000000002);
#35632=CIRCLE('',#109792,0.126999999999999);
#35633=CIRCLE('',#109794,0.126999999999999);
#35634=CIRCLE('',#109796,0.127000000000004);
#35635=CIRCLE('',#109797,0.126999999999999);
#35636=CIRCLE('',#109798,0.126999999999998);
#35637=CIRCLE('',#109800,0.126999999999999);
#35638=CIRCLE('',#109803,0.126999999999998);
#35639=CIRCLE('',#109805,0.127000000000004);
#35640=CIRCLE('',#109807,0.127);
#35641=CIRCLE('',#109808,0.126999999999998);
#35642=CIRCLE('',#109809,0.126999999999998);
#35643=CIRCLE('',#109811,0.127000000000002);
#35644=CIRCLE('',#109813,0.126999999999997);
#35645=CIRCLE('',#109814,0.127000000000003);
#35646=CIRCLE('',#109815,0.126999999999999);
#35647=CIRCLE('',#109817,0.127);
#35648=CIRCLE('',#109820,0.127000000000001);
#35649=CIRCLE('',#109822,0.126999999999997);
#35650=CIRCLE('',#109824,0.127000000000001);
#35651=CIRCLE('',#109825,0.126999999999999);
#35652=CIRCLE('',#109826,0.126999999999999);
#35653=CIRCLE('',#109828,0.126999999999999);
#35654=CIRCLE('',#109831,0.126999999999998);
#35655=CIRCLE('',#109835,0.126999999999999);
#35656=CIRCLE('',#109836,0.127);
#35657=CIRCLE('',#109838,0.127);
#35658=CIRCLE('',#109840,0.127);
#35659=CIRCLE('',#109841,0.127000000000002);
#35660=CIRCLE('',#109842,0.127000000000001);
#35661=CIRCLE('',#109844,0.126999999999998);
#35662=CIRCLE('',#109847,0.126999999999998);
#35663=CIRCLE('',#109849,0.127);
#35664=CIRCLE('',#109851,0.126999999999998);
#35665=CIRCLE('',#109852,0.127);
#35666=CIRCLE('',#109853,0.126999999999999);
#35667=CIRCLE('',#109855,0.127000000000002);
#35668=CIRCLE('',#109857,0.127000000000001);
#35669=CIRCLE('',#109858,0.127);
#35670=CIRCLE('',#109859,0.127);
#35671=CIRCLE('',#109861,0.126999999999996);
#35672=CIRCLE('',#109864,0.126999999999998);
#35673=CIRCLE('',#109866,0.127000000000001);
#35674=CIRCLE('',#109868,0.127000000000001);
#35675=CIRCLE('',#109869,0.127);
#35676=CIRCLE('',#109870,0.127);
#35677=CIRCLE('',#109872,0.127);
#35678=CIRCLE('',#109875,0.127000000000001);
#35679=CIRCLE('',#109879,0.127);
#35680=CIRCLE('',#109880,0.127);
#35681=CIRCLE('',#109882,0.127);
#35682=CIRCLE('',#109884,0.127);
#35683=CIRCLE('',#109885,0.127000000000002);
#35684=CIRCLE('',#109886,0.127000000000002);
#35685=CIRCLE('',#109888,0.126999999999998);
#35686=CIRCLE('',#109891,0.126999999999999);
#35687=CIRCLE('',#109893,0.127);
#35688=CIRCLE('',#109895,0.127000000000003);
#35689=CIRCLE('',#109896,0.126999999999997);
#35690=CIRCLE('',#109897,0.126999999999998);
#35691=CIRCLE('',#109899,0.126999999999999);
#35692=CIRCLE('',#109901,0.127);
#35693=CIRCLE('',#109902,0.127000000000001);
#35694=CIRCLE('',#109903,0.127);
#35695=CIRCLE('',#109905,0.127);
#35696=CIRCLE('',#109908,0.127000000000002);
#35697=CIRCLE('',#109910,0.126999999999997);
#35698=CIRCLE('',#109912,0.126999999999997);
#35699=CIRCLE('',#109913,0.127);
#35700=CIRCLE('',#109914,0.127);
#35701=CIRCLE('',#109916,0.127);
#35702=CIRCLE('',#109919,0.127000000000002);
#35703=CIRCLE('',#109923,0.127000000000002);
#35704=CIRCLE('',#109924,0.127000000000004);
#35705=CIRCLE('',#109926,0.127000000000004);
#35706=CIRCLE('',#109928,0.127000000000004);
#35707=CIRCLE('',#109929,0.127);
#35708=CIRCLE('',#109930,0.126999999999998);
#35709=CIRCLE('',#109932,0.127);
#35710=CIRCLE('',#109935,0.127000000000001);
#35711=CIRCLE('',#109937,0.127000000000004);
#35712=CIRCLE('',#109939,0.126999999999998);
#35713=CIRCLE('',#109940,0.126999999999999);
#35714=CIRCLE('',#109941,0.127);
#35715=CIRCLE('',#109943,0.126999999999999);
#35716=CIRCLE('',#109945,0.127000000000002);
#35717=CIRCLE('',#109946,0.126999999999996);
#35718=CIRCLE('',#109947,0.127000000000004);
#35719=CIRCLE('',#109949,0.127000000000003);
#35720=CIRCLE('',#109952,0.127);
#35721=CIRCLE('',#109954,0.127000000000002);
#35722=CIRCLE('',#109956,0.127);
#35723=CIRCLE('',#109957,0.127000000000004);
#35724=CIRCLE('',#109958,0.127);
#35725=CIRCLE('',#109960,0.127000000000004);
#35726=CIRCLE('',#109963,0.126999999999997);
#35727=CIRCLE('',#109967,0.127);
#35728=CIRCLE('',#109968,0.127);
#35729=CIRCLE('',#109970,0.127);
#35730=CIRCLE('',#109972,0.126999999999999);
#35731=CIRCLE('',#109973,0.126999999999999);
#35732=CIRCLE('',#109974,0.126999999999999);
#35733=CIRCLE('',#109976,0.126999999999998);
#35734=CIRCLE('',#109979,0.127000000000002);
#35735=CIRCLE('',#109981,0.127);
#35736=CIRCLE('',#109983,0.127000000000002);
#35737=CIRCLE('',#109984,0.127000000000002);
#35738=CIRCLE('',#109985,0.127);
#35739=CIRCLE('',#109987,0.126999999999999);
#35740=CIRCLE('',#109989,0.127);
#35741=CIRCLE('',#109990,0.127);
#35742=CIRCLE('',#109991,0.127);
#35743=CIRCLE('',#109993,0.126999999999998);
#35744=CIRCLE('',#109996,0.127);
#35745=CIRCLE('',#109998,0.127000000000002);
#35746=CIRCLE('',#110000,0.127000000000002);
#35747=CIRCLE('',#110001,0.127);
#35748=CIRCLE('',#110002,0.127);
#35749=CIRCLE('',#110004,0.127);
#35750=CIRCLE('',#110007,0.127000000000003);
#35751=CIRCLE('',#110011,0.126999999999998);
#35752=CIRCLE('',#110012,0.127000000000001);
#35753=CIRCLE('',#110014,0.127000000000001);
#35754=CIRCLE('',#110016,0.127000000000001);
#35755=CIRCLE('',#110017,0.127);
#35756=CIRCLE('',#110018,0.127000000000002);
#35757=CIRCLE('',#110020,0.126999999999999);
#35758=CIRCLE('',#110023,0.127000000000001);
#35759=CIRCLE('',#110025,0.126999999999998);
#35760=CIRCLE('',#110027,0.127000000000001);
#35761=CIRCLE('',#110028,0.127);
#35762=CIRCLE('',#110029,0.126999999999999);
#35763=CIRCLE('',#110031,0.126999999999998);
#35764=CIRCLE('',#110033,0.126999999999999);
#35765=CIRCLE('',#110034,0.127000000000003);
#35766=CIRCLE('',#110035,0.127000000000001);
#35767=CIRCLE('',#110037,0.127000000000001);
#35768=CIRCLE('',#110040,0.127);
#35769=CIRCLE('',#110042,0.126999999999999);
#35770=CIRCLE('',#110044,0.126999999999999);
#35771=CIRCLE('',#110045,0.127000000000001);
#35772=CIRCLE('',#110046,0.127000000000001);
#35773=CIRCLE('',#110048,0.127000000000001);
#35774=CIRCLE('',#110051,0.127000000000002);
#35775=CIRCLE('',#110055,0.127000000000001);
#35776=CIRCLE('',#110056,0.127);
#35777=CIRCLE('',#110058,0.127);
#35778=CIRCLE('',#110060,0.127);
#35779=CIRCLE('',#110061,0.127000000000001);
#35780=CIRCLE('',#110062,0.126999999999997);
#35781=CIRCLE('',#110064,0.126999999999999);
#35782=CIRCLE('',#110067,0.127);
#35783=CIRCLE('',#110069,0.127);
#35784=CIRCLE('',#110071,0.126999999999998);
#35785=CIRCLE('',#110072,0.127);
#35786=CIRCLE('',#110073,0.126999999999998);
#35787=CIRCLE('',#110075,0.126999999999998);
#35788=CIRCLE('',#110077,0.127);
#35789=CIRCLE('',#110078,0.126999999999999);
#35790=CIRCLE('',#110079,0.127);
#35791=CIRCLE('',#110081,0.127000000000002);
#35792=CIRCLE('',#110084,0.126999999999998);
#35793=CIRCLE('',#110086,0.127);
#35794=CIRCLE('',#110088,0.126999999999999);
#35795=CIRCLE('',#110089,0.127);
#35796=CIRCLE('',#110090,0.127);
#35797=CIRCLE('',#110092,0.127);
#35798=CIRCLE('',#110095,0.127000000000002);
#35799=CIRCLE('',#110099,0.127);
#35800=CIRCLE('',#110100,0.126999999999999);
#35801=CIRCLE('',#110102,0.126999999999999);
#35802=CIRCLE('',#110104,0.126999999999999);
#35803=CIRCLE('',#110105,0.127000000000002);
#35804=CIRCLE('',#110106,0.127000000000002);
#35805=CIRCLE('',#110108,0.127000000000001);
#35806=CIRCLE('',#110111,0.127000000000003);
#35807=CIRCLE('',#110113,0.126999999999999);
#35808=CIRCLE('',#110115,0.126999999999996);
#35809=CIRCLE('',#110116,0.127000000000003);
#35810=CIRCLE('',#110117,0.127);
#35811=CIRCLE('',#110119,0.127000000000003);
#35812=CIRCLE('',#110121,0.127000000000002);
#35813=CIRCLE('',#110122,0.127);
#35814=CIRCLE('',#110123,0.126999999999999);
#35815=CIRCLE('',#110125,0.127000000000002);
#35816=CIRCLE('',#110128,0.127000000000003);
#35817=CIRCLE('',#110130,0.126999999999998);
#35818=CIRCLE('',#110132,0.126999999999998);
#35819=CIRCLE('',#110133,0.126999999999999);
#35820=CIRCLE('',#110134,0.126999999999999);
#35821=CIRCLE('',#110136,0.126999999999999);
#35822=CIRCLE('',#110139,0.127);
#35823=CIRCLE('',#110143,0.126999999999997);
#35824=CIRCLE('',#110144,0.127);
#35825=CIRCLE('',#110146,0.127);
#35826=CIRCLE('',#110148,0.127);
#35827=CIRCLE('',#110149,0.126999999999997);
#35828=CIRCLE('',#110150,0.127);
#35829=CIRCLE('',#110152,0.126999999999999);
#35830=CIRCLE('',#110155,0.127000000000002);
#35831=CIRCLE('',#110157,0.127);
#35832=CIRCLE('',#110159,0.127000000000004);
#35833=CIRCLE('',#110160,0.127);
#35834=CIRCLE('',#110161,0.126999999999999);
#35835=CIRCLE('',#110163,0.127);
#35836=CIRCLE('',#110165,0.126999999999998);
#35837=CIRCLE('',#110166,0.126999999999997);
#35838=CIRCLE('',#110167,0.127);
#35839=CIRCLE('',#110169,0.127);
#35840=CIRCLE('',#110172,0.127);
#35841=CIRCLE('',#110174,0.127);
#35842=CIRCLE('',#110176,0.126999999999998);
#35843=CIRCLE('',#110177,0.127);
#35844=CIRCLE('',#110178,0.127);
#35845=CIRCLE('',#110180,0.127);
#35846=CIRCLE('',#110183,0.126999999999999);
#35847=CIRCLE('',#110186,65.254);
#35848=CIRCLE('',#110187,0.127);
#35849=CIRCLE('',#110188,65.381);
#35850=CIRCLE('',#110190,68.623);
#35851=CIRCLE('',#110191,0.127);
#35852=CIRCLE('',#110192,68.75);
#35853=CIRCLE('',#110194,68.877);
#35854=CIRCLE('',#110195,0.127);
#35855=CIRCLE('',#110196,68.75);
#35856=CIRCLE('',#110197,68.75);
#35857=CIRCLE('',#110199,65.254);
#35858=CIRCLE('',#110202,72.53);
#35859=CIRCLE('',#110203,72.53);
#35860=CIRCLE('',#110208,65.);
#35861=CIRCLE('',#110209,0.0762);
#35862=CIRCLE('',#110210,65.0762);
#35863=CIRCLE('',#110212,65.1778);
#35864=CIRCLE('',#110213,0.0762);
#35865=CIRCLE('',#110214,65.254);
#35866=CIRCLE('',#110216,65.);
#35867=CIRCLE('',#110218,65.254);
#35868=CIRCLE('',#110222,70.625);
#35869=CIRCLE('',#110223,0.8255);
#35870=CIRCLE('',#110224,71.3206076480316);
#35871=CIRCLE('',#110226,77.1551372062631);
#35872=CIRCLE('',#110227,2.53999999999999);
#35873=CIRCLE('',#110228,74.6340699810941);
#35874=CIRCLE('',#110229,2.54);
#35875=CIRCLE('',#110231,25.);
#35876=CIRCLE('',#110232,1.27);
#35877=CIRCLE('',#110233,23.73);
#35878=CIRCLE('',#110234,1.27);
#35879=CIRCLE('',#110236,25.);
#35880=CIRCLE('',#110237,1.27);
#35881=CIRCLE('',#110238,23.73);
#35882=CIRCLE('',#110239,1.27);
#35883=CIRCLE('',#110240,0.634999999999997);
#35884=CIRCLE('',#110241,1.905);
#35885=CIRCLE('',#110242,2.54);
#35886=CIRCLE('',#110243,1.905);
#35887=CIRCLE('',#110244,0.634999999999997);
#35888=CIRCLE('',#110245,1.905);
#35889=CIRCLE('',#110246,2.54);
#35890=CIRCLE('',#110247,1.905);
#35891=CIRCLE('',#110248,0.634999999999997);
#35892=CIRCLE('',#110249,1.905);
#35893=CIRCLE('',#110250,2.54);
#35894=CIRCLE('',#110251,1.905);
#35895=CIRCLE('',#110253,80.);
#35896=CIRCLE('',#110254,81.905);
#35897=CIRCLE('',#110255,1.905);
#35898=CIRCLE('',#110256,0.634999999999997);
#35899=CIRCLE('',#110257,1.905);
#35900=CIRCLE('',#110258,2.54);
#35901=CIRCLE('',#110260,2.54);
#35902=CIRCLE('',#110262,2.54);
#35903=CIRCLE('',#110264,79.9526680629224);
#35904=CIRCLE('',#110265,80.);
#35905=CIRCLE('',#110267,72.53);
#35906=CIRCLE('',#110268,72.53);
#35907=CIRCLE('',#110270,8.4455);
#35908=CIRCLE('',#110271,8.4455);
#35909=CIRCLE('',#110273,8.4455);
#35910=CIRCLE('',#110274,8.4455);
#35911=CIRCLE('',#110276,8.4455);
#35912=CIRCLE('',#110277,8.4455);
#35913=CIRCLE('',#110279,8.4455);
#35914=CIRCLE('',#110280,8.4455);
#35915=CIRCLE('',#110282,80.);
#35916=CIRCLE('',#110284,79.9526680629224);
#35917=CIRCLE('',#110285,79.7261349468031);
#35918=CIRCLE('',#110286,79.7261349468031);
#35919=CIRCLE('',#110287,79.9526680629224);
#35920=CIRCLE('',#110288,79.7261349468031);
#35921=CIRCLE('',#110289,79.9526680629224);
#35922=CIRCLE('',#110290,79.7261349468032);
#35923=CIRCLE('',#110291,79.9526680629224);
#35924=CIRCLE('',#110293,25.);
#35925=CIRCLE('',#110294,25.);
#35926=CIRCLE('',#110295,25.);
#35927=CIRCLE('',#110296,25.);
#35928=CIRCLE('',#110298,25.);
#35929=CIRCLE('',#110299,25.);
#35930=CIRCLE('',#110300,25.);
#35931=CIRCLE('',#110301,25.);
#35932=CIRCLE('',#110306,25.);
#35933=CIRCLE('',#110307,25.);
#35934=CIRCLE('',#110308,25.);
#35935=CIRCLE('',#110310,25.);
#35936=CIRCLE('',#110311,25.);
#35937=CIRCLE('',#110312,25.);
#35938=CIRCLE('',#110315,24.492);
#35939=CIRCLE('',#110316,24.492);
#35940=CIRCLE('',#110319,24.492);
#35941=CIRCLE('',#110320,24.492);
#35942=CIRCLE('',#110323,24.492);
#35943=CIRCLE('',#110324,24.492);
#35944=CIRCLE('',#110327,24.492);
#35945=CIRCLE('',#110328,24.492);
#35946=CIRCLE('',#110331,78.7299999999993);
#35947=CIRCLE('',#110333,7.54337262320408);
#35948=CIRCLE('',#110335,7.54337262320413);
#35949=CIRCLE('',#110337,81.2699999999993);
#35950=CIRCLE('',#110339,80.);
#35951=CIRCLE('',#110340,80.);
#35952=CIRCLE('',#110342,1.27);
#35953=CIRCLE('',#110343,2.54);
#35954=CIRCLE('',#110345,1.27);
#35955=CIRCLE('',#110346,2.54);
#35956=CIRCLE('',#110347,80.);
#35957=CIRCLE('',#110349,80.);
#35958=CIRCLE('',#110351,82.2472021719721);
#35959=CIRCLE('',#110352,23.73);
#35960=CIRCLE('',#110354,80.);
#35961=CIRCLE('',#110356,82.2472021719721);
#35962=CIRCLE('',#110357,23.73);
#35963=CIRCLE('',#110359,80.);
#35964=CIRCLE('',#110360,80.);
#35965=CIRCLE('',#110362,82.2472021719721);
#35966=CIRCLE('',#110364,82.2472021719721);
#35967=CIRCLE('',#110369,26.905);
#35968=CIRCLE('',#110370,26.905);
#35969=CIRCLE('',#110371,81.905);
#35970=CIRCLE('',#110375,26.905);
#35971=CIRCLE('',#110376,26.905);
#35972=CIRCLE('',#110377,0.635);
#35973=CIRCLE('',#110378,81.905);
#35974=CIRCLE('',#110379,0.635);
#35975=CIRCLE('',#110383,26.905);
#35976=CIRCLE('',#110384,26.905);
#35977=CIRCLE('',#110391,6.26916093810295);
#35978=CIRCLE('',#110393,6.26916093808705);
#35979=CIRCLE('',#110397,2.54);
#35980=CIRCLE('',#110398,2.54);
#35981=CIRCLE('',#110400,2.54);
#35982=CIRCLE('',#110401,2.54);
#35983=CIRCLE('',#110403,2.54);
#35984=CIRCLE('',#110405,2.54);
#35985=CIRCLE('',#110407,2.54);
#35986=CIRCLE('',#110409,2.54);
#35987=CIRCLE('',#110410,1.905);
#35988=CIRCLE('',#110411,1.905);
#35989=CIRCLE('',#110413,1.905);
#35990=CIRCLE('',#110415,1.905);
#35991=CIRCLE('',#110417,1.905);
#35992=CIRCLE('',#110418,1.905);
#35993=CIRCLE('',#110420,1.905);
#35994=CIRCLE('',#110423,1.905);
#35995=CIRCLE('',#110425,1.905);
#35996=CIRCLE('',#110427,1.905);
#35997=CIRCLE('',#110429,1.905);
#35998=CIRCLE('',#110432,1.905);
#35999=CIRCLE('',#110434,1.905);
#36000=CIRCLE('',#110437,1.905);
#36001=CIRCLE('',#110439,1.905);
#36002=CIRCLE('',#110442,1.905);
#36003=CIRCLE('',#110444,1.905);
#36004=CIRCLE('',#110445,1.905);
#36005=CIRCLE('',#110446,1.905);
#36006=CIRCLE('',#110448,1.905);
#36007=CIRCLE('',#110450,1.27);
#36008=CIRCLE('',#110452,1.27);
#36009=CIRCLE('',#110459,1.27);
#36010=CIRCLE('',#110461,1.27);
#36011=CIRCLE('',#110463,2.54);
#36012=CIRCLE('',#110465,2.54000000000001);
#36013=CIRCLE('',#110466,2.54);
#36014=CIRCLE('',#110468,2.54);
#36015=CIRCLE('',#110469,2.54);
#36016=CIRCLE('',#110471,2.54);
#36017=CIRCLE('',#110473,2.54);
#36018=CIRCLE('',#110475,2.54);
#36019=CIRCLE('',#110476,1.27);
#36020=CIRCLE('',#110477,1.27);
#36021=CIRCLE('',#110479,1.27);
#36022=CIRCLE('',#110480,1.27);
#36023=CIRCLE('',#110482,1.905);
#36024=CIRCLE('',#110484,1.905);
#36025=CIRCLE('',#110486,1.27);
#36026=CIRCLE('',#110487,1.27);
#36027=CIRCLE('',#110488,1.27);
#36028=CIRCLE('',#110489,1.27);
#36029=CIRCLE('',#110490,1.27);
#36030=CIRCLE('',#110491,1.27);
#36031=CIRCLE('',#110492,1.27);
#36032=CIRCLE('',#110493,1.27);
#36033=CIRCLE('',#110494,1.27);
#36034=CIRCLE('',#110495,1.27);
#36035=CIRCLE('',#110496,1.27);
#36036=CIRCLE('',#110497,1.27);
#36037=CIRCLE('',#110498,1.27);
#36038=CIRCLE('',#110499,1.27);
#36039=CIRCLE('',#110500,1.27);
#36040=CIRCLE('',#110501,1.27);
#36041=CIRCLE('',#110502,1.27);
#36042=CIRCLE('',#110503,2.54);
#36043=CIRCLE('',#110505,2.54);
#36044=CIRCLE('',#110509,0.952500000000001);
#36045=CIRCLE('',#110511,1.905);
#36046=CIRCLE('',#110512,0.0635);
#36047=CIRCLE('',#110513,1.87908163265306);
#36048=CIRCLE('',#110514,1.905);
#36049=CIRCLE('',#110516,1.905);
#36050=CIRCLE('',#110517,0.0635);
#36051=CIRCLE('',#110518,1.8415);
#36052=CIRCLE('',#110519,1.905);
#36053=CIRCLE('',#110520,1.016);
#36054=CIRCLE('',#110521,0.889782955715898);
#36055=CIRCLE('',#110522,1.016);
#36056=CIRCLE('',#110525,1.27);
#36057=CIRCLE('',#110526,1.26090609359413);
#36058=CIRCLE('',#110529,3.17500000000001);
#36059=CIRCLE('',#110532,66.0995441972308);
#36060=CIRCLE('',#110533,0.127);
#36061=CIRCLE('',#110534,66.2265441972308);
#36062=CIRCLE('',#110535,66.0995441972308);
#36063=CIRCLE('',#110537,66.3535441972308);
#36064=CIRCLE('',#110538,0.127);
#36065=CIRCLE('',#110539,66.4805441972308);
#36066=CIRCLE('',#110540,66.4805441972308);
#36067=CIRCLE('',#110543,66.0995441972308);
#36068=CIRCLE('',#110545,66.4805441972308);
#36069=CIRCLE('',#110549,56.0881943187058);
#36070=CIRCLE('',#110550,0.381);
#36071=CIRCLE('',#110551,56.4113006433414);
#36072=CIRCLE('',#110553,50.889);
#36073=CIRCLE('',#110554,0.381);
#36074=CIRCLE('',#110555,51.27);
#36075=CIRCLE('',#110556,51.27);
#36076=CIRCLE('',#110558,50.);
#36077=CIRCLE('',#110559,50.);
#36078=CIRCLE('',#110560,0.381);
#36079=CIRCLE('',#110561,50.381);
#36080=CIRCLE('',#110563,56.5223703788014);
#36081=CIRCLE('',#110564,0.254);
#36082=CIRCLE('',#110565,56.7377745952251);
#36083=CIRCLE('',#110567,57.4087519663171);
#36084=CIRCLE('',#110568,0.254);
#36085=CIRCLE('',#110569,57.6241561827409);
#36086=CIRCLE('',#110571,56.875);
#36087=CIRCLE('',#110572,56.875);
#36088=CIRCLE('',#110576,51.27);
#36089=CIRCLE('',#110578,50.);
#36090=CIRCLE('',#110580,65.);
#36091=CIRCLE('',#110581,65.);
#36092=CIRCLE('',#110595,4.74980000000001);
#36093=CIRCLE('',#110597,4.74980000000001);
#36094=CIRCLE('',#110604,4.74980000000001);
#36095=CIRCLE('',#110606,4.74975596129106);
#36096=CIRCLE('',#110607,4.7227361454377);
#36097=CIRCLE('',#110608,4.84835211827671);
#36098=CIRCLE('',#110609,3.13054999999999);
#36099=CIRCLE('',#110611,4.74980000000001);
#36100=CIRCLE('',#110612,4.72926310421554);
#36101=CIRCLE('',#110613,4.77210660304414);
#36102=CIRCLE('',#110614,4.74980000000001);
#36103=CIRCLE('',#110615,3.98780000000001);
#36104=CIRCLE('',#110619,2.7496306570156);
#36105=CIRCLE('',#110620,2.7496306570156);
#36106=CIRCLE('',#110621,2.7496306570156);
#36107=CIRCLE('',#110622,2.7496306570156);
#36108=CIRCLE('',#110623,2.7496306570156);
#36109=CIRCLE('',#110624,2.7496306570156);
#36110=CIRCLE('',#110640,4.72274603343712);
#36111=CIRCLE('',#110647,4.74980000000001);
#36112=CIRCLE('',#110649,4.74980000000001);
#36113=CIRCLE('',#110656,4.74980000000001);
#36114=CIRCLE('',#110658,4.74975596129105);
#36115=CIRCLE('',#110659,4.72273590800283);
#36116=CIRCLE('',#110660,4.84835211827033);
#36117=CIRCLE('',#110661,3.13054999999999);
#36118=CIRCLE('',#110663,4.74980000000001);
#36119=CIRCLE('',#110664,4.72926310421625);
#36120=CIRCLE('',#110665,4.77210660304378);
#36121=CIRCLE('',#110666,4.74980000000001);
#36122=CIRCLE('',#110667,3.98780000000001);
#36123=CIRCLE('',#110671,2.7496306570156);
#36124=CIRCLE('',#110672,2.7496306570156);
#36125=CIRCLE('',#110673,2.7496306570156);
#36126=CIRCLE('',#110674,2.7496306570156);
#36127=CIRCLE('',#110675,2.7496306570156);
#36128=CIRCLE('',#110676,2.7496306570156);
#36129=CIRCLE('',#110692,40.);
#36130=CIRCLE('',#110693,41.2700000000001);
#36131=CIRCLE('',#110695,40.);
#36132=CIRCLE('',#110696,40.);
#36133=CIRCLE('',#110697,41.2700000000001);
#36134=CIRCLE('',#110699,50.);
#36135=CIRCLE('',#110700,48.4864729374055);
#36136=CIRCLE('',#110702,50.);
#36137=CIRCLE('',#110703,50.);
#36138=CIRCLE('',#110704,48.4864729374054);
#36139=CIRCLE('',#110712,65.0000000000002);
#36140=CIRCLE('',#110713,65.0000000000002);
#36141=CIRCLE('',#110715,56.8750000000002);
#36142=CIRCLE('',#110716,56.875);
#36143=CIRCLE('',#110718,74.8702478255888);
#36144=CIRCLE('',#110719,1.5875);
#36145=CIRCLE('',#110720,76.4577478255888);
#36146=CIRCLE('',#110721,76.4577478255888);
#36147=CIRCLE('',#110723,76.4577478255888);
#36148=CIRCLE('',#110725,66.9885441972308);
#36149=CIRCLE('',#110726,66.9885441972308);
#36150=CIRCLE('',#110728,70.625);
#36151=CIRCLE('',#110729,70.625);
#36152=CIRCLE('',#110731,76.5847478255888);
#36153=CIRCLE('',#110732,76.5847478255888);
#36154=CIRCLE('',#110734,8.4455);
#36155=CIRCLE('',#110735,8.4455);
#36156=CIRCLE('',#110737,8.4455);
#36157=CIRCLE('',#110738,8.4455);
#36158=CIRCLE('',#110740,8.4455);
#36159=CIRCLE('',#110741,8.4455);
#36160=CIRCLE('',#110743,8.4455);
#36161=CIRCLE('',#110744,8.4455);
#36162=CIRCLE('',#110746,7.9375);
#36163=CIRCLE('',#110747,7.9375);
#36164=CIRCLE('',#110749,7.93750000000014);
#36165=CIRCLE('',#110750,7.9375);
#36166=CIRCLE('',#110752,7.93749999999989);
#36167=CIRCLE('',#110753,7.9375);
#36168=CIRCLE('',#110755,7.9375);
#36169=CIRCLE('',#110756,7.9375);
#36170=CIRCLE('',#110758,24.492);
#36171=CIRCLE('',#110759,24.492);
#36172=CIRCLE('',#110762,24.492);
#36173=CIRCLE('',#110763,24.492);
#36174=CIRCLE('',#110766,24.492);
#36175=CIRCLE('',#110767,24.492);
#36176=CIRCLE('',#110770,24.492);
#36177=CIRCLE('',#110771,24.492);
#36178=CIRCLE('',#110774,23.73);
#36179=CIRCLE('',#110775,23.73);
#36180=CIRCLE('',#110776,23.73);
#36181=CIRCLE('',#110777,23.73);
#36182=CIRCLE('',#110783,25.);
#36183=CIRCLE('',#110784,25.);
#36184=CIRCLE('',#110785,25.);
#36185=CIRCLE('',#110786,25.);
#36186=CIRCLE('',#110788,25.);
#36187=CIRCLE('',#110791,25.);
#36188=CIRCLE('',#110794,25.);
#36189=CIRCLE('',#110797,25.);
#36190=CIRCLE('',#110800,0.762);
#36191=CIRCLE('',#110801,0.762);
#36192=CIRCLE('',#110803,0.762);
#36193=CIRCLE('',#110805,0.762);
#36194=CIRCLE('',#110807,0.762);
#36195=CIRCLE('',#110809,0.762);
#36196=CIRCLE('',#110811,0.762);
#36197=CIRCLE('',#110813,0.762);
#36198=CIRCLE('',#110817,66.9885441972308);
#36199=CIRCLE('',#110818,66.9885441972308);
#36200=CIRCLE('',#110820,73.6560441972308);
#36201=CIRCLE('',#110821,73.6560441972308);
#36202=CIRCLE('',#110826,73.6560441972308);
#36203=CIRCLE('',#110830,73.6560441972308);
#36204=CIRCLE('',#110840,3.4);
#36205=CIRCLE('',#110841,3.4);
#36206=CIRCLE('',#110844,7.49999999999995);
#36207=CIRCLE('',#110846,7.49999999999995);
#36208=CIRCLE('',#110848,7.49999999999995);
#36209=CIRCLE('',#110850,7.49999999999995);
#36210=CIRCLE('',#110852,7.49999999999995);
#36211=CIRCLE('',#110854,7.49999999999995);
#36212=CIRCLE('',#110856,15.);
#36213=CIRCLE('',#110857,15.);
#36214=CIRCLE('',#110858,15.);
#36215=CIRCLE('',#110860,164.1007636766);
#36216=CIRCLE('',#110861,164.100763676616);
#36217=CIRCLE('',#110863,164.100763676451);
#36218=CIRCLE('',#110864,164.100763676573);
#36219=CIRCLE('',#110866,164.100763676568);
#36220=CIRCLE('',#110868,164.100763676577);
#36221=CIRCLE('',#110870,164.100763676601);
#36222=CIRCLE('',#110872,164.100763676567);
#36223=CIRCLE('',#110878,10.);
#36224=CIRCLE('',#110879,10.);
#36225=CIRCLE('',#110885,2.);
#36226=CIRCLE('',#110886,2.);
#36227=CIRCLE('',#110887,2.);
#36228=CIRCLE('',#110888,2.);
#36229=CIRCLE('',#110889,10.);
#36230=CIRCLE('',#110890,10.);
#36231=CIRCLE('',#110891,10.);
#36232=CIRCLE('',#110892,10.);
#36233=CIRCLE('',#110898,5.);
#36234=CIRCLE('',#110899,5.);
#36235=CIRCLE('',#110901,5.);
#36236=CIRCLE('',#110902,5.);
#36237=CIRCLE('',#110904,5.);
#36238=CIRCLE('',#110905,5.);
#36239=CIRCLE('',#110907,5.);
#36240=CIRCLE('',#110908,5.);
#36241=CIRCLE('',#110909,3.);
#36242=CIRCLE('',#110910,3.);
#36243=CIRCLE('',#110912,3.);
#36244=CIRCLE('',#110914,3.);
#36245=CIRCLE('',#110915,3.);
#36246=CIRCLE('',#110916,3.);
#36247=CIRCLE('',#110918,3.);
#36248=CIRCLE('',#110920,3.);
#36249=CIRCLE('',#110922,5.);
#36250=CIRCLE('',#110923,5.);
#36251=CIRCLE('',#110925,5.);
#36252=CIRCLE('',#110926,5.);
#36253=CIRCLE('',#110928,5.);
#36254=CIRCLE('',#110929,5.);
#36255=CIRCLE('',#110931,5.);
#36256=CIRCLE('',#110932,5.);
#36257=CIRCLE('',#110938,10.);
#36258=CIRCLE('',#110939,10.);
#36259=CIRCLE('',#110941,5.);
#36260=CIRCLE('',#110942,5.);
#36261=CIRCLE('',#110944,5.);
#36262=CIRCLE('',#110946,5.);
#36263=CIRCLE('',#110948,5.);
#36264=CIRCLE('',#110950,5.);
#36265=CIRCLE('',#110952,5.);
#36266=CIRCLE('',#110954,5.);
#36267=CIRCLE('',#110957,5.);
#36268=CIRCLE('',#110958,5.);
#36269=CIRCLE('',#110959,5.);
#36270=CIRCLE('',#110961,5.);
#36271=CIRCLE('',#110963,5.);
#36272=CIRCLE('',#110965,5.);
#36273=CIRCLE('',#110966,5.);
#36274=CIRCLE('',#110967,5.);
#36275=CIRCLE('',#110969,5.);
#36276=CIRCLE('',#110971,5.);
#36277=CIRCLE('',#110973,5.);
#36278=CIRCLE('',#110974,5.);
#36279=CIRCLE('',#110988,6.3);
#36280=CIRCLE('',#110989,6.3);
#36281=CIRCLE('',#110991,9.9216);
#36282=CIRCLE('',#110992,6.29999999999999);
#36283=CIRCLE('',#110993,9.92159999999999);
#36284=CIRCLE('',#110994,6.29999999999999);
#36285=CIRCLE('',#110995,9.92159999999999);
#36286=CIRCLE('',#110996,6.3);
#36287=CIRCLE('',#110997,9.92159999999999);
#36288=CIRCLE('',#111001,9.92159999999999);
#36289=CIRCLE('',#111004,6.3);
#36290=CIRCLE('',#111007,9.92159999999999);
#36291=CIRCLE('',#111010,6.29999999999999);
#36292=CIRCLE('',#111013,9.92159999999999);
#36293=CIRCLE('',#111016,6.29999999999999);
#36294=CIRCLE('',#111019,9.9216);
#36295=CIRCLE('',#111022,1.8);
#36296=CIRCLE('',#111023,1.8);
#36297=CIRCLE('',#111024,1.8);
#36298=CIRCLE('',#111025,1.8);
#36299=CIRCLE('',#111028,1.8);
#36300=CIRCLE('',#111031,1.8);
#36301=CIRCLE('',#111034,1.8);
#36302=CIRCLE('',#111037,1.8);
#36303=CIRCLE('',#111040,2.7);
#36304=CIRCLE('',#111041,2.7);
#36305=CIRCLE('',#111042,2.7);
#36306=CIRCLE('',#111043,2.69999999999999);
#36307=CIRCLE('',#111044,2.69999999999999);
#36308=CIRCLE('',#111045,2.7);
#36309=CIRCLE('',#111046,2.7);
#36310=CIRCLE('',#111047,2.7);
#36311=CIRCLE('',#111048,2.7);
#36312=CIRCLE('',#111049,2.7);
#36313=CIRCLE('',#111050,2.69999999999999);
#36314=CIRCLE('',#111051,2.69999999999999);
#36315=CIRCLE('',#111052,2.7);
#36316=CIRCLE('',#111053,2.7);
#36317=CIRCLE('',#111054,2.7);
#36318=CIRCLE('',#111055,2.69999999999999);
#36319=CIRCLE('',#111056,2.7);
#36320=CIRCLE('',#111057,2.69999999999999);
#36321=CIRCLE('',#111058,2.7);
#36322=CIRCLE('',#111059,2.7);
#36323=CIRCLE('',#111060,2.7);
#36324=CIRCLE('',#111061,2.7);
#36325=CIRCLE('',#111062,2.69999999999999);
#36326=CIRCLE('',#111063,2.69999999999999);
#36327=CIRCLE('',#111065,2.7);
#36328=CIRCLE('',#111066,2.7);
#36329=CIRCLE('',#111067,2.69999999999999);
#36330=CIRCLE('',#111068,2.69999999999999);
#36331=CIRCLE('',#111069,2.69999999999999);
#36332=CIRCLE('',#111070,2.7);
#36333=CIRCLE('',#111071,2.7);
#36334=CIRCLE('',#111072,2.7);
#36335=CIRCLE('',#111073,2.69999999999999);
#36336=CIRCLE('',#111074,2.69999999999999);
#36337=CIRCLE('',#111075,2.69999999999999);
#36338=CIRCLE('',#111076,2.7);
#36339=CIRCLE('',#111077,2.7);
#36340=CIRCLE('',#111078,2.7);
#36341=CIRCLE('',#111079,2.7);
#36342=CIRCLE('',#111080,2.69999999999999);
#36343=CIRCLE('',#111081,2.69999999999999);
#36344=CIRCLE('',#111082,2.7);
#36345=CIRCLE('',#111083,2.7);
#36346=CIRCLE('',#111084,2.7);
#36347=CIRCLE('',#111085,2.69999999999999);
#36348=CIRCLE('',#111086,2.69999999999999);
#36349=CIRCLE('',#111087,2.69999999999999);
#36350=CIRCLE('',#111088,2.7);
#36351=CIRCLE('',#111146,6.29999999999999);
#36352=CIRCLE('',#111147,6.29999999999999);
#36353=CIRCLE('',#111149,9.9216);
#36354=CIRCLE('',#111150,6.29999999999999);
#36355=CIRCLE('',#111151,9.92159999999999);
#36356=CIRCLE('',#111152,9.92159999999998);
#36357=CIRCLE('',#111153,6.3);
#36358=CIRCLE('',#111154,9.92159999999999);
#36359=CIRCLE('',#111155,6.3);
#36360=CIRCLE('',#111158,6.29999999999999);
#36361=CIRCLE('',#111161,9.92159999999999);
#36362=CIRCLE('',#111164,6.3);
#36363=CIRCLE('',#111167,9.92159999999998);
#36364=CIRCLE('',#111171,9.92159999999999);
#36365=CIRCLE('',#111174,6.29999999999999);
#36366=CIRCLE('',#111177,9.9216);
#36367=CIRCLE('',#111180,1.8);
#36368=CIRCLE('',#111181,1.8);
#36369=CIRCLE('',#111182,1.8);
#36370=CIRCLE('',#111183,1.8);
#36371=CIRCLE('',#111186,1.8);
#36372=CIRCLE('',#111189,1.8);
#36373=CIRCLE('',#111192,1.8);
#36374=CIRCLE('',#111195,1.8);
#36375=CIRCLE('',#111198,6.29999999999999);
#36376=CIRCLE('',#111199,6.29999999999999);
#36377=CIRCLE('',#111201,9.9216);
#36378=CIRCLE('',#111202,9.92159999999999);
#36379=CIRCLE('',#111203,6.29999999999999);
#36380=CIRCLE('',#111204,9.92159999999998);
#36381=CIRCLE('',#111205,6.3);
#36382=CIRCLE('',#111206,9.92159999999999);
#36383=CIRCLE('',#111207,6.3);
#36384=CIRCLE('',#111210,6.3);
#36385=CIRCLE('',#111213,9.92159999999999);
#36386=CIRCLE('',#111216,6.3);
#36387=CIRCLE('',#111219,9.92159999999999);
#36388=CIRCLE('',#111222,6.29999999999999);
#36389=CIRCLE('',#111225,9.92159999999999);
#36390=CIRCLE('',#111229,9.92159999999999);
#36391=CIRCLE('',#111232,1.8);
#36392=CIRCLE('',#111233,1.8);
#36393=CIRCLE('',#111234,1.8);
#36394=CIRCLE('',#111235,1.8);
#36395=CIRCLE('',#111238,1.8);
#36396=CIRCLE('',#111241,1.8);
#36397=CIRCLE('',#111244,1.8);
#36398=CIRCLE('',#111247,1.8);
#36399=CIRCLE('',#111250,6.29999999999999);
#36400=CIRCLE('',#111251,6.29999999999999);
#36401=CIRCLE('',#111253,9.9216);
#36402=CIRCLE('',#111254,9.92159999999999);
#36403=CIRCLE('',#111255,6.29999999999999);
#36404=CIRCLE('',#111256,9.92159999999999);
#36405=CIRCLE('',#111257,6.3);
#36406=CIRCLE('',#111258,9.92159999999999);
#36407=CIRCLE('',#111259,6.3);
#36408=CIRCLE('',#111262,6.3);
#36409=CIRCLE('',#111265,9.92159999999999);
#36410=CIRCLE('',#111268,6.3);
#36411=CIRCLE('',#111271,9.92159999999999);
#36412=CIRCLE('',#111274,6.29999999999999);
#36413=CIRCLE('',#111277,9.92159999999999);
#36414=CIRCLE('',#111281,9.9216);
#36415=CIRCLE('',#111284,1.8);
#36416=CIRCLE('',#111285,1.8);
#36417=CIRCLE('',#111286,1.8);
#36418=CIRCLE('',#111287,1.8);
#36419=CIRCLE('',#111290,1.8);
#36420=CIRCLE('',#111293,1.8);
#36421=CIRCLE('',#111296,1.8);
#36422=CIRCLE('',#111299,1.8);
#36423=CIRCLE('',#111307,0.899999999999998);
#36424=CIRCLE('',#111308,0.899999999999998);
#36425=CIRCLE('',#111311,0.899999999999998);
#36426=CIRCLE('',#111312,0.899999999999998);
#36427=CIRCLE('',#111315,0.899999999999998);
#36428=CIRCLE('',#111316,0.899999999999998);
#36429=CIRCLE('',#111319,0.899999999999991);
#36430=CIRCLE('',#111320,0.899999999999991);
#36431=CIRCLE('',#111330,0.899999999999995);
#36432=CIRCLE('',#111331,0.899999999999995);
#36433=CIRCLE('',#111334,0.900000000000001);
#36434=CIRCLE('',#111335,0.900000000000001);
#36435=CIRCLE('',#111338,0.899999999999996);
#36436=CIRCLE('',#111339,0.899999999999996);
#36437=CIRCLE('',#111342,0.899999999999998);
#36438=CIRCLE('',#111343,0.899999999999998);
#36439=CIRCLE('',#111349,0.899999999999998);
#36440=CIRCLE('',#111350,0.899999999999998);
#36441=CIRCLE('',#111353,0.899999999999998);
#36442=CIRCLE('',#111354,0.899999999999998);
#36443=CIRCLE('',#111357,0.899999999999991);
#36444=CIRCLE('',#111358,0.899999999999991);
#36445=CIRCLE('',#111361,0.899999999999998);
#36446=CIRCLE('',#111362,0.899999999999998);
#36447=CIRCLE('',#111368,3.65760000000007);
#36448=CIRCLE('',#111369,3.65760000000007);
#36449=CIRCLE('',#111375,0.899999999999991);
#36450=CIRCLE('',#111376,0.899999999999991);
#36451=CIRCLE('',#111379,0.899999999999998);
#36452=CIRCLE('',#111380,0.899999999999998);
#36453=CIRCLE('',#111383,0.899999999999998);
#36454=CIRCLE('',#111384,0.899999999999998);
#36455=CIRCLE('',#111387,0.899999999999998);
#36456=CIRCLE('',#111388,0.899999999999998);
#36457=CIRCLE('',#111394,0.899999999999998);
#36458=CIRCLE('',#111395,0.899999999999998);
#36459=CIRCLE('',#111398,0.899999999999996);
#36460=CIRCLE('',#111399,0.899999999999998);
#36461=CIRCLE('',#111402,0.900000000000001);
#36462=CIRCLE('',#111403,0.899999999999998);
#36463=CIRCLE('',#111406,0.899999999999995);
#36464=CIRCLE('',#111407,0.899999999999991);
#36465=CIRCLE('',#111416,0.899999999999991);
#36466=CIRCLE('',#111417,0.899999999999995);
#36467=CIRCLE('',#111420,0.899999999999998);
#36468=CIRCLE('',#111421,0.900000000000001);
#36469=CIRCLE('',#111424,0.899999999999998);
#36470=CIRCLE('',#111425,0.899999999999996);
#36471=CIRCLE('',#111428,0.899999999999998);
#36472=CIRCLE('',#111429,0.899999999999998);
#36473=CIRCLE('',#111435,0.899999999999998);
#36474=CIRCLE('',#111436,0.899999999999998);
#36475=CIRCLE('',#111439,0.899999999999998);
#36476=CIRCLE('',#111440,0.899999999999998);
#36477=CIRCLE('',#111443,0.899999999999991);
#36478=CIRCLE('',#111444,0.899999999999991);
#36479=CIRCLE('',#111447,0.899999999999998);
#36480=CIRCLE('',#111448,0.899999999999998);
#36481=CIRCLE('',#111454,3.65760000000007);
#36482=CIRCLE('',#111455,3.65760000000007);
#36483=CIRCLE('',#111461,0.899999999999991);
#36484=CIRCLE('',#111462,0.899999999999991);
#36485=CIRCLE('',#111465,0.899999999999998);
#36486=CIRCLE('',#111466,0.899999999999998);
#36487=CIRCLE('',#111469,0.899999999999998);
#36488=CIRCLE('',#111470,0.899999999999998);
#36489=CIRCLE('',#111473,0.899999999999998);
#36490=CIRCLE('',#111474,0.899999999999998);
#36491=CIRCLE('',#111480,0.899999999999998);
#36492=CIRCLE('',#111481,0.899999999999998);
#36493=CIRCLE('',#111484,0.899999999999998);
#36494=CIRCLE('',#111485,0.899999999999998);
#36495=CIRCLE('',#111488,0.899999999999998);
#36496=CIRCLE('',#111489,0.899999999999998);
#36497=CIRCLE('',#111492,0.899999999999991);
#36498=CIRCLE('',#111493,0.899999999999991);
#36499=CIRCLE('',#111502,0.899999999999995);
#36500=CIRCLE('',#111503,0.899999999999995);
#36501=CIRCLE('',#111506,0.900000000000001);
#36502=CIRCLE('',#111507,0.900000000000001);
#36503=CIRCLE('',#111510,0.899999999999996);
#36504=CIRCLE('',#111511,0.899999999999996);
#36505=CIRCLE('',#111514,0.899999999999998);
#36506=CIRCLE('',#111515,0.899999999999998);
#36507=CIRCLE('',#111521,0.899999999999998);
#36508=CIRCLE('',#111522,0.899999999999998);
#36509=CIRCLE('',#111525,0.899999999999998);
#36510=CIRCLE('',#111526,0.899999999999998);
#36511=CIRCLE('',#111529,0.899999999999991);
#36512=CIRCLE('',#111530,0.899999999999991);
#36513=CIRCLE('',#111533,0.899999999999998);
#36514=CIRCLE('',#111534,0.899999999999998);
#36515=CIRCLE('',#111540,3.65760000000007);
#36516=CIRCLE('',#111541,3.65760000000007);
#36517=CIRCLE('',#111547,0.899999999999991);
#36518=CIRCLE('',#111548,0.899999999999991);
#36519=CIRCLE('',#111551,0.899999999999998);
#36520=CIRCLE('',#111552,0.899999999999998);
#36521=CIRCLE('',#111555,0.899999999999998);
#36522=CIRCLE('',#111556,0.899999999999998);
#36523=CIRCLE('',#111559,0.899999999999998);
#36524=CIRCLE('',#111560,0.899999999999998);
#36525=CIRCLE('',#111566,0.899999999999998);
#36526=CIRCLE('',#111567,0.899999999999998);
#36527=CIRCLE('',#111570,0.899999999999996);
#36528=CIRCLE('',#111571,0.899999999999998);
#36529=CIRCLE('',#111574,0.900000000000001);
#36530=CIRCLE('',#111575,0.899999999999998);
#36531=CIRCLE('',#111578,0.899999999999995);
#36532=CIRCLE('',#111579,0.899999999999991);
#36533=CIRCLE('',#111587,0.899999999999991);
#36534=CIRCLE('',#111588,0.899999999999995);
#36535=CIRCLE('',#111591,0.899999999999998);
#36536=CIRCLE('',#111592,0.900000000000001);
#36537=CIRCLE('',#111595,0.899999999999998);
#36538=CIRCLE('',#111596,0.899999999999996);
#36539=CIRCLE('',#111599,0.899999999999998);
#36540=CIRCLE('',#111600,0.899999999999998);
#36541=CIRCLE('',#111606,0.899999999999998);
#36542=CIRCLE('',#111607,0.899999999999998);
#36543=CIRCLE('',#111610,0.899999999999998);
#36544=CIRCLE('',#111611,0.899999999999998);
#36545=CIRCLE('',#111614,0.899999999999991);
#36546=CIRCLE('',#111615,0.899999999999991);
#36547=CIRCLE('',#111618,0.899999999999998);
#36548=CIRCLE('',#111619,0.899999999999998);
#36549=CIRCLE('',#111625,3.65760000000007);
#36550=CIRCLE('',#111626,3.65760000000007);
#36551=CIRCLE('',#111632,0.899999999999991);
#36552=CIRCLE('',#111633,0.899999999999991);
#36553=CIRCLE('',#111636,0.899999999999998);
#36554=CIRCLE('',#111637,0.899999999999998);
#36555=CIRCLE('',#111640,0.899999999999998);
#36556=CIRCLE('',#111641,0.899999999999998);
#36557=CIRCLE('',#111644,0.899999999999998);
#36558=CIRCLE('',#111645,0.899999999999998);
#36559=VERTEX_POINT('',#142645);
#36560=VERTEX_POINT('',#142647);
#36561=VERTEX_POINT('',#142651);
#36562=VERTEX_POINT('',#142653);
#36563=VERTEX_POINT('',#142657);
#36564=VERTEX_POINT('',#142659);
#36565=VERTEX_POINT('',#142663);
#36566=VERTEX_POINT('',#142665);
#36567=VERTEX_POINT('',#142669);
#36568=VERTEX_POINT('',#142670);
#36569=VERTEX_POINT('',#142672);
#36570=VERTEX_POINT('',#142674);
#36571=VERTEX_POINT('',#142678);
#36572=VERTEX_POINT('',#142680);
#36573=VERTEX_POINT('',#142684);
#36574=VERTEX_POINT('',#142686);
#36575=VERTEX_POINT('',#142693);
#36576=VERTEX_POINT('',#142694);
#36577=VERTEX_POINT('',#142696);
#36578=VERTEX_POINT('',#142698);
#36579=VERTEX_POINT('',#142702);
#36580=VERTEX_POINT('',#142704);
#36581=VERTEX_POINT('',#142708);
#36582=VERTEX_POINT('',#142712);
#36583=VERTEX_POINT('',#142718);
#36584=VERTEX_POINT('',#142720);
#36585=VERTEX_POINT('',#142724);
#36586=VERTEX_POINT('',#142728);
#36587=VERTEX_POINT('',#142734);
#36588=VERTEX_POINT('',#142736);
#36589=VERTEX_POINT('',#142740);
#36590=VERTEX_POINT('',#142744);
#36591=VERTEX_POINT('',#142750);
#36592=VERTEX_POINT('',#142752);
#36593=VERTEX_POINT('',#142756);
#36594=VERTEX_POINT('',#142760);
#36595=VERTEX_POINT('',#142766);
#36596=VERTEX_POINT('',#142767);
#36597=VERTEX_POINT('',#142769);
#36598=VERTEX_POINT('',#142771);
#36599=VERTEX_POINT('',#142773);
#36600=VERTEX_POINT('',#142775);
#36601=VERTEX_POINT('',#142777);
#36602=VERTEX_POINT('',#142779);
#36603=VERTEX_POINT('',#142783);
#36604=VERTEX_POINT('',#142784);
#36605=VERTEX_POINT('',#142786);
#36606=VERTEX_POINT('',#142788);
#36607=VERTEX_POINT('',#142790);
#36608=VERTEX_POINT('',#142792);
#36609=VERTEX_POINT('',#142794);
#36610=VERTEX_POINT('',#142796);
#36611=VERTEX_POINT('',#142800);
#36612=VERTEX_POINT('',#142802);
#36613=VERTEX_POINT('',#142806);
#36614=VERTEX_POINT('',#142808);
#36615=VERTEX_POINT('',#142812);
#36616=VERTEX_POINT('',#142814);
#36617=VERTEX_POINT('',#142818);
#36618=VERTEX_POINT('',#142820);
#36619=VERTEX_POINT('',#142849);
#36620=VERTEX_POINT('',#142850);
#36621=VERTEX_POINT('',#142853);
#36622=VERTEX_POINT('',#142857);
#36623=VERTEX_POINT('',#142859);
#36624=VERTEX_POINT('',#142861);
#36625=VERTEX_POINT('',#142865);
#36626=VERTEX_POINT('',#142866);
#36627=VERTEX_POINT('',#142885);
#36628=VERTEX_POINT('',#142887);
#36629=VERTEX_POINT('',#142943);
#36630=VERTEX_POINT('',#142944);
#36631=VERTEX_POINT('',#142963);
#36632=VERTEX_POINT('',#142965);
#36633=VERTEX_POINT('',#143021);
#36634=VERTEX_POINT('',#143022);
#36635=VERTEX_POINT('',#143042);
#36636=VERTEX_POINT('',#143044);
#36637=VERTEX_POINT('',#143101);
#36638=VERTEX_POINT('',#143102);
#36639=VERTEX_POINT('',#143122);
#36640=VERTEX_POINT('',#143124);
#36641=VERTEX_POINT('',#143181);
#36642=VERTEX_POINT('',#143187);
#36643=VERTEX_POINT('',#143193);
#36644=VERTEX_POINT('',#143194);
#36645=VERTEX_POINT('',#143196);
#36646=VERTEX_POINT('',#143232);
#36647=VERTEX_POINT('',#143270);
#36648=VERTEX_POINT('',#143271);
#36649=VERTEX_POINT('',#143412);
#36650=VERTEX_POINT('',#143413);
#36651=VERTEX_POINT('',#143554);
#36652=VERTEX_POINT('',#143555);
#36653=VERTEX_POINT('',#143696);
#36654=VERTEX_POINT('',#143697);
#36655=VERTEX_POINT('',#143838);
#36656=VERTEX_POINT('',#143839);
#36657=VERTEX_POINT('',#143980);
#36658=VERTEX_POINT('',#143981);
#36659=VERTEX_POINT('',#144122);
#36660=VERTEX_POINT('',#144123);
#36661=VERTEX_POINT('',#144264);
#36662=VERTEX_POINT('',#144265);
#36663=VERTEX_POINT('',#144267);
#36664=VERTEX_POINT('',#144295);
#36665=VERTEX_POINT('',#144297);
#36666=VERTEX_POINT('',#144317);
#36667=VERTEX_POINT('',#144318);
#36668=VERTEX_POINT('',#144355);
#36669=VERTEX_POINT('',#144356);
#36670=VERTEX_POINT('',#144394);
#36671=VERTEX_POINT('',#144395);
#36672=VERTEX_POINT('',#144468);
#36673=VERTEX_POINT('',#144469);
#36674=VERTEX_POINT('',#144508);
#36675=VERTEX_POINT('',#144509);
#36676=VERTEX_POINT('',#144564);
#36677=VERTEX_POINT('',#144565);
#36678=VERTEX_POINT('',#144620);
#36679=VERTEX_POINT('',#144621);
#36680=VERTEX_POINT('',#144676);
#36681=VERTEX_POINT('',#144677);
#36682=VERTEX_POINT('',#144732);
#36683=VERTEX_POINT('',#144733);
#36684=VERTEX_POINT('',#144788);
#36685=VERTEX_POINT('',#144789);
#36686=VERTEX_POINT('',#144844);
#36687=VERTEX_POINT('',#144845);
#36688=VERTEX_POINT('',#144847);
#36689=VERTEX_POINT('',#144874);
#36690=VERTEX_POINT('',#144901);
#36691=VERTEX_POINT('',#144902);
#36692=VERTEX_POINT('',#144971);
#36693=VERTEX_POINT('',#144972);
#36694=VERTEX_POINT('',#145043);
#36695=VERTEX_POINT('',#145044);
#36696=VERTEX_POINT('',#145115);
#36697=VERTEX_POINT('',#145116);
#36698=VERTEX_POINT('',#145187);
#36699=VERTEX_POINT('',#145188);
#36700=VERTEX_POINT('',#145259);
#36701=VERTEX_POINT('',#145260);
#36702=VERTEX_POINT('',#145331);
#36703=VERTEX_POINT('',#145332);
#36704=VERTEX_POINT('',#145403);
#36705=VERTEX_POINT('',#145405);
#36706=VERTEX_POINT('',#145443);
#36707=VERTEX_POINT('',#145444);
#36708=VERTEX_POINT('',#145483);
#36709=VERTEX_POINT('',#145485);
#36710=VERTEX_POINT('',#145524);
#36711=VERTEX_POINT('',#145525);
#36712=VERTEX_POINT('',#145565);
#36713=VERTEX_POINT('',#145576);
#36714=VERTEX_POINT('',#145591);
#36715=VERTEX_POINT('',#145608);
#36716=VERTEX_POINT('',#145802);
#36717=VERTEX_POINT('',#145809);
#36718=VERTEX_POINT('',#145812);
#36719=VERTEX_POINT('',#149841);
#36720=VERTEX_POINT('',#149843);
#36721=VERTEX_POINT('',#154414);
#36722=VERTEX_POINT('',#158489);
#36723=VERTEX_POINT('',#162555);
#36724=VERTEX_POINT('',#162562);
#36725=VERTEX_POINT('',#167146);
#36726=VERTEX_POINT('',#167148);
#36727=VERTEX_POINT('',#167150);
#36728=VERTEX_POINT('',#167154);
#36729=VERTEX_POINT('',#167155);
#36730=VERTEX_POINT('',#167166);
#36731=VERTEX_POINT('',#167168);
#36732=VERTEX_POINT('',#167181);
#36733=VERTEX_POINT('',#167182);
#36734=VERTEX_POINT('',#167191);
#36735=VERTEX_POINT('',#167193);
#36736=VERTEX_POINT('',#167197);
#36737=VERTEX_POINT('',#167198);
#36738=VERTEX_POINT('',#167200);
#36739=VERTEX_POINT('',#167204);
#36740=VERTEX_POINT('',#167215);
#36741=VERTEX_POINT('',#167221);
#36742=VERTEX_POINT('',#167222);
#36743=VERTEX_POINT('',#167224);
#36744=VERTEX_POINT('',#167228);
#36745=VERTEX_POINT('',#167232);
#36746=VERTEX_POINT('',#167235);
#36747=VERTEX_POINT('',#167236);
#36748=VERTEX_POINT('',#167241);
#36749=VERTEX_POINT('',#167243);
#36750=VERTEX_POINT('',#167247);
#36751=VERTEX_POINT('',#167251);
#36752=VERTEX_POINT('',#167253);
#36753=VERTEX_POINT('',#167266);
#36754=VERTEX_POINT('',#167270);
#36755=VERTEX_POINT('',#167285);
#36756=VERTEX_POINT('',#167289);
#36757=VERTEX_POINT('',#167304);
#36758=VERTEX_POINT('',#167308);
#36759=VERTEX_POINT('',#167323);
#36760=VERTEX_POINT('',#167327);
#36761=VERTEX_POINT('',#167343);
#36762=VERTEX_POINT('',#167345);
#36763=VERTEX_POINT('',#167347);
#36764=VERTEX_POINT('',#167349);
#36765=VERTEX_POINT('',#167353);
#36766=VERTEX_POINT('',#167357);
#36767=VERTEX_POINT('',#167372);
#36768=VERTEX_POINT('',#167376);
#36769=VERTEX_POINT('',#167391);
#36770=VERTEX_POINT('',#167395);
#36771=VERTEX_POINT('',#167410);
#36772=VERTEX_POINT('',#167414);
#36773=VERTEX_POINT('',#167429);
#36774=VERTEX_POINT('',#167433);
#36775=VERTEX_POINT('',#167469);
#36776=VERTEX_POINT('',#167471);
#36777=VERTEX_POINT('',#167475);
#36778=VERTEX_POINT('',#167477);
#36779=VERTEX_POINT('',#167483);
#36780=VERTEX_POINT('',#167485);
#36781=VERTEX_POINT('',#167489);
#36782=VERTEX_POINT('',#167491);
#36783=VERTEX_POINT('',#167497);
#36784=VERTEX_POINT('',#167499);
#36785=VERTEX_POINT('',#167503);
#36786=VERTEX_POINT('',#167505);
#36787=VERTEX_POINT('',#167511);
#36788=VERTEX_POINT('',#167513);
#36789=VERTEX_POINT('',#167517);
#36790=VERTEX_POINT('',#167519);
#36791=VERTEX_POINT('',#167525);
#36792=VERTEX_POINT('',#167526);
#36793=VERTEX_POINT('',#167529);
#36794=VERTEX_POINT('',#167533);
#36795=VERTEX_POINT('',#167535);
#36796=VERTEX_POINT('',#167537);
#36797=VERTEX_POINT('',#167541);
#36798=VERTEX_POINT('',#167545);
#36799=VERTEX_POINT('',#167551);
#36800=VERTEX_POINT('',#167553);
#36801=VERTEX_POINT('',#167555);
#36802=VERTEX_POINT('',#167559);
#36803=VERTEX_POINT('',#167560);
#36804=VERTEX_POINT('',#167563);
#36805=VERTEX_POINT('',#167567);
#36806=VERTEX_POINT('',#167571);
#36807=VERTEX_POINT('',#167577);
#36808=VERTEX_POINT('',#167579);
#36809=VERTEX_POINT('',#167583);
#36810=VERTEX_POINT('',#167585);
#36811=VERTEX_POINT('',#167591);
#36812=VERTEX_POINT('',#167592);
#36813=VERTEX_POINT('',#167594);
#36814=VERTEX_POINT('',#167596);
#36815=VERTEX_POINT('',#167600);
#36816=VERTEX_POINT('',#167601);
#36817=VERTEX_POINT('',#167603);
#36818=VERTEX_POINT('',#167605);
#36819=VERTEX_POINT('',#167609);
#36820=VERTEX_POINT('',#167610);
#36821=VERTEX_POINT('',#167612);
#36822=VERTEX_POINT('',#167614);
#36823=VERTEX_POINT('',#167618);
#36824=VERTEX_POINT('',#167619);
#36825=VERTEX_POINT('',#167621);
#36826=VERTEX_POINT('',#167623);
#36827=VERTEX_POINT('',#167625);
#36828=VERTEX_POINT('',#167629);
#36829=VERTEX_POINT('',#167631);
#36830=VERTEX_POINT('',#167633);
#36831=VERTEX_POINT('',#167637);
#36832=VERTEX_POINT('',#167639);
#36833=VERTEX_POINT('',#167643);
#36834=VERTEX_POINT('',#167645);
#36835=VERTEX_POINT('',#167647);
#36836=VERTEX_POINT('',#167651);
#36837=VERTEX_POINT('',#167653);
#36838=VERTEX_POINT('',#167657);
#36839=VERTEX_POINT('',#167659);
#36840=VERTEX_POINT('',#167665);
#36841=VERTEX_POINT('',#167666);
#36842=VERTEX_POINT('',#167668);
#36843=VERTEX_POINT('',#167712);
#36844=VERTEX_POINT('',#167714);
#36845=VERTEX_POINT('',#167716);
#36846=VERTEX_POINT('',#167718);
#36847=VERTEX_POINT('',#167759);
#36848=VERTEX_POINT('',#167761);
#36849=VERTEX_POINT('',#167805);
#36850=VERTEX_POINT('',#167807);
#36851=VERTEX_POINT('',#167809);
#36852=VERTEX_POINT('',#167811);
#36853=VERTEX_POINT('',#167852);
#36854=VERTEX_POINT('',#167854);
#36855=VERTEX_POINT('',#167898);
#36856=VERTEX_POINT('',#167900);
#36857=VERTEX_POINT('',#167902);
#36858=VERTEX_POINT('',#167904);
#36859=VERTEX_POINT('',#167945);
#36860=VERTEX_POINT('',#167947);
#36861=VERTEX_POINT('',#167991);
#36862=VERTEX_POINT('',#167993);
#36863=VERTEX_POINT('',#167995);
#36864=VERTEX_POINT('',#167997);
#36865=VERTEX_POINT('',#168038);
#36866=VERTEX_POINT('',#168040);
#36867=VERTEX_POINT('',#168084);
#36868=VERTEX_POINT('',#168086);
#36869=VERTEX_POINT('',#168088);
#36870=VERTEX_POINT('',#168090);
#36871=VERTEX_POINT('',#168131);
#36872=VERTEX_POINT('',#168133);
#36873=VERTEX_POINT('',#168177);
#36874=VERTEX_POINT('',#168179);
#36875=VERTEX_POINT('',#168181);
#36876=VERTEX_POINT('',#168183);
#36877=VERTEX_POINT('',#168224);
#36878=VERTEX_POINT('',#168226);
#36879=VERTEX_POINT('',#168270);
#36880=VERTEX_POINT('',#168272);
#36881=VERTEX_POINT('',#168274);
#36882=VERTEX_POINT('',#168276);
#36883=VERTEX_POINT('',#168317);
#36884=VERTEX_POINT('',#168319);
#36885=VERTEX_POINT('',#168363);
#36886=VERTEX_POINT('',#168365);
#36887=VERTEX_POINT('',#168367);
#36888=VERTEX_POINT('',#168369);
#36889=VERTEX_POINT('',#168410);
#36890=VERTEX_POINT('',#168412);
#36891=VERTEX_POINT('',#168456);
#36892=VERTEX_POINT('',#168458);
#36893=VERTEX_POINT('',#168460);
#36894=VERTEX_POINT('',#168462);
#36895=VERTEX_POINT('',#168503);
#36896=VERTEX_POINT('',#168505);
#36897=VERTEX_POINT('',#168549);
#36898=VERTEX_POINT('',#168551);
#36899=VERTEX_POINT('',#168553);
#36900=VERTEX_POINT('',#168555);
#36901=VERTEX_POINT('',#168596);
#36902=VERTEX_POINT('',#168598);
#36903=VERTEX_POINT('',#168642);
#36904=VERTEX_POINT('',#168644);
#36905=VERTEX_POINT('',#168646);
#36906=VERTEX_POINT('',#168648);
#36907=VERTEX_POINT('',#168689);
#36908=VERTEX_POINT('',#168691);
#36909=VERTEX_POINT('',#168735);
#36910=VERTEX_POINT('',#168737);
#36911=VERTEX_POINT('',#168739);
#36912=VERTEX_POINT('',#168741);
#36913=VERTEX_POINT('',#168782);
#36914=VERTEX_POINT('',#168784);
#36915=VERTEX_POINT('',#168828);
#36916=VERTEX_POINT('',#168830);
#36917=VERTEX_POINT('',#168832);
#36918=VERTEX_POINT('',#168834);
#36919=VERTEX_POINT('',#168875);
#36920=VERTEX_POINT('',#168877);
#36921=VERTEX_POINT('',#168921);
#36922=VERTEX_POINT('',#168923);
#36923=VERTEX_POINT('',#168925);
#36924=VERTEX_POINT('',#168927);
#36925=VERTEX_POINT('',#168968);
#36926=VERTEX_POINT('',#168970);
#36927=VERTEX_POINT('',#169014);
#36928=VERTEX_POINT('',#169016);
#36929=VERTEX_POINT('',#169018);
#36930=VERTEX_POINT('',#169020);
#36931=VERTEX_POINT('',#169061);
#36932=VERTEX_POINT('',#169063);
#36933=VERTEX_POINT('',#169107);
#36934=VERTEX_POINT('',#169109);
#36935=VERTEX_POINT('',#169111);
#36936=VERTEX_POINT('',#169113);
#36937=VERTEX_POINT('',#169154);
#36938=VERTEX_POINT('',#169156);
#36939=VERTEX_POINT('',#169200);
#36940=VERTEX_POINT('',#169202);
#36941=VERTEX_POINT('',#169204);
#36942=VERTEX_POINT('',#169206);
#36943=VERTEX_POINT('',#169247);
#36944=VERTEX_POINT('',#169249);
#36945=VERTEX_POINT('',#169293);
#36946=VERTEX_POINT('',#169295);
#36947=VERTEX_POINT('',#169297);
#36948=VERTEX_POINT('',#169299);
#36949=VERTEX_POINT('',#169340);
#36950=VERTEX_POINT('',#169342);
#36951=VERTEX_POINT('',#169386);
#36952=VERTEX_POINT('',#169388);
#36953=VERTEX_POINT('',#169390);
#36954=VERTEX_POINT('',#169392);
#36955=VERTEX_POINT('',#169433);
#36956=VERTEX_POINT('',#169435);
#36957=VERTEX_POINT('',#169479);
#36958=VERTEX_POINT('',#169481);
#36959=VERTEX_POINT('',#169483);
#36960=VERTEX_POINT('',#169485);
#36961=VERTEX_POINT('',#169526);
#36962=VERTEX_POINT('',#169528);
#36963=VERTEX_POINT('',#169572);
#36964=VERTEX_POINT('',#169574);
#36965=VERTEX_POINT('',#169576);
#36966=VERTEX_POINT('',#169578);
#36967=VERTEX_POINT('',#169619);
#36968=VERTEX_POINT('',#169621);
#36969=VERTEX_POINT('',#169665);
#36970=VERTEX_POINT('',#169667);
#36971=VERTEX_POINT('',#169669);
#36972=VERTEX_POINT('',#169671);
#36973=VERTEX_POINT('',#169712);
#36974=VERTEX_POINT('',#169714);
#36975=VERTEX_POINT('',#169758);
#36976=VERTEX_POINT('',#169760);
#36977=VERTEX_POINT('',#169762);
#36978=VERTEX_POINT('',#169764);
#36979=VERTEX_POINT('',#169805);
#36980=VERTEX_POINT('',#169807);
#36981=VERTEX_POINT('',#169851);
#36982=VERTEX_POINT('',#169853);
#36983=VERTEX_POINT('',#169855);
#36984=VERTEX_POINT('',#169857);
#36985=VERTEX_POINT('',#169898);
#36986=VERTEX_POINT('',#169900);
#36987=VERTEX_POINT('',#169944);
#36988=VERTEX_POINT('',#169946);
#36989=VERTEX_POINT('',#169948);
#36990=VERTEX_POINT('',#169950);
#36991=VERTEX_POINT('',#169991);
#36992=VERTEX_POINT('',#169993);
#36993=VERTEX_POINT('',#170037);
#36994=VERTEX_POINT('',#170039);
#36995=VERTEX_POINT('',#170041);
#36996=VERTEX_POINT('',#170043);
#36997=VERTEX_POINT('',#170084);
#36998=VERTEX_POINT('',#170086);
#36999=VERTEX_POINT('',#170130);
#37000=VERTEX_POINT('',#170132);
#37001=VERTEX_POINT('',#170134);
#37002=VERTEX_POINT('',#170136);
#37003=VERTEX_POINT('',#170177);
#37004=VERTEX_POINT('',#170179);
#37005=VERTEX_POINT('',#170223);
#37006=VERTEX_POINT('',#170225);
#37007=VERTEX_POINT('',#170227);
#37008=VERTEX_POINT('',#170229);
#37009=VERTEX_POINT('',#170270);
#37010=VERTEX_POINT('',#170272);
#37011=VERTEX_POINT('',#170316);
#37012=VERTEX_POINT('',#170318);
#37013=VERTEX_POINT('',#170320);
#37014=VERTEX_POINT('',#170322);
#37015=VERTEX_POINT('',#170363);
#37016=VERTEX_POINT('',#170365);
#37017=VERTEX_POINT('',#170409);
#37018=VERTEX_POINT('',#170411);
#37019=VERTEX_POINT('',#170413);
#37020=VERTEX_POINT('',#170456);
#37021=VERTEX_POINT('',#170500);
#37022=VERTEX_POINT('',#170502);
#37023=VERTEX_POINT('',#170504);
#37024=VERTEX_POINT('',#170506);
#37025=VERTEX_POINT('',#170547);
#37026=VERTEX_POINT('',#170549);
#37027=VERTEX_POINT('',#170593);
#37028=VERTEX_POINT('',#170595);
#37029=VERTEX_POINT('',#170597);
#37030=VERTEX_POINT('',#170599);
#37031=VERTEX_POINT('',#170640);
#37032=VERTEX_POINT('',#170642);
#37033=VERTEX_POINT('',#170686);
#37034=VERTEX_POINT('',#170688);
#37035=VERTEX_POINT('',#170690);
#37036=VERTEX_POINT('',#170692);
#37037=VERTEX_POINT('',#170733);
#37038=VERTEX_POINT('',#170735);
#37039=VERTEX_POINT('',#170779);
#37040=VERTEX_POINT('',#170781);
#37041=VERTEX_POINT('',#170783);
#37042=VERTEX_POINT('',#170785);
#37043=VERTEX_POINT('',#170826);
#37044=VERTEX_POINT('',#170828);
#37045=VERTEX_POINT('',#170872);
#37046=VERTEX_POINT('',#170874);
#37047=VERTEX_POINT('',#170876);
#37048=VERTEX_POINT('',#170878);
#37049=VERTEX_POINT('',#170919);
#37050=VERTEX_POINT('',#170921);
#37051=VERTEX_POINT('',#170965);
#37052=VERTEX_POINT('',#170967);
#37053=VERTEX_POINT('',#170969);
#37054=VERTEX_POINT('',#170971);
#37055=VERTEX_POINT('',#171012);
#37056=VERTEX_POINT('',#171014);
#37057=VERTEX_POINT('',#171058);
#37058=VERTEX_POINT('',#171060);
#37059=VERTEX_POINT('',#171062);
#37060=VERTEX_POINT('',#171064);
#37061=VERTEX_POINT('',#171105);
#37062=VERTEX_POINT('',#171107);
#37063=VERTEX_POINT('',#171151);
#37064=VERTEX_POINT('',#171153);
#37065=VERTEX_POINT('',#171155);
#37066=VERTEX_POINT('',#171157);
#37067=VERTEX_POINT('',#171198);
#37068=VERTEX_POINT('',#171200);
#37069=VERTEX_POINT('',#171244);
#37070=VERTEX_POINT('',#171246);
#37071=VERTEX_POINT('',#171248);
#37072=VERTEX_POINT('',#171250);
#37073=VERTEX_POINT('',#171291);
#37074=VERTEX_POINT('',#171293);
#37075=VERTEX_POINT('',#171337);
#37076=VERTEX_POINT('',#171339);
#37077=VERTEX_POINT('',#171341);
#37078=VERTEX_POINT('',#171343);
#37079=VERTEX_POINT('',#171384);
#37080=VERTEX_POINT('',#171386);
#37081=VERTEX_POINT('',#171430);
#37082=VERTEX_POINT('',#171432);
#37083=VERTEX_POINT('',#171434);
#37084=VERTEX_POINT('',#171436);
#37085=VERTEX_POINT('',#171477);
#37086=VERTEX_POINT('',#171479);
#37087=VERTEX_POINT('',#171523);
#37088=VERTEX_POINT('',#171525);
#37089=VERTEX_POINT('',#171527);
#37090=VERTEX_POINT('',#171529);
#37091=VERTEX_POINT('',#171570);
#37092=VERTEX_POINT('',#171572);
#37093=VERTEX_POINT('',#171616);
#37094=VERTEX_POINT('',#171618);
#37095=VERTEX_POINT('',#171620);
#37096=VERTEX_POINT('',#171622);
#37097=VERTEX_POINT('',#171663);
#37098=VERTEX_POINT('',#171665);
#37099=VERTEX_POINT('',#171709);
#37100=VERTEX_POINT('',#171711);
#37101=VERTEX_POINT('',#171713);
#37102=VERTEX_POINT('',#171715);
#37103=VERTEX_POINT('',#171756);
#37104=VERTEX_POINT('',#171758);
#37105=VERTEX_POINT('',#171802);
#37106=VERTEX_POINT('',#171804);
#37107=VERTEX_POINT('',#171806);
#37108=VERTEX_POINT('',#171848);
#37109=VERTEX_POINT('',#171892);
#37110=VERTEX_POINT('',#171894);
#37111=VERTEX_POINT('',#171896);
#37112=VERTEX_POINT('',#171898);
#37113=VERTEX_POINT('',#171939);
#37114=VERTEX_POINT('',#171941);
#37115=VERTEX_POINT('',#171985);
#37116=VERTEX_POINT('',#171987);
#37117=VERTEX_POINT('',#171989);
#37118=VERTEX_POINT('',#171991);
#37119=VERTEX_POINT('',#172032);
#37120=VERTEX_POINT('',#172034);
#37121=VERTEX_POINT('',#172078);
#37122=VERTEX_POINT('',#172080);
#37123=VERTEX_POINT('',#172082);
#37124=VERTEX_POINT('',#172084);
#37125=VERTEX_POINT('',#172125);
#37126=VERTEX_POINT('',#172127);
#37127=VERTEX_POINT('',#172171);
#37128=VERTEX_POINT('',#172173);
#37129=VERTEX_POINT('',#172175);
#37130=VERTEX_POINT('',#172177);
#37131=VERTEX_POINT('',#172218);
#37132=VERTEX_POINT('',#172220);
#37133=VERTEX_POINT('',#172264);
#37134=VERTEX_POINT('',#172266);
#37135=VERTEX_POINT('',#172268);
#37136=VERTEX_POINT('',#172270);
#37137=VERTEX_POINT('',#172311);
#37138=VERTEX_POINT('',#172313);
#37139=VERTEX_POINT('',#172357);
#37140=VERTEX_POINT('',#172359);
#37141=VERTEX_POINT('',#172361);
#37142=VERTEX_POINT('',#172363);
#37143=VERTEX_POINT('',#172404);
#37144=VERTEX_POINT('',#172406);
#37145=VERTEX_POINT('',#172450);
#37146=VERTEX_POINT('',#172452);
#37147=VERTEX_POINT('',#172454);
#37148=VERTEX_POINT('',#172456);
#37149=VERTEX_POINT('',#172497);
#37150=VERTEX_POINT('',#172499);
#37151=VERTEX_POINT('',#172543);
#37152=VERTEX_POINT('',#172545);
#37153=VERTEX_POINT('',#172547);
#37154=VERTEX_POINT('',#172549);
#37155=VERTEX_POINT('',#172590);
#37156=VERTEX_POINT('',#172592);
#37157=VERTEX_POINT('',#172636);
#37158=VERTEX_POINT('',#172638);
#37159=VERTEX_POINT('',#172640);
#37160=VERTEX_POINT('',#172642);
#37161=VERTEX_POINT('',#172683);
#37162=VERTEX_POINT('',#172685);
#37163=VERTEX_POINT('',#172729);
#37164=VERTEX_POINT('',#172731);
#37165=VERTEX_POINT('',#172733);
#37166=VERTEX_POINT('',#172735);
#37167=VERTEX_POINT('',#172776);
#37168=VERTEX_POINT('',#172778);
#37169=VERTEX_POINT('',#172822);
#37170=VERTEX_POINT('',#172824);
#37171=VERTEX_POINT('',#172826);
#37172=VERTEX_POINT('',#172828);
#37173=VERTEX_POINT('',#172869);
#37174=VERTEX_POINT('',#172871);
#37175=VERTEX_POINT('',#172915);
#37176=VERTEX_POINT('',#172917);
#37177=VERTEX_POINT('',#172919);
#37178=VERTEX_POINT('',#172921);
#37179=VERTEX_POINT('',#172962);
#37180=VERTEX_POINT('',#172964);
#37181=VERTEX_POINT('',#173008);
#37182=VERTEX_POINT('',#173010);
#37183=VERTEX_POINT('',#173012);
#37184=VERTEX_POINT('',#173014);
#37185=VERTEX_POINT('',#173055);
#37186=VERTEX_POINT('',#173057);
#37187=VERTEX_POINT('',#173101);
#37188=VERTEX_POINT('',#173103);
#37189=VERTEX_POINT('',#173105);
#37190=VERTEX_POINT('',#173107);
#37191=VERTEX_POINT('',#173148);
#37192=VERTEX_POINT('',#173150);
#37193=VERTEX_POINT('',#173194);
#37194=VERTEX_POINT('',#173196);
#37195=VERTEX_POINT('',#173198);
#37196=VERTEX_POINT('',#173241);
#37197=VERTEX_POINT('',#173279);
#37198=VERTEX_POINT('',#173281);
#37199=VERTEX_POINT('',#173283);
#37200=VERTEX_POINT('',#173285);
#37201=VERTEX_POINT('',#173326);
#37202=VERTEX_POINT('',#173328);
#37203=VERTEX_POINT('',#173366);
#37204=VERTEX_POINT('',#173368);
#37205=VERTEX_POINT('',#173370);
#37206=VERTEX_POINT('',#173372);
#37207=VERTEX_POINT('',#173413);
#37208=VERTEX_POINT('',#173415);
#37209=VERTEX_POINT('',#173453);
#37210=VERTEX_POINT('',#173455);
#37211=VERTEX_POINT('',#173457);
#37212=VERTEX_POINT('',#173459);
#37213=VERTEX_POINT('',#173500);
#37214=VERTEX_POINT('',#173502);
#37215=VERTEX_POINT('',#173540);
#37216=VERTEX_POINT('',#173542);
#37217=VERTEX_POINT('',#173544);
#37218=VERTEX_POINT('',#173546);
#37219=VERTEX_POINT('',#173587);
#37220=VERTEX_POINT('',#173589);
#37221=VERTEX_POINT('',#173627);
#37222=VERTEX_POINT('',#173629);
#37223=VERTEX_POINT('',#173631);
#37224=VERTEX_POINT('',#173633);
#37225=VERTEX_POINT('',#173674);
#37226=VERTEX_POINT('',#173676);
#37227=VERTEX_POINT('',#173714);
#37228=VERTEX_POINT('',#173716);
#37229=VERTEX_POINT('',#173718);
#37230=VERTEX_POINT('',#173720);
#37231=VERTEX_POINT('',#173761);
#37232=VERTEX_POINT('',#173763);
#37233=VERTEX_POINT('',#173801);
#37234=VERTEX_POINT('',#173803);
#37235=VERTEX_POINT('',#173805);
#37236=VERTEX_POINT('',#173807);
#37237=VERTEX_POINT('',#173848);
#37238=VERTEX_POINT('',#173850);
#37239=VERTEX_POINT('',#173888);
#37240=VERTEX_POINT('',#173890);
#37241=VERTEX_POINT('',#173892);
#37242=VERTEX_POINT('',#173894);
#37243=VERTEX_POINT('',#173935);
#37244=VERTEX_POINT('',#173937);
#37245=VERTEX_POINT('',#173975);
#37246=VERTEX_POINT('',#173977);
#37247=VERTEX_POINT('',#173979);
#37248=VERTEX_POINT('',#173981);
#37249=VERTEX_POINT('',#174022);
#37250=VERTEX_POINT('',#174024);
#37251=VERTEX_POINT('',#174062);
#37252=VERTEX_POINT('',#174064);
#37253=VERTEX_POINT('',#174066);
#37254=VERTEX_POINT('',#174068);
#37255=VERTEX_POINT('',#174109);
#37256=VERTEX_POINT('',#174111);
#37257=VERTEX_POINT('',#174149);
#37258=VERTEX_POINT('',#174151);
#37259=VERTEX_POINT('',#174153);
#37260=VERTEX_POINT('',#174155);
#37261=VERTEX_POINT('',#174196);
#37262=VERTEX_POINT('',#174198);
#37263=VERTEX_POINT('',#174236);
#37264=VERTEX_POINT('',#174238);
#37265=VERTEX_POINT('',#174240);
#37266=VERTEX_POINT('',#174242);
#37267=VERTEX_POINT('',#174283);
#37268=VERTEX_POINT('',#174285);
#37269=VERTEX_POINT('',#174323);
#37270=VERTEX_POINT('',#174325);
#37271=VERTEX_POINT('',#174327);
#37272=VERTEX_POINT('',#174329);
#37273=VERTEX_POINT('',#174370);
#37274=VERTEX_POINT('',#174372);
#37275=VERTEX_POINT('',#174410);
#37276=VERTEX_POINT('',#174412);
#37277=VERTEX_POINT('',#174414);
#37278=VERTEX_POINT('',#174416);
#37279=VERTEX_POINT('',#174457);
#37280=VERTEX_POINT('',#174459);
#37281=VERTEX_POINT('',#174497);
#37282=VERTEX_POINT('',#174499);
#37283=VERTEX_POINT('',#174501);
#37284=VERTEX_POINT('',#174503);
#37285=VERTEX_POINT('',#174544);
#37286=VERTEX_POINT('',#174546);
#37287=VERTEX_POINT('',#174584);
#37288=VERTEX_POINT('',#174586);
#37289=VERTEX_POINT('',#174588);
#37290=VERTEX_POINT('',#174590);
#37291=VERTEX_POINT('',#174631);
#37292=VERTEX_POINT('',#174633);
#37293=VERTEX_POINT('',#174671);
#37294=VERTEX_POINT('',#174673);
#37295=VERTEX_POINT('',#174675);
#37296=VERTEX_POINT('',#174677);
#37297=VERTEX_POINT('',#174718);
#37298=VERTEX_POINT('',#174720);
#37299=VERTEX_POINT('',#174758);
#37300=VERTEX_POINT('',#174760);
#37301=VERTEX_POINT('',#174762);
#37302=VERTEX_POINT('',#174764);
#37303=VERTEX_POINT('',#174805);
#37304=VERTEX_POINT('',#174807);
#37305=VERTEX_POINT('',#174845);
#37306=VERTEX_POINT('',#174847);
#37307=VERTEX_POINT('',#174849);
#37308=VERTEX_POINT('',#174851);
#37309=VERTEX_POINT('',#174892);
#37310=VERTEX_POINT('',#174894);
#37311=VERTEX_POINT('',#174932);
#37312=VERTEX_POINT('',#174934);
#37313=VERTEX_POINT('',#174936);
#37314=VERTEX_POINT('',#174938);
#37315=VERTEX_POINT('',#174979);
#37316=VERTEX_POINT('',#174981);
#37317=VERTEX_POINT('',#175019);
#37318=VERTEX_POINT('',#175021);
#37319=VERTEX_POINT('',#175023);
#37320=VERTEX_POINT('',#175025);
#37321=VERTEX_POINT('',#175066);
#37322=VERTEX_POINT('',#175068);
#37323=VERTEX_POINT('',#175106);
#37324=VERTEX_POINT('',#175108);
#37325=VERTEX_POINT('',#175110);
#37326=VERTEX_POINT('',#175112);
#37327=VERTEX_POINT('',#175153);
#37328=VERTEX_POINT('',#175155);
#37329=VERTEX_POINT('',#175193);
#37330=VERTEX_POINT('',#175195);
#37331=VERTEX_POINT('',#175197);
#37332=VERTEX_POINT('',#175199);
#37333=VERTEX_POINT('',#175240);
#37334=VERTEX_POINT('',#175242);
#37335=VERTEX_POINT('',#175280);
#37336=VERTEX_POINT('',#175282);
#37337=VERTEX_POINT('',#175284);
#37338=VERTEX_POINT('',#175286);
#37339=VERTEX_POINT('',#175327);
#37340=VERTEX_POINT('',#175329);
#37341=VERTEX_POINT('',#175367);
#37342=VERTEX_POINT('',#175369);
#37343=VERTEX_POINT('',#175371);
#37344=VERTEX_POINT('',#175373);
#37345=VERTEX_POINT('',#175414);
#37346=VERTEX_POINT('',#175416);
#37347=VERTEX_POINT('',#175454);
#37348=VERTEX_POINT('',#175456);
#37349=VERTEX_POINT('',#175458);
#37350=VERTEX_POINT('',#175460);
#37351=VERTEX_POINT('',#175501);
#37352=VERTEX_POINT('',#175503);
#37353=VERTEX_POINT('',#175541);
#37354=VERTEX_POINT('',#175543);
#37355=VERTEX_POINT('',#175545);
#37356=VERTEX_POINT('',#175547);
#37357=VERTEX_POINT('',#175588);
#37358=VERTEX_POINT('',#175590);
#37359=VERTEX_POINT('',#175628);
#37360=VERTEX_POINT('',#175630);
#37361=VERTEX_POINT('',#175632);
#37362=VERTEX_POINT('',#175634);
#37363=VERTEX_POINT('',#175675);
#37364=VERTEX_POINT('',#175677);
#37365=VERTEX_POINT('',#175715);
#37366=VERTEX_POINT('',#175717);
#37367=VERTEX_POINT('',#175719);
#37368=VERTEX_POINT('',#175721);
#37369=VERTEX_POINT('',#175762);
#37370=VERTEX_POINT('',#175764);
#37371=VERTEX_POINT('',#175802);
#37372=VERTEX_POINT('',#175804);
#37373=VERTEX_POINT('',#175806);
#37374=VERTEX_POINT('',#175808);
#37375=VERTEX_POINT('',#175849);
#37376=VERTEX_POINT('',#175852);
#37377=VERTEX_POINT('',#175854);
#37378=VERTEX_POINT('',#175892);
#37379=VERTEX_POINT('',#175894);
#37380=VERTEX_POINT('',#175896);
#37381=VERTEX_POINT('',#175898);
#37382=VERTEX_POINT('',#175939);
#37383=VERTEX_POINT('',#175941);
#37384=VERTEX_POINT('',#175979);
#37385=VERTEX_POINT('',#175981);
#37386=VERTEX_POINT('',#175983);
#37387=VERTEX_POINT('',#175985);
#37388=VERTEX_POINT('',#176026);
#37389=VERTEX_POINT('',#176028);
#37390=VERTEX_POINT('',#176066);
#37391=VERTEX_POINT('',#176068);
#37392=VERTEX_POINT('',#176070);
#37393=VERTEX_POINT('',#176072);
#37394=VERTEX_POINT('',#176113);
#37395=VERTEX_POINT('',#176115);
#37396=VERTEX_POINT('',#176153);
#37397=VERTEX_POINT('',#176155);
#37398=VERTEX_POINT('',#176157);
#37399=VERTEX_POINT('',#176159);
#37400=VERTEX_POINT('',#176200);
#37401=VERTEX_POINT('',#176202);
#37402=VERTEX_POINT('',#176240);
#37403=VERTEX_POINT('',#176242);
#37404=VERTEX_POINT('',#176244);
#37405=VERTEX_POINT('',#176246);
#37406=VERTEX_POINT('',#176287);
#37407=VERTEX_POINT('',#176289);
#37408=VERTEX_POINT('',#176327);
#37409=VERTEX_POINT('',#176329);
#37410=VERTEX_POINT('',#176331);
#37411=VERTEX_POINT('',#176333);
#37412=VERTEX_POINT('',#176374);
#37413=VERTEX_POINT('',#176376);
#37414=VERTEX_POINT('',#176414);
#37415=VERTEX_POINT('',#176416);
#37416=VERTEX_POINT('',#176418);
#37417=VERTEX_POINT('',#176420);
#37418=VERTEX_POINT('',#176461);
#37419=VERTEX_POINT('',#176463);
#37420=VERTEX_POINT('',#176501);
#37421=VERTEX_POINT('',#176503);
#37422=VERTEX_POINT('',#176505);
#37423=VERTEX_POINT('',#176507);
#37424=VERTEX_POINT('',#176548);
#37425=VERTEX_POINT('',#176550);
#37426=VERTEX_POINT('',#176588);
#37427=VERTEX_POINT('',#176590);
#37428=VERTEX_POINT('',#176592);
#37429=VERTEX_POINT('',#176594);
#37430=VERTEX_POINT('',#176635);
#37431=VERTEX_POINT('',#176637);
#37432=VERTEX_POINT('',#176675);
#37433=VERTEX_POINT('',#176677);
#37434=VERTEX_POINT('',#176679);
#37435=VERTEX_POINT('',#176681);
#37436=VERTEX_POINT('',#176722);
#37437=VERTEX_POINT('',#176724);
#37438=VERTEX_POINT('',#176762);
#37439=VERTEX_POINT('',#176764);
#37440=VERTEX_POINT('',#176766);
#37441=VERTEX_POINT('',#176768);
#37442=VERTEX_POINT('',#176809);
#37443=VERTEX_POINT('',#176811);
#37444=VERTEX_POINT('',#176849);
#37445=VERTEX_POINT('',#176851);
#37446=VERTEX_POINT('',#176853);
#37447=VERTEX_POINT('',#176855);
#37448=VERTEX_POINT('',#176896);
#37449=VERTEX_POINT('',#176898);
#37450=VERTEX_POINT('',#176936);
#37451=VERTEX_POINT('',#176938);
#37452=VERTEX_POINT('',#176940);
#37453=VERTEX_POINT('',#176942);
#37454=VERTEX_POINT('',#176983);
#37455=VERTEX_POINT('',#176985);
#37456=VERTEX_POINT('',#177023);
#37457=VERTEX_POINT('',#177025);
#37458=VERTEX_POINT('',#177027);
#37459=VERTEX_POINT('',#177029);
#37460=VERTEX_POINT('',#177070);
#37461=VERTEX_POINT('',#177072);
#37462=VERTEX_POINT('',#177110);
#37463=VERTEX_POINT('',#177112);
#37464=VERTEX_POINT('',#177114);
#37465=VERTEX_POINT('',#177156);
#37466=VERTEX_POINT('',#177194);
#37467=VERTEX_POINT('',#177196);
#37468=VERTEX_POINT('',#177198);
#37469=VERTEX_POINT('',#177200);
#37470=VERTEX_POINT('',#177241);
#37471=VERTEX_POINT('',#177243);
#37472=VERTEX_POINT('',#177281);
#37473=VERTEX_POINT('',#177283);
#37474=VERTEX_POINT('',#177285);
#37475=VERTEX_POINT('',#177287);
#37476=VERTEX_POINT('',#177328);
#37477=VERTEX_POINT('',#177330);
#37478=VERTEX_POINT('',#177368);
#37479=VERTEX_POINT('',#177370);
#37480=VERTEX_POINT('',#177372);
#37481=VERTEX_POINT('',#177374);
#37482=VERTEX_POINT('',#177415);
#37483=VERTEX_POINT('',#177417);
#37484=VERTEX_POINT('',#177455);
#37485=VERTEX_POINT('',#177457);
#37486=VERTEX_POINT('',#177459);
#37487=VERTEX_POINT('',#177461);
#37488=VERTEX_POINT('',#177502);
#37489=VERTEX_POINT('',#177504);
#37490=VERTEX_POINT('',#177542);
#37491=VERTEX_POINT('',#177544);
#37492=VERTEX_POINT('',#177546);
#37493=VERTEX_POINT('',#177548);
#37494=VERTEX_POINT('',#177589);
#37495=VERTEX_POINT('',#177591);
#37496=VERTEX_POINT('',#177629);
#37497=VERTEX_POINT('',#177631);
#37498=VERTEX_POINT('',#177633);
#37499=VERTEX_POINT('',#177635);
#37500=VERTEX_POINT('',#177676);
#37501=VERTEX_POINT('',#177678);
#37502=VERTEX_POINT('',#177716);
#37503=VERTEX_POINT('',#177718);
#37504=VERTEX_POINT('',#177720);
#37505=VERTEX_POINT('',#177722);
#37506=VERTEX_POINT('',#177763);
#37507=VERTEX_POINT('',#177765);
#37508=VERTEX_POINT('',#177803);
#37509=VERTEX_POINT('',#177805);
#37510=VERTEX_POINT('',#177807);
#37511=VERTEX_POINT('',#177809);
#37512=VERTEX_POINT('',#177850);
#37513=VERTEX_POINT('',#177852);
#37514=VERTEX_POINT('',#177890);
#37515=VERTEX_POINT('',#177892);
#37516=VERTEX_POINT('',#177894);
#37517=VERTEX_POINT('',#177896);
#37518=VERTEX_POINT('',#177937);
#37519=VERTEX_POINT('',#177939);
#37520=VERTEX_POINT('',#177977);
#37521=VERTEX_POINT('',#177979);
#37522=VERTEX_POINT('',#177981);
#37523=VERTEX_POINT('',#177983);
#37524=VERTEX_POINT('',#178024);
#37525=VERTEX_POINT('',#178026);
#37526=VERTEX_POINT('',#178064);
#37527=VERTEX_POINT('',#178066);
#37528=VERTEX_POINT('',#178068);
#37529=VERTEX_POINT('',#178070);
#37530=VERTEX_POINT('',#178111);
#37531=VERTEX_POINT('',#178113);
#37532=VERTEX_POINT('',#178151);
#37533=VERTEX_POINT('',#178153);
#37534=VERTEX_POINT('',#178155);
#37535=VERTEX_POINT('',#178157);
#37536=VERTEX_POINT('',#178198);
#37537=VERTEX_POINT('',#178200);
#37538=VERTEX_POINT('',#178238);
#37539=VERTEX_POINT('',#178240);
#37540=VERTEX_POINT('',#178242);
#37541=VERTEX_POINT('',#178244);
#37542=VERTEX_POINT('',#178285);
#37543=VERTEX_POINT('',#178287);
#37544=VERTEX_POINT('',#178325);
#37545=VERTEX_POINT('',#178327);
#37546=VERTEX_POINT('',#178329);
#37547=VERTEX_POINT('',#178331);
#37548=VERTEX_POINT('',#178372);
#37549=VERTEX_POINT('',#178374);
#37550=VERTEX_POINT('',#178412);
#37551=VERTEX_POINT('',#178414);
#37552=VERTEX_POINT('',#178416);
#37553=VERTEX_POINT('',#178459);
#37554=VERTEX_POINT('',#178460);
#37555=VERTEX_POINT('',#178465);
#37556=VERTEX_POINT('',#178469);
#37557=VERTEX_POINT('',#178470);
#37558=VERTEX_POINT('',#178472);
#37559=VERTEX_POINT('',#178474);
#37560=VERTEX_POINT('',#178476);
#37561=VERTEX_POINT('',#178478);
#37562=VERTEX_POINT('',#178482);
#37563=VERTEX_POINT('',#178483);
#37564=VERTEX_POINT('',#178488);
#37565=VERTEX_POINT('',#178489);
#37566=VERTEX_POINT('',#178491);
#37567=VERTEX_POINT('',#178493);
#37568=VERTEX_POINT('',#178497);
#37569=VERTEX_POINT('',#178498);
#37570=VERTEX_POINT('',#178500);
#37571=VERTEX_POINT('',#178502);
#37572=VERTEX_POINT('',#178504);
#37573=VERTEX_POINT('',#178506);
#37574=VERTEX_POINT('',#178510);
#37575=VERTEX_POINT('',#178511);
#37576=VERTEX_POINT('',#178528);
#37577=VERTEX_POINT('',#178529);
#37578=VERTEX_POINT('',#178531);
#37579=VERTEX_POINT('',#178533);
#37580=VERTEX_POINT('',#178535);
#37581=VERTEX_POINT('',#178537);
#37582=VERTEX_POINT('',#178541);
#37583=VERTEX_POINT('',#178543);
#37584=VERTEX_POINT('',#178547);
#37585=VERTEX_POINT('',#178548);
#37586=VERTEX_POINT('',#178550);
#37587=VERTEX_POINT('',#178552);
#37588=VERTEX_POINT('',#178556);
#37589=VERTEX_POINT('',#178557);
#37590=VERTEX_POINT('',#178559);
#37591=VERTEX_POINT('',#178561);
#37592=VERTEX_POINT('',#178563);
#37593=VERTEX_POINT('',#178565);
#37594=VERTEX_POINT('',#178569);
#37595=VERTEX_POINT('',#178571);
#37596=VERTEX_POINT('',#178587);
#37597=VERTEX_POINT('',#178588);
#37598=VERTEX_POINT('',#178590);
#37599=VERTEX_POINT('',#178592);
#37600=VERTEX_POINT('',#178594);
#37601=VERTEX_POINT('',#178596);
#37602=VERTEX_POINT('',#178600);
#37603=VERTEX_POINT('',#178602);
#37604=VERTEX_POINT('',#178606);
#37605=VERTEX_POINT('',#178607);
#37606=VERTEX_POINT('',#178609);
#37607=VERTEX_POINT('',#178611);
#37608=VERTEX_POINT('',#178615);
#37609=VERTEX_POINT('',#178616);
#37610=VERTEX_POINT('',#178618);
#37611=VERTEX_POINT('',#178620);
#37612=VERTEX_POINT('',#178622);
#37613=VERTEX_POINT('',#178624);
#37614=VERTEX_POINT('',#178628);
#37615=VERTEX_POINT('',#178630);
#37616=VERTEX_POINT('',#178646);
#37617=VERTEX_POINT('',#178647);
#37618=VERTEX_POINT('',#178649);
#37619=VERTEX_POINT('',#178651);
#37620=VERTEX_POINT('',#178653);
#37621=VERTEX_POINT('',#178655);
#37622=VERTEX_POINT('',#178659);
#37623=VERTEX_POINT('',#178661);
#37624=VERTEX_POINT('',#178665);
#37625=VERTEX_POINT('',#178666);
#37626=VERTEX_POINT('',#178668);
#37627=VERTEX_POINT('',#178670);
#37628=VERTEX_POINT('',#178674);
#37629=VERTEX_POINT('',#178675);
#37630=VERTEX_POINT('',#178677);
#37631=VERTEX_POINT('',#178679);
#37632=VERTEX_POINT('',#178681);
#37633=VERTEX_POINT('',#178683);
#37634=VERTEX_POINT('',#178687);
#37635=VERTEX_POINT('',#178689);
#37636=VERTEX_POINT('',#178705);
#37637=VERTEX_POINT('',#178706);
#37638=VERTEX_POINT('',#178708);
#37639=VERTEX_POINT('',#178710);
#37640=VERTEX_POINT('',#178712);
#37641=VERTEX_POINT('',#178714);
#37642=VERTEX_POINT('',#178718);
#37643=VERTEX_POINT('',#178720);
#37644=VERTEX_POINT('',#178724);
#37645=VERTEX_POINT('',#178725);
#37646=VERTEX_POINT('',#178727);
#37647=VERTEX_POINT('',#178729);
#37648=VERTEX_POINT('',#178733);
#37649=VERTEX_POINT('',#178734);
#37650=VERTEX_POINT('',#178736);
#37651=VERTEX_POINT('',#178738);
#37652=VERTEX_POINT('',#178740);
#37653=VERTEX_POINT('',#178742);
#37654=VERTEX_POINT('',#178746);
#37655=VERTEX_POINT('',#178748);
#37656=VERTEX_POINT('',#178764);
#37657=VERTEX_POINT('',#178765);
#37658=VERTEX_POINT('',#178767);
#37659=VERTEX_POINT('',#178769);
#37660=VERTEX_POINT('',#178771);
#37661=VERTEX_POINT('',#178773);
#37662=VERTEX_POINT('',#178777);
#37663=VERTEX_POINT('',#178779);
#37664=VERTEX_POINT('',#178783);
#37665=VERTEX_POINT('',#178784);
#37666=VERTEX_POINT('',#178786);
#37667=VERTEX_POINT('',#178788);
#37668=VERTEX_POINT('',#178792);
#37669=VERTEX_POINT('',#178793);
#37670=VERTEX_POINT('',#178795);
#37671=VERTEX_POINT('',#178797);
#37672=VERTEX_POINT('',#178799);
#37673=VERTEX_POINT('',#178801);
#37674=VERTEX_POINT('',#178805);
#37675=VERTEX_POINT('',#178807);
#37676=VERTEX_POINT('',#178823);
#37677=VERTEX_POINT('',#178824);
#37678=VERTEX_POINT('',#178826);
#37679=VERTEX_POINT('',#178828);
#37680=VERTEX_POINT('',#178830);
#37681=VERTEX_POINT('',#178832);
#37682=VERTEX_POINT('',#178836);
#37683=VERTEX_POINT('',#178838);
#37684=VERTEX_POINT('',#178842);
#37685=VERTEX_POINT('',#178843);
#37686=VERTEX_POINT('',#178845);
#37687=VERTEX_POINT('',#178847);
#37688=VERTEX_POINT('',#178851);
#37689=VERTEX_POINT('',#178852);
#37690=VERTEX_POINT('',#178854);
#37691=VERTEX_POINT('',#178856);
#37692=VERTEX_POINT('',#178858);
#37693=VERTEX_POINT('',#178860);
#37694=VERTEX_POINT('',#178864);
#37695=VERTEX_POINT('',#178866);
#37696=VERTEX_POINT('',#178882);
#37697=VERTEX_POINT('',#178883);
#37698=VERTEX_POINT('',#178885);
#37699=VERTEX_POINT('',#178887);
#37700=VERTEX_POINT('',#178889);
#37701=VERTEX_POINT('',#178891);
#37702=VERTEX_POINT('',#178895);
#37703=VERTEX_POINT('',#178897);
#37704=VERTEX_POINT('',#178901);
#37705=VERTEX_POINT('',#178902);
#37706=VERTEX_POINT('',#178904);
#37707=VERTEX_POINT('',#178906);
#37708=VERTEX_POINT('',#178910);
#37709=VERTEX_POINT('',#178911);
#37710=VERTEX_POINT('',#178913);
#37711=VERTEX_POINT('',#178915);
#37712=VERTEX_POINT('',#178917);
#37713=VERTEX_POINT('',#178919);
#37714=VERTEX_POINT('',#178923);
#37715=VERTEX_POINT('',#178925);
#37716=VERTEX_POINT('',#178941);
#37717=VERTEX_POINT('',#178942);
#37718=VERTEX_POINT('',#178944);
#37719=VERTEX_POINT('',#178946);
#37720=VERTEX_POINT('',#178948);
#37721=VERTEX_POINT('',#178950);
#37722=VERTEX_POINT('',#178954);
#37723=VERTEX_POINT('',#178956);
#37724=VERTEX_POINT('',#178960);
#37725=VERTEX_POINT('',#178961);
#37726=VERTEX_POINT('',#178963);
#37727=VERTEX_POINT('',#178965);
#37728=VERTEX_POINT('',#178969);
#37729=VERTEX_POINT('',#178970);
#37730=VERTEX_POINT('',#178972);
#37731=VERTEX_POINT('',#178974);
#37732=VERTEX_POINT('',#178976);
#37733=VERTEX_POINT('',#178978);
#37734=VERTEX_POINT('',#178982);
#37735=VERTEX_POINT('',#178984);
#37736=VERTEX_POINT('',#179000);
#37737=VERTEX_POINT('',#179001);
#37738=VERTEX_POINT('',#179003);
#37739=VERTEX_POINT('',#179005);
#37740=VERTEX_POINT('',#179007);
#37741=VERTEX_POINT('',#179009);
#37742=VERTEX_POINT('',#179013);
#37743=VERTEX_POINT('',#179015);
#37744=VERTEX_POINT('',#179019);
#37745=VERTEX_POINT('',#179020);
#37746=VERTEX_POINT('',#179022);
#37747=VERTEX_POINT('',#179024);
#37748=VERTEX_POINT('',#179028);
#37749=VERTEX_POINT('',#179029);
#37750=VERTEX_POINT('',#179031);
#37751=VERTEX_POINT('',#179033);
#37752=VERTEX_POINT('',#179035);
#37753=VERTEX_POINT('',#179037);
#37754=VERTEX_POINT('',#179041);
#37755=VERTEX_POINT('',#179043);
#37756=VERTEX_POINT('',#179059);
#37757=VERTEX_POINT('',#179060);
#37758=VERTEX_POINT('',#179062);
#37759=VERTEX_POINT('',#179064);
#37760=VERTEX_POINT('',#179066);
#37761=VERTEX_POINT('',#179068);
#37762=VERTEX_POINT('',#179072);
#37763=VERTEX_POINT('',#179074);
#37764=VERTEX_POINT('',#179078);
#37765=VERTEX_POINT('',#179079);
#37766=VERTEX_POINT('',#179081);
#37767=VERTEX_POINT('',#179083);
#37768=VERTEX_POINT('',#179087);
#37769=VERTEX_POINT('',#179088);
#37770=VERTEX_POINT('',#179090);
#37771=VERTEX_POINT('',#179092);
#37772=VERTEX_POINT('',#179094);
#37773=VERTEX_POINT('',#179096);
#37774=VERTEX_POINT('',#179100);
#37775=VERTEX_POINT('',#179102);
#37776=VERTEX_POINT('',#179118);
#37777=VERTEX_POINT('',#179119);
#37778=VERTEX_POINT('',#179121);
#37779=VERTEX_POINT('',#179123);
#37780=VERTEX_POINT('',#179125);
#37781=VERTEX_POINT('',#179127);
#37782=VERTEX_POINT('',#179131);
#37783=VERTEX_POINT('',#179133);
#37784=VERTEX_POINT('',#179137);
#37785=VERTEX_POINT('',#179138);
#37786=VERTEX_POINT('',#179140);
#37787=VERTEX_POINT('',#179142);
#37788=VERTEX_POINT('',#179146);
#37789=VERTEX_POINT('',#179147);
#37790=VERTEX_POINT('',#179149);
#37791=VERTEX_POINT('',#179151);
#37792=VERTEX_POINT('',#179153);
#37793=VERTEX_POINT('',#179155);
#37794=VERTEX_POINT('',#179159);
#37795=VERTEX_POINT('',#179161);
#37796=VERTEX_POINT('',#179177);
#37797=VERTEX_POINT('',#179178);
#37798=VERTEX_POINT('',#179180);
#37799=VERTEX_POINT('',#179182);
#37800=VERTEX_POINT('',#179184);
#37801=VERTEX_POINT('',#179186);
#37802=VERTEX_POINT('',#179190);
#37803=VERTEX_POINT('',#179192);
#37804=VERTEX_POINT('',#179196);
#37805=VERTEX_POINT('',#179197);
#37806=VERTEX_POINT('',#179199);
#37807=VERTEX_POINT('',#179201);
#37808=VERTEX_POINT('',#179205);
#37809=VERTEX_POINT('',#179206);
#37810=VERTEX_POINT('',#179208);
#37811=VERTEX_POINT('',#179210);
#37812=VERTEX_POINT('',#179212);
#37813=VERTEX_POINT('',#179214);
#37814=VERTEX_POINT('',#179218);
#37815=VERTEX_POINT('',#179220);
#37816=VERTEX_POINT('',#179236);
#37817=VERTEX_POINT('',#179237);
#37818=VERTEX_POINT('',#179239);
#37819=VERTEX_POINT('',#179241);
#37820=VERTEX_POINT('',#179243);
#37821=VERTEX_POINT('',#179245);
#37822=VERTEX_POINT('',#179249);
#37823=VERTEX_POINT('',#179251);
#37824=VERTEX_POINT('',#179255);
#37825=VERTEX_POINT('',#179256);
#37826=VERTEX_POINT('',#179258);
#37827=VERTEX_POINT('',#179260);
#37828=VERTEX_POINT('',#179264);
#37829=VERTEX_POINT('',#179265);
#37830=VERTEX_POINT('',#179267);
#37831=VERTEX_POINT('',#179269);
#37832=VERTEX_POINT('',#179271);
#37833=VERTEX_POINT('',#179273);
#37834=VERTEX_POINT('',#179277);
#37835=VERTEX_POINT('',#179279);
#37836=VERTEX_POINT('',#179295);
#37837=VERTEX_POINT('',#179296);
#37838=VERTEX_POINT('',#179298);
#37839=VERTEX_POINT('',#179300);
#37840=VERTEX_POINT('',#179302);
#37841=VERTEX_POINT('',#179304);
#37842=VERTEX_POINT('',#179308);
#37843=VERTEX_POINT('',#179310);
#37844=VERTEX_POINT('',#179314);
#37845=VERTEX_POINT('',#179315);
#37846=VERTEX_POINT('',#179317);
#37847=VERTEX_POINT('',#179319);
#37848=VERTEX_POINT('',#179323);
#37849=VERTEX_POINT('',#179324);
#37850=VERTEX_POINT('',#179326);
#37851=VERTEX_POINT('',#179328);
#37852=VERTEX_POINT('',#179330);
#37853=VERTEX_POINT('',#179332);
#37854=VERTEX_POINT('',#179336);
#37855=VERTEX_POINT('',#179338);
#37856=VERTEX_POINT('',#179354);
#37857=VERTEX_POINT('',#179355);
#37858=VERTEX_POINT('',#179357);
#37859=VERTEX_POINT('',#179359);
#37860=VERTEX_POINT('',#179361);
#37861=VERTEX_POINT('',#179363);
#37862=VERTEX_POINT('',#179367);
#37863=VERTEX_POINT('',#179369);
#37864=VERTEX_POINT('',#179373);
#37865=VERTEX_POINT('',#179374);
#37866=VERTEX_POINT('',#179376);
#37867=VERTEX_POINT('',#179378);
#37868=VERTEX_POINT('',#179382);
#37869=VERTEX_POINT('',#179383);
#37870=VERTEX_POINT('',#179385);
#37871=VERTEX_POINT('',#179387);
#37872=VERTEX_POINT('',#179389);
#37873=VERTEX_POINT('',#179391);
#37874=VERTEX_POINT('',#179395);
#37875=VERTEX_POINT('',#179397);
#37876=VERTEX_POINT('',#179413);
#37877=VERTEX_POINT('',#179414);
#37878=VERTEX_POINT('',#179416);
#37879=VERTEX_POINT('',#179418);
#37880=VERTEX_POINT('',#179420);
#37881=VERTEX_POINT('',#179422);
#37882=VERTEX_POINT('',#179426);
#37883=VERTEX_POINT('',#179428);
#37884=VERTEX_POINT('',#179432);
#37885=VERTEX_POINT('',#179433);
#37886=VERTEX_POINT('',#179435);
#37887=VERTEX_POINT('',#179437);
#37888=VERTEX_POINT('',#179441);
#37889=VERTEX_POINT('',#179442);
#37890=VERTEX_POINT('',#179444);
#37891=VERTEX_POINT('',#179446);
#37892=VERTEX_POINT('',#179448);
#37893=VERTEX_POINT('',#179450);
#37894=VERTEX_POINT('',#179454);
#37895=VERTEX_POINT('',#179456);
#37896=VERTEX_POINT('',#179472);
#37897=VERTEX_POINT('',#179473);
#37898=VERTEX_POINT('',#179475);
#37899=VERTEX_POINT('',#179477);
#37900=VERTEX_POINT('',#179479);
#37901=VERTEX_POINT('',#179481);
#37902=VERTEX_POINT('',#179485);
#37903=VERTEX_POINT('',#179487);
#37904=VERTEX_POINT('',#179491);
#37905=VERTEX_POINT('',#179492);
#37906=VERTEX_POINT('',#179494);
#37907=VERTEX_POINT('',#179496);
#37908=VERTEX_POINT('',#179500);
#37909=VERTEX_POINT('',#179501);
#37910=VERTEX_POINT('',#179503);
#37911=VERTEX_POINT('',#179505);
#37912=VERTEX_POINT('',#179507);
#37913=VERTEX_POINT('',#179509);
#37914=VERTEX_POINT('',#179513);
#37915=VERTEX_POINT('',#179515);
#37916=VERTEX_POINT('',#179531);
#37917=VERTEX_POINT('',#179532);
#37918=VERTEX_POINT('',#179534);
#37919=VERTEX_POINT('',#179536);
#37920=VERTEX_POINT('',#179538);
#37921=VERTEX_POINT('',#179540);
#37922=VERTEX_POINT('',#179544);
#37923=VERTEX_POINT('',#179546);
#37924=VERTEX_POINT('',#179550);
#37925=VERTEX_POINT('',#179551);
#37926=VERTEX_POINT('',#179553);
#37927=VERTEX_POINT('',#179555);
#37928=VERTEX_POINT('',#179559);
#37929=VERTEX_POINT('',#179560);
#37930=VERTEX_POINT('',#179562);
#37931=VERTEX_POINT('',#179564);
#37932=VERTEX_POINT('',#179566);
#37933=VERTEX_POINT('',#179568);
#37934=VERTEX_POINT('',#179572);
#37935=VERTEX_POINT('',#179574);
#37936=VERTEX_POINT('',#179590);
#37937=VERTEX_POINT('',#179591);
#37938=VERTEX_POINT('',#179593);
#37939=VERTEX_POINT('',#179595);
#37940=VERTEX_POINT('',#179597);
#37941=VERTEX_POINT('',#179599);
#37942=VERTEX_POINT('',#179603);
#37943=VERTEX_POINT('',#179605);
#37944=VERTEX_POINT('',#179609);
#37945=VERTEX_POINT('',#179610);
#37946=VERTEX_POINT('',#179612);
#37947=VERTEX_POINT('',#179614);
#37948=VERTEX_POINT('',#179618);
#37949=VERTEX_POINT('',#179619);
#37950=VERTEX_POINT('',#179621);
#37951=VERTEX_POINT('',#179623);
#37952=VERTEX_POINT('',#179625);
#37953=VERTEX_POINT('',#179627);
#37954=VERTEX_POINT('',#179631);
#37955=VERTEX_POINT('',#179633);
#37956=VERTEX_POINT('',#179649);
#37957=VERTEX_POINT('',#179650);
#37958=VERTEX_POINT('',#179652);
#37959=VERTEX_POINT('',#179654);
#37960=VERTEX_POINT('',#179656);
#37961=VERTEX_POINT('',#179658);
#37962=VERTEX_POINT('',#179662);
#37963=VERTEX_POINT('',#179664);
#37964=VERTEX_POINT('',#179668);
#37965=VERTEX_POINT('',#179669);
#37966=VERTEX_POINT('',#179671);
#37967=VERTEX_POINT('',#179673);
#37968=VERTEX_POINT('',#179677);
#37969=VERTEX_POINT('',#179678);
#37970=VERTEX_POINT('',#179680);
#37971=VERTEX_POINT('',#179682);
#37972=VERTEX_POINT('',#179684);
#37973=VERTEX_POINT('',#179686);
#37974=VERTEX_POINT('',#179690);
#37975=VERTEX_POINT('',#179692);
#37976=VERTEX_POINT('',#179708);
#37977=VERTEX_POINT('',#179709);
#37978=VERTEX_POINT('',#179711);
#37979=VERTEX_POINT('',#179713);
#37980=VERTEX_POINT('',#179715);
#37981=VERTEX_POINT('',#179717);
#37982=VERTEX_POINT('',#179721);
#37983=VERTEX_POINT('',#179723);
#37984=VERTEX_POINT('',#179727);
#37985=VERTEX_POINT('',#179728);
#37986=VERTEX_POINT('',#179730);
#37987=VERTEX_POINT('',#179732);
#37988=VERTEX_POINT('',#179736);
#37989=VERTEX_POINT('',#179737);
#37990=VERTEX_POINT('',#179739);
#37991=VERTEX_POINT('',#179741);
#37992=VERTEX_POINT('',#179743);
#37993=VERTEX_POINT('',#179745);
#37994=VERTEX_POINT('',#179749);
#37995=VERTEX_POINT('',#179751);
#37996=VERTEX_POINT('',#179767);
#37997=VERTEX_POINT('',#179768);
#37998=VERTEX_POINT('',#179770);
#37999=VERTEX_POINT('',#179772);
#38000=VERTEX_POINT('',#179774);
#38001=VERTEX_POINT('',#179776);
#38002=VERTEX_POINT('',#179780);
#38003=VERTEX_POINT('',#179782);
#38004=VERTEX_POINT('',#179786);
#38005=VERTEX_POINT('',#179787);
#38006=VERTEX_POINT('',#179789);
#38007=VERTEX_POINT('',#179791);
#38008=VERTEX_POINT('',#179795);
#38009=VERTEX_POINT('',#179796);
#38010=VERTEX_POINT('',#179798);
#38011=VERTEX_POINT('',#179800);
#38012=VERTEX_POINT('',#179802);
#38013=VERTEX_POINT('',#179804);
#38014=VERTEX_POINT('',#179808);
#38015=VERTEX_POINT('',#179810);
#38016=VERTEX_POINT('',#179826);
#38017=VERTEX_POINT('',#179827);
#38018=VERTEX_POINT('',#179829);
#38019=VERTEX_POINT('',#179831);
#38020=VERTEX_POINT('',#179833);
#38021=VERTEX_POINT('',#179835);
#38022=VERTEX_POINT('',#179839);
#38023=VERTEX_POINT('',#179841);
#38024=VERTEX_POINT('',#179845);
#38025=VERTEX_POINT('',#179846);
#38026=VERTEX_POINT('',#179848);
#38027=VERTEX_POINT('',#179850);
#38028=VERTEX_POINT('',#179854);
#38029=VERTEX_POINT('',#179855);
#38030=VERTEX_POINT('',#179857);
#38031=VERTEX_POINT('',#179859);
#38032=VERTEX_POINT('',#179861);
#38033=VERTEX_POINT('',#179863);
#38034=VERTEX_POINT('',#179867);
#38035=VERTEX_POINT('',#179869);
#38036=VERTEX_POINT('',#179885);
#38037=VERTEX_POINT('',#179886);
#38038=VERTEX_POINT('',#179888);
#38039=VERTEX_POINT('',#179890);
#38040=VERTEX_POINT('',#179892);
#38041=VERTEX_POINT('',#179894);
#38042=VERTEX_POINT('',#179898);
#38043=VERTEX_POINT('',#179900);
#38044=VERTEX_POINT('',#179904);
#38045=VERTEX_POINT('',#179905);
#38046=VERTEX_POINT('',#179907);
#38047=VERTEX_POINT('',#179909);
#38048=VERTEX_POINT('',#179913);
#38049=VERTEX_POINT('',#179914);
#38050=VERTEX_POINT('',#179916);
#38051=VERTEX_POINT('',#179918);
#38052=VERTEX_POINT('',#179920);
#38053=VERTEX_POINT('',#179922);
#38054=VERTEX_POINT('',#179926);
#38055=VERTEX_POINT('',#179928);
#38056=VERTEX_POINT('',#179944);
#38057=VERTEX_POINT('',#179945);
#38058=VERTEX_POINT('',#179947);
#38059=VERTEX_POINT('',#179949);
#38060=VERTEX_POINT('',#179951);
#38061=VERTEX_POINT('',#179953);
#38062=VERTEX_POINT('',#179957);
#38063=VERTEX_POINT('',#179959);
#38064=VERTEX_POINT('',#179963);
#38065=VERTEX_POINT('',#179964);
#38066=VERTEX_POINT('',#179966);
#38067=VERTEX_POINT('',#179968);
#38068=VERTEX_POINT('',#179972);
#38069=VERTEX_POINT('',#179973);
#38070=VERTEX_POINT('',#179975);
#38071=VERTEX_POINT('',#179977);
#38072=VERTEX_POINT('',#179979);
#38073=VERTEX_POINT('',#179981);
#38074=VERTEX_POINT('',#179985);
#38075=VERTEX_POINT('',#179987);
#38076=VERTEX_POINT('',#180003);
#38077=VERTEX_POINT('',#180004);
#38078=VERTEX_POINT('',#180006);
#38079=VERTEX_POINT('',#180008);
#38080=VERTEX_POINT('',#180010);
#38081=VERTEX_POINT('',#180012);
#38082=VERTEX_POINT('',#180016);
#38083=VERTEX_POINT('',#180018);
#38084=VERTEX_POINT('',#180022);
#38085=VERTEX_POINT('',#180023);
#38086=VERTEX_POINT('',#180025);
#38087=VERTEX_POINT('',#180027);
#38088=VERTEX_POINT('',#180031);
#38089=VERTEX_POINT('',#180032);
#38090=VERTEX_POINT('',#180034);
#38091=VERTEX_POINT('',#180036);
#38092=VERTEX_POINT('',#180038);
#38093=VERTEX_POINT('',#180040);
#38094=VERTEX_POINT('',#180044);
#38095=VERTEX_POINT('',#180046);
#38096=VERTEX_POINT('',#180062);
#38097=VERTEX_POINT('',#180063);
#38098=VERTEX_POINT('',#180065);
#38099=VERTEX_POINT('',#180067);
#38100=VERTEX_POINT('',#180069);
#38101=VERTEX_POINT('',#180071);
#38102=VERTEX_POINT('',#180075);
#38103=VERTEX_POINT('',#180077);
#38104=VERTEX_POINT('',#180081);
#38105=VERTEX_POINT('',#180082);
#38106=VERTEX_POINT('',#180084);
#38107=VERTEX_POINT('',#180086);
#38108=VERTEX_POINT('',#180090);
#38109=VERTEX_POINT('',#180091);
#38110=VERTEX_POINT('',#180093);
#38111=VERTEX_POINT('',#180095);
#38112=VERTEX_POINT('',#180097);
#38113=VERTEX_POINT('',#180099);
#38114=VERTEX_POINT('',#180103);
#38115=VERTEX_POINT('',#180105);
#38116=VERTEX_POINT('',#180121);
#38117=VERTEX_POINT('',#180122);
#38118=VERTEX_POINT('',#180124);
#38119=VERTEX_POINT('',#180126);
#38120=VERTEX_POINT('',#180128);
#38121=VERTEX_POINT('',#180130);
#38122=VERTEX_POINT('',#180134);
#38123=VERTEX_POINT('',#180136);
#38124=VERTEX_POINT('',#180140);
#38125=VERTEX_POINT('',#180141);
#38126=VERTEX_POINT('',#180143);
#38127=VERTEX_POINT('',#180145);
#38128=VERTEX_POINT('',#180149);
#38129=VERTEX_POINT('',#180150);
#38130=VERTEX_POINT('',#180152);
#38131=VERTEX_POINT('',#180154);
#38132=VERTEX_POINT('',#180156);
#38133=VERTEX_POINT('',#180158);
#38134=VERTEX_POINT('',#180162);
#38135=VERTEX_POINT('',#180164);
#38136=VERTEX_POINT('',#180180);
#38137=VERTEX_POINT('',#180181);
#38138=VERTEX_POINT('',#180183);
#38139=VERTEX_POINT('',#180185);
#38140=VERTEX_POINT('',#180187);
#38141=VERTEX_POINT('',#180189);
#38142=VERTEX_POINT('',#180193);
#38143=VERTEX_POINT('',#180195);
#38144=VERTEX_POINT('',#180199);
#38145=VERTEX_POINT('',#180200);
#38146=VERTEX_POINT('',#180202);
#38147=VERTEX_POINT('',#180204);
#38148=VERTEX_POINT('',#180208);
#38149=VERTEX_POINT('',#180209);
#38150=VERTEX_POINT('',#180211);
#38151=VERTEX_POINT('',#180213);
#38152=VERTEX_POINT('',#180215);
#38153=VERTEX_POINT('',#180217);
#38154=VERTEX_POINT('',#180221);
#38155=VERTEX_POINT('',#180223);
#38156=VERTEX_POINT('',#180239);
#38157=VERTEX_POINT('',#180240);
#38158=VERTEX_POINT('',#180242);
#38159=VERTEX_POINT('',#180244);
#38160=VERTEX_POINT('',#180246);
#38161=VERTEX_POINT('',#180248);
#38162=VERTEX_POINT('',#180252);
#38163=VERTEX_POINT('',#180254);
#38164=VERTEX_POINT('',#180258);
#38165=VERTEX_POINT('',#180259);
#38166=VERTEX_POINT('',#180261);
#38167=VERTEX_POINT('',#180263);
#38168=VERTEX_POINT('',#180267);
#38169=VERTEX_POINT('',#180268);
#38170=VERTEX_POINT('',#180270);
#38171=VERTEX_POINT('',#180272);
#38172=VERTEX_POINT('',#180274);
#38173=VERTEX_POINT('',#180276);
#38174=VERTEX_POINT('',#180280);
#38175=VERTEX_POINT('',#180282);
#38176=VERTEX_POINT('',#180298);
#38177=VERTEX_POINT('',#180299);
#38178=VERTEX_POINT('',#180301);
#38179=VERTEX_POINT('',#180303);
#38180=VERTEX_POINT('',#180305);
#38181=VERTEX_POINT('',#180307);
#38182=VERTEX_POINT('',#180311);
#38183=VERTEX_POINT('',#180313);
#38184=VERTEX_POINT('',#180317);
#38185=VERTEX_POINT('',#180318);
#38186=VERTEX_POINT('',#180320);
#38187=VERTEX_POINT('',#180322);
#38188=VERTEX_POINT('',#180326);
#38189=VERTEX_POINT('',#180327);
#38190=VERTEX_POINT('',#180329);
#38191=VERTEX_POINT('',#180331);
#38192=VERTEX_POINT('',#180333);
#38193=VERTEX_POINT('',#180335);
#38194=VERTEX_POINT('',#180339);
#38195=VERTEX_POINT('',#180341);
#38196=VERTEX_POINT('',#180357);
#38197=VERTEX_POINT('',#180358);
#38198=VERTEX_POINT('',#180360);
#38199=VERTEX_POINT('',#180362);
#38200=VERTEX_POINT('',#180364);
#38201=VERTEX_POINT('',#180366);
#38202=VERTEX_POINT('',#180370);
#38203=VERTEX_POINT('',#180372);
#38204=VERTEX_POINT('',#180376);
#38205=VERTEX_POINT('',#180377);
#38206=VERTEX_POINT('',#180379);
#38207=VERTEX_POINT('',#180381);
#38208=VERTEX_POINT('',#180385);
#38209=VERTEX_POINT('',#180386);
#38210=VERTEX_POINT('',#180388);
#38211=VERTEX_POINT('',#180390);
#38212=VERTEX_POINT('',#180392);
#38213=VERTEX_POINT('',#180394);
#38214=VERTEX_POINT('',#180398);
#38215=VERTEX_POINT('',#180400);
#38216=VERTEX_POINT('',#180416);
#38217=VERTEX_POINT('',#180417);
#38218=VERTEX_POINT('',#180419);
#38219=VERTEX_POINT('',#180421);
#38220=VERTEX_POINT('',#180423);
#38221=VERTEX_POINT('',#180425);
#38222=VERTEX_POINT('',#180429);
#38223=VERTEX_POINT('',#180431);
#38224=VERTEX_POINT('',#180435);
#38225=VERTEX_POINT('',#180436);
#38226=VERTEX_POINT('',#180438);
#38227=VERTEX_POINT('',#180440);
#38228=VERTEX_POINT('',#180444);
#38229=VERTEX_POINT('',#180445);
#38230=VERTEX_POINT('',#180447);
#38231=VERTEX_POINT('',#180449);
#38232=VERTEX_POINT('',#180451);
#38233=VERTEX_POINT('',#180453);
#38234=VERTEX_POINT('',#180457);
#38235=VERTEX_POINT('',#180459);
#38236=VERTEX_POINT('',#180475);
#38237=VERTEX_POINT('',#180476);
#38238=VERTEX_POINT('',#180478);
#38239=VERTEX_POINT('',#180480);
#38240=VERTEX_POINT('',#180482);
#38241=VERTEX_POINT('',#180484);
#38242=VERTEX_POINT('',#180488);
#38243=VERTEX_POINT('',#180490);
#38244=VERTEX_POINT('',#180494);
#38245=VERTEX_POINT('',#180495);
#38246=VERTEX_POINT('',#180497);
#38247=VERTEX_POINT('',#180499);
#38248=VERTEX_POINT('',#180503);
#38249=VERTEX_POINT('',#180504);
#38250=VERTEX_POINT('',#180506);
#38251=VERTEX_POINT('',#180508);
#38252=VERTEX_POINT('',#180510);
#38253=VERTEX_POINT('',#180512);
#38254=VERTEX_POINT('',#180516);
#38255=VERTEX_POINT('',#180518);
#38256=VERTEX_POINT('',#180534);
#38257=VERTEX_POINT('',#180535);
#38258=VERTEX_POINT('',#180537);
#38259=VERTEX_POINT('',#180539);
#38260=VERTEX_POINT('',#180541);
#38261=VERTEX_POINT('',#180543);
#38262=VERTEX_POINT('',#180547);
#38263=VERTEX_POINT('',#180549);
#38264=VERTEX_POINT('',#180553);
#38265=VERTEX_POINT('',#180554);
#38266=VERTEX_POINT('',#180556);
#38267=VERTEX_POINT('',#180558);
#38268=VERTEX_POINT('',#180562);
#38269=VERTEX_POINT('',#180563);
#38270=VERTEX_POINT('',#180565);
#38271=VERTEX_POINT('',#180567);
#38272=VERTEX_POINT('',#180569);
#38273=VERTEX_POINT('',#180571);
#38274=VERTEX_POINT('',#180575);
#38275=VERTEX_POINT('',#180577);
#38276=VERTEX_POINT('',#180593);
#38277=VERTEX_POINT('',#180594);
#38278=VERTEX_POINT('',#180596);
#38279=VERTEX_POINT('',#180598);
#38280=VERTEX_POINT('',#180600);
#38281=VERTEX_POINT('',#180602);
#38282=VERTEX_POINT('',#180606);
#38283=VERTEX_POINT('',#180608);
#38284=VERTEX_POINT('',#180612);
#38285=VERTEX_POINT('',#180613);
#38286=VERTEX_POINT('',#180615);
#38287=VERTEX_POINT('',#180617);
#38288=VERTEX_POINT('',#180621);
#38289=VERTEX_POINT('',#180622);
#38290=VERTEX_POINT('',#180624);
#38291=VERTEX_POINT('',#180626);
#38292=VERTEX_POINT('',#180628);
#38293=VERTEX_POINT('',#180630);
#38294=VERTEX_POINT('',#180634);
#38295=VERTEX_POINT('',#180636);
#38296=VERTEX_POINT('',#180652);
#38297=VERTEX_POINT('',#180653);
#38298=VERTEX_POINT('',#180655);
#38299=VERTEX_POINT('',#180657);
#38300=VERTEX_POINT('',#180659);
#38301=VERTEX_POINT('',#180661);
#38302=VERTEX_POINT('',#180665);
#38303=VERTEX_POINT('',#180667);
#38304=VERTEX_POINT('',#180671);
#38305=VERTEX_POINT('',#180672);
#38306=VERTEX_POINT('',#180674);
#38307=VERTEX_POINT('',#180676);
#38308=VERTEX_POINT('',#180680);
#38309=VERTEX_POINT('',#180681);
#38310=VERTEX_POINT('',#180683);
#38311=VERTEX_POINT('',#180685);
#38312=VERTEX_POINT('',#180687);
#38313=VERTEX_POINT('',#180689);
#38314=VERTEX_POINT('',#180693);
#38315=VERTEX_POINT('',#180695);
#38316=VERTEX_POINT('',#180711);
#38317=VERTEX_POINT('',#180712);
#38318=VERTEX_POINT('',#180714);
#38319=VERTEX_POINT('',#180716);
#38320=VERTEX_POINT('',#180718);
#38321=VERTEX_POINT('',#180720);
#38322=VERTEX_POINT('',#180724);
#38323=VERTEX_POINT('',#180726);
#38324=VERTEX_POINT('',#180730);
#38325=VERTEX_POINT('',#180731);
#38326=VERTEX_POINT('',#180733);
#38327=VERTEX_POINT('',#180735);
#38328=VERTEX_POINT('',#180739);
#38329=VERTEX_POINT('',#180740);
#38330=VERTEX_POINT('',#180742);
#38331=VERTEX_POINT('',#180744);
#38332=VERTEX_POINT('',#180746);
#38333=VERTEX_POINT('',#180748);
#38334=VERTEX_POINT('',#180752);
#38335=VERTEX_POINT('',#180754);
#38336=VERTEX_POINT('',#180770);
#38337=VERTEX_POINT('',#180771);
#38338=VERTEX_POINT('',#180773);
#38339=VERTEX_POINT('',#180775);
#38340=VERTEX_POINT('',#180777);
#38341=VERTEX_POINT('',#180779);
#38342=VERTEX_POINT('',#180783);
#38343=VERTEX_POINT('',#180785);
#38344=VERTEX_POINT('',#180789);
#38345=VERTEX_POINT('',#180790);
#38346=VERTEX_POINT('',#180792);
#38347=VERTEX_POINT('',#180794);
#38348=VERTEX_POINT('',#180798);
#38349=VERTEX_POINT('',#180799);
#38350=VERTEX_POINT('',#180801);
#38351=VERTEX_POINT('',#180803);
#38352=VERTEX_POINT('',#180805);
#38353=VERTEX_POINT('',#180807);
#38354=VERTEX_POINT('',#180811);
#38355=VERTEX_POINT('',#180813);
#38356=VERTEX_POINT('',#180829);
#38357=VERTEX_POINT('',#180830);
#38358=VERTEX_POINT('',#180832);
#38359=VERTEX_POINT('',#180834);
#38360=VERTEX_POINT('',#180836);
#38361=VERTEX_POINT('',#180838);
#38362=VERTEX_POINT('',#180842);
#38363=VERTEX_POINT('',#180844);
#38364=VERTEX_POINT('',#180848);
#38365=VERTEX_POINT('',#180849);
#38366=VERTEX_POINT('',#180851);
#38367=VERTEX_POINT('',#180853);
#38368=VERTEX_POINT('',#180857);
#38369=VERTEX_POINT('',#180858);
#38370=VERTEX_POINT('',#180860);
#38371=VERTEX_POINT('',#180862);
#38372=VERTEX_POINT('',#180864);
#38373=VERTEX_POINT('',#180866);
#38374=VERTEX_POINT('',#180870);
#38375=VERTEX_POINT('',#180872);
#38376=VERTEX_POINT('',#180888);
#38377=VERTEX_POINT('',#180889);
#38378=VERTEX_POINT('',#180891);
#38379=VERTEX_POINT('',#180893);
#38380=VERTEX_POINT('',#180895);
#38381=VERTEX_POINT('',#180897);
#38382=VERTEX_POINT('',#180901);
#38383=VERTEX_POINT('',#180903);
#38384=VERTEX_POINT('',#180907);
#38385=VERTEX_POINT('',#180908);
#38386=VERTEX_POINT('',#180910);
#38387=VERTEX_POINT('',#180912);
#38388=VERTEX_POINT('',#180916);
#38389=VERTEX_POINT('',#180917);
#38390=VERTEX_POINT('',#180919);
#38391=VERTEX_POINT('',#180921);
#38392=VERTEX_POINT('',#180923);
#38393=VERTEX_POINT('',#180925);
#38394=VERTEX_POINT('',#180929);
#38395=VERTEX_POINT('',#180931);
#38396=VERTEX_POINT('',#180947);
#38397=VERTEX_POINT('',#180948);
#38398=VERTEX_POINT('',#180950);
#38399=VERTEX_POINT('',#180952);
#38400=VERTEX_POINT('',#180954);
#38401=VERTEX_POINT('',#180956);
#38402=VERTEX_POINT('',#180960);
#38403=VERTEX_POINT('',#180962);
#38404=VERTEX_POINT('',#180966);
#38405=VERTEX_POINT('',#180967);
#38406=VERTEX_POINT('',#180969);
#38407=VERTEX_POINT('',#180971);
#38408=VERTEX_POINT('',#180975);
#38409=VERTEX_POINT('',#180976);
#38410=VERTEX_POINT('',#180978);
#38411=VERTEX_POINT('',#180980);
#38412=VERTEX_POINT('',#180982);
#38413=VERTEX_POINT('',#180984);
#38414=VERTEX_POINT('',#180988);
#38415=VERTEX_POINT('',#180990);
#38416=VERTEX_POINT('',#181006);
#38417=VERTEX_POINT('',#181007);
#38418=VERTEX_POINT('',#181009);
#38419=VERTEX_POINT('',#181011);
#38420=VERTEX_POINT('',#181013);
#38421=VERTEX_POINT('',#181015);
#38422=VERTEX_POINT('',#181019);
#38423=VERTEX_POINT('',#181021);
#38424=VERTEX_POINT('',#181025);
#38425=VERTEX_POINT('',#181026);
#38426=VERTEX_POINT('',#181028);
#38427=VERTEX_POINT('',#181030);
#38428=VERTEX_POINT('',#181034);
#38429=VERTEX_POINT('',#181035);
#38430=VERTEX_POINT('',#181037);
#38431=VERTEX_POINT('',#181039);
#38432=VERTEX_POINT('',#181041);
#38433=VERTEX_POINT('',#181043);
#38434=VERTEX_POINT('',#181047);
#38435=VERTEX_POINT('',#181049);
#38436=VERTEX_POINT('',#181065);
#38437=VERTEX_POINT('',#181066);
#38438=VERTEX_POINT('',#181068);
#38439=VERTEX_POINT('',#181070);
#38440=VERTEX_POINT('',#181072);
#38441=VERTEX_POINT('',#181074);
#38442=VERTEX_POINT('',#181078);
#38443=VERTEX_POINT('',#181080);
#38444=VERTEX_POINT('',#181084);
#38445=VERTEX_POINT('',#181085);
#38446=VERTEX_POINT('',#181087);
#38447=VERTEX_POINT('',#181089);
#38448=VERTEX_POINT('',#181093);
#38449=VERTEX_POINT('',#181094);
#38450=VERTEX_POINT('',#181096);
#38451=VERTEX_POINT('',#181098);
#38452=VERTEX_POINT('',#181100);
#38453=VERTEX_POINT('',#181102);
#38454=VERTEX_POINT('',#181106);
#38455=VERTEX_POINT('',#181108);
#38456=VERTEX_POINT('',#181124);
#38457=VERTEX_POINT('',#181125);
#38458=VERTEX_POINT('',#181127);
#38459=VERTEX_POINT('',#181129);
#38460=VERTEX_POINT('',#181131);
#38461=VERTEX_POINT('',#181133);
#38462=VERTEX_POINT('',#181137);
#38463=VERTEX_POINT('',#181139);
#38464=VERTEX_POINT('',#181143);
#38465=VERTEX_POINT('',#181144);
#38466=VERTEX_POINT('',#181146);
#38467=VERTEX_POINT('',#181148);
#38468=VERTEX_POINT('',#181152);
#38469=VERTEX_POINT('',#181153);
#38470=VERTEX_POINT('',#181155);
#38471=VERTEX_POINT('',#181157);
#38472=VERTEX_POINT('',#181159);
#38473=VERTEX_POINT('',#181161);
#38474=VERTEX_POINT('',#181165);
#38475=VERTEX_POINT('',#181167);
#38476=VERTEX_POINT('',#181183);
#38477=VERTEX_POINT('',#181184);
#38478=VERTEX_POINT('',#181186);
#38479=VERTEX_POINT('',#181188);
#38480=VERTEX_POINT('',#181190);
#38481=VERTEX_POINT('',#181192);
#38482=VERTEX_POINT('',#181196);
#38483=VERTEX_POINT('',#181198);
#38484=VERTEX_POINT('',#181202);
#38485=VERTEX_POINT('',#181203);
#38486=VERTEX_POINT('',#181205);
#38487=VERTEX_POINT('',#181207);
#38488=VERTEX_POINT('',#181211);
#38489=VERTEX_POINT('',#181212);
#38490=VERTEX_POINT('',#181214);
#38491=VERTEX_POINT('',#181216);
#38492=VERTEX_POINT('',#181218);
#38493=VERTEX_POINT('',#181220);
#38494=VERTEX_POINT('',#181224);
#38495=VERTEX_POINT('',#181226);
#38496=VERTEX_POINT('',#181242);
#38497=VERTEX_POINT('',#181243);
#38498=VERTEX_POINT('',#181245);
#38499=VERTEX_POINT('',#181247);
#38500=VERTEX_POINT('',#181249);
#38501=VERTEX_POINT('',#181251);
#38502=VERTEX_POINT('',#181255);
#38503=VERTEX_POINT('',#181257);
#38504=VERTEX_POINT('',#181261);
#38505=VERTEX_POINT('',#181262);
#38506=VERTEX_POINT('',#181264);
#38507=VERTEX_POINT('',#181266);
#38508=VERTEX_POINT('',#181270);
#38509=VERTEX_POINT('',#181271);
#38510=VERTEX_POINT('',#181273);
#38511=VERTEX_POINT('',#181275);
#38512=VERTEX_POINT('',#181277);
#38513=VERTEX_POINT('',#181279);
#38514=VERTEX_POINT('',#181283);
#38515=VERTEX_POINT('',#181285);
#38516=VERTEX_POINT('',#181301);
#38517=VERTEX_POINT('',#181302);
#38518=VERTEX_POINT('',#181304);
#38519=VERTEX_POINT('',#181306);
#38520=VERTEX_POINT('',#181308);
#38521=VERTEX_POINT('',#181310);
#38522=VERTEX_POINT('',#181314);
#38523=VERTEX_POINT('',#181316);
#38524=VERTEX_POINT('',#181320);
#38525=VERTEX_POINT('',#181321);
#38526=VERTEX_POINT('',#181323);
#38527=VERTEX_POINT('',#181325);
#38528=VERTEX_POINT('',#181329);
#38529=VERTEX_POINT('',#181330);
#38530=VERTEX_POINT('',#181332);
#38531=VERTEX_POINT('',#181334);
#38532=VERTEX_POINT('',#181336);
#38533=VERTEX_POINT('',#181338);
#38534=VERTEX_POINT('',#181342);
#38535=VERTEX_POINT('',#181344);
#38536=VERTEX_POINT('',#181360);
#38537=VERTEX_POINT('',#181361);
#38538=VERTEX_POINT('',#181363);
#38539=VERTEX_POINT('',#181365);
#38540=VERTEX_POINT('',#181367);
#38541=VERTEX_POINT('',#181369);
#38542=VERTEX_POINT('',#181373);
#38543=VERTEX_POINT('',#181375);
#38544=VERTEX_POINT('',#181379);
#38545=VERTEX_POINT('',#181380);
#38546=VERTEX_POINT('',#181382);
#38547=VERTEX_POINT('',#181384);
#38548=VERTEX_POINT('',#181388);
#38549=VERTEX_POINT('',#181389);
#38550=VERTEX_POINT('',#181391);
#38551=VERTEX_POINT('',#181393);
#38552=VERTEX_POINT('',#181395);
#38553=VERTEX_POINT('',#181397);
#38554=VERTEX_POINT('',#181401);
#38555=VERTEX_POINT('',#181403);
#38556=VERTEX_POINT('',#181419);
#38557=VERTEX_POINT('',#181420);
#38558=VERTEX_POINT('',#181422);
#38559=VERTEX_POINT('',#181424);
#38560=VERTEX_POINT('',#181426);
#38561=VERTEX_POINT('',#181428);
#38562=VERTEX_POINT('',#181432);
#38563=VERTEX_POINT('',#181434);
#38564=VERTEX_POINT('',#181438);
#38565=VERTEX_POINT('',#181439);
#38566=VERTEX_POINT('',#181441);
#38567=VERTEX_POINT('',#181443);
#38568=VERTEX_POINT('',#181447);
#38569=VERTEX_POINT('',#181448);
#38570=VERTEX_POINT('',#181450);
#38571=VERTEX_POINT('',#181452);
#38572=VERTEX_POINT('',#181454);
#38573=VERTEX_POINT('',#181456);
#38574=VERTEX_POINT('',#181460);
#38575=VERTEX_POINT('',#181462);
#38576=VERTEX_POINT('',#181478);
#38577=VERTEX_POINT('',#181479);
#38578=VERTEX_POINT('',#181481);
#38579=VERTEX_POINT('',#181483);
#38580=VERTEX_POINT('',#181485);
#38581=VERTEX_POINT('',#181487);
#38582=VERTEX_POINT('',#181491);
#38583=VERTEX_POINT('',#181493);
#38584=VERTEX_POINT('',#181497);
#38585=VERTEX_POINT('',#181498);
#38586=VERTEX_POINT('',#181500);
#38587=VERTEX_POINT('',#181502);
#38588=VERTEX_POINT('',#181506);
#38589=VERTEX_POINT('',#181507);
#38590=VERTEX_POINT('',#181509);
#38591=VERTEX_POINT('',#181511);
#38592=VERTEX_POINT('',#181513);
#38593=VERTEX_POINT('',#181515);
#38594=VERTEX_POINT('',#181519);
#38595=VERTEX_POINT('',#181521);
#38596=VERTEX_POINT('',#181537);
#38597=VERTEX_POINT('',#181538);
#38598=VERTEX_POINT('',#181540);
#38599=VERTEX_POINT('',#181542);
#38600=VERTEX_POINT('',#181544);
#38601=VERTEX_POINT('',#181546);
#38602=VERTEX_POINT('',#181550);
#38603=VERTEX_POINT('',#181552);
#38604=VERTEX_POINT('',#181556);
#38605=VERTEX_POINT('',#181557);
#38606=VERTEX_POINT('',#181559);
#38607=VERTEX_POINT('',#181561);
#38608=VERTEX_POINT('',#181565);
#38609=VERTEX_POINT('',#181566);
#38610=VERTEX_POINT('',#181568);
#38611=VERTEX_POINT('',#181570);
#38612=VERTEX_POINT('',#181572);
#38613=VERTEX_POINT('',#181574);
#38614=VERTEX_POINT('',#181578);
#38615=VERTEX_POINT('',#181580);
#38616=VERTEX_POINT('',#181596);
#38617=VERTEX_POINT('',#181597);
#38618=VERTEX_POINT('',#181599);
#38619=VERTEX_POINT('',#181601);
#38620=VERTEX_POINT('',#181603);
#38621=VERTEX_POINT('',#181605);
#38622=VERTEX_POINT('',#181609);
#38623=VERTEX_POINT('',#181611);
#38624=VERTEX_POINT('',#181615);
#38625=VERTEX_POINT('',#181616);
#38626=VERTEX_POINT('',#181618);
#38627=VERTEX_POINT('',#181620);
#38628=VERTEX_POINT('',#181624);
#38629=VERTEX_POINT('',#181625);
#38630=VERTEX_POINT('',#181627);
#38631=VERTEX_POINT('',#181629);
#38632=VERTEX_POINT('',#181631);
#38633=VERTEX_POINT('',#181633);
#38634=VERTEX_POINT('',#181637);
#38635=VERTEX_POINT('',#181639);
#38636=VERTEX_POINT('',#181655);
#38637=VERTEX_POINT('',#181656);
#38638=VERTEX_POINT('',#181658);
#38639=VERTEX_POINT('',#181660);
#38640=VERTEX_POINT('',#181662);
#38641=VERTEX_POINT('',#181664);
#38642=VERTEX_POINT('',#181668);
#38643=VERTEX_POINT('',#181670);
#38644=VERTEX_POINT('',#181674);
#38645=VERTEX_POINT('',#181675);
#38646=VERTEX_POINT('',#181677);
#38647=VERTEX_POINT('',#181679);
#38648=VERTEX_POINT('',#181683);
#38649=VERTEX_POINT('',#181684);
#38650=VERTEX_POINT('',#181686);
#38651=VERTEX_POINT('',#181688);
#38652=VERTEX_POINT('',#181690);
#38653=VERTEX_POINT('',#181692);
#38654=VERTEX_POINT('',#181696);
#38655=VERTEX_POINT('',#181698);
#38656=VERTEX_POINT('',#181714);
#38657=VERTEX_POINT('',#181715);
#38658=VERTEX_POINT('',#181717);
#38659=VERTEX_POINT('',#181719);
#38660=VERTEX_POINT('',#181721);
#38661=VERTEX_POINT('',#181723);
#38662=VERTEX_POINT('',#181727);
#38663=VERTEX_POINT('',#181729);
#38664=VERTEX_POINT('',#181733);
#38665=VERTEX_POINT('',#181734);
#38666=VERTEX_POINT('',#181736);
#38667=VERTEX_POINT('',#181738);
#38668=VERTEX_POINT('',#181742);
#38669=VERTEX_POINT('',#181743);
#38670=VERTEX_POINT('',#181745);
#38671=VERTEX_POINT('',#181747);
#38672=VERTEX_POINT('',#181749);
#38673=VERTEX_POINT('',#181751);
#38674=VERTEX_POINT('',#181755);
#38675=VERTEX_POINT('',#181757);
#38676=VERTEX_POINT('',#181773);
#38677=VERTEX_POINT('',#181774);
#38678=VERTEX_POINT('',#181776);
#38679=VERTEX_POINT('',#181778);
#38680=VERTEX_POINT('',#181780);
#38681=VERTEX_POINT('',#181782);
#38682=VERTEX_POINT('',#181786);
#38683=VERTEX_POINT('',#181788);
#38684=VERTEX_POINT('',#181792);
#38685=VERTEX_POINT('',#181793);
#38686=VERTEX_POINT('',#181795);
#38687=VERTEX_POINT('',#181797);
#38688=VERTEX_POINT('',#181801);
#38689=VERTEX_POINT('',#181802);
#38690=VERTEX_POINT('',#181804);
#38691=VERTEX_POINT('',#181806);
#38692=VERTEX_POINT('',#181808);
#38693=VERTEX_POINT('',#181810);
#38694=VERTEX_POINT('',#181814);
#38695=VERTEX_POINT('',#181816);
#38696=VERTEX_POINT('',#181832);
#38697=VERTEX_POINT('',#181833);
#38698=VERTEX_POINT('',#181835);
#38699=VERTEX_POINT('',#181837);
#38700=VERTEX_POINT('',#181839);
#38701=VERTEX_POINT('',#181841);
#38702=VERTEX_POINT('',#181845);
#38703=VERTEX_POINT('',#181847);
#38704=VERTEX_POINT('',#181851);
#38705=VERTEX_POINT('',#181852);
#38706=VERTEX_POINT('',#181854);
#38707=VERTEX_POINT('',#181856);
#38708=VERTEX_POINT('',#181860);
#38709=VERTEX_POINT('',#181861);
#38710=VERTEX_POINT('',#181863);
#38711=VERTEX_POINT('',#181865);
#38712=VERTEX_POINT('',#181867);
#38713=VERTEX_POINT('',#181869);
#38714=VERTEX_POINT('',#181873);
#38715=VERTEX_POINT('',#181875);
#38716=VERTEX_POINT('',#181891);
#38717=VERTEX_POINT('',#181892);
#38718=VERTEX_POINT('',#181894);
#38719=VERTEX_POINT('',#181896);
#38720=VERTEX_POINT('',#181898);
#38721=VERTEX_POINT('',#181900);
#38722=VERTEX_POINT('',#181904);
#38723=VERTEX_POINT('',#181906);
#38724=VERTEX_POINT('',#181910);
#38725=VERTEX_POINT('',#181911);
#38726=VERTEX_POINT('',#181913);
#38727=VERTEX_POINT('',#181915);
#38728=VERTEX_POINT('',#181919);
#38729=VERTEX_POINT('',#181920);
#38730=VERTEX_POINT('',#181922);
#38731=VERTEX_POINT('',#181924);
#38732=VERTEX_POINT('',#181926);
#38733=VERTEX_POINT('',#181928);
#38734=VERTEX_POINT('',#181932);
#38735=VERTEX_POINT('',#181934);
#38736=VERTEX_POINT('',#181951);
#38737=VERTEX_POINT('',#181952);
#38738=VERTEX_POINT('',#181954);
#38739=VERTEX_POINT('',#181956);
#38740=VERTEX_POINT('',#181958);
#38741=VERTEX_POINT('',#181960);
#38742=VERTEX_POINT('',#181964);
#38743=VERTEX_POINT('',#181966);
#38744=VERTEX_POINT('',#181970);
#38745=VERTEX_POINT('',#181971);
#38746=VERTEX_POINT('',#181973);
#38747=VERTEX_POINT('',#181975);
#38748=VERTEX_POINT('',#181979);
#38749=VERTEX_POINT('',#181980);
#38750=VERTEX_POINT('',#181982);
#38751=VERTEX_POINT('',#181984);
#38752=VERTEX_POINT('',#181986);
#38753=VERTEX_POINT('',#181988);
#38754=VERTEX_POINT('',#181992);
#38755=VERTEX_POINT('',#181994);
#38756=VERTEX_POINT('',#182012);
#38757=VERTEX_POINT('',#182013);
#38758=VERTEX_POINT('',#182015);
#38759=VERTEX_POINT('',#182017);
#38760=VERTEX_POINT('',#182021);
#38761=VERTEX_POINT('',#182022);
#38762=VERTEX_POINT('',#182024);
#38763=VERTEX_POINT('',#182026);
#38764=VERTEX_POINT('',#182028);
#38765=VERTEX_POINT('',#182030);
#38766=VERTEX_POINT('',#182032);
#38767=VERTEX_POINT('',#182034);
#38768=VERTEX_POINT('',#182036);
#38769=VERTEX_POINT('',#182038);
#38770=VERTEX_POINT('',#182040);
#38771=VERTEX_POINT('',#182042);
#38772=VERTEX_POINT('',#182046);
#38773=VERTEX_POINT('',#182047);
#38774=VERTEX_POINT('',#182049);
#38775=VERTEX_POINT('',#182051);
#38776=VERTEX_POINT('',#182053);
#38777=VERTEX_POINT('',#182055);
#38778=VERTEX_POINT('',#182057);
#38779=VERTEX_POINT('',#182059);
#38780=VERTEX_POINT('',#182061);
#38781=VERTEX_POINT('',#182063);
#38782=VERTEX_POINT('',#182065);
#38783=VERTEX_POINT('',#182067);
#38784=VERTEX_POINT('',#182487);
#38785=VERTEX_POINT('',#182488);
#38786=VERTEX_POINT('',#182490);
#38787=VERTEX_POINT('',#182492);
#38788=VERTEX_POINT('',#182496);
#38789=VERTEX_POINT('',#182497);
#38790=VERTEX_POINT('',#182499);
#38791=VERTEX_POINT('',#182501);
#38792=VERTEX_POINT('',#182503);
#38793=VERTEX_POINT('',#182505);
#38794=VERTEX_POINT('',#182507);
#38795=VERTEX_POINT('',#182509);
#38796=VERTEX_POINT('',#182511);
#38797=VERTEX_POINT('',#182513);
#38798=VERTEX_POINT('',#182515);
#38799=VERTEX_POINT('',#182517);
#38800=VERTEX_POINT('',#182521);
#38801=VERTEX_POINT('',#182522);
#38802=VERTEX_POINT('',#182524);
#38803=VERTEX_POINT('',#182526);
#38804=VERTEX_POINT('',#182528);
#38805=VERTEX_POINT('',#182530);
#38806=VERTEX_POINT('',#182532);
#38807=VERTEX_POINT('',#182534);
#38808=VERTEX_POINT('',#182536);
#38809=VERTEX_POINT('',#182538);
#38810=VERTEX_POINT('',#182540);
#38811=VERTEX_POINT('',#182542);
#38812=VERTEX_POINT('',#182546);
#38813=VERTEX_POINT('',#182547);
#38814=VERTEX_POINT('',#182549);
#38815=VERTEX_POINT('',#182551);
#38816=VERTEX_POINT('',#182555);
#38817=VERTEX_POINT('',#182556);
#38818=VERTEX_POINT('',#182558);
#38819=VERTEX_POINT('',#182560);
#38820=VERTEX_POINT('',#182562);
#38821=VERTEX_POINT('',#182564);
#38822=VERTEX_POINT('',#182566);
#38823=VERTEX_POINT('',#182568);
#38824=VERTEX_POINT('',#182570);
#38825=VERTEX_POINT('',#182572);
#38826=VERTEX_POINT('',#182574);
#38827=VERTEX_POINT('',#182576);
#38828=VERTEX_POINT('',#182580);
#38829=VERTEX_POINT('',#182581);
#38830=VERTEX_POINT('',#182583);
#38831=VERTEX_POINT('',#182585);
#38832=VERTEX_POINT('',#182587);
#38833=VERTEX_POINT('',#182589);
#38834=VERTEX_POINT('',#182591);
#38835=VERTEX_POINT('',#182593);
#38836=VERTEX_POINT('',#182595);
#38837=VERTEX_POINT('',#182597);
#38838=VERTEX_POINT('',#182599);
#38839=VERTEX_POINT('',#182601);
#38840=VERTEX_POINT('',#182605);
#38841=VERTEX_POINT('',#182606);
#38842=VERTEX_POINT('',#182608);
#38843=VERTEX_POINT('',#182610);
#38844=VERTEX_POINT('',#182614);
#38845=VERTEX_POINT('',#182615);
#38846=VERTEX_POINT('',#182617);
#38847=VERTEX_POINT('',#182619);
#38848=VERTEX_POINT('',#182621);
#38849=VERTEX_POINT('',#182623);
#38850=VERTEX_POINT('',#182625);
#38851=VERTEX_POINT('',#182627);
#38852=VERTEX_POINT('',#182629);
#38853=VERTEX_POINT('',#182631);
#38854=VERTEX_POINT('',#182633);
#38855=VERTEX_POINT('',#182635);
#38856=VERTEX_POINT('',#182639);
#38857=VERTEX_POINT('',#182640);
#38858=VERTEX_POINT('',#182642);
#38859=VERTEX_POINT('',#182644);
#38860=VERTEX_POINT('',#182646);
#38861=VERTEX_POINT('',#182648);
#38862=VERTEX_POINT('',#182650);
#38863=VERTEX_POINT('',#182652);
#38864=VERTEX_POINT('',#182654);
#38865=VERTEX_POINT('',#182656);
#38866=VERTEX_POINT('',#182658);
#38867=VERTEX_POINT('',#182660);
#38868=VERTEX_POINT('',#182664);
#38869=VERTEX_POINT('',#182665);
#38870=VERTEX_POINT('',#182667);
#38871=VERTEX_POINT('',#182669);
#38872=VERTEX_POINT('',#182673);
#38873=VERTEX_POINT('',#182674);
#38874=VERTEX_POINT('',#182676);
#38875=VERTEX_POINT('',#182678);
#38876=VERTEX_POINT('',#182680);
#38877=VERTEX_POINT('',#182682);
#38878=VERTEX_POINT('',#182684);
#38879=VERTEX_POINT('',#182686);
#38880=VERTEX_POINT('',#182688);
#38881=VERTEX_POINT('',#182690);
#38882=VERTEX_POINT('',#182692);
#38883=VERTEX_POINT('',#182694);
#38884=VERTEX_POINT('',#182698);
#38885=VERTEX_POINT('',#182699);
#38886=VERTEX_POINT('',#182701);
#38887=VERTEX_POINT('',#182703);
#38888=VERTEX_POINT('',#182705);
#38889=VERTEX_POINT('',#182707);
#38890=VERTEX_POINT('',#182709);
#38891=VERTEX_POINT('',#182711);
#38892=VERTEX_POINT('',#182713);
#38893=VERTEX_POINT('',#182715);
#38894=VERTEX_POINT('',#182717);
#38895=VERTEX_POINT('',#182719);
#38896=VERTEX_POINT('',#182723);
#38897=VERTEX_POINT('',#182724);
#38898=VERTEX_POINT('',#182726);
#38899=VERTEX_POINT('',#182728);
#38900=VERTEX_POINT('',#182732);
#38901=VERTEX_POINT('',#182733);
#38902=VERTEX_POINT('',#182735);
#38903=VERTEX_POINT('',#182737);
#38904=VERTEX_POINT('',#182739);
#38905=VERTEX_POINT('',#182741);
#38906=VERTEX_POINT('',#182743);
#38907=VERTEX_POINT('',#182745);
#38908=VERTEX_POINT('',#182747);
#38909=VERTEX_POINT('',#182749);
#38910=VERTEX_POINT('',#182751);
#38911=VERTEX_POINT('',#182753);
#38912=VERTEX_POINT('',#182757);
#38913=VERTEX_POINT('',#182758);
#38914=VERTEX_POINT('',#182760);
#38915=VERTEX_POINT('',#182762);
#38916=VERTEX_POINT('',#182764);
#38917=VERTEX_POINT('',#182766);
#38918=VERTEX_POINT('',#182768);
#38919=VERTEX_POINT('',#182770);
#38920=VERTEX_POINT('',#182772);
#38921=VERTEX_POINT('',#182774);
#38922=VERTEX_POINT('',#182776);
#38923=VERTEX_POINT('',#182778);
#38924=VERTEX_POINT('',#182782);
#38925=VERTEX_POINT('',#182783);
#38926=VERTEX_POINT('',#182785);
#38927=VERTEX_POINT('',#182787);
#38928=VERTEX_POINT('',#182791);
#38929=VERTEX_POINT('',#182792);
#38930=VERTEX_POINT('',#182794);
#38931=VERTEX_POINT('',#182796);
#38932=VERTEX_POINT('',#182798);
#38933=VERTEX_POINT('',#182800);
#38934=VERTEX_POINT('',#182802);
#38935=VERTEX_POINT('',#182804);
#38936=VERTEX_POINT('',#182806);
#38937=VERTEX_POINT('',#182808);
#38938=VERTEX_POINT('',#182810);
#38939=VERTEX_POINT('',#182812);
#38940=VERTEX_POINT('',#182816);
#38941=VERTEX_POINT('',#182817);
#38942=VERTEX_POINT('',#182819);
#38943=VERTEX_POINT('',#182821);
#38944=VERTEX_POINT('',#182823);
#38945=VERTEX_POINT('',#182825);
#38946=VERTEX_POINT('',#182827);
#38947=VERTEX_POINT('',#182829);
#38948=VERTEX_POINT('',#182831);
#38949=VERTEX_POINT('',#182833);
#38950=VERTEX_POINT('',#182835);
#38951=VERTEX_POINT('',#182837);
#38952=VERTEX_POINT('',#182841);
#38953=VERTEX_POINT('',#182842);
#38954=VERTEX_POINT('',#182844);
#38955=VERTEX_POINT('',#182846);
#38956=VERTEX_POINT('',#182850);
#38957=VERTEX_POINT('',#182851);
#38958=VERTEX_POINT('',#182853);
#38959=VERTEX_POINT('',#182855);
#38960=VERTEX_POINT('',#182857);
#38961=VERTEX_POINT('',#182859);
#38962=VERTEX_POINT('',#182861);
#38963=VERTEX_POINT('',#182863);
#38964=VERTEX_POINT('',#182865);
#38965=VERTEX_POINT('',#182867);
#38966=VERTEX_POINT('',#182869);
#38967=VERTEX_POINT('',#182871);
#38968=VERTEX_POINT('',#182875);
#38969=VERTEX_POINT('',#182876);
#38970=VERTEX_POINT('',#182878);
#38971=VERTEX_POINT('',#182880);
#38972=VERTEX_POINT('',#182882);
#38973=VERTEX_POINT('',#182884);
#38974=VERTEX_POINT('',#182886);
#38975=VERTEX_POINT('',#182888);
#38976=VERTEX_POINT('',#182890);
#38977=VERTEX_POINT('',#182892);
#38978=VERTEX_POINT('',#182894);
#38979=VERTEX_POINT('',#182896);
#38980=VERTEX_POINT('',#182900);
#38981=VERTEX_POINT('',#182901);
#38982=VERTEX_POINT('',#182903);
#38983=VERTEX_POINT('',#182905);
#38984=VERTEX_POINT('',#182909);
#38985=VERTEX_POINT('',#182910);
#38986=VERTEX_POINT('',#182912);
#38987=VERTEX_POINT('',#182914);
#38988=VERTEX_POINT('',#182916);
#38989=VERTEX_POINT('',#182918);
#38990=VERTEX_POINT('',#182920);
#38991=VERTEX_POINT('',#182922);
#38992=VERTEX_POINT('',#182924);
#38993=VERTEX_POINT('',#182926);
#38994=VERTEX_POINT('',#182928);
#38995=VERTEX_POINT('',#182930);
#38996=VERTEX_POINT('',#182934);
#38997=VERTEX_POINT('',#182935);
#38998=VERTEX_POINT('',#182937);
#38999=VERTEX_POINT('',#182939);
#39000=VERTEX_POINT('',#182941);
#39001=VERTEX_POINT('',#182943);
#39002=VERTEX_POINT('',#182945);
#39003=VERTEX_POINT('',#182947);
#39004=VERTEX_POINT('',#182949);
#39005=VERTEX_POINT('',#182951);
#39006=VERTEX_POINT('',#182953);
#39007=VERTEX_POINT('',#182955);
#39008=VERTEX_POINT('',#182959);
#39009=VERTEX_POINT('',#182960);
#39010=VERTEX_POINT('',#182962);
#39011=VERTEX_POINT('',#182964);
#39012=VERTEX_POINT('',#182968);
#39013=VERTEX_POINT('',#182969);
#39014=VERTEX_POINT('',#182971);
#39015=VERTEX_POINT('',#182973);
#39016=VERTEX_POINT('',#182975);
#39017=VERTEX_POINT('',#182977);
#39018=VERTEX_POINT('',#182979);
#39019=VERTEX_POINT('',#182981);
#39020=VERTEX_POINT('',#182983);
#39021=VERTEX_POINT('',#182985);
#39022=VERTEX_POINT('',#182987);
#39023=VERTEX_POINT('',#182989);
#39024=VERTEX_POINT('',#182993);
#39025=VERTEX_POINT('',#182994);
#39026=VERTEX_POINT('',#182996);
#39027=VERTEX_POINT('',#182998);
#39028=VERTEX_POINT('',#183000);
#39029=VERTEX_POINT('',#183002);
#39030=VERTEX_POINT('',#183004);
#39031=VERTEX_POINT('',#183006);
#39032=VERTEX_POINT('',#183008);
#39033=VERTEX_POINT('',#183010);
#39034=VERTEX_POINT('',#183012);
#39035=VERTEX_POINT('',#183014);
#39036=VERTEX_POINT('',#183018);
#39037=VERTEX_POINT('',#183019);
#39038=VERTEX_POINT('',#183021);
#39039=VERTEX_POINT('',#183023);
#39040=VERTEX_POINT('',#183027);
#39041=VERTEX_POINT('',#183028);
#39042=VERTEX_POINT('',#183030);
#39043=VERTEX_POINT('',#183032);
#39044=VERTEX_POINT('',#183034);
#39045=VERTEX_POINT('',#183036);
#39046=VERTEX_POINT('',#183038);
#39047=VERTEX_POINT('',#183040);
#39048=VERTEX_POINT('',#183042);
#39049=VERTEX_POINT('',#183044);
#39050=VERTEX_POINT('',#183046);
#39051=VERTEX_POINT('',#183048);
#39052=VERTEX_POINT('',#183052);
#39053=VERTEX_POINT('',#183053);
#39054=VERTEX_POINT('',#183055);
#39055=VERTEX_POINT('',#183057);
#39056=VERTEX_POINT('',#183059);
#39057=VERTEX_POINT('',#183061);
#39058=VERTEX_POINT('',#183063);
#39059=VERTEX_POINT('',#183065);
#39060=VERTEX_POINT('',#183067);
#39061=VERTEX_POINT('',#183069);
#39062=VERTEX_POINT('',#183071);
#39063=VERTEX_POINT('',#183073);
#39064=VERTEX_POINT('',#183077);
#39065=VERTEX_POINT('',#183078);
#39066=VERTEX_POINT('',#183080);
#39067=VERTEX_POINT('',#183082);
#39068=VERTEX_POINT('',#183086);
#39069=VERTEX_POINT('',#183087);
#39070=VERTEX_POINT('',#183089);
#39071=VERTEX_POINT('',#183091);
#39072=VERTEX_POINT('',#183093);
#39073=VERTEX_POINT('',#183095);
#39074=VERTEX_POINT('',#183097);
#39075=VERTEX_POINT('',#183099);
#39076=VERTEX_POINT('',#183101);
#39077=VERTEX_POINT('',#183103);
#39078=VERTEX_POINT('',#183105);
#39079=VERTEX_POINT('',#183107);
#39080=VERTEX_POINT('',#183111);
#39081=VERTEX_POINT('',#183112);
#39082=VERTEX_POINT('',#183114);
#39083=VERTEX_POINT('',#183116);
#39084=VERTEX_POINT('',#183118);
#39085=VERTEX_POINT('',#183120);
#39086=VERTEX_POINT('',#183122);
#39087=VERTEX_POINT('',#183124);
#39088=VERTEX_POINT('',#183126);
#39089=VERTEX_POINT('',#183128);
#39090=VERTEX_POINT('',#183130);
#39091=VERTEX_POINT('',#183132);
#39092=VERTEX_POINT('',#183136);
#39093=VERTEX_POINT('',#183137);
#39094=VERTEX_POINT('',#183139);
#39095=VERTEX_POINT('',#183141);
#39096=VERTEX_POINT('',#183145);
#39097=VERTEX_POINT('',#183146);
#39098=VERTEX_POINT('',#183148);
#39099=VERTEX_POINT('',#183150);
#39100=VERTEX_POINT('',#183152);
#39101=VERTEX_POINT('',#183154);
#39102=VERTEX_POINT('',#183156);
#39103=VERTEX_POINT('',#183158);
#39104=VERTEX_POINT('',#183160);
#39105=VERTEX_POINT('',#183162);
#39106=VERTEX_POINT('',#183164);
#39107=VERTEX_POINT('',#183166);
#39108=VERTEX_POINT('',#183170);
#39109=VERTEX_POINT('',#183171);
#39110=VERTEX_POINT('',#183173);
#39111=VERTEX_POINT('',#183175);
#39112=VERTEX_POINT('',#183177);
#39113=VERTEX_POINT('',#183179);
#39114=VERTEX_POINT('',#183181);
#39115=VERTEX_POINT('',#183183);
#39116=VERTEX_POINT('',#183185);
#39117=VERTEX_POINT('',#183187);
#39118=VERTEX_POINT('',#183189);
#39119=VERTEX_POINT('',#183191);
#39120=VERTEX_POINT('',#183195);
#39121=VERTEX_POINT('',#183196);
#39122=VERTEX_POINT('',#183198);
#39123=VERTEX_POINT('',#183200);
#39124=VERTEX_POINT('',#183204);
#39125=VERTEX_POINT('',#183205);
#39126=VERTEX_POINT('',#183207);
#39127=VERTEX_POINT('',#183209);
#39128=VERTEX_POINT('',#183211);
#39129=VERTEX_POINT('',#183213);
#39130=VERTEX_POINT('',#183215);
#39131=VERTEX_POINT('',#183217);
#39132=VERTEX_POINT('',#183219);
#39133=VERTEX_POINT('',#183221);
#39134=VERTEX_POINT('',#183223);
#39135=VERTEX_POINT('',#183225);
#39136=VERTEX_POINT('',#183229);
#39137=VERTEX_POINT('',#183230);
#39138=VERTEX_POINT('',#183232);
#39139=VERTEX_POINT('',#183234);
#39140=VERTEX_POINT('',#183236);
#39141=VERTEX_POINT('',#183238);
#39142=VERTEX_POINT('',#183240);
#39143=VERTEX_POINT('',#183242);
#39144=VERTEX_POINT('',#183244);
#39145=VERTEX_POINT('',#183246);
#39146=VERTEX_POINT('',#183248);
#39147=VERTEX_POINT('',#183250);
#39148=VERTEX_POINT('',#183254);
#39149=VERTEX_POINT('',#183255);
#39150=VERTEX_POINT('',#183257);
#39151=VERTEX_POINT('',#183259);
#39152=VERTEX_POINT('',#183263);
#39153=VERTEX_POINT('',#183264);
#39154=VERTEX_POINT('',#183266);
#39155=VERTEX_POINT('',#183268);
#39156=VERTEX_POINT('',#183270);
#39157=VERTEX_POINT('',#183272);
#39158=VERTEX_POINT('',#183274);
#39159=VERTEX_POINT('',#183276);
#39160=VERTEX_POINT('',#183278);
#39161=VERTEX_POINT('',#183280);
#39162=VERTEX_POINT('',#183282);
#39163=VERTEX_POINT('',#183284);
#39164=VERTEX_POINT('',#183288);
#39165=VERTEX_POINT('',#183289);
#39166=VERTEX_POINT('',#183291);
#39167=VERTEX_POINT('',#183293);
#39168=VERTEX_POINT('',#183295);
#39169=VERTEX_POINT('',#183297);
#39170=VERTEX_POINT('',#183299);
#39171=VERTEX_POINT('',#183301);
#39172=VERTEX_POINT('',#183303);
#39173=VERTEX_POINT('',#183305);
#39174=VERTEX_POINT('',#183307);
#39175=VERTEX_POINT('',#183309);
#39176=VERTEX_POINT('',#183313);
#39177=VERTEX_POINT('',#183314);
#39178=VERTEX_POINT('',#183316);
#39179=VERTEX_POINT('',#183318);
#39180=VERTEX_POINT('',#183322);
#39181=VERTEX_POINT('',#183323);
#39182=VERTEX_POINT('',#183325);
#39183=VERTEX_POINT('',#183327);
#39184=VERTEX_POINT('',#183329);
#39185=VERTEX_POINT('',#183331);
#39186=VERTEX_POINT('',#183333);
#39187=VERTEX_POINT('',#183335);
#39188=VERTEX_POINT('',#183337);
#39189=VERTEX_POINT('',#183339);
#39190=VERTEX_POINT('',#183341);
#39191=VERTEX_POINT('',#183343);
#39192=VERTEX_POINT('',#183347);
#39193=VERTEX_POINT('',#183348);
#39194=VERTEX_POINT('',#183350);
#39195=VERTEX_POINT('',#183352);
#39196=VERTEX_POINT('',#183354);
#39197=VERTEX_POINT('',#183356);
#39198=VERTEX_POINT('',#183358);
#39199=VERTEX_POINT('',#183360);
#39200=VERTEX_POINT('',#183362);
#39201=VERTEX_POINT('',#183364);
#39202=VERTEX_POINT('',#183366);
#39203=VERTEX_POINT('',#183368);
#39204=VERTEX_POINT('',#183372);
#39205=VERTEX_POINT('',#183373);
#39206=VERTEX_POINT('',#183375);
#39207=VERTEX_POINT('',#183377);
#39208=VERTEX_POINT('',#183381);
#39209=VERTEX_POINT('',#183382);
#39210=VERTEX_POINT('',#183384);
#39211=VERTEX_POINT('',#183386);
#39212=VERTEX_POINT('',#183388);
#39213=VERTEX_POINT('',#183390);
#39214=VERTEX_POINT('',#183392);
#39215=VERTEX_POINT('',#183394);
#39216=VERTEX_POINT('',#183396);
#39217=VERTEX_POINT('',#183398);
#39218=VERTEX_POINT('',#183400);
#39219=VERTEX_POINT('',#183402);
#39220=VERTEX_POINT('',#183406);
#39221=VERTEX_POINT('',#183407);
#39222=VERTEX_POINT('',#183409);
#39223=VERTEX_POINT('',#183411);
#39224=VERTEX_POINT('',#183413);
#39225=VERTEX_POINT('',#183415);
#39226=VERTEX_POINT('',#183417);
#39227=VERTEX_POINT('',#183419);
#39228=VERTEX_POINT('',#183421);
#39229=VERTEX_POINT('',#183423);
#39230=VERTEX_POINT('',#183425);
#39231=VERTEX_POINT('',#183427);
#39232=VERTEX_POINT('',#183431);
#39233=VERTEX_POINT('',#183432);
#39234=VERTEX_POINT('',#183434);
#39235=VERTEX_POINT('',#183436);
#39236=VERTEX_POINT('',#183440);
#39237=VERTEX_POINT('',#183441);
#39238=VERTEX_POINT('',#183443);
#39239=VERTEX_POINT('',#183445);
#39240=VERTEX_POINT('',#183447);
#39241=VERTEX_POINT('',#183449);
#39242=VERTEX_POINT('',#183451);
#39243=VERTEX_POINT('',#183453);
#39244=VERTEX_POINT('',#183455);
#39245=VERTEX_POINT('',#183457);
#39246=VERTEX_POINT('',#183459);
#39247=VERTEX_POINT('',#183461);
#39248=VERTEX_POINT('',#183465);
#39249=VERTEX_POINT('',#183466);
#39250=VERTEX_POINT('',#183468);
#39251=VERTEX_POINT('',#183470);
#39252=VERTEX_POINT('',#183472);
#39253=VERTEX_POINT('',#183474);
#39254=VERTEX_POINT('',#183476);
#39255=VERTEX_POINT('',#183478);
#39256=VERTEX_POINT('',#183480);
#39257=VERTEX_POINT('',#183482);
#39258=VERTEX_POINT('',#183484);
#39259=VERTEX_POINT('',#183486);
#39260=VERTEX_POINT('',#183490);
#39261=VERTEX_POINT('',#183491);
#39262=VERTEX_POINT('',#183493);
#39263=VERTEX_POINT('',#183495);
#39264=VERTEX_POINT('',#183499);
#39265=VERTEX_POINT('',#183500);
#39266=VERTEX_POINT('',#183502);
#39267=VERTEX_POINT('',#183504);
#39268=VERTEX_POINT('',#183506);
#39269=VERTEX_POINT('',#183508);
#39270=VERTEX_POINT('',#183510);
#39271=VERTEX_POINT('',#183512);
#39272=VERTEX_POINT('',#183514);
#39273=VERTEX_POINT('',#183516);
#39274=VERTEX_POINT('',#183518);
#39275=VERTEX_POINT('',#183520);
#39276=VERTEX_POINT('',#183524);
#39277=VERTEX_POINT('',#183525);
#39278=VERTEX_POINT('',#183527);
#39279=VERTEX_POINT('',#183529);
#39280=VERTEX_POINT('',#183531);
#39281=VERTEX_POINT('',#183533);
#39282=VERTEX_POINT('',#183535);
#39283=VERTEX_POINT('',#183537);
#39284=VERTEX_POINT('',#183539);
#39285=VERTEX_POINT('',#183541);
#39286=VERTEX_POINT('',#183543);
#39287=VERTEX_POINT('',#183545);
#39288=VERTEX_POINT('',#183549);
#39289=VERTEX_POINT('',#183550);
#39290=VERTEX_POINT('',#183552);
#39291=VERTEX_POINT('',#183554);
#39292=VERTEX_POINT('',#183558);
#39293=VERTEX_POINT('',#183559);
#39294=VERTEX_POINT('',#183561);
#39295=VERTEX_POINT('',#183563);
#39296=VERTEX_POINT('',#183565);
#39297=VERTEX_POINT('',#183567);
#39298=VERTEX_POINT('',#183569);
#39299=VERTEX_POINT('',#183571);
#39300=VERTEX_POINT('',#183573);
#39301=VERTEX_POINT('',#183575);
#39302=VERTEX_POINT('',#183577);
#39303=VERTEX_POINT('',#183579);
#39304=VERTEX_POINT('',#183583);
#39305=VERTEX_POINT('',#183584);
#39306=VERTEX_POINT('',#183586);
#39307=VERTEX_POINT('',#183588);
#39308=VERTEX_POINT('',#183590);
#39309=VERTEX_POINT('',#183592);
#39310=VERTEX_POINT('',#183594);
#39311=VERTEX_POINT('',#183596);
#39312=VERTEX_POINT('',#183598);
#39313=VERTEX_POINT('',#183600);
#39314=VERTEX_POINT('',#183602);
#39315=VERTEX_POINT('',#183604);
#39316=VERTEX_POINT('',#183608);
#39317=VERTEX_POINT('',#183609);
#39318=VERTEX_POINT('',#183611);
#39319=VERTEX_POINT('',#183613);
#39320=VERTEX_POINT('',#183617);
#39321=VERTEX_POINT('',#183618);
#39322=VERTEX_POINT('',#183620);
#39323=VERTEX_POINT('',#183622);
#39324=VERTEX_POINT('',#183624);
#39325=VERTEX_POINT('',#183626);
#39326=VERTEX_POINT('',#183628);
#39327=VERTEX_POINT('',#183630);
#39328=VERTEX_POINT('',#183632);
#39329=VERTEX_POINT('',#183634);
#39330=VERTEX_POINT('',#183636);
#39331=VERTEX_POINT('',#183638);
#39332=VERTEX_POINT('',#183642);
#39333=VERTEX_POINT('',#183643);
#39334=VERTEX_POINT('',#183645);
#39335=VERTEX_POINT('',#183647);
#39336=VERTEX_POINT('',#183649);
#39337=VERTEX_POINT('',#183651);
#39338=VERTEX_POINT('',#183653);
#39339=VERTEX_POINT('',#183655);
#39340=VERTEX_POINT('',#183657);
#39341=VERTEX_POINT('',#183659);
#39342=VERTEX_POINT('',#183661);
#39343=VERTEX_POINT('',#183663);
#39344=VERTEX_POINT('',#183667);
#39345=VERTEX_POINT('',#183668);
#39346=VERTEX_POINT('',#183670);
#39347=VERTEX_POINT('',#183672);
#39348=VERTEX_POINT('',#183676);
#39349=VERTEX_POINT('',#183677);
#39350=VERTEX_POINT('',#183679);
#39351=VERTEX_POINT('',#183681);
#39352=VERTEX_POINT('',#183683);
#39353=VERTEX_POINT('',#183685);
#39354=VERTEX_POINT('',#183687);
#39355=VERTEX_POINT('',#183689);
#39356=VERTEX_POINT('',#183691);
#39357=VERTEX_POINT('',#183693);
#39358=VERTEX_POINT('',#183695);
#39359=VERTEX_POINT('',#183697);
#39360=VERTEX_POINT('',#183701);
#39361=VERTEX_POINT('',#183702);
#39362=VERTEX_POINT('',#183704);
#39363=VERTEX_POINT('',#183706);
#39364=VERTEX_POINT('',#183708);
#39365=VERTEX_POINT('',#183710);
#39366=VERTEX_POINT('',#183712);
#39367=VERTEX_POINT('',#183714);
#39368=VERTEX_POINT('',#183716);
#39369=VERTEX_POINT('',#183718);
#39370=VERTEX_POINT('',#183720);
#39371=VERTEX_POINT('',#183722);
#39372=VERTEX_POINT('',#183726);
#39373=VERTEX_POINT('',#183727);
#39374=VERTEX_POINT('',#183729);
#39375=VERTEX_POINT('',#183731);
#39376=VERTEX_POINT('',#183735);
#39377=VERTEX_POINT('',#183736);
#39378=VERTEX_POINT('',#183738);
#39379=VERTEX_POINT('',#183740);
#39380=VERTEX_POINT('',#183742);
#39381=VERTEX_POINT('',#183744);
#39382=VERTEX_POINT('',#183746);
#39383=VERTEX_POINT('',#183748);
#39384=VERTEX_POINT('',#183750);
#39385=VERTEX_POINT('',#183752);
#39386=VERTEX_POINT('',#183754);
#39387=VERTEX_POINT('',#183756);
#39388=VERTEX_POINT('',#183760);
#39389=VERTEX_POINT('',#183761);
#39390=VERTEX_POINT('',#183763);
#39391=VERTEX_POINT('',#183765);
#39392=VERTEX_POINT('',#183767);
#39393=VERTEX_POINT('',#183769);
#39394=VERTEX_POINT('',#183771);
#39395=VERTEX_POINT('',#183773);
#39396=VERTEX_POINT('',#183775);
#39397=VERTEX_POINT('',#183777);
#39398=VERTEX_POINT('',#183779);
#39399=VERTEX_POINT('',#183781);
#39400=VERTEX_POINT('',#183785);
#39401=VERTEX_POINT('',#183786);
#39402=VERTEX_POINT('',#183788);
#39403=VERTEX_POINT('',#183790);
#39404=VERTEX_POINT('',#183794);
#39405=VERTEX_POINT('',#183795);
#39406=VERTEX_POINT('',#183797);
#39407=VERTEX_POINT('',#183799);
#39408=VERTEX_POINT('',#183801);
#39409=VERTEX_POINT('',#183803);
#39410=VERTEX_POINT('',#183805);
#39411=VERTEX_POINT('',#183807);
#39412=VERTEX_POINT('',#183809);
#39413=VERTEX_POINT('',#183811);
#39414=VERTEX_POINT('',#183813);
#39415=VERTEX_POINT('',#183815);
#39416=VERTEX_POINT('',#183819);
#39417=VERTEX_POINT('',#183820);
#39418=VERTEX_POINT('',#183822);
#39419=VERTEX_POINT('',#183824);
#39420=VERTEX_POINT('',#183826);
#39421=VERTEX_POINT('',#183828);
#39422=VERTEX_POINT('',#183830);
#39423=VERTEX_POINT('',#183832);
#39424=VERTEX_POINT('',#183834);
#39425=VERTEX_POINT('',#183836);
#39426=VERTEX_POINT('',#183838);
#39427=VERTEX_POINT('',#183840);
#39428=VERTEX_POINT('',#183844);
#39429=VERTEX_POINT('',#183845);
#39430=VERTEX_POINT('',#183847);
#39431=VERTEX_POINT('',#183849);
#39432=VERTEX_POINT('',#183853);
#39433=VERTEX_POINT('',#183854);
#39434=VERTEX_POINT('',#183856);
#39435=VERTEX_POINT('',#183858);
#39436=VERTEX_POINT('',#183860);
#39437=VERTEX_POINT('',#183862);
#39438=VERTEX_POINT('',#183864);
#39439=VERTEX_POINT('',#183866);
#39440=VERTEX_POINT('',#183868);
#39441=VERTEX_POINT('',#183870);
#39442=VERTEX_POINT('',#183872);
#39443=VERTEX_POINT('',#183874);
#39444=VERTEX_POINT('',#183878);
#39445=VERTEX_POINT('',#183879);
#39446=VERTEX_POINT('',#183881);
#39447=VERTEX_POINT('',#183883);
#39448=VERTEX_POINT('',#183885);
#39449=VERTEX_POINT('',#183887);
#39450=VERTEX_POINT('',#183889);
#39451=VERTEX_POINT('',#183891);
#39452=VERTEX_POINT('',#183893);
#39453=VERTEX_POINT('',#183895);
#39454=VERTEX_POINT('',#183897);
#39455=VERTEX_POINT('',#183899);
#39456=VERTEX_POINT('',#183903);
#39457=VERTEX_POINT('',#183904);
#39458=VERTEX_POINT('',#183906);
#39459=VERTEX_POINT('',#183908);
#39460=VERTEX_POINT('',#183912);
#39461=VERTEX_POINT('',#183913);
#39462=VERTEX_POINT('',#183915);
#39463=VERTEX_POINT('',#183917);
#39464=VERTEX_POINT('',#183919);
#39465=VERTEX_POINT('',#183921);
#39466=VERTEX_POINT('',#183923);
#39467=VERTEX_POINT('',#183925);
#39468=VERTEX_POINT('',#183927);
#39469=VERTEX_POINT('',#183929);
#39470=VERTEX_POINT('',#183931);
#39471=VERTEX_POINT('',#183933);
#39472=VERTEX_POINT('',#183937);
#39473=VERTEX_POINT('',#183938);
#39474=VERTEX_POINT('',#183940);
#39475=VERTEX_POINT('',#183942);
#39476=VERTEX_POINT('',#183944);
#39477=VERTEX_POINT('',#183946);
#39478=VERTEX_POINT('',#183948);
#39479=VERTEX_POINT('',#183950);
#39480=VERTEX_POINT('',#183952);
#39481=VERTEX_POINT('',#183954);
#39482=VERTEX_POINT('',#183956);
#39483=VERTEX_POINT('',#183958);
#39484=VERTEX_POINT('',#183962);
#39485=VERTEX_POINT('',#183963);
#39486=VERTEX_POINT('',#183965);
#39487=VERTEX_POINT('',#183967);
#39488=VERTEX_POINT('',#183971);
#39489=VERTEX_POINT('',#183972);
#39490=VERTEX_POINT('',#183974);
#39491=VERTEX_POINT('',#183976);
#39492=VERTEX_POINT('',#183978);
#39493=VERTEX_POINT('',#183980);
#39494=VERTEX_POINT('',#183982);
#39495=VERTEX_POINT('',#183984);
#39496=VERTEX_POINT('',#183986);
#39497=VERTEX_POINT('',#183988);
#39498=VERTEX_POINT('',#183990);
#39499=VERTEX_POINT('',#183992);
#39500=VERTEX_POINT('',#183996);
#39501=VERTEX_POINT('',#183997);
#39502=VERTEX_POINT('',#183999);
#39503=VERTEX_POINT('',#184001);
#39504=VERTEX_POINT('',#184003);
#39505=VERTEX_POINT('',#184005);
#39506=VERTEX_POINT('',#184007);
#39507=VERTEX_POINT('',#184009);
#39508=VERTEX_POINT('',#184011);
#39509=VERTEX_POINT('',#184013);
#39510=VERTEX_POINT('',#184015);
#39511=VERTEX_POINT('',#184017);
#39512=VERTEX_POINT('',#184021);
#39513=VERTEX_POINT('',#184022);
#39514=VERTEX_POINT('',#184024);
#39515=VERTEX_POINT('',#184026);
#39516=VERTEX_POINT('',#184030);
#39517=VERTEX_POINT('',#184031);
#39518=VERTEX_POINT('',#184033);
#39519=VERTEX_POINT('',#184035);
#39520=VERTEX_POINT('',#184037);
#39521=VERTEX_POINT('',#184039);
#39522=VERTEX_POINT('',#184041);
#39523=VERTEX_POINT('',#184043);
#39524=VERTEX_POINT('',#184045);
#39525=VERTEX_POINT('',#184047);
#39526=VERTEX_POINT('',#184049);
#39527=VERTEX_POINT('',#184051);
#39528=VERTEX_POINT('',#184055);
#39529=VERTEX_POINT('',#184056);
#39530=VERTEX_POINT('',#184058);
#39531=VERTEX_POINT('',#184060);
#39532=VERTEX_POINT('',#184062);
#39533=VERTEX_POINT('',#184064);
#39534=VERTEX_POINT('',#184066);
#39535=VERTEX_POINT('',#184068);
#39536=VERTEX_POINT('',#184070);
#39537=VERTEX_POINT('',#184072);
#39538=VERTEX_POINT('',#184074);
#39539=VERTEX_POINT('',#184076);
#39540=VERTEX_POINT('',#184080);
#39541=VERTEX_POINT('',#184081);
#39542=VERTEX_POINT('',#184083);
#39543=VERTEX_POINT('',#184085);
#39544=VERTEX_POINT('',#184089);
#39545=VERTEX_POINT('',#184090);
#39546=VERTEX_POINT('',#184092);
#39547=VERTEX_POINT('',#184094);
#39548=VERTEX_POINT('',#184096);
#39549=VERTEX_POINT('',#184098);
#39550=VERTEX_POINT('',#184100);
#39551=VERTEX_POINT('',#184102);
#39552=VERTEX_POINT('',#184104);
#39553=VERTEX_POINT('',#184106);
#39554=VERTEX_POINT('',#184108);
#39555=VERTEX_POINT('',#184110);
#39556=VERTEX_POINT('',#184114);
#39557=VERTEX_POINT('',#184115);
#39558=VERTEX_POINT('',#184117);
#39559=VERTEX_POINT('',#184119);
#39560=VERTEX_POINT('',#184121);
#39561=VERTEX_POINT('',#184123);
#39562=VERTEX_POINT('',#184125);
#39563=VERTEX_POINT('',#184127);
#39564=VERTEX_POINT('',#184129);
#39565=VERTEX_POINT('',#184131);
#39566=VERTEX_POINT('',#184133);
#39567=VERTEX_POINT('',#184135);
#39568=VERTEX_POINT('',#184139);
#39569=VERTEX_POINT('',#184140);
#39570=VERTEX_POINT('',#184142);
#39571=VERTEX_POINT('',#184144);
#39572=VERTEX_POINT('',#184148);
#39573=VERTEX_POINT('',#184149);
#39574=VERTEX_POINT('',#184151);
#39575=VERTEX_POINT('',#184153);
#39576=VERTEX_POINT('',#184155);
#39577=VERTEX_POINT('',#184157);
#39578=VERTEX_POINT('',#184159);
#39579=VERTEX_POINT('',#184161);
#39580=VERTEX_POINT('',#184163);
#39581=VERTEX_POINT('',#184165);
#39582=VERTEX_POINT('',#184167);
#39583=VERTEX_POINT('',#184169);
#39584=VERTEX_POINT('',#184173);
#39585=VERTEX_POINT('',#184174);
#39586=VERTEX_POINT('',#184176);
#39587=VERTEX_POINT('',#184178);
#39588=VERTEX_POINT('',#184180);
#39589=VERTEX_POINT('',#184182);
#39590=VERTEX_POINT('',#184184);
#39591=VERTEX_POINT('',#184186);
#39592=VERTEX_POINT('',#184188);
#39593=VERTEX_POINT('',#184190);
#39594=VERTEX_POINT('',#184192);
#39595=VERTEX_POINT('',#184194);
#39596=VERTEX_POINT('',#184201);
#39597=VERTEX_POINT('',#184202);
#39598=VERTEX_POINT('',#184204);
#39599=VERTEX_POINT('',#184206);
#39600=VERTEX_POINT('',#184208);
#39601=VERTEX_POINT('',#184210);
#39602=VERTEX_POINT('',#184212);
#39603=VERTEX_POINT('',#184214);
#39604=VERTEX_POINT('',#184216);
#39605=VERTEX_POINT('',#184218);
#39606=VERTEX_POINT('',#184220);
#39607=VERTEX_POINT('',#184222);
#39608=VERTEX_POINT('',#184226);
#39609=VERTEX_POINT('',#184227);
#39610=VERTEX_POINT('',#184229);
#39611=VERTEX_POINT('',#184231);
#39612=VERTEX_POINT('',#184233);
#39613=VERTEX_POINT('',#184235);
#39614=VERTEX_POINT('',#184237);
#39615=VERTEX_POINT('',#184239);
#39616=VERTEX_POINT('',#184241);
#39617=VERTEX_POINT('',#184243);
#39618=VERTEX_POINT('',#184245);
#39619=VERTEX_POINT('',#184247);
#39620=VERTEX_POINT('',#184251);
#39621=VERTEX_POINT('',#184252);
#39622=VERTEX_POINT('',#184254);
#39623=VERTEX_POINT('',#184256);
#39624=VERTEX_POINT('',#184260);
#39625=VERTEX_POINT('',#184261);
#39626=VERTEX_POINT('',#184263);
#39627=VERTEX_POINT('',#184265);
#39628=VERTEX_POINT('',#184267);
#39629=VERTEX_POINT('',#184269);
#39630=VERTEX_POINT('',#184271);
#39631=VERTEX_POINT('',#184273);
#39632=VERTEX_POINT('',#184275);
#39633=VERTEX_POINT('',#184277);
#39634=VERTEX_POINT('',#184279);
#39635=VERTEX_POINT('',#184281);
#39636=VERTEX_POINT('',#184285);
#39637=VERTEX_POINT('',#184286);
#39638=VERTEX_POINT('',#184288);
#39639=VERTEX_POINT('',#184290);
#39640=VERTEX_POINT('',#184292);
#39641=VERTEX_POINT('',#184294);
#39642=VERTEX_POINT('',#184296);
#39643=VERTEX_POINT('',#184298);
#39644=VERTEX_POINT('',#184300);
#39645=VERTEX_POINT('',#184302);
#39646=VERTEX_POINT('',#184304);
#39647=VERTEX_POINT('',#184306);
#39648=VERTEX_POINT('',#184310);
#39649=VERTEX_POINT('',#184311);
#39650=VERTEX_POINT('',#184313);
#39651=VERTEX_POINT('',#184315);
#39652=VERTEX_POINT('',#184319);
#39653=VERTEX_POINT('',#184320);
#39654=VERTEX_POINT('',#184322);
#39655=VERTEX_POINT('',#184324);
#39656=VERTEX_POINT('',#184326);
#39657=VERTEX_POINT('',#184328);
#39658=VERTEX_POINT('',#184330);
#39659=VERTEX_POINT('',#184332);
#39660=VERTEX_POINT('',#184334);
#39661=VERTEX_POINT('',#184336);
#39662=VERTEX_POINT('',#184338);
#39663=VERTEX_POINT('',#184340);
#39664=VERTEX_POINT('',#184344);
#39665=VERTEX_POINT('',#184345);
#39666=VERTEX_POINT('',#184347);
#39667=VERTEX_POINT('',#184349);
#39668=VERTEX_POINT('',#184351);
#39669=VERTEX_POINT('',#184353);
#39670=VERTEX_POINT('',#184355);
#39671=VERTEX_POINT('',#184357);
#39672=VERTEX_POINT('',#184359);
#39673=VERTEX_POINT('',#184361);
#39674=VERTEX_POINT('',#184363);
#39675=VERTEX_POINT('',#184365);
#39676=VERTEX_POINT('',#184369);
#39677=VERTEX_POINT('',#184370);
#39678=VERTEX_POINT('',#184372);
#39679=VERTEX_POINT('',#184374);
#39680=VERTEX_POINT('',#184378);
#39681=VERTEX_POINT('',#184379);
#39682=VERTEX_POINT('',#184381);
#39683=VERTEX_POINT('',#184383);
#39684=VERTEX_POINT('',#184385);
#39685=VERTEX_POINT('',#184387);
#39686=VERTEX_POINT('',#184389);
#39687=VERTEX_POINT('',#184391);
#39688=VERTEX_POINT('',#184393);
#39689=VERTEX_POINT('',#184395);
#39690=VERTEX_POINT('',#184397);
#39691=VERTEX_POINT('',#184399);
#39692=VERTEX_POINT('',#184403);
#39693=VERTEX_POINT('',#184404);
#39694=VERTEX_POINT('',#184406);
#39695=VERTEX_POINT('',#184408);
#39696=VERTEX_POINT('',#184410);
#39697=VERTEX_POINT('',#184412);
#39698=VERTEX_POINT('',#184414);
#39699=VERTEX_POINT('',#184416);
#39700=VERTEX_POINT('',#184418);
#39701=VERTEX_POINT('',#184420);
#39702=VERTEX_POINT('',#184422);
#39703=VERTEX_POINT('',#184424);
#39704=VERTEX_POINT('',#184428);
#39705=VERTEX_POINT('',#184429);
#39706=VERTEX_POINT('',#184431);
#39707=VERTEX_POINT('',#184433);
#39708=VERTEX_POINT('',#184437);
#39709=VERTEX_POINT('',#184438);
#39710=VERTEX_POINT('',#184440);
#39711=VERTEX_POINT('',#184442);
#39712=VERTEX_POINT('',#184444);
#39713=VERTEX_POINT('',#184446);
#39714=VERTEX_POINT('',#184448);
#39715=VERTEX_POINT('',#184450);
#39716=VERTEX_POINT('',#184452);
#39717=VERTEX_POINT('',#184454);
#39718=VERTEX_POINT('',#184456);
#39719=VERTEX_POINT('',#184458);
#39720=VERTEX_POINT('',#184462);
#39721=VERTEX_POINT('',#184463);
#39722=VERTEX_POINT('',#184465);
#39723=VERTEX_POINT('',#184467);
#39724=VERTEX_POINT('',#184469);
#39725=VERTEX_POINT('',#184471);
#39726=VERTEX_POINT('',#184473);
#39727=VERTEX_POINT('',#184475);
#39728=VERTEX_POINT('',#184477);
#39729=VERTEX_POINT('',#184479);
#39730=VERTEX_POINT('',#184481);
#39731=VERTEX_POINT('',#184483);
#39732=VERTEX_POINT('',#184487);
#39733=VERTEX_POINT('',#184488);
#39734=VERTEX_POINT('',#184490);
#39735=VERTEX_POINT('',#184492);
#39736=VERTEX_POINT('',#184496);
#39737=VERTEX_POINT('',#184497);
#39738=VERTEX_POINT('',#184499);
#39739=VERTEX_POINT('',#184501);
#39740=VERTEX_POINT('',#184503);
#39741=VERTEX_POINT('',#184505);
#39742=VERTEX_POINT('',#184507);
#39743=VERTEX_POINT('',#184509);
#39744=VERTEX_POINT('',#184511);
#39745=VERTEX_POINT('',#184513);
#39746=VERTEX_POINT('',#184515);
#39747=VERTEX_POINT('',#184517);
#39748=VERTEX_POINT('',#184521);
#39749=VERTEX_POINT('',#184522);
#39750=VERTEX_POINT('',#184524);
#39751=VERTEX_POINT('',#184526);
#39752=VERTEX_POINT('',#184528);
#39753=VERTEX_POINT('',#184530);
#39754=VERTEX_POINT('',#184532);
#39755=VERTEX_POINT('',#184534);
#39756=VERTEX_POINT('',#184536);
#39757=VERTEX_POINT('',#184538);
#39758=VERTEX_POINT('',#184540);
#39759=VERTEX_POINT('',#184542);
#39760=VERTEX_POINT('',#184546);
#39761=VERTEX_POINT('',#184547);
#39762=VERTEX_POINT('',#184549);
#39763=VERTEX_POINT('',#184551);
#39764=VERTEX_POINT('',#184555);
#39765=VERTEX_POINT('',#184556);
#39766=VERTEX_POINT('',#184558);
#39767=VERTEX_POINT('',#184560);
#39768=VERTEX_POINT('',#184562);
#39769=VERTEX_POINT('',#184564);
#39770=VERTEX_POINT('',#184566);
#39771=VERTEX_POINT('',#184568);
#39772=VERTEX_POINT('',#184570);
#39773=VERTEX_POINT('',#184572);
#39774=VERTEX_POINT('',#184574);
#39775=VERTEX_POINT('',#184576);
#39776=VERTEX_POINT('',#184580);
#39777=VERTEX_POINT('',#184581);
#39778=VERTEX_POINT('',#184583);
#39779=VERTEX_POINT('',#184585);
#39780=VERTEX_POINT('',#184587);
#39781=VERTEX_POINT('',#184589);
#39782=VERTEX_POINT('',#184591);
#39783=VERTEX_POINT('',#184593);
#39784=VERTEX_POINT('',#184595);
#39785=VERTEX_POINT('',#184597);
#39786=VERTEX_POINT('',#184599);
#39787=VERTEX_POINT('',#184601);
#39788=VERTEX_POINT('',#184605);
#39789=VERTEX_POINT('',#184606);
#39790=VERTEX_POINT('',#184608);
#39791=VERTEX_POINT('',#184610);
#39792=VERTEX_POINT('',#184614);
#39793=VERTEX_POINT('',#184615);
#39794=VERTEX_POINT('',#184617);
#39795=VERTEX_POINT('',#184619);
#39796=VERTEX_POINT('',#184621);
#39797=VERTEX_POINT('',#184623);
#39798=VERTEX_POINT('',#184625);
#39799=VERTEX_POINT('',#184627);
#39800=VERTEX_POINT('',#184629);
#39801=VERTEX_POINT('',#184631);
#39802=VERTEX_POINT('',#184633);
#39803=VERTEX_POINT('',#184635);
#39804=VERTEX_POINT('',#184639);
#39805=VERTEX_POINT('',#184640);
#39806=VERTEX_POINT('',#184642);
#39807=VERTEX_POINT('',#184644);
#39808=VERTEX_POINT('',#184646);
#39809=VERTEX_POINT('',#184648);
#39810=VERTEX_POINT('',#184650);
#39811=VERTEX_POINT('',#184652);
#39812=VERTEX_POINT('',#184654);
#39813=VERTEX_POINT('',#184656);
#39814=VERTEX_POINT('',#184658);
#39815=VERTEX_POINT('',#184660);
#39816=VERTEX_POINT('',#184664);
#39817=VERTEX_POINT('',#184665);
#39818=VERTEX_POINT('',#184667);
#39819=VERTEX_POINT('',#184669);
#39820=VERTEX_POINT('',#184673);
#39821=VERTEX_POINT('',#184674);
#39822=VERTEX_POINT('',#184676);
#39823=VERTEX_POINT('',#184678);
#39824=VERTEX_POINT('',#184680);
#39825=VERTEX_POINT('',#184682);
#39826=VERTEX_POINT('',#184684);
#39827=VERTEX_POINT('',#184686);
#39828=VERTEX_POINT('',#184688);
#39829=VERTEX_POINT('',#184690);
#39830=VERTEX_POINT('',#184692);
#39831=VERTEX_POINT('',#184694);
#39832=VERTEX_POINT('',#184698);
#39833=VERTEX_POINT('',#184699);
#39834=VERTEX_POINT('',#184701);
#39835=VERTEX_POINT('',#184703);
#39836=VERTEX_POINT('',#184705);
#39837=VERTEX_POINT('',#184707);
#39838=VERTEX_POINT('',#184709);
#39839=VERTEX_POINT('',#184711);
#39840=VERTEX_POINT('',#184713);
#39841=VERTEX_POINT('',#184715);
#39842=VERTEX_POINT('',#184717);
#39843=VERTEX_POINT('',#184719);
#39844=VERTEX_POINT('',#184723);
#39845=VERTEX_POINT('',#184724);
#39846=VERTEX_POINT('',#184726);
#39847=VERTEX_POINT('',#184728);
#39848=VERTEX_POINT('',#184732);
#39849=VERTEX_POINT('',#184733);
#39850=VERTEX_POINT('',#184735);
#39851=VERTEX_POINT('',#184737);
#39852=VERTEX_POINT('',#184739);
#39853=VERTEX_POINT('',#184741);
#39854=VERTEX_POINT('',#184743);
#39855=VERTEX_POINT('',#184745);
#39856=VERTEX_POINT('',#184747);
#39857=VERTEX_POINT('',#184749);
#39858=VERTEX_POINT('',#184751);
#39859=VERTEX_POINT('',#184753);
#39860=VERTEX_POINT('',#184757);
#39861=VERTEX_POINT('',#184758);
#39862=VERTEX_POINT('',#184760);
#39863=VERTEX_POINT('',#184762);
#39864=VERTEX_POINT('',#184764);
#39865=VERTEX_POINT('',#184766);
#39866=VERTEX_POINT('',#184768);
#39867=VERTEX_POINT('',#184770);
#39868=VERTEX_POINT('',#184772);
#39869=VERTEX_POINT('',#184774);
#39870=VERTEX_POINT('',#184776);
#39871=VERTEX_POINT('',#184778);
#39872=VERTEX_POINT('',#184782);
#39873=VERTEX_POINT('',#184783);
#39874=VERTEX_POINT('',#184785);
#39875=VERTEX_POINT('',#184787);
#39876=VERTEX_POINT('',#184791);
#39877=VERTEX_POINT('',#184792);
#39878=VERTEX_POINT('',#184794);
#39879=VERTEX_POINT('',#184796);
#39880=VERTEX_POINT('',#184798);
#39881=VERTEX_POINT('',#184800);
#39882=VERTEX_POINT('',#184802);
#39883=VERTEX_POINT('',#184804);
#39884=VERTEX_POINT('',#184806);
#39885=VERTEX_POINT('',#184808);
#39886=VERTEX_POINT('',#184810);
#39887=VERTEX_POINT('',#184812);
#39888=VERTEX_POINT('',#184816);
#39889=VERTEX_POINT('',#184817);
#39890=VERTEX_POINT('',#184819);
#39891=VERTEX_POINT('',#184821);
#39892=VERTEX_POINT('',#184823);
#39893=VERTEX_POINT('',#184825);
#39894=VERTEX_POINT('',#184827);
#39895=VERTEX_POINT('',#184829);
#39896=VERTEX_POINT('',#184831);
#39897=VERTEX_POINT('',#184833);
#39898=VERTEX_POINT('',#184835);
#39899=VERTEX_POINT('',#184837);
#39900=VERTEX_POINT('',#184841);
#39901=VERTEX_POINT('',#184842);
#39902=VERTEX_POINT('',#184844);
#39903=VERTEX_POINT('',#184846);
#39904=VERTEX_POINT('',#184850);
#39905=VERTEX_POINT('',#184851);
#39906=VERTEX_POINT('',#184853);
#39907=VERTEX_POINT('',#184855);
#39908=VERTEX_POINT('',#184857);
#39909=VERTEX_POINT('',#184859);
#39910=VERTEX_POINT('',#184861);
#39911=VERTEX_POINT('',#184863);
#39912=VERTEX_POINT('',#184865);
#39913=VERTEX_POINT('',#184867);
#39914=VERTEX_POINT('',#184869);
#39915=VERTEX_POINT('',#184871);
#39916=VERTEX_POINT('',#184875);
#39917=VERTEX_POINT('',#184876);
#39918=VERTEX_POINT('',#184878);
#39919=VERTEX_POINT('',#184880);
#39920=VERTEX_POINT('',#184882);
#39921=VERTEX_POINT('',#184884);
#39922=VERTEX_POINT('',#184886);
#39923=VERTEX_POINT('',#184888);
#39924=VERTEX_POINT('',#184890);
#39925=VERTEX_POINT('',#184892);
#39926=VERTEX_POINT('',#184894);
#39927=VERTEX_POINT('',#184896);
#39928=VERTEX_POINT('',#184900);
#39929=VERTEX_POINT('',#184901);
#39930=VERTEX_POINT('',#184903);
#39931=VERTEX_POINT('',#184905);
#39932=VERTEX_POINT('',#184909);
#39933=VERTEX_POINT('',#184910);
#39934=VERTEX_POINT('',#184912);
#39935=VERTEX_POINT('',#184914);
#39936=VERTEX_POINT('',#184916);
#39937=VERTEX_POINT('',#184918);
#39938=VERTEX_POINT('',#184920);
#39939=VERTEX_POINT('',#184922);
#39940=VERTEX_POINT('',#184924);
#39941=VERTEX_POINT('',#184926);
#39942=VERTEX_POINT('',#184928);
#39943=VERTEX_POINT('',#184930);
#39944=VERTEX_POINT('',#184934);
#39945=VERTEX_POINT('',#184935);
#39946=VERTEX_POINT('',#184937);
#39947=VERTEX_POINT('',#184939);
#39948=VERTEX_POINT('',#184941);
#39949=VERTEX_POINT('',#184943);
#39950=VERTEX_POINT('',#184945);
#39951=VERTEX_POINT('',#184947);
#39952=VERTEX_POINT('',#184949);
#39953=VERTEX_POINT('',#184951);
#39954=VERTEX_POINT('',#184953);
#39955=VERTEX_POINT('',#184955);
#39956=VERTEX_POINT('',#184959);
#39957=VERTEX_POINT('',#184960);
#39958=VERTEX_POINT('',#184962);
#39959=VERTEX_POINT('',#184964);
#39960=VERTEX_POINT('',#184968);
#39961=VERTEX_POINT('',#184969);
#39962=VERTEX_POINT('',#184971);
#39963=VERTEX_POINT('',#184973);
#39964=VERTEX_POINT('',#184975);
#39965=VERTEX_POINT('',#184977);
#39966=VERTEX_POINT('',#184979);
#39967=VERTEX_POINT('',#184981);
#39968=VERTEX_POINT('',#184983);
#39969=VERTEX_POINT('',#184985);
#39970=VERTEX_POINT('',#184987);
#39971=VERTEX_POINT('',#184989);
#39972=VERTEX_POINT('',#184993);
#39973=VERTEX_POINT('',#184994);
#39974=VERTEX_POINT('',#184996);
#39975=VERTEX_POINT('',#184998);
#39976=VERTEX_POINT('',#185000);
#39977=VERTEX_POINT('',#185002);
#39978=VERTEX_POINT('',#185004);
#39979=VERTEX_POINT('',#185006);
#39980=VERTEX_POINT('',#185008);
#39981=VERTEX_POINT('',#185010);
#39982=VERTEX_POINT('',#185012);
#39983=VERTEX_POINT('',#185014);
#39984=VERTEX_POINT('',#185018);
#39985=VERTEX_POINT('',#185019);
#39986=VERTEX_POINT('',#185021);
#39987=VERTEX_POINT('',#185023);
#39988=VERTEX_POINT('',#185027);
#39989=VERTEX_POINT('',#185028);
#39990=VERTEX_POINT('',#185030);
#39991=VERTEX_POINT('',#185032);
#39992=VERTEX_POINT('',#185034);
#39993=VERTEX_POINT('',#185036);
#39994=VERTEX_POINT('',#185038);
#39995=VERTEX_POINT('',#185040);
#39996=VERTEX_POINT('',#185042);
#39997=VERTEX_POINT('',#185044);
#39998=VERTEX_POINT('',#185046);
#39999=VERTEX_POINT('',#185048);
#40000=VERTEX_POINT('',#185052);
#40001=VERTEX_POINT('',#185053);
#40002=VERTEX_POINT('',#185055);
#40003=VERTEX_POINT('',#185057);
#40004=VERTEX_POINT('',#185059);
#40005=VERTEX_POINT('',#185061);
#40006=VERTEX_POINT('',#185063);
#40007=VERTEX_POINT('',#185065);
#40008=VERTEX_POINT('',#185067);
#40009=VERTEX_POINT('',#185069);
#40010=VERTEX_POINT('',#185071);
#40011=VERTEX_POINT('',#185073);
#40012=VERTEX_POINT('',#185080);
#40013=VERTEX_POINT('',#185081);
#40014=VERTEX_POINT('',#185083);
#40015=VERTEX_POINT('',#185085);
#40016=VERTEX_POINT('',#185087);
#40017=VERTEX_POINT('',#185089);
#40018=VERTEX_POINT('',#185091);
#40019=VERTEX_POINT('',#185093);
#40020=VERTEX_POINT('',#185095);
#40021=VERTEX_POINT('',#185097);
#40022=VERTEX_POINT('',#185099);
#40023=VERTEX_POINT('',#185101);
#40024=VERTEX_POINT('',#185105);
#40025=VERTEX_POINT('',#185106);
#40026=VERTEX_POINT('',#185108);
#40027=VERTEX_POINT('',#185110);
#40028=VERTEX_POINT('',#185112);
#40029=VERTEX_POINT('',#185114);
#40030=VERTEX_POINT('',#185116);
#40031=VERTEX_POINT('',#185118);
#40032=VERTEX_POINT('',#185120);
#40033=VERTEX_POINT('',#185122);
#40034=VERTEX_POINT('',#185124);
#40035=VERTEX_POINT('',#185126);
#40036=VERTEX_POINT('',#185130);
#40037=VERTEX_POINT('',#185131);
#40038=VERTEX_POINT('',#185133);
#40039=VERTEX_POINT('',#185135);
#40040=VERTEX_POINT('',#185139);
#40041=VERTEX_POINT('',#185140);
#40042=VERTEX_POINT('',#185142);
#40043=VERTEX_POINT('',#185144);
#40044=VERTEX_POINT('',#185146);
#40045=VERTEX_POINT('',#185148);
#40046=VERTEX_POINT('',#185150);
#40047=VERTEX_POINT('',#185152);
#40048=VERTEX_POINT('',#185154);
#40049=VERTEX_POINT('',#185156);
#40050=VERTEX_POINT('',#185158);
#40051=VERTEX_POINT('',#185160);
#40052=VERTEX_POINT('',#185164);
#40053=VERTEX_POINT('',#185165);
#40054=VERTEX_POINT('',#185167);
#40055=VERTEX_POINT('',#185169);
#40056=VERTEX_POINT('',#185171);
#40057=VERTEX_POINT('',#185173);
#40058=VERTEX_POINT('',#185175);
#40059=VERTEX_POINT('',#185177);
#40060=VERTEX_POINT('',#185179);
#40061=VERTEX_POINT('',#185181);
#40062=VERTEX_POINT('',#185183);
#40063=VERTEX_POINT('',#185185);
#40064=VERTEX_POINT('',#185189);
#40065=VERTEX_POINT('',#185190);
#40066=VERTEX_POINT('',#185192);
#40067=VERTEX_POINT('',#185194);
#40068=VERTEX_POINT('',#185198);
#40069=VERTEX_POINT('',#185199);
#40070=VERTEX_POINT('',#185201);
#40071=VERTEX_POINT('',#185203);
#40072=VERTEX_POINT('',#185205);
#40073=VERTEX_POINT('',#185207);
#40074=VERTEX_POINT('',#185209);
#40075=VERTEX_POINT('',#185211);
#40076=VERTEX_POINT('',#185213);
#40077=VERTEX_POINT('',#185215);
#40078=VERTEX_POINT('',#185217);
#40079=VERTEX_POINT('',#185219);
#40080=VERTEX_POINT('',#185223);
#40081=VERTEX_POINT('',#185224);
#40082=VERTEX_POINT('',#185226);
#40083=VERTEX_POINT('',#185228);
#40084=VERTEX_POINT('',#185230);
#40085=VERTEX_POINT('',#185232);
#40086=VERTEX_POINT('',#185234);
#40087=VERTEX_POINT('',#185236);
#40088=VERTEX_POINT('',#185238);
#40089=VERTEX_POINT('',#185240);
#40090=VERTEX_POINT('',#185242);
#40091=VERTEX_POINT('',#185244);
#40092=VERTEX_POINT('',#185248);
#40093=VERTEX_POINT('',#185249);
#40094=VERTEX_POINT('',#185251);
#40095=VERTEX_POINT('',#185253);
#40096=VERTEX_POINT('',#185257);
#40097=VERTEX_POINT('',#185258);
#40098=VERTEX_POINT('',#185260);
#40099=VERTEX_POINT('',#185262);
#40100=VERTEX_POINT('',#185264);
#40101=VERTEX_POINT('',#185266);
#40102=VERTEX_POINT('',#185268);
#40103=VERTEX_POINT('',#185270);
#40104=VERTEX_POINT('',#185272);
#40105=VERTEX_POINT('',#185274);
#40106=VERTEX_POINT('',#185276);
#40107=VERTEX_POINT('',#185278);
#40108=VERTEX_POINT('',#185282);
#40109=VERTEX_POINT('',#185283);
#40110=VERTEX_POINT('',#185285);
#40111=VERTEX_POINT('',#185287);
#40112=VERTEX_POINT('',#185289);
#40113=VERTEX_POINT('',#185291);
#40114=VERTEX_POINT('',#185293);
#40115=VERTEX_POINT('',#185295);
#40116=VERTEX_POINT('',#185297);
#40117=VERTEX_POINT('',#185299);
#40118=VERTEX_POINT('',#185301);
#40119=VERTEX_POINT('',#185303);
#40120=VERTEX_POINT('',#185307);
#40121=VERTEX_POINT('',#185308);
#40122=VERTEX_POINT('',#185310);
#40123=VERTEX_POINT('',#185312);
#40124=VERTEX_POINT('',#185316);
#40125=VERTEX_POINT('',#185317);
#40126=VERTEX_POINT('',#185319);
#40127=VERTEX_POINT('',#185321);
#40128=VERTEX_POINT('',#185323);
#40129=VERTEX_POINT('',#185325);
#40130=VERTEX_POINT('',#185327);
#40131=VERTEX_POINT('',#185329);
#40132=VERTEX_POINT('',#185331);
#40133=VERTEX_POINT('',#185333);
#40134=VERTEX_POINT('',#185335);
#40135=VERTEX_POINT('',#185337);
#40136=VERTEX_POINT('',#185341);
#40137=VERTEX_POINT('',#185342);
#40138=VERTEX_POINT('',#185344);
#40139=VERTEX_POINT('',#185346);
#40140=VERTEX_POINT('',#185348);
#40141=VERTEX_POINT('',#185350);
#40142=VERTEX_POINT('',#185352);
#40143=VERTEX_POINT('',#185354);
#40144=VERTEX_POINT('',#185356);
#40145=VERTEX_POINT('',#185358);
#40146=VERTEX_POINT('',#185360);
#40147=VERTEX_POINT('',#185362);
#40148=VERTEX_POINT('',#185366);
#40149=VERTEX_POINT('',#185367);
#40150=VERTEX_POINT('',#185369);
#40151=VERTEX_POINT('',#185371);
#40152=VERTEX_POINT('',#185375);
#40153=VERTEX_POINT('',#185376);
#40154=VERTEX_POINT('',#185378);
#40155=VERTEX_POINT('',#185380);
#40156=VERTEX_POINT('',#185382);
#40157=VERTEX_POINT('',#185384);
#40158=VERTEX_POINT('',#185386);
#40159=VERTEX_POINT('',#185388);
#40160=VERTEX_POINT('',#185390);
#40161=VERTEX_POINT('',#185392);
#40162=VERTEX_POINT('',#185394);
#40163=VERTEX_POINT('',#185396);
#40164=VERTEX_POINT('',#185400);
#40165=VERTEX_POINT('',#185401);
#40166=VERTEX_POINT('',#185403);
#40167=VERTEX_POINT('',#185405);
#40168=VERTEX_POINT('',#185407);
#40169=VERTEX_POINT('',#185409);
#40170=VERTEX_POINT('',#185411);
#40171=VERTEX_POINT('',#185413);
#40172=VERTEX_POINT('',#185415);
#40173=VERTEX_POINT('',#185417);
#40174=VERTEX_POINT('',#185419);
#40175=VERTEX_POINT('',#185421);
#40176=VERTEX_POINT('',#185425);
#40177=VERTEX_POINT('',#185426);
#40178=VERTEX_POINT('',#185428);
#40179=VERTEX_POINT('',#185430);
#40180=VERTEX_POINT('',#185434);
#40181=VERTEX_POINT('',#185435);
#40182=VERTEX_POINT('',#185437);
#40183=VERTEX_POINT('',#185439);
#40184=VERTEX_POINT('',#185441);
#40185=VERTEX_POINT('',#185443);
#40186=VERTEX_POINT('',#185445);
#40187=VERTEX_POINT('',#185447);
#40188=VERTEX_POINT('',#185449);
#40189=VERTEX_POINT('',#185451);
#40190=VERTEX_POINT('',#185453);
#40191=VERTEX_POINT('',#185455);
#40192=VERTEX_POINT('',#185459);
#40193=VERTEX_POINT('',#185460);
#40194=VERTEX_POINT('',#185462);
#40195=VERTEX_POINT('',#185464);
#40196=VERTEX_POINT('',#185466);
#40197=VERTEX_POINT('',#185468);
#40198=VERTEX_POINT('',#185470);
#40199=VERTEX_POINT('',#185472);
#40200=VERTEX_POINT('',#185474);
#40201=VERTEX_POINT('',#185476);
#40202=VERTEX_POINT('',#185478);
#40203=VERTEX_POINT('',#185480);
#40204=VERTEX_POINT('',#185484);
#40205=VERTEX_POINT('',#185485);
#40206=VERTEX_POINT('',#185487);
#40207=VERTEX_POINT('',#185489);
#40208=VERTEX_POINT('',#185493);
#40209=VERTEX_POINT('',#185494);
#40210=VERTEX_POINT('',#185496);
#40211=VERTEX_POINT('',#185498);
#40212=VERTEX_POINT('',#185500);
#40213=VERTEX_POINT('',#185502);
#40214=VERTEX_POINT('',#185504);
#40215=VERTEX_POINT('',#185506);
#40216=VERTEX_POINT('',#185508);
#40217=VERTEX_POINT('',#185510);
#40218=VERTEX_POINT('',#185512);
#40219=VERTEX_POINT('',#185514);
#40220=VERTEX_POINT('',#185518);
#40221=VERTEX_POINT('',#185519);
#40222=VERTEX_POINT('',#185521);
#40223=VERTEX_POINT('',#185523);
#40224=VERTEX_POINT('',#185525);
#40225=VERTEX_POINT('',#185527);
#40226=VERTEX_POINT('',#185529);
#40227=VERTEX_POINT('',#185531);
#40228=VERTEX_POINT('',#185533);
#40229=VERTEX_POINT('',#185535);
#40230=VERTEX_POINT('',#185537);
#40231=VERTEX_POINT('',#185539);
#40232=VERTEX_POINT('',#185543);
#40233=VERTEX_POINT('',#185544);
#40234=VERTEX_POINT('',#185546);
#40235=VERTEX_POINT('',#185548);
#40236=VERTEX_POINT('',#185552);
#40237=VERTEX_POINT('',#185553);
#40238=VERTEX_POINT('',#185555);
#40239=VERTEX_POINT('',#185557);
#40240=VERTEX_POINT('',#185559);
#40241=VERTEX_POINT('',#185561);
#40242=VERTEX_POINT('',#185563);
#40243=VERTEX_POINT('',#185565);
#40244=VERTEX_POINT('',#185567);
#40245=VERTEX_POINT('',#185569);
#40246=VERTEX_POINT('',#185571);
#40247=VERTEX_POINT('',#185573);
#40248=VERTEX_POINT('',#185577);
#40249=VERTEX_POINT('',#185578);
#40250=VERTEX_POINT('',#185580);
#40251=VERTEX_POINT('',#185582);
#40252=VERTEX_POINT('',#185584);
#40253=VERTEX_POINT('',#185586);
#40254=VERTEX_POINT('',#185588);
#40255=VERTEX_POINT('',#185590);
#40256=VERTEX_POINT('',#185592);
#40257=VERTEX_POINT('',#185594);
#40258=VERTEX_POINT('',#185596);
#40259=VERTEX_POINT('',#185598);
#40260=VERTEX_POINT('',#185602);
#40261=VERTEX_POINT('',#185603);
#40262=VERTEX_POINT('',#185605);
#40263=VERTEX_POINT('',#185607);
#40264=VERTEX_POINT('',#185611);
#40265=VERTEX_POINT('',#185612);
#40266=VERTEX_POINT('',#185614);
#40267=VERTEX_POINT('',#185616);
#40268=VERTEX_POINT('',#185618);
#40269=VERTEX_POINT('',#185620);
#40270=VERTEX_POINT('',#185622);
#40271=VERTEX_POINT('',#185624);
#40272=VERTEX_POINT('',#185626);
#40273=VERTEX_POINT('',#185628);
#40274=VERTEX_POINT('',#185630);
#40275=VERTEX_POINT('',#185632);
#40276=VERTEX_POINT('',#185636);
#40277=VERTEX_POINT('',#185637);
#40278=VERTEX_POINT('',#185639);
#40279=VERTEX_POINT('',#185641);
#40280=VERTEX_POINT('',#185643);
#40281=VERTEX_POINT('',#185645);
#40282=VERTEX_POINT('',#185647);
#40283=VERTEX_POINT('',#185649);
#40284=VERTEX_POINT('',#185651);
#40285=VERTEX_POINT('',#185653);
#40286=VERTEX_POINT('',#185655);
#40287=VERTEX_POINT('',#185657);
#40288=VERTEX_POINT('',#185661);
#40289=VERTEX_POINT('',#185662);
#40290=VERTEX_POINT('',#185664);
#40291=VERTEX_POINT('',#185666);
#40292=VERTEX_POINT('',#185670);
#40293=VERTEX_POINT('',#185671);
#40294=VERTEX_POINT('',#185673);
#40295=VERTEX_POINT('',#185675);
#40296=VERTEX_POINT('',#185677);
#40297=VERTEX_POINT('',#185679);
#40298=VERTEX_POINT('',#185681);
#40299=VERTEX_POINT('',#185683);
#40300=VERTEX_POINT('',#185685);
#40301=VERTEX_POINT('',#185687);
#40302=VERTEX_POINT('',#185689);
#40303=VERTEX_POINT('',#185691);
#40304=VERTEX_POINT('',#185695);
#40305=VERTEX_POINT('',#185696);
#40306=VERTEX_POINT('',#185698);
#40307=VERTEX_POINT('',#185700);
#40308=VERTEX_POINT('',#185702);
#40309=VERTEX_POINT('',#185704);
#40310=VERTEX_POINT('',#185706);
#40311=VERTEX_POINT('',#185708);
#40312=VERTEX_POINT('',#185710);
#40313=VERTEX_POINT('',#185712);
#40314=VERTEX_POINT('',#185714);
#40315=VERTEX_POINT('',#185716);
#40316=VERTEX_POINT('',#185720);
#40317=VERTEX_POINT('',#185721);
#40318=VERTEX_POINT('',#185723);
#40319=VERTEX_POINT('',#185725);
#40320=VERTEX_POINT('',#185729);
#40321=VERTEX_POINT('',#185730);
#40322=VERTEX_POINT('',#185732);
#40323=VERTEX_POINT('',#185734);
#40324=VERTEX_POINT('',#185736);
#40325=VERTEX_POINT('',#185738);
#40326=VERTEX_POINT('',#185740);
#40327=VERTEX_POINT('',#185742);
#40328=VERTEX_POINT('',#185744);
#40329=VERTEX_POINT('',#185746);
#40330=VERTEX_POINT('',#185748);
#40331=VERTEX_POINT('',#185750);
#40332=VERTEX_POINT('',#185754);
#40333=VERTEX_POINT('',#185755);
#40334=VERTEX_POINT('',#185757);
#40335=VERTEX_POINT('',#185759);
#40336=VERTEX_POINT('',#185761);
#40337=VERTEX_POINT('',#185763);
#40338=VERTEX_POINT('',#185765);
#40339=VERTEX_POINT('',#185767);
#40340=VERTEX_POINT('',#185769);
#40341=VERTEX_POINT('',#185771);
#40342=VERTEX_POINT('',#185773);
#40343=VERTEX_POINT('',#185775);
#40344=VERTEX_POINT('',#185779);
#40345=VERTEX_POINT('',#185780);
#40346=VERTEX_POINT('',#185782);
#40347=VERTEX_POINT('',#185784);
#40348=VERTEX_POINT('',#185788);
#40349=VERTEX_POINT('',#185789);
#40350=VERTEX_POINT('',#185791);
#40351=VERTEX_POINT('',#185793);
#40352=VERTEX_POINT('',#185795);
#40353=VERTEX_POINT('',#185797);
#40354=VERTEX_POINT('',#185799);
#40355=VERTEX_POINT('',#185801);
#40356=VERTEX_POINT('',#185803);
#40357=VERTEX_POINT('',#185805);
#40358=VERTEX_POINT('',#185807);
#40359=VERTEX_POINT('',#185809);
#40360=VERTEX_POINT('',#185813);
#40361=VERTEX_POINT('',#185814);
#40362=VERTEX_POINT('',#185816);
#40363=VERTEX_POINT('',#185818);
#40364=VERTEX_POINT('',#185820);
#40365=VERTEX_POINT('',#185822);
#40366=VERTEX_POINT('',#185824);
#40367=VERTEX_POINT('',#185826);
#40368=VERTEX_POINT('',#185828);
#40369=VERTEX_POINT('',#185830);
#40370=VERTEX_POINT('',#185832);
#40371=VERTEX_POINT('',#185834);
#40372=VERTEX_POINT('',#185838);
#40373=VERTEX_POINT('',#185839);
#40374=VERTEX_POINT('',#185841);
#40375=VERTEX_POINT('',#185843);
#40376=VERTEX_POINT('',#185847);
#40377=VERTEX_POINT('',#185848);
#40378=VERTEX_POINT('',#185850);
#40379=VERTEX_POINT('',#185852);
#40380=VERTEX_POINT('',#185854);
#40381=VERTEX_POINT('',#185856);
#40382=VERTEX_POINT('',#185858);
#40383=VERTEX_POINT('',#185860);
#40384=VERTEX_POINT('',#185862);
#40385=VERTEX_POINT('',#185864);
#40386=VERTEX_POINT('',#185866);
#40387=VERTEX_POINT('',#185868);
#40388=VERTEX_POINT('',#185872);
#40389=VERTEX_POINT('',#185873);
#40390=VERTEX_POINT('',#185875);
#40391=VERTEX_POINT('',#185877);
#40392=VERTEX_POINT('',#185879);
#40393=VERTEX_POINT('',#185881);
#40394=VERTEX_POINT('',#185883);
#40395=VERTEX_POINT('',#185885);
#40396=VERTEX_POINT('',#185887);
#40397=VERTEX_POINT('',#185889);
#40398=VERTEX_POINT('',#185891);
#40399=VERTEX_POINT('',#185893);
#40400=VERTEX_POINT('',#185897);
#40401=VERTEX_POINT('',#185898);
#40402=VERTEX_POINT('',#185900);
#40403=VERTEX_POINT('',#185902);
#40404=VERTEX_POINT('',#185906);
#40405=VERTEX_POINT('',#185907);
#40406=VERTEX_POINT('',#185909);
#40407=VERTEX_POINT('',#185911);
#40408=VERTEX_POINT('',#185913);
#40409=VERTEX_POINT('',#185915);
#40410=VERTEX_POINT('',#185917);
#40411=VERTEX_POINT('',#185919);
#40412=VERTEX_POINT('',#185921);
#40413=VERTEX_POINT('',#185923);
#40414=VERTEX_POINT('',#185925);
#40415=VERTEX_POINT('',#185927);
#40416=VERTEX_POINT('',#185931);
#40417=VERTEX_POINT('',#185932);
#40418=VERTEX_POINT('',#185934);
#40419=VERTEX_POINT('',#185936);
#40420=VERTEX_POINT('',#185938);
#40421=VERTEX_POINT('',#185940);
#40422=VERTEX_POINT('',#185942);
#40423=VERTEX_POINT('',#185944);
#40424=VERTEX_POINT('',#185946);
#40425=VERTEX_POINT('',#185948);
#40426=VERTEX_POINT('',#185950);
#40427=VERTEX_POINT('',#185952);
#40428=VERTEX_POINT('',#210488);
#40429=VERTEX_POINT('',#210489);
#40430=VERTEX_POINT('',#210491);
#40431=VERTEX_POINT('',#210493);
#40432=VERTEX_POINT('',#210497);
#40433=VERTEX_POINT('',#210498);
#40434=VERTEX_POINT('',#210500);
#40435=VERTEX_POINT('',#210502);
#40436=VERTEX_POINT('',#210506);
#40437=VERTEX_POINT('',#210507);
#40438=VERTEX_POINT('',#210509);
#40439=VERTEX_POINT('',#210511);
#40440=VERTEX_POINT('',#210515);
#40441=VERTEX_POINT('',#210516);
#40442=VERTEX_POINT('',#210518);
#40443=VERTEX_POINT('',#210520);
#40444=VERTEX_POINT('',#210522);
#40445=VERTEX_POINT('',#210526);
#40446=VERTEX_POINT('',#210528);
#40447=VERTEX_POINT('',#210530);
#40448=VERTEX_POINT('',#210534);
#40449=VERTEX_POINT('',#210536);
#40450=VERTEX_POINT('',#210540);
#40451=VERTEX_POINT('',#210542);
#40452=VERTEX_POINT('',#210544);
#40453=VERTEX_POINT('',#210548);
#40454=VERTEX_POINT('',#210550);
#40455=VERTEX_POINT('',#210554);
#40456=VERTEX_POINT('',#210556);
#40457=VERTEX_POINT('',#210562);
#40458=VERTEX_POINT('',#210563);
#40459=VERTEX_POINT('',#210565);
#40460=VERTEX_POINT('',#210609);
#40461=VERTEX_POINT('',#210611);
#40462=VERTEX_POINT('',#210613);
#40463=VERTEX_POINT('',#210615);
#40464=VERTEX_POINT('',#210656);
#40465=VERTEX_POINT('',#210658);
#40466=VERTEX_POINT('',#210702);
#40467=VERTEX_POINT('',#210704);
#40468=VERTEX_POINT('',#210706);
#40469=VERTEX_POINT('',#210708);
#40470=VERTEX_POINT('',#210749);
#40471=VERTEX_POINT('',#210751);
#40472=VERTEX_POINT('',#210795);
#40473=VERTEX_POINT('',#210797);
#40474=VERTEX_POINT('',#210799);
#40475=VERTEX_POINT('',#210801);
#40476=VERTEX_POINT('',#210842);
#40477=VERTEX_POINT('',#210844);
#40478=VERTEX_POINT('',#210888);
#40479=VERTEX_POINT('',#210890);
#40480=VERTEX_POINT('',#210892);
#40481=VERTEX_POINT('',#210894);
#40482=VERTEX_POINT('',#210935);
#40483=VERTEX_POINT('',#210937);
#40484=VERTEX_POINT('',#210981);
#40485=VERTEX_POINT('',#210983);
#40486=VERTEX_POINT('',#210985);
#40487=VERTEX_POINT('',#210987);
#40488=VERTEX_POINT('',#211028);
#40489=VERTEX_POINT('',#211030);
#40490=VERTEX_POINT('',#211074);
#40491=VERTEX_POINT('',#211076);
#40492=VERTEX_POINT('',#211078);
#40493=VERTEX_POINT('',#211080);
#40494=VERTEX_POINT('',#211121);
#40495=VERTEX_POINT('',#211123);
#40496=VERTEX_POINT('',#211167);
#40497=VERTEX_POINT('',#211169);
#40498=VERTEX_POINT('',#211171);
#40499=VERTEX_POINT('',#211173);
#40500=VERTEX_POINT('',#211214);
#40501=VERTEX_POINT('',#211216);
#40502=VERTEX_POINT('',#211260);
#40503=VERTEX_POINT('',#211262);
#40504=VERTEX_POINT('',#211264);
#40505=VERTEX_POINT('',#211266);
#40506=VERTEX_POINT('',#211307);
#40507=VERTEX_POINT('',#211309);
#40508=VERTEX_POINT('',#211353);
#40509=VERTEX_POINT('',#211355);
#40510=VERTEX_POINT('',#211357);
#40511=VERTEX_POINT('',#211359);
#40512=VERTEX_POINT('',#211400);
#40513=VERTEX_POINT('',#211402);
#40514=VERTEX_POINT('',#211446);
#40515=VERTEX_POINT('',#211448);
#40516=VERTEX_POINT('',#211450);
#40517=VERTEX_POINT('',#211452);
#40518=VERTEX_POINT('',#211493);
#40519=VERTEX_POINT('',#211495);
#40520=VERTEX_POINT('',#211539);
#40521=VERTEX_POINT('',#211541);
#40522=VERTEX_POINT('',#211543);
#40523=VERTEX_POINT('',#211545);
#40524=VERTEX_POINT('',#211586);
#40525=VERTEX_POINT('',#211588);
#40526=VERTEX_POINT('',#211632);
#40527=VERTEX_POINT('',#211634);
#40528=VERTEX_POINT('',#211636);
#40529=VERTEX_POINT('',#211638);
#40530=VERTEX_POINT('',#211679);
#40531=VERTEX_POINT('',#211681);
#40532=VERTEX_POINT('',#211725);
#40533=VERTEX_POINT('',#211727);
#40534=VERTEX_POINT('',#211729);
#40535=VERTEX_POINT('',#211731);
#40536=VERTEX_POINT('',#211772);
#40537=VERTEX_POINT('',#211774);
#40538=VERTEX_POINT('',#211818);
#40539=VERTEX_POINT('',#211820);
#40540=VERTEX_POINT('',#211822);
#40541=VERTEX_POINT('',#211824);
#40542=VERTEX_POINT('',#211865);
#40543=VERTEX_POINT('',#211867);
#40544=VERTEX_POINT('',#211911);
#40545=VERTEX_POINT('',#211913);
#40546=VERTEX_POINT('',#211915);
#40547=VERTEX_POINT('',#211917);
#40548=VERTEX_POINT('',#211958);
#40549=VERTEX_POINT('',#211960);
#40550=VERTEX_POINT('',#212004);
#40551=VERTEX_POINT('',#212006);
#40552=VERTEX_POINT('',#212008);
#40553=VERTEX_POINT('',#212010);
#40554=VERTEX_POINT('',#212051);
#40555=VERTEX_POINT('',#212053);
#40556=VERTEX_POINT('',#212097);
#40557=VERTEX_POINT('',#212099);
#40558=VERTEX_POINT('',#212101);
#40559=VERTEX_POINT('',#212103);
#40560=VERTEX_POINT('',#212144);
#40561=VERTEX_POINT('',#212146);
#40562=VERTEX_POINT('',#212190);
#40563=VERTEX_POINT('',#212192);
#40564=VERTEX_POINT('',#212194);
#40565=VERTEX_POINT('',#212196);
#40566=VERTEX_POINT('',#212237);
#40567=VERTEX_POINT('',#212239);
#40568=VERTEX_POINT('',#212283);
#40569=VERTEX_POINT('',#212285);
#40570=VERTEX_POINT('',#212287);
#40571=VERTEX_POINT('',#212289);
#40572=VERTEX_POINT('',#212330);
#40573=VERTEX_POINT('',#212332);
#40574=VERTEX_POINT('',#212376);
#40575=VERTEX_POINT('',#212378);
#40576=VERTEX_POINT('',#212380);
#40577=VERTEX_POINT('',#212382);
#40578=VERTEX_POINT('',#212423);
#40579=VERTEX_POINT('',#212425);
#40580=VERTEX_POINT('',#212469);
#40581=VERTEX_POINT('',#212471);
#40582=VERTEX_POINT('',#212473);
#40583=VERTEX_POINT('',#212475);
#40584=VERTEX_POINT('',#212516);
#40585=VERTEX_POINT('',#212518);
#40586=VERTEX_POINT('',#212562);
#40587=VERTEX_POINT('',#212564);
#40588=VERTEX_POINT('',#212566);
#40589=VERTEX_POINT('',#212568);
#40590=VERTEX_POINT('',#212609);
#40591=VERTEX_POINT('',#212611);
#40592=VERTEX_POINT('',#212655);
#40593=VERTEX_POINT('',#212657);
#40594=VERTEX_POINT('',#212659);
#40595=VERTEX_POINT('',#212661);
#40596=VERTEX_POINT('',#212702);
#40597=VERTEX_POINT('',#212704);
#40598=VERTEX_POINT('',#212748);
#40599=VERTEX_POINT('',#212750);
#40600=VERTEX_POINT('',#212752);
#40601=VERTEX_POINT('',#212754);
#40602=VERTEX_POINT('',#212795);
#40603=VERTEX_POINT('',#212797);
#40604=VERTEX_POINT('',#212841);
#40605=VERTEX_POINT('',#212843);
#40606=VERTEX_POINT('',#212845);
#40607=VERTEX_POINT('',#212847);
#40608=VERTEX_POINT('',#212888);
#40609=VERTEX_POINT('',#212890);
#40610=VERTEX_POINT('',#212934);
#40611=VERTEX_POINT('',#212936);
#40612=VERTEX_POINT('',#212938);
#40613=VERTEX_POINT('',#212940);
#40614=VERTEX_POINT('',#212981);
#40615=VERTEX_POINT('',#212983);
#40616=VERTEX_POINT('',#213027);
#40617=VERTEX_POINT('',#213029);
#40618=VERTEX_POINT('',#213031);
#40619=VERTEX_POINT('',#213033);
#40620=VERTEX_POINT('',#213074);
#40621=VERTEX_POINT('',#213076);
#40622=VERTEX_POINT('',#213120);
#40623=VERTEX_POINT('',#213122);
#40624=VERTEX_POINT('',#213124);
#40625=VERTEX_POINT('',#213126);
#40626=VERTEX_POINT('',#213167);
#40627=VERTEX_POINT('',#213169);
#40628=VERTEX_POINT('',#213213);
#40629=VERTEX_POINT('',#213215);
#40630=VERTEX_POINT('',#213217);
#40631=VERTEX_POINT('',#213219);
#40632=VERTEX_POINT('',#213260);
#40633=VERTEX_POINT('',#213262);
#40634=VERTEX_POINT('',#213306);
#40635=VERTEX_POINT('',#213308);
#40636=VERTEX_POINT('',#213310);
#40637=VERTEX_POINT('',#213353);
#40638=VERTEX_POINT('',#213397);
#40639=VERTEX_POINT('',#213399);
#40640=VERTEX_POINT('',#213401);
#40641=VERTEX_POINT('',#213403);
#40642=VERTEX_POINT('',#213444);
#40643=VERTEX_POINT('',#213446);
#40644=VERTEX_POINT('',#213490);
#40645=VERTEX_POINT('',#213492);
#40646=VERTEX_POINT('',#213494);
#40647=VERTEX_POINT('',#213496);
#40648=VERTEX_POINT('',#213537);
#40649=VERTEX_POINT('',#213539);
#40650=VERTEX_POINT('',#213583);
#40651=VERTEX_POINT('',#213585);
#40652=VERTEX_POINT('',#213587);
#40653=VERTEX_POINT('',#213589);
#40654=VERTEX_POINT('',#213630);
#40655=VERTEX_POINT('',#213632);
#40656=VERTEX_POINT('',#213676);
#40657=VERTEX_POINT('',#213678);
#40658=VERTEX_POINT('',#213680);
#40659=VERTEX_POINT('',#213682);
#40660=VERTEX_POINT('',#213723);
#40661=VERTEX_POINT('',#213725);
#40662=VERTEX_POINT('',#213769);
#40663=VERTEX_POINT('',#213771);
#40664=VERTEX_POINT('',#213773);
#40665=VERTEX_POINT('',#213775);
#40666=VERTEX_POINT('',#213816);
#40667=VERTEX_POINT('',#213818);
#40668=VERTEX_POINT('',#213862);
#40669=VERTEX_POINT('',#213864);
#40670=VERTEX_POINT('',#213866);
#40671=VERTEX_POINT('',#213868);
#40672=VERTEX_POINT('',#213909);
#40673=VERTEX_POINT('',#213911);
#40674=VERTEX_POINT('',#213955);
#40675=VERTEX_POINT('',#213957);
#40676=VERTEX_POINT('',#213959);
#40677=VERTEX_POINT('',#213961);
#40678=VERTEX_POINT('',#214002);
#40679=VERTEX_POINT('',#214004);
#40680=VERTEX_POINT('',#214048);
#40681=VERTEX_POINT('',#214050);
#40682=VERTEX_POINT('',#214052);
#40683=VERTEX_POINT('',#214054);
#40684=VERTEX_POINT('',#214095);
#40685=VERTEX_POINT('',#214097);
#40686=VERTEX_POINT('',#214141);
#40687=VERTEX_POINT('',#214143);
#40688=VERTEX_POINT('',#214145);
#40689=VERTEX_POINT('',#214147);
#40690=VERTEX_POINT('',#214188);
#40691=VERTEX_POINT('',#214190);
#40692=VERTEX_POINT('',#214234);
#40693=VERTEX_POINT('',#214236);
#40694=VERTEX_POINT('',#214238);
#40695=VERTEX_POINT('',#214240);
#40696=VERTEX_POINT('',#214281);
#40697=VERTEX_POINT('',#214283);
#40698=VERTEX_POINT('',#214327);
#40699=VERTEX_POINT('',#214329);
#40700=VERTEX_POINT('',#214331);
#40701=VERTEX_POINT('',#214333);
#40702=VERTEX_POINT('',#214374);
#40703=VERTEX_POINT('',#214376);
#40704=VERTEX_POINT('',#214420);
#40705=VERTEX_POINT('',#214422);
#40706=VERTEX_POINT('',#214424);
#40707=VERTEX_POINT('',#214426);
#40708=VERTEX_POINT('',#214467);
#40709=VERTEX_POINT('',#214469);
#40710=VERTEX_POINT('',#214513);
#40711=VERTEX_POINT('',#214515);
#40712=VERTEX_POINT('',#214517);
#40713=VERTEX_POINT('',#214519);
#40714=VERTEX_POINT('',#214560);
#40715=VERTEX_POINT('',#214562);
#40716=VERTEX_POINT('',#214606);
#40717=VERTEX_POINT('',#214608);
#40718=VERTEX_POINT('',#214610);
#40719=VERTEX_POINT('',#214612);
#40720=VERTEX_POINT('',#214653);
#40721=VERTEX_POINT('',#214655);
#40722=VERTEX_POINT('',#214699);
#40723=VERTEX_POINT('',#214701);
#40724=VERTEX_POINT('',#214703);
#40725=VERTEX_POINT('',#214745);
#40726=VERTEX_POINT('',#214789);
#40727=VERTEX_POINT('',#214791);
#40728=VERTEX_POINT('',#214793);
#40729=VERTEX_POINT('',#214795);
#40730=VERTEX_POINT('',#214836);
#40731=VERTEX_POINT('',#214838);
#40732=VERTEX_POINT('',#214882);
#40733=VERTEX_POINT('',#214884);
#40734=VERTEX_POINT('',#214886);
#40735=VERTEX_POINT('',#214888);
#40736=VERTEX_POINT('',#214929);
#40737=VERTEX_POINT('',#214931);
#40738=VERTEX_POINT('',#214975);
#40739=VERTEX_POINT('',#214977);
#40740=VERTEX_POINT('',#214979);
#40741=VERTEX_POINT('',#214981);
#40742=VERTEX_POINT('',#215022);
#40743=VERTEX_POINT('',#215024);
#40744=VERTEX_POINT('',#215068);
#40745=VERTEX_POINT('',#215070);
#40746=VERTEX_POINT('',#215072);
#40747=VERTEX_POINT('',#215074);
#40748=VERTEX_POINT('',#215115);
#40749=VERTEX_POINT('',#215117);
#40750=VERTEX_POINT('',#215161);
#40751=VERTEX_POINT('',#215163);
#40752=VERTEX_POINT('',#215165);
#40753=VERTEX_POINT('',#215167);
#40754=VERTEX_POINT('',#215208);
#40755=VERTEX_POINT('',#215210);
#40756=VERTEX_POINT('',#215254);
#40757=VERTEX_POINT('',#215256);
#40758=VERTEX_POINT('',#215258);
#40759=VERTEX_POINT('',#215260);
#40760=VERTEX_POINT('',#215301);
#40761=VERTEX_POINT('',#215303);
#40762=VERTEX_POINT('',#215347);
#40763=VERTEX_POINT('',#215349);
#40764=VERTEX_POINT('',#215351);
#40765=VERTEX_POINT('',#215353);
#40766=VERTEX_POINT('',#215394);
#40767=VERTEX_POINT('',#215396);
#40768=VERTEX_POINT('',#215440);
#40769=VERTEX_POINT('',#215442);
#40770=VERTEX_POINT('',#215444);
#40771=VERTEX_POINT('',#215446);
#40772=VERTEX_POINT('',#215487);
#40773=VERTEX_POINT('',#215489);
#40774=VERTEX_POINT('',#215533);
#40775=VERTEX_POINT('',#215535);
#40776=VERTEX_POINT('',#215537);
#40777=VERTEX_POINT('',#215539);
#40778=VERTEX_POINT('',#215580);
#40779=VERTEX_POINT('',#215582);
#40780=VERTEX_POINT('',#215626);
#40781=VERTEX_POINT('',#215628);
#40782=VERTEX_POINT('',#215630);
#40783=VERTEX_POINT('',#215632);
#40784=VERTEX_POINT('',#215673);
#40785=VERTEX_POINT('',#215675);
#40786=VERTEX_POINT('',#215719);
#40787=VERTEX_POINT('',#215721);
#40788=VERTEX_POINT('',#215723);
#40789=VERTEX_POINT('',#215725);
#40790=VERTEX_POINT('',#215766);
#40791=VERTEX_POINT('',#215768);
#40792=VERTEX_POINT('',#215812);
#40793=VERTEX_POINT('',#215814);
#40794=VERTEX_POINT('',#215816);
#40795=VERTEX_POINT('',#215818);
#40796=VERTEX_POINT('',#215859);
#40797=VERTEX_POINT('',#215861);
#40798=VERTEX_POINT('',#215905);
#40799=VERTEX_POINT('',#215907);
#40800=VERTEX_POINT('',#215909);
#40801=VERTEX_POINT('',#215911);
#40802=VERTEX_POINT('',#215952);
#40803=VERTEX_POINT('',#215954);
#40804=VERTEX_POINT('',#215998);
#40805=VERTEX_POINT('',#216000);
#40806=VERTEX_POINT('',#216002);
#40807=VERTEX_POINT('',#216004);
#40808=VERTEX_POINT('',#216045);
#40809=VERTEX_POINT('',#216047);
#40810=VERTEX_POINT('',#216091);
#40811=VERTEX_POINT('',#216093);
#40812=VERTEX_POINT('',#216095);
#40813=VERTEX_POINT('',#216138);
#40814=VERTEX_POINT('',#216176);
#40815=VERTEX_POINT('',#216178);
#40816=VERTEX_POINT('',#216180);
#40817=VERTEX_POINT('',#216182);
#40818=VERTEX_POINT('',#216223);
#40819=VERTEX_POINT('',#216225);
#40820=VERTEX_POINT('',#216263);
#40821=VERTEX_POINT('',#216265);
#40822=VERTEX_POINT('',#216267);
#40823=VERTEX_POINT('',#216269);
#40824=VERTEX_POINT('',#216310);
#40825=VERTEX_POINT('',#216312);
#40826=VERTEX_POINT('',#216350);
#40827=VERTEX_POINT('',#216352);
#40828=VERTEX_POINT('',#216354);
#40829=VERTEX_POINT('',#216356);
#40830=VERTEX_POINT('',#216397);
#40831=VERTEX_POINT('',#216399);
#40832=VERTEX_POINT('',#216437);
#40833=VERTEX_POINT('',#216439);
#40834=VERTEX_POINT('',#216441);
#40835=VERTEX_POINT('',#216443);
#40836=VERTEX_POINT('',#216484);
#40837=VERTEX_POINT('',#216486);
#40838=VERTEX_POINT('',#216524);
#40839=VERTEX_POINT('',#216526);
#40840=VERTEX_POINT('',#216528);
#40841=VERTEX_POINT('',#216530);
#40842=VERTEX_POINT('',#216571);
#40843=VERTEX_POINT('',#216573);
#40844=VERTEX_POINT('',#216611);
#40845=VERTEX_POINT('',#216613);
#40846=VERTEX_POINT('',#216615);
#40847=VERTEX_POINT('',#216617);
#40848=VERTEX_POINT('',#216658);
#40849=VERTEX_POINT('',#216660);
#40850=VERTEX_POINT('',#216698);
#40851=VERTEX_POINT('',#216700);
#40852=VERTEX_POINT('',#216702);
#40853=VERTEX_POINT('',#216704);
#40854=VERTEX_POINT('',#216745);
#40855=VERTEX_POINT('',#216747);
#40856=VERTEX_POINT('',#216785);
#40857=VERTEX_POINT('',#216787);
#40858=VERTEX_POINT('',#216789);
#40859=VERTEX_POINT('',#216791);
#40860=VERTEX_POINT('',#216832);
#40861=VERTEX_POINT('',#216834);
#40862=VERTEX_POINT('',#216872);
#40863=VERTEX_POINT('',#216874);
#40864=VERTEX_POINT('',#216876);
#40865=VERTEX_POINT('',#216878);
#40866=VERTEX_POINT('',#216919);
#40867=VERTEX_POINT('',#216921);
#40868=VERTEX_POINT('',#216959);
#40869=VERTEX_POINT('',#216961);
#40870=VERTEX_POINT('',#216963);
#40871=VERTEX_POINT('',#216965);
#40872=VERTEX_POINT('',#217006);
#40873=VERTEX_POINT('',#217008);
#40874=VERTEX_POINT('',#217046);
#40875=VERTEX_POINT('',#217048);
#40876=VERTEX_POINT('',#217050);
#40877=VERTEX_POINT('',#217052);
#40878=VERTEX_POINT('',#217093);
#40879=VERTEX_POINT('',#217095);
#40880=VERTEX_POINT('',#217133);
#40881=VERTEX_POINT('',#217135);
#40882=VERTEX_POINT('',#217137);
#40883=VERTEX_POINT('',#217139);
#40884=VERTEX_POINT('',#217180);
#40885=VERTEX_POINT('',#217182);
#40886=VERTEX_POINT('',#217220);
#40887=VERTEX_POINT('',#217222);
#40888=VERTEX_POINT('',#217224);
#40889=VERTEX_POINT('',#217226);
#40890=VERTEX_POINT('',#217267);
#40891=VERTEX_POINT('',#217269);
#40892=VERTEX_POINT('',#217307);
#40893=VERTEX_POINT('',#217309);
#40894=VERTEX_POINT('',#217311);
#40895=VERTEX_POINT('',#217313);
#40896=VERTEX_POINT('',#217354);
#40897=VERTEX_POINT('',#217356);
#40898=VERTEX_POINT('',#217394);
#40899=VERTEX_POINT('',#217396);
#40900=VERTEX_POINT('',#217398);
#40901=VERTEX_POINT('',#217400);
#40902=VERTEX_POINT('',#217441);
#40903=VERTEX_POINT('',#217443);
#40904=VERTEX_POINT('',#217481);
#40905=VERTEX_POINT('',#217483);
#40906=VERTEX_POINT('',#217485);
#40907=VERTEX_POINT('',#217487);
#40908=VERTEX_POINT('',#217528);
#40909=VERTEX_POINT('',#217530);
#40910=VERTEX_POINT('',#217568);
#40911=VERTEX_POINT('',#217570);
#40912=VERTEX_POINT('',#217572);
#40913=VERTEX_POINT('',#217574);
#40914=VERTEX_POINT('',#217615);
#40915=VERTEX_POINT('',#217617);
#40916=VERTEX_POINT('',#217655);
#40917=VERTEX_POINT('',#217657);
#40918=VERTEX_POINT('',#217659);
#40919=VERTEX_POINT('',#217661);
#40920=VERTEX_POINT('',#217702);
#40921=VERTEX_POINT('',#217704);
#40922=VERTEX_POINT('',#217742);
#40923=VERTEX_POINT('',#217744);
#40924=VERTEX_POINT('',#217746);
#40925=VERTEX_POINT('',#217748);
#40926=VERTEX_POINT('',#217789);
#40927=VERTEX_POINT('',#217791);
#40928=VERTEX_POINT('',#217829);
#40929=VERTEX_POINT('',#217831);
#40930=VERTEX_POINT('',#217833);
#40931=VERTEX_POINT('',#217835);
#40932=VERTEX_POINT('',#217876);
#40933=VERTEX_POINT('',#217878);
#40934=VERTEX_POINT('',#217916);
#40935=VERTEX_POINT('',#217918);
#40936=VERTEX_POINT('',#217920);
#40937=VERTEX_POINT('',#217922);
#40938=VERTEX_POINT('',#217963);
#40939=VERTEX_POINT('',#217965);
#40940=VERTEX_POINT('',#218003);
#40941=VERTEX_POINT('',#218005);
#40942=VERTEX_POINT('',#218007);
#40943=VERTEX_POINT('',#218009);
#40944=VERTEX_POINT('',#218050);
#40945=VERTEX_POINT('',#218052);
#40946=VERTEX_POINT('',#218090);
#40947=VERTEX_POINT('',#218092);
#40948=VERTEX_POINT('',#218094);
#40949=VERTEX_POINT('',#218096);
#40950=VERTEX_POINT('',#218137);
#40951=VERTEX_POINT('',#218139);
#40952=VERTEX_POINT('',#218177);
#40953=VERTEX_POINT('',#218179);
#40954=VERTEX_POINT('',#218181);
#40955=VERTEX_POINT('',#218183);
#40956=VERTEX_POINT('',#218224);
#40957=VERTEX_POINT('',#218226);
#40958=VERTEX_POINT('',#218264);
#40959=VERTEX_POINT('',#218266);
#40960=VERTEX_POINT('',#218268);
#40961=VERTEX_POINT('',#218270);
#40962=VERTEX_POINT('',#218311);
#40963=VERTEX_POINT('',#218313);
#40964=VERTEX_POINT('',#218351);
#40965=VERTEX_POINT('',#218353);
#40966=VERTEX_POINT('',#218355);
#40967=VERTEX_POINT('',#218357);
#40968=VERTEX_POINT('',#218398);
#40969=VERTEX_POINT('',#218400);
#40970=VERTEX_POINT('',#218438);
#40971=VERTEX_POINT('',#218440);
#40972=VERTEX_POINT('',#218442);
#40973=VERTEX_POINT('',#218444);
#40974=VERTEX_POINT('',#218485);
#40975=VERTEX_POINT('',#218487);
#40976=VERTEX_POINT('',#218525);
#40977=VERTEX_POINT('',#218527);
#40978=VERTEX_POINT('',#218529);
#40979=VERTEX_POINT('',#218531);
#40980=VERTEX_POINT('',#218572);
#40981=VERTEX_POINT('',#218574);
#40982=VERTEX_POINT('',#218612);
#40983=VERTEX_POINT('',#218614);
#40984=VERTEX_POINT('',#218616);
#40985=VERTEX_POINT('',#218618);
#40986=VERTEX_POINT('',#218659);
#40987=VERTEX_POINT('',#218661);
#40988=VERTEX_POINT('',#218699);
#40989=VERTEX_POINT('',#218701);
#40990=VERTEX_POINT('',#218703);
#40991=VERTEX_POINT('',#218705);
#40992=VERTEX_POINT('',#218746);
#40993=VERTEX_POINT('',#218749);
#40994=VERTEX_POINT('',#218751);
#40995=VERTEX_POINT('',#218789);
#40996=VERTEX_POINT('',#218791);
#40997=VERTEX_POINT('',#218793);
#40998=VERTEX_POINT('',#218795);
#40999=VERTEX_POINT('',#218836);
#41000=VERTEX_POINT('',#218838);
#41001=VERTEX_POINT('',#218876);
#41002=VERTEX_POINT('',#218878);
#41003=VERTEX_POINT('',#218880);
#41004=VERTEX_POINT('',#218882);
#41005=VERTEX_POINT('',#218923);
#41006=VERTEX_POINT('',#218925);
#41007=VERTEX_POINT('',#218963);
#41008=VERTEX_POINT('',#218965);
#41009=VERTEX_POINT('',#218967);
#41010=VERTEX_POINT('',#218969);
#41011=VERTEX_POINT('',#219010);
#41012=VERTEX_POINT('',#219012);
#41013=VERTEX_POINT('',#219050);
#41014=VERTEX_POINT('',#219052);
#41015=VERTEX_POINT('',#219054);
#41016=VERTEX_POINT('',#219056);
#41017=VERTEX_POINT('',#219097);
#41018=VERTEX_POINT('',#219099);
#41019=VERTEX_POINT('',#219137);
#41020=VERTEX_POINT('',#219139);
#41021=VERTEX_POINT('',#219141);
#41022=VERTEX_POINT('',#219143);
#41023=VERTEX_POINT('',#219184);
#41024=VERTEX_POINT('',#219186);
#41025=VERTEX_POINT('',#219224);
#41026=VERTEX_POINT('',#219226);
#41027=VERTEX_POINT('',#219228);
#41028=VERTEX_POINT('',#219230);
#41029=VERTEX_POINT('',#219271);
#41030=VERTEX_POINT('',#219273);
#41031=VERTEX_POINT('',#219311);
#41032=VERTEX_POINT('',#219313);
#41033=VERTEX_POINT('',#219315);
#41034=VERTEX_POINT('',#219317);
#41035=VERTEX_POINT('',#219358);
#41036=VERTEX_POINT('',#219360);
#41037=VERTEX_POINT('',#219398);
#41038=VERTEX_POINT('',#219400);
#41039=VERTEX_POINT('',#219402);
#41040=VERTEX_POINT('',#219404);
#41041=VERTEX_POINT('',#219445);
#41042=VERTEX_POINT('',#219447);
#41043=VERTEX_POINT('',#219485);
#41044=VERTEX_POINT('',#219487);
#41045=VERTEX_POINT('',#219489);
#41046=VERTEX_POINT('',#219491);
#41047=VERTEX_POINT('',#219532);
#41048=VERTEX_POINT('',#219534);
#41049=VERTEX_POINT('',#219572);
#41050=VERTEX_POINT('',#219574);
#41051=VERTEX_POINT('',#219576);
#41052=VERTEX_POINT('',#219578);
#41053=VERTEX_POINT('',#219619);
#41054=VERTEX_POINT('',#219621);
#41055=VERTEX_POINT('',#219659);
#41056=VERTEX_POINT('',#219661);
#41057=VERTEX_POINT('',#219663);
#41058=VERTEX_POINT('',#219665);
#41059=VERTEX_POINT('',#219706);
#41060=VERTEX_POINT('',#219708);
#41061=VERTEX_POINT('',#219746);
#41062=VERTEX_POINT('',#219748);
#41063=VERTEX_POINT('',#219750);
#41064=VERTEX_POINT('',#219752);
#41065=VERTEX_POINT('',#219793);
#41066=VERTEX_POINT('',#219795);
#41067=VERTEX_POINT('',#219833);
#41068=VERTEX_POINT('',#219835);
#41069=VERTEX_POINT('',#219837);
#41070=VERTEX_POINT('',#219839);
#41071=VERTEX_POINT('',#219880);
#41072=VERTEX_POINT('',#219882);
#41073=VERTEX_POINT('',#219920);
#41074=VERTEX_POINT('',#219922);
#41075=VERTEX_POINT('',#219924);
#41076=VERTEX_POINT('',#219926);
#41077=VERTEX_POINT('',#219967);
#41078=VERTEX_POINT('',#219969);
#41079=VERTEX_POINT('',#220007);
#41080=VERTEX_POINT('',#220009);
#41081=VERTEX_POINT('',#220011);
#41082=VERTEX_POINT('',#220053);
#41083=VERTEX_POINT('',#220091);
#41084=VERTEX_POINT('',#220093);
#41085=VERTEX_POINT('',#220095);
#41086=VERTEX_POINT('',#220097);
#41087=VERTEX_POINT('',#220138);
#41088=VERTEX_POINT('',#220140);
#41089=VERTEX_POINT('',#220178);
#41090=VERTEX_POINT('',#220180);
#41091=VERTEX_POINT('',#220182);
#41092=VERTEX_POINT('',#220184);
#41093=VERTEX_POINT('',#220225);
#41094=VERTEX_POINT('',#220227);
#41095=VERTEX_POINT('',#220265);
#41096=VERTEX_POINT('',#220267);
#41097=VERTEX_POINT('',#220269);
#41098=VERTEX_POINT('',#220271);
#41099=VERTEX_POINT('',#220312);
#41100=VERTEX_POINT('',#220314);
#41101=VERTEX_POINT('',#220352);
#41102=VERTEX_POINT('',#220354);
#41103=VERTEX_POINT('',#220356);
#41104=VERTEX_POINT('',#220358);
#41105=VERTEX_POINT('',#220399);
#41106=VERTEX_POINT('',#220401);
#41107=VERTEX_POINT('',#220439);
#41108=VERTEX_POINT('',#220441);
#41109=VERTEX_POINT('',#220443);
#41110=VERTEX_POINT('',#220445);
#41111=VERTEX_POINT('',#220486);
#41112=VERTEX_POINT('',#220488);
#41113=VERTEX_POINT('',#220526);
#41114=VERTEX_POINT('',#220528);
#41115=VERTEX_POINT('',#220530);
#41116=VERTEX_POINT('',#220532);
#41117=VERTEX_POINT('',#220573);
#41118=VERTEX_POINT('',#220575);
#41119=VERTEX_POINT('',#220613);
#41120=VERTEX_POINT('',#220615);
#41121=VERTEX_POINT('',#220617);
#41122=VERTEX_POINT('',#220619);
#41123=VERTEX_POINT('',#220660);
#41124=VERTEX_POINT('',#220662);
#41125=VERTEX_POINT('',#220700);
#41126=VERTEX_POINT('',#220702);
#41127=VERTEX_POINT('',#220704);
#41128=VERTEX_POINT('',#220706);
#41129=VERTEX_POINT('',#220747);
#41130=VERTEX_POINT('',#220749);
#41131=VERTEX_POINT('',#220787);
#41132=VERTEX_POINT('',#220789);
#41133=VERTEX_POINT('',#220791);
#41134=VERTEX_POINT('',#220793);
#41135=VERTEX_POINT('',#220834);
#41136=VERTEX_POINT('',#220836);
#41137=VERTEX_POINT('',#220874);
#41138=VERTEX_POINT('',#220876);
#41139=VERTEX_POINT('',#220878);
#41140=VERTEX_POINT('',#220880);
#41141=VERTEX_POINT('',#220921);
#41142=VERTEX_POINT('',#220923);
#41143=VERTEX_POINT('',#220961);
#41144=VERTEX_POINT('',#220963);
#41145=VERTEX_POINT('',#220965);
#41146=VERTEX_POINT('',#220967);
#41147=VERTEX_POINT('',#221008);
#41148=VERTEX_POINT('',#221010);
#41149=VERTEX_POINT('',#221048);
#41150=VERTEX_POINT('',#221050);
#41151=VERTEX_POINT('',#221052);
#41152=VERTEX_POINT('',#221054);
#41153=VERTEX_POINT('',#221095);
#41154=VERTEX_POINT('',#221097);
#41155=VERTEX_POINT('',#221135);
#41156=VERTEX_POINT('',#221137);
#41157=VERTEX_POINT('',#221139);
#41158=VERTEX_POINT('',#221141);
#41159=VERTEX_POINT('',#221182);
#41160=VERTEX_POINT('',#221184);
#41161=VERTEX_POINT('',#221222);
#41162=VERTEX_POINT('',#221224);
#41163=VERTEX_POINT('',#221226);
#41164=VERTEX_POINT('',#221228);
#41165=VERTEX_POINT('',#221269);
#41166=VERTEX_POINT('',#221271);
#41167=VERTEX_POINT('',#221309);
#41168=VERTEX_POINT('',#221311);
#41169=VERTEX_POINT('',#221313);
#41170=VERTEX_POINT('',#221356);
#41171=VERTEX_POINT('',#221357);
#41172=VERTEX_POINT('',#221362);
#41173=VERTEX_POINT('',#221366);
#41174=VERTEX_POINT('',#221367);
#41175=VERTEX_POINT('',#221369);
#41176=VERTEX_POINT('',#221371);
#41177=VERTEX_POINT('',#221373);
#41178=VERTEX_POINT('',#221375);
#41179=VERTEX_POINT('',#221379);
#41180=VERTEX_POINT('',#221380);
#41181=VERTEX_POINT('',#221385);
#41182=VERTEX_POINT('',#221386);
#41183=VERTEX_POINT('',#221388);
#41184=VERTEX_POINT('',#221390);
#41185=VERTEX_POINT('',#221394);
#41186=VERTEX_POINT('',#221395);
#41187=VERTEX_POINT('',#221397);
#41188=VERTEX_POINT('',#221399);
#41189=VERTEX_POINT('',#221401);
#41190=VERTEX_POINT('',#221403);
#41191=VERTEX_POINT('',#221407);
#41192=VERTEX_POINT('',#221408);
#41193=VERTEX_POINT('',#221425);
#41194=VERTEX_POINT('',#221426);
#41195=VERTEX_POINT('',#221428);
#41196=VERTEX_POINT('',#221430);
#41197=VERTEX_POINT('',#221432);
#41198=VERTEX_POINT('',#221434);
#41199=VERTEX_POINT('',#221438);
#41200=VERTEX_POINT('',#221440);
#41201=VERTEX_POINT('',#221444);
#41202=VERTEX_POINT('',#221445);
#41203=VERTEX_POINT('',#221447);
#41204=VERTEX_POINT('',#221449);
#41205=VERTEX_POINT('',#221453);
#41206=VERTEX_POINT('',#221454);
#41207=VERTEX_POINT('',#221456);
#41208=VERTEX_POINT('',#221458);
#41209=VERTEX_POINT('',#221460);
#41210=VERTEX_POINT('',#221462);
#41211=VERTEX_POINT('',#221466);
#41212=VERTEX_POINT('',#221468);
#41213=VERTEX_POINT('',#221484);
#41214=VERTEX_POINT('',#221485);
#41215=VERTEX_POINT('',#221487);
#41216=VERTEX_POINT('',#221489);
#41217=VERTEX_POINT('',#221491);
#41218=VERTEX_POINT('',#221493);
#41219=VERTEX_POINT('',#221497);
#41220=VERTEX_POINT('',#221499);
#41221=VERTEX_POINT('',#221503);
#41222=VERTEX_POINT('',#221504);
#41223=VERTEX_POINT('',#221506);
#41224=VERTEX_POINT('',#221508);
#41225=VERTEX_POINT('',#221512);
#41226=VERTEX_POINT('',#221513);
#41227=VERTEX_POINT('',#221515);
#41228=VERTEX_POINT('',#221517);
#41229=VERTEX_POINT('',#221519);
#41230=VERTEX_POINT('',#221521);
#41231=VERTEX_POINT('',#221525);
#41232=VERTEX_POINT('',#221527);
#41233=VERTEX_POINT('',#221543);
#41234=VERTEX_POINT('',#221544);
#41235=VERTEX_POINT('',#221546);
#41236=VERTEX_POINT('',#221548);
#41237=VERTEX_POINT('',#221550);
#41238=VERTEX_POINT('',#221552);
#41239=VERTEX_POINT('',#221556);
#41240=VERTEX_POINT('',#221558);
#41241=VERTEX_POINT('',#221562);
#41242=VERTEX_POINT('',#221563);
#41243=VERTEX_POINT('',#221565);
#41244=VERTEX_POINT('',#221567);
#41245=VERTEX_POINT('',#221571);
#41246=VERTEX_POINT('',#221572);
#41247=VERTEX_POINT('',#221574);
#41248=VERTEX_POINT('',#221576);
#41249=VERTEX_POINT('',#221578);
#41250=VERTEX_POINT('',#221580);
#41251=VERTEX_POINT('',#221584);
#41252=VERTEX_POINT('',#221586);
#41253=VERTEX_POINT('',#221602);
#41254=VERTEX_POINT('',#221603);
#41255=VERTEX_POINT('',#221605);
#41256=VERTEX_POINT('',#221607);
#41257=VERTEX_POINT('',#221609);
#41258=VERTEX_POINT('',#221611);
#41259=VERTEX_POINT('',#221615);
#41260=VERTEX_POINT('',#221617);
#41261=VERTEX_POINT('',#221621);
#41262=VERTEX_POINT('',#221622);
#41263=VERTEX_POINT('',#221624);
#41264=VERTEX_POINT('',#221626);
#41265=VERTEX_POINT('',#221630);
#41266=VERTEX_POINT('',#221631);
#41267=VERTEX_POINT('',#221633);
#41268=VERTEX_POINT('',#221635);
#41269=VERTEX_POINT('',#221637);
#41270=VERTEX_POINT('',#221639);
#41271=VERTEX_POINT('',#221643);
#41272=VERTEX_POINT('',#221645);
#41273=VERTEX_POINT('',#221661);
#41274=VERTEX_POINT('',#221662);
#41275=VERTEX_POINT('',#221664);
#41276=VERTEX_POINT('',#221666);
#41277=VERTEX_POINT('',#221668);
#41278=VERTEX_POINT('',#221670);
#41279=VERTEX_POINT('',#221674);
#41280=VERTEX_POINT('',#221676);
#41281=VERTEX_POINT('',#221680);
#41282=VERTEX_POINT('',#221681);
#41283=VERTEX_POINT('',#221683);
#41284=VERTEX_POINT('',#221685);
#41285=VERTEX_POINT('',#221689);
#41286=VERTEX_POINT('',#221690);
#41287=VERTEX_POINT('',#221692);
#41288=VERTEX_POINT('',#221694);
#41289=VERTEX_POINT('',#221696);
#41290=VERTEX_POINT('',#221698);
#41291=VERTEX_POINT('',#221702);
#41292=VERTEX_POINT('',#221704);
#41293=VERTEX_POINT('',#221720);
#41294=VERTEX_POINT('',#221721);
#41295=VERTEX_POINT('',#221723);
#41296=VERTEX_POINT('',#221725);
#41297=VERTEX_POINT('',#221727);
#41298=VERTEX_POINT('',#221729);
#41299=VERTEX_POINT('',#221733);
#41300=VERTEX_POINT('',#221735);
#41301=VERTEX_POINT('',#221739);
#41302=VERTEX_POINT('',#221740);
#41303=VERTEX_POINT('',#221742);
#41304=VERTEX_POINT('',#221744);
#41305=VERTEX_POINT('',#221748);
#41306=VERTEX_POINT('',#221749);
#41307=VERTEX_POINT('',#221751);
#41308=VERTEX_POINT('',#221753);
#41309=VERTEX_POINT('',#221755);
#41310=VERTEX_POINT('',#221757);
#41311=VERTEX_POINT('',#221761);
#41312=VERTEX_POINT('',#221763);
#41313=VERTEX_POINT('',#221779);
#41314=VERTEX_POINT('',#221780);
#41315=VERTEX_POINT('',#221782);
#41316=VERTEX_POINT('',#221784);
#41317=VERTEX_POINT('',#221786);
#41318=VERTEX_POINT('',#221788);
#41319=VERTEX_POINT('',#221792);
#41320=VERTEX_POINT('',#221794);
#41321=VERTEX_POINT('',#221798);
#41322=VERTEX_POINT('',#221799);
#41323=VERTEX_POINT('',#221801);
#41324=VERTEX_POINT('',#221803);
#41325=VERTEX_POINT('',#221807);
#41326=VERTEX_POINT('',#221808);
#41327=VERTEX_POINT('',#221810);
#41328=VERTEX_POINT('',#221812);
#41329=VERTEX_POINT('',#221814);
#41330=VERTEX_POINT('',#221816);
#41331=VERTEX_POINT('',#221820);
#41332=VERTEX_POINT('',#221822);
#41333=VERTEX_POINT('',#221838);
#41334=VERTEX_POINT('',#221839);
#41335=VERTEX_POINT('',#221841);
#41336=VERTEX_POINT('',#221843);
#41337=VERTEX_POINT('',#221845);
#41338=VERTEX_POINT('',#221847);
#41339=VERTEX_POINT('',#221851);
#41340=VERTEX_POINT('',#221853);
#41341=VERTEX_POINT('',#221857);
#41342=VERTEX_POINT('',#221858);
#41343=VERTEX_POINT('',#221860);
#41344=VERTEX_POINT('',#221862);
#41345=VERTEX_POINT('',#221866);
#41346=VERTEX_POINT('',#221867);
#41347=VERTEX_POINT('',#221869);
#41348=VERTEX_POINT('',#221871);
#41349=VERTEX_POINT('',#221873);
#41350=VERTEX_POINT('',#221875);
#41351=VERTEX_POINT('',#221879);
#41352=VERTEX_POINT('',#221881);
#41353=VERTEX_POINT('',#221897);
#41354=VERTEX_POINT('',#221898);
#41355=VERTEX_POINT('',#221900);
#41356=VERTEX_POINT('',#221902);
#41357=VERTEX_POINT('',#221904);
#41358=VERTEX_POINT('',#221906);
#41359=VERTEX_POINT('',#221910);
#41360=VERTEX_POINT('',#221912);
#41361=VERTEX_POINT('',#221916);
#41362=VERTEX_POINT('',#221917);
#41363=VERTEX_POINT('',#221919);
#41364=VERTEX_POINT('',#221921);
#41365=VERTEX_POINT('',#221925);
#41366=VERTEX_POINT('',#221926);
#41367=VERTEX_POINT('',#221928);
#41368=VERTEX_POINT('',#221930);
#41369=VERTEX_POINT('',#221932);
#41370=VERTEX_POINT('',#221934);
#41371=VERTEX_POINT('',#221938);
#41372=VERTEX_POINT('',#221940);
#41373=VERTEX_POINT('',#221956);
#41374=VERTEX_POINT('',#221957);
#41375=VERTEX_POINT('',#221959);
#41376=VERTEX_POINT('',#221961);
#41377=VERTEX_POINT('',#221963);
#41378=VERTEX_POINT('',#221965);
#41379=VERTEX_POINT('',#221969);
#41380=VERTEX_POINT('',#221971);
#41381=VERTEX_POINT('',#221975);
#41382=VERTEX_POINT('',#221976);
#41383=VERTEX_POINT('',#221978);
#41384=VERTEX_POINT('',#221980);
#41385=VERTEX_POINT('',#221984);
#41386=VERTEX_POINT('',#221985);
#41387=VERTEX_POINT('',#221987);
#41388=VERTEX_POINT('',#221989);
#41389=VERTEX_POINT('',#221991);
#41390=VERTEX_POINT('',#221993);
#41391=VERTEX_POINT('',#221997);
#41392=VERTEX_POINT('',#221999);
#41393=VERTEX_POINT('',#222015);
#41394=VERTEX_POINT('',#222016);
#41395=VERTEX_POINT('',#222018);
#41396=VERTEX_POINT('',#222020);
#41397=VERTEX_POINT('',#222022);
#41398=VERTEX_POINT('',#222024);
#41399=VERTEX_POINT('',#222028);
#41400=VERTEX_POINT('',#222030);
#41401=VERTEX_POINT('',#222034);
#41402=VERTEX_POINT('',#222035);
#41403=VERTEX_POINT('',#222037);
#41404=VERTEX_POINT('',#222039);
#41405=VERTEX_POINT('',#222043);
#41406=VERTEX_POINT('',#222044);
#41407=VERTEX_POINT('',#222046);
#41408=VERTEX_POINT('',#222048);
#41409=VERTEX_POINT('',#222050);
#41410=VERTEX_POINT('',#222052);
#41411=VERTEX_POINT('',#222056);
#41412=VERTEX_POINT('',#222058);
#41413=VERTEX_POINT('',#222074);
#41414=VERTEX_POINT('',#222075);
#41415=VERTEX_POINT('',#222077);
#41416=VERTEX_POINT('',#222079);
#41417=VERTEX_POINT('',#222081);
#41418=VERTEX_POINT('',#222083);
#41419=VERTEX_POINT('',#222087);
#41420=VERTEX_POINT('',#222089);
#41421=VERTEX_POINT('',#222093);
#41422=VERTEX_POINT('',#222094);
#41423=VERTEX_POINT('',#222096);
#41424=VERTEX_POINT('',#222098);
#41425=VERTEX_POINT('',#222102);
#41426=VERTEX_POINT('',#222103);
#41427=VERTEX_POINT('',#222105);
#41428=VERTEX_POINT('',#222107);
#41429=VERTEX_POINT('',#222109);
#41430=VERTEX_POINT('',#222111);
#41431=VERTEX_POINT('',#222115);
#41432=VERTEX_POINT('',#222117);
#41433=VERTEX_POINT('',#222133);
#41434=VERTEX_POINT('',#222134);
#41435=VERTEX_POINT('',#222136);
#41436=VERTEX_POINT('',#222138);
#41437=VERTEX_POINT('',#222140);
#41438=VERTEX_POINT('',#222142);
#41439=VERTEX_POINT('',#222146);
#41440=VERTEX_POINT('',#222148);
#41441=VERTEX_POINT('',#222152);
#41442=VERTEX_POINT('',#222153);
#41443=VERTEX_POINT('',#222155);
#41444=VERTEX_POINT('',#222157);
#41445=VERTEX_POINT('',#222161);
#41446=VERTEX_POINT('',#222162);
#41447=VERTEX_POINT('',#222164);
#41448=VERTEX_POINT('',#222166);
#41449=VERTEX_POINT('',#222168);
#41450=VERTEX_POINT('',#222170);
#41451=VERTEX_POINT('',#222174);
#41452=VERTEX_POINT('',#222176);
#41453=VERTEX_POINT('',#222192);
#41454=VERTEX_POINT('',#222193);
#41455=VERTEX_POINT('',#222195);
#41456=VERTEX_POINT('',#222197);
#41457=VERTEX_POINT('',#222199);
#41458=VERTEX_POINT('',#222201);
#41459=VERTEX_POINT('',#222205);
#41460=VERTEX_POINT('',#222207);
#41461=VERTEX_POINT('',#222211);
#41462=VERTEX_POINT('',#222212);
#41463=VERTEX_POINT('',#222214);
#41464=VERTEX_POINT('',#222216);
#41465=VERTEX_POINT('',#222220);
#41466=VERTEX_POINT('',#222221);
#41467=VERTEX_POINT('',#222223);
#41468=VERTEX_POINT('',#222225);
#41469=VERTEX_POINT('',#222227);
#41470=VERTEX_POINT('',#222229);
#41471=VERTEX_POINT('',#222233);
#41472=VERTEX_POINT('',#222235);
#41473=VERTEX_POINT('',#222251);
#41474=VERTEX_POINT('',#222252);
#41475=VERTEX_POINT('',#222254);
#41476=VERTEX_POINT('',#222256);
#41477=VERTEX_POINT('',#222258);
#41478=VERTEX_POINT('',#222260);
#41479=VERTEX_POINT('',#222264);
#41480=VERTEX_POINT('',#222266);
#41481=VERTEX_POINT('',#222270);
#41482=VERTEX_POINT('',#222271);
#41483=VERTEX_POINT('',#222273);
#41484=VERTEX_POINT('',#222275);
#41485=VERTEX_POINT('',#222279);
#41486=VERTEX_POINT('',#222280);
#41487=VERTEX_POINT('',#222282);
#41488=VERTEX_POINT('',#222284);
#41489=VERTEX_POINT('',#222286);
#41490=VERTEX_POINT('',#222288);
#41491=VERTEX_POINT('',#222292);
#41492=VERTEX_POINT('',#222294);
#41493=VERTEX_POINT('',#222310);
#41494=VERTEX_POINT('',#222311);
#41495=VERTEX_POINT('',#222313);
#41496=VERTEX_POINT('',#222315);
#41497=VERTEX_POINT('',#222317);
#41498=VERTEX_POINT('',#222319);
#41499=VERTEX_POINT('',#222323);
#41500=VERTEX_POINT('',#222325);
#41501=VERTEX_POINT('',#222329);
#41502=VERTEX_POINT('',#222330);
#41503=VERTEX_POINT('',#222332);
#41504=VERTEX_POINT('',#222334);
#41505=VERTEX_POINT('',#222338);
#41506=VERTEX_POINT('',#222339);
#41507=VERTEX_POINT('',#222341);
#41508=VERTEX_POINT('',#222343);
#41509=VERTEX_POINT('',#222345);
#41510=VERTEX_POINT('',#222347);
#41511=VERTEX_POINT('',#222351);
#41512=VERTEX_POINT('',#222353);
#41513=VERTEX_POINT('',#222369);
#41514=VERTEX_POINT('',#222370);
#41515=VERTEX_POINT('',#222372);
#41516=VERTEX_POINT('',#222374);
#41517=VERTEX_POINT('',#222376);
#41518=VERTEX_POINT('',#222378);
#41519=VERTEX_POINT('',#222382);
#41520=VERTEX_POINT('',#222384);
#41521=VERTEX_POINT('',#222388);
#41522=VERTEX_POINT('',#222389);
#41523=VERTEX_POINT('',#222391);
#41524=VERTEX_POINT('',#222393);
#41525=VERTEX_POINT('',#222397);
#41526=VERTEX_POINT('',#222398);
#41527=VERTEX_POINT('',#222400);
#41528=VERTEX_POINT('',#222402);
#41529=VERTEX_POINT('',#222404);
#41530=VERTEX_POINT('',#222406);
#41531=VERTEX_POINT('',#222410);
#41532=VERTEX_POINT('',#222412);
#41533=VERTEX_POINT('',#222428);
#41534=VERTEX_POINT('',#222429);
#41535=VERTEX_POINT('',#222431);
#41536=VERTEX_POINT('',#222433);
#41537=VERTEX_POINT('',#222435);
#41538=VERTEX_POINT('',#222437);
#41539=VERTEX_POINT('',#222441);
#41540=VERTEX_POINT('',#222443);
#41541=VERTEX_POINT('',#222447);
#41542=VERTEX_POINT('',#222448);
#41543=VERTEX_POINT('',#222450);
#41544=VERTEX_POINT('',#222452);
#41545=VERTEX_POINT('',#222456);
#41546=VERTEX_POINT('',#222457);
#41547=VERTEX_POINT('',#222459);
#41548=VERTEX_POINT('',#222461);
#41549=VERTEX_POINT('',#222463);
#41550=VERTEX_POINT('',#222465);
#41551=VERTEX_POINT('',#222469);
#41552=VERTEX_POINT('',#222471);
#41553=VERTEX_POINT('',#222487);
#41554=VERTEX_POINT('',#222488);
#41555=VERTEX_POINT('',#222490);
#41556=VERTEX_POINT('',#222492);
#41557=VERTEX_POINT('',#222494);
#41558=VERTEX_POINT('',#222496);
#41559=VERTEX_POINT('',#222500);
#41560=VERTEX_POINT('',#222502);
#41561=VERTEX_POINT('',#222506);
#41562=VERTEX_POINT('',#222507);
#41563=VERTEX_POINT('',#222509);
#41564=VERTEX_POINT('',#222511);
#41565=VERTEX_POINT('',#222515);
#41566=VERTEX_POINT('',#222516);
#41567=VERTEX_POINT('',#222518);
#41568=VERTEX_POINT('',#222520);
#41569=VERTEX_POINT('',#222522);
#41570=VERTEX_POINT('',#222524);
#41571=VERTEX_POINT('',#222528);
#41572=VERTEX_POINT('',#222530);
#41573=VERTEX_POINT('',#222546);
#41574=VERTEX_POINT('',#222547);
#41575=VERTEX_POINT('',#222549);
#41576=VERTEX_POINT('',#222551);
#41577=VERTEX_POINT('',#222553);
#41578=VERTEX_POINT('',#222555);
#41579=VERTEX_POINT('',#222559);
#41580=VERTEX_POINT('',#222561);
#41581=VERTEX_POINT('',#222565);
#41582=VERTEX_POINT('',#222566);
#41583=VERTEX_POINT('',#222568);
#41584=VERTEX_POINT('',#222570);
#41585=VERTEX_POINT('',#222574);
#41586=VERTEX_POINT('',#222575);
#41587=VERTEX_POINT('',#222577);
#41588=VERTEX_POINT('',#222579);
#41589=VERTEX_POINT('',#222581);
#41590=VERTEX_POINT('',#222583);
#41591=VERTEX_POINT('',#222587);
#41592=VERTEX_POINT('',#222589);
#41593=VERTEX_POINT('',#222605);
#41594=VERTEX_POINT('',#222606);
#41595=VERTEX_POINT('',#222608);
#41596=VERTEX_POINT('',#222610);
#41597=VERTEX_POINT('',#222612);
#41598=VERTEX_POINT('',#222614);
#41599=VERTEX_POINT('',#222618);
#41600=VERTEX_POINT('',#222620);
#41601=VERTEX_POINT('',#222624);
#41602=VERTEX_POINT('',#222625);
#41603=VERTEX_POINT('',#222627);
#41604=VERTEX_POINT('',#222629);
#41605=VERTEX_POINT('',#222633);
#41606=VERTEX_POINT('',#222634);
#41607=VERTEX_POINT('',#222636);
#41608=VERTEX_POINT('',#222638);
#41609=VERTEX_POINT('',#222640);
#41610=VERTEX_POINT('',#222642);
#41611=VERTEX_POINT('',#222646);
#41612=VERTEX_POINT('',#222648);
#41613=VERTEX_POINT('',#222664);
#41614=VERTEX_POINT('',#222665);
#41615=VERTEX_POINT('',#222667);
#41616=VERTEX_POINT('',#222669);
#41617=VERTEX_POINT('',#222671);
#41618=VERTEX_POINT('',#222673);
#41619=VERTEX_POINT('',#222677);
#41620=VERTEX_POINT('',#222679);
#41621=VERTEX_POINT('',#222683);
#41622=VERTEX_POINT('',#222684);
#41623=VERTEX_POINT('',#222686);
#41624=VERTEX_POINT('',#222688);
#41625=VERTEX_POINT('',#222692);
#41626=VERTEX_POINT('',#222693);
#41627=VERTEX_POINT('',#222695);
#41628=VERTEX_POINT('',#222697);
#41629=VERTEX_POINT('',#222699);
#41630=VERTEX_POINT('',#222701);
#41631=VERTEX_POINT('',#222705);
#41632=VERTEX_POINT('',#222707);
#41633=VERTEX_POINT('',#222723);
#41634=VERTEX_POINT('',#222724);
#41635=VERTEX_POINT('',#222726);
#41636=VERTEX_POINT('',#222728);
#41637=VERTEX_POINT('',#222730);
#41638=VERTEX_POINT('',#222732);
#41639=VERTEX_POINT('',#222736);
#41640=VERTEX_POINT('',#222738);
#41641=VERTEX_POINT('',#222742);
#41642=VERTEX_POINT('',#222743);
#41643=VERTEX_POINT('',#222745);
#41644=VERTEX_POINT('',#222747);
#41645=VERTEX_POINT('',#222751);
#41646=VERTEX_POINT('',#222752);
#41647=VERTEX_POINT('',#222754);
#41648=VERTEX_POINT('',#222756);
#41649=VERTEX_POINT('',#222758);
#41650=VERTEX_POINT('',#222760);
#41651=VERTEX_POINT('',#222764);
#41652=VERTEX_POINT('',#222766);
#41653=VERTEX_POINT('',#222782);
#41654=VERTEX_POINT('',#222783);
#41655=VERTEX_POINT('',#222785);
#41656=VERTEX_POINT('',#222787);
#41657=VERTEX_POINT('',#222789);
#41658=VERTEX_POINT('',#222791);
#41659=VERTEX_POINT('',#222795);
#41660=VERTEX_POINT('',#222797);
#41661=VERTEX_POINT('',#222801);
#41662=VERTEX_POINT('',#222802);
#41663=VERTEX_POINT('',#222804);
#41664=VERTEX_POINT('',#222806);
#41665=VERTEX_POINT('',#222810);
#41666=VERTEX_POINT('',#222811);
#41667=VERTEX_POINT('',#222813);
#41668=VERTEX_POINT('',#222815);
#41669=VERTEX_POINT('',#222817);
#41670=VERTEX_POINT('',#222819);
#41671=VERTEX_POINT('',#222823);
#41672=VERTEX_POINT('',#222825);
#41673=VERTEX_POINT('',#222841);
#41674=VERTEX_POINT('',#222842);
#41675=VERTEX_POINT('',#222844);
#41676=VERTEX_POINT('',#222846);
#41677=VERTEX_POINT('',#222848);
#41678=VERTEX_POINT('',#222850);
#41679=VERTEX_POINT('',#222854);
#41680=VERTEX_POINT('',#222856);
#41681=VERTEX_POINT('',#222860);
#41682=VERTEX_POINT('',#222861);
#41683=VERTEX_POINT('',#222863);
#41684=VERTEX_POINT('',#222865);
#41685=VERTEX_POINT('',#222869);
#41686=VERTEX_POINT('',#222870);
#41687=VERTEX_POINT('',#222872);
#41688=VERTEX_POINT('',#222874);
#41689=VERTEX_POINT('',#222876);
#41690=VERTEX_POINT('',#222878);
#41691=VERTEX_POINT('',#222882);
#41692=VERTEX_POINT('',#222884);
#41693=VERTEX_POINT('',#222900);
#41694=VERTEX_POINT('',#222901);
#41695=VERTEX_POINT('',#222903);
#41696=VERTEX_POINT('',#222905);
#41697=VERTEX_POINT('',#222907);
#41698=VERTEX_POINT('',#222909);
#41699=VERTEX_POINT('',#222913);
#41700=VERTEX_POINT('',#222915);
#41701=VERTEX_POINT('',#222919);
#41702=VERTEX_POINT('',#222920);
#41703=VERTEX_POINT('',#222922);
#41704=VERTEX_POINT('',#222924);
#41705=VERTEX_POINT('',#222928);
#41706=VERTEX_POINT('',#222929);
#41707=VERTEX_POINT('',#222931);
#41708=VERTEX_POINT('',#222933);
#41709=VERTEX_POINT('',#222935);
#41710=VERTEX_POINT('',#222937);
#41711=VERTEX_POINT('',#222941);
#41712=VERTEX_POINT('',#222943);
#41713=VERTEX_POINT('',#222959);
#41714=VERTEX_POINT('',#222960);
#41715=VERTEX_POINT('',#222962);
#41716=VERTEX_POINT('',#222964);
#41717=VERTEX_POINT('',#222966);
#41718=VERTEX_POINT('',#222968);
#41719=VERTEX_POINT('',#222972);
#41720=VERTEX_POINT('',#222974);
#41721=VERTEX_POINT('',#222978);
#41722=VERTEX_POINT('',#222979);
#41723=VERTEX_POINT('',#222981);
#41724=VERTEX_POINT('',#222983);
#41725=VERTEX_POINT('',#222987);
#41726=VERTEX_POINT('',#222988);
#41727=VERTEX_POINT('',#222990);
#41728=VERTEX_POINT('',#222992);
#41729=VERTEX_POINT('',#222994);
#41730=VERTEX_POINT('',#222996);
#41731=VERTEX_POINT('',#223000);
#41732=VERTEX_POINT('',#223002);
#41733=VERTEX_POINT('',#223018);
#41734=VERTEX_POINT('',#223019);
#41735=VERTEX_POINT('',#223021);
#41736=VERTEX_POINT('',#223023);
#41737=VERTEX_POINT('',#223025);
#41738=VERTEX_POINT('',#223027);
#41739=VERTEX_POINT('',#223031);
#41740=VERTEX_POINT('',#223033);
#41741=VERTEX_POINT('',#223037);
#41742=VERTEX_POINT('',#223038);
#41743=VERTEX_POINT('',#223040);
#41744=VERTEX_POINT('',#223042);
#41745=VERTEX_POINT('',#223046);
#41746=VERTEX_POINT('',#223047);
#41747=VERTEX_POINT('',#223049);
#41748=VERTEX_POINT('',#223051);
#41749=VERTEX_POINT('',#223053);
#41750=VERTEX_POINT('',#223055);
#41751=VERTEX_POINT('',#223059);
#41752=VERTEX_POINT('',#223061);
#41753=VERTEX_POINT('',#223077);
#41754=VERTEX_POINT('',#223078);
#41755=VERTEX_POINT('',#223080);
#41756=VERTEX_POINT('',#223082);
#41757=VERTEX_POINT('',#223084);
#41758=VERTEX_POINT('',#223086);
#41759=VERTEX_POINT('',#223090);
#41760=VERTEX_POINT('',#223092);
#41761=VERTEX_POINT('',#223096);
#41762=VERTEX_POINT('',#223097);
#41763=VERTEX_POINT('',#223099);
#41764=VERTEX_POINT('',#223101);
#41765=VERTEX_POINT('',#223105);
#41766=VERTEX_POINT('',#223106);
#41767=VERTEX_POINT('',#223108);
#41768=VERTEX_POINT('',#223110);
#41769=VERTEX_POINT('',#223112);
#41770=VERTEX_POINT('',#223114);
#41771=VERTEX_POINT('',#223118);
#41772=VERTEX_POINT('',#223120);
#41773=VERTEX_POINT('',#223136);
#41774=VERTEX_POINT('',#223137);
#41775=VERTEX_POINT('',#223139);
#41776=VERTEX_POINT('',#223141);
#41777=VERTEX_POINT('',#223143);
#41778=VERTEX_POINT('',#223145);
#41779=VERTEX_POINT('',#223149);
#41780=VERTEX_POINT('',#223151);
#41781=VERTEX_POINT('',#223155);
#41782=VERTEX_POINT('',#223156);
#41783=VERTEX_POINT('',#223158);
#41784=VERTEX_POINT('',#223160);
#41785=VERTEX_POINT('',#223164);
#41786=VERTEX_POINT('',#223165);
#41787=VERTEX_POINT('',#223167);
#41788=VERTEX_POINT('',#223169);
#41789=VERTEX_POINT('',#223171);
#41790=VERTEX_POINT('',#223173);
#41791=VERTEX_POINT('',#223177);
#41792=VERTEX_POINT('',#223179);
#41793=VERTEX_POINT('',#223195);
#41794=VERTEX_POINT('',#223196);
#41795=VERTEX_POINT('',#223198);
#41796=VERTEX_POINT('',#223200);
#41797=VERTEX_POINT('',#223202);
#41798=VERTEX_POINT('',#223204);
#41799=VERTEX_POINT('',#223208);
#41800=VERTEX_POINT('',#223210);
#41801=VERTEX_POINT('',#223214);
#41802=VERTEX_POINT('',#223215);
#41803=VERTEX_POINT('',#223217);
#41804=VERTEX_POINT('',#223219);
#41805=VERTEX_POINT('',#223223);
#41806=VERTEX_POINT('',#223224);
#41807=VERTEX_POINT('',#223226);
#41808=VERTEX_POINT('',#223228);
#41809=VERTEX_POINT('',#223230);
#41810=VERTEX_POINT('',#223232);
#41811=VERTEX_POINT('',#223236);
#41812=VERTEX_POINT('',#223238);
#41813=VERTEX_POINT('',#223254);
#41814=VERTEX_POINT('',#223255);
#41815=VERTEX_POINT('',#223257);
#41816=VERTEX_POINT('',#223259);
#41817=VERTEX_POINT('',#223261);
#41818=VERTEX_POINT('',#223263);
#41819=VERTEX_POINT('',#223267);
#41820=VERTEX_POINT('',#223269);
#41821=VERTEX_POINT('',#223273);
#41822=VERTEX_POINT('',#223274);
#41823=VERTEX_POINT('',#223276);
#41824=VERTEX_POINT('',#223278);
#41825=VERTEX_POINT('',#223282);
#41826=VERTEX_POINT('',#223283);
#41827=VERTEX_POINT('',#223285);
#41828=VERTEX_POINT('',#223287);
#41829=VERTEX_POINT('',#223289);
#41830=VERTEX_POINT('',#223291);
#41831=VERTEX_POINT('',#223295);
#41832=VERTEX_POINT('',#223297);
#41833=VERTEX_POINT('',#223313);
#41834=VERTEX_POINT('',#223314);
#41835=VERTEX_POINT('',#223316);
#41836=VERTEX_POINT('',#223318);
#41837=VERTEX_POINT('',#223320);
#41838=VERTEX_POINT('',#223322);
#41839=VERTEX_POINT('',#223326);
#41840=VERTEX_POINT('',#223328);
#41841=VERTEX_POINT('',#223332);
#41842=VERTEX_POINT('',#223333);
#41843=VERTEX_POINT('',#223335);
#41844=VERTEX_POINT('',#223337);
#41845=VERTEX_POINT('',#223341);
#41846=VERTEX_POINT('',#223342);
#41847=VERTEX_POINT('',#223344);
#41848=VERTEX_POINT('',#223346);
#41849=VERTEX_POINT('',#223348);
#41850=VERTEX_POINT('',#223350);
#41851=VERTEX_POINT('',#223354);
#41852=VERTEX_POINT('',#223356);
#41853=VERTEX_POINT('',#223372);
#41854=VERTEX_POINT('',#223373);
#41855=VERTEX_POINT('',#223375);
#41856=VERTEX_POINT('',#223377);
#41857=VERTEX_POINT('',#223379);
#41858=VERTEX_POINT('',#223381);
#41859=VERTEX_POINT('',#223385);
#41860=VERTEX_POINT('',#223387);
#41861=VERTEX_POINT('',#223391);
#41862=VERTEX_POINT('',#223392);
#41863=VERTEX_POINT('',#223394);
#41864=VERTEX_POINT('',#223396);
#41865=VERTEX_POINT('',#223400);
#41866=VERTEX_POINT('',#223401);
#41867=VERTEX_POINT('',#223403);
#41868=VERTEX_POINT('',#223405);
#41869=VERTEX_POINT('',#223407);
#41870=VERTEX_POINT('',#223409);
#41871=VERTEX_POINT('',#223413);
#41872=VERTEX_POINT('',#223415);
#41873=VERTEX_POINT('',#223431);
#41874=VERTEX_POINT('',#223432);
#41875=VERTEX_POINT('',#223434);
#41876=VERTEX_POINT('',#223436);
#41877=VERTEX_POINT('',#223438);
#41878=VERTEX_POINT('',#223440);
#41879=VERTEX_POINT('',#223444);
#41880=VERTEX_POINT('',#223446);
#41881=VERTEX_POINT('',#223450);
#41882=VERTEX_POINT('',#223451);
#41883=VERTEX_POINT('',#223453);
#41884=VERTEX_POINT('',#223455);
#41885=VERTEX_POINT('',#223459);
#41886=VERTEX_POINT('',#223460);
#41887=VERTEX_POINT('',#223462);
#41888=VERTEX_POINT('',#223464);
#41889=VERTEX_POINT('',#223466);
#41890=VERTEX_POINT('',#223468);
#41891=VERTEX_POINT('',#223472);
#41892=VERTEX_POINT('',#223474);
#41893=VERTEX_POINT('',#223490);
#41894=VERTEX_POINT('',#223491);
#41895=VERTEX_POINT('',#223493);
#41896=VERTEX_POINT('',#223495);
#41897=VERTEX_POINT('',#223497);
#41898=VERTEX_POINT('',#223499);
#41899=VERTEX_POINT('',#223503);
#41900=VERTEX_POINT('',#223505);
#41901=VERTEX_POINT('',#223509);
#41902=VERTEX_POINT('',#223510);
#41903=VERTEX_POINT('',#223512);
#41904=VERTEX_POINT('',#223514);
#41905=VERTEX_POINT('',#223518);
#41906=VERTEX_POINT('',#223519);
#41907=VERTEX_POINT('',#223521);
#41908=VERTEX_POINT('',#223523);
#41909=VERTEX_POINT('',#223525);
#41910=VERTEX_POINT('',#223527);
#41911=VERTEX_POINT('',#223531);
#41912=VERTEX_POINT('',#223533);
#41913=VERTEX_POINT('',#223549);
#41914=VERTEX_POINT('',#223550);
#41915=VERTEX_POINT('',#223552);
#41916=VERTEX_POINT('',#223554);
#41917=VERTEX_POINT('',#223556);
#41918=VERTEX_POINT('',#223558);
#41919=VERTEX_POINT('',#223562);
#41920=VERTEX_POINT('',#223564);
#41921=VERTEX_POINT('',#223568);
#41922=VERTEX_POINT('',#223569);
#41923=VERTEX_POINT('',#223571);
#41924=VERTEX_POINT('',#223573);
#41925=VERTEX_POINT('',#223577);
#41926=VERTEX_POINT('',#223578);
#41927=VERTEX_POINT('',#223580);
#41928=VERTEX_POINT('',#223582);
#41929=VERTEX_POINT('',#223584);
#41930=VERTEX_POINT('',#223586);
#41931=VERTEX_POINT('',#223590);
#41932=VERTEX_POINT('',#223592);
#41933=VERTEX_POINT('',#223608);
#41934=VERTEX_POINT('',#223609);
#41935=VERTEX_POINT('',#223611);
#41936=VERTEX_POINT('',#223613);
#41937=VERTEX_POINT('',#223615);
#41938=VERTEX_POINT('',#223617);
#41939=VERTEX_POINT('',#223621);
#41940=VERTEX_POINT('',#223623);
#41941=VERTEX_POINT('',#223627);
#41942=VERTEX_POINT('',#223628);
#41943=VERTEX_POINT('',#223630);
#41944=VERTEX_POINT('',#223632);
#41945=VERTEX_POINT('',#223636);
#41946=VERTEX_POINT('',#223637);
#41947=VERTEX_POINT('',#223639);
#41948=VERTEX_POINT('',#223641);
#41949=VERTEX_POINT('',#223643);
#41950=VERTEX_POINT('',#223645);
#41951=VERTEX_POINT('',#223649);
#41952=VERTEX_POINT('',#223651);
#41953=VERTEX_POINT('',#223667);
#41954=VERTEX_POINT('',#223668);
#41955=VERTEX_POINT('',#223670);
#41956=VERTEX_POINT('',#223672);
#41957=VERTEX_POINT('',#223674);
#41958=VERTEX_POINT('',#223676);
#41959=VERTEX_POINT('',#223680);
#41960=VERTEX_POINT('',#223682);
#41961=VERTEX_POINT('',#223686);
#41962=VERTEX_POINT('',#223687);
#41963=VERTEX_POINT('',#223689);
#41964=VERTEX_POINT('',#223691);
#41965=VERTEX_POINT('',#223695);
#41966=VERTEX_POINT('',#223696);
#41967=VERTEX_POINT('',#223698);
#41968=VERTEX_POINT('',#223700);
#41969=VERTEX_POINT('',#223702);
#41970=VERTEX_POINT('',#223704);
#41971=VERTEX_POINT('',#223708);
#41972=VERTEX_POINT('',#223710);
#41973=VERTEX_POINT('',#223726);
#41974=VERTEX_POINT('',#223727);
#41975=VERTEX_POINT('',#223729);
#41976=VERTEX_POINT('',#223731);
#41977=VERTEX_POINT('',#223733);
#41978=VERTEX_POINT('',#223735);
#41979=VERTEX_POINT('',#223739);
#41980=VERTEX_POINT('',#223741);
#41981=VERTEX_POINT('',#223745);
#41982=VERTEX_POINT('',#223746);
#41983=VERTEX_POINT('',#223748);
#41984=VERTEX_POINT('',#223750);
#41985=VERTEX_POINT('',#223754);
#41986=VERTEX_POINT('',#223755);
#41987=VERTEX_POINT('',#223757);
#41988=VERTEX_POINT('',#223759);
#41989=VERTEX_POINT('',#223761);
#41990=VERTEX_POINT('',#223763);
#41991=VERTEX_POINT('',#223767);
#41992=VERTEX_POINT('',#223769);
#41993=VERTEX_POINT('',#223785);
#41994=VERTEX_POINT('',#223786);
#41995=VERTEX_POINT('',#223788);
#41996=VERTEX_POINT('',#223790);
#41997=VERTEX_POINT('',#223792);
#41998=VERTEX_POINT('',#223794);
#41999=VERTEX_POINT('',#223798);
#42000=VERTEX_POINT('',#223800);
#42001=VERTEX_POINT('',#223804);
#42002=VERTEX_POINT('',#223805);
#42003=VERTEX_POINT('',#223807);
#42004=VERTEX_POINT('',#223809);
#42005=VERTEX_POINT('',#223813);
#42006=VERTEX_POINT('',#223814);
#42007=VERTEX_POINT('',#223816);
#42008=VERTEX_POINT('',#223818);
#42009=VERTEX_POINT('',#223820);
#42010=VERTEX_POINT('',#223822);
#42011=VERTEX_POINT('',#223826);
#42012=VERTEX_POINT('',#223828);
#42013=VERTEX_POINT('',#223844);
#42014=VERTEX_POINT('',#223845);
#42015=VERTEX_POINT('',#223847);
#42016=VERTEX_POINT('',#223849);
#42017=VERTEX_POINT('',#223851);
#42018=VERTEX_POINT('',#223853);
#42019=VERTEX_POINT('',#223857);
#42020=VERTEX_POINT('',#223859);
#42021=VERTEX_POINT('',#223863);
#42022=VERTEX_POINT('',#223864);
#42023=VERTEX_POINT('',#223866);
#42024=VERTEX_POINT('',#223868);
#42025=VERTEX_POINT('',#223872);
#42026=VERTEX_POINT('',#223873);
#42027=VERTEX_POINT('',#223875);
#42028=VERTEX_POINT('',#223877);
#42029=VERTEX_POINT('',#223879);
#42030=VERTEX_POINT('',#223881);
#42031=VERTEX_POINT('',#223885);
#42032=VERTEX_POINT('',#223887);
#42033=VERTEX_POINT('',#223903);
#42034=VERTEX_POINT('',#223904);
#42035=VERTEX_POINT('',#223906);
#42036=VERTEX_POINT('',#223908);
#42037=VERTEX_POINT('',#223910);
#42038=VERTEX_POINT('',#223912);
#42039=VERTEX_POINT('',#223916);
#42040=VERTEX_POINT('',#223918);
#42041=VERTEX_POINT('',#223922);
#42042=VERTEX_POINT('',#223923);
#42043=VERTEX_POINT('',#223925);
#42044=VERTEX_POINT('',#223927);
#42045=VERTEX_POINT('',#223931);
#42046=VERTEX_POINT('',#223932);
#42047=VERTEX_POINT('',#223934);
#42048=VERTEX_POINT('',#223936);
#42049=VERTEX_POINT('',#223938);
#42050=VERTEX_POINT('',#223940);
#42051=VERTEX_POINT('',#223944);
#42052=VERTEX_POINT('',#223946);
#42053=VERTEX_POINT('',#223962);
#42054=VERTEX_POINT('',#223963);
#42055=VERTEX_POINT('',#223965);
#42056=VERTEX_POINT('',#223967);
#42057=VERTEX_POINT('',#223969);
#42058=VERTEX_POINT('',#223971);
#42059=VERTEX_POINT('',#223975);
#42060=VERTEX_POINT('',#223977);
#42061=VERTEX_POINT('',#223981);
#42062=VERTEX_POINT('',#223982);
#42063=VERTEX_POINT('',#223984);
#42064=VERTEX_POINT('',#223986);
#42065=VERTEX_POINT('',#223990);
#42066=VERTEX_POINT('',#223991);
#42067=VERTEX_POINT('',#223993);
#42068=VERTEX_POINT('',#223995);
#42069=VERTEX_POINT('',#223997);
#42070=VERTEX_POINT('',#223999);
#42071=VERTEX_POINT('',#224003);
#42072=VERTEX_POINT('',#224005);
#42073=VERTEX_POINT('',#224021);
#42074=VERTEX_POINT('',#224022);
#42075=VERTEX_POINT('',#224024);
#42076=VERTEX_POINT('',#224026);
#42077=VERTEX_POINT('',#224028);
#42078=VERTEX_POINT('',#224030);
#42079=VERTEX_POINT('',#224034);
#42080=VERTEX_POINT('',#224036);
#42081=VERTEX_POINT('',#224040);
#42082=VERTEX_POINT('',#224041);
#42083=VERTEX_POINT('',#224043);
#42084=VERTEX_POINT('',#224045);
#42085=VERTEX_POINT('',#224049);
#42086=VERTEX_POINT('',#224050);
#42087=VERTEX_POINT('',#224052);
#42088=VERTEX_POINT('',#224054);
#42089=VERTEX_POINT('',#224056);
#42090=VERTEX_POINT('',#224058);
#42091=VERTEX_POINT('',#224062);
#42092=VERTEX_POINT('',#224064);
#42093=VERTEX_POINT('',#224080);
#42094=VERTEX_POINT('',#224081);
#42095=VERTEX_POINT('',#224083);
#42096=VERTEX_POINT('',#224085);
#42097=VERTEX_POINT('',#224087);
#42098=VERTEX_POINT('',#224089);
#42099=VERTEX_POINT('',#224093);
#42100=VERTEX_POINT('',#224095);
#42101=VERTEX_POINT('',#224099);
#42102=VERTEX_POINT('',#224100);
#42103=VERTEX_POINT('',#224102);
#42104=VERTEX_POINT('',#224104);
#42105=VERTEX_POINT('',#224108);
#42106=VERTEX_POINT('',#224109);
#42107=VERTEX_POINT('',#224111);
#42108=VERTEX_POINT('',#224113);
#42109=VERTEX_POINT('',#224115);
#42110=VERTEX_POINT('',#224117);
#42111=VERTEX_POINT('',#224121);
#42112=VERTEX_POINT('',#224123);
#42113=VERTEX_POINT('',#224139);
#42114=VERTEX_POINT('',#224140);
#42115=VERTEX_POINT('',#224142);
#42116=VERTEX_POINT('',#224144);
#42117=VERTEX_POINT('',#224146);
#42118=VERTEX_POINT('',#224148);
#42119=VERTEX_POINT('',#224152);
#42120=VERTEX_POINT('',#224154);
#42121=VERTEX_POINT('',#224158);
#42122=VERTEX_POINT('',#224159);
#42123=VERTEX_POINT('',#224161);
#42124=VERTEX_POINT('',#224163);
#42125=VERTEX_POINT('',#224167);
#42126=VERTEX_POINT('',#224168);
#42127=VERTEX_POINT('',#224170);
#42128=VERTEX_POINT('',#224172);
#42129=VERTEX_POINT('',#224174);
#42130=VERTEX_POINT('',#224176);
#42131=VERTEX_POINT('',#224180);
#42132=VERTEX_POINT('',#224182);
#42133=VERTEX_POINT('',#224198);
#42134=VERTEX_POINT('',#224199);
#42135=VERTEX_POINT('',#224201);
#42136=VERTEX_POINT('',#224203);
#42137=VERTEX_POINT('',#224205);
#42138=VERTEX_POINT('',#224207);
#42139=VERTEX_POINT('',#224211);
#42140=VERTEX_POINT('',#224213);
#42141=VERTEX_POINT('',#224217);
#42142=VERTEX_POINT('',#224218);
#42143=VERTEX_POINT('',#224220);
#42144=VERTEX_POINT('',#224222);
#42145=VERTEX_POINT('',#224226);
#42146=VERTEX_POINT('',#224227);
#42147=VERTEX_POINT('',#224229);
#42148=VERTEX_POINT('',#224231);
#42149=VERTEX_POINT('',#224233);
#42150=VERTEX_POINT('',#224235);
#42151=VERTEX_POINT('',#224239);
#42152=VERTEX_POINT('',#224241);
#42153=VERTEX_POINT('',#224257);
#42154=VERTEX_POINT('',#224258);
#42155=VERTEX_POINT('',#224260);
#42156=VERTEX_POINT('',#224262);
#42157=VERTEX_POINT('',#224264);
#42158=VERTEX_POINT('',#224266);
#42159=VERTEX_POINT('',#224270);
#42160=VERTEX_POINT('',#224272);
#42161=VERTEX_POINT('',#224276);
#42162=VERTEX_POINT('',#224277);
#42163=VERTEX_POINT('',#224279);
#42164=VERTEX_POINT('',#224281);
#42165=VERTEX_POINT('',#224285);
#42166=VERTEX_POINT('',#224286);
#42167=VERTEX_POINT('',#224288);
#42168=VERTEX_POINT('',#224290);
#42169=VERTEX_POINT('',#224292);
#42170=VERTEX_POINT('',#224294);
#42171=VERTEX_POINT('',#224298);
#42172=VERTEX_POINT('',#224300);
#42173=VERTEX_POINT('',#224316);
#42174=VERTEX_POINT('',#224317);
#42175=VERTEX_POINT('',#224319);
#42176=VERTEX_POINT('',#224321);
#42177=VERTEX_POINT('',#224323);
#42178=VERTEX_POINT('',#224325);
#42179=VERTEX_POINT('',#224329);
#42180=VERTEX_POINT('',#224331);
#42181=VERTEX_POINT('',#224335);
#42182=VERTEX_POINT('',#224336);
#42183=VERTEX_POINT('',#224338);
#42184=VERTEX_POINT('',#224340);
#42185=VERTEX_POINT('',#224344);
#42186=VERTEX_POINT('',#224345);
#42187=VERTEX_POINT('',#224347);
#42188=VERTEX_POINT('',#224349);
#42189=VERTEX_POINT('',#224351);
#42190=VERTEX_POINT('',#224353);
#42191=VERTEX_POINT('',#224357);
#42192=VERTEX_POINT('',#224359);
#42193=VERTEX_POINT('',#224375);
#42194=VERTEX_POINT('',#224376);
#42195=VERTEX_POINT('',#224378);
#42196=VERTEX_POINT('',#224380);
#42197=VERTEX_POINT('',#224382);
#42198=VERTEX_POINT('',#224384);
#42199=VERTEX_POINT('',#224388);
#42200=VERTEX_POINT('',#224390);
#42201=VERTEX_POINT('',#224394);
#42202=VERTEX_POINT('',#224395);
#42203=VERTEX_POINT('',#224397);
#42204=VERTEX_POINT('',#224399);
#42205=VERTEX_POINT('',#224403);
#42206=VERTEX_POINT('',#224404);
#42207=VERTEX_POINT('',#224406);
#42208=VERTEX_POINT('',#224408);
#42209=VERTEX_POINT('',#224410);
#42210=VERTEX_POINT('',#224412);
#42211=VERTEX_POINT('',#224416);
#42212=VERTEX_POINT('',#224418);
#42213=VERTEX_POINT('',#224434);
#42214=VERTEX_POINT('',#224435);
#42215=VERTEX_POINT('',#224437);
#42216=VERTEX_POINT('',#224439);
#42217=VERTEX_POINT('',#224441);
#42218=VERTEX_POINT('',#224443);
#42219=VERTEX_POINT('',#224447);
#42220=VERTEX_POINT('',#224449);
#42221=VERTEX_POINT('',#224453);
#42222=VERTEX_POINT('',#224454);
#42223=VERTEX_POINT('',#224456);
#42224=VERTEX_POINT('',#224458);
#42225=VERTEX_POINT('',#224462);
#42226=VERTEX_POINT('',#224463);
#42227=VERTEX_POINT('',#224465);
#42228=VERTEX_POINT('',#224467);
#42229=VERTEX_POINT('',#224469);
#42230=VERTEX_POINT('',#224471);
#42231=VERTEX_POINT('',#224475);
#42232=VERTEX_POINT('',#224477);
#42233=VERTEX_POINT('',#224493);
#42234=VERTEX_POINT('',#224494);
#42235=VERTEX_POINT('',#224496);
#42236=VERTEX_POINT('',#224498);
#42237=VERTEX_POINT('',#224500);
#42238=VERTEX_POINT('',#224502);
#42239=VERTEX_POINT('',#224506);
#42240=VERTEX_POINT('',#224508);
#42241=VERTEX_POINT('',#224512);
#42242=VERTEX_POINT('',#224513);
#42243=VERTEX_POINT('',#224515);
#42244=VERTEX_POINT('',#224517);
#42245=VERTEX_POINT('',#224521);
#42246=VERTEX_POINT('',#224522);
#42247=VERTEX_POINT('',#224524);
#42248=VERTEX_POINT('',#224526);
#42249=VERTEX_POINT('',#224528);
#42250=VERTEX_POINT('',#224530);
#42251=VERTEX_POINT('',#224534);
#42252=VERTEX_POINT('',#224536);
#42253=VERTEX_POINT('',#224552);
#42254=VERTEX_POINT('',#224553);
#42255=VERTEX_POINT('',#224555);
#42256=VERTEX_POINT('',#224557);
#42257=VERTEX_POINT('',#224559);
#42258=VERTEX_POINT('',#224561);
#42259=VERTEX_POINT('',#224565);
#42260=VERTEX_POINT('',#224567);
#42261=VERTEX_POINT('',#224571);
#42262=VERTEX_POINT('',#224572);
#42263=VERTEX_POINT('',#224574);
#42264=VERTEX_POINT('',#224576);
#42265=VERTEX_POINT('',#224580);
#42266=VERTEX_POINT('',#224581);
#42267=VERTEX_POINT('',#224583);
#42268=VERTEX_POINT('',#224585);
#42269=VERTEX_POINT('',#224587);
#42270=VERTEX_POINT('',#224589);
#42271=VERTEX_POINT('',#224593);
#42272=VERTEX_POINT('',#224595);
#42273=VERTEX_POINT('',#224611);
#42274=VERTEX_POINT('',#224612);
#42275=VERTEX_POINT('',#224614);
#42276=VERTEX_POINT('',#224616);
#42277=VERTEX_POINT('',#224618);
#42278=VERTEX_POINT('',#224620);
#42279=VERTEX_POINT('',#224624);
#42280=VERTEX_POINT('',#224626);
#42281=VERTEX_POINT('',#224630);
#42282=VERTEX_POINT('',#224631);
#42283=VERTEX_POINT('',#224633);
#42284=VERTEX_POINT('',#224635);
#42285=VERTEX_POINT('',#224639);
#42286=VERTEX_POINT('',#224640);
#42287=VERTEX_POINT('',#224642);
#42288=VERTEX_POINT('',#224644);
#42289=VERTEX_POINT('',#224646);
#42290=VERTEX_POINT('',#224648);
#42291=VERTEX_POINT('',#224652);
#42292=VERTEX_POINT('',#224654);
#42293=VERTEX_POINT('',#224670);
#42294=VERTEX_POINT('',#224671);
#42295=VERTEX_POINT('',#224673);
#42296=VERTEX_POINT('',#224675);
#42297=VERTEX_POINT('',#224677);
#42298=VERTEX_POINT('',#224679);
#42299=VERTEX_POINT('',#224683);
#42300=VERTEX_POINT('',#224685);
#42301=VERTEX_POINT('',#224689);
#42302=VERTEX_POINT('',#224690);
#42303=VERTEX_POINT('',#224692);
#42304=VERTEX_POINT('',#224694);
#42305=VERTEX_POINT('',#224698);
#42306=VERTEX_POINT('',#224699);
#42307=VERTEX_POINT('',#224701);
#42308=VERTEX_POINT('',#224703);
#42309=VERTEX_POINT('',#224705);
#42310=VERTEX_POINT('',#224707);
#42311=VERTEX_POINT('',#224711);
#42312=VERTEX_POINT('',#224713);
#42313=VERTEX_POINT('',#224729);
#42314=VERTEX_POINT('',#224730);
#42315=VERTEX_POINT('',#224732);
#42316=VERTEX_POINT('',#224734);
#42317=VERTEX_POINT('',#224736);
#42318=VERTEX_POINT('',#224738);
#42319=VERTEX_POINT('',#224742);
#42320=VERTEX_POINT('',#224744);
#42321=VERTEX_POINT('',#224748);
#42322=VERTEX_POINT('',#224749);
#42323=VERTEX_POINT('',#224751);
#42324=VERTEX_POINT('',#224753);
#42325=VERTEX_POINT('',#224757);
#42326=VERTEX_POINT('',#224758);
#42327=VERTEX_POINT('',#224760);
#42328=VERTEX_POINT('',#224762);
#42329=VERTEX_POINT('',#224764);
#42330=VERTEX_POINT('',#224766);
#42331=VERTEX_POINT('',#224770);
#42332=VERTEX_POINT('',#224772);
#42333=VERTEX_POINT('',#224788);
#42334=VERTEX_POINT('',#224789);
#42335=VERTEX_POINT('',#224791);
#42336=VERTEX_POINT('',#224793);
#42337=VERTEX_POINT('',#224795);
#42338=VERTEX_POINT('',#224797);
#42339=VERTEX_POINT('',#224801);
#42340=VERTEX_POINT('',#224803);
#42341=VERTEX_POINT('',#224807);
#42342=VERTEX_POINT('',#224808);
#42343=VERTEX_POINT('',#224810);
#42344=VERTEX_POINT('',#224812);
#42345=VERTEX_POINT('',#224816);
#42346=VERTEX_POINT('',#224817);
#42347=VERTEX_POINT('',#224819);
#42348=VERTEX_POINT('',#224821);
#42349=VERTEX_POINT('',#224823);
#42350=VERTEX_POINT('',#224825);
#42351=VERTEX_POINT('',#224829);
#42352=VERTEX_POINT('',#224831);
#42353=VERTEX_POINT('',#224848);
#42354=VERTEX_POINT('',#224849);
#42355=VERTEX_POINT('',#224851);
#42356=VERTEX_POINT('',#224853);
#42357=VERTEX_POINT('',#224855);
#42358=VERTEX_POINT('',#224857);
#42359=VERTEX_POINT('',#224861);
#42360=VERTEX_POINT('',#224863);
#42361=VERTEX_POINT('',#224867);
#42362=VERTEX_POINT('',#224868);
#42363=VERTEX_POINT('',#224870);
#42364=VERTEX_POINT('',#224872);
#42365=VERTEX_POINT('',#224876);
#42366=VERTEX_POINT('',#224877);
#42367=VERTEX_POINT('',#224879);
#42368=VERTEX_POINT('',#224881);
#42369=VERTEX_POINT('',#224883);
#42370=VERTEX_POINT('',#224885);
#42371=VERTEX_POINT('',#224889);
#42372=VERTEX_POINT('',#224891);
#42373=VERTEX_POINT('',#224909);
#42374=VERTEX_POINT('',#224910);
#42375=VERTEX_POINT('',#224912);
#42376=VERTEX_POINT('',#224914);
#42377=VERTEX_POINT('',#224918);
#42378=VERTEX_POINT('',#224919);
#42379=VERTEX_POINT('',#224921);
#42380=VERTEX_POINT('',#224923);
#42381=VERTEX_POINT('',#224925);
#42382=VERTEX_POINT('',#224927);
#42383=VERTEX_POINT('',#224929);
#42384=VERTEX_POINT('',#224931);
#42385=VERTEX_POINT('',#224933);
#42386=VERTEX_POINT('',#224935);
#42387=VERTEX_POINT('',#224937);
#42388=VERTEX_POINT('',#224939);
#42389=VERTEX_POINT('',#224943);
#42390=VERTEX_POINT('',#224944);
#42391=VERTEX_POINT('',#224946);
#42392=VERTEX_POINT('',#224948);
#42393=VERTEX_POINT('',#224950);
#42394=VERTEX_POINT('',#224952);
#42395=VERTEX_POINT('',#224954);
#42396=VERTEX_POINT('',#224956);
#42397=VERTEX_POINT('',#224958);
#42398=VERTEX_POINT('',#224960);
#42399=VERTEX_POINT('',#224962);
#42400=VERTEX_POINT('',#224964);
#42401=VERTEX_POINT('',#225384);
#42402=VERTEX_POINT('',#225385);
#42403=VERTEX_POINT('',#225387);
#42404=VERTEX_POINT('',#225389);
#42405=VERTEX_POINT('',#225393);
#42406=VERTEX_POINT('',#225394);
#42407=VERTEX_POINT('',#225396);
#42408=VERTEX_POINT('',#225398);
#42409=VERTEX_POINT('',#225400);
#42410=VERTEX_POINT('',#225402);
#42411=VERTEX_POINT('',#225404);
#42412=VERTEX_POINT('',#225406);
#42413=VERTEX_POINT('',#225408);
#42414=VERTEX_POINT('',#225410);
#42415=VERTEX_POINT('',#225412);
#42416=VERTEX_POINT('',#225414);
#42417=VERTEX_POINT('',#225418);
#42418=VERTEX_POINT('',#225419);
#42419=VERTEX_POINT('',#225421);
#42420=VERTEX_POINT('',#225423);
#42421=VERTEX_POINT('',#225425);
#42422=VERTEX_POINT('',#225427);
#42423=VERTEX_POINT('',#225429);
#42424=VERTEX_POINT('',#225431);
#42425=VERTEX_POINT('',#225433);
#42426=VERTEX_POINT('',#225435);
#42427=VERTEX_POINT('',#225437);
#42428=VERTEX_POINT('',#225439);
#42429=VERTEX_POINT('',#225443);
#42430=VERTEX_POINT('',#225444);
#42431=VERTEX_POINT('',#225446);
#42432=VERTEX_POINT('',#225448);
#42433=VERTEX_POINT('',#225452);
#42434=VERTEX_POINT('',#225453);
#42435=VERTEX_POINT('',#225455);
#42436=VERTEX_POINT('',#225457);
#42437=VERTEX_POINT('',#225459);
#42438=VERTEX_POINT('',#225461);
#42439=VERTEX_POINT('',#225463);
#42440=VERTEX_POINT('',#225465);
#42441=VERTEX_POINT('',#225467);
#42442=VERTEX_POINT('',#225469);
#42443=VERTEX_POINT('',#225471);
#42444=VERTEX_POINT('',#225473);
#42445=VERTEX_POINT('',#225477);
#42446=VERTEX_POINT('',#225478);
#42447=VERTEX_POINT('',#225480);
#42448=VERTEX_POINT('',#225482);
#42449=VERTEX_POINT('',#225484);
#42450=VERTEX_POINT('',#225486);
#42451=VERTEX_POINT('',#225488);
#42452=VERTEX_POINT('',#225490);
#42453=VERTEX_POINT('',#225492);
#42454=VERTEX_POINT('',#225494);
#42455=VERTEX_POINT('',#225496);
#42456=VERTEX_POINT('',#225498);
#42457=VERTEX_POINT('',#225502);
#42458=VERTEX_POINT('',#225503);
#42459=VERTEX_POINT('',#225505);
#42460=VERTEX_POINT('',#225507);
#42461=VERTEX_POINT('',#225511);
#42462=VERTEX_POINT('',#225512);
#42463=VERTEX_POINT('',#225514);
#42464=VERTEX_POINT('',#225516);
#42465=VERTEX_POINT('',#225518);
#42466=VERTEX_POINT('',#225520);
#42467=VERTEX_POINT('',#225522);
#42468=VERTEX_POINT('',#225524);
#42469=VERTEX_POINT('',#225526);
#42470=VERTEX_POINT('',#225528);
#42471=VERTEX_POINT('',#225530);
#42472=VERTEX_POINT('',#225532);
#42473=VERTEX_POINT('',#225536);
#42474=VERTEX_POINT('',#225537);
#42475=VERTEX_POINT('',#225539);
#42476=VERTEX_POINT('',#225541);
#42477=VERTEX_POINT('',#225543);
#42478=VERTEX_POINT('',#225545);
#42479=VERTEX_POINT('',#225547);
#42480=VERTEX_POINT('',#225549);
#42481=VERTEX_POINT('',#225551);
#42482=VERTEX_POINT('',#225553);
#42483=VERTEX_POINT('',#225555);
#42484=VERTEX_POINT('',#225557);
#42485=VERTEX_POINT('',#225561);
#42486=VERTEX_POINT('',#225562);
#42487=VERTEX_POINT('',#225564);
#42488=VERTEX_POINT('',#225566);
#42489=VERTEX_POINT('',#225570);
#42490=VERTEX_POINT('',#225571);
#42491=VERTEX_POINT('',#225573);
#42492=VERTEX_POINT('',#225575);
#42493=VERTEX_POINT('',#225577);
#42494=VERTEX_POINT('',#225579);
#42495=VERTEX_POINT('',#225581);
#42496=VERTEX_POINT('',#225583);
#42497=VERTEX_POINT('',#225585);
#42498=VERTEX_POINT('',#225587);
#42499=VERTEX_POINT('',#225589);
#42500=VERTEX_POINT('',#225591);
#42501=VERTEX_POINT('',#225595);
#42502=VERTEX_POINT('',#225596);
#42503=VERTEX_POINT('',#225598);
#42504=VERTEX_POINT('',#225600);
#42505=VERTEX_POINT('',#225602);
#42506=VERTEX_POINT('',#225604);
#42507=VERTEX_POINT('',#225606);
#42508=VERTEX_POINT('',#225608);
#42509=VERTEX_POINT('',#225610);
#42510=VERTEX_POINT('',#225612);
#42511=VERTEX_POINT('',#225614);
#42512=VERTEX_POINT('',#225616);
#42513=VERTEX_POINT('',#225620);
#42514=VERTEX_POINT('',#225621);
#42515=VERTEX_POINT('',#225623);
#42516=VERTEX_POINT('',#225625);
#42517=VERTEX_POINT('',#225629);
#42518=VERTEX_POINT('',#225630);
#42519=VERTEX_POINT('',#225632);
#42520=VERTEX_POINT('',#225634);
#42521=VERTEX_POINT('',#225636);
#42522=VERTEX_POINT('',#225638);
#42523=VERTEX_POINT('',#225640);
#42524=VERTEX_POINT('',#225642);
#42525=VERTEX_POINT('',#225644);
#42526=VERTEX_POINT('',#225646);
#42527=VERTEX_POINT('',#225648);
#42528=VERTEX_POINT('',#225650);
#42529=VERTEX_POINT('',#225654);
#42530=VERTEX_POINT('',#225655);
#42531=VERTEX_POINT('',#225657);
#42532=VERTEX_POINT('',#225659);
#42533=VERTEX_POINT('',#225661);
#42534=VERTEX_POINT('',#225663);
#42535=VERTEX_POINT('',#225665);
#42536=VERTEX_POINT('',#225667);
#42537=VERTEX_POINT('',#225669);
#42538=VERTEX_POINT('',#225671);
#42539=VERTEX_POINT('',#225673);
#42540=VERTEX_POINT('',#225675);
#42541=VERTEX_POINT('',#225679);
#42542=VERTEX_POINT('',#225680);
#42543=VERTEX_POINT('',#225682);
#42544=VERTEX_POINT('',#225684);
#42545=VERTEX_POINT('',#225688);
#42546=VERTEX_POINT('',#225689);
#42547=VERTEX_POINT('',#225691);
#42548=VERTEX_POINT('',#225693);
#42549=VERTEX_POINT('',#225695);
#42550=VERTEX_POINT('',#225697);
#42551=VERTEX_POINT('',#225699);
#42552=VERTEX_POINT('',#225701);
#42553=VERTEX_POINT('',#225703);
#42554=VERTEX_POINT('',#225705);
#42555=VERTEX_POINT('',#225707);
#42556=VERTEX_POINT('',#225709);
#42557=VERTEX_POINT('',#225713);
#42558=VERTEX_POINT('',#225714);
#42559=VERTEX_POINT('',#225716);
#42560=VERTEX_POINT('',#225718);
#42561=VERTEX_POINT('',#225720);
#42562=VERTEX_POINT('',#225722);
#42563=VERTEX_POINT('',#225724);
#42564=VERTEX_POINT('',#225726);
#42565=VERTEX_POINT('',#225728);
#42566=VERTEX_POINT('',#225730);
#42567=VERTEX_POINT('',#225732);
#42568=VERTEX_POINT('',#225734);
#42569=VERTEX_POINT('',#225738);
#42570=VERTEX_POINT('',#225739);
#42571=VERTEX_POINT('',#225741);
#42572=VERTEX_POINT('',#225743);
#42573=VERTEX_POINT('',#225747);
#42574=VERTEX_POINT('',#225748);
#42575=VERTEX_POINT('',#225750);
#42576=VERTEX_POINT('',#225752);
#42577=VERTEX_POINT('',#225754);
#42578=VERTEX_POINT('',#225756);
#42579=VERTEX_POINT('',#225758);
#42580=VERTEX_POINT('',#225760);
#42581=VERTEX_POINT('',#225762);
#42582=VERTEX_POINT('',#225764);
#42583=VERTEX_POINT('',#225766);
#42584=VERTEX_POINT('',#225768);
#42585=VERTEX_POINT('',#225772);
#42586=VERTEX_POINT('',#225773);
#42587=VERTEX_POINT('',#225775);
#42588=VERTEX_POINT('',#225777);
#42589=VERTEX_POINT('',#225779);
#42590=VERTEX_POINT('',#225781);
#42591=VERTEX_POINT('',#225783);
#42592=VERTEX_POINT('',#225785);
#42593=VERTEX_POINT('',#225787);
#42594=VERTEX_POINT('',#225789);
#42595=VERTEX_POINT('',#225791);
#42596=VERTEX_POINT('',#225793);
#42597=VERTEX_POINT('',#225797);
#42598=VERTEX_POINT('',#225798);
#42599=VERTEX_POINT('',#225800);
#42600=VERTEX_POINT('',#225802);
#42601=VERTEX_POINT('',#225806);
#42602=VERTEX_POINT('',#225807);
#42603=VERTEX_POINT('',#225809);
#42604=VERTEX_POINT('',#225811);
#42605=VERTEX_POINT('',#225813);
#42606=VERTEX_POINT('',#225815);
#42607=VERTEX_POINT('',#225817);
#42608=VERTEX_POINT('',#225819);
#42609=VERTEX_POINT('',#225821);
#42610=VERTEX_POINT('',#225823);
#42611=VERTEX_POINT('',#225825);
#42612=VERTEX_POINT('',#225827);
#42613=VERTEX_POINT('',#225831);
#42614=VERTEX_POINT('',#225832);
#42615=VERTEX_POINT('',#225834);
#42616=VERTEX_POINT('',#225836);
#42617=VERTEX_POINT('',#225838);
#42618=VERTEX_POINT('',#225840);
#42619=VERTEX_POINT('',#225842);
#42620=VERTEX_POINT('',#225844);
#42621=VERTEX_POINT('',#225846);
#42622=VERTEX_POINT('',#225848);
#42623=VERTEX_POINT('',#225850);
#42624=VERTEX_POINT('',#225852);
#42625=VERTEX_POINT('',#225856);
#42626=VERTEX_POINT('',#225857);
#42627=VERTEX_POINT('',#225859);
#42628=VERTEX_POINT('',#225861);
#42629=VERTEX_POINT('',#225865);
#42630=VERTEX_POINT('',#225866);
#42631=VERTEX_POINT('',#225868);
#42632=VERTEX_POINT('',#225870);
#42633=VERTEX_POINT('',#225872);
#42634=VERTEX_POINT('',#225874);
#42635=VERTEX_POINT('',#225876);
#42636=VERTEX_POINT('',#225878);
#42637=VERTEX_POINT('',#225880);
#42638=VERTEX_POINT('',#225882);
#42639=VERTEX_POINT('',#225884);
#42640=VERTEX_POINT('',#225886);
#42641=VERTEX_POINT('',#225890);
#42642=VERTEX_POINT('',#225891);
#42643=VERTEX_POINT('',#225893);
#42644=VERTEX_POINT('',#225895);
#42645=VERTEX_POINT('',#225897);
#42646=VERTEX_POINT('',#225899);
#42647=VERTEX_POINT('',#225901);
#42648=VERTEX_POINT('',#225903);
#42649=VERTEX_POINT('',#225905);
#42650=VERTEX_POINT('',#225907);
#42651=VERTEX_POINT('',#225909);
#42652=VERTEX_POINT('',#225911);
#42653=VERTEX_POINT('',#225915);
#42654=VERTEX_POINT('',#225916);
#42655=VERTEX_POINT('',#225918);
#42656=VERTEX_POINT('',#225920);
#42657=VERTEX_POINT('',#225924);
#42658=VERTEX_POINT('',#225925);
#42659=VERTEX_POINT('',#225927);
#42660=VERTEX_POINT('',#225929);
#42661=VERTEX_POINT('',#225931);
#42662=VERTEX_POINT('',#225933);
#42663=VERTEX_POINT('',#225935);
#42664=VERTEX_POINT('',#225937);
#42665=VERTEX_POINT('',#225939);
#42666=VERTEX_POINT('',#225941);
#42667=VERTEX_POINT('',#225943);
#42668=VERTEX_POINT('',#225945);
#42669=VERTEX_POINT('',#225949);
#42670=VERTEX_POINT('',#225950);
#42671=VERTEX_POINT('',#225952);
#42672=VERTEX_POINT('',#225954);
#42673=VERTEX_POINT('',#225956);
#42674=VERTEX_POINT('',#225958);
#42675=VERTEX_POINT('',#225960);
#42676=VERTEX_POINT('',#225962);
#42677=VERTEX_POINT('',#225964);
#42678=VERTEX_POINT('',#225966);
#42679=VERTEX_POINT('',#225968);
#42680=VERTEX_POINT('',#225970);
#42681=VERTEX_POINT('',#225974);
#42682=VERTEX_POINT('',#225975);
#42683=VERTEX_POINT('',#225977);
#42684=VERTEX_POINT('',#225979);
#42685=VERTEX_POINT('',#225983);
#42686=VERTEX_POINT('',#225984);
#42687=VERTEX_POINT('',#225986);
#42688=VERTEX_POINT('',#225988);
#42689=VERTEX_POINT('',#225990);
#42690=VERTEX_POINT('',#225992);
#42691=VERTEX_POINT('',#225994);
#42692=VERTEX_POINT('',#225996);
#42693=VERTEX_POINT('',#225998);
#42694=VERTEX_POINT('',#226000);
#42695=VERTEX_POINT('',#226002);
#42696=VERTEX_POINT('',#226004);
#42697=VERTEX_POINT('',#226008);
#42698=VERTEX_POINT('',#226009);
#42699=VERTEX_POINT('',#226011);
#42700=VERTEX_POINT('',#226013);
#42701=VERTEX_POINT('',#226015);
#42702=VERTEX_POINT('',#226017);
#42703=VERTEX_POINT('',#226019);
#42704=VERTEX_POINT('',#226021);
#42705=VERTEX_POINT('',#226023);
#42706=VERTEX_POINT('',#226025);
#42707=VERTEX_POINT('',#226027);
#42708=VERTEX_POINT('',#226029);
#42709=VERTEX_POINT('',#226033);
#42710=VERTEX_POINT('',#226034);
#42711=VERTEX_POINT('',#226036);
#42712=VERTEX_POINT('',#226038);
#42713=VERTEX_POINT('',#226042);
#42714=VERTEX_POINT('',#226043);
#42715=VERTEX_POINT('',#226045);
#42716=VERTEX_POINT('',#226047);
#42717=VERTEX_POINT('',#226049);
#42718=VERTEX_POINT('',#226051);
#42719=VERTEX_POINT('',#226053);
#42720=VERTEX_POINT('',#226055);
#42721=VERTEX_POINT('',#226057);
#42722=VERTEX_POINT('',#226059);
#42723=VERTEX_POINT('',#226061);
#42724=VERTEX_POINT('',#226063);
#42725=VERTEX_POINT('',#226067);
#42726=VERTEX_POINT('',#226068);
#42727=VERTEX_POINT('',#226070);
#42728=VERTEX_POINT('',#226072);
#42729=VERTEX_POINT('',#226074);
#42730=VERTEX_POINT('',#226076);
#42731=VERTEX_POINT('',#226078);
#42732=VERTEX_POINT('',#226080);
#42733=VERTEX_POINT('',#226082);
#42734=VERTEX_POINT('',#226084);
#42735=VERTEX_POINT('',#226086);
#42736=VERTEX_POINT('',#226088);
#42737=VERTEX_POINT('',#226092);
#42738=VERTEX_POINT('',#226093);
#42739=VERTEX_POINT('',#226095);
#42740=VERTEX_POINT('',#226097);
#42741=VERTEX_POINT('',#226101);
#42742=VERTEX_POINT('',#226102);
#42743=VERTEX_POINT('',#226104);
#42744=VERTEX_POINT('',#226106);
#42745=VERTEX_POINT('',#226108);
#42746=VERTEX_POINT('',#226110);
#42747=VERTEX_POINT('',#226112);
#42748=VERTEX_POINT('',#226114);
#42749=VERTEX_POINT('',#226116);
#42750=VERTEX_POINT('',#226118);
#42751=VERTEX_POINT('',#226120);
#42752=VERTEX_POINT('',#226122);
#42753=VERTEX_POINT('',#226126);
#42754=VERTEX_POINT('',#226127);
#42755=VERTEX_POINT('',#226129);
#42756=VERTEX_POINT('',#226131);
#42757=VERTEX_POINT('',#226133);
#42758=VERTEX_POINT('',#226135);
#42759=VERTEX_POINT('',#226137);
#42760=VERTEX_POINT('',#226139);
#42761=VERTEX_POINT('',#226141);
#42762=VERTEX_POINT('',#226143);
#42763=VERTEX_POINT('',#226145);
#42764=VERTEX_POINT('',#226147);
#42765=VERTEX_POINT('',#226151);
#42766=VERTEX_POINT('',#226152);
#42767=VERTEX_POINT('',#226154);
#42768=VERTEX_POINT('',#226156);
#42769=VERTEX_POINT('',#226160);
#42770=VERTEX_POINT('',#226161);
#42771=VERTEX_POINT('',#226163);
#42772=VERTEX_POINT('',#226165);
#42773=VERTEX_POINT('',#226167);
#42774=VERTEX_POINT('',#226169);
#42775=VERTEX_POINT('',#226171);
#42776=VERTEX_POINT('',#226173);
#42777=VERTEX_POINT('',#226175);
#42778=VERTEX_POINT('',#226177);
#42779=VERTEX_POINT('',#226179);
#42780=VERTEX_POINT('',#226181);
#42781=VERTEX_POINT('',#226185);
#42782=VERTEX_POINT('',#226186);
#42783=VERTEX_POINT('',#226188);
#42784=VERTEX_POINT('',#226190);
#42785=VERTEX_POINT('',#226192);
#42786=VERTEX_POINT('',#226194);
#42787=VERTEX_POINT('',#226196);
#42788=VERTEX_POINT('',#226198);
#42789=VERTEX_POINT('',#226200);
#42790=VERTEX_POINT('',#226202);
#42791=VERTEX_POINT('',#226204);
#42792=VERTEX_POINT('',#226206);
#42793=VERTEX_POINT('',#226210);
#42794=VERTEX_POINT('',#226211);
#42795=VERTEX_POINT('',#226213);
#42796=VERTEX_POINT('',#226215);
#42797=VERTEX_POINT('',#226219);
#42798=VERTEX_POINT('',#226220);
#42799=VERTEX_POINT('',#226222);
#42800=VERTEX_POINT('',#226224);
#42801=VERTEX_POINT('',#226226);
#42802=VERTEX_POINT('',#226228);
#42803=VERTEX_POINT('',#226230);
#42804=VERTEX_POINT('',#226232);
#42805=VERTEX_POINT('',#226234);
#42806=VERTEX_POINT('',#226236);
#42807=VERTEX_POINT('',#226238);
#42808=VERTEX_POINT('',#226240);
#42809=VERTEX_POINT('',#226244);
#42810=VERTEX_POINT('',#226245);
#42811=VERTEX_POINT('',#226247);
#42812=VERTEX_POINT('',#226249);
#42813=VERTEX_POINT('',#226251);
#42814=VERTEX_POINT('',#226253);
#42815=VERTEX_POINT('',#226255);
#42816=VERTEX_POINT('',#226257);
#42817=VERTEX_POINT('',#226259);
#42818=VERTEX_POINT('',#226261);
#42819=VERTEX_POINT('',#226263);
#42820=VERTEX_POINT('',#226265);
#42821=VERTEX_POINT('',#226269);
#42822=VERTEX_POINT('',#226270);
#42823=VERTEX_POINT('',#226272);
#42824=VERTEX_POINT('',#226274);
#42825=VERTEX_POINT('',#226278);
#42826=VERTEX_POINT('',#226279);
#42827=VERTEX_POINT('',#226281);
#42828=VERTEX_POINT('',#226283);
#42829=VERTEX_POINT('',#226285);
#42830=VERTEX_POINT('',#226287);
#42831=VERTEX_POINT('',#226289);
#42832=VERTEX_POINT('',#226291);
#42833=VERTEX_POINT('',#226293);
#42834=VERTEX_POINT('',#226295);
#42835=VERTEX_POINT('',#226297);
#42836=VERTEX_POINT('',#226299);
#42837=VERTEX_POINT('',#226303);
#42838=VERTEX_POINT('',#226304);
#42839=VERTEX_POINT('',#226306);
#42840=VERTEX_POINT('',#226308);
#42841=VERTEX_POINT('',#226310);
#42842=VERTEX_POINT('',#226312);
#42843=VERTEX_POINT('',#226314);
#42844=VERTEX_POINT('',#226316);
#42845=VERTEX_POINT('',#226318);
#42846=VERTEX_POINT('',#226320);
#42847=VERTEX_POINT('',#226322);
#42848=VERTEX_POINT('',#226324);
#42849=VERTEX_POINT('',#226328);
#42850=VERTEX_POINT('',#226329);
#42851=VERTEX_POINT('',#226331);
#42852=VERTEX_POINT('',#226333);
#42853=VERTEX_POINT('',#226337);
#42854=VERTEX_POINT('',#226338);
#42855=VERTEX_POINT('',#226340);
#42856=VERTEX_POINT('',#226342);
#42857=VERTEX_POINT('',#226344);
#42858=VERTEX_POINT('',#226346);
#42859=VERTEX_POINT('',#226348);
#42860=VERTEX_POINT('',#226350);
#42861=VERTEX_POINT('',#226352);
#42862=VERTEX_POINT('',#226354);
#42863=VERTEX_POINT('',#226356);
#42864=VERTEX_POINT('',#226358);
#42865=VERTEX_POINT('',#226362);
#42866=VERTEX_POINT('',#226363);
#42867=VERTEX_POINT('',#226365);
#42868=VERTEX_POINT('',#226367);
#42869=VERTEX_POINT('',#226369);
#42870=VERTEX_POINT('',#226371);
#42871=VERTEX_POINT('',#226373);
#42872=VERTEX_POINT('',#226375);
#42873=VERTEX_POINT('',#226377);
#42874=VERTEX_POINT('',#226379);
#42875=VERTEX_POINT('',#226381);
#42876=VERTEX_POINT('',#226383);
#42877=VERTEX_POINT('',#226387);
#42878=VERTEX_POINT('',#226388);
#42879=VERTEX_POINT('',#226390);
#42880=VERTEX_POINT('',#226392);
#42881=VERTEX_POINT('',#226396);
#42882=VERTEX_POINT('',#226397);
#42883=VERTEX_POINT('',#226399);
#42884=VERTEX_POINT('',#226401);
#42885=VERTEX_POINT('',#226403);
#42886=VERTEX_POINT('',#226405);
#42887=VERTEX_POINT('',#226407);
#42888=VERTEX_POINT('',#226409);
#42889=VERTEX_POINT('',#226411);
#42890=VERTEX_POINT('',#226413);
#42891=VERTEX_POINT('',#226415);
#42892=VERTEX_POINT('',#226417);
#42893=VERTEX_POINT('',#226421);
#42894=VERTEX_POINT('',#226422);
#42895=VERTEX_POINT('',#226424);
#42896=VERTEX_POINT('',#226426);
#42897=VERTEX_POINT('',#226428);
#42898=VERTEX_POINT('',#226430);
#42899=VERTEX_POINT('',#226432);
#42900=VERTEX_POINT('',#226434);
#42901=VERTEX_POINT('',#226436);
#42902=VERTEX_POINT('',#226438);
#42903=VERTEX_POINT('',#226440);
#42904=VERTEX_POINT('',#226442);
#42905=VERTEX_POINT('',#226446);
#42906=VERTEX_POINT('',#226447);
#42907=VERTEX_POINT('',#226449);
#42908=VERTEX_POINT('',#226451);
#42909=VERTEX_POINT('',#226455);
#42910=VERTEX_POINT('',#226456);
#42911=VERTEX_POINT('',#226458);
#42912=VERTEX_POINT('',#226460);
#42913=VERTEX_POINT('',#226462);
#42914=VERTEX_POINT('',#226464);
#42915=VERTEX_POINT('',#226466);
#42916=VERTEX_POINT('',#226468);
#42917=VERTEX_POINT('',#226470);
#42918=VERTEX_POINT('',#226472);
#42919=VERTEX_POINT('',#226474);
#42920=VERTEX_POINT('',#226476);
#42921=VERTEX_POINT('',#226480);
#42922=VERTEX_POINT('',#226481);
#42923=VERTEX_POINT('',#226483);
#42924=VERTEX_POINT('',#226485);
#42925=VERTEX_POINT('',#226487);
#42926=VERTEX_POINT('',#226489);
#42927=VERTEX_POINT('',#226491);
#42928=VERTEX_POINT('',#226493);
#42929=VERTEX_POINT('',#226495);
#42930=VERTEX_POINT('',#226497);
#42931=VERTEX_POINT('',#226499);
#42932=VERTEX_POINT('',#226501);
#42933=VERTEX_POINT('',#226505);
#42934=VERTEX_POINT('',#226506);
#42935=VERTEX_POINT('',#226508);
#42936=VERTEX_POINT('',#226510);
#42937=VERTEX_POINT('',#226514);
#42938=VERTEX_POINT('',#226515);
#42939=VERTEX_POINT('',#226517);
#42940=VERTEX_POINT('',#226519);
#42941=VERTEX_POINT('',#226521);
#42942=VERTEX_POINT('',#226523);
#42943=VERTEX_POINT('',#226525);
#42944=VERTEX_POINT('',#226527);
#42945=VERTEX_POINT('',#226529);
#42946=VERTEX_POINT('',#226531);
#42947=VERTEX_POINT('',#226533);
#42948=VERTEX_POINT('',#226535);
#42949=VERTEX_POINT('',#226539);
#42950=VERTEX_POINT('',#226540);
#42951=VERTEX_POINT('',#226542);
#42952=VERTEX_POINT('',#226544);
#42953=VERTEX_POINT('',#226546);
#42954=VERTEX_POINT('',#226548);
#42955=VERTEX_POINT('',#226550);
#42956=VERTEX_POINT('',#226552);
#42957=VERTEX_POINT('',#226554);
#42958=VERTEX_POINT('',#226556);
#42959=VERTEX_POINT('',#226558);
#42960=VERTEX_POINT('',#226560);
#42961=VERTEX_POINT('',#226564);
#42962=VERTEX_POINT('',#226565);
#42963=VERTEX_POINT('',#226567);
#42964=VERTEX_POINT('',#226569);
#42965=VERTEX_POINT('',#226573);
#42966=VERTEX_POINT('',#226574);
#42967=VERTEX_POINT('',#226576);
#42968=VERTEX_POINT('',#226578);
#42969=VERTEX_POINT('',#226580);
#42970=VERTEX_POINT('',#226582);
#42971=VERTEX_POINT('',#226584);
#42972=VERTEX_POINT('',#226586);
#42973=VERTEX_POINT('',#226588);
#42974=VERTEX_POINT('',#226590);
#42975=VERTEX_POINT('',#226592);
#42976=VERTEX_POINT('',#226594);
#42977=VERTEX_POINT('',#226598);
#42978=VERTEX_POINT('',#226599);
#42979=VERTEX_POINT('',#226601);
#42980=VERTEX_POINT('',#226603);
#42981=VERTEX_POINT('',#226605);
#42982=VERTEX_POINT('',#226607);
#42983=VERTEX_POINT('',#226609);
#42984=VERTEX_POINT('',#226611);
#42985=VERTEX_POINT('',#226613);
#42986=VERTEX_POINT('',#226615);
#42987=VERTEX_POINT('',#226617);
#42988=VERTEX_POINT('',#226619);
#42989=VERTEX_POINT('',#226623);
#42990=VERTEX_POINT('',#226624);
#42991=VERTEX_POINT('',#226626);
#42992=VERTEX_POINT('',#226628);
#42993=VERTEX_POINT('',#226632);
#42994=VERTEX_POINT('',#226633);
#42995=VERTEX_POINT('',#226635);
#42996=VERTEX_POINT('',#226637);
#42997=VERTEX_POINT('',#226639);
#42998=VERTEX_POINT('',#226641);
#42999=VERTEX_POINT('',#226643);
#43000=VERTEX_POINT('',#226645);
#43001=VERTEX_POINT('',#226647);
#43002=VERTEX_POINT('',#226649);
#43003=VERTEX_POINT('',#226651);
#43004=VERTEX_POINT('',#226653);
#43005=VERTEX_POINT('',#226657);
#43006=VERTEX_POINT('',#226658);
#43007=VERTEX_POINT('',#226660);
#43008=VERTEX_POINT('',#226662);
#43009=VERTEX_POINT('',#226664);
#43010=VERTEX_POINT('',#226666);
#43011=VERTEX_POINT('',#226668);
#43012=VERTEX_POINT('',#226670);
#43013=VERTEX_POINT('',#226672);
#43014=VERTEX_POINT('',#226674);
#43015=VERTEX_POINT('',#226676);
#43016=VERTEX_POINT('',#226678);
#43017=VERTEX_POINT('',#226682);
#43018=VERTEX_POINT('',#226683);
#43019=VERTEX_POINT('',#226685);
#43020=VERTEX_POINT('',#226687);
#43021=VERTEX_POINT('',#226691);
#43022=VERTEX_POINT('',#226692);
#43023=VERTEX_POINT('',#226694);
#43024=VERTEX_POINT('',#226696);
#43025=VERTEX_POINT('',#226698);
#43026=VERTEX_POINT('',#226700);
#43027=VERTEX_POINT('',#226702);
#43028=VERTEX_POINT('',#226704);
#43029=VERTEX_POINT('',#226706);
#43030=VERTEX_POINT('',#226708);
#43031=VERTEX_POINT('',#226710);
#43032=VERTEX_POINT('',#226712);
#43033=VERTEX_POINT('',#226716);
#43034=VERTEX_POINT('',#226717);
#43035=VERTEX_POINT('',#226719);
#43036=VERTEX_POINT('',#226721);
#43037=VERTEX_POINT('',#226723);
#43038=VERTEX_POINT('',#226725);
#43039=VERTEX_POINT('',#226727);
#43040=VERTEX_POINT('',#226729);
#43041=VERTEX_POINT('',#226731);
#43042=VERTEX_POINT('',#226733);
#43043=VERTEX_POINT('',#226735);
#43044=VERTEX_POINT('',#226737);
#43045=VERTEX_POINT('',#226741);
#43046=VERTEX_POINT('',#226742);
#43047=VERTEX_POINT('',#226744);
#43048=VERTEX_POINT('',#226746);
#43049=VERTEX_POINT('',#226750);
#43050=VERTEX_POINT('',#226751);
#43051=VERTEX_POINT('',#226753);
#43052=VERTEX_POINT('',#226755);
#43053=VERTEX_POINT('',#226757);
#43054=VERTEX_POINT('',#226759);
#43055=VERTEX_POINT('',#226761);
#43056=VERTEX_POINT('',#226763);
#43057=VERTEX_POINT('',#226765);
#43058=VERTEX_POINT('',#226767);
#43059=VERTEX_POINT('',#226769);
#43060=VERTEX_POINT('',#226771);
#43061=VERTEX_POINT('',#226775);
#43062=VERTEX_POINT('',#226776);
#43063=VERTEX_POINT('',#226778);
#43064=VERTEX_POINT('',#226780);
#43065=VERTEX_POINT('',#226782);
#43066=VERTEX_POINT('',#226784);
#43067=VERTEX_POINT('',#226786);
#43068=VERTEX_POINT('',#226788);
#43069=VERTEX_POINT('',#226790);
#43070=VERTEX_POINT('',#226792);
#43071=VERTEX_POINT('',#226794);
#43072=VERTEX_POINT('',#226796);
#43073=VERTEX_POINT('',#226800);
#43074=VERTEX_POINT('',#226801);
#43075=VERTEX_POINT('',#226803);
#43076=VERTEX_POINT('',#226805);
#43077=VERTEX_POINT('',#226809);
#43078=VERTEX_POINT('',#226810);
#43079=VERTEX_POINT('',#226812);
#43080=VERTEX_POINT('',#226814);
#43081=VERTEX_POINT('',#226816);
#43082=VERTEX_POINT('',#226818);
#43083=VERTEX_POINT('',#226820);
#43084=VERTEX_POINT('',#226822);
#43085=VERTEX_POINT('',#226824);
#43086=VERTEX_POINT('',#226826);
#43087=VERTEX_POINT('',#226828);
#43088=VERTEX_POINT('',#226830);
#43089=VERTEX_POINT('',#226834);
#43090=VERTEX_POINT('',#226835);
#43091=VERTEX_POINT('',#226837);
#43092=VERTEX_POINT('',#226839);
#43093=VERTEX_POINT('',#226841);
#43094=VERTEX_POINT('',#226843);
#43095=VERTEX_POINT('',#226845);
#43096=VERTEX_POINT('',#226847);
#43097=VERTEX_POINT('',#226849);
#43098=VERTEX_POINT('',#226851);
#43099=VERTEX_POINT('',#226853);
#43100=VERTEX_POINT('',#226855);
#43101=VERTEX_POINT('',#226859);
#43102=VERTEX_POINT('',#226860);
#43103=VERTEX_POINT('',#226862);
#43104=VERTEX_POINT('',#226864);
#43105=VERTEX_POINT('',#226868);
#43106=VERTEX_POINT('',#226869);
#43107=VERTEX_POINT('',#226871);
#43108=VERTEX_POINT('',#226873);
#43109=VERTEX_POINT('',#226875);
#43110=VERTEX_POINT('',#226877);
#43111=VERTEX_POINT('',#226879);
#43112=VERTEX_POINT('',#226881);
#43113=VERTEX_POINT('',#226883);
#43114=VERTEX_POINT('',#226885);
#43115=VERTEX_POINT('',#226887);
#43116=VERTEX_POINT('',#226889);
#43117=VERTEX_POINT('',#226893);
#43118=VERTEX_POINT('',#226894);
#43119=VERTEX_POINT('',#226896);
#43120=VERTEX_POINT('',#226898);
#43121=VERTEX_POINT('',#226900);
#43122=VERTEX_POINT('',#226902);
#43123=VERTEX_POINT('',#226904);
#43124=VERTEX_POINT('',#226906);
#43125=VERTEX_POINT('',#226908);
#43126=VERTEX_POINT('',#226910);
#43127=VERTEX_POINT('',#226912);
#43128=VERTEX_POINT('',#226914);
#43129=VERTEX_POINT('',#226918);
#43130=VERTEX_POINT('',#226919);
#43131=VERTEX_POINT('',#226921);
#43132=VERTEX_POINT('',#226923);
#43133=VERTEX_POINT('',#226927);
#43134=VERTEX_POINT('',#226928);
#43135=VERTEX_POINT('',#226930);
#43136=VERTEX_POINT('',#226932);
#43137=VERTEX_POINT('',#226934);
#43138=VERTEX_POINT('',#226936);
#43139=VERTEX_POINT('',#226938);
#43140=VERTEX_POINT('',#226940);
#43141=VERTEX_POINT('',#226942);
#43142=VERTEX_POINT('',#226944);
#43143=VERTEX_POINT('',#226946);
#43144=VERTEX_POINT('',#226948);
#43145=VERTEX_POINT('',#226952);
#43146=VERTEX_POINT('',#226953);
#43147=VERTEX_POINT('',#226955);
#43148=VERTEX_POINT('',#226957);
#43149=VERTEX_POINT('',#226959);
#43150=VERTEX_POINT('',#226961);
#43151=VERTEX_POINT('',#226963);
#43152=VERTEX_POINT('',#226965);
#43153=VERTEX_POINT('',#226967);
#43154=VERTEX_POINT('',#226969);
#43155=VERTEX_POINT('',#226971);
#43156=VERTEX_POINT('',#226973);
#43157=VERTEX_POINT('',#226977);
#43158=VERTEX_POINT('',#226978);
#43159=VERTEX_POINT('',#226980);
#43160=VERTEX_POINT('',#226982);
#43161=VERTEX_POINT('',#226986);
#43162=VERTEX_POINT('',#226987);
#43163=VERTEX_POINT('',#226989);
#43164=VERTEX_POINT('',#226991);
#43165=VERTEX_POINT('',#226993);
#43166=VERTEX_POINT('',#226995);
#43167=VERTEX_POINT('',#226997);
#43168=VERTEX_POINT('',#226999);
#43169=VERTEX_POINT('',#227001);
#43170=VERTEX_POINT('',#227003);
#43171=VERTEX_POINT('',#227005);
#43172=VERTEX_POINT('',#227007);
#43173=VERTEX_POINT('',#227011);
#43174=VERTEX_POINT('',#227012);
#43175=VERTEX_POINT('',#227014);
#43176=VERTEX_POINT('',#227016);
#43177=VERTEX_POINT('',#227018);
#43178=VERTEX_POINT('',#227020);
#43179=VERTEX_POINT('',#227022);
#43180=VERTEX_POINT('',#227024);
#43181=VERTEX_POINT('',#227026);
#43182=VERTEX_POINT('',#227028);
#43183=VERTEX_POINT('',#227030);
#43184=VERTEX_POINT('',#227032);
#43185=VERTEX_POINT('',#227036);
#43186=VERTEX_POINT('',#227037);
#43187=VERTEX_POINT('',#227039);
#43188=VERTEX_POINT('',#227041);
#43189=VERTEX_POINT('',#227045);
#43190=VERTEX_POINT('',#227046);
#43191=VERTEX_POINT('',#227048);
#43192=VERTEX_POINT('',#227050);
#43193=VERTEX_POINT('',#227052);
#43194=VERTEX_POINT('',#227054);
#43195=VERTEX_POINT('',#227056);
#43196=VERTEX_POINT('',#227058);
#43197=VERTEX_POINT('',#227060);
#43198=VERTEX_POINT('',#227062);
#43199=VERTEX_POINT('',#227064);
#43200=VERTEX_POINT('',#227066);
#43201=VERTEX_POINT('',#227070);
#43202=VERTEX_POINT('',#227071);
#43203=VERTEX_POINT('',#227073);
#43204=VERTEX_POINT('',#227075);
#43205=VERTEX_POINT('',#227077);
#43206=VERTEX_POINT('',#227079);
#43207=VERTEX_POINT('',#227081);
#43208=VERTEX_POINT('',#227083);
#43209=VERTEX_POINT('',#227085);
#43210=VERTEX_POINT('',#227087);
#43211=VERTEX_POINT('',#227089);
#43212=VERTEX_POINT('',#227091);
#43213=VERTEX_POINT('',#227098);
#43214=VERTEX_POINT('',#227099);
#43215=VERTEX_POINT('',#227101);
#43216=VERTEX_POINT('',#227103);
#43217=VERTEX_POINT('',#227105);
#43218=VERTEX_POINT('',#227107);
#43219=VERTEX_POINT('',#227109);
#43220=VERTEX_POINT('',#227111);
#43221=VERTEX_POINT('',#227113);
#43222=VERTEX_POINT('',#227115);
#43223=VERTEX_POINT('',#227117);
#43224=VERTEX_POINT('',#227119);
#43225=VERTEX_POINT('',#227123);
#43226=VERTEX_POINT('',#227124);
#43227=VERTEX_POINT('',#227126);
#43228=VERTEX_POINT('',#227128);
#43229=VERTEX_POINT('',#227130);
#43230=VERTEX_POINT('',#227132);
#43231=VERTEX_POINT('',#227134);
#43232=VERTEX_POINT('',#227136);
#43233=VERTEX_POINT('',#227138);
#43234=VERTEX_POINT('',#227140);
#43235=VERTEX_POINT('',#227142);
#43236=VERTEX_POINT('',#227144);
#43237=VERTEX_POINT('',#227148);
#43238=VERTEX_POINT('',#227149);
#43239=VERTEX_POINT('',#227151);
#43240=VERTEX_POINT('',#227153);
#43241=VERTEX_POINT('',#227157);
#43242=VERTEX_POINT('',#227158);
#43243=VERTEX_POINT('',#227160);
#43244=VERTEX_POINT('',#227162);
#43245=VERTEX_POINT('',#227164);
#43246=VERTEX_POINT('',#227166);
#43247=VERTEX_POINT('',#227168);
#43248=VERTEX_POINT('',#227170);
#43249=VERTEX_POINT('',#227172);
#43250=VERTEX_POINT('',#227174);
#43251=VERTEX_POINT('',#227176);
#43252=VERTEX_POINT('',#227178);
#43253=VERTEX_POINT('',#227182);
#43254=VERTEX_POINT('',#227183);
#43255=VERTEX_POINT('',#227185);
#43256=VERTEX_POINT('',#227187);
#43257=VERTEX_POINT('',#227189);
#43258=VERTEX_POINT('',#227191);
#43259=VERTEX_POINT('',#227193);
#43260=VERTEX_POINT('',#227195);
#43261=VERTEX_POINT('',#227197);
#43262=VERTEX_POINT('',#227199);
#43263=VERTEX_POINT('',#227201);
#43264=VERTEX_POINT('',#227203);
#43265=VERTEX_POINT('',#227207);
#43266=VERTEX_POINT('',#227208);
#43267=VERTEX_POINT('',#227210);
#43268=VERTEX_POINT('',#227212);
#43269=VERTEX_POINT('',#227216);
#43270=VERTEX_POINT('',#227217);
#43271=VERTEX_POINT('',#227219);
#43272=VERTEX_POINT('',#227221);
#43273=VERTEX_POINT('',#227223);
#43274=VERTEX_POINT('',#227225);
#43275=VERTEX_POINT('',#227227);
#43276=VERTEX_POINT('',#227229);
#43277=VERTEX_POINT('',#227231);
#43278=VERTEX_POINT('',#227233);
#43279=VERTEX_POINT('',#227235);
#43280=VERTEX_POINT('',#227237);
#43281=VERTEX_POINT('',#227241);
#43282=VERTEX_POINT('',#227242);
#43283=VERTEX_POINT('',#227244);
#43284=VERTEX_POINT('',#227246);
#43285=VERTEX_POINT('',#227248);
#43286=VERTEX_POINT('',#227250);
#43287=VERTEX_POINT('',#227252);
#43288=VERTEX_POINT('',#227254);
#43289=VERTEX_POINT('',#227256);
#43290=VERTEX_POINT('',#227258);
#43291=VERTEX_POINT('',#227260);
#43292=VERTEX_POINT('',#227262);
#43293=VERTEX_POINT('',#227266);
#43294=VERTEX_POINT('',#227267);
#43295=VERTEX_POINT('',#227269);
#43296=VERTEX_POINT('',#227271);
#43297=VERTEX_POINT('',#227275);
#43298=VERTEX_POINT('',#227276);
#43299=VERTEX_POINT('',#227278);
#43300=VERTEX_POINT('',#227280);
#43301=VERTEX_POINT('',#227282);
#43302=VERTEX_POINT('',#227284);
#43303=VERTEX_POINT('',#227286);
#43304=VERTEX_POINT('',#227288);
#43305=VERTEX_POINT('',#227290);
#43306=VERTEX_POINT('',#227292);
#43307=VERTEX_POINT('',#227294);
#43308=VERTEX_POINT('',#227296);
#43309=VERTEX_POINT('',#227300);
#43310=VERTEX_POINT('',#227301);
#43311=VERTEX_POINT('',#227303);
#43312=VERTEX_POINT('',#227305);
#43313=VERTEX_POINT('',#227307);
#43314=VERTEX_POINT('',#227309);
#43315=VERTEX_POINT('',#227311);
#43316=VERTEX_POINT('',#227313);
#43317=VERTEX_POINT('',#227315);
#43318=VERTEX_POINT('',#227317);
#43319=VERTEX_POINT('',#227319);
#43320=VERTEX_POINT('',#227321);
#43321=VERTEX_POINT('',#227325);
#43322=VERTEX_POINT('',#227326);
#43323=VERTEX_POINT('',#227328);
#43324=VERTEX_POINT('',#227330);
#43325=VERTEX_POINT('',#227334);
#43326=VERTEX_POINT('',#227335);
#43327=VERTEX_POINT('',#227337);
#43328=VERTEX_POINT('',#227339);
#43329=VERTEX_POINT('',#227341);
#43330=VERTEX_POINT('',#227343);
#43331=VERTEX_POINT('',#227345);
#43332=VERTEX_POINT('',#227347);
#43333=VERTEX_POINT('',#227349);
#43334=VERTEX_POINT('',#227351);
#43335=VERTEX_POINT('',#227353);
#43336=VERTEX_POINT('',#227355);
#43337=VERTEX_POINT('',#227359);
#43338=VERTEX_POINT('',#227360);
#43339=VERTEX_POINT('',#227362);
#43340=VERTEX_POINT('',#227364);
#43341=VERTEX_POINT('',#227366);
#43342=VERTEX_POINT('',#227368);
#43343=VERTEX_POINT('',#227370);
#43344=VERTEX_POINT('',#227372);
#43345=VERTEX_POINT('',#227374);
#43346=VERTEX_POINT('',#227376);
#43347=VERTEX_POINT('',#227378);
#43348=VERTEX_POINT('',#227380);
#43349=VERTEX_POINT('',#227384);
#43350=VERTEX_POINT('',#227385);
#43351=VERTEX_POINT('',#227387);
#43352=VERTEX_POINT('',#227389);
#43353=VERTEX_POINT('',#227393);
#43354=VERTEX_POINT('',#227394);
#43355=VERTEX_POINT('',#227396);
#43356=VERTEX_POINT('',#227398);
#43357=VERTEX_POINT('',#227400);
#43358=VERTEX_POINT('',#227402);
#43359=VERTEX_POINT('',#227404);
#43360=VERTEX_POINT('',#227406);
#43361=VERTEX_POINT('',#227408);
#43362=VERTEX_POINT('',#227410);
#43363=VERTEX_POINT('',#227412);
#43364=VERTEX_POINT('',#227414);
#43365=VERTEX_POINT('',#227418);
#43366=VERTEX_POINT('',#227419);
#43367=VERTEX_POINT('',#227421);
#43368=VERTEX_POINT('',#227423);
#43369=VERTEX_POINT('',#227425);
#43370=VERTEX_POINT('',#227427);
#43371=VERTEX_POINT('',#227429);
#43372=VERTEX_POINT('',#227431);
#43373=VERTEX_POINT('',#227433);
#43374=VERTEX_POINT('',#227435);
#43375=VERTEX_POINT('',#227437);
#43376=VERTEX_POINT('',#227439);
#43377=VERTEX_POINT('',#227443);
#43378=VERTEX_POINT('',#227444);
#43379=VERTEX_POINT('',#227446);
#43380=VERTEX_POINT('',#227448);
#43381=VERTEX_POINT('',#227452);
#43382=VERTEX_POINT('',#227453);
#43383=VERTEX_POINT('',#227455);
#43384=VERTEX_POINT('',#227457);
#43385=VERTEX_POINT('',#227459);
#43386=VERTEX_POINT('',#227461);
#43387=VERTEX_POINT('',#227463);
#43388=VERTEX_POINT('',#227465);
#43389=VERTEX_POINT('',#227467);
#43390=VERTEX_POINT('',#227469);
#43391=VERTEX_POINT('',#227471);
#43392=VERTEX_POINT('',#227473);
#43393=VERTEX_POINT('',#227477);
#43394=VERTEX_POINT('',#227478);
#43395=VERTEX_POINT('',#227480);
#43396=VERTEX_POINT('',#227482);
#43397=VERTEX_POINT('',#227484);
#43398=VERTEX_POINT('',#227486);
#43399=VERTEX_POINT('',#227488);
#43400=VERTEX_POINT('',#227490);
#43401=VERTEX_POINT('',#227492);
#43402=VERTEX_POINT('',#227494);
#43403=VERTEX_POINT('',#227496);
#43404=VERTEX_POINT('',#227498);
#43405=VERTEX_POINT('',#227502);
#43406=VERTEX_POINT('',#227503);
#43407=VERTEX_POINT('',#227505);
#43408=VERTEX_POINT('',#227507);
#43409=VERTEX_POINT('',#227511);
#43410=VERTEX_POINT('',#227512);
#43411=VERTEX_POINT('',#227514);
#43412=VERTEX_POINT('',#227516);
#43413=VERTEX_POINT('',#227518);
#43414=VERTEX_POINT('',#227520);
#43415=VERTEX_POINT('',#227522);
#43416=VERTEX_POINT('',#227524);
#43417=VERTEX_POINT('',#227526);
#43418=VERTEX_POINT('',#227528);
#43419=VERTEX_POINT('',#227530);
#43420=VERTEX_POINT('',#227532);
#43421=VERTEX_POINT('',#227536);
#43422=VERTEX_POINT('',#227537);
#43423=VERTEX_POINT('',#227539);
#43424=VERTEX_POINT('',#227541);
#43425=VERTEX_POINT('',#227543);
#43426=VERTEX_POINT('',#227545);
#43427=VERTEX_POINT('',#227547);
#43428=VERTEX_POINT('',#227549);
#43429=VERTEX_POINT('',#227551);
#43430=VERTEX_POINT('',#227553);
#43431=VERTEX_POINT('',#227555);
#43432=VERTEX_POINT('',#227557);
#43433=VERTEX_POINT('',#227561);
#43434=VERTEX_POINT('',#227562);
#43435=VERTEX_POINT('',#227564);
#43436=VERTEX_POINT('',#227566);
#43437=VERTEX_POINT('',#227570);
#43438=VERTEX_POINT('',#227571);
#43439=VERTEX_POINT('',#227573);
#43440=VERTEX_POINT('',#227575);
#43441=VERTEX_POINT('',#227577);
#43442=VERTEX_POINT('',#227579);
#43443=VERTEX_POINT('',#227581);
#43444=VERTEX_POINT('',#227583);
#43445=VERTEX_POINT('',#227585);
#43446=VERTEX_POINT('',#227587);
#43447=VERTEX_POINT('',#227589);
#43448=VERTEX_POINT('',#227591);
#43449=VERTEX_POINT('',#227595);
#43450=VERTEX_POINT('',#227596);
#43451=VERTEX_POINT('',#227598);
#43452=VERTEX_POINT('',#227600);
#43453=VERTEX_POINT('',#227602);
#43454=VERTEX_POINT('',#227604);
#43455=VERTEX_POINT('',#227606);
#43456=VERTEX_POINT('',#227608);
#43457=VERTEX_POINT('',#227610);
#43458=VERTEX_POINT('',#227612);
#43459=VERTEX_POINT('',#227614);
#43460=VERTEX_POINT('',#227616);
#43461=VERTEX_POINT('',#227620);
#43462=VERTEX_POINT('',#227621);
#43463=VERTEX_POINT('',#227623);
#43464=VERTEX_POINT('',#227625);
#43465=VERTEX_POINT('',#227629);
#43466=VERTEX_POINT('',#227630);
#43467=VERTEX_POINT('',#227632);
#43468=VERTEX_POINT('',#227634);
#43469=VERTEX_POINT('',#227636);
#43470=VERTEX_POINT('',#227638);
#43471=VERTEX_POINT('',#227640);
#43472=VERTEX_POINT('',#227642);
#43473=VERTEX_POINT('',#227644);
#43474=VERTEX_POINT('',#227646);
#43475=VERTEX_POINT('',#227648);
#43476=VERTEX_POINT('',#227650);
#43477=VERTEX_POINT('',#227654);
#43478=VERTEX_POINT('',#227655);
#43479=VERTEX_POINT('',#227657);
#43480=VERTEX_POINT('',#227659);
#43481=VERTEX_POINT('',#227661);
#43482=VERTEX_POINT('',#227663);
#43483=VERTEX_POINT('',#227665);
#43484=VERTEX_POINT('',#227667);
#43485=VERTEX_POINT('',#227669);
#43486=VERTEX_POINT('',#227671);
#43487=VERTEX_POINT('',#227673);
#43488=VERTEX_POINT('',#227675);
#43489=VERTEX_POINT('',#227679);
#43490=VERTEX_POINT('',#227680);
#43491=VERTEX_POINT('',#227682);
#43492=VERTEX_POINT('',#227684);
#43493=VERTEX_POINT('',#227688);
#43494=VERTEX_POINT('',#227689);
#43495=VERTEX_POINT('',#227691);
#43496=VERTEX_POINT('',#227693);
#43497=VERTEX_POINT('',#227695);
#43498=VERTEX_POINT('',#227697);
#43499=VERTEX_POINT('',#227699);
#43500=VERTEX_POINT('',#227701);
#43501=VERTEX_POINT('',#227703);
#43502=VERTEX_POINT('',#227705);
#43503=VERTEX_POINT('',#227707);
#43504=VERTEX_POINT('',#227709);
#43505=VERTEX_POINT('',#227713);
#43506=VERTEX_POINT('',#227714);
#43507=VERTEX_POINT('',#227716);
#43508=VERTEX_POINT('',#227718);
#43509=VERTEX_POINT('',#227720);
#43510=VERTEX_POINT('',#227722);
#43511=VERTEX_POINT('',#227724);
#43512=VERTEX_POINT('',#227726);
#43513=VERTEX_POINT('',#227728);
#43514=VERTEX_POINT('',#227730);
#43515=VERTEX_POINT('',#227732);
#43516=VERTEX_POINT('',#227734);
#43517=VERTEX_POINT('',#227738);
#43518=VERTEX_POINT('',#227739);
#43519=VERTEX_POINT('',#227741);
#43520=VERTEX_POINT('',#227743);
#43521=VERTEX_POINT('',#227747);
#43522=VERTEX_POINT('',#227748);
#43523=VERTEX_POINT('',#227750);
#43524=VERTEX_POINT('',#227752);
#43525=VERTEX_POINT('',#227754);
#43526=VERTEX_POINT('',#227756);
#43527=VERTEX_POINT('',#227758);
#43528=VERTEX_POINT('',#227760);
#43529=VERTEX_POINT('',#227762);
#43530=VERTEX_POINT('',#227764);
#43531=VERTEX_POINT('',#227766);
#43532=VERTEX_POINT('',#227768);
#43533=VERTEX_POINT('',#227772);
#43534=VERTEX_POINT('',#227773);
#43535=VERTEX_POINT('',#227775);
#43536=VERTEX_POINT('',#227777);
#43537=VERTEX_POINT('',#227779);
#43538=VERTEX_POINT('',#227781);
#43539=VERTEX_POINT('',#227783);
#43540=VERTEX_POINT('',#227785);
#43541=VERTEX_POINT('',#227787);
#43542=VERTEX_POINT('',#227789);
#43543=VERTEX_POINT('',#227791);
#43544=VERTEX_POINT('',#227793);
#43545=VERTEX_POINT('',#227797);
#43546=VERTEX_POINT('',#227798);
#43547=VERTEX_POINT('',#227800);
#43548=VERTEX_POINT('',#227802);
#43549=VERTEX_POINT('',#227806);
#43550=VERTEX_POINT('',#227807);
#43551=VERTEX_POINT('',#227809);
#43552=VERTEX_POINT('',#227811);
#43553=VERTEX_POINT('',#227813);
#43554=VERTEX_POINT('',#227815);
#43555=VERTEX_POINT('',#227817);
#43556=VERTEX_POINT('',#227819);
#43557=VERTEX_POINT('',#227821);
#43558=VERTEX_POINT('',#227823);
#43559=VERTEX_POINT('',#227825);
#43560=VERTEX_POINT('',#227827);
#43561=VERTEX_POINT('',#227831);
#43562=VERTEX_POINT('',#227832);
#43563=VERTEX_POINT('',#227834);
#43564=VERTEX_POINT('',#227836);
#43565=VERTEX_POINT('',#227838);
#43566=VERTEX_POINT('',#227840);
#43567=VERTEX_POINT('',#227842);
#43568=VERTEX_POINT('',#227844);
#43569=VERTEX_POINT('',#227846);
#43570=VERTEX_POINT('',#227848);
#43571=VERTEX_POINT('',#227850);
#43572=VERTEX_POINT('',#227852);
#43573=VERTEX_POINT('',#227856);
#43574=VERTEX_POINT('',#227857);
#43575=VERTEX_POINT('',#227859);
#43576=VERTEX_POINT('',#227861);
#43577=VERTEX_POINT('',#227865);
#43578=VERTEX_POINT('',#227866);
#43579=VERTEX_POINT('',#227868);
#43580=VERTEX_POINT('',#227870);
#43581=VERTEX_POINT('',#227872);
#43582=VERTEX_POINT('',#227874);
#43583=VERTEX_POINT('',#227876);
#43584=VERTEX_POINT('',#227878);
#43585=VERTEX_POINT('',#227880);
#43586=VERTEX_POINT('',#227882);
#43587=VERTEX_POINT('',#227884);
#43588=VERTEX_POINT('',#227886);
#43589=VERTEX_POINT('',#227890);
#43590=VERTEX_POINT('',#227891);
#43591=VERTEX_POINT('',#227893);
#43592=VERTEX_POINT('',#227895);
#43593=VERTEX_POINT('',#227897);
#43594=VERTEX_POINT('',#227899);
#43595=VERTEX_POINT('',#227901);
#43596=VERTEX_POINT('',#227903);
#43597=VERTEX_POINT('',#227905);
#43598=VERTEX_POINT('',#227907);
#43599=VERTEX_POINT('',#227909);
#43600=VERTEX_POINT('',#227911);
#43601=VERTEX_POINT('',#227915);
#43602=VERTEX_POINT('',#227916);
#43603=VERTEX_POINT('',#227918);
#43604=VERTEX_POINT('',#227920);
#43605=VERTEX_POINT('',#227924);
#43606=VERTEX_POINT('',#227925);
#43607=VERTEX_POINT('',#227927);
#43608=VERTEX_POINT('',#227929);
#43609=VERTEX_POINT('',#227931);
#43610=VERTEX_POINT('',#227933);
#43611=VERTEX_POINT('',#227935);
#43612=VERTEX_POINT('',#227937);
#43613=VERTEX_POINT('',#227939);
#43614=VERTEX_POINT('',#227941);
#43615=VERTEX_POINT('',#227943);
#43616=VERTEX_POINT('',#227945);
#43617=VERTEX_POINT('',#227949);
#43618=VERTEX_POINT('',#227950);
#43619=VERTEX_POINT('',#227952);
#43620=VERTEX_POINT('',#227954);
#43621=VERTEX_POINT('',#227956);
#43622=VERTEX_POINT('',#227958);
#43623=VERTEX_POINT('',#227960);
#43624=VERTEX_POINT('',#227962);
#43625=VERTEX_POINT('',#227964);
#43626=VERTEX_POINT('',#227966);
#43627=VERTEX_POINT('',#227968);
#43628=VERTEX_POINT('',#227970);
#43629=VERTEX_POINT('',#227977);
#43630=VERTEX_POINT('',#227978);
#43631=VERTEX_POINT('',#227980);
#43632=VERTEX_POINT('',#227982);
#43633=VERTEX_POINT('',#227984);
#43634=VERTEX_POINT('',#227986);
#43635=VERTEX_POINT('',#227988);
#43636=VERTEX_POINT('',#227990);
#43637=VERTEX_POINT('',#227992);
#43638=VERTEX_POINT('',#227994);
#43639=VERTEX_POINT('',#227996);
#43640=VERTEX_POINT('',#227998);
#43641=VERTEX_POINT('',#228002);
#43642=VERTEX_POINT('',#228003);
#43643=VERTEX_POINT('',#228005);
#43644=VERTEX_POINT('',#228007);
#43645=VERTEX_POINT('',#228009);
#43646=VERTEX_POINT('',#228011);
#43647=VERTEX_POINT('',#228013);
#43648=VERTEX_POINT('',#228015);
#43649=VERTEX_POINT('',#228017);
#43650=VERTEX_POINT('',#228019);
#43651=VERTEX_POINT('',#228021);
#43652=VERTEX_POINT('',#228023);
#43653=VERTEX_POINT('',#228027);
#43654=VERTEX_POINT('',#228028);
#43655=VERTEX_POINT('',#228030);
#43656=VERTEX_POINT('',#228032);
#43657=VERTEX_POINT('',#228036);
#43658=VERTEX_POINT('',#228037);
#43659=VERTEX_POINT('',#228039);
#43660=VERTEX_POINT('',#228041);
#43661=VERTEX_POINT('',#228043);
#43662=VERTEX_POINT('',#228045);
#43663=VERTEX_POINT('',#228047);
#43664=VERTEX_POINT('',#228049);
#43665=VERTEX_POINT('',#228051);
#43666=VERTEX_POINT('',#228053);
#43667=VERTEX_POINT('',#228055);
#43668=VERTEX_POINT('',#228057);
#43669=VERTEX_POINT('',#228061);
#43670=VERTEX_POINT('',#228062);
#43671=VERTEX_POINT('',#228064);
#43672=VERTEX_POINT('',#228066);
#43673=VERTEX_POINT('',#228068);
#43674=VERTEX_POINT('',#228070);
#43675=VERTEX_POINT('',#228072);
#43676=VERTEX_POINT('',#228074);
#43677=VERTEX_POINT('',#228076);
#43678=VERTEX_POINT('',#228078);
#43679=VERTEX_POINT('',#228080);
#43680=VERTEX_POINT('',#228082);
#43681=VERTEX_POINT('',#228086);
#43682=VERTEX_POINT('',#228087);
#43683=VERTEX_POINT('',#228089);
#43684=VERTEX_POINT('',#228091);
#43685=VERTEX_POINT('',#228095);
#43686=VERTEX_POINT('',#228096);
#43687=VERTEX_POINT('',#228098);
#43688=VERTEX_POINT('',#228100);
#43689=VERTEX_POINT('',#228102);
#43690=VERTEX_POINT('',#228104);
#43691=VERTEX_POINT('',#228106);
#43692=VERTEX_POINT('',#228108);
#43693=VERTEX_POINT('',#228110);
#43694=VERTEX_POINT('',#228112);
#43695=VERTEX_POINT('',#228114);
#43696=VERTEX_POINT('',#228116);
#43697=VERTEX_POINT('',#228120);
#43698=VERTEX_POINT('',#228121);
#43699=VERTEX_POINT('',#228123);
#43700=VERTEX_POINT('',#228125);
#43701=VERTEX_POINT('',#228127);
#43702=VERTEX_POINT('',#228129);
#43703=VERTEX_POINT('',#228131);
#43704=VERTEX_POINT('',#228133);
#43705=VERTEX_POINT('',#228135);
#43706=VERTEX_POINT('',#228137);
#43707=VERTEX_POINT('',#228139);
#43708=VERTEX_POINT('',#228141);
#43709=VERTEX_POINT('',#228145);
#43710=VERTEX_POINT('',#228146);
#43711=VERTEX_POINT('',#228148);
#43712=VERTEX_POINT('',#228150);
#43713=VERTEX_POINT('',#228154);
#43714=VERTEX_POINT('',#228155);
#43715=VERTEX_POINT('',#228157);
#43716=VERTEX_POINT('',#228159);
#43717=VERTEX_POINT('',#228161);
#43718=VERTEX_POINT('',#228163);
#43719=VERTEX_POINT('',#228165);
#43720=VERTEX_POINT('',#228167);
#43721=VERTEX_POINT('',#228169);
#43722=VERTEX_POINT('',#228171);
#43723=VERTEX_POINT('',#228173);
#43724=VERTEX_POINT('',#228175);
#43725=VERTEX_POINT('',#228179);
#43726=VERTEX_POINT('',#228180);
#43727=VERTEX_POINT('',#228182);
#43728=VERTEX_POINT('',#228184);
#43729=VERTEX_POINT('',#228186);
#43730=VERTEX_POINT('',#228188);
#43731=VERTEX_POINT('',#228190);
#43732=VERTEX_POINT('',#228192);
#43733=VERTEX_POINT('',#228194);
#43734=VERTEX_POINT('',#228196);
#43735=VERTEX_POINT('',#228198);
#43736=VERTEX_POINT('',#228200);
#43737=VERTEX_POINT('',#228204);
#43738=VERTEX_POINT('',#228205);
#43739=VERTEX_POINT('',#228207);
#43740=VERTEX_POINT('',#228209);
#43741=VERTEX_POINT('',#228213);
#43742=VERTEX_POINT('',#228214);
#43743=VERTEX_POINT('',#228216);
#43744=VERTEX_POINT('',#228218);
#43745=VERTEX_POINT('',#228220);
#43746=VERTEX_POINT('',#228222);
#43747=VERTEX_POINT('',#228224);
#43748=VERTEX_POINT('',#228226);
#43749=VERTEX_POINT('',#228228);
#43750=VERTEX_POINT('',#228230);
#43751=VERTEX_POINT('',#228232);
#43752=VERTEX_POINT('',#228234);
#43753=VERTEX_POINT('',#228238);
#43754=VERTEX_POINT('',#228239);
#43755=VERTEX_POINT('',#228241);
#43756=VERTEX_POINT('',#228243);
#43757=VERTEX_POINT('',#228245);
#43758=VERTEX_POINT('',#228247);
#43759=VERTEX_POINT('',#228249);
#43760=VERTEX_POINT('',#228251);
#43761=VERTEX_POINT('',#228253);
#43762=VERTEX_POINT('',#228255);
#43763=VERTEX_POINT('',#228257);
#43764=VERTEX_POINT('',#228259);
#43765=VERTEX_POINT('',#228263);
#43766=VERTEX_POINT('',#228264);
#43767=VERTEX_POINT('',#228266);
#43768=VERTEX_POINT('',#228268);
#43769=VERTEX_POINT('',#228272);
#43770=VERTEX_POINT('',#228273);
#43771=VERTEX_POINT('',#228275);
#43772=VERTEX_POINT('',#228277);
#43773=VERTEX_POINT('',#228279);
#43774=VERTEX_POINT('',#228281);
#43775=VERTEX_POINT('',#228283);
#43776=VERTEX_POINT('',#228285);
#43777=VERTEX_POINT('',#228287);
#43778=VERTEX_POINT('',#228289);
#43779=VERTEX_POINT('',#228291);
#43780=VERTEX_POINT('',#228293);
#43781=VERTEX_POINT('',#228297);
#43782=VERTEX_POINT('',#228298);
#43783=VERTEX_POINT('',#228300);
#43784=VERTEX_POINT('',#228302);
#43785=VERTEX_POINT('',#228304);
#43786=VERTEX_POINT('',#228306);
#43787=VERTEX_POINT('',#228308);
#43788=VERTEX_POINT('',#228310);
#43789=VERTEX_POINT('',#228312);
#43790=VERTEX_POINT('',#228314);
#43791=VERTEX_POINT('',#228316);
#43792=VERTEX_POINT('',#228318);
#43793=VERTEX_POINT('',#228322);
#43794=VERTEX_POINT('',#228323);
#43795=VERTEX_POINT('',#228325);
#43796=VERTEX_POINT('',#228327);
#43797=VERTEX_POINT('',#228331);
#43798=VERTEX_POINT('',#228332);
#43799=VERTEX_POINT('',#228334);
#43800=VERTEX_POINT('',#228336);
#43801=VERTEX_POINT('',#228338);
#43802=VERTEX_POINT('',#228340);
#43803=VERTEX_POINT('',#228342);
#43804=VERTEX_POINT('',#228344);
#43805=VERTEX_POINT('',#228346);
#43806=VERTEX_POINT('',#228348);
#43807=VERTEX_POINT('',#228350);
#43808=VERTEX_POINT('',#228352);
#43809=VERTEX_POINT('',#228356);
#43810=VERTEX_POINT('',#228357);
#43811=VERTEX_POINT('',#228359);
#43812=VERTEX_POINT('',#228361);
#43813=VERTEX_POINT('',#228363);
#43814=VERTEX_POINT('',#228365);
#43815=VERTEX_POINT('',#228367);
#43816=VERTEX_POINT('',#228369);
#43817=VERTEX_POINT('',#228371);
#43818=VERTEX_POINT('',#228373);
#43819=VERTEX_POINT('',#228375);
#43820=VERTEX_POINT('',#228377);
#43821=VERTEX_POINT('',#228381);
#43822=VERTEX_POINT('',#228382);
#43823=VERTEX_POINT('',#228384);
#43824=VERTEX_POINT('',#228386);
#43825=VERTEX_POINT('',#228390);
#43826=VERTEX_POINT('',#228391);
#43827=VERTEX_POINT('',#228393);
#43828=VERTEX_POINT('',#228395);
#43829=VERTEX_POINT('',#228397);
#43830=VERTEX_POINT('',#228399);
#43831=VERTEX_POINT('',#228401);
#43832=VERTEX_POINT('',#228403);
#43833=VERTEX_POINT('',#228405);
#43834=VERTEX_POINT('',#228407);
#43835=VERTEX_POINT('',#228409);
#43836=VERTEX_POINT('',#228411);
#43837=VERTEX_POINT('',#228415);
#43838=VERTEX_POINT('',#228416);
#43839=VERTEX_POINT('',#228418);
#43840=VERTEX_POINT('',#228420);
#43841=VERTEX_POINT('',#228422);
#43842=VERTEX_POINT('',#228424);
#43843=VERTEX_POINT('',#228426);
#43844=VERTEX_POINT('',#228428);
#43845=VERTEX_POINT('',#228430);
#43846=VERTEX_POINT('',#228432);
#43847=VERTEX_POINT('',#228434);
#43848=VERTEX_POINT('',#228436);
#43849=VERTEX_POINT('',#228440);
#43850=VERTEX_POINT('',#228441);
#43851=VERTEX_POINT('',#228443);
#43852=VERTEX_POINT('',#228445);
#43853=VERTEX_POINT('',#228449);
#43854=VERTEX_POINT('',#228450);
#43855=VERTEX_POINT('',#228452);
#43856=VERTEX_POINT('',#228454);
#43857=VERTEX_POINT('',#228456);
#43858=VERTEX_POINT('',#228458);
#43859=VERTEX_POINT('',#228460);
#43860=VERTEX_POINT('',#228462);
#43861=VERTEX_POINT('',#228464);
#43862=VERTEX_POINT('',#228466);
#43863=VERTEX_POINT('',#228468);
#43864=VERTEX_POINT('',#228470);
#43865=VERTEX_POINT('',#228474);
#43866=VERTEX_POINT('',#228475);
#43867=VERTEX_POINT('',#228477);
#43868=VERTEX_POINT('',#228479);
#43869=VERTEX_POINT('',#228481);
#43870=VERTEX_POINT('',#228483);
#43871=VERTEX_POINT('',#228485);
#43872=VERTEX_POINT('',#228487);
#43873=VERTEX_POINT('',#228489);
#43874=VERTEX_POINT('',#228491);
#43875=VERTEX_POINT('',#228493);
#43876=VERTEX_POINT('',#228495);
#43877=VERTEX_POINT('',#228499);
#43878=VERTEX_POINT('',#228500);
#43879=VERTEX_POINT('',#228502);
#43880=VERTEX_POINT('',#228504);
#43881=VERTEX_POINT('',#228508);
#43882=VERTEX_POINT('',#228509);
#43883=VERTEX_POINT('',#228511);
#43884=VERTEX_POINT('',#228513);
#43885=VERTEX_POINT('',#228515);
#43886=VERTEX_POINT('',#228517);
#43887=VERTEX_POINT('',#228519);
#43888=VERTEX_POINT('',#228521);
#43889=VERTEX_POINT('',#228523);
#43890=VERTEX_POINT('',#228525);
#43891=VERTEX_POINT('',#228527);
#43892=VERTEX_POINT('',#228529);
#43893=VERTEX_POINT('',#228533);
#43894=VERTEX_POINT('',#228534);
#43895=VERTEX_POINT('',#228536);
#43896=VERTEX_POINT('',#228538);
#43897=VERTEX_POINT('',#228540);
#43898=VERTEX_POINT('',#228542);
#43899=VERTEX_POINT('',#228544);
#43900=VERTEX_POINT('',#228546);
#43901=VERTEX_POINT('',#228548);
#43902=VERTEX_POINT('',#228550);
#43903=VERTEX_POINT('',#228552);
#43904=VERTEX_POINT('',#228554);
#43905=VERTEX_POINT('',#228558);
#43906=VERTEX_POINT('',#228559);
#43907=VERTEX_POINT('',#228561);
#43908=VERTEX_POINT('',#228563);
#43909=VERTEX_POINT('',#228567);
#43910=VERTEX_POINT('',#228568);
#43911=VERTEX_POINT('',#228570);
#43912=VERTEX_POINT('',#228572);
#43913=VERTEX_POINT('',#228574);
#43914=VERTEX_POINT('',#228576);
#43915=VERTEX_POINT('',#228578);
#43916=VERTEX_POINT('',#228580);
#43917=VERTEX_POINT('',#228582);
#43918=VERTEX_POINT('',#228584);
#43919=VERTEX_POINT('',#228586);
#43920=VERTEX_POINT('',#228588);
#43921=VERTEX_POINT('',#228592);
#43922=VERTEX_POINT('',#228593);
#43923=VERTEX_POINT('',#228595);
#43924=VERTEX_POINT('',#228597);
#43925=VERTEX_POINT('',#228599);
#43926=VERTEX_POINT('',#228601);
#43927=VERTEX_POINT('',#228603);
#43928=VERTEX_POINT('',#228605);
#43929=VERTEX_POINT('',#228607);
#43930=VERTEX_POINT('',#228609);
#43931=VERTEX_POINT('',#228611);
#43932=VERTEX_POINT('',#228613);
#43933=VERTEX_POINT('',#228617);
#43934=VERTEX_POINT('',#228618);
#43935=VERTEX_POINT('',#228620);
#43936=VERTEX_POINT('',#228622);
#43937=VERTEX_POINT('',#228626);
#43938=VERTEX_POINT('',#228627);
#43939=VERTEX_POINT('',#228629);
#43940=VERTEX_POINT('',#228631);
#43941=VERTEX_POINT('',#228633);
#43942=VERTEX_POINT('',#228635);
#43943=VERTEX_POINT('',#228637);
#43944=VERTEX_POINT('',#228639);
#43945=VERTEX_POINT('',#228641);
#43946=VERTEX_POINT('',#228643);
#43947=VERTEX_POINT('',#228645);
#43948=VERTEX_POINT('',#228647);
#43949=VERTEX_POINT('',#228651);
#43950=VERTEX_POINT('',#228652);
#43951=VERTEX_POINT('',#228654);
#43952=VERTEX_POINT('',#228656);
#43953=VERTEX_POINT('',#228658);
#43954=VERTEX_POINT('',#228660);
#43955=VERTEX_POINT('',#228662);
#43956=VERTEX_POINT('',#228664);
#43957=VERTEX_POINT('',#228666);
#43958=VERTEX_POINT('',#228668);
#43959=VERTEX_POINT('',#228670);
#43960=VERTEX_POINT('',#228672);
#43961=VERTEX_POINT('',#228676);
#43962=VERTEX_POINT('',#228677);
#43963=VERTEX_POINT('',#228679);
#43964=VERTEX_POINT('',#228681);
#43965=VERTEX_POINT('',#228685);
#43966=VERTEX_POINT('',#228686);
#43967=VERTEX_POINT('',#228688);
#43968=VERTEX_POINT('',#228690);
#43969=VERTEX_POINT('',#228692);
#43970=VERTEX_POINT('',#228694);
#43971=VERTEX_POINT('',#228696);
#43972=VERTEX_POINT('',#228698);
#43973=VERTEX_POINT('',#228700);
#43974=VERTEX_POINT('',#228702);
#43975=VERTEX_POINT('',#228704);
#43976=VERTEX_POINT('',#228706);
#43977=VERTEX_POINT('',#228710);
#43978=VERTEX_POINT('',#228711);
#43979=VERTEX_POINT('',#228713);
#43980=VERTEX_POINT('',#228715);
#43981=VERTEX_POINT('',#228717);
#43982=VERTEX_POINT('',#228719);
#43983=VERTEX_POINT('',#228721);
#43984=VERTEX_POINT('',#228723);
#43985=VERTEX_POINT('',#228725);
#43986=VERTEX_POINT('',#228727);
#43987=VERTEX_POINT('',#228729);
#43988=VERTEX_POINT('',#228731);
#43989=VERTEX_POINT('',#228735);
#43990=VERTEX_POINT('',#228736);
#43991=VERTEX_POINT('',#228738);
#43992=VERTEX_POINT('',#228740);
#43993=VERTEX_POINT('',#228744);
#43994=VERTEX_POINT('',#228745);
#43995=VERTEX_POINT('',#228747);
#43996=VERTEX_POINT('',#228749);
#43997=VERTEX_POINT('',#228751);
#43998=VERTEX_POINT('',#228753);
#43999=VERTEX_POINT('',#228755);
#44000=VERTEX_POINT('',#228757);
#44001=VERTEX_POINT('',#228759);
#44002=VERTEX_POINT('',#228761);
#44003=VERTEX_POINT('',#228763);
#44004=VERTEX_POINT('',#228765);
#44005=VERTEX_POINT('',#228769);
#44006=VERTEX_POINT('',#228770);
#44007=VERTEX_POINT('',#228772);
#44008=VERTEX_POINT('',#228774);
#44009=VERTEX_POINT('',#228776);
#44010=VERTEX_POINT('',#228778);
#44011=VERTEX_POINT('',#228780);
#44012=VERTEX_POINT('',#228782);
#44013=VERTEX_POINT('',#228784);
#44014=VERTEX_POINT('',#228786);
#44015=VERTEX_POINT('',#228788);
#44016=VERTEX_POINT('',#228790);
#44017=VERTEX_POINT('',#228794);
#44018=VERTEX_POINT('',#228795);
#44019=VERTEX_POINT('',#228797);
#44020=VERTEX_POINT('',#228799);
#44021=VERTEX_POINT('',#228803);
#44022=VERTEX_POINT('',#228804);
#44023=VERTEX_POINT('',#228806);
#44024=VERTEX_POINT('',#228808);
#44025=VERTEX_POINT('',#228810);
#44026=VERTEX_POINT('',#228812);
#44027=VERTEX_POINT('',#228814);
#44028=VERTEX_POINT('',#228816);
#44029=VERTEX_POINT('',#228818);
#44030=VERTEX_POINT('',#228820);
#44031=VERTEX_POINT('',#228822);
#44032=VERTEX_POINT('',#228824);
#44033=VERTEX_POINT('',#228828);
#44034=VERTEX_POINT('',#228829);
#44035=VERTEX_POINT('',#228831);
#44036=VERTEX_POINT('',#228833);
#44037=VERTEX_POINT('',#228835);
#44038=VERTEX_POINT('',#228837);
#44039=VERTEX_POINT('',#228839);
#44040=VERTEX_POINT('',#228841);
#44041=VERTEX_POINT('',#228843);
#44042=VERTEX_POINT('',#228845);
#44043=VERTEX_POINT('',#228847);
#44044=VERTEX_POINT('',#228849);
#44045=VERTEX_POINT('',#253385);
#44046=VERTEX_POINT('',#253387);
#44047=VERTEX_POINT('',#253391);
#44048=VERTEX_POINT('',#253393);
#44049=VERTEX_POINT('',#253397);
#44050=VERTEX_POINT('',#253399);
#44051=VERTEX_POINT('',#253401);
#44052=VERTEX_POINT('',#253405);
#44053=VERTEX_POINT('',#253411);
#44054=VERTEX_POINT('',#253413);
#44055=VERTEX_POINT('',#253420);
#44056=VERTEX_POINT('',#253422);
#44057=VERTEX_POINT('',#253426);
#44058=VERTEX_POINT('',#253428);
#44059=VERTEX_POINT('',#253432);
#44060=VERTEX_POINT('',#253436);
#44061=VERTEX_POINT('',#253442);
#44062=VERTEX_POINT('',#253444);
#44063=VERTEX_POINT('',#253448);
#44064=VERTEX_POINT('',#253449);
#44065=VERTEX_POINT('',#253451);
#44066=VERTEX_POINT('',#253453);
#44067=VERTEX_POINT('',#253457);
#44068=VERTEX_POINT('',#253458);
#44069=VERTEX_POINT('',#253460);
#44070=VERTEX_POINT('',#253462);
#44071=VERTEX_POINT('',#253466);
#44072=VERTEX_POINT('',#253467);
#44073=VERTEX_POINT('',#253469);
#44074=VERTEX_POINT('',#253471);
#44075=VERTEX_POINT('',#253483);
#44076=VERTEX_POINT('',#253484);
#44077=VERTEX_POINT('',#253486);
#44078=VERTEX_POINT('',#253488);
#44079=VERTEX_POINT('',#253500);
#44080=VERTEX_POINT('',#253501);
#44081=VERTEX_POINT('',#253503);
#44082=VERTEX_POINT('',#253505);
#44083=VERTEX_POINT('',#253517);
#44084=VERTEX_POINT('',#253518);
#44085=VERTEX_POINT('',#253520);
#44086=VERTEX_POINT('',#253522);
#44087=VERTEX_POINT('',#253526);
#44088=VERTEX_POINT('',#253528);
#44089=VERTEX_POINT('',#253540);
#44090=VERTEX_POINT('',#253542);
#44091=VERTEX_POINT('',#253546);
#44092=VERTEX_POINT('',#253548);
#44093=VERTEX_POINT('',#253550);
#44094=VERTEX_POINT('',#253555);
#44095=VERTEX_POINT('',#253580);
#44096=VERTEX_POINT('',#253582);
#44097=VERTEX_POINT('',#253605);
#44098=VERTEX_POINT('',#253628);
#44099=VERTEX_POINT('',#253632);
#44100=VERTEX_POINT('',#253633);
#44101=VERTEX_POINT('',#253645);
#44102=VERTEX_POINT('',#253647);
#44103=VERTEX_POINT('',#253651);
#44104=VERTEX_POINT('',#253653);
#44105=VERTEX_POINT('',#253657);
#44106=VERTEX_POINT('',#253659);
#44107=VERTEX_POINT('',#253663);
#44108=VERTEX_POINT('',#253665);
#44109=VERTEX_POINT('',#253669);
#44110=VERTEX_POINT('',#253671);
#44111=VERTEX_POINT('',#253675);
#44112=VERTEX_POINT('',#253677);
#44113=VERTEX_POINT('',#253681);
#44114=VERTEX_POINT('',#253692);
#44115=VERTEX_POINT('',#253694);
#44116=VERTEX_POINT('',#253699);
#44117=VERTEX_POINT('',#253755);
#44118=VERTEX_POINT('',#253757);
#44119=VERTEX_POINT('',#253811);
#44120=VERTEX_POINT('',#253816);
#44121=VERTEX_POINT('',#253872);
#44122=VERTEX_POINT('',#253874);
#44123=VERTEX_POINT('',#253924);
#44124=VERTEX_POINT('',#253929);
#44125=VERTEX_POINT('',#253931);
#44126=VERTEX_POINT('',#253936);
#44127=VERTEX_POINT('',#253992);
#44128=VERTEX_POINT('',#253994);
#44129=VERTEX_POINT('',#254044);
#44130=VERTEX_POINT('',#254049);
#44131=VERTEX_POINT('',#254051);
#44132=VERTEX_POINT('',#254056);
#44133=VERTEX_POINT('',#254106);
#44134=VERTEX_POINT('',#254108);
#44135=VERTEX_POINT('',#254158);
#44136=VERTEX_POINT('',#254163);
#44137=VERTEX_POINT('',#254176);
#44138=VERTEX_POINT('',#254177);
#44139=VERTEX_POINT('',#254179);
#44140=VERTEX_POINT('',#254181);
#44141=VERTEX_POINT('',#254183);
#44142=VERTEX_POINT('',#254190);
#44143=VERTEX_POINT('',#254192);
#44144=VERTEX_POINT('',#254194);
#44145=VERTEX_POINT('',#254196);
#44146=VERTEX_POINT('',#254249);
#44147=VERTEX_POINT('',#254253);
#44148=VERTEX_POINT('',#254254);
#44149=VERTEX_POINT('',#254256);
#44150=VERTEX_POINT('',#254258);
#44151=VERTEX_POINT('',#254260);
#44152=VERTEX_POINT('',#254319);
#44153=VERTEX_POINT('',#254321);
#44154=VERTEX_POINT('',#254323);
#44155=VERTEX_POINT('',#254325);
#44156=VERTEX_POINT('',#254378);
#44157=VERTEX_POINT('',#254382);
#44158=VERTEX_POINT('',#254383);
#44159=VERTEX_POINT('',#254391);
#44160=VERTEX_POINT('',#254392);
#44161=VERTEX_POINT('',#254394);
#44162=VERTEX_POINT('',#254396);
#44163=VERTEX_POINT('',#254400);
#44164=VERTEX_POINT('',#254402);
#44165=VERTEX_POINT('',#254404);
#44166=VERTEX_POINT('',#254465);
#44167=VERTEX_POINT('',#254520);
#44168=VERTEX_POINT('',#254522);
#44169=VERTEX_POINT('',#254524);
#44170=VERTEX_POINT('',#254584);
#44171=VERTEX_POINT('',#254586);
#44172=VERTEX_POINT('',#254588);
#44173=VERTEX_POINT('',#254597);
#44174=VERTEX_POINT('',#254598);
#44175=VERTEX_POINT('',#254661);
#44176=VERTEX_POINT('',#254662);
#44177=VERTEX_POINT('',#254664);
#44178=VERTEX_POINT('',#254666);
#44179=VERTEX_POINT('',#254670);
#44180=VERTEX_POINT('',#254672);
#44181=VERTEX_POINT('',#254676);
#44182=VERTEX_POINT('',#254678);
#44183=VERTEX_POINT('',#254682);
#44184=VERTEX_POINT('',#254684);
#44185=VERTEX_POINT('',#254688);
#44186=VERTEX_POINT('',#254690);
#44187=VERTEX_POINT('',#254694);
#44188=VERTEX_POINT('',#254696);
#44189=VERTEX_POINT('',#254700);
#44190=VERTEX_POINT('',#254702);
#44191=VERTEX_POINT('',#254709);
#44192=VERTEX_POINT('',#254756);
#44193=VERTEX_POINT('',#254758);
#44194=VERTEX_POINT('',#254760);
#44195=VERTEX_POINT('',#254809);
#44196=VERTEX_POINT('',#254810);
#44197=VERTEX_POINT('',#254815);
#44198=VERTEX_POINT('',#254817);
#44199=VERTEX_POINT('',#254819);
#44200=VERTEX_POINT('',#254830);
#44201=VERTEX_POINT('',#254838);
#44202=VERTEX_POINT('',#254845);
#44203=VERTEX_POINT('',#254849);
#44204=VERTEX_POINT('',#254850);
#44205=VERTEX_POINT('',#254852);
#44206=VERTEX_POINT('',#254854);
#44207=VERTEX_POINT('',#254859);
#44208=VERTEX_POINT('',#254861);
#44209=VERTEX_POINT('',#254863);
#44210=VERTEX_POINT('',#254870);
#44211=VERTEX_POINT('',#254963);
#44212=VERTEX_POINT('',#254970);
#44213=VERTEX_POINT('',#254994);
#44214=VERTEX_POINT('',#254995);
#44215=VERTEX_POINT('',#254997);
#44216=VERTEX_POINT('',#254999);
#44217=VERTEX_POINT('',#255003);
#44218=VERTEX_POINT('',#255005);
#44219=VERTEX_POINT('',#255023);
#44220=VERTEX_POINT('',#255027);
#44221=VERTEX_POINT('',#255028);
#44222=VERTEX_POINT('',#255030);
#44223=VERTEX_POINT('',#255045);
#44224=VERTEX_POINT('',#255047);
#44225=VERTEX_POINT('',#255051);
#44226=VERTEX_POINT('',#255052);
#44227=VERTEX_POINT('',#255057);
#44228=VERTEX_POINT('',#255058);
#44229=VERTEX_POINT('',#255060);
#44230=VERTEX_POINT('',#255062);
#44231=VERTEX_POINT('',#255068);
#44232=VERTEX_POINT('',#255069);
#44233=VERTEX_POINT('',#255071);
#44234=VERTEX_POINT('',#255073);
#44235=VERTEX_POINT('',#255077);
#44236=VERTEX_POINT('',#255078);
#44237=VERTEX_POINT('',#255080);
#44238=VERTEX_POINT('',#255082);
#44239=VERTEX_POINT('',#255086);
#44240=VERTEX_POINT('',#255088);
#44241=VERTEX_POINT('',#255092);
#44242=VERTEX_POINT('',#255094);
#44243=VERTEX_POINT('',#255098);
#44244=VERTEX_POINT('',#255100);
#44245=VERTEX_POINT('',#255153);
#44246=VERTEX_POINT('',#255163);
#44247=VERTEX_POINT('',#255165);
#44248=VERTEX_POINT('',#255173);
#44249=VERTEX_POINT('',#255225);
#44250=VERTEX_POINT('',#255278);
#44251=VERTEX_POINT('',#255289);
#44252=VERTEX_POINT('',#255290);
#44253=VERTEX_POINT('',#255292);
#44254=VERTEX_POINT('',#255294);
#44255=VERTEX_POINT('',#255300);
#44256=VERTEX_POINT('',#255302);
#44257=VERTEX_POINT('',#255361);
#44258=VERTEX_POINT('',#255362);
#44259=VERTEX_POINT('',#255364);
#44260=VERTEX_POINT('',#255417);
#44261=VERTEX_POINT('',#255428);
#44262=VERTEX_POINT('',#255429);
#44263=VERTEX_POINT('',#255431);
#44264=VERTEX_POINT('',#255433);
#44265=VERTEX_POINT('',#255435);
#44266=VERTEX_POINT('',#255437);
#44267=VERTEX_POINT('',#255439);
#44268=VERTEX_POINT('',#255441);
#44269=VERTEX_POINT('',#255445);
#44270=VERTEX_POINT('',#255447);
#44271=VERTEX_POINT('',#255455);
#44272=VERTEX_POINT('',#255505);
#44273=VERTEX_POINT('',#255509);
#44274=VERTEX_POINT('',#255511);
#44275=VERTEX_POINT('',#255564);
#44276=VERTEX_POINT('',#255575);
#44277=VERTEX_POINT('',#255576);
#44278=VERTEX_POINT('',#255578);
#44279=VERTEX_POINT('',#255580);
#44280=VERTEX_POINT('',#255585);
#44281=VERTEX_POINT('',#255587);
#44282=VERTEX_POINT('',#255625);
#44283=VERTEX_POINT('',#255707);
#44284=VERTEX_POINT('',#255720);
#44285=VERTEX_POINT('',#255802);
#44286=VERTEX_POINT('',#255815);
#44287=VERTEX_POINT('',#255896);
#44288=VERTEX_POINT('',#255909);
#44289=VERTEX_POINT('',#255920);
#44290=VERTEX_POINT('',#255954);
#44291=VERTEX_POINT('',#255967);
#44292=VERTEX_POINT('',#256048);
#44293=VERTEX_POINT('',#256061);
#44294=VERTEX_POINT('',#256142);
#44295=VERTEX_POINT('',#256166);
#44296=VERTEX_POINT('',#256190);
#44297=VERTEX_POINT('',#257718);
#44298=VERTEX_POINT('',#257952);
#44299=VERTEX_POINT('',#258186);
#44300=VERTEX_POINT('',#258420);
#44301=VERTEX_POINT('',#258654);
#44302=VERTEX_POINT('',#258882);
#44303=VERTEX_POINT('',#258896);
#44304=VERTEX_POINT('',#259067);
#44305=VERTEX_POINT('',#259304);
#44306=VERTEX_POINT('',#260910);
#44307=VERTEX_POINT('',#260911);
#44308=VERTEX_POINT('',#260914);
#44309=VERTEX_POINT('',#260915);
#44310=VERTEX_POINT('',#260917);
#44311=VERTEX_POINT('',#260922);
#44312=VERTEX_POINT('',#260923);
#44313=VERTEX_POINT('',#260925);
#44314=VERTEX_POINT('',#260995);
#44315=VERTEX_POINT('',#260996);
#44316=VERTEX_POINT('',#261223);
#44317=VERTEX_POINT('',#261225);
#44318=VERTEX_POINT('',#261263);
#44319=VERTEX_POINT('',#261265);
#44320=VERTEX_POINT('',#261274);
#44321=VERTEX_POINT('',#261325);
#44322=VERTEX_POINT('',#261327);
#44323=VERTEX_POINT('',#261413);
#44324=VERTEX_POINT('',#261477);
#44325=VERTEX_POINT('',#261478);
#44326=VERTEX_POINT('',#261480);
#44327=VERTEX_POINT('',#261485);
#44328=VERTEX_POINT('',#261487);
#44329=VERTEX_POINT('',#261489);
#44330=VERTEX_POINT('',#261493);
#44331=VERTEX_POINT('',#261528);
#44332=VERTEX_POINT('',#261530);
#44333=VERTEX_POINT('',#261569);
#44334=VERTEX_POINT('',#261573);
#44335=VERTEX_POINT('',#261579);
#44336=VERTEX_POINT('',#261581);
#44337=VERTEX_POINT('',#261585);
#44338=VERTEX_POINT('',#261587);
#44339=VERTEX_POINT('',#261589);
#44340=VERTEX_POINT('',#261593);
#44341=VERTEX_POINT('',#261594);
#44342=VERTEX_POINT('',#261597);
#44343=VERTEX_POINT('',#261601);
#44344=VERTEX_POINT('',#261603);
#44345=VERTEX_POINT('',#261607);
#44346=VERTEX_POINT('',#261609);
#44347=VERTEX_POINT('',#261613);
#44348=VERTEX_POINT('',#261615);
#44349=VERTEX_POINT('',#261623);
#44350=VERTEX_POINT('',#261627);
#44351=VERTEX_POINT('',#261631);
#44352=VERTEX_POINT('',#261633);
#44353=VERTEX_POINT('',#261642);
#44354=VERTEX_POINT('',#261643);
#44355=VERTEX_POINT('',#261645);
#44356=VERTEX_POINT('',#261661);
#44357=VERTEX_POINT('',#261679);
#44358=VERTEX_POINT('',#261680);
#44359=VERTEX_POINT('',#261717);
#44360=VERTEX_POINT('',#261718);
#44361=VERTEX_POINT('',#261755);
#44362=VERTEX_POINT('',#261756);
#44363=VERTEX_POINT('',#261793);
#44364=VERTEX_POINT('',#261794);
#44365=VERTEX_POINT('',#261831);
#44366=VERTEX_POINT('',#261832);
#44367=VERTEX_POINT('',#261869);
#44368=VERTEX_POINT('',#261870);
#44369=VERTEX_POINT('',#261872);
#44370=VERTEX_POINT('',#261885);
#44371=VERTEX_POINT('',#261886);
#44372=VERTEX_POINT('',#261924);
#44373=VERTEX_POINT('',#261939);
#44374=VERTEX_POINT('',#261940);
#44375=VERTEX_POINT('',#262015);
#44376=VERTEX_POINT('',#262016);
#44377=VERTEX_POINT('',#262091);
#44378=VERTEX_POINT('',#262092);
#44379=VERTEX_POINT('',#262167);
#44380=VERTEX_POINT('',#262168);
#44381=VERTEX_POINT('',#262243);
#44382=VERTEX_POINT('',#262244);
#44383=VERTEX_POINT('',#262321);
#44384=VERTEX_POINT('',#262322);
#44385=VERTEX_POINT('',#262324);
#44386=VERTEX_POINT('',#262387);
#44387=VERTEX_POINT('',#262389);
#44388=VERTEX_POINT('',#262392);
#44389=VERTEX_POINT('',#262396);
#44390=VERTEX_POINT('',#262397);
#44391=VERTEX_POINT('',#262402);
#44392=VERTEX_POINT('',#262428);
#44393=VERTEX_POINT('',#262429);
#44394=VERTEX_POINT('',#262431);
#44395=VERTEX_POINT('',#262433);
#44396=VERTEX_POINT('',#262435);
#44397=VERTEX_POINT('',#262437);
#44398=VERTEX_POINT('',#262465);
#44399=VERTEX_POINT('',#262466);
#44400=VERTEX_POINT('',#262468);
#44401=VERTEX_POINT('',#262470);
#44402=VERTEX_POINT('',#262472);
#44403=VERTEX_POINT('',#262474);
#44404=VERTEX_POINT('',#263169);
#44405=VERTEX_POINT('',#263170);
#44406=VERTEX_POINT('',#263172);
#44407=VERTEX_POINT('',#263188);
#44408=VERTEX_POINT('',#263206);
#44409=VERTEX_POINT('',#263207);
#44410=VERTEX_POINT('',#263244);
#44411=VERTEX_POINT('',#263245);
#44412=VERTEX_POINT('',#263282);
#44413=VERTEX_POINT('',#263283);
#44414=VERTEX_POINT('',#263320);
#44415=VERTEX_POINT('',#263321);
#44416=VERTEX_POINT('',#263358);
#44417=VERTEX_POINT('',#263359);
#44418=VERTEX_POINT('',#263396);
#44419=VERTEX_POINT('',#263397);
#44420=VERTEX_POINT('',#263399);
#44421=VERTEX_POINT('',#263412);
#44422=VERTEX_POINT('',#263413);
#44423=VERTEX_POINT('',#263451);
#44424=VERTEX_POINT('',#263466);
#44425=VERTEX_POINT('',#263467);
#44426=VERTEX_POINT('',#263542);
#44427=VERTEX_POINT('',#263543);
#44428=VERTEX_POINT('',#263618);
#44429=VERTEX_POINT('',#263619);
#44430=VERTEX_POINT('',#263694);
#44431=VERTEX_POINT('',#263695);
#44432=VERTEX_POINT('',#263770);
#44433=VERTEX_POINT('',#263771);
#44434=VERTEX_POINT('',#263848);
#44435=VERTEX_POINT('',#263849);
#44436=VERTEX_POINT('',#263851);
#44437=VERTEX_POINT('',#263914);
#44438=VERTEX_POINT('',#263916);
#44439=VERTEX_POINT('',#263919);
#44440=VERTEX_POINT('',#263923);
#44441=VERTEX_POINT('',#263924);
#44442=VERTEX_POINT('',#263929);
#44443=VERTEX_POINT('',#263955);
#44444=VERTEX_POINT('',#263956);
#44445=VERTEX_POINT('',#263958);
#44446=VERTEX_POINT('',#263960);
#44447=VERTEX_POINT('',#263962);
#44448=VERTEX_POINT('',#263964);
#44449=VERTEX_POINT('',#263992);
#44450=VERTEX_POINT('',#263993);
#44451=VERTEX_POINT('',#263995);
#44452=VERTEX_POINT('',#263997);
#44453=VERTEX_POINT('',#263999);
#44454=VERTEX_POINT('',#264001);
#44455=VERTEX_POINT('',#264696);
#44456=VERTEX_POINT('',#264698);
#44457=VERTEX_POINT('',#264702);
#44458=VERTEX_POINT('',#264703);
#44459=VERTEX_POINT('',#264706);
#44460=VERTEX_POINT('',#264710);
#44461=VERTEX_POINT('',#264712);
#44462=VERTEX_POINT('',#264716);
#44463=VERTEX_POINT('',#264717);
#44464=VERTEX_POINT('',#264720);
#44465=VERTEX_POINT('',#264724);
#44466=VERTEX_POINT('',#264726);
#44467=VERTEX_POINT('',#264765);
#44468=VERTEX_POINT('',#264766);
#44469=VERTEX_POINT('',#264805);
#44470=VERTEX_POINT('',#264842);
#44471=VERTEX_POINT('',#264844);
#44472=VERTEX_POINT('',#264888);
#44473=VERTEX_POINT('',#264890);
#44474=VERTEX_POINT('',#264894);
#44475=VERTEX_POINT('',#264896);
#44476=VERTEX_POINT('',#264900);
#44477=VERTEX_POINT('',#264902);
#44478=VERTEX_POINT('',#264904);
#44479=VERTEX_POINT('',#264908);
#44480=VERTEX_POINT('',#264912);
#44481=VERTEX_POINT('',#264913);
#44482=VERTEX_POINT('',#264915);
#44483=VERTEX_POINT('',#264917);
#44484=VERTEX_POINT('',#264921);
#44485=VERTEX_POINT('',#264923);
#44486=VERTEX_POINT('',#264927);
#44487=VERTEX_POINT('',#264929);
#44488=VERTEX_POINT('',#264933);
#44489=VERTEX_POINT('',#264935);
#44490=VERTEX_POINT('',#264939);
#44491=VERTEX_POINT('',#264941);
#44492=VERTEX_POINT('',#264945);
#44493=VERTEX_POINT('',#264947);
#44494=VERTEX_POINT('',#264951);
#44495=VERTEX_POINT('',#264953);
#44496=VERTEX_POINT('',#264957);
#44497=VERTEX_POINT('',#264959);
#44498=VERTEX_POINT('',#264963);
#44499=VERTEX_POINT('',#264965);
#44500=VERTEX_POINT('',#264969);
#44501=VERTEX_POINT('',#264971);
#44502=VERTEX_POINT('',#264975);
#44503=VERTEX_POINT('',#264977);
#44504=VERTEX_POINT('',#264981);
#44505=VERTEX_POINT('',#264982);
#44506=VERTEX_POINT('',#264984);
#44507=VERTEX_POINT('',#264986);
#44508=VERTEX_POINT('',#264990);
#44509=VERTEX_POINT('',#264992);
#44510=VERTEX_POINT('',#264996);
#44511=VERTEX_POINT('',#264998);
#44512=VERTEX_POINT('',#265002);
#44513=VERTEX_POINT('',#265004);
#44514=VERTEX_POINT('',#265008);
#44515=VERTEX_POINT('',#265010);
#44516=VERTEX_POINT('',#265014);
#44517=VERTEX_POINT('',#265016);
#44518=VERTEX_POINT('',#265020);
#44519=VERTEX_POINT('',#265022);
#44520=VERTEX_POINT('',#265029);
#44521=VERTEX_POINT('',#265030);
#44522=VERTEX_POINT('',#265032);
#44523=VERTEX_POINT('',#265034);
#44524=VERTEX_POINT('',#265036);
#44525=VERTEX_POINT('',#265038);
#44526=VERTEX_POINT('',#265040);
#44527=VERTEX_POINT('',#265042);
#44528=VERTEX_POINT('',#265050);
#44529=VERTEX_POINT('',#265051);
#44530=VERTEX_POINT('',#265053);
#44531=VERTEX_POINT('',#265055);
#44532=VERTEX_POINT('',#265057);
#44533=VERTEX_POINT('',#265059);
#44534=VERTEX_POINT('',#265061);
#44535=VERTEX_POINT('',#265063);
#44536=VERTEX_POINT('',#265067);
#44537=VERTEX_POINT('',#265069);
#44538=VERTEX_POINT('',#265073);
#44539=VERTEX_POINT('',#265077);
#44540=VERTEX_POINT('',#265081);
#44541=VERTEX_POINT('',#265085);
#44542=VERTEX_POINT('',#265089);
#44543=VERTEX_POINT('',#265093);
#44544=VERTEX_POINT('',#265116);
#44545=VERTEX_POINT('',#265117);
#44546=VERTEX_POINT('',#265119);
#44547=VERTEX_POINT('',#265121);
#44548=VERTEX_POINT('',#265125);
#44549=VERTEX_POINT('',#265127);
#44550=VERTEX_POINT('',#265130);
#44551=VERTEX_POINT('',#265132);
#44552=VERTEX_POINT('',#265139);
#44553=VERTEX_POINT('',#265141);
#44554=VERTEX_POINT('',#265149);
#44555=VERTEX_POINT('',#265151);
#44556=VERTEX_POINT('',#265322);
#44557=VERTEX_POINT('',#265323);
#44558=VERTEX_POINT('',#265332);
#44559=VERTEX_POINT('',#265338);
#44560=VERTEX_POINT('',#265509);
#44561=VERTEX_POINT('',#265511);
#44562=VERTEX_POINT('',#265680);
#44563=VERTEX_POINT('',#265689);
#44564=VERTEX_POINT('',#266026);
#44565=VERTEX_POINT('',#266027);
#44566=VERTEX_POINT('',#266036);
#44567=VERTEX_POINT('',#266044);
#44568=VERTEX_POINT('',#266213);
#44569=VERTEX_POINT('',#266215);
#44570=VERTEX_POINT('',#266386);
#44571=VERTEX_POINT('',#266395);
#44572=VERTEX_POINT('',#266569);
#44573=VERTEX_POINT('',#266571);
#44574=VERTEX_POINT('',#266575);
#44575=VERTEX_POINT('',#266578);
#44576=VERTEX_POINT('',#266613);
#44577=VERTEX_POINT('',#266616);
#44578=VERTEX_POINT('',#266617);
#44579=VERTEX_POINT('',#266624);
#44580=VERTEX_POINT('',#266635);
#44581=VERTEX_POINT('',#266653);
#44582=VERTEX_POINT('',#266654);
#44583=VERTEX_POINT('',#266674);
#44584=VERTEX_POINT('',#266695);
#44585=VERTEX_POINT('',#266696);
#44586=VERTEX_POINT('',#266703);
#44587=VERTEX_POINT('',#266714);
#44588=VERTEX_POINT('',#266732);
#44589=VERTEX_POINT('',#266733);
#44590=VERTEX_POINT('',#266752);
#44591=VERTEX_POINT('',#266774);
#44592=VERTEX_POINT('',#266775);
#44593=VERTEX_POINT('',#266786);
#44594=VERTEX_POINT('',#266793);
#44595=VERTEX_POINT('',#266811);
#44596=VERTEX_POINT('',#266812);
#44597=VERTEX_POINT('',#266831);
#44598=VERTEX_POINT('',#266853);
#44599=VERTEX_POINT('',#266854);
#44600=VERTEX_POINT('',#266865);
#44601=VERTEX_POINT('',#266872);
#44602=VERTEX_POINT('',#266890);
#44603=VERTEX_POINT('',#266891);
#44604=VERTEX_POINT('',#266910);
#44605=VERTEX_POINT('',#266932);
#44606=VERTEX_POINT('',#266933);
#44607=VERTEX_POINT('',#266940);
#44608=VERTEX_POINT('',#266951);
#44609=VERTEX_POINT('',#266968);
#44610=VERTEX_POINT('',#266969);
#44611=VERTEX_POINT('',#266980);
#44612=VERTEX_POINT('',#266987);
#44613=VERTEX_POINT('',#267005);
#44614=VERTEX_POINT('',#267006);
#44615=VERTEX_POINT('',#267026);
#44616=VERTEX_POINT('',#267047);
#44617=VERTEX_POINT('',#267048);
#44618=VERTEX_POINT('',#267055);
#44619=VERTEX_POINT('',#267066);
#44620=VERTEX_POINT('',#267083);
#44621=VERTEX_POINT('',#267084);
#44622=VERTEX_POINT('',#267095);
#44623=VERTEX_POINT('',#267102);
#44624=VERTEX_POINT('',#267123);
#44625=VERTEX_POINT('',#268100);
#44626=VERTEX_POINT('',#268101);
#44627=VERTEX_POINT('',#268109);
#44628=VERTEX_POINT('',#268111);
#44629=VERTEX_POINT('',#268123);
#44630=VERTEX_POINT('',#271696);
#44631=VERTEX_POINT('',#271697);
#44632=VERTEX_POINT('',#271699);
#44633=VERTEX_POINT('',#271711);
#44634=VERTEX_POINT('',#271713);
#44635=VERTEX_POINT('',#272376);
#44636=VERTEX_POINT('',#272377);
#44637=VERTEX_POINT('',#272379);
#44638=VERTEX_POINT('',#272717);
#44639=VERTEX_POINT('',#272718);
#44640=VERTEX_POINT('',#272723);
#44641=VERTEX_POINT('',#273058);
#44642=VERTEX_POINT('',#273059);
#44643=VERTEX_POINT('',#273067);
#44644=VERTEX_POINT('',#273399);
#44645=VERTEX_POINT('',#273400);
#44646=VERTEX_POINT('',#273408);
#44647=VERTEX_POINT('',#273743);
#44648=VERTEX_POINT('',#273744);
#44649=VERTEX_POINT('',#273746);
#44650=VERTEX_POINT('',#273748);
#44651=VERTEX_POINT('',#273752);
#44652=VERTEX_POINT('',#273753);
#44653=VERTEX_POINT('',#273755);
#44654=VERTEX_POINT('',#273757);
#44655=VERTEX_POINT('',#273759);
#44656=VERTEX_POINT('',#273761);
#44657=VERTEX_POINT('',#273765);
#44658=VERTEX_POINT('',#273766);
#44659=VERTEX_POINT('',#273768);
#44660=VERTEX_POINT('',#273770);
#44661=VERTEX_POINT('',#273772);
#44662=VERTEX_POINT('',#273775);
#44663=VERTEX_POINT('',#273779);
#44664=VERTEX_POINT('',#273780);
#44665=VERTEX_POINT('',#273782);
#44666=VERTEX_POINT('',#273784);
#44667=VERTEX_POINT('',#273788);
#44668=VERTEX_POINT('',#273789);
#44669=VERTEX_POINT('',#273791);
#44670=VERTEX_POINT('',#273793);
#44671=VERTEX_POINT('',#273795);
#44672=VERTEX_POINT('',#273798);
#44673=VERTEX_POINT('',#273802);
#44674=VERTEX_POINT('',#273803);
#44675=VERTEX_POINT('',#273805);
#44676=VERTEX_POINT('',#273807);
#44677=VERTEX_POINT('',#273811);
#44678=VERTEX_POINT('',#273812);
#44679=VERTEX_POINT('',#273814);
#44680=VERTEX_POINT('',#273816);
#44681=VERTEX_POINT('',#273818);
#44682=VERTEX_POINT('',#273820);
#44683=VERTEX_POINT('',#273822);
#44684=VERTEX_POINT('',#273824);
#44685=VERTEX_POINT('',#273827);
#44686=VERTEX_POINT('',#273828);
#44687=VERTEX_POINT('',#273830);
#44688=VERTEX_POINT('',#273832);
#44689=VERTEX_POINT('',#273834);
#44690=VERTEX_POINT('',#273836);
#44691=VERTEX_POINT('',#273838);
#44692=VERTEX_POINT('',#273840);
#44693=VERTEX_POINT('',#273844);
#44694=VERTEX_POINT('',#273845);
#44695=VERTEX_POINT('',#273847);
#44696=VERTEX_POINT('',#273849);
#44697=VERTEX_POINT('',#273853);
#44698=VERTEX_POINT('',#273854);
#44699=VERTEX_POINT('',#273856);
#44700=VERTEX_POINT('',#273858);
#44701=VERTEX_POINT('',#273862);
#44702=VERTEX_POINT('',#273863);
#44703=VERTEX_POINT('',#273865);
#44704=VERTEX_POINT('',#273867);
#44705=VERTEX_POINT('',#273871);
#44706=VERTEX_POINT('',#273872);
#44707=VERTEX_POINT('',#273874);
#44708=VERTEX_POINT('',#273876);
#44709=VERTEX_POINT('',#273941);
#44710=VERTEX_POINT('',#273955);
#44711=VERTEX_POINT('',#273969);
#44712=VERTEX_POINT('',#273983);
#44713=VERTEX_POINT('',#273996);
#44714=VERTEX_POINT('',#273998);
#44715=VERTEX_POINT('',#274002);
#44716=VERTEX_POINT('',#274004);
#44717=VERTEX_POINT('',#274006);
#44718=VERTEX_POINT('',#274008);
#44719=VERTEX_POINT('',#274010);
#44720=VERTEX_POINT('',#274014);
#44721=VERTEX_POINT('',#274016);
#44722=VERTEX_POINT('',#274020);
#44723=VERTEX_POINT('',#274022);
#44724=VERTEX_POINT('',#274024);
#44725=VERTEX_POINT('',#274029);
#44726=VERTEX_POINT('',#274030);
#44727=VERTEX_POINT('',#274119);
#44728=VERTEX_POINT('',#274120);
#44729=VERTEX_POINT('',#274122);
#44730=VERTEX_POINT('',#274124);
#44731=VERTEX_POINT('',#274128);
#44732=VERTEX_POINT('',#274130);
#44733=VERTEX_POINT('',#274134);
#44734=VERTEX_POINT('',#274138);
#44735=VERTEX_POINT('',#274152);
#44736=VERTEX_POINT('',#274153);
#44737=VERTEX_POINT('',#274155);
#44738=VERTEX_POINT('',#274157);
#44739=VERTEX_POINT('',#274161);
#44740=VERTEX_POINT('',#274162);
#44741=VERTEX_POINT('',#274164);
#44742=VERTEX_POINT('',#274166);
#44743=VERTEX_POINT('',#274168);
#44744=VERTEX_POINT('',#274170);
#44745=VERTEX_POINT('',#274172);
#44746=VERTEX_POINT('',#274174);
#44747=VERTEX_POINT('',#274176);
#44748=VERTEX_POINT('',#274178);
#44749=VERTEX_POINT('',#274180);
#44750=VERTEX_POINT('',#274182);
#44751=VERTEX_POINT('',#274184);
#44752=VERTEX_POINT('',#274186);
#44753=VERTEX_POINT('',#274191);
#44754=VERTEX_POINT('',#274195);
#44755=VERTEX_POINT('',#274199);
#44756=VERTEX_POINT('',#274203);
#44757=VERTEX_POINT('',#274207);
#44758=VERTEX_POINT('',#274211);
#44759=VERTEX_POINT('',#274215);
#44760=VERTEX_POINT('',#274219);
#44761=VERTEX_POINT('',#274223);
#44762=VERTEX_POINT('',#274227);
#44763=VERTEX_POINT('',#274231);
#44764=VERTEX_POINT('',#274235);
#44765=VERTEX_POINT('',#274239);
#44766=VERTEX_POINT('',#274243);
#44767=VERTEX_POINT('',#274250);
#44768=VERTEX_POINT('',#274251);
#44769=VERTEX_POINT('',#274253);
#44770=VERTEX_POINT('',#274255);
#44771=VERTEX_POINT('',#274257);
#44772=VERTEX_POINT('',#274259);
#44773=VERTEX_POINT('',#274261);
#44774=VERTEX_POINT('',#274263);
#44775=VERTEX_POINT('',#274267);
#44776=VERTEX_POINT('',#274269);
#44777=VERTEX_POINT('',#274273);
#44778=VERTEX_POINT('',#274277);
#44779=VERTEX_POINT('',#274281);
#44780=VERTEX_POINT('',#274285);
#44781=VERTEX_POINT('',#274289);
#44782=VERTEX_POINT('',#274293);
#44783=VERTEX_POINT('',#274300);
#44784=VERTEX_POINT('',#274301);
#44785=VERTEX_POINT('',#274303);
#44786=VERTEX_POINT('',#274305);
#44787=VERTEX_POINT('',#274307);
#44788=VERTEX_POINT('',#274309);
#44789=VERTEX_POINT('',#274311);
#44790=VERTEX_POINT('',#274313);
#44791=VERTEX_POINT('',#274315);
#44792=VERTEX_POINT('',#274317);
#44793=VERTEX_POINT('',#274319);
#44794=VERTEX_POINT('',#274321);
#44795=VERTEX_POINT('',#274323);
#44796=VERTEX_POINT('',#274325);
#44797=VERTEX_POINT('',#274327);
#44798=VERTEX_POINT('',#274329);
#44799=VERTEX_POINT('',#274331);
#44800=VERTEX_POINT('',#274333);
#44801=VERTEX_POINT('',#274335);
#44802=VERTEX_POINT('',#274337);
#44803=VERTEX_POINT('',#274339);
#44804=VERTEX_POINT('',#274341);
#44805=VERTEX_POINT('',#274343);
#44806=VERTEX_POINT('',#274345);
#44807=VERTEX_POINT('',#274347);
#44808=VERTEX_POINT('',#274349);
#44809=VERTEX_POINT('',#274351);
#44810=VERTEX_POINT('',#274353);
#44811=VERTEX_POINT('',#274355);
#44812=VERTEX_POINT('',#274357);
#44813=VERTEX_POINT('',#274359);
#44814=VERTEX_POINT('',#274361);
#44815=VERTEX_POINT('',#274363);
#44816=VERTEX_POINT('',#274365);
#44817=VERTEX_POINT('',#274367);
#44818=VERTEX_POINT('',#274369);
#44819=VERTEX_POINT('',#274371);
#44820=VERTEX_POINT('',#274373);
#44821=VERTEX_POINT('',#274375);
#44822=VERTEX_POINT('',#274377);
#44823=VERTEX_POINT('',#274379);
#44824=VERTEX_POINT('',#274381);
#44825=VERTEX_POINT('',#274383);
#44826=VERTEX_POINT('',#274385);
#44827=VERTEX_POINT('',#274387);
#44828=VERTEX_POINT('',#274389);
#44829=VERTEX_POINT('',#274391);
#44830=VERTEX_POINT('',#274393);
#44831=VERTEX_POINT('',#274395);
#44832=VERTEX_POINT('',#274397);
#44833=VERTEX_POINT('',#274399);
#44834=VERTEX_POINT('',#274401);
#44835=VERTEX_POINT('',#274403);
#44836=VERTEX_POINT('',#274405);
#44837=VERTEX_POINT('',#274407);
#44838=VERTEX_POINT('',#274409);
#44839=VERTEX_POINT('',#274413);
#44840=VERTEX_POINT('',#274414);
#44841=VERTEX_POINT('',#274416);
#44842=VERTEX_POINT('',#274418);
#44843=VERTEX_POINT('',#274420);
#44844=VERTEX_POINT('',#274422);
#44845=VERTEX_POINT('',#274424);
#44846=VERTEX_POINT('',#274426);
#44847=VERTEX_POINT('',#274428);
#44848=VERTEX_POINT('',#274430);
#44849=VERTEX_POINT('',#274432);
#44850=VERTEX_POINT('',#274434);
#44851=VERTEX_POINT('',#274436);
#44852=VERTEX_POINT('',#274438);
#44853=VERTEX_POINT('',#274440);
#44854=VERTEX_POINT('',#274442);
#44855=VERTEX_POINT('',#274444);
#44856=VERTEX_POINT('',#274446);
#44857=VERTEX_POINT('',#274448);
#44858=VERTEX_POINT('',#274450);
#44859=VERTEX_POINT('',#274452);
#44860=VERTEX_POINT('',#274454);
#44861=VERTEX_POINT('',#274456);
#44862=VERTEX_POINT('',#274458);
#44863=VERTEX_POINT('',#274460);
#44864=VERTEX_POINT('',#274462);
#44865=VERTEX_POINT('',#274464);
#44866=VERTEX_POINT('',#274466);
#44867=VERTEX_POINT('',#274468);
#44868=VERTEX_POINT('',#274470);
#44869=VERTEX_POINT('',#274472);
#44870=VERTEX_POINT('',#274474);
#44871=VERTEX_POINT('',#274476);
#44872=VERTEX_POINT('',#274478);
#44873=VERTEX_POINT('',#274480);
#44874=VERTEX_POINT('',#274482);
#44875=VERTEX_POINT('',#274484);
#44876=VERTEX_POINT('',#274486);
#44877=VERTEX_POINT('',#274488);
#44878=VERTEX_POINT('',#274490);
#44879=VERTEX_POINT('',#274492);
#44880=VERTEX_POINT('',#274494);
#44881=VERTEX_POINT('',#274496);
#44882=VERTEX_POINT('',#274498);
#44883=VERTEX_POINT('',#274500);
#44884=VERTEX_POINT('',#274502);
#44885=VERTEX_POINT('',#274504);
#44886=VERTEX_POINT('',#274506);
#44887=VERTEX_POINT('',#274508);
#44888=VERTEX_POINT('',#274510);
#44889=VERTEX_POINT('',#274512);
#44890=VERTEX_POINT('',#274514);
#44891=VERTEX_POINT('',#274516);
#44892=VERTEX_POINT('',#274518);
#44893=VERTEX_POINT('',#274520);
#44894=VERTEX_POINT('',#274522);
#44895=VERTEX_POINT('',#274638);
#44896=VERTEX_POINT('',#274639);
#44897=VERTEX_POINT('',#274641);
#44898=VERTEX_POINT('',#274643);
#44899=VERTEX_POINT('',#274647);
#44900=VERTEX_POINT('',#274648);
#44901=VERTEX_POINT('',#274650);
#44902=VERTEX_POINT('',#274652);
#44903=VERTEX_POINT('',#274654);
#44904=VERTEX_POINT('',#274656);
#44905=VERTEX_POINT('',#274659);
#44906=VERTEX_POINT('',#274661);
#44907=VERTEX_POINT('',#274663);
#44908=VERTEX_POINT('',#274665);
#44909=VERTEX_POINT('',#274667);
#44910=VERTEX_POINT('',#274669);
#44911=VERTEX_POINT('',#274671);
#44912=VERTEX_POINT('',#274673);
#44913=VERTEX_POINT('',#274677);
#44914=VERTEX_POINT('',#274679);
#44915=VERTEX_POINT('',#274683);
#44916=VERTEX_POINT('',#274687);
#44917=VERTEX_POINT('',#274691);
#44918=VERTEX_POINT('',#274695);
#44919=VERTEX_POINT('',#274699);
#44920=VERTEX_POINT('',#274703);
#44921=VERTEX_POINT('',#274707);
#44922=VERTEX_POINT('',#274713);
#44923=VERTEX_POINT('',#274717);
#44924=VERTEX_POINT('',#274721);
#44925=VERTEX_POINT('',#274725);
#44926=VERTEX_POINT('',#274729);
#44927=VERTEX_POINT('',#274736);
#44928=VERTEX_POINT('',#274737);
#44929=VERTEX_POINT('',#274739);
#44930=VERTEX_POINT('',#274741);
#44931=VERTEX_POINT('',#274743);
#44932=VERTEX_POINT('',#274745);
#44933=VERTEX_POINT('',#274747);
#44934=VERTEX_POINT('',#274749);
#44935=VERTEX_POINT('',#274753);
#44936=VERTEX_POINT('',#274755);
#44937=VERTEX_POINT('',#274759);
#44938=VERTEX_POINT('',#274763);
#44939=VERTEX_POINT('',#274767);
#44940=VERTEX_POINT('',#274771);
#44941=VERTEX_POINT('',#274775);
#44942=VERTEX_POINT('',#274779);
#44943=VERTEX_POINT('',#274786);
#44944=VERTEX_POINT('',#274787);
#44945=VERTEX_POINT('',#274789);
#44946=VERTEX_POINT('',#274791);
#44947=VERTEX_POINT('',#274795);
#44948=VERTEX_POINT('',#274796);
#44949=VERTEX_POINT('',#274799);
#44950=VERTEX_POINT('',#274801);
#44951=VERTEX_POINT('',#274803);
#44952=VERTEX_POINT('',#274805);
#44953=VERTEX_POINT('',#274807);
#44954=VERTEX_POINT('',#274809);
#44955=VERTEX_POINT('',#274811);
#44956=VERTEX_POINT('',#274813);
#44957=VERTEX_POINT('',#274815);
#44958=VERTEX_POINT('',#274817);
#44959=VERTEX_POINT('',#274819);
#44960=VERTEX_POINT('',#274821);
#44961=VERTEX_POINT('',#274825);
#44962=VERTEX_POINT('',#274827);
#44963=VERTEX_POINT('',#274831);
#44964=VERTEX_POINT('',#274835);
#44965=VERTEX_POINT('',#274839);
#44966=VERTEX_POINT('',#274843);
#44967=VERTEX_POINT('',#274847);
#44968=VERTEX_POINT('',#274851);
#44969=VERTEX_POINT('',#274855);
#44970=VERTEX_POINT('',#274859);
#44971=VERTEX_POINT('',#274863);
#44972=VERTEX_POINT('',#274867);
#44973=VERTEX_POINT('',#274871);
#44974=VERTEX_POINT('',#274877);
#44975=VERTEX_POINT('',#274884);
#44976=VERTEX_POINT('',#274885);
#44977=VERTEX_POINT('',#274887);
#44978=VERTEX_POINT('',#274889);
#44979=VERTEX_POINT('',#274891);
#44980=VERTEX_POINT('',#274893);
#44981=VERTEX_POINT('',#274895);
#44982=VERTEX_POINT('',#274897);
#44983=VERTEX_POINT('',#274901);
#44984=VERTEX_POINT('',#274903);
#44985=VERTEX_POINT('',#274907);
#44986=VERTEX_POINT('',#274911);
#44987=VERTEX_POINT('',#274915);
#44988=VERTEX_POINT('',#274919);
#44989=VERTEX_POINT('',#274923);
#44990=VERTEX_POINT('',#274927);
#44991=VERTEX_POINT('',#274934);
#44992=VERTEX_POINT('',#274935);
#44993=VERTEX_POINT('',#274937);
#44994=VERTEX_POINT('',#274939);
#44995=VERTEX_POINT('',#274943);
#44996=VERTEX_POINT('',#274944);
#44997=VERTEX_POINT('',#274947);
#44998=VERTEX_POINT('',#274949);
#44999=VERTEX_POINT('',#274951);
#45000=VERTEX_POINT('',#274953);
#45001=VERTEX_POINT('',#274955);
#45002=VERTEX_POINT('',#274957);
#45003=VERTEX_POINT('',#274959);
#45004=VERTEX_POINT('',#274961);
#45005=VERTEX_POINT('',#274963);
#45006=VERTEX_POINT('',#274965);
#45007=VERTEX_POINT('',#274967);
#45008=VERTEX_POINT('',#274969);
#45009=VERTEX_POINT('',#274973);
#45010=VERTEX_POINT('',#274975);
#45011=VERTEX_POINT('',#274979);
#45012=VERTEX_POINT('',#274983);
#45013=VERTEX_POINT('',#274987);
#45014=VERTEX_POINT('',#274991);
#45015=VERTEX_POINT('',#274995);
#45016=VERTEX_POINT('',#274999);
#45017=VERTEX_POINT('',#275003);
#45018=VERTEX_POINT('',#275007);
#45019=VERTEX_POINT('',#275011);
#45020=VERTEX_POINT('',#275015);
#45021=VERTEX_POINT('',#275019);
#45022=VERTEX_POINT('',#275025);
#45023=VERTEX_POINT('',#275032);
#45024=VERTEX_POINT('',#275033);
#45025=VERTEX_POINT('',#275035);
#45026=VERTEX_POINT('',#275037);
#45027=VERTEX_POINT('',#275039);
#45028=VERTEX_POINT('',#275041);
#45029=VERTEX_POINT('',#275043);
#45030=VERTEX_POINT('',#275045);
#45031=VERTEX_POINT('',#275049);
#45032=VERTEX_POINT('',#275051);
#45033=VERTEX_POINT('',#275055);
#45034=VERTEX_POINT('',#275059);
#45035=VERTEX_POINT('',#275063);
#45036=VERTEX_POINT('',#275067);
#45037=VERTEX_POINT('',#275071);
#45038=VERTEX_POINT('',#275075);
#45039=VERTEX_POINT('',#275082);
#45040=VERTEX_POINT('',#275083);
#45041=VERTEX_POINT('',#275085);
#45042=VERTEX_POINT('',#275087);
#45043=VERTEX_POINT('',#275091);
#45044=VERTEX_POINT('',#275092);
#45045=VERTEX_POINT('',#275094);
#45046=VERTEX_POINT('',#275096);
#45047=VERTEX_POINT('',#275100);
#45048=VERTEX_POINT('',#275101);
#45049=VERTEX_POINT('',#275103);
#45050=VERTEX_POINT('',#275105);
#45051=VERTEX_POINT('',#275109);
#45052=VERTEX_POINT('',#275111);
#45053=VERTEX_POINT('',#275115);
#45054=VERTEX_POINT('',#275117);
#45055=VERTEX_POINT('',#275121);
#45056=VERTEX_POINT('',#275123);
#45057=VERTEX_POINT('',#275127);
#45058=VERTEX_POINT('',#275129);
#45059=VERTEX_POINT('',#275133);
#45060=VERTEX_POINT('',#275135);
#45061=VERTEX_POINT('',#275139);
#45062=VERTEX_POINT('',#275141);
#45063=VERTEX_POINT('',#275145);
#45064=VERTEX_POINT('',#275147);
#45065=VERTEX_POINT('',#275151);
#45066=VERTEX_POINT('',#275153);
#45067=VERTEX_POINT('',#275157);
#45068=VERTEX_POINT('',#275159);
#45069=VERTEX_POINT('',#275163);
#45070=VERTEX_POINT('',#275165);
#45071=VERTEX_POINT('',#275169);
#45072=VERTEX_POINT('',#275171);
#45073=VERTEX_POINT('',#275175);
#45074=VERTEX_POINT('',#275177);
#45075=VERTEX_POINT('',#275181);
#45076=VERTEX_POINT('',#275183);
#45077=VERTEX_POINT('',#275187);
#45078=VERTEX_POINT('',#275188);
#45079=VERTEX_POINT('',#275190);
#45080=VERTEX_POINT('',#275192);
#45081=VERTEX_POINT('',#275196);
#45082=VERTEX_POINT('',#275198);
#45083=VERTEX_POINT('',#275202);
#45084=VERTEX_POINT('',#275204);
#45085=VERTEX_POINT('',#275208);
#45086=VERTEX_POINT('',#275210);
#45087=VERTEX_POINT('',#275214);
#45088=VERTEX_POINT('',#275216);
#45089=VERTEX_POINT('',#275220);
#45090=VERTEX_POINT('',#275222);
#45091=VERTEX_POINT('',#275226);
#45092=VERTEX_POINT('',#275228);
#45093=VERTEX_POINT('',#275232);
#45094=VERTEX_POINT('',#275234);
#45095=VERTEX_POINT('',#275238);
#45096=VERTEX_POINT('',#275240);
#45097=VERTEX_POINT('',#275244);
#45098=VERTEX_POINT('',#275246);
#45099=VERTEX_POINT('',#275250);
#45100=VERTEX_POINT('',#275252);
#45101=VERTEX_POINT('',#275256);
#45102=VERTEX_POINT('',#275258);
#45103=VERTEX_POINT('',#275262);
#45104=VERTEX_POINT('',#275264);
#45105=VERTEX_POINT('',#275268);
#45106=VERTEX_POINT('',#275270);
#45107=VERTEX_POINT('',#275274);
#45108=VERTEX_POINT('',#275276);
#45109=VERTEX_POINT('',#275280);
#45110=VERTEX_POINT('',#275282);
#45111=VERTEX_POINT('',#275286);
#45112=VERTEX_POINT('',#275288);
#45113=VERTEX_POINT('',#275292);
#45114=VERTEX_POINT('',#275294);
#45115=VERTEX_POINT('',#275298);
#45116=VERTEX_POINT('',#275300);
#45117=VERTEX_POINT('',#275307);
#45118=VERTEX_POINT('',#275308);
#45119=VERTEX_POINT('',#275310);
#45120=VERTEX_POINT('',#275312);
#45121=VERTEX_POINT('',#275316);
#45122=VERTEX_POINT('',#275318);
#45123=VERTEX_POINT('',#275322);
#45124=VERTEX_POINT('',#275324);
#45125=VERTEX_POINT('',#275328);
#45126=VERTEX_POINT('',#275330);
#45127=VERTEX_POINT('',#275334);
#45128=VERTEX_POINT('',#275336);
#45129=VERTEX_POINT('',#275340);
#45130=VERTEX_POINT('',#275342);
#45131=VERTEX_POINT('',#275346);
#45132=VERTEX_POINT('',#275348);
#45133=VERTEX_POINT('',#275352);
#45134=VERTEX_POINT('',#275354);
#45135=VERTEX_POINT('',#275358);
#45136=VERTEX_POINT('',#275360);
#45137=VERTEX_POINT('',#275364);
#45138=VERTEX_POINT('',#275366);
#45139=VERTEX_POINT('',#275370);
#45140=VERTEX_POINT('',#275372);
#45141=VERTEX_POINT('',#275376);
#45142=VERTEX_POINT('',#275378);
#45143=VERTEX_POINT('',#275382);
#45144=VERTEX_POINT('',#275384);
#45145=VERTEX_POINT('',#275388);
#45146=VERTEX_POINT('',#275390);
#45147=VERTEX_POINT('',#275394);
#45148=VERTEX_POINT('',#275396);
#45149=VERTEX_POINT('',#275400);
#45150=VERTEX_POINT('',#275402);
#45151=VERTEX_POINT('',#275406);
#45152=VERTEX_POINT('',#275408);
#45153=VERTEX_POINT('',#275412);
#45154=VERTEX_POINT('',#275414);
#45155=VERTEX_POINT('',#275421);
#45156=VERTEX_POINT('',#275422);
#45157=VERTEX_POINT('',#275424);
#45158=VERTEX_POINT('',#275426);
#45159=VERTEX_POINT('',#275430);
#45160=VERTEX_POINT('',#275432);
#45161=VERTEX_POINT('',#275436);
#45162=VERTEX_POINT('',#275438);
#45163=VERTEX_POINT('',#275442);
#45164=VERTEX_POINT('',#275444);
#45165=VERTEX_POINT('',#275448);
#45166=VERTEX_POINT('',#275450);
#45167=VERTEX_POINT('',#275454);
#45168=VERTEX_POINT('',#275456);
#45169=VERTEX_POINT('',#275460);
#45170=VERTEX_POINT('',#275462);
#45171=VERTEX_POINT('',#275466);
#45172=VERTEX_POINT('',#275468);
#45173=VERTEX_POINT('',#275472);
#45174=VERTEX_POINT('',#275474);
#45175=VERTEX_POINT('',#275478);
#45176=VERTEX_POINT('',#275480);
#45177=VERTEX_POINT('',#275484);
#45178=VERTEX_POINT('',#275486);
#45179=VERTEX_POINT('',#275490);
#45180=VERTEX_POINT('',#275492);
#45181=VERTEX_POINT('',#275499);
#45182=VERTEX_POINT('',#275500);
#45183=VERTEX_POINT('',#275502);
#45184=VERTEX_POINT('',#275504);
#45185=VERTEX_POINT('',#275508);
#45186=VERTEX_POINT('',#275510);
#45187=VERTEX_POINT('',#275514);
#45188=VERTEX_POINT('',#275516);
#45189=VERTEX_POINT('',#275520);
#45190=VERTEX_POINT('',#275522);
#45191=VERTEX_POINT('',#275526);
#45192=VERTEX_POINT('',#275528);
#45193=VERTEX_POINT('',#275532);
#45194=VERTEX_POINT('',#275534);
#45195=VERTEX_POINT('',#275538);
#45196=VERTEX_POINT('',#275540);
#45197=VERTEX_POINT('',#275544);
#45198=VERTEX_POINT('',#275546);
#45199=VERTEX_POINT('',#275550);
#45200=VERTEX_POINT('',#275552);
#45201=VERTEX_POINT('',#275556);
#45202=VERTEX_POINT('',#275558);
#45203=VERTEX_POINT('',#275562);
#45204=VERTEX_POINT('',#275564);
#45205=VERTEX_POINT('',#275568);
#45206=VERTEX_POINT('',#275570);
#45207=VERTEX_POINT('',#275574);
#45208=VERTEX_POINT('',#275576);
#45209=VERTEX_POINT('',#275580);
#45210=VERTEX_POINT('',#275582);
#45211=VERTEX_POINT('',#275586);
#45212=VERTEX_POINT('',#275588);
#45213=VERTEX_POINT('',#275592);
#45214=VERTEX_POINT('',#275594);
#45215=VERTEX_POINT('',#275598);
#45216=VERTEX_POINT('',#275600);
#45217=VERTEX_POINT('',#275604);
#45218=VERTEX_POINT('',#275606);
#45219=VERTEX_POINT('',#275610);
#45220=VERTEX_POINT('',#275612);
#45221=VERTEX_POINT('',#275616);
#45222=VERTEX_POINT('',#275618);
#45223=VERTEX_POINT('',#275622);
#45224=VERTEX_POINT('',#275624);
#45225=VERTEX_POINT('',#275628);
#45226=VERTEX_POINT('',#275630);
#45227=VERTEX_POINT('',#275634);
#45228=VERTEX_POINT('',#275636);
#45229=VERTEX_POINT('',#275640);
#45230=VERTEX_POINT('',#275642);
#45231=VERTEX_POINT('',#275646);
#45232=VERTEX_POINT('',#275648);
#45233=VERTEX_POINT('',#275652);
#45234=VERTEX_POINT('',#275654);
#45235=VERTEX_POINT('',#275658);
#45236=VERTEX_POINT('',#275660);
#45237=VERTEX_POINT('',#275664);
#45238=VERTEX_POINT('',#275666);
#45239=VERTEX_POINT('',#275670);
#45240=VERTEX_POINT('',#275672);
#45241=VERTEX_POINT('',#275676);
#45242=VERTEX_POINT('',#275678);
#45243=VERTEX_POINT('',#275682);
#45244=VERTEX_POINT('',#275684);
#45245=VERTEX_POINT('',#275688);
#45246=VERTEX_POINT('',#275690);
#45247=VERTEX_POINT('',#275694);
#45248=VERTEX_POINT('',#275696);
#45249=VERTEX_POINT('',#275700);
#45250=VERTEX_POINT('',#275702);
#45251=VERTEX_POINT('',#275706);
#45252=VERTEX_POINT('',#275708);
#45253=VERTEX_POINT('',#275712);
#45254=VERTEX_POINT('',#275714);
#45255=VERTEX_POINT('',#275718);
#45256=VERTEX_POINT('',#275720);
#45257=VERTEX_POINT('',#275724);
#45258=VERTEX_POINT('',#275726);
#45259=VERTEX_POINT('',#275733);
#45260=VERTEX_POINT('',#275734);
#45261=VERTEX_POINT('',#275736);
#45262=VERTEX_POINT('',#275738);
#45263=VERTEX_POINT('',#275742);
#45264=VERTEX_POINT('',#275744);
#45265=VERTEX_POINT('',#275748);
#45266=VERTEX_POINT('',#275750);
#45267=VERTEX_POINT('',#275754);
#45268=VERTEX_POINT('',#275756);
#45269=VERTEX_POINT('',#275760);
#45270=VERTEX_POINT('',#275762);
#45271=VERTEX_POINT('',#275766);
#45272=VERTEX_POINT('',#275768);
#45273=VERTEX_POINT('',#275772);
#45274=VERTEX_POINT('',#275774);
#45275=VERTEX_POINT('',#275778);
#45276=VERTEX_POINT('',#275780);
#45277=VERTEX_POINT('',#275784);
#45278=VERTEX_POINT('',#275786);
#45279=VERTEX_POINT('',#275790);
#45280=VERTEX_POINT('',#275792);
#45281=VERTEX_POINT('',#275796);
#45282=VERTEX_POINT('',#275798);
#45283=VERTEX_POINT('',#275802);
#45284=VERTEX_POINT('',#275804);
#45285=VERTEX_POINT('',#275811);
#45286=VERTEX_POINT('',#275812);
#45287=VERTEX_POINT('',#275814);
#45288=VERTEX_POINT('',#275816);
#45289=VERTEX_POINT('',#275820);
#45290=VERTEX_POINT('',#275822);
#45291=VERTEX_POINT('',#275826);
#45292=VERTEX_POINT('',#275828);
#45293=VERTEX_POINT('',#275832);
#45294=VERTEX_POINT('',#275834);
#45295=VERTEX_POINT('',#275838);
#45296=VERTEX_POINT('',#275840);
#45297=VERTEX_POINT('',#275844);
#45298=VERTEX_POINT('',#275846);
#45299=VERTEX_POINT('',#275850);
#45300=VERTEX_POINT('',#275852);
#45301=VERTEX_POINT('',#275856);
#45302=VERTEX_POINT('',#275858);
#45303=VERTEX_POINT('',#275862);
#45304=VERTEX_POINT('',#275864);
#45305=VERTEX_POINT('',#275868);
#45306=VERTEX_POINT('',#275870);
#45307=VERTEX_POINT('',#275874);
#45308=VERTEX_POINT('',#275876);
#45309=VERTEX_POINT('',#275880);
#45310=VERTEX_POINT('',#275882);
#45311=VERTEX_POINT('',#275886);
#45312=VERTEX_POINT('',#275888);
#45313=VERTEX_POINT('',#275892);
#45314=VERTEX_POINT('',#275894);
#45315=VERTEX_POINT('',#275898);
#45316=VERTEX_POINT('',#275900);
#45317=VERTEX_POINT('',#275904);
#45318=VERTEX_POINT('',#275906);
#45319=VERTEX_POINT('',#275910);
#45320=VERTEX_POINT('',#275912);
#45321=VERTEX_POINT('',#275916);
#45322=VERTEX_POINT('',#275918);
#45323=VERTEX_POINT('',#275922);
#45324=VERTEX_POINT('',#275924);
#45325=VERTEX_POINT('',#275928);
#45326=VERTEX_POINT('',#275930);
#45327=VERTEX_POINT('',#275934);
#45328=VERTEX_POINT('',#275936);
#45329=VERTEX_POINT('',#275940);
#45330=VERTEX_POINT('',#275942);
#45331=VERTEX_POINT('',#275946);
#45332=VERTEX_POINT('',#275948);
#45333=VERTEX_POINT('',#275952);
#45334=VERTEX_POINT('',#275954);
#45335=VERTEX_POINT('',#275958);
#45336=VERTEX_POINT('',#275960);
#45337=VERTEX_POINT('',#275964);
#45338=VERTEX_POINT('',#275966);
#45339=VERTEX_POINT('',#275970);
#45340=VERTEX_POINT('',#275972);
#45341=VERTEX_POINT('',#275976);
#45342=VERTEX_POINT('',#275978);
#45343=VERTEX_POINT('',#275982);
#45344=VERTEX_POINT('',#275984);
#45345=VERTEX_POINT('',#275988);
#45346=VERTEX_POINT('',#275990);
#45347=VERTEX_POINT('',#275994);
#45348=VERTEX_POINT('',#275996);
#45349=VERTEX_POINT('',#276000);
#45350=VERTEX_POINT('',#276002);
#45351=VERTEX_POINT('',#276006);
#45352=VERTEX_POINT('',#276008);
#45353=VERTEX_POINT('',#276012);
#45354=VERTEX_POINT('',#276014);
#45355=VERTEX_POINT('',#276018);
#45356=VERTEX_POINT('',#276020);
#45357=VERTEX_POINT('',#276024);
#45358=VERTEX_POINT('',#276026);
#45359=VERTEX_POINT('',#276030);
#45360=VERTEX_POINT('',#276032);
#45361=VERTEX_POINT('',#276036);
#45362=VERTEX_POINT('',#276038);
#45363=VERTEX_POINT('',#276045);
#45364=VERTEX_POINT('',#276046);
#45365=VERTEX_POINT('',#276048);
#45366=VERTEX_POINT('',#276050);
#45367=VERTEX_POINT('',#276054);
#45368=VERTEX_POINT('',#276056);
#45369=VERTEX_POINT('',#276060);
#45370=VERTEX_POINT('',#276062);
#45371=VERTEX_POINT('',#276066);
#45372=VERTEX_POINT('',#276068);
#45373=VERTEX_POINT('',#276072);
#45374=VERTEX_POINT('',#276074);
#45375=VERTEX_POINT('',#276078);
#45376=VERTEX_POINT('',#276080);
#45377=VERTEX_POINT('',#276084);
#45378=VERTEX_POINT('',#276086);
#45379=VERTEX_POINT('',#276090);
#45380=VERTEX_POINT('',#276092);
#45381=VERTEX_POINT('',#276096);
#45382=VERTEX_POINT('',#276098);
#45383=VERTEX_POINT('',#276102);
#45384=VERTEX_POINT('',#276104);
#45385=VERTEX_POINT('',#276108);
#45386=VERTEX_POINT('',#276110);
#45387=VERTEX_POINT('',#276114);
#45388=VERTEX_POINT('',#276116);
#45389=VERTEX_POINT('',#276123);
#45390=VERTEX_POINT('',#276125);
#45391=VERTEX_POINT('',#276129);
#45392=VERTEX_POINT('',#276131);
#45393=VERTEX_POINT('',#276135);
#45394=VERTEX_POINT('',#276137);
#45395=VERTEX_POINT('',#276141);
#45396=VERTEX_POINT('',#276143);
#45397=VERTEX_POINT('',#276147);
#45398=VERTEX_POINT('',#276149);
#45399=VERTEX_POINT('',#276153);
#45400=VERTEX_POINT('',#276155);
#45401=VERTEX_POINT('',#276159);
#45402=VERTEX_POINT('',#276161);
#45403=VERTEX_POINT('',#276165);
#45404=VERTEX_POINT('',#276167);
#45405=VERTEX_POINT('',#276171);
#45406=VERTEX_POINT('',#276173);
#45407=VERTEX_POINT('',#276177);
#45408=VERTEX_POINT('',#276179);
#45409=VERTEX_POINT('',#276183);
#45410=VERTEX_POINT('',#276185);
#45411=VERTEX_POINT('',#276189);
#45412=VERTEX_POINT('',#276191);
#45413=VERTEX_POINT('',#276195);
#45414=VERTEX_POINT('',#276197);
#45415=VERTEX_POINT('',#276201);
#45416=VERTEX_POINT('',#276203);
#45417=VERTEX_POINT('',#276207);
#45418=VERTEX_POINT('',#276209);
#45419=VERTEX_POINT('',#276213);
#45420=VERTEX_POINT('',#276215);
#45421=VERTEX_POINT('',#276219);
#45422=VERTEX_POINT('',#276221);
#45423=VERTEX_POINT('',#276225);
#45424=VERTEX_POINT('',#276227);
#45425=VERTEX_POINT('',#276231);
#45426=VERTEX_POINT('',#276233);
#45427=VERTEX_POINT('',#276237);
#45428=VERTEX_POINT('',#276239);
#45429=VERTEX_POINT('',#276243);
#45430=VERTEX_POINT('',#276245);
#45431=VERTEX_POINT('',#276249);
#45432=VERTEX_POINT('',#276251);
#45433=VERTEX_POINT('',#276255);
#45434=VERTEX_POINT('',#276257);
#45435=VERTEX_POINT('',#276261);
#45436=VERTEX_POINT('',#276263);
#45437=VERTEX_POINT('',#276267);
#45438=VERTEX_POINT('',#276269);
#45439=VERTEX_POINT('',#276273);
#45440=VERTEX_POINT('',#276275);
#45441=VERTEX_POINT('',#276279);
#45442=VERTEX_POINT('',#276281);
#45443=VERTEX_POINT('',#276285);
#45444=VERTEX_POINT('',#276287);
#45445=VERTEX_POINT('',#276291);
#45446=VERTEX_POINT('',#276293);
#45447=VERTEX_POINT('',#276297);
#45448=VERTEX_POINT('',#276299);
#45449=VERTEX_POINT('',#276303);
#45450=VERTEX_POINT('',#276305);
#45451=VERTEX_POINT('',#276309);
#45452=VERTEX_POINT('',#276311);
#45453=VERTEX_POINT('',#276315);
#45454=VERTEX_POINT('',#276317);
#45455=VERTEX_POINT('',#276321);
#45456=VERTEX_POINT('',#276323);
#45457=VERTEX_POINT('',#276327);
#45458=VERTEX_POINT('',#276329);
#45459=VERTEX_POINT('',#276333);
#45460=VERTEX_POINT('',#276335);
#45461=VERTEX_POINT('',#276339);
#45462=VERTEX_POINT('',#276341);
#45463=VERTEX_POINT('',#276348);
#45464=VERTEX_POINT('',#276350);
#45465=VERTEX_POINT('',#276357);
#45466=VERTEX_POINT('',#276359);
#45467=VERTEX_POINT('',#276366);
#45468=VERTEX_POINT('',#276367);
#45469=VERTEX_POINT('',#276369);
#45470=VERTEX_POINT('',#276371);
#45471=VERTEX_POINT('',#276373);
#45472=VERTEX_POINT('',#276375);
#45473=VERTEX_POINT('',#276377);
#45474=VERTEX_POINT('',#276379);
#45475=VERTEX_POINT('',#276383);
#45476=VERTEX_POINT('',#276384);
#45477=VERTEX_POINT('',#276389);
#45478=VERTEX_POINT('',#276393);
#45479=VERTEX_POINT('',#276397);
#45480=VERTEX_POINT('',#276401);
#45481=VERTEX_POINT('',#276405);
#45482=VERTEX_POINT('',#276409);
#45483=VERTEX_POINT('',#276416);
#45484=VERTEX_POINT('',#276417);
#45485=VERTEX_POINT('',#276419);
#45486=VERTEX_POINT('',#276421);
#45487=VERTEX_POINT('',#276425);
#45488=VERTEX_POINT('',#276427);
#45489=VERTEX_POINT('',#276431);
#45490=VERTEX_POINT('',#276433);
#45491=EDGE_CURVE('',#36559,#36559,#30412,.T.);
#45492=EDGE_CURVE('',#36559,#36560,#19958,.T.);
#45493=EDGE_CURVE('',#36560,#36560,#30413,.T.);
#45494=EDGE_CURVE('',#36561,#36561,#30414,.T.);
#45495=EDGE_CURVE('',#36561,#36562,#19959,.T.);
#45496=EDGE_CURVE('',#36562,#36562,#30415,.T.);
#45497=EDGE_CURVE('',#36563,#36563,#30416,.T.);
#45498=EDGE_CURVE('',#36563,#36564,#19960,.T.);
#45499=EDGE_CURVE('',#36564,#36564,#30417,.T.);
#45500=EDGE_CURVE('',#36565,#36565,#30418,.T.);
#45501=EDGE_CURVE('',#36565,#36566,#19961,.T.);
#45502=EDGE_CURVE('',#36566,#36566,#30419,.T.);
#45503=EDGE_CURVE('',#36567,#36568,#19962,.T.);
#45504=EDGE_CURVE('',#36569,#36567,#19963,.T.);
#45505=EDGE_CURVE('',#36569,#36570,#19964,.T.);
#45506=EDGE_CURVE('',#36570,#36568,#19965,.T.);
#45507=EDGE_CURVE('',#36571,#36567,#19966,.T.);
#45508=EDGE_CURVE('',#36572,#36571,#19967,.T.);
#45509=EDGE_CURVE('',#36572,#36569,#19968,.T.);
#45510=EDGE_CURVE('',#36573,#36571,#19969,.T.);
#45511=EDGE_CURVE('',#36574,#36573,#19970,.T.);
#45512=EDGE_CURVE('',#36574,#36572,#19971,.T.);
#45513=EDGE_CURVE('',#36568,#36573,#19972,.T.);
#45514=EDGE_CURVE('',#36570,#36574,#19973,.T.);
#45515=EDGE_CURVE('',#36575,#36576,#19974,.T.);
#45516=EDGE_CURVE('',#36577,#36575,#19975,.T.);
#45517=EDGE_CURVE('',#36578,#36577,#19976,.T.);
#45518=EDGE_CURVE('',#36576,#36578,#19977,.T.);
#45519=EDGE_CURVE('',#36579,#36574,#19978,.T.);
#45520=EDGE_CURVE('',#36580,#36570,#19979,.T.);
#45521=EDGE_CURVE('',#36579,#36580,#19980,.T.);
#45522=EDGE_CURVE('',#36581,#36569,#19981,.T.);
#45523=EDGE_CURVE('',#36580,#36581,#19982,.T.);
#45524=EDGE_CURVE('',#36582,#36572,#19983,.T.);
#45525=EDGE_CURVE('',#36582,#36579,#19984,.T.);
#45526=EDGE_CURVE('',#36581,#36582,#19985,.T.);
#45527=EDGE_CURVE('',#36583,#36576,#19986,.T.);
#45528=EDGE_CURVE('',#36584,#36583,#19987,.T.);
#45529=EDGE_CURVE('',#36584,#36575,#19988,.T.);
#45530=EDGE_CURVE('',#36585,#36584,#19989,.T.);
#45531=EDGE_CURVE('',#36585,#36577,#19990,.T.);
#45532=EDGE_CURVE('',#36586,#36585,#19991,.T.);
#45533=EDGE_CURVE('',#36586,#36578,#19992,.T.);
#45534=EDGE_CURVE('',#36583,#36586,#19993,.T.);
#45535=EDGE_CURVE('',#36587,#36586,#19994,.T.);
#45536=EDGE_CURVE('',#36587,#36588,#19995,.T.);
#45537=EDGE_CURVE('',#36588,#36583,#19996,.T.);
#45538=EDGE_CURVE('',#36588,#36589,#19997,.T.);
#45539=EDGE_CURVE('',#36589,#36584,#19998,.T.);
#45540=EDGE_CURVE('',#36590,#36585,#19999,.T.);
#45541=EDGE_CURVE('',#36590,#36587,#20000,.T.);
#45542=EDGE_CURVE('',#36589,#36590,#20001,.T.);
#45543=EDGE_CURVE('',#36591,#36587,#20002,.T.);
#45544=EDGE_CURVE('',#36591,#36592,#20003,.T.);
#45545=EDGE_CURVE('',#36592,#36588,#20004,.T.);
#45546=EDGE_CURVE('',#36592,#36593,#20005,.T.);
#45547=EDGE_CURVE('',#36593,#36589,#20006,.T.);
#45548=EDGE_CURVE('',#36593,#36594,#20007,.T.);
#45549=EDGE_CURVE('',#36594,#36590,#20008,.T.);
#45550=EDGE_CURVE('',#36594,#36591,#20009,.T.);
#45551=EDGE_CURVE('',#36595,#36596,#20010,.T.);
#45552=EDGE_CURVE('',#36596,#36597,#30420,.T.);
#45553=EDGE_CURVE('',#36597,#36598,#20011,.T.);
#45554=EDGE_CURVE('',#36598,#36599,#30421,.T.);
#45555=EDGE_CURVE('',#36599,#36600,#20012,.T.);
#45556=EDGE_CURVE('',#36600,#36601,#30422,.T.);
#45557=EDGE_CURVE('',#36601,#36602,#20013,.T.);
#45558=EDGE_CURVE('',#36602,#36595,#30423,.T.);
#45559=EDGE_CURVE('',#36603,#36604,#20014,.T.);
#45560=EDGE_CURVE('',#36604,#36605,#30424,.T.);
#45561=EDGE_CURVE('',#36605,#36606,#20015,.T.);
#45562=EDGE_CURVE('',#36606,#36607,#30425,.T.);
#45563=EDGE_CURVE('',#36607,#36608,#20016,.T.);
#45564=EDGE_CURVE('',#36608,#36609,#30426,.T.);
#45565=EDGE_CURVE('',#36609,#36610,#20017,.T.);
#45566=EDGE_CURVE('',#36610,#36603,#30427,.T.);
#45567=EDGE_CURVE('',#36603,#36611,#20018,.T.);
#45568=EDGE_CURVE('',#36611,#36612,#20019,.T.);
#45569=EDGE_CURVE('',#36612,#36604,#20020,.T.);
#45570=EDGE_CURVE('',#36605,#36613,#20021,.T.);
#45571=EDGE_CURVE('',#36613,#36614,#20022,.T.);
#45572=EDGE_CURVE('',#36614,#36606,#20023,.T.);
#45573=EDGE_CURVE('',#36607,#36615,#20024,.T.);
#45574=EDGE_CURVE('',#36615,#36616,#20025,.T.);
#45575=EDGE_CURVE('',#36616,#36608,#20026,.T.);
#45576=EDGE_CURVE('',#36609,#36617,#20027,.T.);
#45577=EDGE_CURVE('',#36617,#36618,#20028,.T.);
#45578=EDGE_CURVE('',#36618,#36610,#20029,.T.);
#45579=EDGE_CURVE('',#36612,#36613,#30428,.T.);
#45580=EDGE_CURVE('',#36618,#36611,#30429,.T.);
#45581=EDGE_CURVE('',#36616,#36617,#30430,.T.);
#45582=EDGE_CURVE('',#36614,#36615,#30431,.T.);
#45583=EDGE_CURVE('',#36615,#36600,#30432,.T.);
#45584=EDGE_CURVE('',#36601,#36614,#30433,.T.);
#45585=EDGE_CURVE('',#36602,#36613,#30434,.T.);
#45586=EDGE_CURVE('',#36616,#36599,#30435,.T.);
#45587=EDGE_CURVE('',#36595,#36612,#30436,.T.);
#45588=EDGE_CURVE('',#36617,#36598,#30437,.T.);
#45589=EDGE_CURVE('',#36596,#36611,#30438,.T.);
#45590=EDGE_CURVE('',#36618,#36597,#30439,.T.);
#45591=EDGE_CURVE('',#36619,#36620,#30440,.T.);
#45592=EDGE_CURVE('',#36620,#36619,#30441,.T.);
#45593=EDGE_CURVE('',#36620,#36621,#30442,.T.);
#45594=EDGE_CURVE('',#36621,#36621,#30443,.T.);
#45595=EDGE_CURVE('',#36622,#36622,#30444,.T.);
#45596=EDGE_CURVE('',#36622,#36623,#30445,.T.);
#45597=EDGE_CURVE('',#36624,#36623,#30446,.T.);
#45598=EDGE_CURVE('',#36623,#36624,#30447,.T.);
#45599=EDGE_CURVE('',#36625,#36626,#4173,.T.);
#45600=EDGE_CURVE('',#36626,#36627,#20030,.T.);
#45601=EDGE_CURVE('',#36627,#36628,#4174,.T.);
#45602=EDGE_CURVE('',#36628,#36627,#4175,.T.);
#45603=EDGE_CURVE('',#36626,#36625,#4176,.T.);
#45604=EDGE_CURVE('',#36629,#36630,#4177,.T.);
#45605=EDGE_CURVE('',#36630,#36631,#20031,.T.);
#45606=EDGE_CURVE('',#36631,#36632,#4178,.T.);
#45607=EDGE_CURVE('',#36632,#36631,#4179,.T.);
#45608=EDGE_CURVE('',#36630,#36629,#4180,.T.);
#45609=EDGE_CURVE('',#36633,#36634,#4181,.T.);
#45610=EDGE_CURVE('',#36634,#36635,#20032,.T.);
#45611=EDGE_CURVE('',#36635,#36636,#4182,.T.);
#45612=EDGE_CURVE('',#36636,#36635,#4183,.T.);
#45613=EDGE_CURVE('',#36634,#36633,#4184,.T.);
#45614=EDGE_CURVE('',#36637,#36638,#4185,.T.);
#45615=EDGE_CURVE('',#36638,#36639,#20033,.T.);
#45616=EDGE_CURVE('',#36639,#36640,#4186,.T.);
#45617=EDGE_CURVE('',#36640,#36639,#4187,.T.);
#45618=EDGE_CURVE('',#36638,#36637,#4188,.T.);
#45619=EDGE_CURVE('',#36641,#36641,#30448,.T.);
#45620=EDGE_CURVE('',#36641,#36640,#20034,.T.);
#45621=EDGE_CURVE('',#36639,#36624,#20035,.T.);
#45622=EDGE_CURVE('',#36619,#36638,#20036,.T.);
#45623=EDGE_CURVE('',#36637,#36642,#20037,.T.);
#45624=EDGE_CURVE('',#36642,#36642,#30449,.T.);
#45625=EDGE_CURVE('',#36643,#36644,#20038,.T.);
#45626=EDGE_CURVE('',#36645,#36643,#4065,.T.);
#45627=EDGE_CURVE('',#36646,#36645,#20039,.T.);
#45628=EDGE_CURVE('',#36646,#36644,#4066,.T.);
#45629=EDGE_CURVE('',#36647,#36648,#20040,.T.);
#45630=EDGE_CURVE('',#36643,#36647,#4067,.T.);
#45631=EDGE_CURVE('',#36644,#36648,#4068,.T.);
#45632=EDGE_CURVE('',#36649,#36650,#20041,.T.);
#45633=EDGE_CURVE('',#36647,#36649,#4069,.T.);
#45634=EDGE_CURVE('',#36648,#36650,#4070,.T.);
#45635=EDGE_CURVE('',#36651,#36652,#20042,.T.);
#45636=EDGE_CURVE('',#36649,#36651,#4071,.T.);
#45637=EDGE_CURVE('',#36650,#36652,#4072,.T.);
#45638=EDGE_CURVE('',#36653,#36654,#20043,.T.);
#45639=EDGE_CURVE('',#36651,#36653,#4073,.T.);
#45640=EDGE_CURVE('',#36652,#36654,#4074,.T.);
#45641=EDGE_CURVE('',#36655,#36656,#20044,.T.);
#45642=EDGE_CURVE('',#36653,#36655,#4075,.T.);
#45643=EDGE_CURVE('',#36654,#36656,#4076,.T.);
#45644=EDGE_CURVE('',#36657,#36658,#20045,.T.);
#45645=EDGE_CURVE('',#36655,#36657,#4077,.T.);
#45646=EDGE_CURVE('',#36656,#36658,#4078,.T.);
#45647=EDGE_CURVE('',#36659,#36660,#20046,.T.);
#45648=EDGE_CURVE('',#36657,#36659,#4079,.T.);
#45649=EDGE_CURVE('',#36658,#36660,#4080,.T.);
#45650=EDGE_CURVE('',#36661,#36662,#20047,.T.);
#45651=EDGE_CURVE('',#36663,#36661,#4189,.F.);
#45652=EDGE_CURVE('',#36663,#36663,#30450,.T.);
#45653=EDGE_CURVE('',#36664,#36663,#20048,.T.);
#45654=EDGE_CURVE('',#36665,#36664,#20049,.T.);
#45655=EDGE_CURVE('',#36662,#36665,#4190,.T.);
#45656=EDGE_CURVE('',#36666,#36667,#4191,.T.);
#45657=EDGE_CURVE('',#36667,#36666,#4192,.T.);
#45658=EDGE_CURVE('',#36668,#36669,#4193,.T.);
#45659=EDGE_CURVE('',#36669,#36668,#4194,.T.);
#45660=EDGE_CURVE('',#36670,#36671,#20050,.T.);
#45661=EDGE_CURVE('',#36661,#36670,#4195,.F.);
#45662=EDGE_CURVE('',#36665,#36662,#4196,.T.);
#45663=EDGE_CURVE('',#36664,#36671,#4197,.T.);
#45664=EDGE_CURVE('',#36672,#36673,#4198,.T.);
#45665=EDGE_CURVE('',#36673,#36672,#4199,.T.);
#45666=EDGE_CURVE('',#36674,#36675,#20051,.T.);
#45667=EDGE_CURVE('',#36670,#36674,#4200,.F.);
#45668=EDGE_CURVE('',#36671,#36675,#4201,.T.);
#45669=EDGE_CURVE('',#36676,#36677,#20052,.T.);
#45670=EDGE_CURVE('',#36674,#36676,#4202,.F.);
#45671=EDGE_CURVE('',#36675,#36677,#4203,.T.);
#45672=EDGE_CURVE('',#36678,#36679,#20053,.T.);
#45673=EDGE_CURVE('',#36676,#36678,#4204,.F.);
#45674=EDGE_CURVE('',#36677,#36679,#4205,.T.);
#45675=EDGE_CURVE('',#36680,#36681,#20054,.T.);
#45676=EDGE_CURVE('',#36678,#36680,#4206,.F.);
#45677=EDGE_CURVE('',#36679,#36681,#4207,.T.);
#45678=EDGE_CURVE('',#36682,#36683,#20055,.T.);
#45679=EDGE_CURVE('',#36680,#36682,#4208,.F.);
#45680=EDGE_CURVE('',#36681,#36683,#4209,.T.);
#45681=EDGE_CURVE('',#36684,#36685,#20056,.T.);
#45682=EDGE_CURVE('',#36682,#36684,#4210,.F.);
#45683=EDGE_CURVE('',#36683,#36685,#4211,.T.);
#45684=EDGE_CURVE('',#36686,#36687,#20057,.T.);
#45685=EDGE_CURVE('',#36686,#36688,#4212,.T.);
#45686=EDGE_CURVE('',#36689,#36688,#30451,.T.);
#45687=EDGE_CURVE('',#36689,#36687,#4213,.T.);
#45688=EDGE_CURVE('',#36690,#36691,#20058,.T.);
#45689=EDGE_CURVE('',#36690,#36686,#4214,.T.);
#45690=EDGE_CURVE('',#36687,#36691,#4215,.T.);
#45691=EDGE_CURVE('',#36692,#36693,#20059,.T.);
#45692=EDGE_CURVE('',#36692,#36690,#4216,.T.);
#45693=EDGE_CURVE('',#36691,#36693,#4217,.T.);
#45694=EDGE_CURVE('',#36694,#36695,#20060,.T.);
#45695=EDGE_CURVE('',#36694,#36692,#4218,.T.);
#45696=EDGE_CURVE('',#36693,#36695,#4219,.T.);
#45697=EDGE_CURVE('',#36696,#36697,#20061,.T.);
#45698=EDGE_CURVE('',#36696,#36694,#4220,.T.);
#45699=EDGE_CURVE('',#36695,#36697,#4221,.T.);
#45700=EDGE_CURVE('',#36698,#36699,#20062,.T.);
#45701=EDGE_CURVE('',#36698,#36696,#4222,.T.);
#45702=EDGE_CURVE('',#36697,#36699,#4223,.T.);
#45703=EDGE_CURVE('',#36700,#36701,#20063,.T.);
#45704=EDGE_CURVE('',#36700,#36698,#4224,.T.);
#45705=EDGE_CURVE('',#36699,#36701,#4225,.T.);
#45706=EDGE_CURVE('',#36702,#36703,#20064,.T.);
#45707=EDGE_CURVE('',#36702,#36700,#4226,.T.);
#45708=EDGE_CURVE('',#36701,#36703,#4227,.T.);
#45709=EDGE_CURVE('',#36669,#36704,#20065,.T.);
#45710=EDGE_CURVE('',#36704,#36705,#4228,.T.);
#45711=EDGE_CURVE('',#36705,#36704,#4229,.T.);
#45712=EDGE_CURVE('',#36706,#36707,#4230,.T.);
#45713=EDGE_CURVE('',#36707,#36667,#20066,.T.);
#45714=EDGE_CURVE('',#36707,#36706,#4231,.T.);
#45715=EDGE_CURVE('',#36673,#36708,#20067,.T.);
#45716=EDGE_CURVE('',#36708,#36709,#4232,.T.);
#45717=EDGE_CURVE('',#36709,#36708,#4233,.T.);
#45718=EDGE_CURVE('',#36710,#36711,#4234,.T.);
#45719=EDGE_CURVE('',#36711,#36665,#20068,.T.);
#45720=EDGE_CURVE('',#36711,#36710,#4235,.T.);
#45721=EDGE_CURVE('',#36703,#36712,#4236,.T.);
#45722=EDGE_CURVE('',#36713,#36712,#20069,.T.);
#45723=EDGE_CURVE('',#36713,#36702,#4237,.T.);
#45724=EDGE_CURVE('',#36685,#36714,#4238,.T.);
#45725=EDGE_CURVE('',#36714,#36715,#4239,.T.);
#45726=EDGE_CURVE('',#36715,#36716,#30452,.T.);
#45727=EDGE_CURVE('',#36684,#36716,#4240,.F.);
#45728=EDGE_CURVE('',#36717,#36717,#30453,.T.);
#45729=EDGE_CURVE('',#36717,#36711,#20070,.T.);
#45730=EDGE_CURVE('',#36710,#36718,#20071,.T.);
#45731=EDGE_CURVE('',#36718,#36718,#30454,.T.);
#45732=EDGE_CURVE('',#36719,#36689,#336,.T.);
#45733=EDGE_CURVE('',#36720,#36719,#4081,.T.);
#45734=EDGE_CURVE('',#36712,#36720,#20072,.T.);
#45735=EDGE_CURVE('',#36688,#36721,#4241,.T.);
#45736=EDGE_CURVE('',#36645,#36713,#20073,.T.);
#45737=EDGE_CURVE('',#36659,#36721,#4082,.T.);
#45738=EDGE_CURVE('',#36722,#36716,#20074,.T.);
#45739=EDGE_CURVE('',#36660,#36722,#4083,.T.);
#45740=EDGE_CURVE('',#36663,#36646,#20075,.T.);
#45741=EDGE_CURVE('',#36715,#36723,#4242,.T.);
#45742=EDGE_CURVE('',#36724,#36664,#20076,.T.);
#45743=EDGE_CURVE('',#36724,#36723,#4084,.T.);
#45744=EDGE_CURVE('',#36723,#36719,#30455,.T.);
#45745=EDGE_CURVE('',#36720,#36724,#20077,.T.);
#45746=EDGE_CURVE('',#36721,#36722,#337,.T.);
#45747=EDGE_CURVE('',#36725,#36725,#30456,.T.);
#45748=EDGE_CURVE('',#36725,#36726,#30457,.T.);
#45749=EDGE_CURVE('',#36726,#36727,#30458,.T.);
#45750=EDGE_CURVE('',#36727,#36726,#30459,.T.);
#45751=EDGE_CURVE('',#36728,#36729,#4243,.F.);
#45752=EDGE_CURVE('',#36730,#36728,#20078,.T.);
#45753=EDGE_CURVE('',#36731,#36730,#4244,.F.);
#45754=EDGE_CURVE('',#36729,#36731,#20079,.T.);
#45755=EDGE_CURVE('',#36732,#36733,#30460,.T.);
#45756=EDGE_CURVE('',#36731,#36732,#4085,.T.);
#45757=EDGE_CURVE('',#36733,#36730,#4086,.T.);
#45758=EDGE_CURVE('',#36734,#36734,#30461,.T.);
#45759=EDGE_CURVE('',#36734,#36735,#20080,.T.);
#45760=EDGE_CURVE('',#36735,#36735,#30462,.T.);
#45761=EDGE_CURVE('',#36736,#36737,#30463,.T.);
#45762=EDGE_CURVE('',#36738,#36736,#4087,.T.);
#45763=EDGE_CURVE('',#36738,#36739,#4245,.T.);
#45764=EDGE_CURVE('',#36740,#36739,#4088,.T.);
#45765=EDGE_CURVE('',#36737,#36740,#30464,.T.);
#45766=EDGE_CURVE('',#36741,#36742,#30465,.T.);
#45767=EDGE_CURVE('',#36742,#36743,#30466,.T.);
#45768=EDGE_CURVE('',#36743,#36736,#30467,.T.);
#45769=EDGE_CURVE('',#36737,#36727,#20081,.T.);
#45770=EDGE_CURVE('',#36740,#36744,#30468,.T.);
#45771=EDGE_CURVE('',#36744,#36741,#30469,.T.);
#45772=EDGE_CURVE('',#36745,#36745,#30470,.T.);
#45773=EDGE_CURVE('',#36746,#36747,#30471,.T.);
#45774=EDGE_CURVE('',#36747,#36746,#30472,.T.);
#45775=EDGE_CURVE('',#36747,#36745,#30473,.T.);
#45776=EDGE_CURVE('',#36746,#36748,#20082,.T.);
#45777=EDGE_CURVE('',#36749,#36748,#30474,.T.);
#45778=EDGE_CURVE('',#36748,#36749,#30475,.T.);
#45779=EDGE_CURVE('',#36750,#36750,#30476,.T.);
#45780=EDGE_CURVE('',#36750,#36749,#30477,.T.);
#45781=EDGE_CURVE('',#36751,#36751,#30478,.T.);
#45782=EDGE_CURVE('',#36751,#36752,#20083,.T.);
#45783=EDGE_CURVE('',#36752,#36752,#30479,.T.);
#45784=EDGE_CURVE('',#36728,#36741,#4089,.T.);
#45785=EDGE_CURVE('',#36742,#36729,#4090,.T.);
#45786=EDGE_CURVE('',#36753,#36744,#4091,.T.);
#45787=EDGE_CURVE('',#36753,#36754,#4246,.T.);
#45788=EDGE_CURVE('',#36741,#36754,#4092,.T.);
#45789=EDGE_CURVE('',#36755,#36740,#4093,.T.);
#45790=EDGE_CURVE('',#36755,#36756,#4247,.T.);
#45791=EDGE_CURVE('',#36744,#36756,#4094,.T.);
#45792=EDGE_CURVE('',#36757,#36743,#4095,.T.);
#45793=EDGE_CURVE('',#36757,#36758,#4248,.T.);
#45794=EDGE_CURVE('',#36736,#36758,#4096,.T.);
#45795=EDGE_CURVE('',#36759,#36742,#4097,.T.);
#45796=EDGE_CURVE('',#36759,#36760,#4249,.T.);
#45797=EDGE_CURVE('',#36743,#36760,#4098,.T.);
#45798=EDGE_CURVE('',#36733,#36761,#30480,.T.);
#45799=EDGE_CURVE('',#36761,#36762,#30481,.T.);
#45800=EDGE_CURVE('',#36762,#36763,#30482,.T.);
#45801=EDGE_CURVE('',#36763,#36764,#30483,.T.);
#45802=EDGE_CURVE('',#36764,#36732,#30484,.T.);
#45803=EDGE_CURVE('',#36765,#36764,#4099,.T.);
#45804=EDGE_CURVE('',#36765,#36766,#4250,.T.);
#45805=EDGE_CURVE('',#36732,#36766,#4100,.T.);
#45806=EDGE_CURVE('',#36767,#36763,#4101,.T.);
#45807=EDGE_CURVE('',#36767,#36768,#4251,.T.);
#45808=EDGE_CURVE('',#36764,#36768,#4102,.T.);
#45809=EDGE_CURVE('',#36769,#36762,#4103,.T.);
#45810=EDGE_CURVE('',#36769,#36770,#4252,.T.);
#45811=EDGE_CURVE('',#36763,#36770,#4104,.T.);
#45812=EDGE_CURVE('',#36771,#36761,#4105,.T.);
#45813=EDGE_CURVE('',#36771,#36772,#4253,.T.);
#45814=EDGE_CURVE('',#36762,#36772,#4106,.T.);
#45815=EDGE_CURVE('',#36773,#36733,#4107,.T.);
#45816=EDGE_CURVE('',#36773,#36774,#4254,.T.);
#45817=EDGE_CURVE('',#36761,#36774,#4108,.T.);
#45818=EDGE_CURVE('',#36754,#36773,#20084,.T.);
#45819=EDGE_CURVE('',#36774,#36753,#20085,.T.);
#45820=EDGE_CURVE('',#36756,#36771,#20086,.T.);
#45821=EDGE_CURVE('',#36772,#36755,#20087,.T.);
#45822=EDGE_CURVE('',#36739,#36769,#20088,.T.);
#45823=EDGE_CURVE('',#36758,#36767,#20089,.T.);
#45824=EDGE_CURVE('',#36770,#36738,#20090,.T.);
#45825=EDGE_CURVE('',#36760,#36765,#20091,.T.);
#45826=EDGE_CURVE('',#36768,#36757,#20092,.T.);
#45827=EDGE_CURVE('',#36766,#36759,#20093,.T.);
#45828=EDGE_CURVE('',#36775,#36775,#30485,.T.);
#45829=EDGE_CURVE('',#36775,#36776,#20094,.T.);
#45830=EDGE_CURVE('',#36776,#36776,#30486,.T.);
#45831=EDGE_CURVE('',#36777,#36777,#30487,.T.);
#45832=EDGE_CURVE('',#36777,#36778,#20095,.T.);
#45833=EDGE_CURVE('',#36778,#36778,#30488,.T.);
#45834=EDGE_CURVE('',#36779,#36779,#30489,.T.);
#45835=EDGE_CURVE('',#36779,#36780,#20096,.T.);
#45836=EDGE_CURVE('',#36780,#36780,#30490,.T.);
#45837=EDGE_CURVE('',#36781,#36781,#30491,.T.);
#45838=EDGE_CURVE('',#36781,#36782,#20097,.T.);
#45839=EDGE_CURVE('',#36782,#36782,#30492,.T.);
#45840=EDGE_CURVE('',#36783,#36783,#30493,.T.);
#45841=EDGE_CURVE('',#36783,#36784,#20098,.T.);
#45842=EDGE_CURVE('',#36784,#36784,#30494,.T.);
#45843=EDGE_CURVE('',#36785,#36785,#30495,.T.);
#45844=EDGE_CURVE('',#36785,#36786,#20099,.T.);
#45845=EDGE_CURVE('',#36786,#36786,#30496,.T.);
#45846=EDGE_CURVE('',#36787,#36787,#30497,.T.);
#45847=EDGE_CURVE('',#36787,#36788,#20100,.T.);
#45848=EDGE_CURVE('',#36788,#36788,#30498,.T.);
#45849=EDGE_CURVE('',#36789,#36789,#30499,.T.);
#45850=EDGE_CURVE('',#36789,#36790,#20101,.T.);
#45851=EDGE_CURVE('',#36790,#36790,#30500,.T.);
#45852=EDGE_CURVE('',#36791,#36792,#30501,.T.);
#45853=EDGE_CURVE('',#36792,#36791,#30502,.T.);
#45854=EDGE_CURVE('',#36792,#36793,#30503,.T.);
#45855=EDGE_CURVE('',#36793,#36793,#30504,.T.);
#45856=EDGE_CURVE('',#36794,#36794,#30505,.T.);
#45857=EDGE_CURVE('',#36794,#36795,#30506,.T.);
#45858=EDGE_CURVE('',#36796,#36795,#30507,.T.);
#45859=EDGE_CURVE('',#36795,#36796,#30508,.T.);
#45860=EDGE_CURVE('',#36797,#36797,#30509,.T.);
#45861=EDGE_CURVE('',#36797,#36796,#20102,.T.);
#45862=EDGE_CURVE('',#36791,#36798,#20103,.T.);
#45863=EDGE_CURVE('',#36798,#36798,#30510,.T.);
#45864=EDGE_CURVE('',#36799,#36799,#30511,.T.);
#45865=EDGE_CURVE('',#36799,#36800,#30512,.T.);
#45866=EDGE_CURVE('',#36801,#36800,#30513,.T.);
#45867=EDGE_CURVE('',#36800,#36801,#30514,.T.);
#45868=EDGE_CURVE('',#36802,#36803,#30515,.T.);
#45869=EDGE_CURVE('',#36803,#36802,#30516,.T.);
#45870=EDGE_CURVE('',#36803,#36804,#30517,.T.);
#45871=EDGE_CURVE('',#36804,#36804,#30518,.T.);
#45872=EDGE_CURVE('',#36805,#36805,#30519,.T.);
#45873=EDGE_CURVE('',#36805,#36801,#20104,.T.);
#45874=EDGE_CURVE('',#36802,#36806,#20105,.T.);
#45875=EDGE_CURVE('',#36806,#36806,#30520,.T.);
#45876=EDGE_CURVE('',#36807,#36807,#30521,.T.);
#45877=EDGE_CURVE('',#36807,#36808,#20106,.T.);
#45878=EDGE_CURVE('',#36808,#36808,#30522,.T.);
#45879=EDGE_CURVE('',#36809,#36809,#30523,.T.);
#45880=EDGE_CURVE('',#36809,#36810,#20107,.T.);
#45881=EDGE_CURVE('',#36810,#36810,#30524,.T.);
#45882=EDGE_CURVE('',#36811,#36812,#30525,.T.);
#45883=EDGE_CURVE('',#36813,#36811,#30526,.T.);
#45884=EDGE_CURVE('',#36814,#36813,#30527,.T.);
#45885=EDGE_CURVE('',#36814,#36812,#30528,.T.);
#45886=EDGE_CURVE('',#36815,#36816,#30529,.T.);
#45887=EDGE_CURVE('',#36817,#36815,#30530,.T.);
#45888=EDGE_CURVE('',#36818,#36817,#30531,.T.);
#45889=EDGE_CURVE('',#36818,#36816,#30532,.T.);
#45890=EDGE_CURVE('',#36819,#36820,#30533,.T.);
#45891=EDGE_CURVE('',#36821,#36819,#30534,.T.);
#45892=EDGE_CURVE('',#36822,#36821,#30535,.T.);
#45893=EDGE_CURVE('',#36822,#36820,#30536,.T.);
#45894=EDGE_CURVE('',#36823,#36824,#30537,.T.);
#45895=EDGE_CURVE('',#36825,#36823,#30538,.T.);
#45896=EDGE_CURVE('',#36826,#36825,#30539,.T.);
#45897=EDGE_CURVE('',#36826,#36827,#30540,.T.);
#45898=EDGE_CURVE('',#36824,#36827,#30541,.T.);
#45899=EDGE_CURVE('',#36828,#36828,#30542,.T.);
#45900=EDGE_CURVE('',#36828,#36829,#30543,.T.);
#45901=EDGE_CURVE('',#36830,#36829,#30544,.T.);
#45902=EDGE_CURVE('',#36829,#36830,#30545,.T.);
#45903=EDGE_CURVE('',#36831,#36831,#30546,.T.);
#45904=EDGE_CURVE('',#36831,#36832,#30547,.T.);
#45905=EDGE_CURVE('',#36832,#36832,#30548,.T.);
#45906=EDGE_CURVE('',#36833,#36833,#30549,.T.);
#45907=EDGE_CURVE('',#36833,#36834,#30550,.T.);
#45908=EDGE_CURVE('',#36835,#36834,#30551,.T.);
#45909=EDGE_CURVE('',#36834,#36835,#30552,.T.);
#45910=EDGE_CURVE('',#36836,#36836,#30553,.T.);
#45911=EDGE_CURVE('',#36836,#36837,#30554,.T.);
#45912=EDGE_CURVE('',#36837,#36837,#30555,.T.);
#45913=EDGE_CURVE('',#36838,#36838,#30556,.T.);
#45914=EDGE_CURVE('',#36838,#36839,#20108,.T.);
#45915=EDGE_CURVE('',#36839,#36839,#30557,.T.);
#45916=EDGE_CURVE('',#36839,#36836,#20109,.T.);
#45917=EDGE_CURVE('',#36840,#36841,#30558,.T.);
#45918=EDGE_CURVE('',#36841,#36842,#4255,.T.);
#45919=EDGE_CURVE('',#36842,#36843,#20110,.T.);
#45920=EDGE_CURVE('',#36843,#36844,#30559,.T.);
#45921=EDGE_CURVE('',#36844,#36845,#20111,.T.);
#45922=EDGE_CURVE('',#36845,#36846,#4256,.T.);
#45923=EDGE_CURVE('',#36846,#36847,#30560,.T.);
#45924=EDGE_CURVE('',#36847,#36848,#4257,.T.);
#45925=EDGE_CURVE('',#36848,#36849,#20112,.T.);
#45926=EDGE_CURVE('',#36849,#36850,#30561,.T.);
#45927=EDGE_CURVE('',#36850,#36851,#20113,.T.);
#45928=EDGE_CURVE('',#36851,#36852,#4258,.T.);
#45929=EDGE_CURVE('',#36852,#36853,#30562,.T.);
#45930=EDGE_CURVE('',#36853,#36854,#4259,.T.);
#45931=EDGE_CURVE('',#36854,#36855,#20114,.T.);
#45932=EDGE_CURVE('',#36855,#36856,#30563,.T.);
#45933=EDGE_CURVE('',#36856,#36857,#20115,.T.);
#45934=EDGE_CURVE('',#36857,#36858,#4260,.T.);
#45935=EDGE_CURVE('',#36858,#36859,#30564,.T.);
#45936=EDGE_CURVE('',#36859,#36860,#4261,.T.);
#45937=EDGE_CURVE('',#36860,#36861,#20116,.T.);
#45938=EDGE_CURVE('',#36861,#36862,#30565,.T.);
#45939=EDGE_CURVE('',#36862,#36863,#20117,.T.);
#45940=EDGE_CURVE('',#36863,#36864,#4262,.T.);
#45941=EDGE_CURVE('',#36864,#36865,#30566,.T.);
#45942=EDGE_CURVE('',#36865,#36866,#4263,.T.);
#45943=EDGE_CURVE('',#36866,#36867,#20118,.T.);
#45944=EDGE_CURVE('',#36867,#36868,#30567,.T.);
#45945=EDGE_CURVE('',#36868,#36869,#20119,.T.);
#45946=EDGE_CURVE('',#36869,#36870,#4264,.T.);
#45947=EDGE_CURVE('',#36870,#36871,#30568,.T.);
#45948=EDGE_CURVE('',#36871,#36872,#4265,.T.);
#45949=EDGE_CURVE('',#36872,#36873,#20120,.T.);
#45950=EDGE_CURVE('',#36873,#36874,#30569,.T.);
#45951=EDGE_CURVE('',#36874,#36875,#20121,.T.);
#45952=EDGE_CURVE('',#36875,#36876,#4266,.T.);
#45953=EDGE_CURVE('',#36876,#36877,#30570,.T.);
#45954=EDGE_CURVE('',#36877,#36878,#4267,.T.);
#45955=EDGE_CURVE('',#36878,#36879,#20122,.T.);
#45956=EDGE_CURVE('',#36879,#36880,#30571,.T.);
#45957=EDGE_CURVE('',#36880,#36881,#20123,.T.);
#45958=EDGE_CURVE('',#36881,#36882,#4268,.T.);
#45959=EDGE_CURVE('',#36882,#36883,#30572,.T.);
#45960=EDGE_CURVE('',#36883,#36884,#4269,.T.);
#45961=EDGE_CURVE('',#36884,#36885,#20124,.T.);
#45962=EDGE_CURVE('',#36885,#36886,#30573,.T.);
#45963=EDGE_CURVE('',#36886,#36887,#20125,.T.);
#45964=EDGE_CURVE('',#36887,#36888,#4270,.T.);
#45965=EDGE_CURVE('',#36888,#36889,#30574,.T.);
#45966=EDGE_CURVE('',#36889,#36890,#4271,.T.);
#45967=EDGE_CURVE('',#36890,#36891,#20126,.T.);
#45968=EDGE_CURVE('',#36891,#36892,#30575,.T.);
#45969=EDGE_CURVE('',#36892,#36893,#20127,.T.);
#45970=EDGE_CURVE('',#36893,#36894,#4272,.T.);
#45971=EDGE_CURVE('',#36894,#36895,#30576,.T.);
#45972=EDGE_CURVE('',#36895,#36896,#4273,.T.);
#45973=EDGE_CURVE('',#36896,#36897,#20128,.T.);
#45974=EDGE_CURVE('',#36897,#36898,#30577,.T.);
#45975=EDGE_CURVE('',#36898,#36899,#20129,.T.);
#45976=EDGE_CURVE('',#36899,#36900,#4274,.T.);
#45977=EDGE_CURVE('',#36900,#36901,#30578,.T.);
#45978=EDGE_CURVE('',#36901,#36902,#4275,.T.);
#45979=EDGE_CURVE('',#36902,#36903,#20130,.T.);
#45980=EDGE_CURVE('',#36903,#36904,#30579,.T.);
#45981=EDGE_CURVE('',#36904,#36905,#20131,.T.);
#45982=EDGE_CURVE('',#36905,#36906,#4276,.T.);
#45983=EDGE_CURVE('',#36906,#36907,#30580,.T.);
#45984=EDGE_CURVE('',#36907,#36908,#4277,.T.);
#45985=EDGE_CURVE('',#36908,#36909,#20132,.T.);
#45986=EDGE_CURVE('',#36909,#36910,#30581,.T.);
#45987=EDGE_CURVE('',#36910,#36911,#20133,.T.);
#45988=EDGE_CURVE('',#36911,#36912,#4278,.T.);
#45989=EDGE_CURVE('',#36912,#36913,#30582,.T.);
#45990=EDGE_CURVE('',#36913,#36914,#4279,.T.);
#45991=EDGE_CURVE('',#36914,#36915,#20134,.T.);
#45992=EDGE_CURVE('',#36915,#36916,#30583,.T.);
#45993=EDGE_CURVE('',#36916,#36917,#20135,.T.);
#45994=EDGE_CURVE('',#36917,#36918,#4280,.T.);
#45995=EDGE_CURVE('',#36918,#36919,#30584,.T.);
#45996=EDGE_CURVE('',#36919,#36920,#4281,.T.);
#45997=EDGE_CURVE('',#36920,#36921,#20136,.T.);
#45998=EDGE_CURVE('',#36921,#36922,#30585,.T.);
#45999=EDGE_CURVE('',#36922,#36923,#20137,.T.);
#46000=EDGE_CURVE('',#36923,#36924,#4282,.T.);
#46001=EDGE_CURVE('',#36924,#36925,#30586,.T.);
#46002=EDGE_CURVE('',#36925,#36926,#4283,.T.);
#46003=EDGE_CURVE('',#36926,#36927,#20138,.T.);
#46004=EDGE_CURVE('',#36927,#36928,#30587,.T.);
#46005=EDGE_CURVE('',#36928,#36929,#20139,.T.);
#46006=EDGE_CURVE('',#36929,#36930,#4284,.T.);
#46007=EDGE_CURVE('',#36930,#36931,#30588,.T.);
#46008=EDGE_CURVE('',#36931,#36932,#4285,.T.);
#46009=EDGE_CURVE('',#36932,#36933,#20140,.T.);
#46010=EDGE_CURVE('',#36933,#36934,#30589,.T.);
#46011=EDGE_CURVE('',#36934,#36935,#20141,.T.);
#46012=EDGE_CURVE('',#36935,#36936,#4286,.T.);
#46013=EDGE_CURVE('',#36936,#36937,#30590,.T.);
#46014=EDGE_CURVE('',#36937,#36938,#4287,.T.);
#46015=EDGE_CURVE('',#36938,#36939,#20142,.T.);
#46016=EDGE_CURVE('',#36939,#36940,#30591,.T.);
#46017=EDGE_CURVE('',#36940,#36941,#20143,.T.);
#46018=EDGE_CURVE('',#36941,#36942,#4288,.T.);
#46019=EDGE_CURVE('',#36942,#36943,#30592,.T.);
#46020=EDGE_CURVE('',#36943,#36944,#4289,.T.);
#46021=EDGE_CURVE('',#36944,#36945,#20144,.T.);
#46022=EDGE_CURVE('',#36945,#36946,#30593,.T.);
#46023=EDGE_CURVE('',#36946,#36947,#20145,.T.);
#46024=EDGE_CURVE('',#36947,#36948,#4290,.T.);
#46025=EDGE_CURVE('',#36948,#36949,#30594,.T.);
#46026=EDGE_CURVE('',#36949,#36950,#4291,.T.);
#46027=EDGE_CURVE('',#36950,#36951,#20146,.T.);
#46028=EDGE_CURVE('',#36951,#36952,#30595,.T.);
#46029=EDGE_CURVE('',#36952,#36953,#20147,.T.);
#46030=EDGE_CURVE('',#36953,#36954,#4292,.T.);
#46031=EDGE_CURVE('',#36954,#36955,#30596,.T.);
#46032=EDGE_CURVE('',#36955,#36956,#4293,.T.);
#46033=EDGE_CURVE('',#36956,#36957,#20148,.T.);
#46034=EDGE_CURVE('',#36957,#36958,#30597,.T.);
#46035=EDGE_CURVE('',#36958,#36959,#20149,.T.);
#46036=EDGE_CURVE('',#36959,#36960,#4294,.T.);
#46037=EDGE_CURVE('',#36960,#36961,#30598,.T.);
#46038=EDGE_CURVE('',#36961,#36962,#4295,.T.);
#46039=EDGE_CURVE('',#36962,#36963,#20150,.T.);
#46040=EDGE_CURVE('',#36963,#36964,#30599,.T.);
#46041=EDGE_CURVE('',#36964,#36965,#20151,.T.);
#46042=EDGE_CURVE('',#36965,#36966,#4296,.T.);
#46043=EDGE_CURVE('',#36966,#36967,#30600,.T.);
#46044=EDGE_CURVE('',#36967,#36968,#4297,.T.);
#46045=EDGE_CURVE('',#36968,#36969,#20152,.T.);
#46046=EDGE_CURVE('',#36969,#36970,#30601,.T.);
#46047=EDGE_CURVE('',#36970,#36971,#20153,.T.);
#46048=EDGE_CURVE('',#36971,#36972,#4298,.T.);
#46049=EDGE_CURVE('',#36972,#36973,#30602,.T.);
#46050=EDGE_CURVE('',#36973,#36974,#4299,.T.);
#46051=EDGE_CURVE('',#36974,#36975,#20154,.T.);
#46052=EDGE_CURVE('',#36975,#36976,#30603,.T.);
#46053=EDGE_CURVE('',#36976,#36977,#20155,.T.);
#46054=EDGE_CURVE('',#36977,#36978,#4300,.T.);
#46055=EDGE_CURVE('',#36978,#36979,#30604,.T.);
#46056=EDGE_CURVE('',#36979,#36980,#4301,.T.);
#46057=EDGE_CURVE('',#36980,#36981,#20156,.T.);
#46058=EDGE_CURVE('',#36981,#36982,#30605,.T.);
#46059=EDGE_CURVE('',#36982,#36983,#20157,.T.);
#46060=EDGE_CURVE('',#36983,#36984,#4302,.T.);
#46061=EDGE_CURVE('',#36984,#36985,#30606,.T.);
#46062=EDGE_CURVE('',#36985,#36986,#4303,.T.);
#46063=EDGE_CURVE('',#36986,#36987,#20158,.T.);
#46064=EDGE_CURVE('',#36987,#36988,#30607,.T.);
#46065=EDGE_CURVE('',#36988,#36989,#20159,.T.);
#46066=EDGE_CURVE('',#36989,#36990,#4304,.T.);
#46067=EDGE_CURVE('',#36990,#36991,#30608,.T.);
#46068=EDGE_CURVE('',#36991,#36992,#4305,.T.);
#46069=EDGE_CURVE('',#36992,#36993,#20160,.T.);
#46070=EDGE_CURVE('',#36993,#36994,#30609,.T.);
#46071=EDGE_CURVE('',#36994,#36995,#20161,.T.);
#46072=EDGE_CURVE('',#36995,#36996,#4306,.T.);
#46073=EDGE_CURVE('',#36996,#36997,#30610,.T.);
#46074=EDGE_CURVE('',#36997,#36998,#4307,.T.);
#46075=EDGE_CURVE('',#36998,#36999,#20162,.T.);
#46076=EDGE_CURVE('',#36999,#37000,#30611,.T.);
#46077=EDGE_CURVE('',#37000,#37001,#20163,.T.);
#46078=EDGE_CURVE('',#37001,#37002,#4308,.T.);
#46079=EDGE_CURVE('',#37002,#37003,#30612,.T.);
#46080=EDGE_CURVE('',#37003,#37004,#4309,.T.);
#46081=EDGE_CURVE('',#37004,#37005,#20164,.T.);
#46082=EDGE_CURVE('',#37005,#37006,#30613,.T.);
#46083=EDGE_CURVE('',#37006,#37007,#20165,.T.);
#46084=EDGE_CURVE('',#37007,#37008,#4310,.T.);
#46085=EDGE_CURVE('',#37008,#37009,#30614,.T.);
#46086=EDGE_CURVE('',#37009,#37010,#4311,.T.);
#46087=EDGE_CURVE('',#37010,#37011,#20166,.T.);
#46088=EDGE_CURVE('',#37011,#37012,#30615,.T.);
#46089=EDGE_CURVE('',#37012,#37013,#20167,.T.);
#46090=EDGE_CURVE('',#37013,#37014,#4312,.T.);
#46091=EDGE_CURVE('',#37014,#37015,#30616,.T.);
#46092=EDGE_CURVE('',#37015,#37016,#4313,.T.);
#46093=EDGE_CURVE('',#37016,#37017,#20168,.T.);
#46094=EDGE_CURVE('',#37017,#37018,#30617,.T.);
#46095=EDGE_CURVE('',#37018,#37019,#20169,.T.);
#46096=EDGE_CURVE('',#37019,#36823,#4314,.T.);
#46097=EDGE_CURVE('',#36824,#36835,#20170,.T.);
#46098=EDGE_CURVE('',#36827,#37020,#4315,.T.);
#46099=EDGE_CURVE('',#37020,#37021,#20171,.T.);
#46100=EDGE_CURVE('',#37021,#37022,#30618,.T.);
#46101=EDGE_CURVE('',#37022,#37023,#20172,.T.);
#46102=EDGE_CURVE('',#37023,#37024,#4316,.T.);
#46103=EDGE_CURVE('',#37024,#37025,#30619,.T.);
#46104=EDGE_CURVE('',#37025,#37026,#4317,.T.);
#46105=EDGE_CURVE('',#37026,#37027,#20173,.T.);
#46106=EDGE_CURVE('',#37027,#37028,#30620,.T.);
#46107=EDGE_CURVE('',#37028,#37029,#20174,.T.);
#46108=EDGE_CURVE('',#37029,#37030,#4318,.T.);
#46109=EDGE_CURVE('',#37030,#37031,#30621,.T.);
#46110=EDGE_CURVE('',#37031,#37032,#4319,.T.);
#46111=EDGE_CURVE('',#37032,#37033,#20175,.T.);
#46112=EDGE_CURVE('',#37033,#37034,#30622,.T.);
#46113=EDGE_CURVE('',#37034,#37035,#20176,.T.);
#46114=EDGE_CURVE('',#37035,#37036,#4320,.T.);
#46115=EDGE_CURVE('',#37036,#37037,#30623,.T.);
#46116=EDGE_CURVE('',#37037,#37038,#4321,.T.);
#46117=EDGE_CURVE('',#37038,#37039,#20177,.T.);
#46118=EDGE_CURVE('',#37039,#37040,#30624,.T.);
#46119=EDGE_CURVE('',#37040,#37041,#20178,.T.);
#46120=EDGE_CURVE('',#37041,#37042,#4322,.T.);
#46121=EDGE_CURVE('',#37042,#37043,#30625,.T.);
#46122=EDGE_CURVE('',#37043,#37044,#4323,.T.);
#46123=EDGE_CURVE('',#37044,#37045,#20179,.T.);
#46124=EDGE_CURVE('',#37045,#37046,#30626,.T.);
#46125=EDGE_CURVE('',#37046,#37047,#20180,.T.);
#46126=EDGE_CURVE('',#37047,#37048,#4324,.T.);
#46127=EDGE_CURVE('',#37048,#37049,#30627,.T.);
#46128=EDGE_CURVE('',#37049,#37050,#4325,.T.);
#46129=EDGE_CURVE('',#37050,#37051,#20181,.T.);
#46130=EDGE_CURVE('',#37051,#37052,#30628,.T.);
#46131=EDGE_CURVE('',#37052,#37053,#20182,.T.);
#46132=EDGE_CURVE('',#37053,#37054,#4326,.T.);
#46133=EDGE_CURVE('',#37054,#37055,#30629,.T.);
#46134=EDGE_CURVE('',#37055,#37056,#4327,.T.);
#46135=EDGE_CURVE('',#37056,#37057,#20183,.T.);
#46136=EDGE_CURVE('',#37057,#37058,#30630,.T.);
#46137=EDGE_CURVE('',#37058,#37059,#20184,.T.);
#46138=EDGE_CURVE('',#37059,#37060,#4328,.T.);
#46139=EDGE_CURVE('',#37060,#37061,#30631,.T.);
#46140=EDGE_CURVE('',#37061,#37062,#4329,.T.);
#46141=EDGE_CURVE('',#37062,#37063,#20185,.T.);
#46142=EDGE_CURVE('',#37063,#37064,#30632,.T.);
#46143=EDGE_CURVE('',#37064,#37065,#20186,.T.);
#46144=EDGE_CURVE('',#37065,#37066,#4330,.T.);
#46145=EDGE_CURVE('',#37066,#37067,#30633,.T.);
#46146=EDGE_CURVE('',#37067,#37068,#4331,.T.);
#46147=EDGE_CURVE('',#37068,#37069,#20187,.T.);
#46148=EDGE_CURVE('',#37069,#37070,#30634,.T.);
#46149=EDGE_CURVE('',#37070,#37071,#20188,.T.);
#46150=EDGE_CURVE('',#37071,#37072,#4332,.T.);
#46151=EDGE_CURVE('',#37072,#37073,#30635,.T.);
#46152=EDGE_CURVE('',#37073,#37074,#4333,.T.);
#46153=EDGE_CURVE('',#37074,#37075,#20189,.T.);
#46154=EDGE_CURVE('',#37075,#37076,#30636,.T.);
#46155=EDGE_CURVE('',#37076,#37077,#20190,.T.);
#46156=EDGE_CURVE('',#37077,#37078,#4334,.T.);
#46157=EDGE_CURVE('',#37078,#37079,#30637,.T.);
#46158=EDGE_CURVE('',#37079,#37080,#4335,.T.);
#46159=EDGE_CURVE('',#37080,#37081,#20191,.T.);
#46160=EDGE_CURVE('',#37081,#37082,#30638,.T.);
#46161=EDGE_CURVE('',#37082,#37083,#20192,.T.);
#46162=EDGE_CURVE('',#37083,#37084,#4336,.T.);
#46163=EDGE_CURVE('',#37084,#37085,#30639,.T.);
#46164=EDGE_CURVE('',#37085,#37086,#4337,.T.);
#46165=EDGE_CURVE('',#37086,#37087,#20193,.T.);
#46166=EDGE_CURVE('',#37087,#37088,#30640,.T.);
#46167=EDGE_CURVE('',#37088,#37089,#20194,.T.);
#46168=EDGE_CURVE('',#37089,#37090,#4338,.T.);
#46169=EDGE_CURVE('',#37090,#37091,#30641,.T.);
#46170=EDGE_CURVE('',#37091,#37092,#4339,.T.);
#46171=EDGE_CURVE('',#37092,#37093,#20195,.T.);
#46172=EDGE_CURVE('',#37093,#37094,#30642,.T.);
#46173=EDGE_CURVE('',#37094,#37095,#20196,.T.);
#46174=EDGE_CURVE('',#37095,#37096,#4340,.T.);
#46175=EDGE_CURVE('',#37096,#37097,#30643,.T.);
#46176=EDGE_CURVE('',#37097,#37098,#4341,.T.);
#46177=EDGE_CURVE('',#37098,#37099,#20197,.T.);
#46178=EDGE_CURVE('',#37099,#37100,#30644,.T.);
#46179=EDGE_CURVE('',#37100,#37101,#20198,.T.);
#46180=EDGE_CURVE('',#37101,#37102,#4342,.T.);
#46181=EDGE_CURVE('',#37102,#37103,#30645,.T.);
#46182=EDGE_CURVE('',#37103,#37104,#4343,.T.);
#46183=EDGE_CURVE('',#37104,#37105,#20199,.T.);
#46184=EDGE_CURVE('',#37105,#37106,#30646,.T.);
#46185=EDGE_CURVE('',#37106,#37107,#20200,.T.);
#46186=EDGE_CURVE('',#37107,#36815,#4344,.T.);
#46187=EDGE_CURVE('',#36816,#37108,#4345,.T.);
#46188=EDGE_CURVE('',#37108,#37109,#20201,.T.);
#46189=EDGE_CURVE('',#37109,#37110,#30647,.T.);
#46190=EDGE_CURVE('',#37110,#37111,#20202,.T.);
#46191=EDGE_CURVE('',#37111,#37112,#4346,.T.);
#46192=EDGE_CURVE('',#37112,#37113,#30648,.T.);
#46193=EDGE_CURVE('',#37113,#37114,#4347,.T.);
#46194=EDGE_CURVE('',#37114,#37115,#20203,.T.);
#46195=EDGE_CURVE('',#37115,#37116,#30649,.T.);
#46196=EDGE_CURVE('',#37116,#37117,#20204,.T.);
#46197=EDGE_CURVE('',#37117,#37118,#4348,.T.);
#46198=EDGE_CURVE('',#37118,#37119,#30650,.T.);
#46199=EDGE_CURVE('',#37119,#37120,#4349,.T.);
#46200=EDGE_CURVE('',#37120,#37121,#20205,.T.);
#46201=EDGE_CURVE('',#37121,#37122,#30651,.T.);
#46202=EDGE_CURVE('',#37122,#37123,#20206,.T.);
#46203=EDGE_CURVE('',#37123,#37124,#4350,.T.);
#46204=EDGE_CURVE('',#37124,#37125,#30652,.T.);
#46205=EDGE_CURVE('',#37125,#37126,#4351,.T.);
#46206=EDGE_CURVE('',#37126,#37127,#20207,.T.);
#46207=EDGE_CURVE('',#37127,#37128,#30653,.T.);
#46208=EDGE_CURVE('',#37128,#37129,#20208,.T.);
#46209=EDGE_CURVE('',#37129,#37130,#4352,.T.);
#46210=EDGE_CURVE('',#37130,#37131,#30654,.T.);
#46211=EDGE_CURVE('',#37131,#37132,#4353,.T.);
#46212=EDGE_CURVE('',#37132,#37133,#20209,.T.);
#46213=EDGE_CURVE('',#37133,#37134,#30655,.T.);
#46214=EDGE_CURVE('',#37134,#37135,#20210,.T.);
#46215=EDGE_CURVE('',#37135,#37136,#4354,.T.);
#46216=EDGE_CURVE('',#37136,#37137,#30656,.T.);
#46217=EDGE_CURVE('',#37137,#37138,#4355,.T.);
#46218=EDGE_CURVE('',#37138,#37139,#20211,.T.);
#46219=EDGE_CURVE('',#37139,#37140,#30657,.T.);
#46220=EDGE_CURVE('',#37140,#37141,#20212,.T.);
#46221=EDGE_CURVE('',#37141,#37142,#4356,.T.);
#46222=EDGE_CURVE('',#37142,#37143,#30658,.T.);
#46223=EDGE_CURVE('',#37143,#37144,#4357,.T.);
#46224=EDGE_CURVE('',#37144,#37145,#20213,.T.);
#46225=EDGE_CURVE('',#37145,#37146,#30659,.T.);
#46226=EDGE_CURVE('',#37146,#37147,#20214,.T.);
#46227=EDGE_CURVE('',#37147,#37148,#4358,.T.);
#46228=EDGE_CURVE('',#37148,#37149,#30660,.T.);
#46229=EDGE_CURVE('',#37149,#37150,#4359,.T.);
#46230=EDGE_CURVE('',#37150,#37151,#20215,.T.);
#46231=EDGE_CURVE('',#37151,#37152,#30661,.T.);
#46232=EDGE_CURVE('',#37152,#37153,#20216,.T.);
#46233=EDGE_CURVE('',#37153,#37154,#4360,.T.);
#46234=EDGE_CURVE('',#37154,#37155,#30662,.T.);
#46235=EDGE_CURVE('',#37155,#37156,#4361,.T.);
#46236=EDGE_CURVE('',#37156,#37157,#20217,.T.);
#46237=EDGE_CURVE('',#37157,#37158,#30663,.T.);
#46238=EDGE_CURVE('',#37158,#37159,#20218,.T.);
#46239=EDGE_CURVE('',#37159,#37160,#4362,.T.);
#46240=EDGE_CURVE('',#37160,#37161,#30664,.T.);
#46241=EDGE_CURVE('',#37161,#37162,#4363,.T.);
#46242=EDGE_CURVE('',#37162,#37163,#20219,.T.);
#46243=EDGE_CURVE('',#37163,#37164,#30665,.T.);
#46244=EDGE_CURVE('',#37164,#37165,#20220,.T.);
#46245=EDGE_CURVE('',#37165,#37166,#4364,.T.);
#46246=EDGE_CURVE('',#37166,#37167,#30666,.T.);
#46247=EDGE_CURVE('',#37167,#37168,#4365,.T.);
#46248=EDGE_CURVE('',#37168,#37169,#20221,.T.);
#46249=EDGE_CURVE('',#37169,#37170,#30667,.T.);
#46250=EDGE_CURVE('',#37170,#37171,#20222,.T.);
#46251=EDGE_CURVE('',#37171,#37172,#4366,.T.);
#46252=EDGE_CURVE('',#37172,#37173,#30668,.T.);
#46253=EDGE_CURVE('',#37173,#37174,#4367,.T.);
#46254=EDGE_CURVE('',#37174,#37175,#20223,.T.);
#46255=EDGE_CURVE('',#37175,#37176,#30669,.T.);
#46256=EDGE_CURVE('',#37176,#37177,#20224,.T.);
#46257=EDGE_CURVE('',#37177,#37178,#4368,.T.);
#46258=EDGE_CURVE('',#37178,#37179,#30670,.T.);
#46259=EDGE_CURVE('',#37179,#37180,#4369,.T.);
#46260=EDGE_CURVE('',#37180,#37181,#20225,.T.);
#46261=EDGE_CURVE('',#37181,#37182,#30671,.T.);
#46262=EDGE_CURVE('',#37182,#37183,#20226,.T.);
#46263=EDGE_CURVE('',#37183,#37184,#4370,.T.);
#46264=EDGE_CURVE('',#37184,#37185,#30672,.T.);
#46265=EDGE_CURVE('',#37185,#37186,#4371,.T.);
#46266=EDGE_CURVE('',#37186,#37187,#20227,.T.);
#46267=EDGE_CURVE('',#37187,#37188,#30673,.T.);
#46268=EDGE_CURVE('',#37188,#37189,#20228,.T.);
#46269=EDGE_CURVE('',#37189,#37190,#4372,.T.);
#46270=EDGE_CURVE('',#37190,#37191,#30674,.T.);
#46271=EDGE_CURVE('',#37191,#37192,#4373,.T.);
#46272=EDGE_CURVE('',#37192,#37193,#20229,.T.);
#46273=EDGE_CURVE('',#37193,#37194,#30675,.T.);
#46274=EDGE_CURVE('',#37194,#37195,#20230,.T.);
#46275=EDGE_CURVE('',#37195,#36840,#4374,.T.);
#46276=EDGE_CURVE('',#36821,#37196,#4375,.T.);
#46277=EDGE_CURVE('',#37196,#37197,#20231,.T.);
#46278=EDGE_CURVE('',#37197,#37198,#30676,.T.);
#46279=EDGE_CURVE('',#37198,#37199,#20232,.T.);
#46280=EDGE_CURVE('',#37199,#37200,#4376,.T.);
#46281=EDGE_CURVE('',#37200,#37201,#30677,.T.);
#46282=EDGE_CURVE('',#37201,#37202,#4377,.T.);
#46283=EDGE_CURVE('',#37202,#37203,#20233,.T.);
#46284=EDGE_CURVE('',#37203,#37204,#30678,.T.);
#46285=EDGE_CURVE('',#37204,#37205,#20234,.T.);
#46286=EDGE_CURVE('',#37205,#37206,#4378,.T.);
#46287=EDGE_CURVE('',#37206,#37207,#30679,.T.);
#46288=EDGE_CURVE('',#37207,#37208,#4379,.T.);
#46289=EDGE_CURVE('',#37208,#37209,#20235,.T.);
#46290=EDGE_CURVE('',#37209,#37210,#30680,.T.);
#46291=EDGE_CURVE('',#37210,#37211,#20236,.T.);
#46292=EDGE_CURVE('',#37211,#37212,#4380,.T.);
#46293=EDGE_CURVE('',#37212,#37213,#30681,.T.);
#46294=EDGE_CURVE('',#37213,#37214,#4381,.T.);
#46295=EDGE_CURVE('',#37214,#37215,#20237,.T.);
#46296=EDGE_CURVE('',#37215,#37216,#30682,.T.);
#46297=EDGE_CURVE('',#37216,#37217,#20238,.T.);
#46298=EDGE_CURVE('',#37217,#37218,#4382,.T.);
#46299=EDGE_CURVE('',#37218,#37219,#30683,.T.);
#46300=EDGE_CURVE('',#37219,#37220,#4383,.T.);
#46301=EDGE_CURVE('',#37220,#37221,#20239,.T.);
#46302=EDGE_CURVE('',#37221,#37222,#30684,.T.);
#46303=EDGE_CURVE('',#37222,#37223,#20240,.T.);
#46304=EDGE_CURVE('',#37223,#37224,#4384,.T.);
#46305=EDGE_CURVE('',#37224,#37225,#30685,.T.);
#46306=EDGE_CURVE('',#37225,#37226,#4385,.T.);
#46307=EDGE_CURVE('',#37226,#37227,#20241,.T.);
#46308=EDGE_CURVE('',#37227,#37228,#30686,.T.);
#46309=EDGE_CURVE('',#37228,#37229,#20242,.T.);
#46310=EDGE_CURVE('',#37229,#37230,#4386,.T.);
#46311=EDGE_CURVE('',#37230,#37231,#30687,.T.);
#46312=EDGE_CURVE('',#37231,#37232,#4387,.T.);
#46313=EDGE_CURVE('',#37232,#37233,#20243,.T.);
#46314=EDGE_CURVE('',#37233,#37234,#30688,.T.);
#46315=EDGE_CURVE('',#37234,#37235,#20244,.T.);
#46316=EDGE_CURVE('',#37235,#37236,#4388,.T.);
#46317=EDGE_CURVE('',#37236,#37237,#30689,.T.);
#46318=EDGE_CURVE('',#37237,#37238,#4389,.T.);
#46319=EDGE_CURVE('',#37238,#37239,#20245,.T.);
#46320=EDGE_CURVE('',#37239,#37240,#30690,.T.);
#46321=EDGE_CURVE('',#37240,#37241,#20246,.T.);
#46322=EDGE_CURVE('',#37241,#37242,#4390,.T.);
#46323=EDGE_CURVE('',#37242,#37243,#30691,.T.);
#46324=EDGE_CURVE('',#37243,#37244,#4391,.T.);
#46325=EDGE_CURVE('',#37244,#37245,#20247,.T.);
#46326=EDGE_CURVE('',#37245,#37246,#30692,.T.);
#46327=EDGE_CURVE('',#37246,#37247,#20248,.T.);
#46328=EDGE_CURVE('',#37247,#37248,#4392,.T.);
#46329=EDGE_CURVE('',#37248,#37249,#30693,.T.);
#46330=EDGE_CURVE('',#37249,#37250,#4393,.T.);
#46331=EDGE_CURVE('',#37250,#37251,#20249,.T.);
#46332=EDGE_CURVE('',#37251,#37252,#30694,.T.);
#46333=EDGE_CURVE('',#37252,#37253,#20250,.T.);
#46334=EDGE_CURVE('',#37253,#37254,#4394,.T.);
#46335=EDGE_CURVE('',#37254,#37255,#30695,.T.);
#46336=EDGE_CURVE('',#37255,#37256,#4395,.T.);
#46337=EDGE_CURVE('',#37256,#37257,#20251,.T.);
#46338=EDGE_CURVE('',#37257,#37258,#30696,.T.);
#46339=EDGE_CURVE('',#37258,#37259,#20252,.T.);
#46340=EDGE_CURVE('',#37259,#37260,#4396,.T.);
#46341=EDGE_CURVE('',#37260,#37261,#30697,.T.);
#46342=EDGE_CURVE('',#37261,#37262,#4397,.T.);
#46343=EDGE_CURVE('',#37262,#37263,#20253,.T.);
#46344=EDGE_CURVE('',#37263,#37264,#30698,.T.);
#46345=EDGE_CURVE('',#37264,#37265,#20254,.T.);
#46346=EDGE_CURVE('',#37265,#37266,#4398,.T.);
#46347=EDGE_CURVE('',#37266,#37267,#30699,.T.);
#46348=EDGE_CURVE('',#37267,#37268,#4399,.T.);
#46349=EDGE_CURVE('',#37268,#37269,#20255,.T.);
#46350=EDGE_CURVE('',#37269,#37270,#30700,.T.);
#46351=EDGE_CURVE('',#37270,#37271,#20256,.T.);
#46352=EDGE_CURVE('',#37271,#37272,#4400,.T.);
#46353=EDGE_CURVE('',#37272,#37273,#30701,.T.);
#46354=EDGE_CURVE('',#37273,#37274,#4401,.T.);
#46355=EDGE_CURVE('',#37274,#37275,#20257,.T.);
#46356=EDGE_CURVE('',#37275,#37276,#30702,.T.);
#46357=EDGE_CURVE('',#37276,#37277,#20258,.T.);
#46358=EDGE_CURVE('',#37277,#37278,#4402,.T.);
#46359=EDGE_CURVE('',#37278,#37279,#30703,.T.);
#46360=EDGE_CURVE('',#37279,#37280,#4403,.T.);
#46361=EDGE_CURVE('',#37280,#37281,#20259,.T.);
#46362=EDGE_CURVE('',#37281,#37282,#30704,.T.);
#46363=EDGE_CURVE('',#37282,#37283,#20260,.T.);
#46364=EDGE_CURVE('',#37283,#37284,#4404,.T.);
#46365=EDGE_CURVE('',#37284,#37285,#30705,.T.);
#46366=EDGE_CURVE('',#37285,#37286,#4405,.T.);
#46367=EDGE_CURVE('',#37286,#37287,#20261,.T.);
#46368=EDGE_CURVE('',#37287,#37288,#30706,.T.);
#46369=EDGE_CURVE('',#37288,#37289,#20262,.T.);
#46370=EDGE_CURVE('',#37289,#37290,#4406,.T.);
#46371=EDGE_CURVE('',#37290,#37291,#30707,.T.);
#46372=EDGE_CURVE('',#37291,#37292,#4407,.T.);
#46373=EDGE_CURVE('',#37292,#37293,#20263,.T.);
#46374=EDGE_CURVE('',#37293,#37294,#30708,.T.);
#46375=EDGE_CURVE('',#37294,#37295,#20264,.T.);
#46376=EDGE_CURVE('',#37295,#37296,#4408,.T.);
#46377=EDGE_CURVE('',#37296,#37297,#30709,.T.);
#46378=EDGE_CURVE('',#37297,#37298,#4409,.T.);
#46379=EDGE_CURVE('',#37298,#37299,#20265,.T.);
#46380=EDGE_CURVE('',#37299,#37300,#30710,.T.);
#46381=EDGE_CURVE('',#37300,#37301,#20266,.T.);
#46382=EDGE_CURVE('',#37301,#37302,#4410,.T.);
#46383=EDGE_CURVE('',#37302,#37303,#30711,.T.);
#46384=EDGE_CURVE('',#37303,#37304,#4411,.T.);
#46385=EDGE_CURVE('',#37304,#37305,#20267,.T.);
#46386=EDGE_CURVE('',#37305,#37306,#30712,.T.);
#46387=EDGE_CURVE('',#37306,#37307,#20268,.T.);
#46388=EDGE_CURVE('',#37307,#37308,#4412,.T.);
#46389=EDGE_CURVE('',#37308,#37309,#30713,.T.);
#46390=EDGE_CURVE('',#37309,#37310,#4413,.T.);
#46391=EDGE_CURVE('',#37310,#37311,#20269,.T.);
#46392=EDGE_CURVE('',#37311,#37312,#30714,.T.);
#46393=EDGE_CURVE('',#37312,#37313,#20270,.T.);
#46394=EDGE_CURVE('',#37313,#37314,#4414,.T.);
#46395=EDGE_CURVE('',#37314,#37315,#30715,.T.);
#46396=EDGE_CURVE('',#37315,#37316,#4415,.T.);
#46397=EDGE_CURVE('',#37316,#37317,#20271,.T.);
#46398=EDGE_CURVE('',#37317,#37318,#30716,.T.);
#46399=EDGE_CURVE('',#37318,#37319,#20272,.T.);
#46400=EDGE_CURVE('',#37319,#37320,#4416,.T.);
#46401=EDGE_CURVE('',#37320,#37321,#30717,.T.);
#46402=EDGE_CURVE('',#37321,#37322,#4417,.T.);
#46403=EDGE_CURVE('',#37322,#37323,#20273,.T.);
#46404=EDGE_CURVE('',#37323,#37324,#30718,.T.);
#46405=EDGE_CURVE('',#37324,#37325,#20274,.T.);
#46406=EDGE_CURVE('',#37325,#37326,#4418,.T.);
#46407=EDGE_CURVE('',#37326,#37327,#30719,.T.);
#46408=EDGE_CURVE('',#37327,#37328,#4419,.T.);
#46409=EDGE_CURVE('',#37328,#37329,#20275,.T.);
#46410=EDGE_CURVE('',#37329,#37330,#30720,.T.);
#46411=EDGE_CURVE('',#37330,#37331,#20276,.T.);
#46412=EDGE_CURVE('',#37331,#37332,#4420,.T.);
#46413=EDGE_CURVE('',#37332,#37333,#30721,.T.);
#46414=EDGE_CURVE('',#37333,#37334,#4421,.T.);
#46415=EDGE_CURVE('',#37334,#37335,#20277,.T.);
#46416=EDGE_CURVE('',#37335,#37336,#30722,.T.);
#46417=EDGE_CURVE('',#37336,#37337,#20278,.T.);
#46418=EDGE_CURVE('',#37337,#37338,#4422,.T.);
#46419=EDGE_CURVE('',#37338,#37339,#30723,.T.);
#46420=EDGE_CURVE('',#37339,#37340,#4423,.T.);
#46421=EDGE_CURVE('',#37340,#37341,#20279,.T.);
#46422=EDGE_CURVE('',#37341,#37342,#30724,.T.);
#46423=EDGE_CURVE('',#37342,#37343,#20280,.T.);
#46424=EDGE_CURVE('',#37343,#37344,#4424,.T.);
#46425=EDGE_CURVE('',#37344,#37345,#30725,.T.);
#46426=EDGE_CURVE('',#37345,#37346,#4425,.T.);
#46427=EDGE_CURVE('',#37346,#37347,#20281,.T.);
#46428=EDGE_CURVE('',#37347,#37348,#30726,.T.);
#46429=EDGE_CURVE('',#37348,#37349,#20282,.T.);
#46430=EDGE_CURVE('',#37349,#37350,#4426,.T.);
#46431=EDGE_CURVE('',#37350,#37351,#30727,.T.);
#46432=EDGE_CURVE('',#37351,#37352,#4427,.T.);
#46433=EDGE_CURVE('',#37352,#37353,#20283,.T.);
#46434=EDGE_CURVE('',#37353,#37354,#30728,.T.);
#46435=EDGE_CURVE('',#37354,#37355,#20284,.T.);
#46436=EDGE_CURVE('',#37355,#37356,#4428,.T.);
#46437=EDGE_CURVE('',#37356,#37357,#30729,.T.);
#46438=EDGE_CURVE('',#37357,#37358,#4429,.T.);
#46439=EDGE_CURVE('',#37358,#37359,#20285,.T.);
#46440=EDGE_CURVE('',#37359,#37360,#30730,.T.);
#46441=EDGE_CURVE('',#37360,#37361,#20286,.T.);
#46442=EDGE_CURVE('',#37361,#37362,#4430,.T.);
#46443=EDGE_CURVE('',#37362,#37363,#30731,.T.);
#46444=EDGE_CURVE('',#37363,#37364,#4431,.T.);
#46445=EDGE_CURVE('',#37364,#37365,#20287,.T.);
#46446=EDGE_CURVE('',#37365,#37366,#30732,.T.);
#46447=EDGE_CURVE('',#37366,#37367,#20288,.T.);
#46448=EDGE_CURVE('',#37367,#37368,#4432,.T.);
#46449=EDGE_CURVE('',#37368,#37369,#30733,.T.);
#46450=EDGE_CURVE('',#37369,#37370,#4433,.T.);
#46451=EDGE_CURVE('',#37370,#37371,#20289,.T.);
#46452=EDGE_CURVE('',#37371,#37372,#30734,.T.);
#46453=EDGE_CURVE('',#37372,#37373,#20290,.T.);
#46454=EDGE_CURVE('',#37373,#37374,#4434,.T.);
#46455=EDGE_CURVE('',#37374,#37375,#30735,.T.);
#46456=EDGE_CURVE('',#37375,#36831,#20291,.T.);
#46457=EDGE_CURVE('',#37375,#37376,#30736,.T.);
#46458=EDGE_CURVE('',#37376,#37377,#4435,.T.);
#46459=EDGE_CURVE('',#37377,#37378,#20292,.T.);
#46460=EDGE_CURVE('',#37378,#37379,#30737,.T.);
#46461=EDGE_CURVE('',#37379,#37380,#20293,.T.);
#46462=EDGE_CURVE('',#37380,#37381,#4436,.T.);
#46463=EDGE_CURVE('',#37381,#37382,#30738,.T.);
#46464=EDGE_CURVE('',#37382,#37383,#4437,.T.);
#46465=EDGE_CURVE('',#37383,#37384,#20294,.T.);
#46466=EDGE_CURVE('',#37384,#37385,#30739,.T.);
#46467=EDGE_CURVE('',#37385,#37386,#20295,.T.);
#46468=EDGE_CURVE('',#37386,#37387,#4438,.T.);
#46469=EDGE_CURVE('',#37387,#37388,#30740,.T.);
#46470=EDGE_CURVE('',#37388,#37389,#4439,.T.);
#46471=EDGE_CURVE('',#37389,#37390,#20296,.T.);
#46472=EDGE_CURVE('',#37390,#37391,#30741,.T.);
#46473=EDGE_CURVE('',#37391,#37392,#20297,.T.);
#46474=EDGE_CURVE('',#37392,#37393,#4440,.T.);
#46475=EDGE_CURVE('',#37393,#37394,#30742,.T.);
#46476=EDGE_CURVE('',#37394,#37395,#4441,.T.);
#46477=EDGE_CURVE('',#37395,#37396,#20298,.T.);
#46478=EDGE_CURVE('',#37396,#37397,#30743,.T.);
#46479=EDGE_CURVE('',#37397,#37398,#20299,.T.);
#46480=EDGE_CURVE('',#37398,#37399,#4442,.T.);
#46481=EDGE_CURVE('',#37399,#37400,#30744,.T.);
#46482=EDGE_CURVE('',#37400,#37401,#4443,.T.);
#46483=EDGE_CURVE('',#37401,#37402,#20300,.T.);
#46484=EDGE_CURVE('',#37402,#37403,#30745,.T.);
#46485=EDGE_CURVE('',#37403,#37404,#20301,.T.);
#46486=EDGE_CURVE('',#37404,#37405,#4444,.T.);
#46487=EDGE_CURVE('',#37405,#37406,#30746,.T.);
#46488=EDGE_CURVE('',#37406,#37407,#4445,.T.);
#46489=EDGE_CURVE('',#37407,#37408,#20302,.T.);
#46490=EDGE_CURVE('',#37408,#37409,#30747,.T.);
#46491=EDGE_CURVE('',#37409,#37410,#20303,.T.);
#46492=EDGE_CURVE('',#37410,#37411,#4446,.T.);
#46493=EDGE_CURVE('',#37411,#37412,#30748,.T.);
#46494=EDGE_CURVE('',#37412,#37413,#4447,.T.);
#46495=EDGE_CURVE('',#37413,#37414,#20304,.T.);
#46496=EDGE_CURVE('',#37414,#37415,#30749,.T.);
#46497=EDGE_CURVE('',#37415,#37416,#20305,.T.);
#46498=EDGE_CURVE('',#37416,#37417,#4448,.T.);
#46499=EDGE_CURVE('',#37417,#37418,#30750,.T.);
#46500=EDGE_CURVE('',#37418,#37419,#4449,.T.);
#46501=EDGE_CURVE('',#37419,#37420,#20306,.T.);
#46502=EDGE_CURVE('',#37420,#37421,#30751,.T.);
#46503=EDGE_CURVE('',#37421,#37422,#20307,.T.);
#46504=EDGE_CURVE('',#37422,#37423,#4450,.T.);
#46505=EDGE_CURVE('',#37423,#37424,#30752,.T.);
#46506=EDGE_CURVE('',#37424,#37425,#4451,.T.);
#46507=EDGE_CURVE('',#37425,#37426,#20308,.T.);
#46508=EDGE_CURVE('',#37426,#37427,#30753,.T.);
#46509=EDGE_CURVE('',#37427,#37428,#20309,.T.);
#46510=EDGE_CURVE('',#37428,#37429,#4452,.T.);
#46511=EDGE_CURVE('',#37429,#37430,#30754,.T.);
#46512=EDGE_CURVE('',#37430,#37431,#4453,.T.);
#46513=EDGE_CURVE('',#37431,#37432,#20310,.T.);
#46514=EDGE_CURVE('',#37432,#37433,#30755,.T.);
#46515=EDGE_CURVE('',#37433,#37434,#20311,.T.);
#46516=EDGE_CURVE('',#37434,#37435,#4454,.T.);
#46517=EDGE_CURVE('',#37435,#37436,#30756,.T.);
#46518=EDGE_CURVE('',#37436,#37437,#4455,.T.);
#46519=EDGE_CURVE('',#37437,#37438,#20312,.T.);
#46520=EDGE_CURVE('',#37438,#37439,#30757,.T.);
#46521=EDGE_CURVE('',#37439,#37440,#20313,.T.);
#46522=EDGE_CURVE('',#37440,#37441,#4456,.T.);
#46523=EDGE_CURVE('',#37441,#37442,#30758,.T.);
#46524=EDGE_CURVE('',#37442,#37443,#4457,.T.);
#46525=EDGE_CURVE('',#37443,#37444,#20314,.T.);
#46526=EDGE_CURVE('',#37444,#37445,#30759,.T.);
#46527=EDGE_CURVE('',#37445,#37446,#20315,.T.);
#46528=EDGE_CURVE('',#37446,#37447,#4458,.T.);
#46529=EDGE_CURVE('',#37447,#37448,#30760,.T.);
#46530=EDGE_CURVE('',#37448,#37449,#4459,.T.);
#46531=EDGE_CURVE('',#37449,#37450,#20316,.T.);
#46532=EDGE_CURVE('',#37450,#37451,#30761,.T.);
#46533=EDGE_CURVE('',#37451,#37452,#20317,.T.);
#46534=EDGE_CURVE('',#37452,#37453,#4460,.T.);
#46535=EDGE_CURVE('',#37453,#37454,#30762,.T.);
#46536=EDGE_CURVE('',#37454,#37455,#4461,.T.);
#46537=EDGE_CURVE('',#37455,#37456,#20318,.T.);
#46538=EDGE_CURVE('',#37456,#37457,#30763,.T.);
#46539=EDGE_CURVE('',#37457,#37458,#20319,.T.);
#46540=EDGE_CURVE('',#37458,#37459,#4462,.T.);
#46541=EDGE_CURVE('',#37459,#37460,#30764,.T.);
#46542=EDGE_CURVE('',#37460,#37461,#4463,.T.);
#46543=EDGE_CURVE('',#37461,#37462,#20320,.T.);
#46544=EDGE_CURVE('',#37462,#37463,#30765,.T.);
#46545=EDGE_CURVE('',#37463,#37464,#20321,.T.);
#46546=EDGE_CURVE('',#37464,#36814,#4464,.T.);
#46547=EDGE_CURVE('',#36813,#37465,#4465,.T.);
#46548=EDGE_CURVE('',#37465,#37466,#20322,.T.);
#46549=EDGE_CURVE('',#37466,#37467,#30766,.T.);
#46550=EDGE_CURVE('',#37467,#37468,#20323,.T.);
#46551=EDGE_CURVE('',#37468,#37469,#4466,.T.);
#46552=EDGE_CURVE('',#37469,#37470,#30767,.T.);
#46553=EDGE_CURVE('',#37470,#37471,#4467,.T.);
#46554=EDGE_CURVE('',#37471,#37472,#20324,.T.);
#46555=EDGE_CURVE('',#37472,#37473,#30768,.T.);
#46556=EDGE_CURVE('',#37473,#37474,#20325,.T.);
#46557=EDGE_CURVE('',#37474,#37475,#4468,.T.);
#46558=EDGE_CURVE('',#37475,#37476,#30769,.T.);
#46559=EDGE_CURVE('',#37476,#37477,#4469,.T.);
#46560=EDGE_CURVE('',#37477,#37478,#20326,.T.);
#46561=EDGE_CURVE('',#37478,#37479,#30770,.T.);
#46562=EDGE_CURVE('',#37479,#37480,#20327,.T.);
#46563=EDGE_CURVE('',#37480,#37481,#4470,.T.);
#46564=EDGE_CURVE('',#37481,#37482,#30771,.T.);
#46565=EDGE_CURVE('',#37482,#37483,#4471,.T.);
#46566=EDGE_CURVE('',#37483,#37484,#20328,.T.);
#46567=EDGE_CURVE('',#37484,#37485,#30772,.T.);
#46568=EDGE_CURVE('',#37485,#37486,#20329,.T.);
#46569=EDGE_CURVE('',#37486,#37487,#4472,.T.);
#46570=EDGE_CURVE('',#37487,#37488,#30773,.T.);
#46571=EDGE_CURVE('',#37488,#37489,#4473,.T.);
#46572=EDGE_CURVE('',#37489,#37490,#20330,.T.);
#46573=EDGE_CURVE('',#37490,#37491,#30774,.T.);
#46574=EDGE_CURVE('',#37491,#37492,#20331,.T.);
#46575=EDGE_CURVE('',#37492,#37493,#4474,.T.);
#46576=EDGE_CURVE('',#37493,#37494,#30775,.T.);
#46577=EDGE_CURVE('',#37494,#37495,#4475,.T.);
#46578=EDGE_CURVE('',#37495,#37496,#20332,.T.);
#46579=EDGE_CURVE('',#37496,#37497,#30776,.T.);
#46580=EDGE_CURVE('',#37497,#37498,#20333,.T.);
#46581=EDGE_CURVE('',#37498,#37499,#4476,.T.);
#46582=EDGE_CURVE('',#37499,#37500,#30777,.T.);
#46583=EDGE_CURVE('',#37500,#37501,#4477,.T.);
#46584=EDGE_CURVE('',#37501,#37502,#20334,.T.);
#46585=EDGE_CURVE('',#37502,#37503,#30778,.T.);
#46586=EDGE_CURVE('',#37503,#37504,#20335,.T.);
#46587=EDGE_CURVE('',#37504,#37505,#4478,.T.);
#46588=EDGE_CURVE('',#37505,#37506,#30779,.T.);
#46589=EDGE_CURVE('',#37506,#37507,#4479,.T.);
#46590=EDGE_CURVE('',#37507,#37508,#20336,.T.);
#46591=EDGE_CURVE('',#37508,#37509,#30780,.T.);
#46592=EDGE_CURVE('',#37509,#37510,#20337,.T.);
#46593=EDGE_CURVE('',#37510,#37511,#4480,.T.);
#46594=EDGE_CURVE('',#37511,#37512,#30781,.T.);
#46595=EDGE_CURVE('',#37512,#37513,#4481,.T.);
#46596=EDGE_CURVE('',#37513,#37514,#20338,.T.);
#46597=EDGE_CURVE('',#37514,#37515,#30782,.T.);
#46598=EDGE_CURVE('',#37515,#37516,#20339,.T.);
#46599=EDGE_CURVE('',#37516,#37517,#4482,.T.);
#46600=EDGE_CURVE('',#37517,#37518,#30783,.T.);
#46601=EDGE_CURVE('',#37518,#37519,#4483,.T.);
#46602=EDGE_CURVE('',#37519,#37520,#20340,.T.);
#46603=EDGE_CURVE('',#37520,#37521,#30784,.T.);
#46604=EDGE_CURVE('',#37521,#37522,#20341,.T.);
#46605=EDGE_CURVE('',#37522,#37523,#4484,.T.);
#46606=EDGE_CURVE('',#37523,#37524,#30785,.T.);
#46607=EDGE_CURVE('',#37524,#37525,#4485,.T.);
#46608=EDGE_CURVE('',#37525,#37526,#20342,.T.);
#46609=EDGE_CURVE('',#37526,#37527,#30786,.T.);
#46610=EDGE_CURVE('',#37527,#37528,#20343,.T.);
#46611=EDGE_CURVE('',#37528,#37529,#4486,.T.);
#46612=EDGE_CURVE('',#37529,#37530,#30787,.T.);
#46613=EDGE_CURVE('',#37530,#37531,#4487,.T.);
#46614=EDGE_CURVE('',#37531,#37532,#20344,.T.);
#46615=EDGE_CURVE('',#37532,#37533,#30788,.T.);
#46616=EDGE_CURVE('',#37533,#37534,#20345,.T.);
#46617=EDGE_CURVE('',#37534,#37535,#4488,.T.);
#46618=EDGE_CURVE('',#37535,#37536,#30789,.T.);
#46619=EDGE_CURVE('',#37536,#37537,#4489,.T.);
#46620=EDGE_CURVE('',#37537,#37538,#20346,.T.);
#46621=EDGE_CURVE('',#37538,#37539,#30790,.T.);
#46622=EDGE_CURVE('',#37539,#37540,#20347,.T.);
#46623=EDGE_CURVE('',#37540,#37541,#4490,.T.);
#46624=EDGE_CURVE('',#37541,#37542,#30791,.T.);
#46625=EDGE_CURVE('',#37542,#37543,#4491,.T.);
#46626=EDGE_CURVE('',#37543,#37544,#20348,.T.);
#46627=EDGE_CURVE('',#37544,#37545,#30792,.T.);
#46628=EDGE_CURVE('',#37545,#37546,#20349,.T.);
#46629=EDGE_CURVE('',#37546,#37547,#4492,.T.);
#46630=EDGE_CURVE('',#37547,#37548,#30793,.T.);
#46631=EDGE_CURVE('',#37548,#37549,#4493,.T.);
#46632=EDGE_CURVE('',#37549,#37550,#20350,.T.);
#46633=EDGE_CURVE('',#37550,#37551,#30794,.T.);
#46634=EDGE_CURVE('',#37551,#37552,#20351,.T.);
#46635=EDGE_CURVE('',#37552,#36822,#4494,.T.);
#46636=EDGE_CURVE('',#37553,#37554,#30795,.T.);
#46637=EDGE_CURVE('',#37554,#36830,#20352,.T.);
#46638=EDGE_CURVE('',#37554,#37553,#30796,.T.);
#46639=EDGE_CURVE('',#37553,#37555,#20353,.T.);
#46640=EDGE_CURVE('',#37555,#37555,#30797,.T.);
#46641=EDGE_CURVE('',#37556,#37557,#30798,.T.);
#46642=EDGE_CURVE('',#37556,#37558,#20354,.T.);
#46643=EDGE_CURVE('',#37558,#37559,#30799,.T.);
#46644=EDGE_CURVE('',#37559,#37560,#20355,.T.);
#46645=EDGE_CURVE('',#37561,#37560,#30800,.T.);
#46646=EDGE_CURVE('',#37557,#37561,#30801,.T.);
#46647=EDGE_CURVE('',#37562,#37563,#30802,.T.);
#46648=EDGE_CURVE('',#37563,#37557,#20356,.T.);
#46649=EDGE_CURVE('',#37561,#37562,#20357,.T.);
#46650=EDGE_CURVE('',#37564,#37565,#30803,.T.);
#46651=EDGE_CURVE('',#37565,#37566,#20358,.T.);
#46652=EDGE_CURVE('',#37566,#37567,#30804,.T.);
#46653=EDGE_CURVE('',#37567,#37564,#20359,.T.);
#46654=EDGE_CURVE('',#37568,#37569,#30805,.T.);
#46655=EDGE_CURVE('',#37568,#37570,#20360,.T.);
#46656=EDGE_CURVE('',#37570,#37571,#30806,.T.);
#46657=EDGE_CURVE('',#37571,#37572,#20361,.T.);
#46658=EDGE_CURVE('',#37573,#37572,#30807,.T.);
#46659=EDGE_CURVE('',#37569,#37573,#30808,.T.);
#46660=EDGE_CURVE('',#37574,#37575,#30809,.T.);
#46661=EDGE_CURVE('',#37575,#37569,#20362,.T.);
#46662=EDGE_CURVE('',#37573,#37574,#20363,.T.);
#46663=EDGE_CURVE('',#37558,#37379,#30810,.T.);
#46664=EDGE_CURVE('',#37378,#37559,#30811,.T.);
#46665=EDGE_CURVE('',#37193,#37575,#338,.T.);
#46666=EDGE_CURVE('',#37574,#37194,#339,.T.);
#46667=EDGE_CURVE('',#37570,#37565,#340,.T.);
#46668=EDGE_CURVE('',#37564,#37571,#341,.T.);
#46669=EDGE_CURVE('',#37566,#37563,#342,.T.);
#46670=EDGE_CURVE('',#37562,#37567,#343,.T.);
#46671=EDGE_CURVE('',#37576,#37577,#30812,.T.);
#46672=EDGE_CURVE('',#37577,#37578,#20364,.T.);
#46673=EDGE_CURVE('',#37579,#37578,#30813,.T.);
#46674=EDGE_CURVE('',#37580,#37579,#30814,.T.);
#46675=EDGE_CURVE('',#37581,#37580,#30815,.T.);
#46676=EDGE_CURVE('',#37581,#37576,#20365,.T.);
#46677=EDGE_CURVE('',#37579,#37582,#20366,.T.);
#46678=EDGE_CURVE('',#37582,#37583,#30816,.T.);
#46679=EDGE_CURVE('',#37583,#37580,#20367,.T.);
#46680=EDGE_CURVE('',#37584,#37585,#30817,.T.);
#46681=EDGE_CURVE('',#37585,#37586,#20368,.T.);
#46682=EDGE_CURVE('',#37586,#37587,#30818,.T.);
#46683=EDGE_CURVE('',#37587,#37584,#20369,.T.);
#46684=EDGE_CURVE('',#37588,#37589,#30819,.T.);
#46685=EDGE_CURVE('',#37589,#37590,#20370,.T.);
#46686=EDGE_CURVE('',#37591,#37590,#30820,.T.);
#46687=EDGE_CURVE('',#37592,#37591,#30821,.T.);
#46688=EDGE_CURVE('',#37593,#37592,#30822,.T.);
#46689=EDGE_CURVE('',#37593,#37588,#20371,.T.);
#46690=EDGE_CURVE('',#37591,#37594,#20372,.T.);
#46691=EDGE_CURVE('',#37594,#37595,#30823,.T.);
#46692=EDGE_CURVE('',#37595,#37592,#20373,.T.);
#46693=EDGE_CURVE('',#37384,#37577,#30824,.T.);
#46694=EDGE_CURVE('',#37576,#37385,#30825,.T.);
#46695=EDGE_CURVE('',#37594,#37188,#344,.T.);
#46696=EDGE_CURVE('',#37187,#37595,#345,.T.);
#46697=EDGE_CURVE('',#37586,#37589,#346,.T.);
#46698=EDGE_CURVE('',#37588,#37587,#347,.T.);
#46699=EDGE_CURVE('',#37582,#37585,#348,.T.);
#46700=EDGE_CURVE('',#37584,#37583,#349,.T.);
#46701=EDGE_CURVE('',#37596,#37597,#30826,.T.);
#46702=EDGE_CURVE('',#37597,#37598,#20374,.T.);
#46703=EDGE_CURVE('',#37599,#37598,#30827,.T.);
#46704=EDGE_CURVE('',#37600,#37599,#30828,.T.);
#46705=EDGE_CURVE('',#37601,#37600,#30829,.T.);
#46706=EDGE_CURVE('',#37601,#37596,#20375,.T.);
#46707=EDGE_CURVE('',#37599,#37602,#20376,.T.);
#46708=EDGE_CURVE('',#37602,#37603,#30830,.T.);
#46709=EDGE_CURVE('',#37603,#37600,#20377,.T.);
#46710=EDGE_CURVE('',#37604,#37605,#30831,.T.);
#46711=EDGE_CURVE('',#37605,#37606,#20378,.T.);
#46712=EDGE_CURVE('',#37606,#37607,#30832,.T.);
#46713=EDGE_CURVE('',#37607,#37604,#20379,.T.);
#46714=EDGE_CURVE('',#37608,#37609,#30833,.T.);
#46715=EDGE_CURVE('',#37609,#37610,#20380,.T.);
#46716=EDGE_CURVE('',#37611,#37610,#30834,.T.);
#46717=EDGE_CURVE('',#37612,#37611,#30835,.T.);
#46718=EDGE_CURVE('',#37613,#37612,#30836,.T.);
#46719=EDGE_CURVE('',#37613,#37608,#20381,.T.);
#46720=EDGE_CURVE('',#37611,#37614,#20382,.T.);
#46721=EDGE_CURVE('',#37614,#37615,#30837,.T.);
#46722=EDGE_CURVE('',#37615,#37612,#20383,.T.);
#46723=EDGE_CURVE('',#37390,#37597,#30838,.T.);
#46724=EDGE_CURVE('',#37596,#37391,#30839,.T.);
#46725=EDGE_CURVE('',#37614,#37182,#350,.T.);
#46726=EDGE_CURVE('',#37181,#37615,#351,.T.);
#46727=EDGE_CURVE('',#37606,#37609,#352,.T.);
#46728=EDGE_CURVE('',#37608,#37607,#353,.T.);
#46729=EDGE_CURVE('',#37602,#37605,#354,.T.);
#46730=EDGE_CURVE('',#37604,#37603,#355,.T.);
#46731=EDGE_CURVE('',#37616,#37617,#30840,.T.);
#46732=EDGE_CURVE('',#37617,#37618,#20384,.T.);
#46733=EDGE_CURVE('',#37619,#37618,#30841,.T.);
#46734=EDGE_CURVE('',#37620,#37619,#30842,.T.);
#46735=EDGE_CURVE('',#37621,#37620,#30843,.T.);
#46736=EDGE_CURVE('',#37621,#37616,#20385,.T.);
#46737=EDGE_CURVE('',#37619,#37622,#20386,.T.);
#46738=EDGE_CURVE('',#37622,#37623,#30844,.T.);
#46739=EDGE_CURVE('',#37623,#37620,#20387,.T.);
#46740=EDGE_CURVE('',#37624,#37625,#30845,.T.);
#46741=EDGE_CURVE('',#37625,#37626,#20388,.T.);
#46742=EDGE_CURVE('',#37626,#37627,#30846,.T.);
#46743=EDGE_CURVE('',#37627,#37624,#20389,.T.);
#46744=EDGE_CURVE('',#37628,#37629,#30847,.T.);
#46745=EDGE_CURVE('',#37629,#37630,#20390,.T.);
#46746=EDGE_CURVE('',#37631,#37630,#30848,.T.);
#46747=EDGE_CURVE('',#37632,#37631,#30849,.T.);
#46748=EDGE_CURVE('',#37633,#37632,#30850,.T.);
#46749=EDGE_CURVE('',#37633,#37628,#20391,.T.);
#46750=EDGE_CURVE('',#37631,#37634,#20392,.T.);
#46751=EDGE_CURVE('',#37634,#37635,#30851,.T.);
#46752=EDGE_CURVE('',#37635,#37632,#20393,.T.);
#46753=EDGE_CURVE('',#37396,#37617,#30852,.T.);
#46754=EDGE_CURVE('',#37616,#37397,#30853,.T.);
#46755=EDGE_CURVE('',#37634,#37176,#356,.T.);
#46756=EDGE_CURVE('',#37175,#37635,#357,.T.);
#46757=EDGE_CURVE('',#37626,#37629,#358,.T.);
#46758=EDGE_CURVE('',#37628,#37627,#359,.T.);
#46759=EDGE_CURVE('',#37622,#37625,#360,.T.);
#46760=EDGE_CURVE('',#37624,#37623,#361,.T.);
#46761=EDGE_CURVE('',#37636,#37637,#30854,.T.);
#46762=EDGE_CURVE('',#37637,#37638,#20394,.T.);
#46763=EDGE_CURVE('',#37639,#37638,#30855,.T.);
#46764=EDGE_CURVE('',#37640,#37639,#30856,.T.);
#46765=EDGE_CURVE('',#37641,#37640,#30857,.T.);
#46766=EDGE_CURVE('',#37641,#37636,#20395,.T.);
#46767=EDGE_CURVE('',#37639,#37642,#20396,.T.);
#46768=EDGE_CURVE('',#37642,#37643,#30858,.T.);
#46769=EDGE_CURVE('',#37643,#37640,#20397,.T.);
#46770=EDGE_CURVE('',#37644,#37645,#30859,.T.);
#46771=EDGE_CURVE('',#37645,#37646,#20398,.T.);
#46772=EDGE_CURVE('',#37646,#37647,#30860,.T.);
#46773=EDGE_CURVE('',#37647,#37644,#20399,.T.);
#46774=EDGE_CURVE('',#37648,#37649,#30861,.T.);
#46775=EDGE_CURVE('',#37649,#37650,#20400,.T.);
#46776=EDGE_CURVE('',#37651,#37650,#30862,.T.);
#46777=EDGE_CURVE('',#37652,#37651,#30863,.T.);
#46778=EDGE_CURVE('',#37653,#37652,#30864,.T.);
#46779=EDGE_CURVE('',#37653,#37648,#20401,.T.);
#46780=EDGE_CURVE('',#37651,#37654,#20402,.T.);
#46781=EDGE_CURVE('',#37654,#37655,#30865,.T.);
#46782=EDGE_CURVE('',#37655,#37652,#20403,.T.);
#46783=EDGE_CURVE('',#37402,#37637,#30866,.T.);
#46784=EDGE_CURVE('',#37636,#37403,#30867,.T.);
#46785=EDGE_CURVE('',#37654,#37170,#362,.T.);
#46786=EDGE_CURVE('',#37169,#37655,#363,.T.);
#46787=EDGE_CURVE('',#37646,#37649,#364,.T.);
#46788=EDGE_CURVE('',#37648,#37647,#365,.T.);
#46789=EDGE_CURVE('',#37642,#37645,#366,.T.);
#46790=EDGE_CURVE('',#37644,#37643,#367,.T.);
#46791=EDGE_CURVE('',#37656,#37657,#30868,.T.);
#46792=EDGE_CURVE('',#37657,#37658,#20404,.T.);
#46793=EDGE_CURVE('',#37659,#37658,#30869,.T.);
#46794=EDGE_CURVE('',#37660,#37659,#30870,.T.);
#46795=EDGE_CURVE('',#37661,#37660,#30871,.T.);
#46796=EDGE_CURVE('',#37661,#37656,#20405,.T.);
#46797=EDGE_CURVE('',#37659,#37662,#20406,.T.);
#46798=EDGE_CURVE('',#37662,#37663,#30872,.T.);
#46799=EDGE_CURVE('',#37663,#37660,#20407,.T.);
#46800=EDGE_CURVE('',#37664,#37665,#30873,.T.);
#46801=EDGE_CURVE('',#37665,#37666,#20408,.T.);
#46802=EDGE_CURVE('',#37666,#37667,#30874,.T.);
#46803=EDGE_CURVE('',#37667,#37664,#20409,.T.);
#46804=EDGE_CURVE('',#37668,#37669,#30875,.T.);
#46805=EDGE_CURVE('',#37669,#37670,#20410,.T.);
#46806=EDGE_CURVE('',#37671,#37670,#30876,.T.);
#46807=EDGE_CURVE('',#37672,#37671,#30877,.T.);
#46808=EDGE_CURVE('',#37673,#37672,#30878,.T.);
#46809=EDGE_CURVE('',#37673,#37668,#20411,.T.);
#46810=EDGE_CURVE('',#37671,#37674,#20412,.T.);
#46811=EDGE_CURVE('',#37674,#37675,#30879,.T.);
#46812=EDGE_CURVE('',#37675,#37672,#20413,.T.);
#46813=EDGE_CURVE('',#37408,#37657,#30880,.T.);
#46814=EDGE_CURVE('',#37656,#37409,#30881,.T.);
#46815=EDGE_CURVE('',#37674,#37164,#368,.T.);
#46816=EDGE_CURVE('',#37163,#37675,#369,.T.);
#46817=EDGE_CURVE('',#37666,#37669,#370,.T.);
#46818=EDGE_CURVE('',#37668,#37667,#371,.T.);
#46819=EDGE_CURVE('',#37662,#37665,#372,.T.);
#46820=EDGE_CURVE('',#37664,#37663,#373,.T.);
#46821=EDGE_CURVE('',#37676,#37677,#30882,.T.);
#46822=EDGE_CURVE('',#37677,#37678,#20414,.T.);
#46823=EDGE_CURVE('',#37679,#37678,#30883,.T.);
#46824=EDGE_CURVE('',#37680,#37679,#30884,.T.);
#46825=EDGE_CURVE('',#37681,#37680,#30885,.T.);
#46826=EDGE_CURVE('',#37681,#37676,#20415,.T.);
#46827=EDGE_CURVE('',#37679,#37682,#20416,.T.);
#46828=EDGE_CURVE('',#37682,#37683,#30886,.T.);
#46829=EDGE_CURVE('',#37683,#37680,#20417,.T.);
#46830=EDGE_CURVE('',#37684,#37685,#30887,.T.);
#46831=EDGE_CURVE('',#37685,#37686,#20418,.T.);
#46832=EDGE_CURVE('',#37686,#37687,#30888,.T.);
#46833=EDGE_CURVE('',#37687,#37684,#20419,.T.);
#46834=EDGE_CURVE('',#37688,#37689,#30889,.T.);
#46835=EDGE_CURVE('',#37689,#37690,#20420,.T.);
#46836=EDGE_CURVE('',#37691,#37690,#30890,.T.);
#46837=EDGE_CURVE('',#37692,#37691,#30891,.T.);
#46838=EDGE_CURVE('',#37693,#37692,#30892,.T.);
#46839=EDGE_CURVE('',#37693,#37688,#20421,.T.);
#46840=EDGE_CURVE('',#37691,#37694,#20422,.T.);
#46841=EDGE_CURVE('',#37694,#37695,#30893,.T.);
#46842=EDGE_CURVE('',#37695,#37692,#20423,.T.);
#46843=EDGE_CURVE('',#37414,#37677,#30894,.T.);
#46844=EDGE_CURVE('',#37676,#37415,#30895,.T.);
#46845=EDGE_CURVE('',#37694,#37158,#374,.T.);
#46846=EDGE_CURVE('',#37157,#37695,#375,.T.);
#46847=EDGE_CURVE('',#37686,#37689,#376,.T.);
#46848=EDGE_CURVE('',#37688,#37687,#377,.T.);
#46849=EDGE_CURVE('',#37682,#37685,#378,.T.);
#46850=EDGE_CURVE('',#37684,#37683,#379,.T.);
#46851=EDGE_CURVE('',#37696,#37697,#30896,.T.);
#46852=EDGE_CURVE('',#37697,#37698,#20424,.T.);
#46853=EDGE_CURVE('',#37699,#37698,#30897,.T.);
#46854=EDGE_CURVE('',#37700,#37699,#30898,.T.);
#46855=EDGE_CURVE('',#37701,#37700,#30899,.T.);
#46856=EDGE_CURVE('',#37701,#37696,#20425,.T.);
#46857=EDGE_CURVE('',#37699,#37702,#20426,.T.);
#46858=EDGE_CURVE('',#37702,#37703,#30900,.T.);
#46859=EDGE_CURVE('',#37703,#37700,#20427,.T.);
#46860=EDGE_CURVE('',#37704,#37705,#30901,.T.);
#46861=EDGE_CURVE('',#37705,#37706,#20428,.T.);
#46862=EDGE_CURVE('',#37706,#37707,#30902,.T.);
#46863=EDGE_CURVE('',#37707,#37704,#20429,.T.);
#46864=EDGE_CURVE('',#37708,#37709,#30903,.T.);
#46865=EDGE_CURVE('',#37709,#37710,#20430,.T.);
#46866=EDGE_CURVE('',#37711,#37710,#30904,.T.);
#46867=EDGE_CURVE('',#37712,#37711,#30905,.T.);
#46868=EDGE_CURVE('',#37713,#37712,#30906,.T.);
#46869=EDGE_CURVE('',#37713,#37708,#20431,.T.);
#46870=EDGE_CURVE('',#37711,#37714,#20432,.T.);
#46871=EDGE_CURVE('',#37714,#37715,#30907,.T.);
#46872=EDGE_CURVE('',#37715,#37712,#20433,.T.);
#46873=EDGE_CURVE('',#37420,#37697,#30908,.T.);
#46874=EDGE_CURVE('',#37696,#37421,#30909,.T.);
#46875=EDGE_CURVE('',#37714,#37152,#380,.T.);
#46876=EDGE_CURVE('',#37151,#37715,#381,.T.);
#46877=EDGE_CURVE('',#37706,#37709,#382,.T.);
#46878=EDGE_CURVE('',#37708,#37707,#383,.T.);
#46879=EDGE_CURVE('',#37702,#37705,#384,.T.);
#46880=EDGE_CURVE('',#37704,#37703,#385,.T.);
#46881=EDGE_CURVE('',#37716,#37717,#30910,.T.);
#46882=EDGE_CURVE('',#37717,#37718,#20434,.T.);
#46883=EDGE_CURVE('',#37719,#37718,#30911,.T.);
#46884=EDGE_CURVE('',#37720,#37719,#30912,.T.);
#46885=EDGE_CURVE('',#37721,#37720,#30913,.T.);
#46886=EDGE_CURVE('',#37721,#37716,#20435,.T.);
#46887=EDGE_CURVE('',#37719,#37722,#20436,.T.);
#46888=EDGE_CURVE('',#37722,#37723,#30914,.T.);
#46889=EDGE_CURVE('',#37723,#37720,#20437,.T.);
#46890=EDGE_CURVE('',#37724,#37725,#30915,.T.);
#46891=EDGE_CURVE('',#37725,#37726,#20438,.T.);
#46892=EDGE_CURVE('',#37726,#37727,#30916,.T.);
#46893=EDGE_CURVE('',#37727,#37724,#20439,.T.);
#46894=EDGE_CURVE('',#37728,#37729,#30917,.T.);
#46895=EDGE_CURVE('',#37729,#37730,#20440,.T.);
#46896=EDGE_CURVE('',#37731,#37730,#30918,.T.);
#46897=EDGE_CURVE('',#37732,#37731,#30919,.T.);
#46898=EDGE_CURVE('',#37733,#37732,#30920,.T.);
#46899=EDGE_CURVE('',#37733,#37728,#20441,.T.);
#46900=EDGE_CURVE('',#37731,#37734,#20442,.T.);
#46901=EDGE_CURVE('',#37734,#37735,#30921,.T.);
#46902=EDGE_CURVE('',#37735,#37732,#20443,.T.);
#46903=EDGE_CURVE('',#37426,#37717,#30922,.T.);
#46904=EDGE_CURVE('',#37716,#37427,#30923,.T.);
#46905=EDGE_CURVE('',#37734,#37146,#386,.T.);
#46906=EDGE_CURVE('',#37145,#37735,#387,.T.);
#46907=EDGE_CURVE('',#37726,#37729,#388,.T.);
#46908=EDGE_CURVE('',#37728,#37727,#389,.T.);
#46909=EDGE_CURVE('',#37722,#37725,#390,.T.);
#46910=EDGE_CURVE('',#37724,#37723,#391,.T.);
#46911=EDGE_CURVE('',#37736,#37737,#30924,.T.);
#46912=EDGE_CURVE('',#37737,#37738,#20444,.T.);
#46913=EDGE_CURVE('',#37739,#37738,#30925,.T.);
#46914=EDGE_CURVE('',#37740,#37739,#30926,.T.);
#46915=EDGE_CURVE('',#37741,#37740,#30927,.T.);
#46916=EDGE_CURVE('',#37741,#37736,#20445,.T.);
#46917=EDGE_CURVE('',#37739,#37742,#20446,.T.);
#46918=EDGE_CURVE('',#37742,#37743,#30928,.T.);
#46919=EDGE_CURVE('',#37743,#37740,#20447,.T.);
#46920=EDGE_CURVE('',#37744,#37745,#30929,.T.);
#46921=EDGE_CURVE('',#37745,#37746,#20448,.T.);
#46922=EDGE_CURVE('',#37746,#37747,#30930,.T.);
#46923=EDGE_CURVE('',#37747,#37744,#20449,.T.);
#46924=EDGE_CURVE('',#37748,#37749,#30931,.T.);
#46925=EDGE_CURVE('',#37749,#37750,#20450,.T.);
#46926=EDGE_CURVE('',#37751,#37750,#30932,.T.);
#46927=EDGE_CURVE('',#37752,#37751,#30933,.T.);
#46928=EDGE_CURVE('',#37753,#37752,#30934,.T.);
#46929=EDGE_CURVE('',#37753,#37748,#20451,.T.);
#46930=EDGE_CURVE('',#37751,#37754,#20452,.T.);
#46931=EDGE_CURVE('',#37754,#37755,#30935,.T.);
#46932=EDGE_CURVE('',#37755,#37752,#20453,.T.);
#46933=EDGE_CURVE('',#37432,#37737,#30936,.T.);
#46934=EDGE_CURVE('',#37736,#37433,#30937,.T.);
#46935=EDGE_CURVE('',#37754,#37140,#392,.T.);
#46936=EDGE_CURVE('',#37139,#37755,#393,.T.);
#46937=EDGE_CURVE('',#37746,#37749,#394,.T.);
#46938=EDGE_CURVE('',#37748,#37747,#395,.T.);
#46939=EDGE_CURVE('',#37742,#37745,#396,.T.);
#46940=EDGE_CURVE('',#37744,#37743,#397,.T.);
#46941=EDGE_CURVE('',#37756,#37757,#30938,.T.);
#46942=EDGE_CURVE('',#37757,#37758,#20454,.T.);
#46943=EDGE_CURVE('',#37759,#37758,#30939,.T.);
#46944=EDGE_CURVE('',#37760,#37759,#30940,.T.);
#46945=EDGE_CURVE('',#37761,#37760,#30941,.T.);
#46946=EDGE_CURVE('',#37761,#37756,#20455,.T.);
#46947=EDGE_CURVE('',#37759,#37762,#20456,.T.);
#46948=EDGE_CURVE('',#37762,#37763,#30942,.T.);
#46949=EDGE_CURVE('',#37763,#37760,#20457,.T.);
#46950=EDGE_CURVE('',#37764,#37765,#30943,.T.);
#46951=EDGE_CURVE('',#37765,#37766,#20458,.T.);
#46952=EDGE_CURVE('',#37766,#37767,#30944,.T.);
#46953=EDGE_CURVE('',#37767,#37764,#20459,.T.);
#46954=EDGE_CURVE('',#37768,#37769,#30945,.T.);
#46955=EDGE_CURVE('',#37769,#37770,#20460,.T.);
#46956=EDGE_CURVE('',#37771,#37770,#30946,.T.);
#46957=EDGE_CURVE('',#37772,#37771,#30947,.T.);
#46958=EDGE_CURVE('',#37773,#37772,#30948,.T.);
#46959=EDGE_CURVE('',#37773,#37768,#20461,.T.);
#46960=EDGE_CURVE('',#37771,#37774,#20462,.T.);
#46961=EDGE_CURVE('',#37774,#37775,#30949,.T.);
#46962=EDGE_CURVE('',#37775,#37772,#20463,.T.);
#46963=EDGE_CURVE('',#37438,#37757,#30950,.T.);
#46964=EDGE_CURVE('',#37756,#37439,#30951,.T.);
#46965=EDGE_CURVE('',#37774,#37134,#398,.T.);
#46966=EDGE_CURVE('',#37133,#37775,#399,.T.);
#46967=EDGE_CURVE('',#37766,#37769,#400,.T.);
#46968=EDGE_CURVE('',#37768,#37767,#401,.T.);
#46969=EDGE_CURVE('',#37762,#37765,#402,.T.);
#46970=EDGE_CURVE('',#37764,#37763,#403,.T.);
#46971=EDGE_CURVE('',#37776,#37777,#30952,.T.);
#46972=EDGE_CURVE('',#37777,#37778,#20464,.T.);
#46973=EDGE_CURVE('',#37779,#37778,#30953,.T.);
#46974=EDGE_CURVE('',#37780,#37779,#30954,.T.);
#46975=EDGE_CURVE('',#37781,#37780,#30955,.T.);
#46976=EDGE_CURVE('',#37781,#37776,#20465,.T.);
#46977=EDGE_CURVE('',#37779,#37782,#20466,.T.);
#46978=EDGE_CURVE('',#37782,#37783,#30956,.T.);
#46979=EDGE_CURVE('',#37783,#37780,#20467,.T.);
#46980=EDGE_CURVE('',#37784,#37785,#30957,.T.);
#46981=EDGE_CURVE('',#37785,#37786,#20468,.T.);
#46982=EDGE_CURVE('',#37786,#37787,#30958,.T.);
#46983=EDGE_CURVE('',#37787,#37784,#20469,.T.);
#46984=EDGE_CURVE('',#37788,#37789,#30959,.T.);
#46985=EDGE_CURVE('',#37789,#37790,#20470,.T.);
#46986=EDGE_CURVE('',#37791,#37790,#30960,.T.);
#46987=EDGE_CURVE('',#37792,#37791,#30961,.T.);
#46988=EDGE_CURVE('',#37793,#37792,#30962,.T.);
#46989=EDGE_CURVE('',#37793,#37788,#20471,.T.);
#46990=EDGE_CURVE('',#37791,#37794,#20472,.T.);
#46991=EDGE_CURVE('',#37794,#37795,#30963,.T.);
#46992=EDGE_CURVE('',#37795,#37792,#20473,.T.);
#46993=EDGE_CURVE('',#37444,#37777,#30964,.T.);
#46994=EDGE_CURVE('',#37776,#37445,#30965,.T.);
#46995=EDGE_CURVE('',#37794,#37128,#404,.T.);
#46996=EDGE_CURVE('',#37127,#37795,#405,.T.);
#46997=EDGE_CURVE('',#37786,#37789,#406,.T.);
#46998=EDGE_CURVE('',#37788,#37787,#407,.T.);
#46999=EDGE_CURVE('',#37782,#37785,#408,.T.);
#47000=EDGE_CURVE('',#37784,#37783,#409,.T.);
#47001=EDGE_CURVE('',#37796,#37797,#30966,.T.);
#47002=EDGE_CURVE('',#37797,#37798,#20474,.T.);
#47003=EDGE_CURVE('',#37799,#37798,#30967,.T.);
#47004=EDGE_CURVE('',#37800,#37799,#30968,.T.);
#47005=EDGE_CURVE('',#37801,#37800,#30969,.T.);
#47006=EDGE_CURVE('',#37801,#37796,#20475,.T.);
#47007=EDGE_CURVE('',#37799,#37802,#20476,.T.);
#47008=EDGE_CURVE('',#37802,#37803,#30970,.T.);
#47009=EDGE_CURVE('',#37803,#37800,#20477,.T.);
#47010=EDGE_CURVE('',#37804,#37805,#30971,.T.);
#47011=EDGE_CURVE('',#37805,#37806,#20478,.T.);
#47012=EDGE_CURVE('',#37806,#37807,#30972,.T.);
#47013=EDGE_CURVE('',#37807,#37804,#20479,.T.);
#47014=EDGE_CURVE('',#37808,#37809,#30973,.T.);
#47015=EDGE_CURVE('',#37809,#37810,#20480,.T.);
#47016=EDGE_CURVE('',#37811,#37810,#30974,.T.);
#47017=EDGE_CURVE('',#37812,#37811,#30975,.T.);
#47018=EDGE_CURVE('',#37813,#37812,#30976,.T.);
#47019=EDGE_CURVE('',#37813,#37808,#20481,.T.);
#47020=EDGE_CURVE('',#37811,#37814,#20482,.T.);
#47021=EDGE_CURVE('',#37814,#37815,#30977,.T.);
#47022=EDGE_CURVE('',#37815,#37812,#20483,.T.);
#47023=EDGE_CURVE('',#37450,#37797,#30978,.T.);
#47024=EDGE_CURVE('',#37796,#37451,#30979,.T.);
#47025=EDGE_CURVE('',#37814,#37122,#410,.T.);
#47026=EDGE_CURVE('',#37121,#37815,#411,.T.);
#47027=EDGE_CURVE('',#37806,#37809,#412,.T.);
#47028=EDGE_CURVE('',#37808,#37807,#413,.T.);
#47029=EDGE_CURVE('',#37802,#37805,#414,.T.);
#47030=EDGE_CURVE('',#37804,#37803,#415,.T.);
#47031=EDGE_CURVE('',#37816,#37817,#30980,.T.);
#47032=EDGE_CURVE('',#37817,#37818,#20484,.T.);
#47033=EDGE_CURVE('',#37819,#37818,#30981,.T.);
#47034=EDGE_CURVE('',#37820,#37819,#30982,.T.);
#47035=EDGE_CURVE('',#37821,#37820,#30983,.T.);
#47036=EDGE_CURVE('',#37821,#37816,#20485,.T.);
#47037=EDGE_CURVE('',#37819,#37822,#20486,.T.);
#47038=EDGE_CURVE('',#37822,#37823,#30984,.T.);
#47039=EDGE_CURVE('',#37823,#37820,#20487,.T.);
#47040=EDGE_CURVE('',#37824,#37825,#30985,.T.);
#47041=EDGE_CURVE('',#37825,#37826,#20488,.T.);
#47042=EDGE_CURVE('',#37826,#37827,#30986,.T.);
#47043=EDGE_CURVE('',#37827,#37824,#20489,.T.);
#47044=EDGE_CURVE('',#37828,#37829,#30987,.T.);
#47045=EDGE_CURVE('',#37829,#37830,#20490,.T.);
#47046=EDGE_CURVE('',#37831,#37830,#30988,.T.);
#47047=EDGE_CURVE('',#37832,#37831,#30989,.T.);
#47048=EDGE_CURVE('',#37833,#37832,#30990,.T.);
#47049=EDGE_CURVE('',#37833,#37828,#20491,.T.);
#47050=EDGE_CURVE('',#37831,#37834,#20492,.T.);
#47051=EDGE_CURVE('',#37834,#37835,#30991,.T.);
#47052=EDGE_CURVE('',#37835,#37832,#20493,.T.);
#47053=EDGE_CURVE('',#37456,#37817,#30992,.T.);
#47054=EDGE_CURVE('',#37816,#37457,#30993,.T.);
#47055=EDGE_CURVE('',#37834,#37116,#416,.T.);
#47056=EDGE_CURVE('',#37115,#37835,#417,.T.);
#47057=EDGE_CURVE('',#37826,#37829,#418,.T.);
#47058=EDGE_CURVE('',#37828,#37827,#419,.T.);
#47059=EDGE_CURVE('',#37822,#37825,#420,.T.);
#47060=EDGE_CURVE('',#37824,#37823,#421,.T.);
#47061=EDGE_CURVE('',#37836,#37837,#30994,.T.);
#47062=EDGE_CURVE('',#37837,#37838,#20494,.T.);
#47063=EDGE_CURVE('',#37839,#37838,#30995,.T.);
#47064=EDGE_CURVE('',#37840,#37839,#30996,.T.);
#47065=EDGE_CURVE('',#37841,#37840,#30997,.T.);
#47066=EDGE_CURVE('',#37841,#37836,#20495,.T.);
#47067=EDGE_CURVE('',#37839,#37842,#20496,.T.);
#47068=EDGE_CURVE('',#37842,#37843,#30998,.T.);
#47069=EDGE_CURVE('',#37843,#37840,#20497,.T.);
#47070=EDGE_CURVE('',#37844,#37845,#30999,.T.);
#47071=EDGE_CURVE('',#37845,#37846,#20498,.T.);
#47072=EDGE_CURVE('',#37846,#37847,#31000,.T.);
#47073=EDGE_CURVE('',#37847,#37844,#20499,.T.);
#47074=EDGE_CURVE('',#37848,#37849,#31001,.T.);
#47075=EDGE_CURVE('',#37849,#37850,#20500,.T.);
#47076=EDGE_CURVE('',#37851,#37850,#31002,.T.);
#47077=EDGE_CURVE('',#37852,#37851,#31003,.T.);
#47078=EDGE_CURVE('',#37853,#37852,#31004,.T.);
#47079=EDGE_CURVE('',#37853,#37848,#20501,.T.);
#47080=EDGE_CURVE('',#37851,#37854,#20502,.T.);
#47081=EDGE_CURVE('',#37854,#37855,#31005,.T.);
#47082=EDGE_CURVE('',#37855,#37852,#20503,.T.);
#47083=EDGE_CURVE('',#37462,#37837,#31006,.T.);
#47084=EDGE_CURVE('',#37836,#37463,#31007,.T.);
#47085=EDGE_CURVE('',#37854,#37110,#422,.T.);
#47086=EDGE_CURVE('',#37109,#37855,#423,.T.);
#47087=EDGE_CURVE('',#37846,#37849,#424,.T.);
#47088=EDGE_CURVE('',#37848,#37847,#425,.T.);
#47089=EDGE_CURVE('',#37842,#37845,#426,.T.);
#47090=EDGE_CURVE('',#37844,#37843,#427,.T.);
#47091=EDGE_CURVE('',#37856,#37857,#31008,.T.);
#47092=EDGE_CURVE('',#37857,#37858,#20504,.T.);
#47093=EDGE_CURVE('',#37859,#37858,#31009,.T.);
#47094=EDGE_CURVE('',#37860,#37859,#31010,.T.);
#47095=EDGE_CURVE('',#37861,#37860,#31011,.T.);
#47096=EDGE_CURVE('',#37861,#37856,#20505,.T.);
#47097=EDGE_CURVE('',#37859,#37862,#20506,.T.);
#47098=EDGE_CURVE('',#37862,#37863,#31012,.T.);
#47099=EDGE_CURVE('',#37863,#37860,#20507,.T.);
#47100=EDGE_CURVE('',#37864,#37865,#31013,.T.);
#47101=EDGE_CURVE('',#37865,#37866,#20508,.T.);
#47102=EDGE_CURVE('',#37866,#37867,#31014,.T.);
#47103=EDGE_CURVE('',#37867,#37864,#20509,.T.);
#47104=EDGE_CURVE('',#37868,#37869,#31015,.T.);
#47105=EDGE_CURVE('',#37869,#37870,#20510,.T.);
#47106=EDGE_CURVE('',#37871,#37870,#31016,.T.);
#47107=EDGE_CURVE('',#37872,#37871,#31017,.T.);
#47108=EDGE_CURVE('',#37873,#37872,#31018,.T.);
#47109=EDGE_CURVE('',#37873,#37868,#20511,.T.);
#47110=EDGE_CURVE('',#37871,#37874,#20512,.T.);
#47111=EDGE_CURVE('',#37874,#37875,#31019,.T.);
#47112=EDGE_CURVE('',#37875,#37872,#20513,.T.);
#47113=EDGE_CURVE('',#37466,#37857,#31020,.T.);
#47114=EDGE_CURVE('',#37856,#37467,#31021,.T.);
#47115=EDGE_CURVE('',#37874,#37106,#428,.T.);
#47116=EDGE_CURVE('',#37105,#37875,#429,.T.);
#47117=EDGE_CURVE('',#37866,#37869,#430,.T.);
#47118=EDGE_CURVE('',#37868,#37867,#431,.T.);
#47119=EDGE_CURVE('',#37862,#37865,#432,.T.);
#47120=EDGE_CURVE('',#37864,#37863,#433,.T.);
#47121=EDGE_CURVE('',#37876,#37877,#31022,.T.);
#47122=EDGE_CURVE('',#37877,#37878,#20514,.T.);
#47123=EDGE_CURVE('',#37879,#37878,#31023,.T.);
#47124=EDGE_CURVE('',#37880,#37879,#31024,.T.);
#47125=EDGE_CURVE('',#37881,#37880,#31025,.T.);
#47126=EDGE_CURVE('',#37881,#37876,#20515,.T.);
#47127=EDGE_CURVE('',#37879,#37882,#20516,.T.);
#47128=EDGE_CURVE('',#37882,#37883,#31026,.T.);
#47129=EDGE_CURVE('',#37883,#37880,#20517,.T.);
#47130=EDGE_CURVE('',#37884,#37885,#31027,.T.);
#47131=EDGE_CURVE('',#37885,#37886,#20518,.T.);
#47132=EDGE_CURVE('',#37886,#37887,#31028,.T.);
#47133=EDGE_CURVE('',#37887,#37884,#20519,.T.);
#47134=EDGE_CURVE('',#37888,#37889,#31029,.T.);
#47135=EDGE_CURVE('',#37889,#37890,#20520,.T.);
#47136=EDGE_CURVE('',#37891,#37890,#31030,.T.);
#47137=EDGE_CURVE('',#37892,#37891,#31031,.T.);
#47138=EDGE_CURVE('',#37893,#37892,#31032,.T.);
#47139=EDGE_CURVE('',#37893,#37888,#20521,.T.);
#47140=EDGE_CURVE('',#37891,#37894,#20522,.T.);
#47141=EDGE_CURVE('',#37894,#37895,#31033,.T.);
#47142=EDGE_CURVE('',#37895,#37892,#20523,.T.);
#47143=EDGE_CURVE('',#37472,#37877,#31034,.T.);
#47144=EDGE_CURVE('',#37876,#37473,#31035,.T.);
#47145=EDGE_CURVE('',#37894,#37100,#434,.T.);
#47146=EDGE_CURVE('',#37099,#37895,#435,.T.);
#47147=EDGE_CURVE('',#37886,#37889,#436,.T.);
#47148=EDGE_CURVE('',#37888,#37887,#437,.T.);
#47149=EDGE_CURVE('',#37882,#37885,#438,.T.);
#47150=EDGE_CURVE('',#37884,#37883,#439,.T.);
#47151=EDGE_CURVE('',#37896,#37897,#31036,.T.);
#47152=EDGE_CURVE('',#37897,#37898,#20524,.T.);
#47153=EDGE_CURVE('',#37899,#37898,#31037,.T.);
#47154=EDGE_CURVE('',#37900,#37899,#31038,.T.);
#47155=EDGE_CURVE('',#37901,#37900,#31039,.T.);
#47156=EDGE_CURVE('',#37901,#37896,#20525,.T.);
#47157=EDGE_CURVE('',#37899,#37902,#20526,.T.);
#47158=EDGE_CURVE('',#37902,#37903,#31040,.T.);
#47159=EDGE_CURVE('',#37903,#37900,#20527,.T.);
#47160=EDGE_CURVE('',#37904,#37905,#31041,.T.);
#47161=EDGE_CURVE('',#37905,#37906,#20528,.T.);
#47162=EDGE_CURVE('',#37906,#37907,#31042,.T.);
#47163=EDGE_CURVE('',#37907,#37904,#20529,.T.);
#47164=EDGE_CURVE('',#37908,#37909,#31043,.T.);
#47165=EDGE_CURVE('',#37909,#37910,#20530,.T.);
#47166=EDGE_CURVE('',#37911,#37910,#31044,.T.);
#47167=EDGE_CURVE('',#37912,#37911,#31045,.T.);
#47168=EDGE_CURVE('',#37913,#37912,#31046,.T.);
#47169=EDGE_CURVE('',#37913,#37908,#20531,.T.);
#47170=EDGE_CURVE('',#37911,#37914,#20532,.T.);
#47171=EDGE_CURVE('',#37914,#37915,#31047,.T.);
#47172=EDGE_CURVE('',#37915,#37912,#20533,.T.);
#47173=EDGE_CURVE('',#37478,#37897,#31048,.T.);
#47174=EDGE_CURVE('',#37896,#37479,#31049,.T.);
#47175=EDGE_CURVE('',#37914,#37094,#440,.T.);
#47176=EDGE_CURVE('',#37093,#37915,#441,.T.);
#47177=EDGE_CURVE('',#37906,#37909,#442,.T.);
#47178=EDGE_CURVE('',#37908,#37907,#443,.T.);
#47179=EDGE_CURVE('',#37902,#37905,#444,.T.);
#47180=EDGE_CURVE('',#37904,#37903,#445,.T.);
#47181=EDGE_CURVE('',#37916,#37917,#31050,.T.);
#47182=EDGE_CURVE('',#37917,#37918,#20534,.T.);
#47183=EDGE_CURVE('',#37919,#37918,#31051,.T.);
#47184=EDGE_CURVE('',#37920,#37919,#31052,.T.);
#47185=EDGE_CURVE('',#37921,#37920,#31053,.T.);
#47186=EDGE_CURVE('',#37921,#37916,#20535,.T.);
#47187=EDGE_CURVE('',#37919,#37922,#20536,.T.);
#47188=EDGE_CURVE('',#37922,#37923,#31054,.T.);
#47189=EDGE_CURVE('',#37923,#37920,#20537,.T.);
#47190=EDGE_CURVE('',#37924,#37925,#31055,.T.);
#47191=EDGE_CURVE('',#37925,#37926,#20538,.T.);
#47192=EDGE_CURVE('',#37926,#37927,#31056,.T.);
#47193=EDGE_CURVE('',#37927,#37924,#20539,.T.);
#47194=EDGE_CURVE('',#37928,#37929,#31057,.T.);
#47195=EDGE_CURVE('',#37929,#37930,#20540,.T.);
#47196=EDGE_CURVE('',#37931,#37930,#31058,.T.);
#47197=EDGE_CURVE('',#37932,#37931,#31059,.T.);
#47198=EDGE_CURVE('',#37933,#37932,#31060,.T.);
#47199=EDGE_CURVE('',#37933,#37928,#20541,.T.);
#47200=EDGE_CURVE('',#37931,#37934,#20542,.T.);
#47201=EDGE_CURVE('',#37934,#37935,#31061,.T.);
#47202=EDGE_CURVE('',#37935,#37932,#20543,.T.);
#47203=EDGE_CURVE('',#37484,#37917,#31062,.T.);
#47204=EDGE_CURVE('',#37916,#37485,#31063,.T.);
#47205=EDGE_CURVE('',#37934,#37088,#446,.T.);
#47206=EDGE_CURVE('',#37087,#37935,#447,.T.);
#47207=EDGE_CURVE('',#37926,#37929,#448,.T.);
#47208=EDGE_CURVE('',#37928,#37927,#449,.T.);
#47209=EDGE_CURVE('',#37922,#37925,#450,.T.);
#47210=EDGE_CURVE('',#37924,#37923,#451,.T.);
#47211=EDGE_CURVE('',#37936,#37937,#31064,.T.);
#47212=EDGE_CURVE('',#37937,#37938,#20544,.T.);
#47213=EDGE_CURVE('',#37939,#37938,#31065,.T.);
#47214=EDGE_CURVE('',#37940,#37939,#31066,.T.);
#47215=EDGE_CURVE('',#37941,#37940,#31067,.T.);
#47216=EDGE_CURVE('',#37941,#37936,#20545,.T.);
#47217=EDGE_CURVE('',#37939,#37942,#20546,.T.);
#47218=EDGE_CURVE('',#37942,#37943,#31068,.T.);
#47219=EDGE_CURVE('',#37943,#37940,#20547,.T.);
#47220=EDGE_CURVE('',#37944,#37945,#31069,.T.);
#47221=EDGE_CURVE('',#37945,#37946,#20548,.T.);
#47222=EDGE_CURVE('',#37946,#37947,#31070,.T.);
#47223=EDGE_CURVE('',#37947,#37944,#20549,.T.);
#47224=EDGE_CURVE('',#37948,#37949,#31071,.T.);
#47225=EDGE_CURVE('',#37949,#37950,#20550,.T.);
#47226=EDGE_CURVE('',#37951,#37950,#31072,.T.);
#47227=EDGE_CURVE('',#37952,#37951,#31073,.T.);
#47228=EDGE_CURVE('',#37953,#37952,#31074,.T.);
#47229=EDGE_CURVE('',#37953,#37948,#20551,.T.);
#47230=EDGE_CURVE('',#37951,#37954,#20552,.T.);
#47231=EDGE_CURVE('',#37954,#37955,#31075,.T.);
#47232=EDGE_CURVE('',#37955,#37952,#20553,.T.);
#47233=EDGE_CURVE('',#37490,#37937,#31076,.T.);
#47234=EDGE_CURVE('',#37936,#37491,#31077,.T.);
#47235=EDGE_CURVE('',#37954,#37082,#452,.T.);
#47236=EDGE_CURVE('',#37081,#37955,#453,.T.);
#47237=EDGE_CURVE('',#37946,#37949,#454,.T.);
#47238=EDGE_CURVE('',#37948,#37947,#455,.T.);
#47239=EDGE_CURVE('',#37942,#37945,#456,.T.);
#47240=EDGE_CURVE('',#37944,#37943,#457,.T.);
#47241=EDGE_CURVE('',#37956,#37957,#31078,.T.);
#47242=EDGE_CURVE('',#37957,#37958,#20554,.T.);
#47243=EDGE_CURVE('',#37959,#37958,#31079,.T.);
#47244=EDGE_CURVE('',#37960,#37959,#31080,.T.);
#47245=EDGE_CURVE('',#37961,#37960,#31081,.T.);
#47246=EDGE_CURVE('',#37961,#37956,#20555,.T.);
#47247=EDGE_CURVE('',#37959,#37962,#20556,.T.);
#47248=EDGE_CURVE('',#37962,#37963,#31082,.T.);
#47249=EDGE_CURVE('',#37963,#37960,#20557,.T.);
#47250=EDGE_CURVE('',#37964,#37965,#31083,.T.);
#47251=EDGE_CURVE('',#37965,#37966,#20558,.T.);
#47252=EDGE_CURVE('',#37966,#37967,#31084,.T.);
#47253=EDGE_CURVE('',#37967,#37964,#20559,.T.);
#47254=EDGE_CURVE('',#37968,#37969,#31085,.T.);
#47255=EDGE_CURVE('',#37969,#37970,#20560,.T.);
#47256=EDGE_CURVE('',#37971,#37970,#31086,.T.);
#47257=EDGE_CURVE('',#37972,#37971,#31087,.T.);
#47258=EDGE_CURVE('',#37973,#37972,#31088,.T.);
#47259=EDGE_CURVE('',#37973,#37968,#20561,.T.);
#47260=EDGE_CURVE('',#37971,#37974,#20562,.T.);
#47261=EDGE_CURVE('',#37974,#37975,#31089,.T.);
#47262=EDGE_CURVE('',#37975,#37972,#20563,.T.);
#47263=EDGE_CURVE('',#37496,#37957,#31090,.T.);
#47264=EDGE_CURVE('',#37956,#37497,#31091,.T.);
#47265=EDGE_CURVE('',#37974,#37076,#458,.T.);
#47266=EDGE_CURVE('',#37075,#37975,#459,.T.);
#47267=EDGE_CURVE('',#37966,#37969,#460,.T.);
#47268=EDGE_CURVE('',#37968,#37967,#461,.T.);
#47269=EDGE_CURVE('',#37962,#37965,#462,.T.);
#47270=EDGE_CURVE('',#37964,#37963,#463,.T.);
#47271=EDGE_CURVE('',#37976,#37977,#31092,.T.);
#47272=EDGE_CURVE('',#37977,#37978,#20564,.T.);
#47273=EDGE_CURVE('',#37979,#37978,#31093,.T.);
#47274=EDGE_CURVE('',#37980,#37979,#31094,.T.);
#47275=EDGE_CURVE('',#37981,#37980,#31095,.T.);
#47276=EDGE_CURVE('',#37981,#37976,#20565,.T.);
#47277=EDGE_CURVE('',#37979,#37982,#20566,.T.);
#47278=EDGE_CURVE('',#37982,#37983,#31096,.T.);
#47279=EDGE_CURVE('',#37983,#37980,#20567,.T.);
#47280=EDGE_CURVE('',#37984,#37985,#31097,.T.);
#47281=EDGE_CURVE('',#37985,#37986,#20568,.T.);
#47282=EDGE_CURVE('',#37986,#37987,#31098,.T.);
#47283=EDGE_CURVE('',#37987,#37984,#20569,.T.);
#47284=EDGE_CURVE('',#37988,#37989,#31099,.T.);
#47285=EDGE_CURVE('',#37989,#37990,#20570,.T.);
#47286=EDGE_CURVE('',#37991,#37990,#31100,.T.);
#47287=EDGE_CURVE('',#37992,#37991,#31101,.T.);
#47288=EDGE_CURVE('',#37993,#37992,#31102,.T.);
#47289=EDGE_CURVE('',#37993,#37988,#20571,.T.);
#47290=EDGE_CURVE('',#37991,#37994,#20572,.T.);
#47291=EDGE_CURVE('',#37994,#37995,#31103,.T.);
#47292=EDGE_CURVE('',#37995,#37992,#20573,.T.);
#47293=EDGE_CURVE('',#37502,#37977,#31104,.T.);
#47294=EDGE_CURVE('',#37976,#37503,#31105,.T.);
#47295=EDGE_CURVE('',#37994,#37070,#464,.T.);
#47296=EDGE_CURVE('',#37069,#37995,#465,.T.);
#47297=EDGE_CURVE('',#37986,#37989,#466,.T.);
#47298=EDGE_CURVE('',#37988,#37987,#467,.T.);
#47299=EDGE_CURVE('',#37982,#37985,#468,.T.);
#47300=EDGE_CURVE('',#37984,#37983,#469,.T.);
#47301=EDGE_CURVE('',#37996,#37997,#31106,.T.);
#47302=EDGE_CURVE('',#37997,#37998,#20574,.T.);
#47303=EDGE_CURVE('',#37999,#37998,#31107,.T.);
#47304=EDGE_CURVE('',#38000,#37999,#31108,.T.);
#47305=EDGE_CURVE('',#38001,#38000,#31109,.T.);
#47306=EDGE_CURVE('',#38001,#37996,#20575,.T.);
#47307=EDGE_CURVE('',#37999,#38002,#20576,.T.);
#47308=EDGE_CURVE('',#38002,#38003,#31110,.T.);
#47309=EDGE_CURVE('',#38003,#38000,#20577,.T.);
#47310=EDGE_CURVE('',#38004,#38005,#31111,.T.);
#47311=EDGE_CURVE('',#38005,#38006,#20578,.T.);
#47312=EDGE_CURVE('',#38006,#38007,#31112,.T.);
#47313=EDGE_CURVE('',#38007,#38004,#20579,.T.);
#47314=EDGE_CURVE('',#38008,#38009,#31113,.T.);
#47315=EDGE_CURVE('',#38009,#38010,#20580,.T.);
#47316=EDGE_CURVE('',#38011,#38010,#31114,.T.);
#47317=EDGE_CURVE('',#38012,#38011,#31115,.T.);
#47318=EDGE_CURVE('',#38013,#38012,#31116,.T.);
#47319=EDGE_CURVE('',#38013,#38008,#20581,.T.);
#47320=EDGE_CURVE('',#38011,#38014,#20582,.T.);
#47321=EDGE_CURVE('',#38014,#38015,#31117,.T.);
#47322=EDGE_CURVE('',#38015,#38012,#20583,.T.);
#47323=EDGE_CURVE('',#37508,#37997,#31118,.T.);
#47324=EDGE_CURVE('',#37996,#37509,#31119,.T.);
#47325=EDGE_CURVE('',#38014,#37064,#470,.T.);
#47326=EDGE_CURVE('',#37063,#38015,#471,.T.);
#47327=EDGE_CURVE('',#38006,#38009,#472,.T.);
#47328=EDGE_CURVE('',#38008,#38007,#473,.T.);
#47329=EDGE_CURVE('',#38002,#38005,#474,.T.);
#47330=EDGE_CURVE('',#38004,#38003,#475,.T.);
#47331=EDGE_CURVE('',#38016,#38017,#31120,.T.);
#47332=EDGE_CURVE('',#38017,#38018,#20584,.T.);
#47333=EDGE_CURVE('',#38019,#38018,#31121,.T.);
#47334=EDGE_CURVE('',#38020,#38019,#31122,.T.);
#47335=EDGE_CURVE('',#38021,#38020,#31123,.T.);
#47336=EDGE_CURVE('',#38021,#38016,#20585,.T.);
#47337=EDGE_CURVE('',#38019,#38022,#20586,.T.);
#47338=EDGE_CURVE('',#38022,#38023,#31124,.T.);
#47339=EDGE_CURVE('',#38023,#38020,#20587,.T.);
#47340=EDGE_CURVE('',#38024,#38025,#31125,.T.);
#47341=EDGE_CURVE('',#38025,#38026,#20588,.T.);
#47342=EDGE_CURVE('',#38026,#38027,#31126,.T.);
#47343=EDGE_CURVE('',#38027,#38024,#20589,.T.);
#47344=EDGE_CURVE('',#38028,#38029,#31127,.T.);
#47345=EDGE_CURVE('',#38029,#38030,#20590,.T.);
#47346=EDGE_CURVE('',#38031,#38030,#31128,.T.);
#47347=EDGE_CURVE('',#38032,#38031,#31129,.T.);
#47348=EDGE_CURVE('',#38033,#38032,#31130,.T.);
#47349=EDGE_CURVE('',#38033,#38028,#20591,.T.);
#47350=EDGE_CURVE('',#38031,#38034,#20592,.T.);
#47351=EDGE_CURVE('',#38034,#38035,#31131,.T.);
#47352=EDGE_CURVE('',#38035,#38032,#20593,.T.);
#47353=EDGE_CURVE('',#37514,#38017,#31132,.T.);
#47354=EDGE_CURVE('',#38016,#37515,#31133,.T.);
#47355=EDGE_CURVE('',#38034,#37058,#476,.T.);
#47356=EDGE_CURVE('',#37057,#38035,#477,.T.);
#47357=EDGE_CURVE('',#38026,#38029,#478,.T.);
#47358=EDGE_CURVE('',#38028,#38027,#479,.T.);
#47359=EDGE_CURVE('',#38022,#38025,#480,.T.);
#47360=EDGE_CURVE('',#38024,#38023,#481,.T.);
#47361=EDGE_CURVE('',#38036,#38037,#31134,.T.);
#47362=EDGE_CURVE('',#38037,#38038,#20594,.T.);
#47363=EDGE_CURVE('',#38039,#38038,#31135,.T.);
#47364=EDGE_CURVE('',#38040,#38039,#31136,.T.);
#47365=EDGE_CURVE('',#38041,#38040,#31137,.T.);
#47366=EDGE_CURVE('',#38041,#38036,#20595,.T.);
#47367=EDGE_CURVE('',#38039,#38042,#20596,.T.);
#47368=EDGE_CURVE('',#38042,#38043,#31138,.T.);
#47369=EDGE_CURVE('',#38043,#38040,#20597,.T.);
#47370=EDGE_CURVE('',#38044,#38045,#31139,.T.);
#47371=EDGE_CURVE('',#38045,#38046,#20598,.T.);
#47372=EDGE_CURVE('',#38046,#38047,#31140,.T.);
#47373=EDGE_CURVE('',#38047,#38044,#20599,.T.);
#47374=EDGE_CURVE('',#38048,#38049,#31141,.T.);
#47375=EDGE_CURVE('',#38049,#38050,#20600,.T.);
#47376=EDGE_CURVE('',#38051,#38050,#31142,.T.);
#47377=EDGE_CURVE('',#38052,#38051,#31143,.T.);
#47378=EDGE_CURVE('',#38053,#38052,#31144,.T.);
#47379=EDGE_CURVE('',#38053,#38048,#20601,.T.);
#47380=EDGE_CURVE('',#38051,#38054,#20602,.T.);
#47381=EDGE_CURVE('',#38054,#38055,#31145,.T.);
#47382=EDGE_CURVE('',#38055,#38052,#20603,.T.);
#47383=EDGE_CURVE('',#37520,#38037,#31146,.T.);
#47384=EDGE_CURVE('',#38036,#37521,#31147,.T.);
#47385=EDGE_CURVE('',#38054,#37052,#482,.T.);
#47386=EDGE_CURVE('',#37051,#38055,#483,.T.);
#47387=EDGE_CURVE('',#38046,#38049,#484,.T.);
#47388=EDGE_CURVE('',#38048,#38047,#485,.T.);
#47389=EDGE_CURVE('',#38042,#38045,#486,.T.);
#47390=EDGE_CURVE('',#38044,#38043,#487,.T.);
#47391=EDGE_CURVE('',#38056,#38057,#31148,.T.);
#47392=EDGE_CURVE('',#38057,#38058,#20604,.T.);
#47393=EDGE_CURVE('',#38059,#38058,#31149,.T.);
#47394=EDGE_CURVE('',#38060,#38059,#31150,.T.);
#47395=EDGE_CURVE('',#38061,#38060,#31151,.T.);
#47396=EDGE_CURVE('',#38061,#38056,#20605,.T.);
#47397=EDGE_CURVE('',#38059,#38062,#20606,.T.);
#47398=EDGE_CURVE('',#38062,#38063,#31152,.T.);
#47399=EDGE_CURVE('',#38063,#38060,#20607,.T.);
#47400=EDGE_CURVE('',#38064,#38065,#31153,.T.);
#47401=EDGE_CURVE('',#38065,#38066,#20608,.T.);
#47402=EDGE_CURVE('',#38066,#38067,#31154,.T.);
#47403=EDGE_CURVE('',#38067,#38064,#20609,.T.);
#47404=EDGE_CURVE('',#38068,#38069,#31155,.T.);
#47405=EDGE_CURVE('',#38069,#38070,#20610,.T.);
#47406=EDGE_CURVE('',#38071,#38070,#31156,.T.);
#47407=EDGE_CURVE('',#38072,#38071,#31157,.T.);
#47408=EDGE_CURVE('',#38073,#38072,#31158,.T.);
#47409=EDGE_CURVE('',#38073,#38068,#20611,.T.);
#47410=EDGE_CURVE('',#38071,#38074,#20612,.T.);
#47411=EDGE_CURVE('',#38074,#38075,#31159,.T.);
#47412=EDGE_CURVE('',#38075,#38072,#20613,.T.);
#47413=EDGE_CURVE('',#37526,#38057,#31160,.T.);
#47414=EDGE_CURVE('',#38056,#37527,#31161,.T.);
#47415=EDGE_CURVE('',#38074,#37046,#488,.T.);
#47416=EDGE_CURVE('',#37045,#38075,#489,.T.);
#47417=EDGE_CURVE('',#38066,#38069,#490,.T.);
#47418=EDGE_CURVE('',#38068,#38067,#491,.T.);
#47419=EDGE_CURVE('',#38062,#38065,#492,.T.);
#47420=EDGE_CURVE('',#38064,#38063,#493,.T.);
#47421=EDGE_CURVE('',#38076,#38077,#31162,.T.);
#47422=EDGE_CURVE('',#38077,#38078,#20614,.T.);
#47423=EDGE_CURVE('',#38079,#38078,#31163,.T.);
#47424=EDGE_CURVE('',#38080,#38079,#31164,.T.);
#47425=EDGE_CURVE('',#38081,#38080,#31165,.T.);
#47426=EDGE_CURVE('',#38081,#38076,#20615,.T.);
#47427=EDGE_CURVE('',#38079,#38082,#20616,.T.);
#47428=EDGE_CURVE('',#38082,#38083,#31166,.T.);
#47429=EDGE_CURVE('',#38083,#38080,#20617,.T.);
#47430=EDGE_CURVE('',#38084,#38085,#31167,.T.);
#47431=EDGE_CURVE('',#38085,#38086,#20618,.T.);
#47432=EDGE_CURVE('',#38086,#38087,#31168,.T.);
#47433=EDGE_CURVE('',#38087,#38084,#20619,.T.);
#47434=EDGE_CURVE('',#38088,#38089,#31169,.T.);
#47435=EDGE_CURVE('',#38089,#38090,#20620,.T.);
#47436=EDGE_CURVE('',#38091,#38090,#31170,.T.);
#47437=EDGE_CURVE('',#38092,#38091,#31171,.T.);
#47438=EDGE_CURVE('',#38093,#38092,#31172,.T.);
#47439=EDGE_CURVE('',#38093,#38088,#20621,.T.);
#47440=EDGE_CURVE('',#38091,#38094,#20622,.T.);
#47441=EDGE_CURVE('',#38094,#38095,#31173,.T.);
#47442=EDGE_CURVE('',#38095,#38092,#20623,.T.);
#47443=EDGE_CURVE('',#37532,#38077,#31174,.T.);
#47444=EDGE_CURVE('',#38076,#37533,#31175,.T.);
#47445=EDGE_CURVE('',#38094,#37040,#494,.T.);
#47446=EDGE_CURVE('',#37039,#38095,#495,.T.);
#47447=EDGE_CURVE('',#38086,#38089,#496,.T.);
#47448=EDGE_CURVE('',#38088,#38087,#497,.T.);
#47449=EDGE_CURVE('',#38082,#38085,#498,.T.);
#47450=EDGE_CURVE('',#38084,#38083,#499,.T.);
#47451=EDGE_CURVE('',#38096,#38097,#31176,.T.);
#47452=EDGE_CURVE('',#38097,#38098,#20624,.T.);
#47453=EDGE_CURVE('',#38099,#38098,#31177,.T.);
#47454=EDGE_CURVE('',#38100,#38099,#31178,.T.);
#47455=EDGE_CURVE('',#38101,#38100,#31179,.T.);
#47456=EDGE_CURVE('',#38101,#38096,#20625,.T.);
#47457=EDGE_CURVE('',#38099,#38102,#20626,.T.);
#47458=EDGE_CURVE('',#38102,#38103,#31180,.T.);
#47459=EDGE_CURVE('',#38103,#38100,#20627,.T.);
#47460=EDGE_CURVE('',#38104,#38105,#31181,.T.);
#47461=EDGE_CURVE('',#38105,#38106,#20628,.T.);
#47462=EDGE_CURVE('',#38106,#38107,#31182,.T.);
#47463=EDGE_CURVE('',#38107,#38104,#20629,.T.);
#47464=EDGE_CURVE('',#38108,#38109,#31183,.T.);
#47465=EDGE_CURVE('',#38109,#38110,#20630,.T.);
#47466=EDGE_CURVE('',#38111,#38110,#31184,.T.);
#47467=EDGE_CURVE('',#38112,#38111,#31185,.T.);
#47468=EDGE_CURVE('',#38113,#38112,#31186,.T.);
#47469=EDGE_CURVE('',#38113,#38108,#20631,.T.);
#47470=EDGE_CURVE('',#38111,#38114,#20632,.T.);
#47471=EDGE_CURVE('',#38114,#38115,#31187,.T.);
#47472=EDGE_CURVE('',#38115,#38112,#20633,.T.);
#47473=EDGE_CURVE('',#37538,#38097,#31188,.T.);
#47474=EDGE_CURVE('',#38096,#37539,#31189,.T.);
#47475=EDGE_CURVE('',#38114,#37034,#500,.T.);
#47476=EDGE_CURVE('',#37033,#38115,#501,.T.);
#47477=EDGE_CURVE('',#38106,#38109,#502,.T.);
#47478=EDGE_CURVE('',#38108,#38107,#503,.T.);
#47479=EDGE_CURVE('',#38102,#38105,#504,.T.);
#47480=EDGE_CURVE('',#38104,#38103,#505,.T.);
#47481=EDGE_CURVE('',#38116,#38117,#31190,.T.);
#47482=EDGE_CURVE('',#38117,#38118,#20634,.T.);
#47483=EDGE_CURVE('',#38119,#38118,#31191,.T.);
#47484=EDGE_CURVE('',#38120,#38119,#31192,.T.);
#47485=EDGE_CURVE('',#38121,#38120,#31193,.T.);
#47486=EDGE_CURVE('',#38121,#38116,#20635,.T.);
#47487=EDGE_CURVE('',#38119,#38122,#20636,.T.);
#47488=EDGE_CURVE('',#38122,#38123,#31194,.T.);
#47489=EDGE_CURVE('',#38123,#38120,#20637,.T.);
#47490=EDGE_CURVE('',#38124,#38125,#31195,.T.);
#47491=EDGE_CURVE('',#38125,#38126,#20638,.T.);
#47492=EDGE_CURVE('',#38126,#38127,#31196,.T.);
#47493=EDGE_CURVE('',#38127,#38124,#20639,.T.);
#47494=EDGE_CURVE('',#38128,#38129,#31197,.T.);
#47495=EDGE_CURVE('',#38129,#38130,#20640,.T.);
#47496=EDGE_CURVE('',#38131,#38130,#31198,.T.);
#47497=EDGE_CURVE('',#38132,#38131,#31199,.T.);
#47498=EDGE_CURVE('',#38133,#38132,#31200,.T.);
#47499=EDGE_CURVE('',#38133,#38128,#20641,.T.);
#47500=EDGE_CURVE('',#38131,#38134,#20642,.T.);
#47501=EDGE_CURVE('',#38134,#38135,#31201,.T.);
#47502=EDGE_CURVE('',#38135,#38132,#20643,.T.);
#47503=EDGE_CURVE('',#37544,#38117,#31202,.T.);
#47504=EDGE_CURVE('',#38116,#37545,#31203,.T.);
#47505=EDGE_CURVE('',#38134,#37028,#506,.T.);
#47506=EDGE_CURVE('',#37027,#38135,#507,.T.);
#47507=EDGE_CURVE('',#38126,#38129,#508,.T.);
#47508=EDGE_CURVE('',#38128,#38127,#509,.T.);
#47509=EDGE_CURVE('',#38122,#38125,#510,.T.);
#47510=EDGE_CURVE('',#38124,#38123,#511,.T.);
#47511=EDGE_CURVE('',#38136,#38137,#31204,.T.);
#47512=EDGE_CURVE('',#38137,#38138,#20644,.T.);
#47513=EDGE_CURVE('',#38139,#38138,#31205,.T.);
#47514=EDGE_CURVE('',#38140,#38139,#31206,.T.);
#47515=EDGE_CURVE('',#38141,#38140,#31207,.T.);
#47516=EDGE_CURVE('',#38141,#38136,#20645,.T.);
#47517=EDGE_CURVE('',#38139,#38142,#20646,.T.);
#47518=EDGE_CURVE('',#38142,#38143,#31208,.T.);
#47519=EDGE_CURVE('',#38143,#38140,#20647,.T.);
#47520=EDGE_CURVE('',#38144,#38145,#31209,.T.);
#47521=EDGE_CURVE('',#38145,#38146,#20648,.T.);
#47522=EDGE_CURVE('',#38146,#38147,#31210,.T.);
#47523=EDGE_CURVE('',#38147,#38144,#20649,.T.);
#47524=EDGE_CURVE('',#38148,#38149,#31211,.T.);
#47525=EDGE_CURVE('',#38149,#38150,#20650,.T.);
#47526=EDGE_CURVE('',#38151,#38150,#31212,.T.);
#47527=EDGE_CURVE('',#38152,#38151,#31213,.T.);
#47528=EDGE_CURVE('',#38153,#38152,#31214,.T.);
#47529=EDGE_CURVE('',#38153,#38148,#20651,.T.);
#47530=EDGE_CURVE('',#38151,#38154,#20652,.T.);
#47531=EDGE_CURVE('',#38154,#38155,#31215,.T.);
#47532=EDGE_CURVE('',#38155,#38152,#20653,.T.);
#47533=EDGE_CURVE('',#37550,#38137,#31216,.T.);
#47534=EDGE_CURVE('',#38136,#37551,#31217,.T.);
#47535=EDGE_CURVE('',#38154,#37022,#512,.T.);
#47536=EDGE_CURVE('',#37021,#38155,#513,.T.);
#47537=EDGE_CURVE('',#38146,#38149,#514,.T.);
#47538=EDGE_CURVE('',#38148,#38147,#515,.T.);
#47539=EDGE_CURVE('',#38142,#38145,#516,.T.);
#47540=EDGE_CURVE('',#38144,#38143,#517,.T.);
#47541=EDGE_CURVE('',#38156,#38157,#31218,.T.);
#47542=EDGE_CURVE('',#38157,#38158,#20654,.T.);
#47543=EDGE_CURVE('',#38159,#38158,#31219,.T.);
#47544=EDGE_CURVE('',#38160,#38159,#31220,.T.);
#47545=EDGE_CURVE('',#38161,#38160,#31221,.T.);
#47546=EDGE_CURVE('',#38161,#38156,#20655,.T.);
#47547=EDGE_CURVE('',#38159,#38162,#20656,.T.);
#47548=EDGE_CURVE('',#38162,#38163,#31222,.T.);
#47549=EDGE_CURVE('',#38163,#38160,#20657,.T.);
#47550=EDGE_CURVE('',#38164,#38165,#31223,.T.);
#47551=EDGE_CURVE('',#38165,#38166,#20658,.T.);
#47552=EDGE_CURVE('',#38166,#38167,#31224,.T.);
#47553=EDGE_CURVE('',#38167,#38164,#20659,.T.);
#47554=EDGE_CURVE('',#38168,#38169,#31225,.T.);
#47555=EDGE_CURVE('',#38169,#38170,#20660,.T.);
#47556=EDGE_CURVE('',#38171,#38170,#31226,.T.);
#47557=EDGE_CURVE('',#38172,#38171,#31227,.T.);
#47558=EDGE_CURVE('',#38173,#38172,#31228,.T.);
#47559=EDGE_CURVE('',#38173,#38168,#20661,.T.);
#47560=EDGE_CURVE('',#38171,#38174,#20662,.T.);
#47561=EDGE_CURVE('',#38174,#38175,#31229,.T.);
#47562=EDGE_CURVE('',#38175,#38172,#20663,.T.);
#47563=EDGE_CURVE('',#37197,#38157,#31230,.T.);
#47564=EDGE_CURVE('',#38156,#37198,#31231,.T.);
#47565=EDGE_CURVE('',#38174,#37018,#518,.T.);
#47566=EDGE_CURVE('',#37017,#38175,#519,.T.);
#47567=EDGE_CURVE('',#38166,#38169,#520,.T.);
#47568=EDGE_CURVE('',#38168,#38167,#521,.T.);
#47569=EDGE_CURVE('',#38162,#38165,#522,.T.);
#47570=EDGE_CURVE('',#38164,#38163,#523,.T.);
#47571=EDGE_CURVE('',#38176,#38177,#31232,.T.);
#47572=EDGE_CURVE('',#38177,#38178,#20664,.T.);
#47573=EDGE_CURVE('',#38179,#38178,#31233,.T.);
#47574=EDGE_CURVE('',#38180,#38179,#31234,.T.);
#47575=EDGE_CURVE('',#38181,#38180,#31235,.T.);
#47576=EDGE_CURVE('',#38181,#38176,#20665,.T.);
#47577=EDGE_CURVE('',#38179,#38182,#20666,.T.);
#47578=EDGE_CURVE('',#38182,#38183,#31236,.T.);
#47579=EDGE_CURVE('',#38183,#38180,#20667,.T.);
#47580=EDGE_CURVE('',#38184,#38185,#31237,.T.);
#47581=EDGE_CURVE('',#38185,#38186,#20668,.T.);
#47582=EDGE_CURVE('',#38186,#38187,#31238,.T.);
#47583=EDGE_CURVE('',#38187,#38184,#20669,.T.);
#47584=EDGE_CURVE('',#38188,#38189,#31239,.T.);
#47585=EDGE_CURVE('',#38189,#38190,#20670,.T.);
#47586=EDGE_CURVE('',#38191,#38190,#31240,.T.);
#47587=EDGE_CURVE('',#38192,#38191,#31241,.T.);
#47588=EDGE_CURVE('',#38193,#38192,#31242,.T.);
#47589=EDGE_CURVE('',#38193,#38188,#20671,.T.);
#47590=EDGE_CURVE('',#38191,#38194,#20672,.T.);
#47591=EDGE_CURVE('',#38194,#38195,#31243,.T.);
#47592=EDGE_CURVE('',#38195,#38192,#20673,.T.);
#47593=EDGE_CURVE('',#37203,#38177,#31244,.T.);
#47594=EDGE_CURVE('',#38176,#37204,#31245,.T.);
#47595=EDGE_CURVE('',#38194,#37012,#524,.T.);
#47596=EDGE_CURVE('',#37011,#38195,#525,.T.);
#47597=EDGE_CURVE('',#38186,#38189,#526,.T.);
#47598=EDGE_CURVE('',#38188,#38187,#527,.T.);
#47599=EDGE_CURVE('',#38182,#38185,#528,.T.);
#47600=EDGE_CURVE('',#38184,#38183,#529,.T.);
#47601=EDGE_CURVE('',#38196,#38197,#31246,.T.);
#47602=EDGE_CURVE('',#38197,#38198,#20674,.T.);
#47603=EDGE_CURVE('',#38199,#38198,#31247,.T.);
#47604=EDGE_CURVE('',#38200,#38199,#31248,.T.);
#47605=EDGE_CURVE('',#38201,#38200,#31249,.T.);
#47606=EDGE_CURVE('',#38201,#38196,#20675,.T.);
#47607=EDGE_CURVE('',#38199,#38202,#20676,.T.);
#47608=EDGE_CURVE('',#38202,#38203,#31250,.T.);
#47609=EDGE_CURVE('',#38203,#38200,#20677,.T.);
#47610=EDGE_CURVE('',#38204,#38205,#31251,.T.);
#47611=EDGE_CURVE('',#38205,#38206,#20678,.T.);
#47612=EDGE_CURVE('',#38206,#38207,#31252,.T.);
#47613=EDGE_CURVE('',#38207,#38204,#20679,.T.);
#47614=EDGE_CURVE('',#38208,#38209,#31253,.T.);
#47615=EDGE_CURVE('',#38209,#38210,#20680,.T.);
#47616=EDGE_CURVE('',#38211,#38210,#31254,.T.);
#47617=EDGE_CURVE('',#38212,#38211,#31255,.T.);
#47618=EDGE_CURVE('',#38213,#38212,#31256,.T.);
#47619=EDGE_CURVE('',#38213,#38208,#20681,.T.);
#47620=EDGE_CURVE('',#38211,#38214,#20682,.T.);
#47621=EDGE_CURVE('',#38214,#38215,#31257,.T.);
#47622=EDGE_CURVE('',#38215,#38212,#20683,.T.);
#47623=EDGE_CURVE('',#37209,#38197,#31258,.T.);
#47624=EDGE_CURVE('',#38196,#37210,#31259,.T.);
#47625=EDGE_CURVE('',#38214,#37006,#530,.T.);
#47626=EDGE_CURVE('',#37005,#38215,#531,.T.);
#47627=EDGE_CURVE('',#38206,#38209,#532,.T.);
#47628=EDGE_CURVE('',#38208,#38207,#533,.T.);
#47629=EDGE_CURVE('',#38202,#38205,#534,.T.);
#47630=EDGE_CURVE('',#38204,#38203,#535,.T.);
#47631=EDGE_CURVE('',#38216,#38217,#31260,.T.);
#47632=EDGE_CURVE('',#38217,#38218,#20684,.T.);
#47633=EDGE_CURVE('',#38219,#38218,#31261,.T.);
#47634=EDGE_CURVE('',#38220,#38219,#31262,.T.);
#47635=EDGE_CURVE('',#38221,#38220,#31263,.T.);
#47636=EDGE_CURVE('',#38221,#38216,#20685,.T.);
#47637=EDGE_CURVE('',#38219,#38222,#20686,.T.);
#47638=EDGE_CURVE('',#38222,#38223,#31264,.T.);
#47639=EDGE_CURVE('',#38223,#38220,#20687,.T.);
#47640=EDGE_CURVE('',#38224,#38225,#31265,.T.);
#47641=EDGE_CURVE('',#38225,#38226,#20688,.T.);
#47642=EDGE_CURVE('',#38226,#38227,#31266,.T.);
#47643=EDGE_CURVE('',#38227,#38224,#20689,.T.);
#47644=EDGE_CURVE('',#38228,#38229,#31267,.T.);
#47645=EDGE_CURVE('',#38229,#38230,#20690,.T.);
#47646=EDGE_CURVE('',#38231,#38230,#31268,.T.);
#47647=EDGE_CURVE('',#38232,#38231,#31269,.T.);
#47648=EDGE_CURVE('',#38233,#38232,#31270,.T.);
#47649=EDGE_CURVE('',#38233,#38228,#20691,.T.);
#47650=EDGE_CURVE('',#38231,#38234,#20692,.T.);
#47651=EDGE_CURVE('',#38234,#38235,#31271,.T.);
#47652=EDGE_CURVE('',#38235,#38232,#20693,.T.);
#47653=EDGE_CURVE('',#37215,#38217,#31272,.T.);
#47654=EDGE_CURVE('',#38216,#37216,#31273,.T.);
#47655=EDGE_CURVE('',#38234,#37000,#536,.T.);
#47656=EDGE_CURVE('',#36999,#38235,#537,.T.);
#47657=EDGE_CURVE('',#38226,#38229,#538,.T.);
#47658=EDGE_CURVE('',#38228,#38227,#539,.T.);
#47659=EDGE_CURVE('',#38222,#38225,#540,.T.);
#47660=EDGE_CURVE('',#38224,#38223,#541,.T.);
#47661=EDGE_CURVE('',#38236,#38237,#31274,.T.);
#47662=EDGE_CURVE('',#38237,#38238,#20694,.T.);
#47663=EDGE_CURVE('',#38239,#38238,#31275,.T.);
#47664=EDGE_CURVE('',#38240,#38239,#31276,.T.);
#47665=EDGE_CURVE('',#38241,#38240,#31277,.T.);
#47666=EDGE_CURVE('',#38241,#38236,#20695,.T.);
#47667=EDGE_CURVE('',#38239,#38242,#20696,.T.);
#47668=EDGE_CURVE('',#38242,#38243,#31278,.T.);
#47669=EDGE_CURVE('',#38243,#38240,#20697,.T.);
#47670=EDGE_CURVE('',#38244,#38245,#31279,.T.);
#47671=EDGE_CURVE('',#38245,#38246,#20698,.T.);
#47672=EDGE_CURVE('',#38246,#38247,#31280,.T.);
#47673=EDGE_CURVE('',#38247,#38244,#20699,.T.);
#47674=EDGE_CURVE('',#38248,#38249,#31281,.T.);
#47675=EDGE_CURVE('',#38249,#38250,#20700,.T.);
#47676=EDGE_CURVE('',#38251,#38250,#31282,.T.);
#47677=EDGE_CURVE('',#38252,#38251,#31283,.T.);
#47678=EDGE_CURVE('',#38253,#38252,#31284,.T.);
#47679=EDGE_CURVE('',#38253,#38248,#20701,.T.);
#47680=EDGE_CURVE('',#38251,#38254,#20702,.T.);
#47681=EDGE_CURVE('',#38254,#38255,#31285,.T.);
#47682=EDGE_CURVE('',#38255,#38252,#20703,.T.);
#47683=EDGE_CURVE('',#37221,#38237,#31286,.T.);
#47684=EDGE_CURVE('',#38236,#37222,#31287,.T.);
#47685=EDGE_CURVE('',#38254,#36994,#542,.T.);
#47686=EDGE_CURVE('',#36993,#38255,#543,.T.);
#47687=EDGE_CURVE('',#38246,#38249,#544,.T.);
#47688=EDGE_CURVE('',#38248,#38247,#545,.T.);
#47689=EDGE_CURVE('',#38242,#38245,#546,.T.);
#47690=EDGE_CURVE('',#38244,#38243,#547,.T.);
#47691=EDGE_CURVE('',#38256,#38257,#31288,.T.);
#47692=EDGE_CURVE('',#38257,#38258,#20704,.T.);
#47693=EDGE_CURVE('',#38259,#38258,#31289,.T.);
#47694=EDGE_CURVE('',#38260,#38259,#31290,.T.);
#47695=EDGE_CURVE('',#38261,#38260,#31291,.T.);
#47696=EDGE_CURVE('',#38261,#38256,#20705,.T.);
#47697=EDGE_CURVE('',#38259,#38262,#20706,.T.);
#47698=EDGE_CURVE('',#38262,#38263,#31292,.T.);
#47699=EDGE_CURVE('',#38263,#38260,#20707,.T.);
#47700=EDGE_CURVE('',#38264,#38265,#31293,.T.);
#47701=EDGE_CURVE('',#38265,#38266,#20708,.T.);
#47702=EDGE_CURVE('',#38266,#38267,#31294,.T.);
#47703=EDGE_CURVE('',#38267,#38264,#20709,.T.);
#47704=EDGE_CURVE('',#38268,#38269,#31295,.T.);
#47705=EDGE_CURVE('',#38269,#38270,#20710,.T.);
#47706=EDGE_CURVE('',#38271,#38270,#31296,.T.);
#47707=EDGE_CURVE('',#38272,#38271,#31297,.T.);
#47708=EDGE_CURVE('',#38273,#38272,#31298,.T.);
#47709=EDGE_CURVE('',#38273,#38268,#20711,.T.);
#47710=EDGE_CURVE('',#38271,#38274,#20712,.T.);
#47711=EDGE_CURVE('',#38274,#38275,#31299,.T.);
#47712=EDGE_CURVE('',#38275,#38272,#20713,.T.);
#47713=EDGE_CURVE('',#37227,#38257,#31300,.T.);
#47714=EDGE_CURVE('',#38256,#37228,#31301,.T.);
#47715=EDGE_CURVE('',#38274,#36988,#548,.T.);
#47716=EDGE_CURVE('',#36987,#38275,#549,.T.);
#47717=EDGE_CURVE('',#38266,#38269,#550,.T.);
#47718=EDGE_CURVE('',#38268,#38267,#551,.T.);
#47719=EDGE_CURVE('',#38262,#38265,#552,.T.);
#47720=EDGE_CURVE('',#38264,#38263,#553,.T.);
#47721=EDGE_CURVE('',#38276,#38277,#31302,.T.);
#47722=EDGE_CURVE('',#38277,#38278,#20714,.T.);
#47723=EDGE_CURVE('',#38279,#38278,#31303,.T.);
#47724=EDGE_CURVE('',#38280,#38279,#31304,.T.);
#47725=EDGE_CURVE('',#38281,#38280,#31305,.T.);
#47726=EDGE_CURVE('',#38281,#38276,#20715,.T.);
#47727=EDGE_CURVE('',#38279,#38282,#20716,.T.);
#47728=EDGE_CURVE('',#38282,#38283,#31306,.T.);
#47729=EDGE_CURVE('',#38283,#38280,#20717,.T.);
#47730=EDGE_CURVE('',#38284,#38285,#31307,.T.);
#47731=EDGE_CURVE('',#38285,#38286,#20718,.T.);
#47732=EDGE_CURVE('',#38286,#38287,#31308,.T.);
#47733=EDGE_CURVE('',#38287,#38284,#20719,.T.);
#47734=EDGE_CURVE('',#38288,#38289,#31309,.T.);
#47735=EDGE_CURVE('',#38289,#38290,#20720,.T.);
#47736=EDGE_CURVE('',#38291,#38290,#31310,.T.);
#47737=EDGE_CURVE('',#38292,#38291,#31311,.T.);
#47738=EDGE_CURVE('',#38293,#38292,#31312,.T.);
#47739=EDGE_CURVE('',#38293,#38288,#20721,.T.);
#47740=EDGE_CURVE('',#38291,#38294,#20722,.T.);
#47741=EDGE_CURVE('',#38294,#38295,#31313,.T.);
#47742=EDGE_CURVE('',#38295,#38292,#20723,.T.);
#47743=EDGE_CURVE('',#37233,#38277,#31314,.T.);
#47744=EDGE_CURVE('',#38276,#37234,#31315,.T.);
#47745=EDGE_CURVE('',#38294,#36982,#554,.T.);
#47746=EDGE_CURVE('',#36981,#38295,#555,.T.);
#47747=EDGE_CURVE('',#38286,#38289,#556,.T.);
#47748=EDGE_CURVE('',#38288,#38287,#557,.T.);
#47749=EDGE_CURVE('',#38282,#38285,#558,.T.);
#47750=EDGE_CURVE('',#38284,#38283,#559,.T.);
#47751=EDGE_CURVE('',#38296,#38297,#31316,.T.);
#47752=EDGE_CURVE('',#38297,#38298,#20724,.T.);
#47753=EDGE_CURVE('',#38299,#38298,#31317,.T.);
#47754=EDGE_CURVE('',#38300,#38299,#31318,.T.);
#47755=EDGE_CURVE('',#38301,#38300,#31319,.T.);
#47756=EDGE_CURVE('',#38301,#38296,#20725,.T.);
#47757=EDGE_CURVE('',#38299,#38302,#20726,.T.);
#47758=EDGE_CURVE('',#38302,#38303,#31320,.T.);
#47759=EDGE_CURVE('',#38303,#38300,#20727,.T.);
#47760=EDGE_CURVE('',#38304,#38305,#31321,.T.);
#47761=EDGE_CURVE('',#38305,#38306,#20728,.T.);
#47762=EDGE_CURVE('',#38306,#38307,#31322,.T.);
#47763=EDGE_CURVE('',#38307,#38304,#20729,.T.);
#47764=EDGE_CURVE('',#38308,#38309,#31323,.T.);
#47765=EDGE_CURVE('',#38309,#38310,#20730,.T.);
#47766=EDGE_CURVE('',#38311,#38310,#31324,.T.);
#47767=EDGE_CURVE('',#38312,#38311,#31325,.T.);
#47768=EDGE_CURVE('',#38313,#38312,#31326,.T.);
#47769=EDGE_CURVE('',#38313,#38308,#20731,.T.);
#47770=EDGE_CURVE('',#38311,#38314,#20732,.T.);
#47771=EDGE_CURVE('',#38314,#38315,#31327,.T.);
#47772=EDGE_CURVE('',#38315,#38312,#20733,.T.);
#47773=EDGE_CURVE('',#37239,#38297,#31328,.T.);
#47774=EDGE_CURVE('',#38296,#37240,#31329,.T.);
#47775=EDGE_CURVE('',#38314,#36976,#560,.T.);
#47776=EDGE_CURVE('',#36975,#38315,#561,.T.);
#47777=EDGE_CURVE('',#38306,#38309,#562,.T.);
#47778=EDGE_CURVE('',#38308,#38307,#563,.T.);
#47779=EDGE_CURVE('',#38302,#38305,#564,.T.);
#47780=EDGE_CURVE('',#38304,#38303,#565,.T.);
#47781=EDGE_CURVE('',#38316,#38317,#31330,.T.);
#47782=EDGE_CURVE('',#38317,#38318,#20734,.T.);
#47783=EDGE_CURVE('',#38319,#38318,#31331,.T.);
#47784=EDGE_CURVE('',#38320,#38319,#31332,.T.);
#47785=EDGE_CURVE('',#38321,#38320,#31333,.T.);
#47786=EDGE_CURVE('',#38321,#38316,#20735,.T.);
#47787=EDGE_CURVE('',#38319,#38322,#20736,.T.);
#47788=EDGE_CURVE('',#38322,#38323,#31334,.T.);
#47789=EDGE_CURVE('',#38323,#38320,#20737,.T.);
#47790=EDGE_CURVE('',#38324,#38325,#31335,.T.);
#47791=EDGE_CURVE('',#38325,#38326,#20738,.T.);
#47792=EDGE_CURVE('',#38326,#38327,#31336,.T.);
#47793=EDGE_CURVE('',#38327,#38324,#20739,.T.);
#47794=EDGE_CURVE('',#38328,#38329,#31337,.T.);
#47795=EDGE_CURVE('',#38329,#38330,#20740,.T.);
#47796=EDGE_CURVE('',#38331,#38330,#31338,.T.);
#47797=EDGE_CURVE('',#38332,#38331,#31339,.T.);
#47798=EDGE_CURVE('',#38333,#38332,#31340,.T.);
#47799=EDGE_CURVE('',#38333,#38328,#20741,.T.);
#47800=EDGE_CURVE('',#38331,#38334,#20742,.T.);
#47801=EDGE_CURVE('',#38334,#38335,#31341,.T.);
#47802=EDGE_CURVE('',#38335,#38332,#20743,.T.);
#47803=EDGE_CURVE('',#37245,#38317,#31342,.T.);
#47804=EDGE_CURVE('',#38316,#37246,#31343,.T.);
#47805=EDGE_CURVE('',#38334,#36970,#566,.T.);
#47806=EDGE_CURVE('',#36969,#38335,#567,.T.);
#47807=EDGE_CURVE('',#38326,#38329,#568,.T.);
#47808=EDGE_CURVE('',#38328,#38327,#569,.T.);
#47809=EDGE_CURVE('',#38322,#38325,#570,.T.);
#47810=EDGE_CURVE('',#38324,#38323,#571,.T.);
#47811=EDGE_CURVE('',#38336,#38337,#31344,.T.);
#47812=EDGE_CURVE('',#38337,#38338,#20744,.T.);
#47813=EDGE_CURVE('',#38339,#38338,#31345,.T.);
#47814=EDGE_CURVE('',#38340,#38339,#31346,.T.);
#47815=EDGE_CURVE('',#38341,#38340,#31347,.T.);
#47816=EDGE_CURVE('',#38341,#38336,#20745,.T.);
#47817=EDGE_CURVE('',#38339,#38342,#20746,.T.);
#47818=EDGE_CURVE('',#38342,#38343,#31348,.T.);
#47819=EDGE_CURVE('',#38343,#38340,#20747,.T.);
#47820=EDGE_CURVE('',#38344,#38345,#31349,.T.);
#47821=EDGE_CURVE('',#38345,#38346,#20748,.T.);
#47822=EDGE_CURVE('',#38346,#38347,#31350,.T.);
#47823=EDGE_CURVE('',#38347,#38344,#20749,.T.);
#47824=EDGE_CURVE('',#38348,#38349,#31351,.T.);
#47825=EDGE_CURVE('',#38349,#38350,#20750,.T.);
#47826=EDGE_CURVE('',#38351,#38350,#31352,.T.);
#47827=EDGE_CURVE('',#38352,#38351,#31353,.T.);
#47828=EDGE_CURVE('',#38353,#38352,#31354,.T.);
#47829=EDGE_CURVE('',#38353,#38348,#20751,.T.);
#47830=EDGE_CURVE('',#38351,#38354,#20752,.T.);
#47831=EDGE_CURVE('',#38354,#38355,#31355,.T.);
#47832=EDGE_CURVE('',#38355,#38352,#20753,.T.);
#47833=EDGE_CURVE('',#37251,#38337,#31356,.T.);
#47834=EDGE_CURVE('',#38336,#37252,#31357,.T.);
#47835=EDGE_CURVE('',#38354,#36964,#572,.T.);
#47836=EDGE_CURVE('',#36963,#38355,#573,.T.);
#47837=EDGE_CURVE('',#38346,#38349,#574,.T.);
#47838=EDGE_CURVE('',#38348,#38347,#575,.T.);
#47839=EDGE_CURVE('',#38342,#38345,#576,.T.);
#47840=EDGE_CURVE('',#38344,#38343,#577,.T.);
#47841=EDGE_CURVE('',#38356,#38357,#31358,.T.);
#47842=EDGE_CURVE('',#38357,#38358,#20754,.T.);
#47843=EDGE_CURVE('',#38359,#38358,#31359,.T.);
#47844=EDGE_CURVE('',#38360,#38359,#31360,.T.);
#47845=EDGE_CURVE('',#38361,#38360,#31361,.T.);
#47846=EDGE_CURVE('',#38361,#38356,#20755,.T.);
#47847=EDGE_CURVE('',#38359,#38362,#20756,.T.);
#47848=EDGE_CURVE('',#38362,#38363,#31362,.T.);
#47849=EDGE_CURVE('',#38363,#38360,#20757,.T.);
#47850=EDGE_CURVE('',#38364,#38365,#31363,.T.);
#47851=EDGE_CURVE('',#38365,#38366,#20758,.T.);
#47852=EDGE_CURVE('',#38366,#38367,#31364,.T.);
#47853=EDGE_CURVE('',#38367,#38364,#20759,.T.);
#47854=EDGE_CURVE('',#38368,#38369,#31365,.T.);
#47855=EDGE_CURVE('',#38369,#38370,#20760,.T.);
#47856=EDGE_CURVE('',#38371,#38370,#31366,.T.);
#47857=EDGE_CURVE('',#38372,#38371,#31367,.T.);
#47858=EDGE_CURVE('',#38373,#38372,#31368,.T.);
#47859=EDGE_CURVE('',#38373,#38368,#20761,.T.);
#47860=EDGE_CURVE('',#38371,#38374,#20762,.T.);
#47861=EDGE_CURVE('',#38374,#38375,#31369,.T.);
#47862=EDGE_CURVE('',#38375,#38372,#20763,.T.);
#47863=EDGE_CURVE('',#37257,#38357,#31370,.T.);
#47864=EDGE_CURVE('',#38356,#37258,#31371,.T.);
#47865=EDGE_CURVE('',#38374,#36958,#578,.T.);
#47866=EDGE_CURVE('',#36957,#38375,#579,.T.);
#47867=EDGE_CURVE('',#38366,#38369,#580,.T.);
#47868=EDGE_CURVE('',#38368,#38367,#581,.T.);
#47869=EDGE_CURVE('',#38362,#38365,#582,.T.);
#47870=EDGE_CURVE('',#38364,#38363,#583,.T.);
#47871=EDGE_CURVE('',#38376,#38377,#31372,.T.);
#47872=EDGE_CURVE('',#38377,#38378,#20764,.T.);
#47873=EDGE_CURVE('',#38379,#38378,#31373,.T.);
#47874=EDGE_CURVE('',#38380,#38379,#31374,.T.);
#47875=EDGE_CURVE('',#38381,#38380,#31375,.T.);
#47876=EDGE_CURVE('',#38381,#38376,#20765,.T.);
#47877=EDGE_CURVE('',#38379,#38382,#20766,.T.);
#47878=EDGE_CURVE('',#38382,#38383,#31376,.T.);
#47879=EDGE_CURVE('',#38383,#38380,#20767,.T.);
#47880=EDGE_CURVE('',#38384,#38385,#31377,.T.);
#47881=EDGE_CURVE('',#38385,#38386,#20768,.T.);
#47882=EDGE_CURVE('',#38386,#38387,#31378,.T.);
#47883=EDGE_CURVE('',#38387,#38384,#20769,.T.);
#47884=EDGE_CURVE('',#38388,#38389,#31379,.T.);
#47885=EDGE_CURVE('',#38389,#38390,#20770,.T.);
#47886=EDGE_CURVE('',#38391,#38390,#31380,.T.);
#47887=EDGE_CURVE('',#38392,#38391,#31381,.T.);
#47888=EDGE_CURVE('',#38393,#38392,#31382,.T.);
#47889=EDGE_CURVE('',#38393,#38388,#20771,.T.);
#47890=EDGE_CURVE('',#38391,#38394,#20772,.T.);
#47891=EDGE_CURVE('',#38394,#38395,#31383,.T.);
#47892=EDGE_CURVE('',#38395,#38392,#20773,.T.);
#47893=EDGE_CURVE('',#37263,#38377,#31384,.T.);
#47894=EDGE_CURVE('',#38376,#37264,#31385,.T.);
#47895=EDGE_CURVE('',#38394,#36952,#584,.T.);
#47896=EDGE_CURVE('',#36951,#38395,#585,.T.);
#47897=EDGE_CURVE('',#38386,#38389,#586,.T.);
#47898=EDGE_CURVE('',#38388,#38387,#587,.T.);
#47899=EDGE_CURVE('',#38382,#38385,#588,.T.);
#47900=EDGE_CURVE('',#38384,#38383,#589,.T.);
#47901=EDGE_CURVE('',#38396,#38397,#31386,.T.);
#47902=EDGE_CURVE('',#38397,#38398,#20774,.T.);
#47903=EDGE_CURVE('',#38399,#38398,#31387,.T.);
#47904=EDGE_CURVE('',#38400,#38399,#31388,.T.);
#47905=EDGE_CURVE('',#38401,#38400,#31389,.T.);
#47906=EDGE_CURVE('',#38401,#38396,#20775,.T.);
#47907=EDGE_CURVE('',#38399,#38402,#20776,.T.);
#47908=EDGE_CURVE('',#38402,#38403,#31390,.T.);
#47909=EDGE_CURVE('',#38403,#38400,#20777,.T.);
#47910=EDGE_CURVE('',#38404,#38405,#31391,.T.);
#47911=EDGE_CURVE('',#38405,#38406,#20778,.T.);
#47912=EDGE_CURVE('',#38406,#38407,#31392,.T.);
#47913=EDGE_CURVE('',#38407,#38404,#20779,.T.);
#47914=EDGE_CURVE('',#38408,#38409,#31393,.T.);
#47915=EDGE_CURVE('',#38409,#38410,#20780,.T.);
#47916=EDGE_CURVE('',#38411,#38410,#31394,.T.);
#47917=EDGE_CURVE('',#38412,#38411,#31395,.T.);
#47918=EDGE_CURVE('',#38413,#38412,#31396,.T.);
#47919=EDGE_CURVE('',#38413,#38408,#20781,.T.);
#47920=EDGE_CURVE('',#38411,#38414,#20782,.T.);
#47921=EDGE_CURVE('',#38414,#38415,#31397,.T.);
#47922=EDGE_CURVE('',#38415,#38412,#20783,.T.);
#47923=EDGE_CURVE('',#37269,#38397,#31398,.T.);
#47924=EDGE_CURVE('',#38396,#37270,#31399,.T.);
#47925=EDGE_CURVE('',#38414,#36946,#590,.T.);
#47926=EDGE_CURVE('',#36945,#38415,#591,.T.);
#47927=EDGE_CURVE('',#38406,#38409,#592,.T.);
#47928=EDGE_CURVE('',#38408,#38407,#593,.T.);
#47929=EDGE_CURVE('',#38402,#38405,#594,.T.);
#47930=EDGE_CURVE('',#38404,#38403,#595,.T.);
#47931=EDGE_CURVE('',#38416,#38417,#31400,.T.);
#47932=EDGE_CURVE('',#38417,#38418,#20784,.T.);
#47933=EDGE_CURVE('',#38419,#38418,#31401,.T.);
#47934=EDGE_CURVE('',#38420,#38419,#31402,.T.);
#47935=EDGE_CURVE('',#38421,#38420,#31403,.T.);
#47936=EDGE_CURVE('',#38421,#38416,#20785,.T.);
#47937=EDGE_CURVE('',#38419,#38422,#20786,.T.);
#47938=EDGE_CURVE('',#38422,#38423,#31404,.T.);
#47939=EDGE_CURVE('',#38423,#38420,#20787,.T.);
#47940=EDGE_CURVE('',#38424,#38425,#31405,.T.);
#47941=EDGE_CURVE('',#38425,#38426,#20788,.T.);
#47942=EDGE_CURVE('',#38426,#38427,#31406,.T.);
#47943=EDGE_CURVE('',#38427,#38424,#20789,.T.);
#47944=EDGE_CURVE('',#38428,#38429,#31407,.T.);
#47945=EDGE_CURVE('',#38429,#38430,#20790,.T.);
#47946=EDGE_CURVE('',#38431,#38430,#31408,.T.);
#47947=EDGE_CURVE('',#38432,#38431,#31409,.T.);
#47948=EDGE_CURVE('',#38433,#38432,#31410,.T.);
#47949=EDGE_CURVE('',#38433,#38428,#20791,.T.);
#47950=EDGE_CURVE('',#38431,#38434,#20792,.T.);
#47951=EDGE_CURVE('',#38434,#38435,#31411,.T.);
#47952=EDGE_CURVE('',#38435,#38432,#20793,.T.);
#47953=EDGE_CURVE('',#37275,#38417,#31412,.T.);
#47954=EDGE_CURVE('',#38416,#37276,#31413,.T.);
#47955=EDGE_CURVE('',#38434,#36940,#596,.T.);
#47956=EDGE_CURVE('',#36939,#38435,#597,.T.);
#47957=EDGE_CURVE('',#38426,#38429,#598,.T.);
#47958=EDGE_CURVE('',#38428,#38427,#599,.T.);
#47959=EDGE_CURVE('',#38422,#38425,#600,.T.);
#47960=EDGE_CURVE('',#38424,#38423,#601,.T.);
#47961=EDGE_CURVE('',#38436,#38437,#31414,.T.);
#47962=EDGE_CURVE('',#38437,#38438,#20794,.T.);
#47963=EDGE_CURVE('',#38439,#38438,#31415,.T.);
#47964=EDGE_CURVE('',#38440,#38439,#31416,.T.);
#47965=EDGE_CURVE('',#38441,#38440,#31417,.T.);
#47966=EDGE_CURVE('',#38441,#38436,#20795,.T.);
#47967=EDGE_CURVE('',#38439,#38442,#20796,.T.);
#47968=EDGE_CURVE('',#38442,#38443,#31418,.T.);
#47969=EDGE_CURVE('',#38443,#38440,#20797,.T.);
#47970=EDGE_CURVE('',#38444,#38445,#31419,.T.);
#47971=EDGE_CURVE('',#38445,#38446,#20798,.T.);
#47972=EDGE_CURVE('',#38446,#38447,#31420,.T.);
#47973=EDGE_CURVE('',#38447,#38444,#20799,.T.);
#47974=EDGE_CURVE('',#38448,#38449,#31421,.T.);
#47975=EDGE_CURVE('',#38449,#38450,#20800,.T.);
#47976=EDGE_CURVE('',#38451,#38450,#31422,.T.);
#47977=EDGE_CURVE('',#38452,#38451,#31423,.T.);
#47978=EDGE_CURVE('',#38453,#38452,#31424,.T.);
#47979=EDGE_CURVE('',#38453,#38448,#20801,.T.);
#47980=EDGE_CURVE('',#38451,#38454,#20802,.T.);
#47981=EDGE_CURVE('',#38454,#38455,#31425,.T.);
#47982=EDGE_CURVE('',#38455,#38452,#20803,.T.);
#47983=EDGE_CURVE('',#37281,#38437,#31426,.T.);
#47984=EDGE_CURVE('',#38436,#37282,#31427,.T.);
#47985=EDGE_CURVE('',#38454,#36934,#602,.T.);
#47986=EDGE_CURVE('',#36933,#38455,#603,.T.);
#47987=EDGE_CURVE('',#38446,#38449,#604,.T.);
#47988=EDGE_CURVE('',#38448,#38447,#605,.T.);
#47989=EDGE_CURVE('',#38442,#38445,#606,.T.);
#47990=EDGE_CURVE('',#38444,#38443,#607,.T.);
#47991=EDGE_CURVE('',#38456,#38457,#31428,.T.);
#47992=EDGE_CURVE('',#38457,#38458,#20804,.T.);
#47993=EDGE_CURVE('',#38459,#38458,#31429,.T.);
#47994=EDGE_CURVE('',#38460,#38459,#31430,.T.);
#47995=EDGE_CURVE('',#38461,#38460,#31431,.T.);
#47996=EDGE_CURVE('',#38461,#38456,#20805,.T.);
#47997=EDGE_CURVE('',#38459,#38462,#20806,.T.);
#47998=EDGE_CURVE('',#38462,#38463,#31432,.T.);
#47999=EDGE_CURVE('',#38463,#38460,#20807,.T.);
#48000=EDGE_CURVE('',#38464,#38465,#31433,.T.);
#48001=EDGE_CURVE('',#38465,#38466,#20808,.T.);
#48002=EDGE_CURVE('',#38466,#38467,#31434,.T.);
#48003=EDGE_CURVE('',#38467,#38464,#20809,.T.);
#48004=EDGE_CURVE('',#38468,#38469,#31435,.T.);
#48005=EDGE_CURVE('',#38469,#38470,#20810,.T.);
#48006=EDGE_CURVE('',#38471,#38470,#31436,.T.);
#48007=EDGE_CURVE('',#38472,#38471,#31437,.T.);
#48008=EDGE_CURVE('',#38473,#38472,#31438,.T.);
#48009=EDGE_CURVE('',#38473,#38468,#20811,.T.);
#48010=EDGE_CURVE('',#38471,#38474,#20812,.T.);
#48011=EDGE_CURVE('',#38474,#38475,#31439,.T.);
#48012=EDGE_CURVE('',#38475,#38472,#20813,.T.);
#48013=EDGE_CURVE('',#37287,#38457,#31440,.T.);
#48014=EDGE_CURVE('',#38456,#37288,#31441,.T.);
#48015=EDGE_CURVE('',#38474,#36928,#608,.T.);
#48016=EDGE_CURVE('',#36927,#38475,#609,.T.);
#48017=EDGE_CURVE('',#38466,#38469,#610,.T.);
#48018=EDGE_CURVE('',#38468,#38467,#611,.T.);
#48019=EDGE_CURVE('',#38462,#38465,#612,.T.);
#48020=EDGE_CURVE('',#38464,#38463,#613,.T.);
#48021=EDGE_CURVE('',#38476,#38477,#31442,.T.);
#48022=EDGE_CURVE('',#38477,#38478,#20814,.T.);
#48023=EDGE_CURVE('',#38479,#38478,#31443,.T.);
#48024=EDGE_CURVE('',#38480,#38479,#31444,.T.);
#48025=EDGE_CURVE('',#38481,#38480,#31445,.T.);
#48026=EDGE_CURVE('',#38481,#38476,#20815,.T.);
#48027=EDGE_CURVE('',#38479,#38482,#20816,.T.);
#48028=EDGE_CURVE('',#38482,#38483,#31446,.T.);
#48029=EDGE_CURVE('',#38483,#38480,#20817,.T.);
#48030=EDGE_CURVE('',#38484,#38485,#31447,.T.);
#48031=EDGE_CURVE('',#38485,#38486,#20818,.T.);
#48032=EDGE_CURVE('',#38486,#38487,#31448,.T.);
#48033=EDGE_CURVE('',#38487,#38484,#20819,.T.);
#48034=EDGE_CURVE('',#38488,#38489,#31449,.T.);
#48035=EDGE_CURVE('',#38489,#38490,#20820,.T.);
#48036=EDGE_CURVE('',#38491,#38490,#31450,.T.);
#48037=EDGE_CURVE('',#38492,#38491,#31451,.T.);
#48038=EDGE_CURVE('',#38493,#38492,#31452,.T.);
#48039=EDGE_CURVE('',#38493,#38488,#20821,.T.);
#48040=EDGE_CURVE('',#38491,#38494,#20822,.T.);
#48041=EDGE_CURVE('',#38494,#38495,#31453,.T.);
#48042=EDGE_CURVE('',#38495,#38492,#20823,.T.);
#48043=EDGE_CURVE('',#37293,#38477,#31454,.T.);
#48044=EDGE_CURVE('',#38476,#37294,#31455,.T.);
#48045=EDGE_CURVE('',#38494,#36922,#614,.T.);
#48046=EDGE_CURVE('',#36921,#38495,#615,.T.);
#48047=EDGE_CURVE('',#38486,#38489,#616,.T.);
#48048=EDGE_CURVE('',#38488,#38487,#617,.T.);
#48049=EDGE_CURVE('',#38482,#38485,#618,.T.);
#48050=EDGE_CURVE('',#38484,#38483,#619,.T.);
#48051=EDGE_CURVE('',#38496,#38497,#31456,.T.);
#48052=EDGE_CURVE('',#38497,#38498,#20824,.T.);
#48053=EDGE_CURVE('',#38499,#38498,#31457,.T.);
#48054=EDGE_CURVE('',#38500,#38499,#31458,.T.);
#48055=EDGE_CURVE('',#38501,#38500,#31459,.T.);
#48056=EDGE_CURVE('',#38501,#38496,#20825,.T.);
#48057=EDGE_CURVE('',#38499,#38502,#20826,.T.);
#48058=EDGE_CURVE('',#38502,#38503,#31460,.T.);
#48059=EDGE_CURVE('',#38503,#38500,#20827,.T.);
#48060=EDGE_CURVE('',#38504,#38505,#31461,.T.);
#48061=EDGE_CURVE('',#38505,#38506,#20828,.T.);
#48062=EDGE_CURVE('',#38506,#38507,#31462,.T.);
#48063=EDGE_CURVE('',#38507,#38504,#20829,.T.);
#48064=EDGE_CURVE('',#38508,#38509,#31463,.T.);
#48065=EDGE_CURVE('',#38509,#38510,#20830,.T.);
#48066=EDGE_CURVE('',#38511,#38510,#31464,.T.);
#48067=EDGE_CURVE('',#38512,#38511,#31465,.T.);
#48068=EDGE_CURVE('',#38513,#38512,#31466,.T.);
#48069=EDGE_CURVE('',#38513,#38508,#20831,.T.);
#48070=EDGE_CURVE('',#38511,#38514,#20832,.T.);
#48071=EDGE_CURVE('',#38514,#38515,#31467,.T.);
#48072=EDGE_CURVE('',#38515,#38512,#20833,.T.);
#48073=EDGE_CURVE('',#37299,#38497,#31468,.T.);
#48074=EDGE_CURVE('',#38496,#37300,#31469,.T.);
#48075=EDGE_CURVE('',#38514,#36916,#620,.T.);
#48076=EDGE_CURVE('',#36915,#38515,#621,.T.);
#48077=EDGE_CURVE('',#38506,#38509,#622,.T.);
#48078=EDGE_CURVE('',#38508,#38507,#623,.T.);
#48079=EDGE_CURVE('',#38502,#38505,#624,.T.);
#48080=EDGE_CURVE('',#38504,#38503,#625,.T.);
#48081=EDGE_CURVE('',#38516,#38517,#31470,.T.);
#48082=EDGE_CURVE('',#38517,#38518,#20834,.T.);
#48083=EDGE_CURVE('',#38519,#38518,#31471,.T.);
#48084=EDGE_CURVE('',#38520,#38519,#31472,.T.);
#48085=EDGE_CURVE('',#38521,#38520,#31473,.T.);
#48086=EDGE_CURVE('',#38521,#38516,#20835,.T.);
#48087=EDGE_CURVE('',#38519,#38522,#20836,.T.);
#48088=EDGE_CURVE('',#38522,#38523,#31474,.T.);
#48089=EDGE_CURVE('',#38523,#38520,#20837,.T.);
#48090=EDGE_CURVE('',#38524,#38525,#31475,.T.);
#48091=EDGE_CURVE('',#38525,#38526,#20838,.T.);
#48092=EDGE_CURVE('',#38526,#38527,#31476,.T.);
#48093=EDGE_CURVE('',#38527,#38524,#20839,.T.);
#48094=EDGE_CURVE('',#38528,#38529,#31477,.T.);
#48095=EDGE_CURVE('',#38529,#38530,#20840,.T.);
#48096=EDGE_CURVE('',#38531,#38530,#31478,.T.);
#48097=EDGE_CURVE('',#38532,#38531,#31479,.T.);
#48098=EDGE_CURVE('',#38533,#38532,#31480,.T.);
#48099=EDGE_CURVE('',#38533,#38528,#20841,.T.);
#48100=EDGE_CURVE('',#38531,#38534,#20842,.T.);
#48101=EDGE_CURVE('',#38534,#38535,#31481,.T.);
#48102=EDGE_CURVE('',#38535,#38532,#20843,.T.);
#48103=EDGE_CURVE('',#37305,#38517,#31482,.T.);
#48104=EDGE_CURVE('',#38516,#37306,#31483,.T.);
#48105=EDGE_CURVE('',#38534,#36910,#626,.T.);
#48106=EDGE_CURVE('',#36909,#38535,#627,.T.);
#48107=EDGE_CURVE('',#38526,#38529,#628,.T.);
#48108=EDGE_CURVE('',#38528,#38527,#629,.T.);
#48109=EDGE_CURVE('',#38522,#38525,#630,.T.);
#48110=EDGE_CURVE('',#38524,#38523,#631,.T.);
#48111=EDGE_CURVE('',#38536,#38537,#31484,.T.);
#48112=EDGE_CURVE('',#38537,#38538,#20844,.T.);
#48113=EDGE_CURVE('',#38539,#38538,#31485,.T.);
#48114=EDGE_CURVE('',#38540,#38539,#31486,.T.);
#48115=EDGE_CURVE('',#38541,#38540,#31487,.T.);
#48116=EDGE_CURVE('',#38541,#38536,#20845,.T.);
#48117=EDGE_CURVE('',#38539,#38542,#20846,.T.);
#48118=EDGE_CURVE('',#38542,#38543,#31488,.T.);
#48119=EDGE_CURVE('',#38543,#38540,#20847,.T.);
#48120=EDGE_CURVE('',#38544,#38545,#31489,.T.);
#48121=EDGE_CURVE('',#38545,#38546,#20848,.T.);
#48122=EDGE_CURVE('',#38546,#38547,#31490,.T.);
#48123=EDGE_CURVE('',#38547,#38544,#20849,.T.);
#48124=EDGE_CURVE('',#38548,#38549,#31491,.T.);
#48125=EDGE_CURVE('',#38549,#38550,#20850,.T.);
#48126=EDGE_CURVE('',#38551,#38550,#31492,.T.);
#48127=EDGE_CURVE('',#38552,#38551,#31493,.T.);
#48128=EDGE_CURVE('',#38553,#38552,#31494,.T.);
#48129=EDGE_CURVE('',#38553,#38548,#20851,.T.);
#48130=EDGE_CURVE('',#38551,#38554,#20852,.T.);
#48131=EDGE_CURVE('',#38554,#38555,#31495,.T.);
#48132=EDGE_CURVE('',#38555,#38552,#20853,.T.);
#48133=EDGE_CURVE('',#37311,#38537,#31496,.T.);
#48134=EDGE_CURVE('',#38536,#37312,#31497,.T.);
#48135=EDGE_CURVE('',#38554,#36904,#632,.T.);
#48136=EDGE_CURVE('',#36903,#38555,#633,.T.);
#48137=EDGE_CURVE('',#38546,#38549,#634,.T.);
#48138=EDGE_CURVE('',#38548,#38547,#635,.T.);
#48139=EDGE_CURVE('',#38542,#38545,#636,.T.);
#48140=EDGE_CURVE('',#38544,#38543,#637,.T.);
#48141=EDGE_CURVE('',#38556,#38557,#31498,.T.);
#48142=EDGE_CURVE('',#38557,#38558,#20854,.T.);
#48143=EDGE_CURVE('',#38559,#38558,#31499,.T.);
#48144=EDGE_CURVE('',#38560,#38559,#31500,.T.);
#48145=EDGE_CURVE('',#38561,#38560,#31501,.T.);
#48146=EDGE_CURVE('',#38561,#38556,#20855,.T.);
#48147=EDGE_CURVE('',#38559,#38562,#20856,.T.);
#48148=EDGE_CURVE('',#38562,#38563,#31502,.T.);
#48149=EDGE_CURVE('',#38563,#38560,#20857,.T.);
#48150=EDGE_CURVE('',#38564,#38565,#31503,.T.);
#48151=EDGE_CURVE('',#38565,#38566,#20858,.T.);
#48152=EDGE_CURVE('',#38566,#38567,#31504,.T.);
#48153=EDGE_CURVE('',#38567,#38564,#20859,.T.);
#48154=EDGE_CURVE('',#38568,#38569,#31505,.T.);
#48155=EDGE_CURVE('',#38569,#38570,#20860,.T.);
#48156=EDGE_CURVE('',#38571,#38570,#31506,.T.);
#48157=EDGE_CURVE('',#38572,#38571,#31507,.T.);
#48158=EDGE_CURVE('',#38573,#38572,#31508,.T.);
#48159=EDGE_CURVE('',#38573,#38568,#20861,.T.);
#48160=EDGE_CURVE('',#38571,#38574,#20862,.T.);
#48161=EDGE_CURVE('',#38574,#38575,#31509,.T.);
#48162=EDGE_CURVE('',#38575,#38572,#20863,.T.);
#48163=EDGE_CURVE('',#37317,#38557,#31510,.T.);
#48164=EDGE_CURVE('',#38556,#37318,#31511,.T.);
#48165=EDGE_CURVE('',#38574,#36898,#638,.T.);
#48166=EDGE_CURVE('',#36897,#38575,#639,.T.);
#48167=EDGE_CURVE('',#38566,#38569,#640,.T.);
#48168=EDGE_CURVE('',#38568,#38567,#641,.T.);
#48169=EDGE_CURVE('',#38562,#38565,#642,.T.);
#48170=EDGE_CURVE('',#38564,#38563,#643,.T.);
#48171=EDGE_CURVE('',#38576,#38577,#31512,.T.);
#48172=EDGE_CURVE('',#38577,#38578,#20864,.T.);
#48173=EDGE_CURVE('',#38579,#38578,#31513,.T.);
#48174=EDGE_CURVE('',#38580,#38579,#31514,.T.);
#48175=EDGE_CURVE('',#38581,#38580,#31515,.T.);
#48176=EDGE_CURVE('',#38581,#38576,#20865,.T.);
#48177=EDGE_CURVE('',#38579,#38582,#20866,.T.);
#48178=EDGE_CURVE('',#38582,#38583,#31516,.T.);
#48179=EDGE_CURVE('',#38583,#38580,#20867,.T.);
#48180=EDGE_CURVE('',#38584,#38585,#31517,.T.);
#48181=EDGE_CURVE('',#38585,#38586,#20868,.T.);
#48182=EDGE_CURVE('',#38586,#38587,#31518,.T.);
#48183=EDGE_CURVE('',#38587,#38584,#20869,.T.);
#48184=EDGE_CURVE('',#38588,#38589,#31519,.T.);
#48185=EDGE_CURVE('',#38589,#38590,#20870,.T.);
#48186=EDGE_CURVE('',#38591,#38590,#31520,.T.);
#48187=EDGE_CURVE('',#38592,#38591,#31521,.T.);
#48188=EDGE_CURVE('',#38593,#38592,#31522,.T.);
#48189=EDGE_CURVE('',#38593,#38588,#20871,.T.);
#48190=EDGE_CURVE('',#38591,#38594,#20872,.T.);
#48191=EDGE_CURVE('',#38594,#38595,#31523,.T.);
#48192=EDGE_CURVE('',#38595,#38592,#20873,.T.);
#48193=EDGE_CURVE('',#37323,#38577,#31524,.T.);
#48194=EDGE_CURVE('',#38576,#37324,#31525,.T.);
#48195=EDGE_CURVE('',#38594,#36892,#644,.T.);
#48196=EDGE_CURVE('',#36891,#38595,#645,.T.);
#48197=EDGE_CURVE('',#38586,#38589,#646,.T.);
#48198=EDGE_CURVE('',#38588,#38587,#647,.T.);
#48199=EDGE_CURVE('',#38582,#38585,#648,.T.);
#48200=EDGE_CURVE('',#38584,#38583,#649,.T.);
#48201=EDGE_CURVE('',#38596,#38597,#31526,.T.);
#48202=EDGE_CURVE('',#38597,#38598,#20874,.T.);
#48203=EDGE_CURVE('',#38599,#38598,#31527,.T.);
#48204=EDGE_CURVE('',#38600,#38599,#31528,.T.);
#48205=EDGE_CURVE('',#38601,#38600,#31529,.T.);
#48206=EDGE_CURVE('',#38601,#38596,#20875,.T.);
#48207=EDGE_CURVE('',#38599,#38602,#20876,.T.);
#48208=EDGE_CURVE('',#38602,#38603,#31530,.T.);
#48209=EDGE_CURVE('',#38603,#38600,#20877,.T.);
#48210=EDGE_CURVE('',#38604,#38605,#31531,.T.);
#48211=EDGE_CURVE('',#38605,#38606,#20878,.T.);
#48212=EDGE_CURVE('',#38606,#38607,#31532,.T.);
#48213=EDGE_CURVE('',#38607,#38604,#20879,.T.);
#48214=EDGE_CURVE('',#38608,#38609,#31533,.T.);
#48215=EDGE_CURVE('',#38609,#38610,#20880,.T.);
#48216=EDGE_CURVE('',#38611,#38610,#31534,.T.);
#48217=EDGE_CURVE('',#38612,#38611,#31535,.T.);
#48218=EDGE_CURVE('',#38613,#38612,#31536,.T.);
#48219=EDGE_CURVE('',#38613,#38608,#20881,.T.);
#48220=EDGE_CURVE('',#38611,#38614,#20882,.T.);
#48221=EDGE_CURVE('',#38614,#38615,#31537,.T.);
#48222=EDGE_CURVE('',#38615,#38612,#20883,.T.);
#48223=EDGE_CURVE('',#37329,#38597,#31538,.T.);
#48224=EDGE_CURVE('',#38596,#37330,#31539,.T.);
#48225=EDGE_CURVE('',#38614,#36886,#650,.T.);
#48226=EDGE_CURVE('',#36885,#38615,#651,.T.);
#48227=EDGE_CURVE('',#38606,#38609,#652,.T.);
#48228=EDGE_CURVE('',#38608,#38607,#653,.T.);
#48229=EDGE_CURVE('',#38602,#38605,#654,.T.);
#48230=EDGE_CURVE('',#38604,#38603,#655,.T.);
#48231=EDGE_CURVE('',#38616,#38617,#31540,.T.);
#48232=EDGE_CURVE('',#38617,#38618,#20884,.T.);
#48233=EDGE_CURVE('',#38619,#38618,#31541,.T.);
#48234=EDGE_CURVE('',#38620,#38619,#31542,.T.);
#48235=EDGE_CURVE('',#38621,#38620,#31543,.T.);
#48236=EDGE_CURVE('',#38621,#38616,#20885,.T.);
#48237=EDGE_CURVE('',#38619,#38622,#20886,.T.);
#48238=EDGE_CURVE('',#38622,#38623,#31544,.T.);
#48239=EDGE_CURVE('',#38623,#38620,#20887,.T.);
#48240=EDGE_CURVE('',#38624,#38625,#31545,.T.);
#48241=EDGE_CURVE('',#38625,#38626,#20888,.T.);
#48242=EDGE_CURVE('',#38626,#38627,#31546,.T.);
#48243=EDGE_CURVE('',#38627,#38624,#20889,.T.);
#48244=EDGE_CURVE('',#38628,#38629,#31547,.T.);
#48245=EDGE_CURVE('',#38629,#38630,#20890,.T.);
#48246=EDGE_CURVE('',#38631,#38630,#31548,.T.);
#48247=EDGE_CURVE('',#38632,#38631,#31549,.T.);
#48248=EDGE_CURVE('',#38633,#38632,#31550,.T.);
#48249=EDGE_CURVE('',#38633,#38628,#20891,.T.);
#48250=EDGE_CURVE('',#38631,#38634,#20892,.T.);
#48251=EDGE_CURVE('',#38634,#38635,#31551,.T.);
#48252=EDGE_CURVE('',#38635,#38632,#20893,.T.);
#48253=EDGE_CURVE('',#37335,#38617,#31552,.T.);
#48254=EDGE_CURVE('',#38616,#37336,#31553,.T.);
#48255=EDGE_CURVE('',#38634,#36880,#656,.T.);
#48256=EDGE_CURVE('',#36879,#38635,#657,.T.);
#48257=EDGE_CURVE('',#38626,#38629,#658,.T.);
#48258=EDGE_CURVE('',#38628,#38627,#659,.T.);
#48259=EDGE_CURVE('',#38622,#38625,#660,.T.);
#48260=EDGE_CURVE('',#38624,#38623,#661,.T.);
#48261=EDGE_CURVE('',#38636,#38637,#31554,.T.);
#48262=EDGE_CURVE('',#38637,#38638,#20894,.T.);
#48263=EDGE_CURVE('',#38639,#38638,#31555,.T.);
#48264=EDGE_CURVE('',#38640,#38639,#31556,.T.);
#48265=EDGE_CURVE('',#38641,#38640,#31557,.T.);
#48266=EDGE_CURVE('',#38641,#38636,#20895,.T.);
#48267=EDGE_CURVE('',#38639,#38642,#20896,.T.);
#48268=EDGE_CURVE('',#38642,#38643,#31558,.T.);
#48269=EDGE_CURVE('',#38643,#38640,#20897,.T.);
#48270=EDGE_CURVE('',#38644,#38645,#31559,.T.);
#48271=EDGE_CURVE('',#38645,#38646,#20898,.T.);
#48272=EDGE_CURVE('',#38646,#38647,#31560,.T.);
#48273=EDGE_CURVE('',#38647,#38644,#20899,.T.);
#48274=EDGE_CURVE('',#38648,#38649,#31561,.T.);
#48275=EDGE_CURVE('',#38649,#38650,#20900,.T.);
#48276=EDGE_CURVE('',#38651,#38650,#31562,.T.);
#48277=EDGE_CURVE('',#38652,#38651,#31563,.T.);
#48278=EDGE_CURVE('',#38653,#38652,#31564,.T.);
#48279=EDGE_CURVE('',#38653,#38648,#20901,.T.);
#48280=EDGE_CURVE('',#38651,#38654,#20902,.T.);
#48281=EDGE_CURVE('',#38654,#38655,#31565,.T.);
#48282=EDGE_CURVE('',#38655,#38652,#20903,.T.);
#48283=EDGE_CURVE('',#37341,#38637,#31566,.T.);
#48284=EDGE_CURVE('',#38636,#37342,#31567,.T.);
#48285=EDGE_CURVE('',#38654,#36874,#662,.T.);
#48286=EDGE_CURVE('',#36873,#38655,#663,.T.);
#48287=EDGE_CURVE('',#38646,#38649,#664,.T.);
#48288=EDGE_CURVE('',#38648,#38647,#665,.T.);
#48289=EDGE_CURVE('',#38642,#38645,#666,.T.);
#48290=EDGE_CURVE('',#38644,#38643,#667,.T.);
#48291=EDGE_CURVE('',#38656,#38657,#31568,.T.);
#48292=EDGE_CURVE('',#38657,#38658,#20904,.T.);
#48293=EDGE_CURVE('',#38659,#38658,#31569,.T.);
#48294=EDGE_CURVE('',#38660,#38659,#31570,.T.);
#48295=EDGE_CURVE('',#38661,#38660,#31571,.T.);
#48296=EDGE_CURVE('',#38661,#38656,#20905,.T.);
#48297=EDGE_CURVE('',#38659,#38662,#20906,.T.);
#48298=EDGE_CURVE('',#38662,#38663,#31572,.T.);
#48299=EDGE_CURVE('',#38663,#38660,#20907,.T.);
#48300=EDGE_CURVE('',#38664,#38665,#31573,.T.);
#48301=EDGE_CURVE('',#38665,#38666,#20908,.T.);
#48302=EDGE_CURVE('',#38666,#38667,#31574,.T.);
#48303=EDGE_CURVE('',#38667,#38664,#20909,.T.);
#48304=EDGE_CURVE('',#38668,#38669,#31575,.T.);
#48305=EDGE_CURVE('',#38669,#38670,#20910,.T.);
#48306=EDGE_CURVE('',#38671,#38670,#31576,.T.);
#48307=EDGE_CURVE('',#38672,#38671,#31577,.T.);
#48308=EDGE_CURVE('',#38673,#38672,#31578,.T.);
#48309=EDGE_CURVE('',#38673,#38668,#20911,.T.);
#48310=EDGE_CURVE('',#38671,#38674,#20912,.T.);
#48311=EDGE_CURVE('',#38674,#38675,#31579,.T.);
#48312=EDGE_CURVE('',#38675,#38672,#20913,.T.);
#48313=EDGE_CURVE('',#37347,#38657,#31580,.T.);
#48314=EDGE_CURVE('',#38656,#37348,#31581,.T.);
#48315=EDGE_CURVE('',#38674,#36868,#668,.T.);
#48316=EDGE_CURVE('',#36867,#38675,#669,.T.);
#48317=EDGE_CURVE('',#38666,#38669,#670,.T.);
#48318=EDGE_CURVE('',#38668,#38667,#671,.T.);
#48319=EDGE_CURVE('',#38662,#38665,#672,.T.);
#48320=EDGE_CURVE('',#38664,#38663,#673,.T.);
#48321=EDGE_CURVE('',#38676,#38677,#31582,.T.);
#48322=EDGE_CURVE('',#38677,#38678,#20914,.T.);
#48323=EDGE_CURVE('',#38679,#38678,#31583,.T.);
#48324=EDGE_CURVE('',#38680,#38679,#31584,.T.);
#48325=EDGE_CURVE('',#38681,#38680,#31585,.T.);
#48326=EDGE_CURVE('',#38681,#38676,#20915,.T.);
#48327=EDGE_CURVE('',#38679,#38682,#20916,.T.);
#48328=EDGE_CURVE('',#38682,#38683,#31586,.T.);
#48329=EDGE_CURVE('',#38683,#38680,#20917,.T.);
#48330=EDGE_CURVE('',#38684,#38685,#31587,.T.);
#48331=EDGE_CURVE('',#38685,#38686,#20918,.T.);
#48332=EDGE_CURVE('',#38686,#38687,#31588,.T.);
#48333=EDGE_CURVE('',#38687,#38684,#20919,.T.);
#48334=EDGE_CURVE('',#38688,#38689,#31589,.T.);
#48335=EDGE_CURVE('',#38689,#38690,#20920,.T.);
#48336=EDGE_CURVE('',#38691,#38690,#31590,.T.);
#48337=EDGE_CURVE('',#38692,#38691,#31591,.T.);
#48338=EDGE_CURVE('',#38693,#38692,#31592,.T.);
#48339=EDGE_CURVE('',#38693,#38688,#20921,.T.);
#48340=EDGE_CURVE('',#38691,#38694,#20922,.T.);
#48341=EDGE_CURVE('',#38694,#38695,#31593,.T.);
#48342=EDGE_CURVE('',#38695,#38692,#20923,.T.);
#48343=EDGE_CURVE('',#37353,#38677,#31594,.T.);
#48344=EDGE_CURVE('',#38676,#37354,#31595,.T.);
#48345=EDGE_CURVE('',#38694,#36862,#674,.T.);
#48346=EDGE_CURVE('',#36861,#38695,#675,.T.);
#48347=EDGE_CURVE('',#38686,#38689,#676,.T.);
#48348=EDGE_CURVE('',#38688,#38687,#677,.T.);
#48349=EDGE_CURVE('',#38682,#38685,#678,.T.);
#48350=EDGE_CURVE('',#38684,#38683,#679,.T.);
#48351=EDGE_CURVE('',#38696,#38697,#31596,.T.);
#48352=EDGE_CURVE('',#38697,#38698,#20924,.T.);
#48353=EDGE_CURVE('',#38699,#38698,#31597,.T.);
#48354=EDGE_CURVE('',#38700,#38699,#31598,.T.);
#48355=EDGE_CURVE('',#38701,#38700,#31599,.T.);
#48356=EDGE_CURVE('',#38701,#38696,#20925,.T.);
#48357=EDGE_CURVE('',#38699,#38702,#20926,.T.);
#48358=EDGE_CURVE('',#38702,#38703,#31600,.T.);
#48359=EDGE_CURVE('',#38703,#38700,#20927,.T.);
#48360=EDGE_CURVE('',#38704,#38705,#31601,.T.);
#48361=EDGE_CURVE('',#38705,#38706,#20928,.T.);
#48362=EDGE_CURVE('',#38706,#38707,#31602,.T.);
#48363=EDGE_CURVE('',#38707,#38704,#20929,.T.);
#48364=EDGE_CURVE('',#38708,#38709,#31603,.T.);
#48365=EDGE_CURVE('',#38709,#38710,#20930,.T.);
#48366=EDGE_CURVE('',#38711,#38710,#31604,.T.);
#48367=EDGE_CURVE('',#38712,#38711,#31605,.T.);
#48368=EDGE_CURVE('',#38713,#38712,#31606,.T.);
#48369=EDGE_CURVE('',#38713,#38708,#20931,.T.);
#48370=EDGE_CURVE('',#38711,#38714,#20932,.T.);
#48371=EDGE_CURVE('',#38714,#38715,#31607,.T.);
#48372=EDGE_CURVE('',#38715,#38712,#20933,.T.);
#48373=EDGE_CURVE('',#37359,#38697,#31608,.T.);
#48374=EDGE_CURVE('',#38696,#37360,#31609,.T.);
#48375=EDGE_CURVE('',#38714,#36856,#680,.T.);
#48376=EDGE_CURVE('',#36855,#38715,#681,.T.);
#48377=EDGE_CURVE('',#38706,#38709,#682,.T.);
#48378=EDGE_CURVE('',#38708,#38707,#683,.T.);
#48379=EDGE_CURVE('',#38702,#38705,#684,.T.);
#48380=EDGE_CURVE('',#38704,#38703,#685,.T.);
#48381=EDGE_CURVE('',#38716,#38717,#31610,.T.);
#48382=EDGE_CURVE('',#38717,#38718,#20934,.T.);
#48383=EDGE_CURVE('',#38719,#38718,#31611,.T.);
#48384=EDGE_CURVE('',#38720,#38719,#31612,.T.);
#48385=EDGE_CURVE('',#38721,#38720,#31613,.T.);
#48386=EDGE_CURVE('',#38721,#38716,#20935,.T.);
#48387=EDGE_CURVE('',#38719,#38722,#20936,.T.);
#48388=EDGE_CURVE('',#38722,#38723,#31614,.T.);
#48389=EDGE_CURVE('',#38723,#38720,#20937,.T.);
#48390=EDGE_CURVE('',#38724,#38725,#31615,.T.);
#48391=EDGE_CURVE('',#38725,#38726,#20938,.T.);
#48392=EDGE_CURVE('',#38726,#38727,#31616,.T.);
#48393=EDGE_CURVE('',#38727,#38724,#20939,.T.);
#48394=EDGE_CURVE('',#38728,#38729,#31617,.T.);
#48395=EDGE_CURVE('',#38729,#38730,#20940,.T.);
#48396=EDGE_CURVE('',#38731,#38730,#31618,.T.);
#48397=EDGE_CURVE('',#38732,#38731,#31619,.T.);
#48398=EDGE_CURVE('',#38733,#38732,#31620,.T.);
#48399=EDGE_CURVE('',#38733,#38728,#20941,.T.);
#48400=EDGE_CURVE('',#38731,#38734,#20942,.T.);
#48401=EDGE_CURVE('',#38734,#38735,#31621,.T.);
#48402=EDGE_CURVE('',#38735,#38732,#20943,.T.);
#48403=EDGE_CURVE('',#37365,#38717,#31622,.T.);
#48404=EDGE_CURVE('',#38716,#37366,#31623,.T.);
#48405=EDGE_CURVE('',#38734,#36850,#686,.T.);
#48406=EDGE_CURVE('',#36849,#38735,#687,.T.);
#48407=EDGE_CURVE('',#38726,#38729,#688,.T.);
#48408=EDGE_CURVE('',#38728,#38727,#689,.T.);
#48409=EDGE_CURVE('',#38722,#38725,#690,.T.);
#48410=EDGE_CURVE('',#38724,#38723,#691,.T.);
#48411=EDGE_CURVE('',#38736,#38737,#31624,.T.);
#48412=EDGE_CURVE('',#38737,#38738,#20944,.T.);
#48413=EDGE_CURVE('',#38739,#38738,#31625,.T.);
#48414=EDGE_CURVE('',#38740,#38739,#31626,.T.);
#48415=EDGE_CURVE('',#38741,#38740,#31627,.T.);
#48416=EDGE_CURVE('',#38741,#38736,#20945,.T.);
#48417=EDGE_CURVE('',#38739,#38742,#20946,.T.);
#48418=EDGE_CURVE('',#38742,#38743,#31628,.T.);
#48419=EDGE_CURVE('',#38743,#38740,#20947,.T.);
#48420=EDGE_CURVE('',#38744,#38745,#31629,.T.);
#48421=EDGE_CURVE('',#38745,#38746,#20948,.T.);
#48422=EDGE_CURVE('',#38746,#38747,#31630,.T.);
#48423=EDGE_CURVE('',#38747,#38744,#20949,.T.);
#48424=EDGE_CURVE('',#38748,#38749,#31631,.T.);
#48425=EDGE_CURVE('',#38749,#38750,#20950,.T.);
#48426=EDGE_CURVE('',#38751,#38750,#31632,.T.);
#48427=EDGE_CURVE('',#38752,#38751,#31633,.T.);
#48428=EDGE_CURVE('',#38753,#38752,#31634,.T.);
#48429=EDGE_CURVE('',#38753,#38748,#20951,.T.);
#48430=EDGE_CURVE('',#38751,#38754,#20952,.T.);
#48431=EDGE_CURVE('',#38754,#38755,#31635,.T.);
#48432=EDGE_CURVE('',#38755,#38752,#20953,.T.);
#48433=EDGE_CURVE('',#37371,#38737,#31636,.T.);
#48434=EDGE_CURVE('',#38736,#37372,#31637,.T.);
#48435=EDGE_CURVE('',#38754,#36844,#692,.T.);
#48436=EDGE_CURVE('',#36843,#38755,#693,.T.);
#48437=EDGE_CURVE('',#38746,#38749,#694,.T.);
#48438=EDGE_CURVE('',#38748,#38747,#695,.T.);
#48439=EDGE_CURVE('',#38742,#38745,#696,.T.);
#48440=EDGE_CURVE('',#38744,#38743,#697,.T.);
#48441=EDGE_CURVE('',#38756,#38757,#20954,.T.);
#48442=EDGE_CURVE('',#38757,#38758,#31638,.T.);
#48443=EDGE_CURVE('',#38758,#38759,#20955,.T.);
#48444=EDGE_CURVE('',#38759,#38756,#31639,.T.);
#48445=EDGE_CURVE('',#38760,#38761,#698,.T.);
#48446=EDGE_CURVE('',#38761,#38762,#20956,.T.);
#48447=EDGE_CURVE('',#38762,#38763,#20957,.T.);
#48448=EDGE_CURVE('',#38763,#38764,#20958,.T.);
#48449=EDGE_CURVE('',#38764,#38765,#699,.T.);
#48450=EDGE_CURVE('',#38765,#38766,#20959,.T.);
#48451=EDGE_CURVE('',#38766,#38767,#20960,.T.);
#48452=EDGE_CURVE('',#38767,#38768,#700,.T.);
#48453=EDGE_CURVE('',#38768,#38769,#20961,.T.);
#48454=EDGE_CURVE('',#38769,#38770,#701,.T.);
#48455=EDGE_CURVE('',#38770,#38771,#20962,.T.);
#48456=EDGE_CURVE('',#38771,#38760,#20963,.T.);
#48457=EDGE_CURVE('',#38772,#38773,#702,.T.);
#48458=EDGE_CURVE('',#38773,#38774,#20964,.T.);
#48459=EDGE_CURVE('',#38774,#38775,#20965,.T.);
#48460=EDGE_CURVE('',#38775,#38776,#20966,.T.);
#48461=EDGE_CURVE('',#38776,#38777,#703,.T.);
#48462=EDGE_CURVE('',#38777,#38778,#20967,.T.);
#48463=EDGE_CURVE('',#38778,#38779,#20968,.T.);
#48464=EDGE_CURVE('',#38779,#38780,#704,.T.);
#48465=EDGE_CURVE('',#38780,#38781,#20969,.T.);
#48466=EDGE_CURVE('',#38781,#38782,#705,.T.);
#48467=EDGE_CURVE('',#38782,#38783,#20970,.T.);
#48468=EDGE_CURVE('',#38783,#38772,#20971,.T.);
#48469=EDGE_CURVE('',#38774,#38757,#4495,.T.);
#48470=EDGE_CURVE('',#38756,#38775,#4496,.T.);
#48471=EDGE_CURVE('',#38758,#38763,#4497,.T.);
#48472=EDGE_CURVE('',#38762,#38759,#4498,.T.);
#48473=EDGE_CURVE('',#38783,#38753,#706,.T.);
#48474=EDGE_CURVE('',#38748,#38782,#31640,.T.);
#48475=EDGE_CURVE('',#38747,#38781,#31641,.T.);
#48476=EDGE_CURVE('',#38772,#38755,#31642,.T.);
#48477=EDGE_CURVE('',#38744,#38780,#31643,.T.);
#48478=EDGE_CURVE('',#38773,#36843,#31644,.T.);
#48479=EDGE_CURVE('',#38743,#38779,#31645,.T.);
#48480=EDGE_CURVE('',#38774,#36842,#31646,.T.);
#48481=EDGE_CURVE('',#38741,#38778,#707,.T.);
#48482=EDGE_CURVE('',#38757,#36841,#31647,.T.);
#48483=EDGE_CURVE('',#38736,#38777,#31648,.T.);
#48484=EDGE_CURVE('',#38758,#36840,#31649,.T.);
#48485=EDGE_CURVE('',#37372,#38776,#31650,.T.);
#48486=EDGE_CURVE('',#38763,#37195,#31651,.T.);
#48487=EDGE_CURVE('',#37373,#38775,#31652,.T.);
#48488=EDGE_CURVE('',#38764,#37194,#31653,.T.);
#48489=EDGE_CURVE('',#37374,#38756,#31654,.T.);
#48490=EDGE_CURVE('',#38765,#37574,#31655,.T.);
#48491=EDGE_CURVE('',#37376,#38759,#31656,.T.);
#48492=EDGE_CURVE('',#38766,#37572,#708,.T.);
#48493=EDGE_CURVE('',#37377,#38762,#31657,.T.);
#48494=EDGE_CURVE('',#38767,#37571,#31658,.T.);
#48495=EDGE_CURVE('',#37378,#38761,#31659,.T.);
#48496=EDGE_CURVE('',#38768,#37564,#31660,.T.);
#48497=EDGE_CURVE('',#37559,#38760,#31661,.T.);
#48498=EDGE_CURVE('',#38769,#37567,#31662,.T.);
#48499=EDGE_CURVE('',#37560,#38771,#709,.T.);
#48500=EDGE_CURVE('',#38770,#37562,#31663,.T.);
#48501=EDGE_CURVE('',#38784,#38785,#20972,.T.);
#48502=EDGE_CURVE('',#38785,#38786,#31664,.T.);
#48503=EDGE_CURVE('',#38786,#38787,#20973,.T.);
#48504=EDGE_CURVE('',#38787,#38784,#31665,.T.);
#48505=EDGE_CURVE('',#38788,#38789,#710,.T.);
#48506=EDGE_CURVE('',#38789,#38790,#20974,.T.);
#48507=EDGE_CURVE('',#38790,#38791,#20975,.T.);
#48508=EDGE_CURVE('',#38791,#38792,#20976,.T.);
#48509=EDGE_CURVE('',#38792,#38793,#711,.T.);
#48510=EDGE_CURVE('',#38793,#38794,#20977,.T.);
#48511=EDGE_CURVE('',#38794,#38795,#20978,.T.);
#48512=EDGE_CURVE('',#38795,#38796,#712,.T.);
#48513=EDGE_CURVE('',#38796,#38797,#20979,.T.);
#48514=EDGE_CURVE('',#38797,#38798,#713,.T.);
#48515=EDGE_CURVE('',#38798,#38799,#20980,.T.);
#48516=EDGE_CURVE('',#38799,#38788,#20981,.T.);
#48517=EDGE_CURVE('',#38800,#38801,#714,.T.);
#48518=EDGE_CURVE('',#38801,#38802,#20982,.T.);
#48519=EDGE_CURVE('',#38802,#38803,#20983,.T.);
#48520=EDGE_CURVE('',#38803,#38804,#20984,.T.);
#48521=EDGE_CURVE('',#38804,#38805,#715,.T.);
#48522=EDGE_CURVE('',#38805,#38806,#20985,.T.);
#48523=EDGE_CURVE('',#38806,#38807,#20986,.T.);
#48524=EDGE_CURVE('',#38807,#38808,#716,.T.);
#48525=EDGE_CURVE('',#38808,#38809,#20987,.T.);
#48526=EDGE_CURVE('',#38809,#38810,#717,.T.);
#48527=EDGE_CURVE('',#38810,#38811,#20988,.T.);
#48528=EDGE_CURVE('',#38811,#38800,#20989,.T.);
#48529=EDGE_CURVE('',#38812,#38813,#20990,.T.);
#48530=EDGE_CURVE('',#38813,#38814,#31666,.T.);
#48531=EDGE_CURVE('',#38814,#38815,#20991,.T.);
#48532=EDGE_CURVE('',#38815,#38812,#31667,.T.);
#48533=EDGE_CURVE('',#38816,#38817,#718,.T.);
#48534=EDGE_CURVE('',#38817,#38818,#20992,.T.);
#48535=EDGE_CURVE('',#38818,#38819,#20993,.T.);
#48536=EDGE_CURVE('',#38819,#38820,#20994,.T.);
#48537=EDGE_CURVE('',#38820,#38821,#719,.T.);
#48538=EDGE_CURVE('',#38821,#38822,#20995,.T.);
#48539=EDGE_CURVE('',#38822,#38823,#20996,.T.);
#48540=EDGE_CURVE('',#38823,#38824,#720,.T.);
#48541=EDGE_CURVE('',#38824,#38825,#20997,.T.);
#48542=EDGE_CURVE('',#38825,#38826,#721,.T.);
#48543=EDGE_CURVE('',#38826,#38827,#20998,.T.);
#48544=EDGE_CURVE('',#38827,#38816,#20999,.T.);
#48545=EDGE_CURVE('',#38828,#38829,#722,.T.);
#48546=EDGE_CURVE('',#38829,#38830,#21000,.T.);
#48547=EDGE_CURVE('',#38830,#38831,#21001,.T.);
#48548=EDGE_CURVE('',#38831,#38832,#21002,.T.);
#48549=EDGE_CURVE('',#38832,#38833,#723,.T.);
#48550=EDGE_CURVE('',#38833,#38834,#21003,.T.);
#48551=EDGE_CURVE('',#38834,#38835,#21004,.T.);
#48552=EDGE_CURVE('',#38835,#38836,#724,.T.);
#48553=EDGE_CURVE('',#38836,#38837,#21005,.T.);
#48554=EDGE_CURVE('',#38837,#38838,#725,.T.);
#48555=EDGE_CURVE('',#38838,#38839,#21006,.T.);
#48556=EDGE_CURVE('',#38839,#38828,#21007,.T.);
#48557=EDGE_CURVE('',#38840,#38841,#21008,.T.);
#48558=EDGE_CURVE('',#38841,#38842,#31668,.T.);
#48559=EDGE_CURVE('',#38842,#38843,#21009,.T.);
#48560=EDGE_CURVE('',#38843,#38840,#31669,.T.);
#48561=EDGE_CURVE('',#38844,#38845,#726,.T.);
#48562=EDGE_CURVE('',#38845,#38846,#21010,.T.);
#48563=EDGE_CURVE('',#38846,#38847,#21011,.T.);
#48564=EDGE_CURVE('',#38847,#38848,#21012,.T.);
#48565=EDGE_CURVE('',#38848,#38849,#727,.T.);
#48566=EDGE_CURVE('',#38849,#38850,#21013,.T.);
#48567=EDGE_CURVE('',#38850,#38851,#21014,.T.);
#48568=EDGE_CURVE('',#38851,#38852,#728,.T.);
#48569=EDGE_CURVE('',#38852,#38853,#21015,.T.);
#48570=EDGE_CURVE('',#38853,#38854,#729,.T.);
#48571=EDGE_CURVE('',#38854,#38855,#21016,.T.);
#48572=EDGE_CURVE('',#38855,#38844,#21017,.T.);
#48573=EDGE_CURVE('',#38856,#38857,#730,.T.);
#48574=EDGE_CURVE('',#38857,#38858,#21018,.T.);
#48575=EDGE_CURVE('',#38858,#38859,#21019,.T.);
#48576=EDGE_CURVE('',#38859,#38860,#21020,.T.);
#48577=EDGE_CURVE('',#38860,#38861,#731,.T.);
#48578=EDGE_CURVE('',#38861,#38862,#21021,.T.);
#48579=EDGE_CURVE('',#38862,#38863,#21022,.T.);
#48580=EDGE_CURVE('',#38863,#38864,#732,.T.);
#48581=EDGE_CURVE('',#38864,#38865,#21023,.T.);
#48582=EDGE_CURVE('',#38865,#38866,#733,.T.);
#48583=EDGE_CURVE('',#38866,#38867,#21024,.T.);
#48584=EDGE_CURVE('',#38867,#38856,#21025,.T.);
#48585=EDGE_CURVE('',#38868,#38869,#21026,.T.);
#48586=EDGE_CURVE('',#38869,#38870,#31670,.T.);
#48587=EDGE_CURVE('',#38870,#38871,#21027,.T.);
#48588=EDGE_CURVE('',#38871,#38868,#31671,.T.);
#48589=EDGE_CURVE('',#38872,#38873,#734,.T.);
#48590=EDGE_CURVE('',#38873,#38874,#21028,.T.);
#48591=EDGE_CURVE('',#38874,#38875,#21029,.T.);
#48592=EDGE_CURVE('',#38875,#38876,#21030,.T.);
#48593=EDGE_CURVE('',#38876,#38877,#735,.T.);
#48594=EDGE_CURVE('',#38877,#38878,#21031,.T.);
#48595=EDGE_CURVE('',#38878,#38879,#21032,.T.);
#48596=EDGE_CURVE('',#38879,#38880,#736,.T.);
#48597=EDGE_CURVE('',#38880,#38881,#21033,.T.);
#48598=EDGE_CURVE('',#38881,#38882,#737,.T.);
#48599=EDGE_CURVE('',#38882,#38883,#21034,.T.);
#48600=EDGE_CURVE('',#38883,#38872,#21035,.T.);
#48601=EDGE_CURVE('',#38884,#38885,#738,.T.);
#48602=EDGE_CURVE('',#38885,#38886,#21036,.T.);
#48603=EDGE_CURVE('',#38886,#38887,#21037,.T.);
#48604=EDGE_CURVE('',#38887,#38888,#21038,.T.);
#48605=EDGE_CURVE('',#38888,#38889,#739,.T.);
#48606=EDGE_CURVE('',#38889,#38890,#21039,.T.);
#48607=EDGE_CURVE('',#38890,#38891,#21040,.T.);
#48608=EDGE_CURVE('',#38891,#38892,#740,.T.);
#48609=EDGE_CURVE('',#38892,#38893,#21041,.T.);
#48610=EDGE_CURVE('',#38893,#38894,#741,.T.);
#48611=EDGE_CURVE('',#38894,#38895,#21042,.T.);
#48612=EDGE_CURVE('',#38895,#38884,#21043,.T.);
#48613=EDGE_CURVE('',#38896,#38897,#21044,.T.);
#48614=EDGE_CURVE('',#38897,#38898,#31672,.T.);
#48615=EDGE_CURVE('',#38898,#38899,#21045,.T.);
#48616=EDGE_CURVE('',#38899,#38896,#31673,.T.);
#48617=EDGE_CURVE('',#38900,#38901,#742,.T.);
#48618=EDGE_CURVE('',#38901,#38902,#21046,.T.);
#48619=EDGE_CURVE('',#38902,#38903,#21047,.T.);
#48620=EDGE_CURVE('',#38903,#38904,#21048,.T.);
#48621=EDGE_CURVE('',#38904,#38905,#743,.T.);
#48622=EDGE_CURVE('',#38905,#38906,#21049,.T.);
#48623=EDGE_CURVE('',#38906,#38907,#21050,.T.);
#48624=EDGE_CURVE('',#38907,#38908,#744,.T.);
#48625=EDGE_CURVE('',#38908,#38909,#21051,.T.);
#48626=EDGE_CURVE('',#38909,#38910,#745,.T.);
#48627=EDGE_CURVE('',#38910,#38911,#21052,.T.);
#48628=EDGE_CURVE('',#38911,#38900,#21053,.T.);
#48629=EDGE_CURVE('',#38912,#38913,#746,.T.);
#48630=EDGE_CURVE('',#38913,#38914,#21054,.T.);
#48631=EDGE_CURVE('',#38914,#38915,#21055,.T.);
#48632=EDGE_CURVE('',#38915,#38916,#21056,.T.);
#48633=EDGE_CURVE('',#38916,#38917,#747,.T.);
#48634=EDGE_CURVE('',#38917,#38918,#21057,.T.);
#48635=EDGE_CURVE('',#38918,#38919,#21058,.T.);
#48636=EDGE_CURVE('',#38919,#38920,#748,.T.);
#48637=EDGE_CURVE('',#38920,#38921,#21059,.T.);
#48638=EDGE_CURVE('',#38921,#38922,#749,.T.);
#48639=EDGE_CURVE('',#38922,#38923,#21060,.T.);
#48640=EDGE_CURVE('',#38923,#38912,#21061,.T.);
#48641=EDGE_CURVE('',#38924,#38925,#21062,.T.);
#48642=EDGE_CURVE('',#38925,#38926,#31674,.T.);
#48643=EDGE_CURVE('',#38926,#38927,#21063,.T.);
#48644=EDGE_CURVE('',#38927,#38924,#31675,.T.);
#48645=EDGE_CURVE('',#38928,#38929,#750,.T.);
#48646=EDGE_CURVE('',#38929,#38930,#21064,.T.);
#48647=EDGE_CURVE('',#38930,#38931,#21065,.T.);
#48648=EDGE_CURVE('',#38931,#38932,#21066,.T.);
#48649=EDGE_CURVE('',#38932,#38933,#751,.T.);
#48650=EDGE_CURVE('',#38933,#38934,#21067,.T.);
#48651=EDGE_CURVE('',#38934,#38935,#21068,.T.);
#48652=EDGE_CURVE('',#38935,#38936,#752,.T.);
#48653=EDGE_CURVE('',#38936,#38937,#21069,.T.);
#48654=EDGE_CURVE('',#38937,#38938,#753,.T.);
#48655=EDGE_CURVE('',#38938,#38939,#21070,.T.);
#48656=EDGE_CURVE('',#38939,#38928,#21071,.T.);
#48657=EDGE_CURVE('',#38940,#38941,#754,.T.);
#48658=EDGE_CURVE('',#38941,#38942,#21072,.T.);
#48659=EDGE_CURVE('',#38942,#38943,#21073,.T.);
#48660=EDGE_CURVE('',#38943,#38944,#21074,.T.);
#48661=EDGE_CURVE('',#38944,#38945,#755,.T.);
#48662=EDGE_CURVE('',#38945,#38946,#21075,.T.);
#48663=EDGE_CURVE('',#38946,#38947,#21076,.T.);
#48664=EDGE_CURVE('',#38947,#38948,#756,.T.);
#48665=EDGE_CURVE('',#38948,#38949,#21077,.T.);
#48666=EDGE_CURVE('',#38949,#38950,#757,.T.);
#48667=EDGE_CURVE('',#38950,#38951,#21078,.T.);
#48668=EDGE_CURVE('',#38951,#38940,#21079,.T.);
#48669=EDGE_CURVE('',#38952,#38953,#21080,.T.);
#48670=EDGE_CURVE('',#38953,#38954,#31676,.T.);
#48671=EDGE_CURVE('',#38954,#38955,#21081,.T.);
#48672=EDGE_CURVE('',#38955,#38952,#31677,.T.);
#48673=EDGE_CURVE('',#38956,#38957,#758,.T.);
#48674=EDGE_CURVE('',#38957,#38958,#21082,.T.);
#48675=EDGE_CURVE('',#38958,#38959,#21083,.T.);
#48676=EDGE_CURVE('',#38959,#38960,#21084,.T.);
#48677=EDGE_CURVE('',#38960,#38961,#759,.T.);
#48678=EDGE_CURVE('',#38961,#38962,#21085,.T.);
#48679=EDGE_CURVE('',#38962,#38963,#21086,.T.);
#48680=EDGE_CURVE('',#38963,#38964,#760,.T.);
#48681=EDGE_CURVE('',#38964,#38965,#21087,.T.);
#48682=EDGE_CURVE('',#38965,#38966,#761,.T.);
#48683=EDGE_CURVE('',#38966,#38967,#21088,.T.);
#48684=EDGE_CURVE('',#38967,#38956,#21089,.T.);
#48685=EDGE_CURVE('',#38968,#38969,#762,.T.);
#48686=EDGE_CURVE('',#38969,#38970,#21090,.T.);
#48687=EDGE_CURVE('',#38970,#38971,#21091,.T.);
#48688=EDGE_CURVE('',#38971,#38972,#21092,.T.);
#48689=EDGE_CURVE('',#38972,#38973,#763,.T.);
#48690=EDGE_CURVE('',#38973,#38974,#21093,.T.);
#48691=EDGE_CURVE('',#38974,#38975,#21094,.T.);
#48692=EDGE_CURVE('',#38975,#38976,#764,.T.);
#48693=EDGE_CURVE('',#38976,#38977,#21095,.T.);
#48694=EDGE_CURVE('',#38977,#38978,#765,.T.);
#48695=EDGE_CURVE('',#38978,#38979,#21096,.T.);
#48696=EDGE_CURVE('',#38979,#38968,#21097,.T.);
#48697=EDGE_CURVE('',#38980,#38981,#21098,.T.);
#48698=EDGE_CURVE('',#38981,#38982,#31678,.T.);
#48699=EDGE_CURVE('',#38982,#38983,#21099,.T.);
#48700=EDGE_CURVE('',#38983,#38980,#31679,.T.);
#48701=EDGE_CURVE('',#38984,#38985,#766,.T.);
#48702=EDGE_CURVE('',#38985,#38986,#21100,.T.);
#48703=EDGE_CURVE('',#38986,#38987,#21101,.T.);
#48704=EDGE_CURVE('',#38987,#38988,#21102,.T.);
#48705=EDGE_CURVE('',#38988,#38989,#767,.T.);
#48706=EDGE_CURVE('',#38989,#38990,#21103,.T.);
#48707=EDGE_CURVE('',#38990,#38991,#21104,.T.);
#48708=EDGE_CURVE('',#38991,#38992,#768,.T.);
#48709=EDGE_CURVE('',#38992,#38993,#21105,.T.);
#48710=EDGE_CURVE('',#38993,#38994,#769,.T.);
#48711=EDGE_CURVE('',#38994,#38995,#21106,.T.);
#48712=EDGE_CURVE('',#38995,#38984,#21107,.T.);
#48713=EDGE_CURVE('',#38996,#38997,#770,.T.);
#48714=EDGE_CURVE('',#38997,#38998,#21108,.T.);
#48715=EDGE_CURVE('',#38998,#38999,#21109,.T.);
#48716=EDGE_CURVE('',#38999,#39000,#21110,.T.);
#48717=EDGE_CURVE('',#39000,#39001,#771,.T.);
#48718=EDGE_CURVE('',#39001,#39002,#21111,.T.);
#48719=EDGE_CURVE('',#39002,#39003,#21112,.T.);
#48720=EDGE_CURVE('',#39003,#39004,#772,.T.);
#48721=EDGE_CURVE('',#39004,#39005,#21113,.T.);
#48722=EDGE_CURVE('',#39005,#39006,#773,.T.);
#48723=EDGE_CURVE('',#39006,#39007,#21114,.T.);
#48724=EDGE_CURVE('',#39007,#38996,#21115,.T.);
#48725=EDGE_CURVE('',#39008,#39009,#21116,.T.);
#48726=EDGE_CURVE('',#39009,#39010,#31680,.T.);
#48727=EDGE_CURVE('',#39010,#39011,#21117,.T.);
#48728=EDGE_CURVE('',#39011,#39008,#31681,.T.);
#48729=EDGE_CURVE('',#39012,#39013,#774,.T.);
#48730=EDGE_CURVE('',#39013,#39014,#21118,.T.);
#48731=EDGE_CURVE('',#39014,#39015,#21119,.T.);
#48732=EDGE_CURVE('',#39015,#39016,#21120,.T.);
#48733=EDGE_CURVE('',#39016,#39017,#775,.T.);
#48734=EDGE_CURVE('',#39017,#39018,#21121,.T.);
#48735=EDGE_CURVE('',#39018,#39019,#21122,.T.);
#48736=EDGE_CURVE('',#39019,#39020,#776,.T.);
#48737=EDGE_CURVE('',#39020,#39021,#21123,.T.);
#48738=EDGE_CURVE('',#39021,#39022,#777,.T.);
#48739=EDGE_CURVE('',#39022,#39023,#21124,.T.);
#48740=EDGE_CURVE('',#39023,#39012,#21125,.T.);
#48741=EDGE_CURVE('',#39024,#39025,#778,.T.);
#48742=EDGE_CURVE('',#39025,#39026,#21126,.T.);
#48743=EDGE_CURVE('',#39026,#39027,#21127,.T.);
#48744=EDGE_CURVE('',#39027,#39028,#21128,.T.);
#48745=EDGE_CURVE('',#39028,#39029,#779,.T.);
#48746=EDGE_CURVE('',#39029,#39030,#21129,.T.);
#48747=EDGE_CURVE('',#39030,#39031,#21130,.T.);
#48748=EDGE_CURVE('',#39031,#39032,#780,.T.);
#48749=EDGE_CURVE('',#39032,#39033,#21131,.T.);
#48750=EDGE_CURVE('',#39033,#39034,#781,.T.);
#48751=EDGE_CURVE('',#39034,#39035,#21132,.T.);
#48752=EDGE_CURVE('',#39035,#39024,#21133,.T.);
#48753=EDGE_CURVE('',#39036,#39037,#21134,.T.);
#48754=EDGE_CURVE('',#39037,#39038,#31682,.T.);
#48755=EDGE_CURVE('',#39038,#39039,#21135,.T.);
#48756=EDGE_CURVE('',#39039,#39036,#31683,.T.);
#48757=EDGE_CURVE('',#39040,#39041,#782,.T.);
#48758=EDGE_CURVE('',#39041,#39042,#21136,.T.);
#48759=EDGE_CURVE('',#39042,#39043,#21137,.T.);
#48760=EDGE_CURVE('',#39043,#39044,#21138,.T.);
#48761=EDGE_CURVE('',#39044,#39045,#783,.T.);
#48762=EDGE_CURVE('',#39045,#39046,#21139,.T.);
#48763=EDGE_CURVE('',#39046,#39047,#21140,.T.);
#48764=EDGE_CURVE('',#39047,#39048,#784,.T.);
#48765=EDGE_CURVE('',#39048,#39049,#21141,.T.);
#48766=EDGE_CURVE('',#39049,#39050,#785,.T.);
#48767=EDGE_CURVE('',#39050,#39051,#21142,.T.);
#48768=EDGE_CURVE('',#39051,#39040,#21143,.T.);
#48769=EDGE_CURVE('',#39052,#39053,#786,.T.);
#48770=EDGE_CURVE('',#39053,#39054,#21144,.T.);
#48771=EDGE_CURVE('',#39054,#39055,#21145,.T.);
#48772=EDGE_CURVE('',#39055,#39056,#21146,.T.);
#48773=EDGE_CURVE('',#39056,#39057,#787,.T.);
#48774=EDGE_CURVE('',#39057,#39058,#21147,.T.);
#48775=EDGE_CURVE('',#39058,#39059,#21148,.T.);
#48776=EDGE_CURVE('',#39059,#39060,#788,.T.);
#48777=EDGE_CURVE('',#39060,#39061,#21149,.T.);
#48778=EDGE_CURVE('',#39061,#39062,#789,.T.);
#48779=EDGE_CURVE('',#39062,#39063,#21150,.T.);
#48780=EDGE_CURVE('',#39063,#39052,#21151,.T.);
#48781=EDGE_CURVE('',#39064,#39065,#21152,.T.);
#48782=EDGE_CURVE('',#39065,#39066,#31684,.T.);
#48783=EDGE_CURVE('',#39066,#39067,#21153,.T.);
#48784=EDGE_CURVE('',#39067,#39064,#31685,.T.);
#48785=EDGE_CURVE('',#39068,#39069,#790,.T.);
#48786=EDGE_CURVE('',#39069,#39070,#21154,.T.);
#48787=EDGE_CURVE('',#39070,#39071,#21155,.T.);
#48788=EDGE_CURVE('',#39071,#39072,#21156,.T.);
#48789=EDGE_CURVE('',#39072,#39073,#791,.T.);
#48790=EDGE_CURVE('',#39073,#39074,#21157,.T.);
#48791=EDGE_CURVE('',#39074,#39075,#21158,.T.);
#48792=EDGE_CURVE('',#39075,#39076,#792,.T.);
#48793=EDGE_CURVE('',#39076,#39077,#21159,.T.);
#48794=EDGE_CURVE('',#39077,#39078,#793,.T.);
#48795=EDGE_CURVE('',#39078,#39079,#21160,.T.);
#48796=EDGE_CURVE('',#39079,#39068,#21161,.T.);
#48797=EDGE_CURVE('',#39080,#39081,#794,.T.);
#48798=EDGE_CURVE('',#39081,#39082,#21162,.T.);
#48799=EDGE_CURVE('',#39082,#39083,#21163,.T.);
#48800=EDGE_CURVE('',#39083,#39084,#21164,.T.);
#48801=EDGE_CURVE('',#39084,#39085,#795,.T.);
#48802=EDGE_CURVE('',#39085,#39086,#21165,.T.);
#48803=EDGE_CURVE('',#39086,#39087,#21166,.T.);
#48804=EDGE_CURVE('',#39087,#39088,#796,.T.);
#48805=EDGE_CURVE('',#39088,#39089,#21167,.T.);
#48806=EDGE_CURVE('',#39089,#39090,#797,.T.);
#48807=EDGE_CURVE('',#39090,#39091,#21168,.T.);
#48808=EDGE_CURVE('',#39091,#39080,#21169,.T.);
#48809=EDGE_CURVE('',#39092,#39093,#21170,.T.);
#48810=EDGE_CURVE('',#39093,#39094,#31686,.T.);
#48811=EDGE_CURVE('',#39094,#39095,#21171,.T.);
#48812=EDGE_CURVE('',#39095,#39092,#31687,.T.);
#48813=EDGE_CURVE('',#39096,#39097,#798,.T.);
#48814=EDGE_CURVE('',#39097,#39098,#21172,.T.);
#48815=EDGE_CURVE('',#39098,#39099,#21173,.T.);
#48816=EDGE_CURVE('',#39099,#39100,#21174,.T.);
#48817=EDGE_CURVE('',#39100,#39101,#799,.T.);
#48818=EDGE_CURVE('',#39101,#39102,#21175,.T.);
#48819=EDGE_CURVE('',#39102,#39103,#21176,.T.);
#48820=EDGE_CURVE('',#39103,#39104,#800,.T.);
#48821=EDGE_CURVE('',#39104,#39105,#21177,.T.);
#48822=EDGE_CURVE('',#39105,#39106,#801,.T.);
#48823=EDGE_CURVE('',#39106,#39107,#21178,.T.);
#48824=EDGE_CURVE('',#39107,#39096,#21179,.T.);
#48825=EDGE_CURVE('',#39108,#39109,#802,.T.);
#48826=EDGE_CURVE('',#39109,#39110,#21180,.T.);
#48827=EDGE_CURVE('',#39110,#39111,#21181,.T.);
#48828=EDGE_CURVE('',#39111,#39112,#21182,.T.);
#48829=EDGE_CURVE('',#39112,#39113,#803,.T.);
#48830=EDGE_CURVE('',#39113,#39114,#21183,.T.);
#48831=EDGE_CURVE('',#39114,#39115,#21184,.T.);
#48832=EDGE_CURVE('',#39115,#39116,#804,.T.);
#48833=EDGE_CURVE('',#39116,#39117,#21185,.T.);
#48834=EDGE_CURVE('',#39117,#39118,#805,.T.);
#48835=EDGE_CURVE('',#39118,#39119,#21186,.T.);
#48836=EDGE_CURVE('',#39119,#39108,#21187,.T.);
#48837=EDGE_CURVE('',#39120,#39121,#21188,.T.);
#48838=EDGE_CURVE('',#39121,#39122,#31688,.T.);
#48839=EDGE_CURVE('',#39122,#39123,#21189,.T.);
#48840=EDGE_CURVE('',#39123,#39120,#31689,.T.);
#48841=EDGE_CURVE('',#39124,#39125,#806,.T.);
#48842=EDGE_CURVE('',#39125,#39126,#21190,.T.);
#48843=EDGE_CURVE('',#39126,#39127,#21191,.T.);
#48844=EDGE_CURVE('',#39127,#39128,#21192,.T.);
#48845=EDGE_CURVE('',#39128,#39129,#807,.T.);
#48846=EDGE_CURVE('',#39129,#39130,#21193,.T.);
#48847=EDGE_CURVE('',#39130,#39131,#21194,.T.);
#48848=EDGE_CURVE('',#39131,#39132,#808,.T.);
#48849=EDGE_CURVE('',#39132,#39133,#21195,.T.);
#48850=EDGE_CURVE('',#39133,#39134,#809,.T.);
#48851=EDGE_CURVE('',#39134,#39135,#21196,.T.);
#48852=EDGE_CURVE('',#39135,#39124,#21197,.T.);
#48853=EDGE_CURVE('',#39136,#39137,#810,.T.);
#48854=EDGE_CURVE('',#39137,#39138,#21198,.T.);
#48855=EDGE_CURVE('',#39138,#39139,#21199,.T.);
#48856=EDGE_CURVE('',#39139,#39140,#21200,.T.);
#48857=EDGE_CURVE('',#39140,#39141,#811,.T.);
#48858=EDGE_CURVE('',#39141,#39142,#21201,.T.);
#48859=EDGE_CURVE('',#39142,#39143,#21202,.T.);
#48860=EDGE_CURVE('',#39143,#39144,#812,.T.);
#48861=EDGE_CURVE('',#39144,#39145,#21203,.T.);
#48862=EDGE_CURVE('',#39145,#39146,#813,.T.);
#48863=EDGE_CURVE('',#39146,#39147,#21204,.T.);
#48864=EDGE_CURVE('',#39147,#39136,#21205,.T.);
#48865=EDGE_CURVE('',#39148,#39149,#21206,.T.);
#48866=EDGE_CURVE('',#39149,#39150,#31690,.T.);
#48867=EDGE_CURVE('',#39150,#39151,#21207,.T.);
#48868=EDGE_CURVE('',#39151,#39148,#31691,.T.);
#48869=EDGE_CURVE('',#39152,#39153,#814,.T.);
#48870=EDGE_CURVE('',#39153,#39154,#21208,.T.);
#48871=EDGE_CURVE('',#39154,#39155,#21209,.T.);
#48872=EDGE_CURVE('',#39155,#39156,#21210,.T.);
#48873=EDGE_CURVE('',#39156,#39157,#815,.T.);
#48874=EDGE_CURVE('',#39157,#39158,#21211,.T.);
#48875=EDGE_CURVE('',#39158,#39159,#21212,.T.);
#48876=EDGE_CURVE('',#39159,#39160,#816,.T.);
#48877=EDGE_CURVE('',#39160,#39161,#21213,.T.);
#48878=EDGE_CURVE('',#39161,#39162,#817,.T.);
#48879=EDGE_CURVE('',#39162,#39163,#21214,.T.);
#48880=EDGE_CURVE('',#39163,#39152,#21215,.T.);
#48881=EDGE_CURVE('',#39164,#39165,#818,.T.);
#48882=EDGE_CURVE('',#39165,#39166,#21216,.T.);
#48883=EDGE_CURVE('',#39166,#39167,#21217,.T.);
#48884=EDGE_CURVE('',#39167,#39168,#21218,.T.);
#48885=EDGE_CURVE('',#39168,#39169,#819,.T.);
#48886=EDGE_CURVE('',#39169,#39170,#21219,.T.);
#48887=EDGE_CURVE('',#39170,#39171,#21220,.T.);
#48888=EDGE_CURVE('',#39171,#39172,#820,.T.);
#48889=EDGE_CURVE('',#39172,#39173,#21221,.T.);
#48890=EDGE_CURVE('',#39173,#39174,#821,.T.);
#48891=EDGE_CURVE('',#39174,#39175,#21222,.T.);
#48892=EDGE_CURVE('',#39175,#39164,#21223,.T.);
#48893=EDGE_CURVE('',#39176,#39177,#21224,.T.);
#48894=EDGE_CURVE('',#39177,#39178,#31692,.T.);
#48895=EDGE_CURVE('',#39178,#39179,#21225,.T.);
#48896=EDGE_CURVE('',#39179,#39176,#31693,.T.);
#48897=EDGE_CURVE('',#39180,#39181,#822,.T.);
#48898=EDGE_CURVE('',#39181,#39182,#21226,.T.);
#48899=EDGE_CURVE('',#39182,#39183,#21227,.T.);
#48900=EDGE_CURVE('',#39183,#39184,#21228,.T.);
#48901=EDGE_CURVE('',#39184,#39185,#823,.T.);
#48902=EDGE_CURVE('',#39185,#39186,#21229,.T.);
#48903=EDGE_CURVE('',#39186,#39187,#21230,.T.);
#48904=EDGE_CURVE('',#39187,#39188,#824,.T.);
#48905=EDGE_CURVE('',#39188,#39189,#21231,.T.);
#48906=EDGE_CURVE('',#39189,#39190,#825,.T.);
#48907=EDGE_CURVE('',#39190,#39191,#21232,.T.);
#48908=EDGE_CURVE('',#39191,#39180,#21233,.T.);
#48909=EDGE_CURVE('',#39192,#39193,#826,.T.);
#48910=EDGE_CURVE('',#39193,#39194,#21234,.T.);
#48911=EDGE_CURVE('',#39194,#39195,#21235,.T.);
#48912=EDGE_CURVE('',#39195,#39196,#21236,.T.);
#48913=EDGE_CURVE('',#39196,#39197,#827,.T.);
#48914=EDGE_CURVE('',#39197,#39198,#21237,.T.);
#48915=EDGE_CURVE('',#39198,#39199,#21238,.T.);
#48916=EDGE_CURVE('',#39199,#39200,#828,.T.);
#48917=EDGE_CURVE('',#39200,#39201,#21239,.T.);
#48918=EDGE_CURVE('',#39201,#39202,#829,.T.);
#48919=EDGE_CURVE('',#39202,#39203,#21240,.T.);
#48920=EDGE_CURVE('',#39203,#39192,#21241,.T.);
#48921=EDGE_CURVE('',#39204,#39205,#21242,.T.);
#48922=EDGE_CURVE('',#39205,#39206,#31694,.T.);
#48923=EDGE_CURVE('',#39206,#39207,#21243,.T.);
#48924=EDGE_CURVE('',#39207,#39204,#31695,.T.);
#48925=EDGE_CURVE('',#39208,#39209,#830,.T.);
#48926=EDGE_CURVE('',#39209,#39210,#21244,.T.);
#48927=EDGE_CURVE('',#39210,#39211,#21245,.T.);
#48928=EDGE_CURVE('',#39211,#39212,#21246,.T.);
#48929=EDGE_CURVE('',#39212,#39213,#831,.T.);
#48930=EDGE_CURVE('',#39213,#39214,#21247,.T.);
#48931=EDGE_CURVE('',#39214,#39215,#21248,.T.);
#48932=EDGE_CURVE('',#39215,#39216,#832,.T.);
#48933=EDGE_CURVE('',#39216,#39217,#21249,.T.);
#48934=EDGE_CURVE('',#39217,#39218,#833,.T.);
#48935=EDGE_CURVE('',#39218,#39219,#21250,.T.);
#48936=EDGE_CURVE('',#39219,#39208,#21251,.T.);
#48937=EDGE_CURVE('',#39220,#39221,#834,.T.);
#48938=EDGE_CURVE('',#39221,#39222,#21252,.T.);
#48939=EDGE_CURVE('',#39222,#39223,#21253,.T.);
#48940=EDGE_CURVE('',#39223,#39224,#21254,.T.);
#48941=EDGE_CURVE('',#39224,#39225,#835,.T.);
#48942=EDGE_CURVE('',#39225,#39226,#21255,.T.);
#48943=EDGE_CURVE('',#39226,#39227,#21256,.T.);
#48944=EDGE_CURVE('',#39227,#39228,#836,.T.);
#48945=EDGE_CURVE('',#39228,#39229,#21257,.T.);
#48946=EDGE_CURVE('',#39229,#39230,#837,.T.);
#48947=EDGE_CURVE('',#39230,#39231,#21258,.T.);
#48948=EDGE_CURVE('',#39231,#39220,#21259,.T.);
#48949=EDGE_CURVE('',#39232,#39233,#21260,.T.);
#48950=EDGE_CURVE('',#39233,#39234,#31696,.T.);
#48951=EDGE_CURVE('',#39234,#39235,#21261,.T.);
#48952=EDGE_CURVE('',#39235,#39232,#31697,.T.);
#48953=EDGE_CURVE('',#39236,#39237,#838,.T.);
#48954=EDGE_CURVE('',#39237,#39238,#21262,.T.);
#48955=EDGE_CURVE('',#39238,#39239,#21263,.T.);
#48956=EDGE_CURVE('',#39239,#39240,#21264,.T.);
#48957=EDGE_CURVE('',#39240,#39241,#839,.T.);
#48958=EDGE_CURVE('',#39241,#39242,#21265,.T.);
#48959=EDGE_CURVE('',#39242,#39243,#21266,.T.);
#48960=EDGE_CURVE('',#39243,#39244,#840,.T.);
#48961=EDGE_CURVE('',#39244,#39245,#21267,.T.);
#48962=EDGE_CURVE('',#39245,#39246,#841,.T.);
#48963=EDGE_CURVE('',#39246,#39247,#21268,.T.);
#48964=EDGE_CURVE('',#39247,#39236,#21269,.T.);
#48965=EDGE_CURVE('',#39248,#39249,#842,.T.);
#48966=EDGE_CURVE('',#39249,#39250,#21270,.T.);
#48967=EDGE_CURVE('',#39250,#39251,#21271,.T.);
#48968=EDGE_CURVE('',#39251,#39252,#21272,.T.);
#48969=EDGE_CURVE('',#39252,#39253,#843,.T.);
#48970=EDGE_CURVE('',#39253,#39254,#21273,.T.);
#48971=EDGE_CURVE('',#39254,#39255,#21274,.T.);
#48972=EDGE_CURVE('',#39255,#39256,#844,.T.);
#48973=EDGE_CURVE('',#39256,#39257,#21275,.T.);
#48974=EDGE_CURVE('',#39257,#39258,#845,.T.);
#48975=EDGE_CURVE('',#39258,#39259,#21276,.T.);
#48976=EDGE_CURVE('',#39259,#39248,#21277,.T.);
#48977=EDGE_CURVE('',#39260,#39261,#21278,.T.);
#48978=EDGE_CURVE('',#39261,#39262,#31698,.T.);
#48979=EDGE_CURVE('',#39262,#39263,#21279,.T.);
#48980=EDGE_CURVE('',#39263,#39260,#31699,.T.);
#48981=EDGE_CURVE('',#39264,#39265,#846,.T.);
#48982=EDGE_CURVE('',#39265,#39266,#21280,.T.);
#48983=EDGE_CURVE('',#39266,#39267,#21281,.T.);
#48984=EDGE_CURVE('',#39267,#39268,#21282,.T.);
#48985=EDGE_CURVE('',#39268,#39269,#847,.T.);
#48986=EDGE_CURVE('',#39269,#39270,#21283,.T.);
#48987=EDGE_CURVE('',#39270,#39271,#21284,.T.);
#48988=EDGE_CURVE('',#39271,#39272,#848,.T.);
#48989=EDGE_CURVE('',#39272,#39273,#21285,.T.);
#48990=EDGE_CURVE('',#39273,#39274,#849,.T.);
#48991=EDGE_CURVE('',#39274,#39275,#21286,.T.);
#48992=EDGE_CURVE('',#39275,#39264,#21287,.T.);
#48993=EDGE_CURVE('',#39276,#39277,#850,.T.);
#48994=EDGE_CURVE('',#39277,#39278,#21288,.T.);
#48995=EDGE_CURVE('',#39278,#39279,#21289,.T.);
#48996=EDGE_CURVE('',#39279,#39280,#21290,.T.);
#48997=EDGE_CURVE('',#39280,#39281,#851,.T.);
#48998=EDGE_CURVE('',#39281,#39282,#21291,.T.);
#48999=EDGE_CURVE('',#39282,#39283,#21292,.T.);
#49000=EDGE_CURVE('',#39283,#39284,#852,.T.);
#49001=EDGE_CURVE('',#39284,#39285,#21293,.T.);
#49002=EDGE_CURVE('',#39285,#39286,#853,.T.);
#49003=EDGE_CURVE('',#39286,#39287,#21294,.T.);
#49004=EDGE_CURVE('',#39287,#39276,#21295,.T.);
#49005=EDGE_CURVE('',#39288,#39289,#21296,.T.);
#49006=EDGE_CURVE('',#39289,#39290,#31700,.T.);
#49007=EDGE_CURVE('',#39290,#39291,#21297,.T.);
#49008=EDGE_CURVE('',#39291,#39288,#31701,.T.);
#49009=EDGE_CURVE('',#39292,#39293,#854,.T.);
#49010=EDGE_CURVE('',#39293,#39294,#21298,.T.);
#49011=EDGE_CURVE('',#39294,#39295,#21299,.T.);
#49012=EDGE_CURVE('',#39295,#39296,#21300,.T.);
#49013=EDGE_CURVE('',#39296,#39297,#855,.T.);
#49014=EDGE_CURVE('',#39297,#39298,#21301,.T.);
#49015=EDGE_CURVE('',#39298,#39299,#21302,.T.);
#49016=EDGE_CURVE('',#39299,#39300,#856,.T.);
#49017=EDGE_CURVE('',#39300,#39301,#21303,.T.);
#49018=EDGE_CURVE('',#39301,#39302,#857,.T.);
#49019=EDGE_CURVE('',#39302,#39303,#21304,.T.);
#49020=EDGE_CURVE('',#39303,#39292,#21305,.T.);
#49021=EDGE_CURVE('',#39304,#39305,#858,.T.);
#49022=EDGE_CURVE('',#39305,#39306,#21306,.T.);
#49023=EDGE_CURVE('',#39306,#39307,#21307,.T.);
#49024=EDGE_CURVE('',#39307,#39308,#21308,.T.);
#49025=EDGE_CURVE('',#39308,#39309,#859,.T.);
#49026=EDGE_CURVE('',#39309,#39310,#21309,.T.);
#49027=EDGE_CURVE('',#39310,#39311,#21310,.T.);
#49028=EDGE_CURVE('',#39311,#39312,#860,.T.);
#49029=EDGE_CURVE('',#39312,#39313,#21311,.T.);
#49030=EDGE_CURVE('',#39313,#39314,#861,.T.);
#49031=EDGE_CURVE('',#39314,#39315,#21312,.T.);
#49032=EDGE_CURVE('',#39315,#39304,#21313,.T.);
#49033=EDGE_CURVE('',#39316,#39317,#21314,.T.);
#49034=EDGE_CURVE('',#39317,#39318,#31702,.T.);
#49035=EDGE_CURVE('',#39318,#39319,#21315,.T.);
#49036=EDGE_CURVE('',#39319,#39316,#31703,.T.);
#49037=EDGE_CURVE('',#39320,#39321,#862,.T.);
#49038=EDGE_CURVE('',#39321,#39322,#21316,.T.);
#49039=EDGE_CURVE('',#39322,#39323,#21317,.T.);
#49040=EDGE_CURVE('',#39323,#39324,#21318,.T.);
#49041=EDGE_CURVE('',#39324,#39325,#863,.T.);
#49042=EDGE_CURVE('',#39325,#39326,#21319,.T.);
#49043=EDGE_CURVE('',#39326,#39327,#21320,.T.);
#49044=EDGE_CURVE('',#39327,#39328,#864,.T.);
#49045=EDGE_CURVE('',#39328,#39329,#21321,.T.);
#49046=EDGE_CURVE('',#39329,#39330,#865,.T.);
#49047=EDGE_CURVE('',#39330,#39331,#21322,.T.);
#49048=EDGE_CURVE('',#39331,#39320,#21323,.T.);
#49049=EDGE_CURVE('',#39332,#39333,#866,.T.);
#49050=EDGE_CURVE('',#39333,#39334,#21324,.T.);
#49051=EDGE_CURVE('',#39334,#39335,#21325,.T.);
#49052=EDGE_CURVE('',#39335,#39336,#21326,.T.);
#49053=EDGE_CURVE('',#39336,#39337,#867,.T.);
#49054=EDGE_CURVE('',#39337,#39338,#21327,.T.);
#49055=EDGE_CURVE('',#39338,#39339,#21328,.T.);
#49056=EDGE_CURVE('',#39339,#39340,#868,.T.);
#49057=EDGE_CURVE('',#39340,#39341,#21329,.T.);
#49058=EDGE_CURVE('',#39341,#39342,#869,.T.);
#49059=EDGE_CURVE('',#39342,#39343,#21330,.T.);
#49060=EDGE_CURVE('',#39343,#39332,#21331,.T.);
#49061=EDGE_CURVE('',#39344,#39345,#21332,.T.);
#49062=EDGE_CURVE('',#39345,#39346,#31704,.T.);
#49063=EDGE_CURVE('',#39346,#39347,#21333,.T.);
#49064=EDGE_CURVE('',#39347,#39344,#31705,.T.);
#49065=EDGE_CURVE('',#39348,#39349,#870,.T.);
#49066=EDGE_CURVE('',#39349,#39350,#21334,.T.);
#49067=EDGE_CURVE('',#39350,#39351,#21335,.T.);
#49068=EDGE_CURVE('',#39351,#39352,#21336,.T.);
#49069=EDGE_CURVE('',#39352,#39353,#871,.T.);
#49070=EDGE_CURVE('',#39353,#39354,#21337,.T.);
#49071=EDGE_CURVE('',#39354,#39355,#21338,.T.);
#49072=EDGE_CURVE('',#39355,#39356,#872,.T.);
#49073=EDGE_CURVE('',#39356,#39357,#21339,.T.);
#49074=EDGE_CURVE('',#39357,#39358,#873,.T.);
#49075=EDGE_CURVE('',#39358,#39359,#21340,.T.);
#49076=EDGE_CURVE('',#39359,#39348,#21341,.T.);
#49077=EDGE_CURVE('',#39360,#39361,#874,.T.);
#49078=EDGE_CURVE('',#39361,#39362,#21342,.T.);
#49079=EDGE_CURVE('',#39362,#39363,#21343,.T.);
#49080=EDGE_CURVE('',#39363,#39364,#21344,.T.);
#49081=EDGE_CURVE('',#39364,#39365,#875,.T.);
#49082=EDGE_CURVE('',#39365,#39366,#21345,.T.);
#49083=EDGE_CURVE('',#39366,#39367,#21346,.T.);
#49084=EDGE_CURVE('',#39367,#39368,#876,.T.);
#49085=EDGE_CURVE('',#39368,#39369,#21347,.T.);
#49086=EDGE_CURVE('',#39369,#39370,#877,.T.);
#49087=EDGE_CURVE('',#39370,#39371,#21348,.T.);
#49088=EDGE_CURVE('',#39371,#39360,#21349,.T.);
#49089=EDGE_CURVE('',#39372,#39373,#21350,.T.);
#49090=EDGE_CURVE('',#39373,#39374,#31706,.T.);
#49091=EDGE_CURVE('',#39374,#39375,#21351,.T.);
#49092=EDGE_CURVE('',#39375,#39372,#31707,.T.);
#49093=EDGE_CURVE('',#39376,#39377,#878,.T.);
#49094=EDGE_CURVE('',#39377,#39378,#21352,.T.);
#49095=EDGE_CURVE('',#39378,#39379,#21353,.T.);
#49096=EDGE_CURVE('',#39379,#39380,#21354,.T.);
#49097=EDGE_CURVE('',#39380,#39381,#879,.T.);
#49098=EDGE_CURVE('',#39381,#39382,#21355,.T.);
#49099=EDGE_CURVE('',#39382,#39383,#21356,.T.);
#49100=EDGE_CURVE('',#39383,#39384,#880,.T.);
#49101=EDGE_CURVE('',#39384,#39385,#21357,.T.);
#49102=EDGE_CURVE('',#39385,#39386,#881,.T.);
#49103=EDGE_CURVE('',#39386,#39387,#21358,.T.);
#49104=EDGE_CURVE('',#39387,#39376,#21359,.T.);
#49105=EDGE_CURVE('',#39388,#39389,#882,.T.);
#49106=EDGE_CURVE('',#39389,#39390,#21360,.T.);
#49107=EDGE_CURVE('',#39390,#39391,#21361,.T.);
#49108=EDGE_CURVE('',#39391,#39392,#21362,.T.);
#49109=EDGE_CURVE('',#39392,#39393,#883,.T.);
#49110=EDGE_CURVE('',#39393,#39394,#21363,.T.);
#49111=EDGE_CURVE('',#39394,#39395,#21364,.T.);
#49112=EDGE_CURVE('',#39395,#39396,#884,.T.);
#49113=EDGE_CURVE('',#39396,#39397,#21365,.T.);
#49114=EDGE_CURVE('',#39397,#39398,#885,.T.);
#49115=EDGE_CURVE('',#39398,#39399,#21366,.T.);
#49116=EDGE_CURVE('',#39399,#39388,#21367,.T.);
#49117=EDGE_CURVE('',#39400,#39401,#21368,.T.);
#49118=EDGE_CURVE('',#39401,#39402,#31708,.T.);
#49119=EDGE_CURVE('',#39402,#39403,#21369,.T.);
#49120=EDGE_CURVE('',#39403,#39400,#31709,.T.);
#49121=EDGE_CURVE('',#39404,#39405,#886,.T.);
#49122=EDGE_CURVE('',#39405,#39406,#21370,.T.);
#49123=EDGE_CURVE('',#39406,#39407,#21371,.T.);
#49124=EDGE_CURVE('',#39407,#39408,#21372,.T.);
#49125=EDGE_CURVE('',#39408,#39409,#887,.T.);
#49126=EDGE_CURVE('',#39409,#39410,#21373,.T.);
#49127=EDGE_CURVE('',#39410,#39411,#21374,.T.);
#49128=EDGE_CURVE('',#39411,#39412,#888,.T.);
#49129=EDGE_CURVE('',#39412,#39413,#21375,.T.);
#49130=EDGE_CURVE('',#39413,#39414,#889,.T.);
#49131=EDGE_CURVE('',#39414,#39415,#21376,.T.);
#49132=EDGE_CURVE('',#39415,#39404,#21377,.T.);
#49133=EDGE_CURVE('',#39416,#39417,#890,.T.);
#49134=EDGE_CURVE('',#39417,#39418,#21378,.T.);
#49135=EDGE_CURVE('',#39418,#39419,#21379,.T.);
#49136=EDGE_CURVE('',#39419,#39420,#21380,.T.);
#49137=EDGE_CURVE('',#39420,#39421,#891,.T.);
#49138=EDGE_CURVE('',#39421,#39422,#21381,.T.);
#49139=EDGE_CURVE('',#39422,#39423,#21382,.T.);
#49140=EDGE_CURVE('',#39423,#39424,#892,.T.);
#49141=EDGE_CURVE('',#39424,#39425,#21383,.T.);
#49142=EDGE_CURVE('',#39425,#39426,#893,.T.);
#49143=EDGE_CURVE('',#39426,#39427,#21384,.T.);
#49144=EDGE_CURVE('',#39427,#39416,#21385,.T.);
#49145=EDGE_CURVE('',#39428,#39429,#21386,.T.);
#49146=EDGE_CURVE('',#39429,#39430,#31710,.T.);
#49147=EDGE_CURVE('',#39430,#39431,#21387,.T.);
#49148=EDGE_CURVE('',#39431,#39428,#31711,.T.);
#49149=EDGE_CURVE('',#39432,#39433,#894,.T.);
#49150=EDGE_CURVE('',#39433,#39434,#21388,.T.);
#49151=EDGE_CURVE('',#39434,#39435,#21389,.T.);
#49152=EDGE_CURVE('',#39435,#39436,#21390,.T.);
#49153=EDGE_CURVE('',#39436,#39437,#895,.T.);
#49154=EDGE_CURVE('',#39437,#39438,#21391,.T.);
#49155=EDGE_CURVE('',#39438,#39439,#21392,.T.);
#49156=EDGE_CURVE('',#39439,#39440,#896,.T.);
#49157=EDGE_CURVE('',#39440,#39441,#21393,.T.);
#49158=EDGE_CURVE('',#39441,#39442,#897,.T.);
#49159=EDGE_CURVE('',#39442,#39443,#21394,.T.);
#49160=EDGE_CURVE('',#39443,#39432,#21395,.T.);
#49161=EDGE_CURVE('',#39444,#39445,#898,.T.);
#49162=EDGE_CURVE('',#39445,#39446,#21396,.T.);
#49163=EDGE_CURVE('',#39446,#39447,#21397,.T.);
#49164=EDGE_CURVE('',#39447,#39448,#21398,.T.);
#49165=EDGE_CURVE('',#39448,#39449,#899,.T.);
#49166=EDGE_CURVE('',#39449,#39450,#21399,.T.);
#49167=EDGE_CURVE('',#39450,#39451,#21400,.T.);
#49168=EDGE_CURVE('',#39451,#39452,#900,.T.);
#49169=EDGE_CURVE('',#39452,#39453,#21401,.T.);
#49170=EDGE_CURVE('',#39453,#39454,#901,.T.);
#49171=EDGE_CURVE('',#39454,#39455,#21402,.T.);
#49172=EDGE_CURVE('',#39455,#39444,#21403,.T.);
#49173=EDGE_CURVE('',#39456,#39457,#21404,.T.);
#49174=EDGE_CURVE('',#39457,#39458,#31712,.T.);
#49175=EDGE_CURVE('',#39458,#39459,#21405,.T.);
#49176=EDGE_CURVE('',#39459,#39456,#31713,.T.);
#49177=EDGE_CURVE('',#39460,#39461,#902,.T.);
#49178=EDGE_CURVE('',#39461,#39462,#21406,.T.);
#49179=EDGE_CURVE('',#39462,#39463,#21407,.T.);
#49180=EDGE_CURVE('',#39463,#39464,#21408,.T.);
#49181=EDGE_CURVE('',#39464,#39465,#903,.T.);
#49182=EDGE_CURVE('',#39465,#39466,#21409,.T.);
#49183=EDGE_CURVE('',#39466,#39467,#21410,.T.);
#49184=EDGE_CURVE('',#39467,#39468,#904,.T.);
#49185=EDGE_CURVE('',#39468,#39469,#21411,.T.);
#49186=EDGE_CURVE('',#39469,#39470,#905,.T.);
#49187=EDGE_CURVE('',#39470,#39471,#21412,.T.);
#49188=EDGE_CURVE('',#39471,#39460,#21413,.T.);
#49189=EDGE_CURVE('',#39472,#39473,#906,.T.);
#49190=EDGE_CURVE('',#39473,#39474,#21414,.T.);
#49191=EDGE_CURVE('',#39474,#39475,#21415,.T.);
#49192=EDGE_CURVE('',#39475,#39476,#21416,.T.);
#49193=EDGE_CURVE('',#39476,#39477,#907,.T.);
#49194=EDGE_CURVE('',#39477,#39478,#21417,.T.);
#49195=EDGE_CURVE('',#39478,#39479,#21418,.T.);
#49196=EDGE_CURVE('',#39479,#39480,#908,.T.);
#49197=EDGE_CURVE('',#39480,#39481,#21419,.T.);
#49198=EDGE_CURVE('',#39481,#39482,#909,.T.);
#49199=EDGE_CURVE('',#39482,#39483,#21420,.T.);
#49200=EDGE_CURVE('',#39483,#39472,#21421,.T.);
#49201=EDGE_CURVE('',#39484,#39485,#21422,.T.);
#49202=EDGE_CURVE('',#39485,#39486,#31714,.T.);
#49203=EDGE_CURVE('',#39486,#39487,#21423,.T.);
#49204=EDGE_CURVE('',#39487,#39484,#31715,.T.);
#49205=EDGE_CURVE('',#39488,#39489,#910,.T.);
#49206=EDGE_CURVE('',#39489,#39490,#21424,.T.);
#49207=EDGE_CURVE('',#39490,#39491,#21425,.T.);
#49208=EDGE_CURVE('',#39491,#39492,#21426,.T.);
#49209=EDGE_CURVE('',#39492,#39493,#911,.T.);
#49210=EDGE_CURVE('',#39493,#39494,#21427,.T.);
#49211=EDGE_CURVE('',#39494,#39495,#21428,.T.);
#49212=EDGE_CURVE('',#39495,#39496,#912,.T.);
#49213=EDGE_CURVE('',#39496,#39497,#21429,.T.);
#49214=EDGE_CURVE('',#39497,#39498,#913,.T.);
#49215=EDGE_CURVE('',#39498,#39499,#21430,.T.);
#49216=EDGE_CURVE('',#39499,#39488,#21431,.T.);
#49217=EDGE_CURVE('',#39500,#39501,#914,.T.);
#49218=EDGE_CURVE('',#39501,#39502,#21432,.T.);
#49219=EDGE_CURVE('',#39502,#39503,#21433,.T.);
#49220=EDGE_CURVE('',#39503,#39504,#21434,.T.);
#49221=EDGE_CURVE('',#39504,#39505,#915,.T.);
#49222=EDGE_CURVE('',#39505,#39506,#21435,.T.);
#49223=EDGE_CURVE('',#39506,#39507,#21436,.T.);
#49224=EDGE_CURVE('',#39507,#39508,#916,.T.);
#49225=EDGE_CURVE('',#39508,#39509,#21437,.T.);
#49226=EDGE_CURVE('',#39509,#39510,#917,.T.);
#49227=EDGE_CURVE('',#39510,#39511,#21438,.T.);
#49228=EDGE_CURVE('',#39511,#39500,#21439,.T.);
#49229=EDGE_CURVE('',#39512,#39513,#21440,.T.);
#49230=EDGE_CURVE('',#39513,#39514,#31716,.T.);
#49231=EDGE_CURVE('',#39514,#39515,#21441,.T.);
#49232=EDGE_CURVE('',#39515,#39512,#31717,.T.);
#49233=EDGE_CURVE('',#39516,#39517,#918,.T.);
#49234=EDGE_CURVE('',#39517,#39518,#21442,.T.);
#49235=EDGE_CURVE('',#39518,#39519,#21443,.T.);
#49236=EDGE_CURVE('',#39519,#39520,#21444,.T.);
#49237=EDGE_CURVE('',#39520,#39521,#919,.T.);
#49238=EDGE_CURVE('',#39521,#39522,#21445,.T.);
#49239=EDGE_CURVE('',#39522,#39523,#21446,.T.);
#49240=EDGE_CURVE('',#39523,#39524,#920,.T.);
#49241=EDGE_CURVE('',#39524,#39525,#21447,.T.);
#49242=EDGE_CURVE('',#39525,#39526,#921,.T.);
#49243=EDGE_CURVE('',#39526,#39527,#21448,.T.);
#49244=EDGE_CURVE('',#39527,#39516,#21449,.T.);
#49245=EDGE_CURVE('',#39528,#39529,#922,.T.);
#49246=EDGE_CURVE('',#39529,#39530,#21450,.T.);
#49247=EDGE_CURVE('',#39530,#39531,#21451,.T.);
#49248=EDGE_CURVE('',#39531,#39532,#21452,.T.);
#49249=EDGE_CURVE('',#39532,#39533,#923,.T.);
#49250=EDGE_CURVE('',#39533,#39534,#21453,.T.);
#49251=EDGE_CURVE('',#39534,#39535,#21454,.T.);
#49252=EDGE_CURVE('',#39535,#39536,#924,.T.);
#49253=EDGE_CURVE('',#39536,#39537,#21455,.T.);
#49254=EDGE_CURVE('',#39537,#39538,#925,.T.);
#49255=EDGE_CURVE('',#39538,#39539,#21456,.T.);
#49256=EDGE_CURVE('',#39539,#39528,#21457,.T.);
#49257=EDGE_CURVE('',#39540,#39541,#21458,.T.);
#49258=EDGE_CURVE('',#39541,#39542,#31718,.T.);
#49259=EDGE_CURVE('',#39542,#39543,#21459,.T.);
#49260=EDGE_CURVE('',#39543,#39540,#31719,.T.);
#49261=EDGE_CURVE('',#39544,#39545,#926,.T.);
#49262=EDGE_CURVE('',#39545,#39546,#21460,.T.);
#49263=EDGE_CURVE('',#39546,#39547,#21461,.T.);
#49264=EDGE_CURVE('',#39547,#39548,#21462,.T.);
#49265=EDGE_CURVE('',#39548,#39549,#927,.T.);
#49266=EDGE_CURVE('',#39549,#39550,#21463,.T.);
#49267=EDGE_CURVE('',#39550,#39551,#21464,.T.);
#49268=EDGE_CURVE('',#39551,#39552,#928,.T.);
#49269=EDGE_CURVE('',#39552,#39553,#21465,.T.);
#49270=EDGE_CURVE('',#39553,#39554,#929,.T.);
#49271=EDGE_CURVE('',#39554,#39555,#21466,.T.);
#49272=EDGE_CURVE('',#39555,#39544,#21467,.T.);
#49273=EDGE_CURVE('',#39556,#39557,#930,.T.);
#49274=EDGE_CURVE('',#39557,#39558,#21468,.T.);
#49275=EDGE_CURVE('',#39558,#39559,#21469,.T.);
#49276=EDGE_CURVE('',#39559,#39560,#21470,.T.);
#49277=EDGE_CURVE('',#39560,#39561,#931,.T.);
#49278=EDGE_CURVE('',#39561,#39562,#21471,.T.);
#49279=EDGE_CURVE('',#39562,#39563,#21472,.T.);
#49280=EDGE_CURVE('',#39563,#39564,#932,.T.);
#49281=EDGE_CURVE('',#39564,#39565,#21473,.T.);
#49282=EDGE_CURVE('',#39565,#39566,#933,.T.);
#49283=EDGE_CURVE('',#39566,#39567,#21474,.T.);
#49284=EDGE_CURVE('',#39567,#39556,#21475,.T.);
#49285=EDGE_CURVE('',#39568,#39569,#21476,.T.);
#49286=EDGE_CURVE('',#39569,#39570,#31720,.T.);
#49287=EDGE_CURVE('',#39570,#39571,#21477,.T.);
#49288=EDGE_CURVE('',#39571,#39568,#31721,.T.);
#49289=EDGE_CURVE('',#39572,#39573,#934,.T.);
#49290=EDGE_CURVE('',#39573,#39574,#21478,.T.);
#49291=EDGE_CURVE('',#39574,#39575,#21479,.T.);
#49292=EDGE_CURVE('',#39575,#39576,#21480,.T.);
#49293=EDGE_CURVE('',#39576,#39577,#935,.T.);
#49294=EDGE_CURVE('',#39577,#39578,#21481,.T.);
#49295=EDGE_CURVE('',#39578,#39579,#21482,.T.);
#49296=EDGE_CURVE('',#39579,#39580,#936,.T.);
#49297=EDGE_CURVE('',#39580,#39581,#21483,.T.);
#49298=EDGE_CURVE('',#39581,#39582,#937,.T.);
#49299=EDGE_CURVE('',#39582,#39583,#21484,.T.);
#49300=EDGE_CURVE('',#39583,#39572,#21485,.T.);
#49301=EDGE_CURVE('',#39584,#39585,#938,.T.);
#49302=EDGE_CURVE('',#39585,#39586,#21486,.T.);
#49303=EDGE_CURVE('',#39586,#39587,#21487,.T.);
#49304=EDGE_CURVE('',#39587,#39588,#21488,.T.);
#49305=EDGE_CURVE('',#39588,#39589,#939,.T.);
#49306=EDGE_CURVE('',#39589,#39590,#21489,.T.);
#49307=EDGE_CURVE('',#39590,#39591,#21490,.T.);
#49308=EDGE_CURVE('',#39591,#39592,#940,.T.);
#49309=EDGE_CURVE('',#39592,#39593,#21491,.T.);
#49310=EDGE_CURVE('',#39593,#39594,#941,.T.);
#49311=EDGE_CURVE('',#39594,#39595,#21492,.T.);
#49312=EDGE_CURVE('',#39595,#39584,#21493,.T.);
#49313=EDGE_CURVE('',#36820,#36826,#21494,.T.);
#49314=EDGE_CURVE('',#36825,#36819,#21495,.T.);
#49315=EDGE_CURVE('',#39596,#39597,#942,.T.);
#49316=EDGE_CURVE('',#39597,#39598,#21496,.T.);
#49317=EDGE_CURVE('',#39598,#39599,#21497,.T.);
#49318=EDGE_CURVE('',#39599,#39600,#21498,.T.);
#49319=EDGE_CURVE('',#39600,#39601,#943,.T.);
#49320=EDGE_CURVE('',#39601,#39602,#21499,.T.);
#49321=EDGE_CURVE('',#39602,#39603,#21500,.T.);
#49322=EDGE_CURVE('',#39603,#39604,#944,.T.);
#49323=EDGE_CURVE('',#39604,#39605,#21501,.T.);
#49324=EDGE_CURVE('',#39605,#39606,#945,.T.);
#49325=EDGE_CURVE('',#39606,#39607,#21502,.T.);
#49326=EDGE_CURVE('',#39607,#39596,#21503,.T.);
#49327=EDGE_CURVE('',#39608,#39609,#946,.T.);
#49328=EDGE_CURVE('',#39609,#39610,#21504,.T.);
#49329=EDGE_CURVE('',#39610,#39611,#21505,.T.);
#49330=EDGE_CURVE('',#39611,#39612,#21506,.T.);
#49331=EDGE_CURVE('',#39612,#39613,#947,.T.);
#49332=EDGE_CURVE('',#39613,#39614,#21507,.T.);
#49333=EDGE_CURVE('',#39614,#39615,#21508,.T.);
#49334=EDGE_CURVE('',#39615,#39616,#948,.T.);
#49335=EDGE_CURVE('',#39616,#39617,#21509,.T.);
#49336=EDGE_CURVE('',#39617,#39618,#949,.T.);
#49337=EDGE_CURVE('',#39618,#39619,#21510,.T.);
#49338=EDGE_CURVE('',#39619,#39608,#21511,.T.);
#49339=EDGE_CURVE('',#39620,#39621,#21512,.T.);
#49340=EDGE_CURVE('',#39621,#39622,#31722,.T.);
#49341=EDGE_CURVE('',#39622,#39623,#21513,.T.);
#49342=EDGE_CURVE('',#39623,#39620,#31723,.T.);
#49343=EDGE_CURVE('',#39624,#39625,#950,.T.);
#49344=EDGE_CURVE('',#39625,#39626,#21514,.T.);
#49345=EDGE_CURVE('',#39626,#39627,#21515,.T.);
#49346=EDGE_CURVE('',#39627,#39628,#21516,.T.);
#49347=EDGE_CURVE('',#39628,#39629,#951,.T.);
#49348=EDGE_CURVE('',#39629,#39630,#21517,.T.);
#49349=EDGE_CURVE('',#39630,#39631,#21518,.T.);
#49350=EDGE_CURVE('',#39631,#39632,#952,.T.);
#49351=EDGE_CURVE('',#39632,#39633,#21519,.T.);
#49352=EDGE_CURVE('',#39633,#39634,#953,.T.);
#49353=EDGE_CURVE('',#39634,#39635,#21520,.T.);
#49354=EDGE_CURVE('',#39635,#39624,#21521,.T.);
#49355=EDGE_CURVE('',#39636,#39637,#954,.T.);
#49356=EDGE_CURVE('',#39637,#39638,#21522,.T.);
#49357=EDGE_CURVE('',#39638,#39639,#21523,.T.);
#49358=EDGE_CURVE('',#39639,#39640,#21524,.T.);
#49359=EDGE_CURVE('',#39640,#39641,#955,.T.);
#49360=EDGE_CURVE('',#39641,#39642,#21525,.T.);
#49361=EDGE_CURVE('',#39642,#39643,#21526,.T.);
#49362=EDGE_CURVE('',#39643,#39644,#956,.T.);
#49363=EDGE_CURVE('',#39644,#39645,#21527,.T.);
#49364=EDGE_CURVE('',#39645,#39646,#957,.T.);
#49365=EDGE_CURVE('',#39646,#39647,#21528,.T.);
#49366=EDGE_CURVE('',#39647,#39636,#21529,.T.);
#49367=EDGE_CURVE('',#39648,#39649,#21530,.T.);
#49368=EDGE_CURVE('',#39649,#39650,#31724,.T.);
#49369=EDGE_CURVE('',#39650,#39651,#21531,.T.);
#49370=EDGE_CURVE('',#39651,#39648,#31725,.T.);
#49371=EDGE_CURVE('',#39652,#39653,#958,.T.);
#49372=EDGE_CURVE('',#39653,#39654,#21532,.T.);
#49373=EDGE_CURVE('',#39654,#39655,#21533,.T.);
#49374=EDGE_CURVE('',#39655,#39656,#21534,.T.);
#49375=EDGE_CURVE('',#39656,#39657,#959,.T.);
#49376=EDGE_CURVE('',#39657,#39658,#21535,.T.);
#49377=EDGE_CURVE('',#39658,#39659,#21536,.T.);
#49378=EDGE_CURVE('',#39659,#39660,#960,.T.);
#49379=EDGE_CURVE('',#39660,#39661,#21537,.T.);
#49380=EDGE_CURVE('',#39661,#39662,#961,.T.);
#49381=EDGE_CURVE('',#39662,#39663,#21538,.T.);
#49382=EDGE_CURVE('',#39663,#39652,#21539,.T.);
#49383=EDGE_CURVE('',#39664,#39665,#962,.T.);
#49384=EDGE_CURVE('',#39665,#39666,#21540,.T.);
#49385=EDGE_CURVE('',#39666,#39667,#21541,.T.);
#49386=EDGE_CURVE('',#39667,#39668,#21542,.T.);
#49387=EDGE_CURVE('',#39668,#39669,#963,.T.);
#49388=EDGE_CURVE('',#39669,#39670,#21543,.T.);
#49389=EDGE_CURVE('',#39670,#39671,#21544,.T.);
#49390=EDGE_CURVE('',#39671,#39672,#964,.T.);
#49391=EDGE_CURVE('',#39672,#39673,#21545,.T.);
#49392=EDGE_CURVE('',#39673,#39674,#965,.T.);
#49393=EDGE_CURVE('',#39674,#39675,#21546,.T.);
#49394=EDGE_CURVE('',#39675,#39664,#21547,.T.);
#49395=EDGE_CURVE('',#39676,#39677,#21548,.T.);
#49396=EDGE_CURVE('',#39677,#39678,#31726,.T.);
#49397=EDGE_CURVE('',#39678,#39679,#21549,.T.);
#49398=EDGE_CURVE('',#39679,#39676,#31727,.T.);
#49399=EDGE_CURVE('',#39680,#39681,#966,.T.);
#49400=EDGE_CURVE('',#39681,#39682,#21550,.T.);
#49401=EDGE_CURVE('',#39682,#39683,#21551,.T.);
#49402=EDGE_CURVE('',#39683,#39684,#21552,.T.);
#49403=EDGE_CURVE('',#39684,#39685,#967,.T.);
#49404=EDGE_CURVE('',#39685,#39686,#21553,.T.);
#49405=EDGE_CURVE('',#39686,#39687,#21554,.T.);
#49406=EDGE_CURVE('',#39687,#39688,#968,.T.);
#49407=EDGE_CURVE('',#39688,#39689,#21555,.T.);
#49408=EDGE_CURVE('',#39689,#39690,#969,.T.);
#49409=EDGE_CURVE('',#39690,#39691,#21556,.T.);
#49410=EDGE_CURVE('',#39691,#39680,#21557,.T.);
#49411=EDGE_CURVE('',#39692,#39693,#970,.T.);
#49412=EDGE_CURVE('',#39693,#39694,#21558,.T.);
#49413=EDGE_CURVE('',#39694,#39695,#21559,.T.);
#49414=EDGE_CURVE('',#39695,#39696,#21560,.T.);
#49415=EDGE_CURVE('',#39696,#39697,#971,.T.);
#49416=EDGE_CURVE('',#39697,#39698,#21561,.T.);
#49417=EDGE_CURVE('',#39698,#39699,#21562,.T.);
#49418=EDGE_CURVE('',#39699,#39700,#972,.T.);
#49419=EDGE_CURVE('',#39700,#39701,#21563,.T.);
#49420=EDGE_CURVE('',#39701,#39702,#973,.T.);
#49421=EDGE_CURVE('',#39702,#39703,#21564,.T.);
#49422=EDGE_CURVE('',#39703,#39692,#21565,.T.);
#49423=EDGE_CURVE('',#39704,#39705,#21566,.T.);
#49424=EDGE_CURVE('',#39705,#39706,#31728,.T.);
#49425=EDGE_CURVE('',#39706,#39707,#21567,.T.);
#49426=EDGE_CURVE('',#39707,#39704,#31729,.T.);
#49427=EDGE_CURVE('',#39708,#39709,#974,.T.);
#49428=EDGE_CURVE('',#39709,#39710,#21568,.T.);
#49429=EDGE_CURVE('',#39710,#39711,#21569,.T.);
#49430=EDGE_CURVE('',#39711,#39712,#21570,.T.);
#49431=EDGE_CURVE('',#39712,#39713,#975,.T.);
#49432=EDGE_CURVE('',#39713,#39714,#21571,.T.);
#49433=EDGE_CURVE('',#39714,#39715,#21572,.T.);
#49434=EDGE_CURVE('',#39715,#39716,#976,.T.);
#49435=EDGE_CURVE('',#39716,#39717,#21573,.T.);
#49436=EDGE_CURVE('',#39717,#39718,#977,.T.);
#49437=EDGE_CURVE('',#39718,#39719,#21574,.T.);
#49438=EDGE_CURVE('',#39719,#39708,#21575,.T.);
#49439=EDGE_CURVE('',#39720,#39721,#978,.T.);
#49440=EDGE_CURVE('',#39721,#39722,#21576,.T.);
#49441=EDGE_CURVE('',#39722,#39723,#21577,.T.);
#49442=EDGE_CURVE('',#39723,#39724,#21578,.T.);
#49443=EDGE_CURVE('',#39724,#39725,#979,.T.);
#49444=EDGE_CURVE('',#39725,#39726,#21579,.T.);
#49445=EDGE_CURVE('',#39726,#39727,#21580,.T.);
#49446=EDGE_CURVE('',#39727,#39728,#980,.T.);
#49447=EDGE_CURVE('',#39728,#39729,#21581,.T.);
#49448=EDGE_CURVE('',#39729,#39730,#981,.T.);
#49449=EDGE_CURVE('',#39730,#39731,#21582,.T.);
#49450=EDGE_CURVE('',#39731,#39720,#21583,.T.);
#49451=EDGE_CURVE('',#39732,#39733,#21584,.T.);
#49452=EDGE_CURVE('',#39733,#39734,#31730,.T.);
#49453=EDGE_CURVE('',#39734,#39735,#21585,.T.);
#49454=EDGE_CURVE('',#39735,#39732,#31731,.T.);
#49455=EDGE_CURVE('',#39736,#39737,#982,.T.);
#49456=EDGE_CURVE('',#39737,#39738,#21586,.T.);
#49457=EDGE_CURVE('',#39738,#39739,#21587,.T.);
#49458=EDGE_CURVE('',#39739,#39740,#21588,.T.);
#49459=EDGE_CURVE('',#39740,#39741,#983,.T.);
#49460=EDGE_CURVE('',#39741,#39742,#21589,.T.);
#49461=EDGE_CURVE('',#39742,#39743,#21590,.T.);
#49462=EDGE_CURVE('',#39743,#39744,#984,.T.);
#49463=EDGE_CURVE('',#39744,#39745,#21591,.T.);
#49464=EDGE_CURVE('',#39745,#39746,#985,.T.);
#49465=EDGE_CURVE('',#39746,#39747,#21592,.T.);
#49466=EDGE_CURVE('',#39747,#39736,#21593,.T.);
#49467=EDGE_CURVE('',#39748,#39749,#986,.T.);
#49468=EDGE_CURVE('',#39749,#39750,#21594,.T.);
#49469=EDGE_CURVE('',#39750,#39751,#21595,.T.);
#49470=EDGE_CURVE('',#39751,#39752,#21596,.T.);
#49471=EDGE_CURVE('',#39752,#39753,#987,.T.);
#49472=EDGE_CURVE('',#39753,#39754,#21597,.T.);
#49473=EDGE_CURVE('',#39754,#39755,#21598,.T.);
#49474=EDGE_CURVE('',#39755,#39756,#988,.T.);
#49475=EDGE_CURVE('',#39756,#39757,#21599,.T.);
#49476=EDGE_CURVE('',#39757,#39758,#989,.T.);
#49477=EDGE_CURVE('',#39758,#39759,#21600,.T.);
#49478=EDGE_CURVE('',#39759,#39748,#21601,.T.);
#49479=EDGE_CURVE('',#39760,#39761,#21602,.T.);
#49480=EDGE_CURVE('',#39761,#39762,#31732,.T.);
#49481=EDGE_CURVE('',#39762,#39763,#21603,.T.);
#49482=EDGE_CURVE('',#39763,#39760,#31733,.T.);
#49483=EDGE_CURVE('',#39764,#39765,#990,.T.);
#49484=EDGE_CURVE('',#39765,#39766,#21604,.T.);
#49485=EDGE_CURVE('',#39766,#39767,#21605,.T.);
#49486=EDGE_CURVE('',#39767,#39768,#21606,.T.);
#49487=EDGE_CURVE('',#39768,#39769,#991,.T.);
#49488=EDGE_CURVE('',#39769,#39770,#21607,.T.);
#49489=EDGE_CURVE('',#39770,#39771,#21608,.T.);
#49490=EDGE_CURVE('',#39771,#39772,#992,.T.);
#49491=EDGE_CURVE('',#39772,#39773,#21609,.T.);
#49492=EDGE_CURVE('',#39773,#39774,#993,.T.);
#49493=EDGE_CURVE('',#39774,#39775,#21610,.T.);
#49494=EDGE_CURVE('',#39775,#39764,#21611,.T.);
#49495=EDGE_CURVE('',#39776,#39777,#994,.T.);
#49496=EDGE_CURVE('',#39777,#39778,#21612,.T.);
#49497=EDGE_CURVE('',#39778,#39779,#21613,.T.);
#49498=EDGE_CURVE('',#39779,#39780,#21614,.T.);
#49499=EDGE_CURVE('',#39780,#39781,#995,.T.);
#49500=EDGE_CURVE('',#39781,#39782,#21615,.T.);
#49501=EDGE_CURVE('',#39782,#39783,#21616,.T.);
#49502=EDGE_CURVE('',#39783,#39784,#996,.T.);
#49503=EDGE_CURVE('',#39784,#39785,#21617,.T.);
#49504=EDGE_CURVE('',#39785,#39786,#997,.T.);
#49505=EDGE_CURVE('',#39786,#39787,#21618,.T.);
#49506=EDGE_CURVE('',#39787,#39776,#21619,.T.);
#49507=EDGE_CURVE('',#39788,#39789,#21620,.T.);
#49508=EDGE_CURVE('',#39789,#39790,#31734,.T.);
#49509=EDGE_CURVE('',#39790,#39791,#21621,.T.);
#49510=EDGE_CURVE('',#39791,#39788,#31735,.T.);
#49511=EDGE_CURVE('',#39792,#39793,#998,.T.);
#49512=EDGE_CURVE('',#39793,#39794,#21622,.T.);
#49513=EDGE_CURVE('',#39794,#39795,#21623,.T.);
#49514=EDGE_CURVE('',#39795,#39796,#21624,.T.);
#49515=EDGE_CURVE('',#39796,#39797,#999,.T.);
#49516=EDGE_CURVE('',#39797,#39798,#21625,.T.);
#49517=EDGE_CURVE('',#39798,#39799,#21626,.T.);
#49518=EDGE_CURVE('',#39799,#39800,#1000,.T.);
#49519=EDGE_CURVE('',#39800,#39801,#21627,.T.);
#49520=EDGE_CURVE('',#39801,#39802,#1001,.T.);
#49521=EDGE_CURVE('',#39802,#39803,#21628,.T.);
#49522=EDGE_CURVE('',#39803,#39792,#21629,.T.);
#49523=EDGE_CURVE('',#39804,#39805,#1002,.T.);
#49524=EDGE_CURVE('',#39805,#39806,#21630,.T.);
#49525=EDGE_CURVE('',#39806,#39807,#21631,.T.);
#49526=EDGE_CURVE('',#39807,#39808,#21632,.T.);
#49527=EDGE_CURVE('',#39808,#39809,#1003,.T.);
#49528=EDGE_CURVE('',#39809,#39810,#21633,.T.);
#49529=EDGE_CURVE('',#39810,#39811,#21634,.T.);
#49530=EDGE_CURVE('',#39811,#39812,#1004,.T.);
#49531=EDGE_CURVE('',#39812,#39813,#21635,.T.);
#49532=EDGE_CURVE('',#39813,#39814,#1005,.T.);
#49533=EDGE_CURVE('',#39814,#39815,#21636,.T.);
#49534=EDGE_CURVE('',#39815,#39804,#21637,.T.);
#49535=EDGE_CURVE('',#39816,#39817,#21638,.T.);
#49536=EDGE_CURVE('',#39817,#39818,#31736,.T.);
#49537=EDGE_CURVE('',#39818,#39819,#21639,.T.);
#49538=EDGE_CURVE('',#39819,#39816,#31737,.T.);
#49539=EDGE_CURVE('',#39820,#39821,#1006,.T.);
#49540=EDGE_CURVE('',#39821,#39822,#21640,.T.);
#49541=EDGE_CURVE('',#39822,#39823,#21641,.T.);
#49542=EDGE_CURVE('',#39823,#39824,#21642,.T.);
#49543=EDGE_CURVE('',#39824,#39825,#1007,.T.);
#49544=EDGE_CURVE('',#39825,#39826,#21643,.T.);
#49545=EDGE_CURVE('',#39826,#39827,#21644,.T.);
#49546=EDGE_CURVE('',#39827,#39828,#1008,.T.);
#49547=EDGE_CURVE('',#39828,#39829,#21645,.T.);
#49548=EDGE_CURVE('',#39829,#39830,#1009,.T.);
#49549=EDGE_CURVE('',#39830,#39831,#21646,.T.);
#49550=EDGE_CURVE('',#39831,#39820,#21647,.T.);
#49551=EDGE_CURVE('',#39832,#39833,#1010,.T.);
#49552=EDGE_CURVE('',#39833,#39834,#21648,.T.);
#49553=EDGE_CURVE('',#39834,#39835,#21649,.T.);
#49554=EDGE_CURVE('',#39835,#39836,#21650,.T.);
#49555=EDGE_CURVE('',#39836,#39837,#1011,.T.);
#49556=EDGE_CURVE('',#39837,#39838,#21651,.T.);
#49557=EDGE_CURVE('',#39838,#39839,#21652,.T.);
#49558=EDGE_CURVE('',#39839,#39840,#1012,.T.);
#49559=EDGE_CURVE('',#39840,#39841,#21653,.T.);
#49560=EDGE_CURVE('',#39841,#39842,#1013,.T.);
#49561=EDGE_CURVE('',#39842,#39843,#21654,.T.);
#49562=EDGE_CURVE('',#39843,#39832,#21655,.T.);
#49563=EDGE_CURVE('',#39844,#39845,#21656,.T.);
#49564=EDGE_CURVE('',#39845,#39846,#31738,.T.);
#49565=EDGE_CURVE('',#39846,#39847,#21657,.T.);
#49566=EDGE_CURVE('',#39847,#39844,#31739,.T.);
#49567=EDGE_CURVE('',#39848,#39849,#1014,.T.);
#49568=EDGE_CURVE('',#39849,#39850,#21658,.T.);
#49569=EDGE_CURVE('',#39850,#39851,#21659,.T.);
#49570=EDGE_CURVE('',#39851,#39852,#21660,.T.);
#49571=EDGE_CURVE('',#39852,#39853,#1015,.T.);
#49572=EDGE_CURVE('',#39853,#39854,#21661,.T.);
#49573=EDGE_CURVE('',#39854,#39855,#21662,.T.);
#49574=EDGE_CURVE('',#39855,#39856,#1016,.T.);
#49575=EDGE_CURVE('',#39856,#39857,#21663,.T.);
#49576=EDGE_CURVE('',#39857,#39858,#1017,.T.);
#49577=EDGE_CURVE('',#39858,#39859,#21664,.T.);
#49578=EDGE_CURVE('',#39859,#39848,#21665,.T.);
#49579=EDGE_CURVE('',#39860,#39861,#1018,.T.);
#49580=EDGE_CURVE('',#39861,#39862,#21666,.T.);
#49581=EDGE_CURVE('',#39862,#39863,#21667,.T.);
#49582=EDGE_CURVE('',#39863,#39864,#21668,.T.);
#49583=EDGE_CURVE('',#39864,#39865,#1019,.T.);
#49584=EDGE_CURVE('',#39865,#39866,#21669,.T.);
#49585=EDGE_CURVE('',#39866,#39867,#21670,.T.);
#49586=EDGE_CURVE('',#39867,#39868,#1020,.T.);
#49587=EDGE_CURVE('',#39868,#39869,#21671,.T.);
#49588=EDGE_CURVE('',#39869,#39870,#1021,.T.);
#49589=EDGE_CURVE('',#39870,#39871,#21672,.T.);
#49590=EDGE_CURVE('',#39871,#39860,#21673,.T.);
#49591=EDGE_CURVE('',#39872,#39873,#21674,.T.);
#49592=EDGE_CURVE('',#39873,#39874,#31740,.T.);
#49593=EDGE_CURVE('',#39874,#39875,#21675,.T.);
#49594=EDGE_CURVE('',#39875,#39872,#31741,.T.);
#49595=EDGE_CURVE('',#39876,#39877,#1022,.T.);
#49596=EDGE_CURVE('',#39877,#39878,#21676,.T.);
#49597=EDGE_CURVE('',#39878,#39879,#21677,.T.);
#49598=EDGE_CURVE('',#39879,#39880,#21678,.T.);
#49599=EDGE_CURVE('',#39880,#39881,#1023,.T.);
#49600=EDGE_CURVE('',#39881,#39882,#21679,.T.);
#49601=EDGE_CURVE('',#39882,#39883,#21680,.T.);
#49602=EDGE_CURVE('',#39883,#39884,#1024,.T.);
#49603=EDGE_CURVE('',#39884,#39885,#21681,.T.);
#49604=EDGE_CURVE('',#39885,#39886,#1025,.T.);
#49605=EDGE_CURVE('',#39886,#39887,#21682,.T.);
#49606=EDGE_CURVE('',#39887,#39876,#21683,.T.);
#49607=EDGE_CURVE('',#39888,#39889,#1026,.T.);
#49608=EDGE_CURVE('',#39889,#39890,#21684,.T.);
#49609=EDGE_CURVE('',#39890,#39891,#21685,.T.);
#49610=EDGE_CURVE('',#39891,#39892,#21686,.T.);
#49611=EDGE_CURVE('',#39892,#39893,#1027,.T.);
#49612=EDGE_CURVE('',#39893,#39894,#21687,.T.);
#49613=EDGE_CURVE('',#39894,#39895,#21688,.T.);
#49614=EDGE_CURVE('',#39895,#39896,#1028,.T.);
#49615=EDGE_CURVE('',#39896,#39897,#21689,.T.);
#49616=EDGE_CURVE('',#39897,#39898,#1029,.T.);
#49617=EDGE_CURVE('',#39898,#39899,#21690,.T.);
#49618=EDGE_CURVE('',#39899,#39888,#21691,.T.);
#49619=EDGE_CURVE('',#39900,#39901,#21692,.T.);
#49620=EDGE_CURVE('',#39901,#39902,#31742,.T.);
#49621=EDGE_CURVE('',#39902,#39903,#21693,.T.);
#49622=EDGE_CURVE('',#39903,#39900,#31743,.T.);
#49623=EDGE_CURVE('',#39904,#39905,#1030,.T.);
#49624=EDGE_CURVE('',#39905,#39906,#21694,.T.);
#49625=EDGE_CURVE('',#39906,#39907,#21695,.T.);
#49626=EDGE_CURVE('',#39907,#39908,#21696,.T.);
#49627=EDGE_CURVE('',#39908,#39909,#1031,.T.);
#49628=EDGE_CURVE('',#39909,#39910,#21697,.T.);
#49629=EDGE_CURVE('',#39910,#39911,#21698,.T.);
#49630=EDGE_CURVE('',#39911,#39912,#1032,.T.);
#49631=EDGE_CURVE('',#39912,#39913,#21699,.T.);
#49632=EDGE_CURVE('',#39913,#39914,#1033,.T.);
#49633=EDGE_CURVE('',#39914,#39915,#21700,.T.);
#49634=EDGE_CURVE('',#39915,#39904,#21701,.T.);
#49635=EDGE_CURVE('',#39916,#39917,#1034,.T.);
#49636=EDGE_CURVE('',#39917,#39918,#21702,.T.);
#49637=EDGE_CURVE('',#39918,#39919,#21703,.T.);
#49638=EDGE_CURVE('',#39919,#39920,#21704,.T.);
#49639=EDGE_CURVE('',#39920,#39921,#1035,.T.);
#49640=EDGE_CURVE('',#39921,#39922,#21705,.T.);
#49641=EDGE_CURVE('',#39922,#39923,#21706,.T.);
#49642=EDGE_CURVE('',#39923,#39924,#1036,.T.);
#49643=EDGE_CURVE('',#39924,#39925,#21707,.T.);
#49644=EDGE_CURVE('',#39925,#39926,#1037,.T.);
#49645=EDGE_CURVE('',#39926,#39927,#21708,.T.);
#49646=EDGE_CURVE('',#39927,#39916,#21709,.T.);
#49647=EDGE_CURVE('',#39928,#39929,#21710,.T.);
#49648=EDGE_CURVE('',#39929,#39930,#31744,.T.);
#49649=EDGE_CURVE('',#39930,#39931,#21711,.T.);
#49650=EDGE_CURVE('',#39931,#39928,#31745,.T.);
#49651=EDGE_CURVE('',#39932,#39933,#1038,.T.);
#49652=EDGE_CURVE('',#39933,#39934,#21712,.T.);
#49653=EDGE_CURVE('',#39934,#39935,#21713,.T.);
#49654=EDGE_CURVE('',#39935,#39936,#21714,.T.);
#49655=EDGE_CURVE('',#39936,#39937,#1039,.T.);
#49656=EDGE_CURVE('',#39937,#39938,#21715,.T.);
#49657=EDGE_CURVE('',#39938,#39939,#21716,.T.);
#49658=EDGE_CURVE('',#39939,#39940,#1040,.T.);
#49659=EDGE_CURVE('',#39940,#39941,#21717,.T.);
#49660=EDGE_CURVE('',#39941,#39942,#1041,.T.);
#49661=EDGE_CURVE('',#39942,#39943,#21718,.T.);
#49662=EDGE_CURVE('',#39943,#39932,#21719,.T.);
#49663=EDGE_CURVE('',#39944,#39945,#1042,.T.);
#49664=EDGE_CURVE('',#39945,#39946,#21720,.T.);
#49665=EDGE_CURVE('',#39946,#39947,#21721,.T.);
#49666=EDGE_CURVE('',#39947,#39948,#21722,.T.);
#49667=EDGE_CURVE('',#39948,#39949,#1043,.T.);
#49668=EDGE_CURVE('',#39949,#39950,#21723,.T.);
#49669=EDGE_CURVE('',#39950,#39951,#21724,.T.);
#49670=EDGE_CURVE('',#39951,#39952,#1044,.T.);
#49671=EDGE_CURVE('',#39952,#39953,#21725,.T.);
#49672=EDGE_CURVE('',#39953,#39954,#1045,.T.);
#49673=EDGE_CURVE('',#39954,#39955,#21726,.T.);
#49674=EDGE_CURVE('',#39955,#39944,#21727,.T.);
#49675=EDGE_CURVE('',#39956,#39957,#21728,.T.);
#49676=EDGE_CURVE('',#39957,#39958,#31746,.T.);
#49677=EDGE_CURVE('',#39958,#39959,#21729,.T.);
#49678=EDGE_CURVE('',#39959,#39956,#31747,.T.);
#49679=EDGE_CURVE('',#39960,#39961,#1046,.T.);
#49680=EDGE_CURVE('',#39961,#39962,#21730,.T.);
#49681=EDGE_CURVE('',#39962,#39963,#21731,.T.);
#49682=EDGE_CURVE('',#39963,#39964,#21732,.T.);
#49683=EDGE_CURVE('',#39964,#39965,#1047,.T.);
#49684=EDGE_CURVE('',#39965,#39966,#21733,.T.);
#49685=EDGE_CURVE('',#39966,#39967,#21734,.T.);
#49686=EDGE_CURVE('',#39967,#39968,#1048,.T.);
#49687=EDGE_CURVE('',#39968,#39969,#21735,.T.);
#49688=EDGE_CURVE('',#39969,#39970,#1049,.T.);
#49689=EDGE_CURVE('',#39970,#39971,#21736,.T.);
#49690=EDGE_CURVE('',#39971,#39960,#21737,.T.);
#49691=EDGE_CURVE('',#39972,#39973,#1050,.T.);
#49692=EDGE_CURVE('',#39973,#39974,#21738,.T.);
#49693=EDGE_CURVE('',#39974,#39975,#21739,.T.);
#49694=EDGE_CURVE('',#39975,#39976,#21740,.T.);
#49695=EDGE_CURVE('',#39976,#39977,#1051,.T.);
#49696=EDGE_CURVE('',#39977,#39978,#21741,.T.);
#49697=EDGE_CURVE('',#39978,#39979,#21742,.T.);
#49698=EDGE_CURVE('',#39979,#39980,#1052,.T.);
#49699=EDGE_CURVE('',#39980,#39981,#21743,.T.);
#49700=EDGE_CURVE('',#39981,#39982,#1053,.T.);
#49701=EDGE_CURVE('',#39982,#39983,#21744,.T.);
#49702=EDGE_CURVE('',#39983,#39972,#21745,.T.);
#49703=EDGE_CURVE('',#39984,#39985,#21746,.T.);
#49704=EDGE_CURVE('',#39985,#39986,#31748,.T.);
#49705=EDGE_CURVE('',#39986,#39987,#21747,.T.);
#49706=EDGE_CURVE('',#39987,#39984,#31749,.T.);
#49707=EDGE_CURVE('',#39988,#39989,#1054,.T.);
#49708=EDGE_CURVE('',#39989,#39990,#21748,.T.);
#49709=EDGE_CURVE('',#39990,#39991,#21749,.T.);
#49710=EDGE_CURVE('',#39991,#39992,#21750,.T.);
#49711=EDGE_CURVE('',#39992,#39993,#1055,.T.);
#49712=EDGE_CURVE('',#39993,#39994,#21751,.T.);
#49713=EDGE_CURVE('',#39994,#39995,#21752,.T.);
#49714=EDGE_CURVE('',#39995,#39996,#1056,.T.);
#49715=EDGE_CURVE('',#39996,#39997,#21753,.T.);
#49716=EDGE_CURVE('',#39997,#39998,#1057,.T.);
#49717=EDGE_CURVE('',#39998,#39999,#21754,.T.);
#49718=EDGE_CURVE('',#39999,#39988,#21755,.T.);
#49719=EDGE_CURVE('',#40000,#40001,#1058,.T.);
#49720=EDGE_CURVE('',#40001,#40002,#21756,.T.);
#49721=EDGE_CURVE('',#40002,#40003,#21757,.T.);
#49722=EDGE_CURVE('',#40003,#40004,#21758,.T.);
#49723=EDGE_CURVE('',#40004,#40005,#1059,.T.);
#49724=EDGE_CURVE('',#40005,#40006,#21759,.T.);
#49725=EDGE_CURVE('',#40006,#40007,#21760,.T.);
#49726=EDGE_CURVE('',#40007,#40008,#1060,.T.);
#49727=EDGE_CURVE('',#40008,#40009,#21761,.T.);
#49728=EDGE_CURVE('',#40009,#40010,#1061,.T.);
#49729=EDGE_CURVE('',#40010,#40011,#21762,.T.);
#49730=EDGE_CURVE('',#40011,#40000,#21763,.T.);
#49731=EDGE_CURVE('',#36812,#36818,#21764,.T.);
#49732=EDGE_CURVE('',#36817,#36811,#21765,.T.);
#49733=EDGE_CURVE('',#40012,#40013,#1062,.T.);
#49734=EDGE_CURVE('',#40013,#40014,#21766,.T.);
#49735=EDGE_CURVE('',#40014,#40015,#21767,.T.);
#49736=EDGE_CURVE('',#40015,#40016,#21768,.T.);
#49737=EDGE_CURVE('',#40016,#40017,#1063,.T.);
#49738=EDGE_CURVE('',#40017,#40018,#21769,.T.);
#49739=EDGE_CURVE('',#40018,#40019,#21770,.T.);
#49740=EDGE_CURVE('',#40019,#40020,#1064,.T.);
#49741=EDGE_CURVE('',#40020,#40021,#21771,.T.);
#49742=EDGE_CURVE('',#40021,#40022,#1065,.T.);
#49743=EDGE_CURVE('',#40022,#40023,#21772,.T.);
#49744=EDGE_CURVE('',#40023,#40012,#21773,.T.);
#49745=EDGE_CURVE('',#40024,#40025,#1066,.T.);
#49746=EDGE_CURVE('',#40025,#40026,#21774,.T.);
#49747=EDGE_CURVE('',#40026,#40027,#21775,.T.);
#49748=EDGE_CURVE('',#40027,#40028,#21776,.T.);
#49749=EDGE_CURVE('',#40028,#40029,#1067,.T.);
#49750=EDGE_CURVE('',#40029,#40030,#21777,.T.);
#49751=EDGE_CURVE('',#40030,#40031,#21778,.T.);
#49752=EDGE_CURVE('',#40031,#40032,#1068,.T.);
#49753=EDGE_CURVE('',#40032,#40033,#21779,.T.);
#49754=EDGE_CURVE('',#40033,#40034,#1069,.T.);
#49755=EDGE_CURVE('',#40034,#40035,#21780,.T.);
#49756=EDGE_CURVE('',#40035,#40024,#21781,.T.);
#49757=EDGE_CURVE('',#40036,#40037,#21782,.T.);
#49758=EDGE_CURVE('',#40037,#40038,#31750,.T.);
#49759=EDGE_CURVE('',#40038,#40039,#21783,.T.);
#49760=EDGE_CURVE('',#40039,#40036,#31751,.T.);
#49761=EDGE_CURVE('',#40040,#40041,#1070,.T.);
#49762=EDGE_CURVE('',#40041,#40042,#21784,.T.);
#49763=EDGE_CURVE('',#40042,#40043,#21785,.T.);
#49764=EDGE_CURVE('',#40043,#40044,#21786,.T.);
#49765=EDGE_CURVE('',#40044,#40045,#1071,.T.);
#49766=EDGE_CURVE('',#40045,#40046,#21787,.T.);
#49767=EDGE_CURVE('',#40046,#40047,#21788,.T.);
#49768=EDGE_CURVE('',#40047,#40048,#1072,.T.);
#49769=EDGE_CURVE('',#40048,#40049,#21789,.T.);
#49770=EDGE_CURVE('',#40049,#40050,#1073,.T.);
#49771=EDGE_CURVE('',#40050,#40051,#21790,.T.);
#49772=EDGE_CURVE('',#40051,#40040,#21791,.T.);
#49773=EDGE_CURVE('',#40052,#40053,#1074,.T.);
#49774=EDGE_CURVE('',#40053,#40054,#21792,.T.);
#49775=EDGE_CURVE('',#40054,#40055,#21793,.T.);
#49776=EDGE_CURVE('',#40055,#40056,#21794,.T.);
#49777=EDGE_CURVE('',#40056,#40057,#1075,.T.);
#49778=EDGE_CURVE('',#40057,#40058,#21795,.T.);
#49779=EDGE_CURVE('',#40058,#40059,#21796,.T.);
#49780=EDGE_CURVE('',#40059,#40060,#1076,.T.);
#49781=EDGE_CURVE('',#40060,#40061,#21797,.T.);
#49782=EDGE_CURVE('',#40061,#40062,#1077,.T.);
#49783=EDGE_CURVE('',#40062,#40063,#21798,.T.);
#49784=EDGE_CURVE('',#40063,#40052,#21799,.T.);
#49785=EDGE_CURVE('',#40064,#40065,#21800,.T.);
#49786=EDGE_CURVE('',#40065,#40066,#31752,.T.);
#49787=EDGE_CURVE('',#40066,#40067,#21801,.T.);
#49788=EDGE_CURVE('',#40067,#40064,#31753,.T.);
#49789=EDGE_CURVE('',#40068,#40069,#1078,.T.);
#49790=EDGE_CURVE('',#40069,#40070,#21802,.T.);
#49791=EDGE_CURVE('',#40070,#40071,#21803,.T.);
#49792=EDGE_CURVE('',#40071,#40072,#21804,.T.);
#49793=EDGE_CURVE('',#40072,#40073,#1079,.T.);
#49794=EDGE_CURVE('',#40073,#40074,#21805,.T.);
#49795=EDGE_CURVE('',#40074,#40075,#21806,.T.);
#49796=EDGE_CURVE('',#40075,#40076,#1080,.T.);
#49797=EDGE_CURVE('',#40076,#40077,#21807,.T.);
#49798=EDGE_CURVE('',#40077,#40078,#1081,.T.);
#49799=EDGE_CURVE('',#40078,#40079,#21808,.T.);
#49800=EDGE_CURVE('',#40079,#40068,#21809,.T.);
#49801=EDGE_CURVE('',#40080,#40081,#1082,.T.);
#49802=EDGE_CURVE('',#40081,#40082,#21810,.T.);
#49803=EDGE_CURVE('',#40082,#40083,#21811,.T.);
#49804=EDGE_CURVE('',#40083,#40084,#21812,.T.);
#49805=EDGE_CURVE('',#40084,#40085,#1083,.T.);
#49806=EDGE_CURVE('',#40085,#40086,#21813,.T.);
#49807=EDGE_CURVE('',#40086,#40087,#21814,.T.);
#49808=EDGE_CURVE('',#40087,#40088,#1084,.T.);
#49809=EDGE_CURVE('',#40088,#40089,#21815,.T.);
#49810=EDGE_CURVE('',#40089,#40090,#1085,.T.);
#49811=EDGE_CURVE('',#40090,#40091,#21816,.T.);
#49812=EDGE_CURVE('',#40091,#40080,#21817,.T.);
#49813=EDGE_CURVE('',#40092,#40093,#21818,.T.);
#49814=EDGE_CURVE('',#40093,#40094,#31754,.T.);
#49815=EDGE_CURVE('',#40094,#40095,#21819,.T.);
#49816=EDGE_CURVE('',#40095,#40092,#31755,.T.);
#49817=EDGE_CURVE('',#40096,#40097,#1086,.T.);
#49818=EDGE_CURVE('',#40097,#40098,#21820,.T.);
#49819=EDGE_CURVE('',#40098,#40099,#21821,.T.);
#49820=EDGE_CURVE('',#40099,#40100,#21822,.T.);
#49821=EDGE_CURVE('',#40100,#40101,#1087,.T.);
#49822=EDGE_CURVE('',#40101,#40102,#21823,.T.);
#49823=EDGE_CURVE('',#40102,#40103,#21824,.T.);
#49824=EDGE_CURVE('',#40103,#40104,#1088,.T.);
#49825=EDGE_CURVE('',#40104,#40105,#21825,.T.);
#49826=EDGE_CURVE('',#40105,#40106,#1089,.T.);
#49827=EDGE_CURVE('',#40106,#40107,#21826,.T.);
#49828=EDGE_CURVE('',#40107,#40096,#21827,.T.);
#49829=EDGE_CURVE('',#40108,#40109,#1090,.T.);
#49830=EDGE_CURVE('',#40109,#40110,#21828,.T.);
#49831=EDGE_CURVE('',#40110,#40111,#21829,.T.);
#49832=EDGE_CURVE('',#40111,#40112,#21830,.T.);
#49833=EDGE_CURVE('',#40112,#40113,#1091,.T.);
#49834=EDGE_CURVE('',#40113,#40114,#21831,.T.);
#49835=EDGE_CURVE('',#40114,#40115,#21832,.T.);
#49836=EDGE_CURVE('',#40115,#40116,#1092,.T.);
#49837=EDGE_CURVE('',#40116,#40117,#21833,.T.);
#49838=EDGE_CURVE('',#40117,#40118,#1093,.T.);
#49839=EDGE_CURVE('',#40118,#40119,#21834,.T.);
#49840=EDGE_CURVE('',#40119,#40108,#21835,.T.);
#49841=EDGE_CURVE('',#40120,#40121,#21836,.T.);
#49842=EDGE_CURVE('',#40121,#40122,#31756,.T.);
#49843=EDGE_CURVE('',#40122,#40123,#21837,.T.);
#49844=EDGE_CURVE('',#40123,#40120,#31757,.T.);
#49845=EDGE_CURVE('',#40124,#40125,#1094,.T.);
#49846=EDGE_CURVE('',#40125,#40126,#21838,.T.);
#49847=EDGE_CURVE('',#40126,#40127,#21839,.T.);
#49848=EDGE_CURVE('',#40127,#40128,#21840,.T.);
#49849=EDGE_CURVE('',#40128,#40129,#1095,.T.);
#49850=EDGE_CURVE('',#40129,#40130,#21841,.T.);
#49851=EDGE_CURVE('',#40130,#40131,#21842,.T.);
#49852=EDGE_CURVE('',#40131,#40132,#1096,.T.);
#49853=EDGE_CURVE('',#40132,#40133,#21843,.T.);
#49854=EDGE_CURVE('',#40133,#40134,#1097,.T.);
#49855=EDGE_CURVE('',#40134,#40135,#21844,.T.);
#49856=EDGE_CURVE('',#40135,#40124,#21845,.T.);
#49857=EDGE_CURVE('',#40136,#40137,#1098,.T.);
#49858=EDGE_CURVE('',#40137,#40138,#21846,.T.);
#49859=EDGE_CURVE('',#40138,#40139,#21847,.T.);
#49860=EDGE_CURVE('',#40139,#40140,#21848,.T.);
#49861=EDGE_CURVE('',#40140,#40141,#1099,.T.);
#49862=EDGE_CURVE('',#40141,#40142,#21849,.T.);
#49863=EDGE_CURVE('',#40142,#40143,#21850,.T.);
#49864=EDGE_CURVE('',#40143,#40144,#1100,.T.);
#49865=EDGE_CURVE('',#40144,#40145,#21851,.T.);
#49866=EDGE_CURVE('',#40145,#40146,#1101,.T.);
#49867=EDGE_CURVE('',#40146,#40147,#21852,.T.);
#49868=EDGE_CURVE('',#40147,#40136,#21853,.T.);
#49869=EDGE_CURVE('',#40148,#40149,#21854,.T.);
#49870=EDGE_CURVE('',#40149,#40150,#31758,.T.);
#49871=EDGE_CURVE('',#40150,#40151,#21855,.T.);
#49872=EDGE_CURVE('',#40151,#40148,#31759,.T.);
#49873=EDGE_CURVE('',#40152,#40153,#1102,.T.);
#49874=EDGE_CURVE('',#40153,#40154,#21856,.T.);
#49875=EDGE_CURVE('',#40154,#40155,#21857,.T.);
#49876=EDGE_CURVE('',#40155,#40156,#21858,.T.);
#49877=EDGE_CURVE('',#40156,#40157,#1103,.T.);
#49878=EDGE_CURVE('',#40157,#40158,#21859,.T.);
#49879=EDGE_CURVE('',#40158,#40159,#21860,.T.);
#49880=EDGE_CURVE('',#40159,#40160,#1104,.T.);
#49881=EDGE_CURVE('',#40160,#40161,#21861,.T.);
#49882=EDGE_CURVE('',#40161,#40162,#1105,.T.);
#49883=EDGE_CURVE('',#40162,#40163,#21862,.T.);
#49884=EDGE_CURVE('',#40163,#40152,#21863,.T.);
#49885=EDGE_CURVE('',#40164,#40165,#1106,.T.);
#49886=EDGE_CURVE('',#40165,#40166,#21864,.T.);
#49887=EDGE_CURVE('',#40166,#40167,#21865,.T.);
#49888=EDGE_CURVE('',#40167,#40168,#21866,.T.);
#49889=EDGE_CURVE('',#40168,#40169,#1107,.T.);
#49890=EDGE_CURVE('',#40169,#40170,#21867,.T.);
#49891=EDGE_CURVE('',#40170,#40171,#21868,.T.);
#49892=EDGE_CURVE('',#40171,#40172,#1108,.T.);
#49893=EDGE_CURVE('',#40172,#40173,#21869,.T.);
#49894=EDGE_CURVE('',#40173,#40174,#1109,.T.);
#49895=EDGE_CURVE('',#40174,#40175,#21870,.T.);
#49896=EDGE_CURVE('',#40175,#40164,#21871,.T.);
#49897=EDGE_CURVE('',#40176,#40177,#21872,.T.);
#49898=EDGE_CURVE('',#40177,#40178,#31760,.T.);
#49899=EDGE_CURVE('',#40178,#40179,#21873,.T.);
#49900=EDGE_CURVE('',#40179,#40176,#31761,.T.);
#49901=EDGE_CURVE('',#40180,#40181,#1110,.T.);
#49902=EDGE_CURVE('',#40181,#40182,#21874,.T.);
#49903=EDGE_CURVE('',#40182,#40183,#21875,.T.);
#49904=EDGE_CURVE('',#40183,#40184,#21876,.T.);
#49905=EDGE_CURVE('',#40184,#40185,#1111,.T.);
#49906=EDGE_CURVE('',#40185,#40186,#21877,.T.);
#49907=EDGE_CURVE('',#40186,#40187,#21878,.T.);
#49908=EDGE_CURVE('',#40187,#40188,#1112,.T.);
#49909=EDGE_CURVE('',#40188,#40189,#21879,.T.);
#49910=EDGE_CURVE('',#40189,#40190,#1113,.T.);
#49911=EDGE_CURVE('',#40190,#40191,#21880,.T.);
#49912=EDGE_CURVE('',#40191,#40180,#21881,.T.);
#49913=EDGE_CURVE('',#40192,#40193,#1114,.T.);
#49914=EDGE_CURVE('',#40193,#40194,#21882,.T.);
#49915=EDGE_CURVE('',#40194,#40195,#21883,.T.);
#49916=EDGE_CURVE('',#40195,#40196,#21884,.T.);
#49917=EDGE_CURVE('',#40196,#40197,#1115,.T.);
#49918=EDGE_CURVE('',#40197,#40198,#21885,.T.);
#49919=EDGE_CURVE('',#40198,#40199,#21886,.T.);
#49920=EDGE_CURVE('',#40199,#40200,#1116,.T.);
#49921=EDGE_CURVE('',#40200,#40201,#21887,.T.);
#49922=EDGE_CURVE('',#40201,#40202,#1117,.T.);
#49923=EDGE_CURVE('',#40202,#40203,#21888,.T.);
#49924=EDGE_CURVE('',#40203,#40192,#21889,.T.);
#49925=EDGE_CURVE('',#40204,#40205,#21890,.T.);
#49926=EDGE_CURVE('',#40205,#40206,#31762,.T.);
#49927=EDGE_CURVE('',#40206,#40207,#21891,.T.);
#49928=EDGE_CURVE('',#40207,#40204,#31763,.T.);
#49929=EDGE_CURVE('',#40208,#40209,#1118,.T.);
#49930=EDGE_CURVE('',#40209,#40210,#21892,.T.);
#49931=EDGE_CURVE('',#40210,#40211,#21893,.T.);
#49932=EDGE_CURVE('',#40211,#40212,#21894,.T.);
#49933=EDGE_CURVE('',#40212,#40213,#1119,.T.);
#49934=EDGE_CURVE('',#40213,#40214,#21895,.T.);
#49935=EDGE_CURVE('',#40214,#40215,#21896,.T.);
#49936=EDGE_CURVE('',#40215,#40216,#1120,.T.);
#49937=EDGE_CURVE('',#40216,#40217,#21897,.T.);
#49938=EDGE_CURVE('',#40217,#40218,#1121,.T.);
#49939=EDGE_CURVE('',#40218,#40219,#21898,.T.);
#49940=EDGE_CURVE('',#40219,#40208,#21899,.T.);
#49941=EDGE_CURVE('',#40220,#40221,#1122,.T.);
#49942=EDGE_CURVE('',#40221,#40222,#21900,.T.);
#49943=EDGE_CURVE('',#40222,#40223,#21901,.T.);
#49944=EDGE_CURVE('',#40223,#40224,#21902,.T.);
#49945=EDGE_CURVE('',#40224,#40225,#1123,.T.);
#49946=EDGE_CURVE('',#40225,#40226,#21903,.T.);
#49947=EDGE_CURVE('',#40226,#40227,#21904,.T.);
#49948=EDGE_CURVE('',#40227,#40228,#1124,.T.);
#49949=EDGE_CURVE('',#40228,#40229,#21905,.T.);
#49950=EDGE_CURVE('',#40229,#40230,#1125,.T.);
#49951=EDGE_CURVE('',#40230,#40231,#21906,.T.);
#49952=EDGE_CURVE('',#40231,#40220,#21907,.T.);
#49953=EDGE_CURVE('',#40232,#40233,#21908,.T.);
#49954=EDGE_CURVE('',#40233,#40234,#31764,.T.);
#49955=EDGE_CURVE('',#40234,#40235,#21909,.T.);
#49956=EDGE_CURVE('',#40235,#40232,#31765,.T.);
#49957=EDGE_CURVE('',#40236,#40237,#1126,.T.);
#49958=EDGE_CURVE('',#40237,#40238,#21910,.T.);
#49959=EDGE_CURVE('',#40238,#40239,#21911,.T.);
#49960=EDGE_CURVE('',#40239,#40240,#21912,.T.);
#49961=EDGE_CURVE('',#40240,#40241,#1127,.T.);
#49962=EDGE_CURVE('',#40241,#40242,#21913,.T.);
#49963=EDGE_CURVE('',#40242,#40243,#21914,.T.);
#49964=EDGE_CURVE('',#40243,#40244,#1128,.T.);
#49965=EDGE_CURVE('',#40244,#40245,#21915,.T.);
#49966=EDGE_CURVE('',#40245,#40246,#1129,.T.);
#49967=EDGE_CURVE('',#40246,#40247,#21916,.T.);
#49968=EDGE_CURVE('',#40247,#40236,#21917,.T.);
#49969=EDGE_CURVE('',#40248,#40249,#1130,.T.);
#49970=EDGE_CURVE('',#40249,#40250,#21918,.T.);
#49971=EDGE_CURVE('',#40250,#40251,#21919,.T.);
#49972=EDGE_CURVE('',#40251,#40252,#21920,.T.);
#49973=EDGE_CURVE('',#40252,#40253,#1131,.T.);
#49974=EDGE_CURVE('',#40253,#40254,#21921,.T.);
#49975=EDGE_CURVE('',#40254,#40255,#21922,.T.);
#49976=EDGE_CURVE('',#40255,#40256,#1132,.T.);
#49977=EDGE_CURVE('',#40256,#40257,#21923,.T.);
#49978=EDGE_CURVE('',#40257,#40258,#1133,.T.);
#49979=EDGE_CURVE('',#40258,#40259,#21924,.T.);
#49980=EDGE_CURVE('',#40259,#40248,#21925,.T.);
#49981=EDGE_CURVE('',#40260,#40261,#21926,.T.);
#49982=EDGE_CURVE('',#40261,#40262,#31766,.T.);
#49983=EDGE_CURVE('',#40262,#40263,#21927,.T.);
#49984=EDGE_CURVE('',#40263,#40260,#31767,.T.);
#49985=EDGE_CURVE('',#40264,#40265,#1134,.T.);
#49986=EDGE_CURVE('',#40265,#40266,#21928,.T.);
#49987=EDGE_CURVE('',#40266,#40267,#21929,.T.);
#49988=EDGE_CURVE('',#40267,#40268,#21930,.T.);
#49989=EDGE_CURVE('',#40268,#40269,#1135,.T.);
#49990=EDGE_CURVE('',#40269,#40270,#21931,.T.);
#49991=EDGE_CURVE('',#40270,#40271,#21932,.T.);
#49992=EDGE_CURVE('',#40271,#40272,#1136,.T.);
#49993=EDGE_CURVE('',#40272,#40273,#21933,.T.);
#49994=EDGE_CURVE('',#40273,#40274,#1137,.T.);
#49995=EDGE_CURVE('',#40274,#40275,#21934,.T.);
#49996=EDGE_CURVE('',#40275,#40264,#21935,.T.);
#49997=EDGE_CURVE('',#40276,#40277,#1138,.T.);
#49998=EDGE_CURVE('',#40277,#40278,#21936,.T.);
#49999=EDGE_CURVE('',#40278,#40279,#21937,.T.);
#50000=EDGE_CURVE('',#40279,#40280,#21938,.T.);
#50001=EDGE_CURVE('',#40280,#40281,#1139,.T.);
#50002=EDGE_CURVE('',#40281,#40282,#21939,.T.);
#50003=EDGE_CURVE('',#40282,#40283,#21940,.T.);
#50004=EDGE_CURVE('',#40283,#40284,#1140,.T.);
#50005=EDGE_CURVE('',#40284,#40285,#21941,.T.);
#50006=EDGE_CURVE('',#40285,#40286,#1141,.T.);
#50007=EDGE_CURVE('',#40286,#40287,#21942,.T.);
#50008=EDGE_CURVE('',#40287,#40276,#21943,.T.);
#50009=EDGE_CURVE('',#40288,#40289,#21944,.T.);
#50010=EDGE_CURVE('',#40289,#40290,#31768,.T.);
#50011=EDGE_CURVE('',#40290,#40291,#21945,.T.);
#50012=EDGE_CURVE('',#40291,#40288,#31769,.T.);
#50013=EDGE_CURVE('',#40292,#40293,#1142,.T.);
#50014=EDGE_CURVE('',#40293,#40294,#21946,.T.);
#50015=EDGE_CURVE('',#40294,#40295,#21947,.T.);
#50016=EDGE_CURVE('',#40295,#40296,#21948,.T.);
#50017=EDGE_CURVE('',#40296,#40297,#1143,.T.);
#50018=EDGE_CURVE('',#40297,#40298,#21949,.T.);
#50019=EDGE_CURVE('',#40298,#40299,#21950,.T.);
#50020=EDGE_CURVE('',#40299,#40300,#1144,.T.);
#50021=EDGE_CURVE('',#40300,#40301,#21951,.T.);
#50022=EDGE_CURVE('',#40301,#40302,#1145,.T.);
#50023=EDGE_CURVE('',#40302,#40303,#21952,.T.);
#50024=EDGE_CURVE('',#40303,#40292,#21953,.T.);
#50025=EDGE_CURVE('',#40304,#40305,#1146,.T.);
#50026=EDGE_CURVE('',#40305,#40306,#21954,.T.);
#50027=EDGE_CURVE('',#40306,#40307,#21955,.T.);
#50028=EDGE_CURVE('',#40307,#40308,#21956,.T.);
#50029=EDGE_CURVE('',#40308,#40309,#1147,.T.);
#50030=EDGE_CURVE('',#40309,#40310,#21957,.T.);
#50031=EDGE_CURVE('',#40310,#40311,#21958,.T.);
#50032=EDGE_CURVE('',#40311,#40312,#1148,.T.);
#50033=EDGE_CURVE('',#40312,#40313,#21959,.T.);
#50034=EDGE_CURVE('',#40313,#40314,#1149,.T.);
#50035=EDGE_CURVE('',#40314,#40315,#21960,.T.);
#50036=EDGE_CURVE('',#40315,#40304,#21961,.T.);
#50037=EDGE_CURVE('',#40316,#40317,#21962,.T.);
#50038=EDGE_CURVE('',#40317,#40318,#31770,.T.);
#50039=EDGE_CURVE('',#40318,#40319,#21963,.T.);
#50040=EDGE_CURVE('',#40319,#40316,#31771,.T.);
#50041=EDGE_CURVE('',#40320,#40321,#1150,.T.);
#50042=EDGE_CURVE('',#40321,#40322,#21964,.T.);
#50043=EDGE_CURVE('',#40322,#40323,#21965,.T.);
#50044=EDGE_CURVE('',#40323,#40324,#21966,.T.);
#50045=EDGE_CURVE('',#40324,#40325,#1151,.T.);
#50046=EDGE_CURVE('',#40325,#40326,#21967,.T.);
#50047=EDGE_CURVE('',#40326,#40327,#21968,.T.);
#50048=EDGE_CURVE('',#40327,#40328,#1152,.T.);
#50049=EDGE_CURVE('',#40328,#40329,#21969,.T.);
#50050=EDGE_CURVE('',#40329,#40330,#1153,.T.);
#50051=EDGE_CURVE('',#40330,#40331,#21970,.T.);
#50052=EDGE_CURVE('',#40331,#40320,#21971,.T.);
#50053=EDGE_CURVE('',#40332,#40333,#1154,.T.);
#50054=EDGE_CURVE('',#40333,#40334,#21972,.T.);
#50055=EDGE_CURVE('',#40334,#40335,#21973,.T.);
#50056=EDGE_CURVE('',#40335,#40336,#21974,.T.);
#50057=EDGE_CURVE('',#40336,#40337,#1155,.T.);
#50058=EDGE_CURVE('',#40337,#40338,#21975,.T.);
#50059=EDGE_CURVE('',#40338,#40339,#21976,.T.);
#50060=EDGE_CURVE('',#40339,#40340,#1156,.T.);
#50061=EDGE_CURVE('',#40340,#40341,#21977,.T.);
#50062=EDGE_CURVE('',#40341,#40342,#1157,.T.);
#50063=EDGE_CURVE('',#40342,#40343,#21978,.T.);
#50064=EDGE_CURVE('',#40343,#40332,#21979,.T.);
#50065=EDGE_CURVE('',#40344,#40345,#21980,.T.);
#50066=EDGE_CURVE('',#40345,#40346,#31772,.T.);
#50067=EDGE_CURVE('',#40346,#40347,#21981,.T.);
#50068=EDGE_CURVE('',#40347,#40344,#31773,.T.);
#50069=EDGE_CURVE('',#40348,#40349,#1158,.T.);
#50070=EDGE_CURVE('',#40349,#40350,#21982,.T.);
#50071=EDGE_CURVE('',#40350,#40351,#21983,.T.);
#50072=EDGE_CURVE('',#40351,#40352,#21984,.T.);
#50073=EDGE_CURVE('',#40352,#40353,#1159,.T.);
#50074=EDGE_CURVE('',#40353,#40354,#21985,.T.);
#50075=EDGE_CURVE('',#40354,#40355,#21986,.T.);
#50076=EDGE_CURVE('',#40355,#40356,#1160,.T.);
#50077=EDGE_CURVE('',#40356,#40357,#21987,.T.);
#50078=EDGE_CURVE('',#40357,#40358,#1161,.T.);
#50079=EDGE_CURVE('',#40358,#40359,#21988,.T.);
#50080=EDGE_CURVE('',#40359,#40348,#21989,.T.);
#50081=EDGE_CURVE('',#40360,#40361,#1162,.T.);
#50082=EDGE_CURVE('',#40361,#40362,#21990,.T.);
#50083=EDGE_CURVE('',#40362,#40363,#21991,.T.);
#50084=EDGE_CURVE('',#40363,#40364,#21992,.T.);
#50085=EDGE_CURVE('',#40364,#40365,#1163,.T.);
#50086=EDGE_CURVE('',#40365,#40366,#21993,.T.);
#50087=EDGE_CURVE('',#40366,#40367,#21994,.T.);
#50088=EDGE_CURVE('',#40367,#40368,#1164,.T.);
#50089=EDGE_CURVE('',#40368,#40369,#21995,.T.);
#50090=EDGE_CURVE('',#40369,#40370,#1165,.T.);
#50091=EDGE_CURVE('',#40370,#40371,#21996,.T.);
#50092=EDGE_CURVE('',#40371,#40360,#21997,.T.);
#50093=EDGE_CURVE('',#40372,#40373,#21998,.T.);
#50094=EDGE_CURVE('',#40373,#40374,#31774,.T.);
#50095=EDGE_CURVE('',#40374,#40375,#21999,.T.);
#50096=EDGE_CURVE('',#40375,#40372,#31775,.T.);
#50097=EDGE_CURVE('',#40376,#40377,#1166,.T.);
#50098=EDGE_CURVE('',#40377,#40378,#22000,.T.);
#50099=EDGE_CURVE('',#40378,#40379,#22001,.T.);
#50100=EDGE_CURVE('',#40379,#40380,#22002,.T.);
#50101=EDGE_CURVE('',#40380,#40381,#1167,.T.);
#50102=EDGE_CURVE('',#40381,#40382,#22003,.T.);
#50103=EDGE_CURVE('',#40382,#40383,#22004,.T.);
#50104=EDGE_CURVE('',#40383,#40384,#1168,.T.);
#50105=EDGE_CURVE('',#40384,#40385,#22005,.T.);
#50106=EDGE_CURVE('',#40385,#40386,#1169,.T.);
#50107=EDGE_CURVE('',#40386,#40387,#22006,.T.);
#50108=EDGE_CURVE('',#40387,#40376,#22007,.T.);
#50109=EDGE_CURVE('',#40388,#40389,#1170,.T.);
#50110=EDGE_CURVE('',#40389,#40390,#22008,.T.);
#50111=EDGE_CURVE('',#40390,#40391,#22009,.T.);
#50112=EDGE_CURVE('',#40391,#40392,#22010,.T.);
#50113=EDGE_CURVE('',#40392,#40393,#1171,.T.);
#50114=EDGE_CURVE('',#40393,#40394,#22011,.T.);
#50115=EDGE_CURVE('',#40394,#40395,#22012,.T.);
#50116=EDGE_CURVE('',#40395,#40396,#1172,.T.);
#50117=EDGE_CURVE('',#40396,#40397,#22013,.T.);
#50118=EDGE_CURVE('',#40397,#40398,#1173,.T.);
#50119=EDGE_CURVE('',#40398,#40399,#22014,.T.);
#50120=EDGE_CURVE('',#40399,#40388,#22015,.T.);
#50121=EDGE_CURVE('',#40400,#40401,#22016,.T.);
#50122=EDGE_CURVE('',#40401,#40402,#31776,.T.);
#50123=EDGE_CURVE('',#40402,#40403,#22017,.T.);
#50124=EDGE_CURVE('',#40403,#40400,#31777,.T.);
#50125=EDGE_CURVE('',#40404,#40405,#1174,.T.);
#50126=EDGE_CURVE('',#40405,#40406,#22018,.T.);
#50127=EDGE_CURVE('',#40406,#40407,#22019,.T.);
#50128=EDGE_CURVE('',#40407,#40408,#22020,.T.);
#50129=EDGE_CURVE('',#40408,#40409,#1175,.T.);
#50130=EDGE_CURVE('',#40409,#40410,#22021,.T.);
#50131=EDGE_CURVE('',#40410,#40411,#22022,.T.);
#50132=EDGE_CURVE('',#40411,#40412,#1176,.T.);
#50133=EDGE_CURVE('',#40412,#40413,#22023,.T.);
#50134=EDGE_CURVE('',#40413,#40414,#1177,.T.);
#50135=EDGE_CURVE('',#40414,#40415,#22024,.T.);
#50136=EDGE_CURVE('',#40415,#40404,#22025,.T.);
#50137=EDGE_CURVE('',#40416,#40417,#1178,.T.);
#50138=EDGE_CURVE('',#40417,#40418,#22026,.T.);
#50139=EDGE_CURVE('',#40418,#40419,#22027,.T.);
#50140=EDGE_CURVE('',#40419,#40420,#22028,.T.);
#50141=EDGE_CURVE('',#40420,#40421,#1179,.T.);
#50142=EDGE_CURVE('',#40421,#40422,#22029,.T.);
#50143=EDGE_CURVE('',#40422,#40423,#22030,.T.);
#50144=EDGE_CURVE('',#40423,#40424,#1180,.T.);
#50145=EDGE_CURVE('',#40424,#40425,#22031,.T.);
#50146=EDGE_CURVE('',#40425,#40426,#1181,.T.);
#50147=EDGE_CURVE('',#40426,#40427,#22032,.T.);
#50148=EDGE_CURVE('',#40427,#40416,#22033,.T.);
#50149=EDGE_CURVE('',#38802,#38785,#4499,.T.);
#50150=EDGE_CURVE('',#38784,#38803,#4500,.T.);
#50151=EDGE_CURVE('',#38786,#38791,#4501,.T.);
#50152=EDGE_CURVE('',#38790,#38787,#4502,.T.);
#50153=EDGE_CURVE('',#38830,#38813,#4503,.T.);
#50154=EDGE_CURVE('',#38812,#38831,#4504,.T.);
#50155=EDGE_CURVE('',#38814,#38819,#4505,.T.);
#50156=EDGE_CURVE('',#38818,#38815,#4506,.T.);
#50157=EDGE_CURVE('',#38858,#38841,#4507,.T.);
#50158=EDGE_CURVE('',#38840,#38859,#4508,.T.);
#50159=EDGE_CURVE('',#38842,#38847,#4509,.T.);
#50160=EDGE_CURVE('',#38846,#38843,#4510,.T.);
#50161=EDGE_CURVE('',#38886,#38869,#4511,.T.);
#50162=EDGE_CURVE('',#38868,#38887,#4512,.T.);
#50163=EDGE_CURVE('',#38870,#38875,#4513,.T.);
#50164=EDGE_CURVE('',#38874,#38871,#4514,.T.);
#50165=EDGE_CURVE('',#38914,#38897,#4515,.T.);
#50166=EDGE_CURVE('',#38896,#38915,#4516,.T.);
#50167=EDGE_CURVE('',#38898,#38903,#4517,.T.);
#50168=EDGE_CURVE('',#38902,#38899,#4518,.T.);
#50169=EDGE_CURVE('',#38942,#38925,#4519,.T.);
#50170=EDGE_CURVE('',#38924,#38943,#4520,.T.);
#50171=EDGE_CURVE('',#38926,#38931,#4521,.T.);
#50172=EDGE_CURVE('',#38930,#38927,#4522,.T.);
#50173=EDGE_CURVE('',#38970,#38953,#4523,.T.);
#50174=EDGE_CURVE('',#38952,#38971,#4524,.T.);
#50175=EDGE_CURVE('',#38954,#38959,#4525,.T.);
#50176=EDGE_CURVE('',#38958,#38955,#4526,.T.);
#50177=EDGE_CURVE('',#38998,#38981,#4527,.T.);
#50178=EDGE_CURVE('',#38980,#38999,#4528,.T.);
#50179=EDGE_CURVE('',#38982,#38987,#4529,.T.);
#50180=EDGE_CURVE('',#38986,#38983,#4530,.T.);
#50181=EDGE_CURVE('',#39026,#39009,#4531,.T.);
#50182=EDGE_CURVE('',#39008,#39027,#4532,.T.);
#50183=EDGE_CURVE('',#39010,#39015,#4533,.T.);
#50184=EDGE_CURVE('',#39014,#39011,#4534,.T.);
#50185=EDGE_CURVE('',#39054,#39037,#4535,.T.);
#50186=EDGE_CURVE('',#39036,#39055,#4536,.T.);
#50187=EDGE_CURVE('',#39038,#39043,#4537,.T.);
#50188=EDGE_CURVE('',#39042,#39039,#4538,.T.);
#50189=EDGE_CURVE('',#39082,#39065,#4539,.T.);
#50190=EDGE_CURVE('',#39064,#39083,#4540,.T.);
#50191=EDGE_CURVE('',#39066,#39071,#4541,.T.);
#50192=EDGE_CURVE('',#39070,#39067,#4542,.T.);
#50193=EDGE_CURVE('',#39110,#39093,#4543,.T.);
#50194=EDGE_CURVE('',#39092,#39111,#4544,.T.);
#50195=EDGE_CURVE('',#39094,#39099,#4545,.T.);
#50196=EDGE_CURVE('',#39098,#39095,#4546,.T.);
#50197=EDGE_CURVE('',#39138,#39121,#4547,.T.);
#50198=EDGE_CURVE('',#39120,#39139,#4548,.T.);
#50199=EDGE_CURVE('',#39122,#39127,#4549,.T.);
#50200=EDGE_CURVE('',#39126,#39123,#4550,.T.);
#50201=EDGE_CURVE('',#39166,#39149,#4551,.T.);
#50202=EDGE_CURVE('',#39148,#39167,#4552,.T.);
#50203=EDGE_CURVE('',#39150,#39155,#4553,.T.);
#50204=EDGE_CURVE('',#39154,#39151,#4554,.T.);
#50205=EDGE_CURVE('',#39194,#39177,#4555,.T.);
#50206=EDGE_CURVE('',#39176,#39195,#4556,.T.);
#50207=EDGE_CURVE('',#39178,#39183,#4557,.T.);
#50208=EDGE_CURVE('',#39182,#39179,#4558,.T.);
#50209=EDGE_CURVE('',#39222,#39205,#4559,.T.);
#50210=EDGE_CURVE('',#39204,#39223,#4560,.T.);
#50211=EDGE_CURVE('',#39206,#39211,#4561,.T.);
#50212=EDGE_CURVE('',#39210,#39207,#4562,.T.);
#50213=EDGE_CURVE('',#39250,#39233,#4563,.T.);
#50214=EDGE_CURVE('',#39232,#39251,#4564,.T.);
#50215=EDGE_CURVE('',#39234,#39239,#4565,.T.);
#50216=EDGE_CURVE('',#39238,#39235,#4566,.T.);
#50217=EDGE_CURVE('',#39278,#39261,#4567,.T.);
#50218=EDGE_CURVE('',#39260,#39279,#4568,.T.);
#50219=EDGE_CURVE('',#39262,#39267,#4569,.T.);
#50220=EDGE_CURVE('',#39266,#39263,#4570,.T.);
#50221=EDGE_CURVE('',#39306,#39289,#4571,.T.);
#50222=EDGE_CURVE('',#39288,#39307,#4572,.T.);
#50223=EDGE_CURVE('',#39290,#39295,#4573,.T.);
#50224=EDGE_CURVE('',#39294,#39291,#4574,.T.);
#50225=EDGE_CURVE('',#39334,#39317,#4575,.T.);
#50226=EDGE_CURVE('',#39316,#39335,#4576,.T.);
#50227=EDGE_CURVE('',#39318,#39323,#4577,.T.);
#50228=EDGE_CURVE('',#39322,#39319,#4578,.T.);
#50229=EDGE_CURVE('',#39362,#39345,#4579,.T.);
#50230=EDGE_CURVE('',#39344,#39363,#4580,.T.);
#50231=EDGE_CURVE('',#39346,#39351,#4581,.T.);
#50232=EDGE_CURVE('',#39350,#39347,#4582,.T.);
#50233=EDGE_CURVE('',#39390,#39373,#4583,.T.);
#50234=EDGE_CURVE('',#39372,#39391,#4584,.T.);
#50235=EDGE_CURVE('',#39374,#39379,#4585,.T.);
#50236=EDGE_CURVE('',#39378,#39375,#4586,.T.);
#50237=EDGE_CURVE('',#39418,#39401,#4587,.T.);
#50238=EDGE_CURVE('',#39400,#39419,#4588,.T.);
#50239=EDGE_CURVE('',#39402,#39407,#4589,.T.);
#50240=EDGE_CURVE('',#39406,#39403,#4590,.T.);
#50241=EDGE_CURVE('',#39446,#39429,#4591,.T.);
#50242=EDGE_CURVE('',#39428,#39447,#4592,.T.);
#50243=EDGE_CURVE('',#39430,#39435,#4593,.T.);
#50244=EDGE_CURVE('',#39434,#39431,#4594,.T.);
#50245=EDGE_CURVE('',#39474,#39457,#4595,.T.);
#50246=EDGE_CURVE('',#39456,#39475,#4596,.T.);
#50247=EDGE_CURVE('',#39458,#39463,#4597,.T.);
#50248=EDGE_CURVE('',#39462,#39459,#4598,.T.);
#50249=EDGE_CURVE('',#39502,#39485,#4599,.T.);
#50250=EDGE_CURVE('',#39484,#39503,#4600,.T.);
#50251=EDGE_CURVE('',#39486,#39491,#4601,.T.);
#50252=EDGE_CURVE('',#39490,#39487,#4602,.T.);
#50253=EDGE_CURVE('',#39530,#39513,#4603,.T.);
#50254=EDGE_CURVE('',#39512,#39531,#4604,.T.);
#50255=EDGE_CURVE('',#39514,#39519,#4605,.T.);
#50256=EDGE_CURVE('',#39518,#39515,#4606,.T.);
#50257=EDGE_CURVE('',#39558,#39541,#4607,.T.);
#50258=EDGE_CURVE('',#39540,#39559,#4608,.T.);
#50259=EDGE_CURVE('',#39542,#39547,#4609,.T.);
#50260=EDGE_CURVE('',#39546,#39543,#4610,.T.);
#50261=EDGE_CURVE('',#39586,#39569,#4611,.T.);
#50262=EDGE_CURVE('',#39568,#39587,#4612,.T.);
#50263=EDGE_CURVE('',#39570,#39575,#4613,.T.);
#50264=EDGE_CURVE('',#39574,#39571,#4614,.T.);
#50265=EDGE_CURVE('',#39610,#36826,#4615,.T.);
#50266=EDGE_CURVE('',#36820,#39611,#4616,.T.);
#50267=EDGE_CURVE('',#36825,#39599,#4617,.T.);
#50268=EDGE_CURVE('',#39598,#36819,#4618,.T.);
#50269=EDGE_CURVE('',#39638,#39621,#4619,.T.);
#50270=EDGE_CURVE('',#39620,#39639,#4620,.T.);
#50271=EDGE_CURVE('',#39622,#39627,#4621,.T.);
#50272=EDGE_CURVE('',#39626,#39623,#4622,.T.);
#50273=EDGE_CURVE('',#39666,#39649,#4623,.T.);
#50274=EDGE_CURVE('',#39648,#39667,#4624,.T.);
#50275=EDGE_CURVE('',#39650,#39655,#4625,.T.);
#50276=EDGE_CURVE('',#39654,#39651,#4626,.T.);
#50277=EDGE_CURVE('',#39694,#39677,#4627,.T.);
#50278=EDGE_CURVE('',#39676,#39695,#4628,.T.);
#50279=EDGE_CURVE('',#39678,#39683,#4629,.T.);
#50280=EDGE_CURVE('',#39682,#39679,#4630,.T.);
#50281=EDGE_CURVE('',#39722,#39705,#4631,.T.);
#50282=EDGE_CURVE('',#39704,#39723,#4632,.T.);
#50283=EDGE_CURVE('',#39706,#39711,#4633,.T.);
#50284=EDGE_CURVE('',#39710,#39707,#4634,.T.);
#50285=EDGE_CURVE('',#39750,#39733,#4635,.T.);
#50286=EDGE_CURVE('',#39732,#39751,#4636,.T.);
#50287=EDGE_CURVE('',#39734,#39739,#4637,.T.);
#50288=EDGE_CURVE('',#39738,#39735,#4638,.T.);
#50289=EDGE_CURVE('',#39778,#39761,#4639,.T.);
#50290=EDGE_CURVE('',#39760,#39779,#4640,.T.);
#50291=EDGE_CURVE('',#39762,#39767,#4641,.T.);
#50292=EDGE_CURVE('',#39766,#39763,#4642,.T.);
#50293=EDGE_CURVE('',#39806,#39789,#4643,.T.);
#50294=EDGE_CURVE('',#39788,#39807,#4644,.T.);
#50295=EDGE_CURVE('',#39790,#39795,#4645,.T.);
#50296=EDGE_CURVE('',#39794,#39791,#4646,.T.);
#50297=EDGE_CURVE('',#39834,#39817,#4647,.T.);
#50298=EDGE_CURVE('',#39816,#39835,#4648,.T.);
#50299=EDGE_CURVE('',#39818,#39823,#4649,.T.);
#50300=EDGE_CURVE('',#39822,#39819,#4650,.T.);
#50301=EDGE_CURVE('',#39862,#39845,#4651,.T.);
#50302=EDGE_CURVE('',#39844,#39863,#4652,.T.);
#50303=EDGE_CURVE('',#39846,#39851,#4653,.T.);
#50304=EDGE_CURVE('',#39850,#39847,#4654,.T.);
#50305=EDGE_CURVE('',#39890,#39873,#4655,.T.);
#50306=EDGE_CURVE('',#39872,#39891,#4656,.T.);
#50307=EDGE_CURVE('',#39874,#39879,#4657,.T.);
#50308=EDGE_CURVE('',#39878,#39875,#4658,.T.);
#50309=EDGE_CURVE('',#39918,#39901,#4659,.T.);
#50310=EDGE_CURVE('',#39900,#39919,#4660,.T.);
#50311=EDGE_CURVE('',#39902,#39907,#4661,.T.);
#50312=EDGE_CURVE('',#39906,#39903,#4662,.T.);
#50313=EDGE_CURVE('',#39946,#39929,#4663,.T.);
#50314=EDGE_CURVE('',#39928,#39947,#4664,.T.);
#50315=EDGE_CURVE('',#39930,#39935,#4665,.T.);
#50316=EDGE_CURVE('',#39934,#39931,#4666,.T.);
#50317=EDGE_CURVE('',#39974,#39957,#4667,.T.);
#50318=EDGE_CURVE('',#39956,#39975,#4668,.T.);
#50319=EDGE_CURVE('',#39958,#39963,#4669,.T.);
#50320=EDGE_CURVE('',#39962,#39959,#4670,.T.);
#50321=EDGE_CURVE('',#40002,#39985,#4671,.T.);
#50322=EDGE_CURVE('',#39984,#40003,#4672,.T.);
#50323=EDGE_CURVE('',#39986,#39991,#4673,.T.);
#50324=EDGE_CURVE('',#39990,#39987,#4674,.T.);
#50325=EDGE_CURVE('',#40026,#36818,#4675,.T.);
#50326=EDGE_CURVE('',#36812,#40027,#4676,.T.);
#50327=EDGE_CURVE('',#36817,#40015,#4677,.T.);
#50328=EDGE_CURVE('',#40014,#36811,#4678,.T.);
#50329=EDGE_CURVE('',#40054,#40037,#4679,.T.);
#50330=EDGE_CURVE('',#40036,#40055,#4680,.T.);
#50331=EDGE_CURVE('',#40038,#40043,#4681,.T.);
#50332=EDGE_CURVE('',#40042,#40039,#4682,.T.);
#50333=EDGE_CURVE('',#40082,#40065,#4683,.T.);
#50334=EDGE_CURVE('',#40064,#40083,#4684,.T.);
#50335=EDGE_CURVE('',#40066,#40071,#4685,.T.);
#50336=EDGE_CURVE('',#40070,#40067,#4686,.T.);
#50337=EDGE_CURVE('',#40110,#40093,#4687,.T.);
#50338=EDGE_CURVE('',#40092,#40111,#4688,.T.);
#50339=EDGE_CURVE('',#40094,#40099,#4689,.T.);
#50340=EDGE_CURVE('',#40098,#40095,#4690,.T.);
#50341=EDGE_CURVE('',#40138,#40121,#4691,.T.);
#50342=EDGE_CURVE('',#40120,#40139,#4692,.T.);
#50343=EDGE_CURVE('',#40122,#40127,#4693,.T.);
#50344=EDGE_CURVE('',#40126,#40123,#4694,.T.);
#50345=EDGE_CURVE('',#40166,#40149,#4695,.T.);
#50346=EDGE_CURVE('',#40148,#40167,#4696,.T.);
#50347=EDGE_CURVE('',#40150,#40155,#4697,.T.);
#50348=EDGE_CURVE('',#40154,#40151,#4698,.T.);
#50349=EDGE_CURVE('',#40194,#40177,#4699,.T.);
#50350=EDGE_CURVE('',#40176,#40195,#4700,.T.);
#50351=EDGE_CURVE('',#40178,#40183,#4701,.T.);
#50352=EDGE_CURVE('',#40182,#40179,#4702,.T.);
#50353=EDGE_CURVE('',#40222,#40205,#4703,.T.);
#50354=EDGE_CURVE('',#40204,#40223,#4704,.T.);
#50355=EDGE_CURVE('',#40206,#40211,#4705,.T.);
#50356=EDGE_CURVE('',#40210,#40207,#4706,.T.);
#50357=EDGE_CURVE('',#40250,#40233,#4707,.T.);
#50358=EDGE_CURVE('',#40232,#40251,#4708,.T.);
#50359=EDGE_CURVE('',#40234,#40239,#4709,.T.);
#50360=EDGE_CURVE('',#40238,#40235,#4710,.T.);
#50361=EDGE_CURVE('',#40278,#40261,#4711,.T.);
#50362=EDGE_CURVE('',#40260,#40279,#4712,.T.);
#50363=EDGE_CURVE('',#40262,#40267,#4713,.T.);
#50364=EDGE_CURVE('',#40266,#40263,#4714,.T.);
#50365=EDGE_CURVE('',#40306,#40289,#4715,.T.);
#50366=EDGE_CURVE('',#40288,#40307,#4716,.T.);
#50367=EDGE_CURVE('',#40290,#40295,#4717,.T.);
#50368=EDGE_CURVE('',#40294,#40291,#4718,.T.);
#50369=EDGE_CURVE('',#40334,#40317,#4719,.T.);
#50370=EDGE_CURVE('',#40316,#40335,#4720,.T.);
#50371=EDGE_CURVE('',#40318,#40323,#4721,.T.);
#50372=EDGE_CURVE('',#40322,#40319,#4722,.T.);
#50373=EDGE_CURVE('',#40362,#40345,#4723,.T.);
#50374=EDGE_CURVE('',#40344,#40363,#4724,.T.);
#50375=EDGE_CURVE('',#40346,#40351,#4725,.T.);
#50376=EDGE_CURVE('',#40350,#40347,#4726,.T.);
#50377=EDGE_CURVE('',#40390,#40373,#4727,.T.);
#50378=EDGE_CURVE('',#40372,#40391,#4728,.T.);
#50379=EDGE_CURVE('',#40374,#40379,#4729,.T.);
#50380=EDGE_CURVE('',#40378,#40375,#4730,.T.);
#50381=EDGE_CURVE('',#40418,#40401,#4731,.T.);
#50382=EDGE_CURVE('',#40400,#40419,#4732,.T.);
#50383=EDGE_CURVE('',#40402,#40407,#4733,.T.);
#50384=EDGE_CURVE('',#40406,#40403,#4734,.T.);
#50385=EDGE_CURVE('',#38811,#38733,#1182,.T.);
#50386=EDGE_CURVE('',#38728,#38810,#31778,.T.);
#50387=EDGE_CURVE('',#38727,#38809,#31779,.T.);
#50388=EDGE_CURVE('',#38800,#38735,#31780,.T.);
#50389=EDGE_CURVE('',#38724,#38808,#31781,.T.);
#50390=EDGE_CURVE('',#38801,#36849,#31782,.T.);
#50391=EDGE_CURVE('',#38723,#38807,#31783,.T.);
#50392=EDGE_CURVE('',#38802,#36848,#31784,.T.);
#50393=EDGE_CURVE('',#38721,#38806,#1183,.T.);
#50394=EDGE_CURVE('',#38785,#36847,#31785,.T.);
#50395=EDGE_CURVE('',#38716,#38805,#31786,.T.);
#50396=EDGE_CURVE('',#38786,#36846,#31787,.T.);
#50397=EDGE_CURVE('',#37366,#38804,#31788,.T.);
#50398=EDGE_CURVE('',#38791,#36845,#31789,.T.);
#50399=EDGE_CURVE('',#37367,#38803,#31790,.T.);
#50400=EDGE_CURVE('',#38792,#36844,#31791,.T.);
#50401=EDGE_CURVE('',#37368,#38784,#31792,.T.);
#50402=EDGE_CURVE('',#38793,#38754,#31793,.T.);
#50403=EDGE_CURVE('',#37369,#38787,#31794,.T.);
#50404=EDGE_CURVE('',#38794,#38750,#1184,.T.);
#50405=EDGE_CURVE('',#37370,#38790,#31795,.T.);
#50406=EDGE_CURVE('',#38795,#38749,#31796,.T.);
#50407=EDGE_CURVE('',#37371,#38789,#31797,.T.);
#50408=EDGE_CURVE('',#38796,#38746,#31798,.T.);
#50409=EDGE_CURVE('',#38737,#38788,#31799,.T.);
#50410=EDGE_CURVE('',#38797,#38745,#31800,.T.);
#50411=EDGE_CURVE('',#38738,#38799,#1185,.T.);
#50412=EDGE_CURVE('',#38798,#38742,#31801,.T.);
#50413=EDGE_CURVE('',#38839,#38713,#1186,.T.);
#50414=EDGE_CURVE('',#38708,#38838,#31802,.T.);
#50415=EDGE_CURVE('',#38707,#38837,#31803,.T.);
#50416=EDGE_CURVE('',#38828,#38715,#31804,.T.);
#50417=EDGE_CURVE('',#38704,#38836,#31805,.T.);
#50418=EDGE_CURVE('',#38829,#36855,#31806,.T.);
#50419=EDGE_CURVE('',#38703,#38835,#31807,.T.);
#50420=EDGE_CURVE('',#38830,#36854,#31808,.T.);
#50421=EDGE_CURVE('',#38701,#38834,#1187,.T.);
#50422=EDGE_CURVE('',#38813,#36853,#31809,.T.);
#50423=EDGE_CURVE('',#38696,#38833,#31810,.T.);
#50424=EDGE_CURVE('',#38814,#36852,#31811,.T.);
#50425=EDGE_CURVE('',#37360,#38832,#31812,.T.);
#50426=EDGE_CURVE('',#38819,#36851,#31813,.T.);
#50427=EDGE_CURVE('',#37361,#38831,#31814,.T.);
#50428=EDGE_CURVE('',#38820,#36850,#31815,.T.);
#50429=EDGE_CURVE('',#37362,#38812,#31816,.T.);
#50430=EDGE_CURVE('',#38821,#38734,#31817,.T.);
#50431=EDGE_CURVE('',#37363,#38815,#31818,.T.);
#50432=EDGE_CURVE('',#38822,#38730,#1188,.T.);
#50433=EDGE_CURVE('',#37364,#38818,#31819,.T.);
#50434=EDGE_CURVE('',#38823,#38729,#31820,.T.);
#50435=EDGE_CURVE('',#37365,#38817,#31821,.T.);
#50436=EDGE_CURVE('',#38824,#38726,#31822,.T.);
#50437=EDGE_CURVE('',#38717,#38816,#31823,.T.);
#50438=EDGE_CURVE('',#38825,#38725,#31824,.T.);
#50439=EDGE_CURVE('',#38718,#38827,#1189,.T.);
#50440=EDGE_CURVE('',#38826,#38722,#31825,.T.);
#50441=EDGE_CURVE('',#38867,#38693,#1190,.T.);
#50442=EDGE_CURVE('',#38688,#38866,#31826,.T.);
#50443=EDGE_CURVE('',#38687,#38865,#31827,.T.);
#50444=EDGE_CURVE('',#38856,#38695,#31828,.T.);
#50445=EDGE_CURVE('',#38684,#38864,#31829,.T.);
#50446=EDGE_CURVE('',#38857,#36861,#31830,.T.);
#50447=EDGE_CURVE('',#38683,#38863,#31831,.T.);
#50448=EDGE_CURVE('',#38858,#36860,#31832,.T.);
#50449=EDGE_CURVE('',#38681,#38862,#1191,.T.);
#50450=EDGE_CURVE('',#38841,#36859,#31833,.T.);
#50451=EDGE_CURVE('',#38676,#38861,#31834,.T.);
#50452=EDGE_CURVE('',#38842,#36858,#31835,.T.);
#50453=EDGE_CURVE('',#37354,#38860,#31836,.T.);
#50454=EDGE_CURVE('',#38847,#36857,#31837,.T.);
#50455=EDGE_CURVE('',#37355,#38859,#31838,.T.);
#50456=EDGE_CURVE('',#38848,#36856,#31839,.T.);
#50457=EDGE_CURVE('',#37356,#38840,#31840,.T.);
#50458=EDGE_CURVE('',#38849,#38714,#31841,.T.);
#50459=EDGE_CURVE('',#37357,#38843,#31842,.T.);
#50460=EDGE_CURVE('',#38850,#38710,#1192,.T.);
#50461=EDGE_CURVE('',#37358,#38846,#31843,.T.);
#50462=EDGE_CURVE('',#38851,#38709,#31844,.T.);
#50463=EDGE_CURVE('',#37359,#38845,#31845,.T.);
#50464=EDGE_CURVE('',#38852,#38706,#31846,.T.);
#50465=EDGE_CURVE('',#38697,#38844,#31847,.T.);
#50466=EDGE_CURVE('',#38853,#38705,#31848,.T.);
#50467=EDGE_CURVE('',#38698,#38855,#1193,.T.);
#50468=EDGE_CURVE('',#38854,#38702,#31849,.T.);
#50469=EDGE_CURVE('',#38895,#38673,#1194,.T.);
#50470=EDGE_CURVE('',#38668,#38894,#31850,.T.);
#50471=EDGE_CURVE('',#38667,#38893,#31851,.T.);
#50472=EDGE_CURVE('',#38884,#38675,#31852,.T.);
#50473=EDGE_CURVE('',#38664,#38892,#31853,.T.);
#50474=EDGE_CURVE('',#38885,#36867,#31854,.T.);
#50475=EDGE_CURVE('',#38663,#38891,#31855,.T.);
#50476=EDGE_CURVE('',#38886,#36866,#31856,.T.);
#50477=EDGE_CURVE('',#38661,#38890,#1195,.T.);
#50478=EDGE_CURVE('',#38869,#36865,#31857,.T.);
#50479=EDGE_CURVE('',#38656,#38889,#31858,.T.);
#50480=EDGE_CURVE('',#38870,#36864,#31859,.T.);
#50481=EDGE_CURVE('',#37348,#38888,#31860,.T.);
#50482=EDGE_CURVE('',#38875,#36863,#31861,.T.);
#50483=EDGE_CURVE('',#37349,#38887,#31862,.T.);
#50484=EDGE_CURVE('',#38876,#36862,#31863,.T.);
#50485=EDGE_CURVE('',#37350,#38868,#31864,.T.);
#50486=EDGE_CURVE('',#38877,#38694,#31865,.T.);
#50487=EDGE_CURVE('',#37351,#38871,#31866,.T.);
#50488=EDGE_CURVE('',#38878,#38690,#1196,.T.);
#50489=EDGE_CURVE('',#37352,#38874,#31867,.T.);
#50490=EDGE_CURVE('',#38879,#38689,#31868,.T.);
#50491=EDGE_CURVE('',#37353,#38873,#31869,.T.);
#50492=EDGE_CURVE('',#38880,#38686,#31870,.T.);
#50493=EDGE_CURVE('',#38677,#38872,#31871,.T.);
#50494=EDGE_CURVE('',#38881,#38685,#31872,.T.);
#50495=EDGE_CURVE('',#38678,#38883,#1197,.T.);
#50496=EDGE_CURVE('',#38882,#38682,#31873,.T.);
#50497=EDGE_CURVE('',#38923,#38653,#1198,.T.);
#50498=EDGE_CURVE('',#38648,#38922,#31874,.T.);
#50499=EDGE_CURVE('',#38647,#38921,#31875,.T.);
#50500=EDGE_CURVE('',#38912,#38655,#31876,.T.);
#50501=EDGE_CURVE('',#38644,#38920,#31877,.T.);
#50502=EDGE_CURVE('',#38913,#36873,#31878,.T.);
#50503=EDGE_CURVE('',#38643,#38919,#31879,.T.);
#50504=EDGE_CURVE('',#38914,#36872,#31880,.T.);
#50505=EDGE_CURVE('',#38641,#38918,#1199,.T.);
#50506=EDGE_CURVE('',#38897,#36871,#31881,.T.);
#50507=EDGE_CURVE('',#38636,#38917,#31882,.T.);
#50508=EDGE_CURVE('',#38898,#36870,#31883,.T.);
#50509=EDGE_CURVE('',#37342,#38916,#31884,.T.);
#50510=EDGE_CURVE('',#38903,#36869,#31885,.T.);
#50511=EDGE_CURVE('',#37343,#38915,#31886,.T.);
#50512=EDGE_CURVE('',#38904,#36868,#31887,.T.);
#50513=EDGE_CURVE('',#37344,#38896,#31888,.T.);
#50514=EDGE_CURVE('',#38905,#38674,#31889,.T.);
#50515=EDGE_CURVE('',#37345,#38899,#31890,.T.);
#50516=EDGE_CURVE('',#38906,#38670,#1200,.T.);
#50517=EDGE_CURVE('',#37346,#38902,#31891,.T.);
#50518=EDGE_CURVE('',#38907,#38669,#31892,.T.);
#50519=EDGE_CURVE('',#37347,#38901,#31893,.T.);
#50520=EDGE_CURVE('',#38908,#38666,#31894,.T.);
#50521=EDGE_CURVE('',#38657,#38900,#31895,.T.);
#50522=EDGE_CURVE('',#38909,#38665,#31896,.T.);
#50523=EDGE_CURVE('',#38658,#38911,#1201,.T.);
#50524=EDGE_CURVE('',#38910,#38662,#31897,.T.);
#50525=EDGE_CURVE('',#38951,#38633,#1202,.T.);
#50526=EDGE_CURVE('',#38628,#38950,#31898,.T.);
#50527=EDGE_CURVE('',#38627,#38949,#31899,.T.);
#50528=EDGE_CURVE('',#38940,#38635,#31900,.T.);
#50529=EDGE_CURVE('',#38624,#38948,#31901,.T.);
#50530=EDGE_CURVE('',#38941,#36879,#31902,.T.);
#50531=EDGE_CURVE('',#38623,#38947,#31903,.T.);
#50532=EDGE_CURVE('',#38942,#36878,#31904,.T.);
#50533=EDGE_CURVE('',#38621,#38946,#1203,.T.);
#50534=EDGE_CURVE('',#38925,#36877,#31905,.T.);
#50535=EDGE_CURVE('',#38616,#38945,#31906,.T.);
#50536=EDGE_CURVE('',#38926,#36876,#31907,.T.);
#50537=EDGE_CURVE('',#37336,#38944,#31908,.T.);
#50538=EDGE_CURVE('',#38931,#36875,#31909,.T.);
#50539=EDGE_CURVE('',#37337,#38943,#31910,.T.);
#50540=EDGE_CURVE('',#38932,#36874,#31911,.T.);
#50541=EDGE_CURVE('',#37338,#38924,#31912,.T.);
#50542=EDGE_CURVE('',#38933,#38654,#31913,.T.);
#50543=EDGE_CURVE('',#37339,#38927,#31914,.T.);
#50544=EDGE_CURVE('',#38934,#38650,#1204,.T.);
#50545=EDGE_CURVE('',#37340,#38930,#31915,.T.);
#50546=EDGE_CURVE('',#38935,#38649,#31916,.T.);
#50547=EDGE_CURVE('',#37341,#38929,#31917,.T.);
#50548=EDGE_CURVE('',#38936,#38646,#31918,.T.);
#50549=EDGE_CURVE('',#38637,#38928,#31919,.T.);
#50550=EDGE_CURVE('',#38937,#38645,#31920,.T.);
#50551=EDGE_CURVE('',#38638,#38939,#1205,.T.);
#50552=EDGE_CURVE('',#38938,#38642,#31921,.T.);
#50553=EDGE_CURVE('',#38979,#38613,#1206,.T.);
#50554=EDGE_CURVE('',#38608,#38978,#31922,.T.);
#50555=EDGE_CURVE('',#38607,#38977,#31923,.T.);
#50556=EDGE_CURVE('',#38968,#38615,#31924,.T.);
#50557=EDGE_CURVE('',#38604,#38976,#31925,.T.);
#50558=EDGE_CURVE('',#38969,#36885,#31926,.T.);
#50559=EDGE_CURVE('',#38603,#38975,#31927,.T.);
#50560=EDGE_CURVE('',#38970,#36884,#31928,.T.);
#50561=EDGE_CURVE('',#38601,#38974,#1207,.T.);
#50562=EDGE_CURVE('',#38953,#36883,#31929,.T.);
#50563=EDGE_CURVE('',#38596,#38973,#31930,.T.);
#50564=EDGE_CURVE('',#38954,#36882,#31931,.T.);
#50565=EDGE_CURVE('',#37330,#38972,#31932,.T.);
#50566=EDGE_CURVE('',#38959,#36881,#31933,.T.);
#50567=EDGE_CURVE('',#37331,#38971,#31934,.T.);
#50568=EDGE_CURVE('',#38960,#36880,#31935,.T.);
#50569=EDGE_CURVE('',#37332,#38952,#31936,.T.);
#50570=EDGE_CURVE('',#38961,#38634,#31937,.T.);
#50571=EDGE_CURVE('',#37333,#38955,#31938,.T.);
#50572=EDGE_CURVE('',#38962,#38630,#1208,.T.);
#50573=EDGE_CURVE('',#37334,#38958,#31939,.T.);
#50574=EDGE_CURVE('',#38963,#38629,#31940,.T.);
#50575=EDGE_CURVE('',#37335,#38957,#31941,.T.);
#50576=EDGE_CURVE('',#38964,#38626,#31942,.T.);
#50577=EDGE_CURVE('',#38617,#38956,#31943,.T.);
#50578=EDGE_CURVE('',#38965,#38625,#31944,.T.);
#50579=EDGE_CURVE('',#38618,#38967,#1209,.T.);
#50580=EDGE_CURVE('',#38966,#38622,#31945,.T.);
#50581=EDGE_CURVE('',#39007,#38593,#1210,.T.);
#50582=EDGE_CURVE('',#38588,#39006,#31946,.T.);
#50583=EDGE_CURVE('',#38587,#39005,#31947,.T.);
#50584=EDGE_CURVE('',#38996,#38595,#31948,.T.);
#50585=EDGE_CURVE('',#38584,#39004,#31949,.T.);
#50586=EDGE_CURVE('',#38997,#36891,#31950,.T.);
#50587=EDGE_CURVE('',#38583,#39003,#31951,.T.);
#50588=EDGE_CURVE('',#38998,#36890,#31952,.T.);
#50589=EDGE_CURVE('',#38581,#39002,#1211,.T.);
#50590=EDGE_CURVE('',#38981,#36889,#31953,.T.);
#50591=EDGE_CURVE('',#38576,#39001,#31954,.T.);
#50592=EDGE_CURVE('',#38982,#36888,#31955,.T.);
#50593=EDGE_CURVE('',#37324,#39000,#31956,.T.);
#50594=EDGE_CURVE('',#38987,#36887,#31957,.T.);
#50595=EDGE_CURVE('',#37325,#38999,#31958,.T.);
#50596=EDGE_CURVE('',#38988,#36886,#31959,.T.);
#50597=EDGE_CURVE('',#37326,#38980,#31960,.T.);
#50598=EDGE_CURVE('',#38989,#38614,#31961,.T.);
#50599=EDGE_CURVE('',#37327,#38983,#31962,.T.);
#50600=EDGE_CURVE('',#38990,#38610,#1212,.T.);
#50601=EDGE_CURVE('',#37328,#38986,#31963,.T.);
#50602=EDGE_CURVE('',#38991,#38609,#31964,.T.);
#50603=EDGE_CURVE('',#37329,#38985,#31965,.T.);
#50604=EDGE_CURVE('',#38992,#38606,#31966,.T.);
#50605=EDGE_CURVE('',#38597,#38984,#31967,.T.);
#50606=EDGE_CURVE('',#38993,#38605,#31968,.T.);
#50607=EDGE_CURVE('',#38598,#38995,#1213,.T.);
#50608=EDGE_CURVE('',#38994,#38602,#31969,.T.);
#50609=EDGE_CURVE('',#39035,#38573,#1214,.T.);
#50610=EDGE_CURVE('',#38568,#39034,#31970,.T.);
#50611=EDGE_CURVE('',#38567,#39033,#31971,.T.);
#50612=EDGE_CURVE('',#39024,#38575,#31972,.T.);
#50613=EDGE_CURVE('',#38564,#39032,#31973,.T.);
#50614=EDGE_CURVE('',#39025,#36897,#31974,.T.);
#50615=EDGE_CURVE('',#38563,#39031,#31975,.T.);
#50616=EDGE_CURVE('',#39026,#36896,#31976,.T.);
#50617=EDGE_CURVE('',#38561,#39030,#1215,.T.);
#50618=EDGE_CURVE('',#39009,#36895,#31977,.T.);
#50619=EDGE_CURVE('',#38556,#39029,#31978,.T.);
#50620=EDGE_CURVE('',#39010,#36894,#31979,.T.);
#50621=EDGE_CURVE('',#37318,#39028,#31980,.T.);
#50622=EDGE_CURVE('',#39015,#36893,#31981,.T.);
#50623=EDGE_CURVE('',#37319,#39027,#31982,.T.);
#50624=EDGE_CURVE('',#39016,#36892,#31983,.T.);
#50625=EDGE_CURVE('',#37320,#39008,#31984,.T.);
#50626=EDGE_CURVE('',#39017,#38594,#31985,.T.);
#50627=EDGE_CURVE('',#37321,#39011,#31986,.T.);
#50628=EDGE_CURVE('',#39018,#38590,#1216,.T.);
#50629=EDGE_CURVE('',#37322,#39014,#31987,.T.);
#50630=EDGE_CURVE('',#39019,#38589,#31988,.T.);
#50631=EDGE_CURVE('',#37323,#39013,#31989,.T.);
#50632=EDGE_CURVE('',#39020,#38586,#31990,.T.);
#50633=EDGE_CURVE('',#38577,#39012,#31991,.T.);
#50634=EDGE_CURVE('',#39021,#38585,#31992,.T.);
#50635=EDGE_CURVE('',#38578,#39023,#1217,.T.);
#50636=EDGE_CURVE('',#39022,#38582,#31993,.T.);
#50637=EDGE_CURVE('',#39063,#38553,#1218,.T.);
#50638=EDGE_CURVE('',#38548,#39062,#31994,.T.);
#50639=EDGE_CURVE('',#38547,#39061,#31995,.T.);
#50640=EDGE_CURVE('',#39052,#38555,#31996,.T.);
#50641=EDGE_CURVE('',#38544,#39060,#31997,.T.);
#50642=EDGE_CURVE('',#39053,#36903,#31998,.T.);
#50643=EDGE_CURVE('',#38543,#39059,#31999,.T.);
#50644=EDGE_CURVE('',#39054,#36902,#32000,.T.);
#50645=EDGE_CURVE('',#38541,#39058,#1219,.T.);
#50646=EDGE_CURVE('',#39037,#36901,#32001,.T.);
#50647=EDGE_CURVE('',#38536,#39057,#32002,.T.);
#50648=EDGE_CURVE('',#39038,#36900,#32003,.T.);
#50649=EDGE_CURVE('',#37312,#39056,#32004,.T.);
#50650=EDGE_CURVE('',#39043,#36899,#32005,.T.);
#50651=EDGE_CURVE('',#37313,#39055,#32006,.T.);
#50652=EDGE_CURVE('',#39044,#36898,#32007,.T.);
#50653=EDGE_CURVE('',#37314,#39036,#32008,.T.);
#50654=EDGE_CURVE('',#39045,#38574,#32009,.T.);
#50655=EDGE_CURVE('',#37315,#39039,#32010,.T.);
#50656=EDGE_CURVE('',#39046,#38570,#1220,.T.);
#50657=EDGE_CURVE('',#37316,#39042,#32011,.T.);
#50658=EDGE_CURVE('',#39047,#38569,#32012,.T.);
#50659=EDGE_CURVE('',#37317,#39041,#32013,.T.);
#50660=EDGE_CURVE('',#39048,#38566,#32014,.T.);
#50661=EDGE_CURVE('',#38557,#39040,#32015,.T.);
#50662=EDGE_CURVE('',#39049,#38565,#32016,.T.);
#50663=EDGE_CURVE('',#38558,#39051,#1221,.T.);
#50664=EDGE_CURVE('',#39050,#38562,#32017,.T.);
#50665=EDGE_CURVE('',#39091,#38533,#1222,.T.);
#50666=EDGE_CURVE('',#38528,#39090,#32018,.T.);
#50667=EDGE_CURVE('',#38527,#39089,#32019,.T.);
#50668=EDGE_CURVE('',#39080,#38535,#32020,.T.);
#50669=EDGE_CURVE('',#38524,#39088,#32021,.T.);
#50670=EDGE_CURVE('',#39081,#36909,#32022,.T.);
#50671=EDGE_CURVE('',#38523,#39087,#32023,.T.);
#50672=EDGE_CURVE('',#39082,#36908,#32024,.T.);
#50673=EDGE_CURVE('',#38521,#39086,#1223,.T.);
#50674=EDGE_CURVE('',#39065,#36907,#32025,.T.);
#50675=EDGE_CURVE('',#38516,#39085,#32026,.T.);
#50676=EDGE_CURVE('',#39066,#36906,#32027,.T.);
#50677=EDGE_CURVE('',#37306,#39084,#32028,.T.);
#50678=EDGE_CURVE('',#39071,#36905,#32029,.T.);
#50679=EDGE_CURVE('',#37307,#39083,#32030,.T.);
#50680=EDGE_CURVE('',#39072,#36904,#32031,.T.);
#50681=EDGE_CURVE('',#37308,#39064,#32032,.T.);
#50682=EDGE_CURVE('',#39073,#38554,#32033,.T.);
#50683=EDGE_CURVE('',#37309,#39067,#32034,.T.);
#50684=EDGE_CURVE('',#39074,#38550,#1224,.T.);
#50685=EDGE_CURVE('',#37310,#39070,#32035,.T.);
#50686=EDGE_CURVE('',#39075,#38549,#32036,.T.);
#50687=EDGE_CURVE('',#37311,#39069,#32037,.T.);
#50688=EDGE_CURVE('',#39076,#38546,#32038,.T.);
#50689=EDGE_CURVE('',#38537,#39068,#32039,.T.);
#50690=EDGE_CURVE('',#39077,#38545,#32040,.T.);
#50691=EDGE_CURVE('',#38538,#39079,#1225,.T.);
#50692=EDGE_CURVE('',#39078,#38542,#32041,.T.);
#50693=EDGE_CURVE('',#39119,#38513,#1226,.T.);
#50694=EDGE_CURVE('',#38508,#39118,#32042,.T.);
#50695=EDGE_CURVE('',#38507,#39117,#32043,.T.);
#50696=EDGE_CURVE('',#39108,#38515,#32044,.T.);
#50697=EDGE_CURVE('',#38504,#39116,#32045,.T.);
#50698=EDGE_CURVE('',#39109,#36915,#32046,.T.);
#50699=EDGE_CURVE('',#38503,#39115,#32047,.T.);
#50700=EDGE_CURVE('',#39110,#36914,#32048,.T.);
#50701=EDGE_CURVE('',#38501,#39114,#1227,.T.);
#50702=EDGE_CURVE('',#39093,#36913,#32049,.T.);
#50703=EDGE_CURVE('',#38496,#39113,#32050,.T.);
#50704=EDGE_CURVE('',#39094,#36912,#32051,.T.);
#50705=EDGE_CURVE('',#37300,#39112,#32052,.T.);
#50706=EDGE_CURVE('',#39099,#36911,#32053,.T.);
#50707=EDGE_CURVE('',#37301,#39111,#32054,.T.);
#50708=EDGE_CURVE('',#39100,#36910,#32055,.T.);
#50709=EDGE_CURVE('',#37302,#39092,#32056,.T.);
#50710=EDGE_CURVE('',#39101,#38534,#32057,.T.);
#50711=EDGE_CURVE('',#37303,#39095,#32058,.T.);
#50712=EDGE_CURVE('',#39102,#38530,#1228,.T.);
#50713=EDGE_CURVE('',#37304,#39098,#32059,.T.);
#50714=EDGE_CURVE('',#39103,#38529,#32060,.T.);
#50715=EDGE_CURVE('',#37305,#39097,#32061,.T.);
#50716=EDGE_CURVE('',#39104,#38526,#32062,.T.);
#50717=EDGE_CURVE('',#38517,#39096,#32063,.T.);
#50718=EDGE_CURVE('',#39105,#38525,#32064,.T.);
#50719=EDGE_CURVE('',#38518,#39107,#1229,.T.);
#50720=EDGE_CURVE('',#39106,#38522,#32065,.T.);
#50721=EDGE_CURVE('',#39147,#38493,#1230,.T.);
#50722=EDGE_CURVE('',#38488,#39146,#32066,.T.);
#50723=EDGE_CURVE('',#38487,#39145,#32067,.T.);
#50724=EDGE_CURVE('',#39136,#38495,#32068,.T.);
#50725=EDGE_CURVE('',#38484,#39144,#32069,.T.);
#50726=EDGE_CURVE('',#39137,#36921,#32070,.T.);
#50727=EDGE_CURVE('',#38483,#39143,#32071,.T.);
#50728=EDGE_CURVE('',#39138,#36920,#32072,.T.);
#50729=EDGE_CURVE('',#38481,#39142,#1231,.T.);
#50730=EDGE_CURVE('',#39121,#36919,#32073,.T.);
#50731=EDGE_CURVE('',#38476,#39141,#32074,.T.);
#50732=EDGE_CURVE('',#39122,#36918,#32075,.T.);
#50733=EDGE_CURVE('',#37294,#39140,#32076,.T.);
#50734=EDGE_CURVE('',#39127,#36917,#32077,.T.);
#50735=EDGE_CURVE('',#37295,#39139,#32078,.T.);
#50736=EDGE_CURVE('',#39128,#36916,#32079,.T.);
#50737=EDGE_CURVE('',#37296,#39120,#32080,.T.);
#50738=EDGE_CURVE('',#39129,#38514,#32081,.T.);
#50739=EDGE_CURVE('',#37297,#39123,#32082,.T.);
#50740=EDGE_CURVE('',#39130,#38510,#1232,.T.);
#50741=EDGE_CURVE('',#37298,#39126,#32083,.T.);
#50742=EDGE_CURVE('',#39131,#38509,#32084,.T.);
#50743=EDGE_CURVE('',#37299,#39125,#32085,.T.);
#50744=EDGE_CURVE('',#39132,#38506,#32086,.T.);
#50745=EDGE_CURVE('',#38497,#39124,#32087,.T.);
#50746=EDGE_CURVE('',#39133,#38505,#32088,.T.);
#50747=EDGE_CURVE('',#38498,#39135,#1233,.T.);
#50748=EDGE_CURVE('',#39134,#38502,#32089,.T.);
#50749=EDGE_CURVE('',#39175,#38473,#1234,.T.);
#50750=EDGE_CURVE('',#38468,#39174,#32090,.T.);
#50751=EDGE_CURVE('',#38467,#39173,#32091,.T.);
#50752=EDGE_CURVE('',#39164,#38475,#32092,.T.);
#50753=EDGE_CURVE('',#38464,#39172,#32093,.T.);
#50754=EDGE_CURVE('',#39165,#36927,#32094,.T.);
#50755=EDGE_CURVE('',#38463,#39171,#32095,.T.);
#50756=EDGE_CURVE('',#39166,#36926,#32096,.T.);
#50757=EDGE_CURVE('',#38461,#39170,#1235,.T.);
#50758=EDGE_CURVE('',#39149,#36925,#32097,.T.);
#50759=EDGE_CURVE('',#38456,#39169,#32098,.T.);
#50760=EDGE_CURVE('',#39150,#36924,#32099,.T.);
#50761=EDGE_CURVE('',#37288,#39168,#32100,.T.);
#50762=EDGE_CURVE('',#39155,#36923,#32101,.T.);
#50763=EDGE_CURVE('',#37289,#39167,#32102,.T.);
#50764=EDGE_CURVE('',#39156,#36922,#32103,.T.);
#50765=EDGE_CURVE('',#37290,#39148,#32104,.T.);
#50766=EDGE_CURVE('',#39157,#38494,#32105,.T.);
#50767=EDGE_CURVE('',#37291,#39151,#32106,.T.);
#50768=EDGE_CURVE('',#39158,#38490,#1236,.T.);
#50769=EDGE_CURVE('',#37292,#39154,#32107,.T.);
#50770=EDGE_CURVE('',#39159,#38489,#32108,.T.);
#50771=EDGE_CURVE('',#37293,#39153,#32109,.T.);
#50772=EDGE_CURVE('',#39160,#38486,#32110,.T.);
#50773=EDGE_CURVE('',#38477,#39152,#32111,.T.);
#50774=EDGE_CURVE('',#39161,#38485,#32112,.T.);
#50775=EDGE_CURVE('',#38478,#39163,#1237,.T.);
#50776=EDGE_CURVE('',#39162,#38482,#32113,.T.);
#50777=EDGE_CURVE('',#39203,#38453,#1238,.T.);
#50778=EDGE_CURVE('',#38448,#39202,#32114,.T.);
#50779=EDGE_CURVE('',#38447,#39201,#32115,.T.);
#50780=EDGE_CURVE('',#39192,#38455,#32116,.T.);
#50781=EDGE_CURVE('',#38444,#39200,#32117,.T.);
#50782=EDGE_CURVE('',#39193,#36933,#32118,.T.);
#50783=EDGE_CURVE('',#38443,#39199,#32119,.T.);
#50784=EDGE_CURVE('',#39194,#36932,#32120,.T.);
#50785=EDGE_CURVE('',#38441,#39198,#1239,.T.);
#50786=EDGE_CURVE('',#39177,#36931,#32121,.T.);
#50787=EDGE_CURVE('',#38436,#39197,#32122,.T.);
#50788=EDGE_CURVE('',#39178,#36930,#32123,.T.);
#50789=EDGE_CURVE('',#37282,#39196,#32124,.T.);
#50790=EDGE_CURVE('',#39183,#36929,#32125,.T.);
#50791=EDGE_CURVE('',#37283,#39195,#32126,.T.);
#50792=EDGE_CURVE('',#39184,#36928,#32127,.T.);
#50793=EDGE_CURVE('',#37284,#39176,#32128,.T.);
#50794=EDGE_CURVE('',#39185,#38474,#32129,.T.);
#50795=EDGE_CURVE('',#37285,#39179,#32130,.T.);
#50796=EDGE_CURVE('',#39186,#38470,#1240,.T.);
#50797=EDGE_CURVE('',#37286,#39182,#32131,.T.);
#50798=EDGE_CURVE('',#39187,#38469,#32132,.T.);
#50799=EDGE_CURVE('',#37287,#39181,#32133,.T.);
#50800=EDGE_CURVE('',#39188,#38466,#32134,.T.);
#50801=EDGE_CURVE('',#38457,#39180,#32135,.T.);
#50802=EDGE_CURVE('',#39189,#38465,#32136,.T.);
#50803=EDGE_CURVE('',#38458,#39191,#1241,.T.);
#50804=EDGE_CURVE('',#39190,#38462,#32137,.T.);
#50805=EDGE_CURVE('',#39231,#38433,#1242,.T.);
#50806=EDGE_CURVE('',#38428,#39230,#32138,.T.);
#50807=EDGE_CURVE('',#38427,#39229,#32139,.T.);
#50808=EDGE_CURVE('',#39220,#38435,#32140,.T.);
#50809=EDGE_CURVE('',#38424,#39228,#32141,.T.);
#50810=EDGE_CURVE('',#39221,#36939,#32142,.T.);
#50811=EDGE_CURVE('',#38423,#39227,#32143,.T.);
#50812=EDGE_CURVE('',#39222,#36938,#32144,.T.);
#50813=EDGE_CURVE('',#38421,#39226,#1243,.T.);
#50814=EDGE_CURVE('',#39205,#36937,#32145,.T.);
#50815=EDGE_CURVE('',#38416,#39225,#32146,.T.);
#50816=EDGE_CURVE('',#39206,#36936,#32147,.T.);
#50817=EDGE_CURVE('',#37276,#39224,#32148,.T.);
#50818=EDGE_CURVE('',#39211,#36935,#32149,.T.);
#50819=EDGE_CURVE('',#37277,#39223,#32150,.T.);
#50820=EDGE_CURVE('',#39212,#36934,#32151,.T.);
#50821=EDGE_CURVE('',#37278,#39204,#32152,.T.);
#50822=EDGE_CURVE('',#39213,#38454,#32153,.T.);
#50823=EDGE_CURVE('',#37279,#39207,#32154,.T.);
#50824=EDGE_CURVE('',#39214,#38450,#1244,.T.);
#50825=EDGE_CURVE('',#37280,#39210,#32155,.T.);
#50826=EDGE_CURVE('',#39215,#38449,#32156,.T.);
#50827=EDGE_CURVE('',#37281,#39209,#32157,.T.);
#50828=EDGE_CURVE('',#39216,#38446,#32158,.T.);
#50829=EDGE_CURVE('',#38437,#39208,#32159,.T.);
#50830=EDGE_CURVE('',#39217,#38445,#32160,.T.);
#50831=EDGE_CURVE('',#38438,#39219,#1245,.T.);
#50832=EDGE_CURVE('',#39218,#38442,#32161,.T.);
#50833=EDGE_CURVE('',#39259,#38413,#1246,.T.);
#50834=EDGE_CURVE('',#38408,#39258,#32162,.T.);
#50835=EDGE_CURVE('',#38407,#39257,#32163,.T.);
#50836=EDGE_CURVE('',#39248,#38415,#32164,.T.);
#50837=EDGE_CURVE('',#38404,#39256,#32165,.T.);
#50838=EDGE_CURVE('',#39249,#36945,#32166,.T.);
#50839=EDGE_CURVE('',#38403,#39255,#32167,.T.);
#50840=EDGE_CURVE('',#39250,#36944,#32168,.T.);
#50841=EDGE_CURVE('',#38401,#39254,#1247,.T.);
#50842=EDGE_CURVE('',#39233,#36943,#32169,.T.);
#50843=EDGE_CURVE('',#38396,#39253,#32170,.T.);
#50844=EDGE_CURVE('',#39234,#36942,#32171,.T.);
#50845=EDGE_CURVE('',#37270,#39252,#32172,.T.);
#50846=EDGE_CURVE('',#39239,#36941,#32173,.T.);
#50847=EDGE_CURVE('',#37271,#39251,#32174,.T.);
#50848=EDGE_CURVE('',#39240,#36940,#32175,.T.);
#50849=EDGE_CURVE('',#37272,#39232,#32176,.T.);
#50850=EDGE_CURVE('',#39241,#38434,#32177,.T.);
#50851=EDGE_CURVE('',#37273,#39235,#32178,.T.);
#50852=EDGE_CURVE('',#39242,#38430,#1248,.T.);
#50853=EDGE_CURVE('',#37274,#39238,#32179,.T.);
#50854=EDGE_CURVE('',#39243,#38429,#32180,.T.);
#50855=EDGE_CURVE('',#37275,#39237,#32181,.T.);
#50856=EDGE_CURVE('',#39244,#38426,#32182,.T.);
#50857=EDGE_CURVE('',#38417,#39236,#32183,.T.);
#50858=EDGE_CURVE('',#39245,#38425,#32184,.T.);
#50859=EDGE_CURVE('',#38418,#39247,#1249,.T.);
#50860=EDGE_CURVE('',#39246,#38422,#32185,.T.);
#50861=EDGE_CURVE('',#39287,#38393,#1250,.T.);
#50862=EDGE_CURVE('',#38388,#39286,#32186,.T.);
#50863=EDGE_CURVE('',#38387,#39285,#32187,.T.);
#50864=EDGE_CURVE('',#39276,#38395,#32188,.T.);
#50865=EDGE_CURVE('',#38384,#39284,#32189,.T.);
#50866=EDGE_CURVE('',#39277,#36951,#32190,.T.);
#50867=EDGE_CURVE('',#38383,#39283,#32191,.T.);
#50868=EDGE_CURVE('',#39278,#36950,#32192,.T.);
#50869=EDGE_CURVE('',#38381,#39282,#1251,.T.);
#50870=EDGE_CURVE('',#39261,#36949,#32193,.T.);
#50871=EDGE_CURVE('',#38376,#39281,#32194,.T.);
#50872=EDGE_CURVE('',#39262,#36948,#32195,.T.);
#50873=EDGE_CURVE('',#37264,#39280,#32196,.T.);
#50874=EDGE_CURVE('',#39267,#36947,#32197,.T.);
#50875=EDGE_CURVE('',#37265,#39279,#32198,.T.);
#50876=EDGE_CURVE('',#39268,#36946,#32199,.T.);
#50877=EDGE_CURVE('',#37266,#39260,#32200,.T.);
#50878=EDGE_CURVE('',#39269,#38414,#32201,.T.);
#50879=EDGE_CURVE('',#37267,#39263,#32202,.T.);
#50880=EDGE_CURVE('',#39270,#38410,#1252,.T.);
#50881=EDGE_CURVE('',#37268,#39266,#32203,.T.);
#50882=EDGE_CURVE('',#39271,#38409,#32204,.T.);
#50883=EDGE_CURVE('',#37269,#39265,#32205,.T.);
#50884=EDGE_CURVE('',#39272,#38406,#32206,.T.);
#50885=EDGE_CURVE('',#38397,#39264,#32207,.T.);
#50886=EDGE_CURVE('',#39273,#38405,#32208,.T.);
#50887=EDGE_CURVE('',#38398,#39275,#1253,.T.);
#50888=EDGE_CURVE('',#39274,#38402,#32209,.T.);
#50889=EDGE_CURVE('',#39315,#38373,#1254,.T.);
#50890=EDGE_CURVE('',#38368,#39314,#32210,.T.);
#50891=EDGE_CURVE('',#38367,#39313,#32211,.T.);
#50892=EDGE_CURVE('',#39304,#38375,#32212,.T.);
#50893=EDGE_CURVE('',#38364,#39312,#32213,.T.);
#50894=EDGE_CURVE('',#39305,#36957,#32214,.T.);
#50895=EDGE_CURVE('',#38363,#39311,#32215,.T.);
#50896=EDGE_CURVE('',#39306,#36956,#32216,.T.);
#50897=EDGE_CURVE('',#38361,#39310,#1255,.T.);
#50898=EDGE_CURVE('',#39289,#36955,#32217,.T.);
#50899=EDGE_CURVE('',#38356,#39309,#32218,.T.);
#50900=EDGE_CURVE('',#39290,#36954,#32219,.T.);
#50901=EDGE_CURVE('',#37258,#39308,#32220,.T.);
#50902=EDGE_CURVE('',#39295,#36953,#32221,.T.);
#50903=EDGE_CURVE('',#37259,#39307,#32222,.T.);
#50904=EDGE_CURVE('',#39296,#36952,#32223,.T.);
#50905=EDGE_CURVE('',#37260,#39288,#32224,.T.);
#50906=EDGE_CURVE('',#39297,#38394,#32225,.T.);
#50907=EDGE_CURVE('',#37261,#39291,#32226,.T.);
#50908=EDGE_CURVE('',#39298,#38390,#1256,.T.);
#50909=EDGE_CURVE('',#37262,#39294,#32227,.T.);
#50910=EDGE_CURVE('',#39299,#38389,#32228,.T.);
#50911=EDGE_CURVE('',#37263,#39293,#32229,.T.);
#50912=EDGE_CURVE('',#39300,#38386,#32230,.T.);
#50913=EDGE_CURVE('',#38377,#39292,#32231,.T.);
#50914=EDGE_CURVE('',#39301,#38385,#32232,.T.);
#50915=EDGE_CURVE('',#38378,#39303,#1257,.T.);
#50916=EDGE_CURVE('',#39302,#38382,#32233,.T.);
#50917=EDGE_CURVE('',#39343,#38353,#1258,.T.);
#50918=EDGE_CURVE('',#38348,#39342,#32234,.T.);
#50919=EDGE_CURVE('',#38347,#39341,#32235,.T.);
#50920=EDGE_CURVE('',#39332,#38355,#32236,.T.);
#50921=EDGE_CURVE('',#38344,#39340,#32237,.T.);
#50922=EDGE_CURVE('',#39333,#36963,#32238,.T.);
#50923=EDGE_CURVE('',#38343,#39339,#32239,.T.);
#50924=EDGE_CURVE('',#39334,#36962,#32240,.T.);
#50925=EDGE_CURVE('',#38341,#39338,#1259,.T.);
#50926=EDGE_CURVE('',#39317,#36961,#32241,.T.);
#50927=EDGE_CURVE('',#38336,#39337,#32242,.T.);
#50928=EDGE_CURVE('',#39318,#36960,#32243,.T.);
#50929=EDGE_CURVE('',#37252,#39336,#32244,.T.);
#50930=EDGE_CURVE('',#39323,#36959,#32245,.T.);
#50931=EDGE_CURVE('',#37253,#39335,#32246,.T.);
#50932=EDGE_CURVE('',#39324,#36958,#32247,.T.);
#50933=EDGE_CURVE('',#37254,#39316,#32248,.T.);
#50934=EDGE_CURVE('',#39325,#38374,#32249,.T.);
#50935=EDGE_CURVE('',#37255,#39319,#32250,.T.);
#50936=EDGE_CURVE('',#39326,#38370,#1260,.T.);
#50937=EDGE_CURVE('',#37256,#39322,#32251,.T.);
#50938=EDGE_CURVE('',#39327,#38369,#32252,.T.);
#50939=EDGE_CURVE('',#37257,#39321,#32253,.T.);
#50940=EDGE_CURVE('',#39328,#38366,#32254,.T.);
#50941=EDGE_CURVE('',#38357,#39320,#32255,.T.);
#50942=EDGE_CURVE('',#39329,#38365,#32256,.T.);
#50943=EDGE_CURVE('',#38358,#39331,#1261,.T.);
#50944=EDGE_CURVE('',#39330,#38362,#32257,.T.);
#50945=EDGE_CURVE('',#39371,#38333,#1262,.T.);
#50946=EDGE_CURVE('',#38328,#39370,#32258,.T.);
#50947=EDGE_CURVE('',#38327,#39369,#32259,.T.);
#50948=EDGE_CURVE('',#39360,#38335,#32260,.T.);
#50949=EDGE_CURVE('',#38324,#39368,#32261,.T.);
#50950=EDGE_CURVE('',#39361,#36969,#32262,.T.);
#50951=EDGE_CURVE('',#38323,#39367,#32263,.T.);
#50952=EDGE_CURVE('',#39362,#36968,#32264,.T.);
#50953=EDGE_CURVE('',#38321,#39366,#1263,.T.);
#50954=EDGE_CURVE('',#39345,#36967,#32265,.T.);
#50955=EDGE_CURVE('',#38316,#39365,#32266,.T.);
#50956=EDGE_CURVE('',#39346,#36966,#32267,.T.);
#50957=EDGE_CURVE('',#37246,#39364,#32268,.T.);
#50958=EDGE_CURVE('',#39351,#36965,#32269,.T.);
#50959=EDGE_CURVE('',#37247,#39363,#32270,.T.);
#50960=EDGE_CURVE('',#39352,#36964,#32271,.T.);
#50961=EDGE_CURVE('',#37248,#39344,#32272,.T.);
#50962=EDGE_CURVE('',#39353,#38354,#32273,.T.);
#50963=EDGE_CURVE('',#37249,#39347,#32274,.T.);
#50964=EDGE_CURVE('',#39354,#38350,#1264,.T.);
#50965=EDGE_CURVE('',#37250,#39350,#32275,.T.);
#50966=EDGE_CURVE('',#39355,#38349,#32276,.T.);
#50967=EDGE_CURVE('',#37251,#39349,#32277,.T.);
#50968=EDGE_CURVE('',#39356,#38346,#32278,.T.);
#50969=EDGE_CURVE('',#38337,#39348,#32279,.T.);
#50970=EDGE_CURVE('',#39357,#38345,#32280,.T.);
#50971=EDGE_CURVE('',#38338,#39359,#1265,.T.);
#50972=EDGE_CURVE('',#39358,#38342,#32281,.T.);
#50973=EDGE_CURVE('',#39399,#38313,#1266,.T.);
#50974=EDGE_CURVE('',#38308,#39398,#32282,.T.);
#50975=EDGE_CURVE('',#38307,#39397,#32283,.T.);
#50976=EDGE_CURVE('',#39388,#38315,#32284,.T.);
#50977=EDGE_CURVE('',#38304,#39396,#32285,.T.);
#50978=EDGE_CURVE('',#39389,#36975,#32286,.T.);
#50979=EDGE_CURVE('',#38303,#39395,#32287,.T.);
#50980=EDGE_CURVE('',#39390,#36974,#32288,.T.);
#50981=EDGE_CURVE('',#38301,#39394,#1267,.T.);
#50982=EDGE_CURVE('',#39373,#36973,#32289,.T.);
#50983=EDGE_CURVE('',#38296,#39393,#32290,.T.);
#50984=EDGE_CURVE('',#39374,#36972,#32291,.T.);
#50985=EDGE_CURVE('',#37240,#39392,#32292,.T.);
#50986=EDGE_CURVE('',#39379,#36971,#32293,.T.);
#50987=EDGE_CURVE('',#37241,#39391,#32294,.T.);
#50988=EDGE_CURVE('',#39380,#36970,#32295,.T.);
#50989=EDGE_CURVE('',#37242,#39372,#32296,.T.);
#50990=EDGE_CURVE('',#39381,#38334,#32297,.T.);
#50991=EDGE_CURVE('',#37243,#39375,#32298,.T.);
#50992=EDGE_CURVE('',#39382,#38330,#1268,.T.);
#50993=EDGE_CURVE('',#37244,#39378,#32299,.T.);
#50994=EDGE_CURVE('',#39383,#38329,#32300,.T.);
#50995=EDGE_CURVE('',#37245,#39377,#32301,.T.);
#50996=EDGE_CURVE('',#39384,#38326,#32302,.T.);
#50997=EDGE_CURVE('',#38317,#39376,#32303,.T.);
#50998=EDGE_CURVE('',#39385,#38325,#32304,.T.);
#50999=EDGE_CURVE('',#38318,#39387,#1269,.T.);
#51000=EDGE_CURVE('',#39386,#38322,#32305,.T.);
#51001=EDGE_CURVE('',#39427,#38293,#1270,.T.);
#51002=EDGE_CURVE('',#38288,#39426,#32306,.T.);
#51003=EDGE_CURVE('',#38287,#39425,#32307,.T.);
#51004=EDGE_CURVE('',#39416,#38295,#32308,.T.);
#51005=EDGE_CURVE('',#38284,#39424,#32309,.T.);
#51006=EDGE_CURVE('',#39417,#36981,#32310,.T.);
#51007=EDGE_CURVE('',#38283,#39423,#32311,.T.);
#51008=EDGE_CURVE('',#39418,#36980,#32312,.T.);
#51009=EDGE_CURVE('',#38281,#39422,#1271,.T.);
#51010=EDGE_CURVE('',#39401,#36979,#32313,.T.);
#51011=EDGE_CURVE('',#38276,#39421,#32314,.T.);
#51012=EDGE_CURVE('',#39402,#36978,#32315,.T.);
#51013=EDGE_CURVE('',#37234,#39420,#32316,.T.);
#51014=EDGE_CURVE('',#39407,#36977,#32317,.T.);
#51015=EDGE_CURVE('',#37235,#39419,#32318,.T.);
#51016=EDGE_CURVE('',#39408,#36976,#32319,.T.);
#51017=EDGE_CURVE('',#37236,#39400,#32320,.T.);
#51018=EDGE_CURVE('',#39409,#38314,#32321,.T.);
#51019=EDGE_CURVE('',#37237,#39403,#32322,.T.);
#51020=EDGE_CURVE('',#39410,#38310,#1272,.T.);
#51021=EDGE_CURVE('',#37238,#39406,#32323,.T.);
#51022=EDGE_CURVE('',#39411,#38309,#32324,.T.);
#51023=EDGE_CURVE('',#37239,#39405,#32325,.T.);
#51024=EDGE_CURVE('',#39412,#38306,#32326,.T.);
#51025=EDGE_CURVE('',#38297,#39404,#32327,.T.);
#51026=EDGE_CURVE('',#39413,#38305,#32328,.T.);
#51027=EDGE_CURVE('',#38298,#39415,#1273,.T.);
#51028=EDGE_CURVE('',#39414,#38302,#32329,.T.);
#51029=EDGE_CURVE('',#39455,#38273,#1274,.T.);
#51030=EDGE_CURVE('',#38268,#39454,#32330,.T.);
#51031=EDGE_CURVE('',#38267,#39453,#32331,.T.);
#51032=EDGE_CURVE('',#39444,#38275,#32332,.T.);
#51033=EDGE_CURVE('',#38264,#39452,#32333,.T.);
#51034=EDGE_CURVE('',#39445,#36987,#32334,.T.);
#51035=EDGE_CURVE('',#38263,#39451,#32335,.T.);
#51036=EDGE_CURVE('',#39446,#36986,#32336,.T.);
#51037=EDGE_CURVE('',#38261,#39450,#1275,.T.);
#51038=EDGE_CURVE('',#39429,#36985,#32337,.T.);
#51039=EDGE_CURVE('',#38256,#39449,#32338,.T.);
#51040=EDGE_CURVE('',#39430,#36984,#32339,.T.);
#51041=EDGE_CURVE('',#37228,#39448,#32340,.T.);
#51042=EDGE_CURVE('',#39435,#36983,#32341,.T.);
#51043=EDGE_CURVE('',#37229,#39447,#32342,.T.);
#51044=EDGE_CURVE('',#39436,#36982,#32343,.T.);
#51045=EDGE_CURVE('',#37230,#39428,#32344,.T.);
#51046=EDGE_CURVE('',#39437,#38294,#32345,.T.);
#51047=EDGE_CURVE('',#37231,#39431,#32346,.T.);
#51048=EDGE_CURVE('',#39438,#38290,#1276,.T.);
#51049=EDGE_CURVE('',#37232,#39434,#32347,.T.);
#51050=EDGE_CURVE('',#39439,#38289,#32348,.T.);
#51051=EDGE_CURVE('',#37233,#39433,#32349,.T.);
#51052=EDGE_CURVE('',#39440,#38286,#32350,.T.);
#51053=EDGE_CURVE('',#38277,#39432,#32351,.T.);
#51054=EDGE_CURVE('',#39441,#38285,#32352,.T.);
#51055=EDGE_CURVE('',#38278,#39443,#1277,.T.);
#51056=EDGE_CURVE('',#39442,#38282,#32353,.T.);
#51057=EDGE_CURVE('',#39483,#38253,#1278,.T.);
#51058=EDGE_CURVE('',#38248,#39482,#32354,.T.);
#51059=EDGE_CURVE('',#38247,#39481,#32355,.T.);
#51060=EDGE_CURVE('',#39472,#38255,#32356,.T.);
#51061=EDGE_CURVE('',#38244,#39480,#32357,.T.);
#51062=EDGE_CURVE('',#39473,#36993,#32358,.T.);
#51063=EDGE_CURVE('',#38243,#39479,#32359,.T.);
#51064=EDGE_CURVE('',#39474,#36992,#32360,.T.);
#51065=EDGE_CURVE('',#38241,#39478,#1279,.T.);
#51066=EDGE_CURVE('',#39457,#36991,#32361,.T.);
#51067=EDGE_CURVE('',#38236,#39477,#32362,.T.);
#51068=EDGE_CURVE('',#39458,#36990,#32363,.T.);
#51069=EDGE_CURVE('',#37222,#39476,#32364,.T.);
#51070=EDGE_CURVE('',#39463,#36989,#32365,.T.);
#51071=EDGE_CURVE('',#37223,#39475,#32366,.T.);
#51072=EDGE_CURVE('',#39464,#36988,#32367,.T.);
#51073=EDGE_CURVE('',#37224,#39456,#32368,.T.);
#51074=EDGE_CURVE('',#39465,#38274,#32369,.T.);
#51075=EDGE_CURVE('',#37225,#39459,#32370,.T.);
#51076=EDGE_CURVE('',#39466,#38270,#1280,.T.);
#51077=EDGE_CURVE('',#37226,#39462,#32371,.T.);
#51078=EDGE_CURVE('',#39467,#38269,#32372,.T.);
#51079=EDGE_CURVE('',#37227,#39461,#32373,.T.);
#51080=EDGE_CURVE('',#39468,#38266,#32374,.T.);
#51081=EDGE_CURVE('',#38257,#39460,#32375,.T.);
#51082=EDGE_CURVE('',#39469,#38265,#32376,.T.);
#51083=EDGE_CURVE('',#38258,#39471,#1281,.T.);
#51084=EDGE_CURVE('',#39470,#38262,#32377,.T.);
#51085=EDGE_CURVE('',#39511,#38233,#1282,.T.);
#51086=EDGE_CURVE('',#38228,#39510,#32378,.T.);
#51087=EDGE_CURVE('',#38227,#39509,#32379,.T.);
#51088=EDGE_CURVE('',#39500,#38235,#32380,.T.);
#51089=EDGE_CURVE('',#38224,#39508,#32381,.T.);
#51090=EDGE_CURVE('',#39501,#36999,#32382,.T.);
#51091=EDGE_CURVE('',#38223,#39507,#32383,.T.);
#51092=EDGE_CURVE('',#39502,#36998,#32384,.T.);
#51093=EDGE_CURVE('',#38221,#39506,#1283,.T.);
#51094=EDGE_CURVE('',#39485,#36997,#32385,.T.);
#51095=EDGE_CURVE('',#38216,#39505,#32386,.T.);
#51096=EDGE_CURVE('',#39486,#36996,#32387,.T.);
#51097=EDGE_CURVE('',#37216,#39504,#32388,.T.);
#51098=EDGE_CURVE('',#39491,#36995,#32389,.T.);
#51099=EDGE_CURVE('',#37217,#39503,#32390,.T.);
#51100=EDGE_CURVE('',#39492,#36994,#32391,.T.);
#51101=EDGE_CURVE('',#37218,#39484,#32392,.T.);
#51102=EDGE_CURVE('',#39493,#38254,#32393,.T.);
#51103=EDGE_CURVE('',#37219,#39487,#32394,.T.);
#51104=EDGE_CURVE('',#39494,#38250,#1284,.T.);
#51105=EDGE_CURVE('',#37220,#39490,#32395,.T.);
#51106=EDGE_CURVE('',#39495,#38249,#32396,.T.);
#51107=EDGE_CURVE('',#37221,#39489,#32397,.T.);
#51108=EDGE_CURVE('',#39496,#38246,#32398,.T.);
#51109=EDGE_CURVE('',#38237,#39488,#32399,.T.);
#51110=EDGE_CURVE('',#39497,#38245,#32400,.T.);
#51111=EDGE_CURVE('',#38238,#39499,#1285,.T.);
#51112=EDGE_CURVE('',#39498,#38242,#32401,.T.);
#51113=EDGE_CURVE('',#39539,#38213,#1286,.T.);
#51114=EDGE_CURVE('',#38208,#39538,#32402,.T.);
#51115=EDGE_CURVE('',#38207,#39537,#32403,.T.);
#51116=EDGE_CURVE('',#39528,#38215,#32404,.T.);
#51117=EDGE_CURVE('',#38204,#39536,#32405,.T.);
#51118=EDGE_CURVE('',#39529,#37005,#32406,.T.);
#51119=EDGE_CURVE('',#38203,#39535,#32407,.T.);
#51120=EDGE_CURVE('',#39530,#37004,#32408,.T.);
#51121=EDGE_CURVE('',#38201,#39534,#1287,.T.);
#51122=EDGE_CURVE('',#39513,#37003,#32409,.T.);
#51123=EDGE_CURVE('',#38196,#39533,#32410,.T.);
#51124=EDGE_CURVE('',#39514,#37002,#32411,.T.);
#51125=EDGE_CURVE('',#37210,#39532,#32412,.T.);
#51126=EDGE_CURVE('',#39519,#37001,#32413,.T.);
#51127=EDGE_CURVE('',#37211,#39531,#32414,.T.);
#51128=EDGE_CURVE('',#39520,#37000,#32415,.T.);
#51129=EDGE_CURVE('',#37212,#39512,#32416,.T.);
#51130=EDGE_CURVE('',#39521,#38234,#32417,.T.);
#51131=EDGE_CURVE('',#37213,#39515,#32418,.T.);
#51132=EDGE_CURVE('',#39522,#38230,#1288,.T.);
#51133=EDGE_CURVE('',#37214,#39518,#32419,.T.);
#51134=EDGE_CURVE('',#39523,#38229,#32420,.T.);
#51135=EDGE_CURVE('',#37215,#39517,#32421,.T.);
#51136=EDGE_CURVE('',#39524,#38226,#32422,.T.);
#51137=EDGE_CURVE('',#38217,#39516,#32423,.T.);
#51138=EDGE_CURVE('',#39525,#38225,#32424,.T.);
#51139=EDGE_CURVE('',#38218,#39527,#1289,.T.);
#51140=EDGE_CURVE('',#39526,#38222,#32425,.T.);
#51141=EDGE_CURVE('',#39567,#38193,#1290,.T.);
#51142=EDGE_CURVE('',#38188,#39566,#32426,.T.);
#51143=EDGE_CURVE('',#38187,#39565,#32427,.T.);
#51144=EDGE_CURVE('',#39556,#38195,#32428,.T.);
#51145=EDGE_CURVE('',#38184,#39564,#32429,.T.);
#51146=EDGE_CURVE('',#39557,#37011,#32430,.T.);
#51147=EDGE_CURVE('',#38183,#39563,#32431,.T.);
#51148=EDGE_CURVE('',#39558,#37010,#32432,.T.);
#51149=EDGE_CURVE('',#38181,#39562,#1291,.T.);
#51150=EDGE_CURVE('',#39541,#37009,#32433,.T.);
#51151=EDGE_CURVE('',#38176,#39561,#32434,.T.);
#51152=EDGE_CURVE('',#39542,#37008,#32435,.T.);
#51153=EDGE_CURVE('',#37204,#39560,#32436,.T.);
#51154=EDGE_CURVE('',#39547,#37007,#32437,.T.);
#51155=EDGE_CURVE('',#37205,#39559,#32438,.T.);
#51156=EDGE_CURVE('',#39548,#37006,#32439,.T.);
#51157=EDGE_CURVE('',#37206,#39540,#32440,.T.);
#51158=EDGE_CURVE('',#39549,#38214,#32441,.T.);
#51159=EDGE_CURVE('',#37207,#39543,#32442,.T.);
#51160=EDGE_CURVE('',#39550,#38210,#1292,.T.);
#51161=EDGE_CURVE('',#37208,#39546,#32443,.T.);
#51162=EDGE_CURVE('',#39551,#38209,#32444,.T.);
#51163=EDGE_CURVE('',#37209,#39545,#32445,.T.);
#51164=EDGE_CURVE('',#39552,#38206,#32446,.T.);
#51165=EDGE_CURVE('',#38197,#39544,#32447,.T.);
#51166=EDGE_CURVE('',#39553,#38205,#32448,.T.);
#51167=EDGE_CURVE('',#38198,#39555,#1293,.T.);
#51168=EDGE_CURVE('',#39554,#38202,#32449,.T.);
#51169=EDGE_CURVE('',#39595,#38173,#1294,.T.);
#51170=EDGE_CURVE('',#38168,#39594,#32450,.T.);
#51171=EDGE_CURVE('',#38167,#39593,#32451,.T.);
#51172=EDGE_CURVE('',#39584,#38175,#32452,.T.);
#51173=EDGE_CURVE('',#38164,#39592,#32453,.T.);
#51174=EDGE_CURVE('',#39585,#37017,#32454,.T.);
#51175=EDGE_CURVE('',#38163,#39591,#32455,.T.);
#51176=EDGE_CURVE('',#39586,#37016,#32456,.T.);
#51177=EDGE_CURVE('',#38161,#39590,#1295,.T.);
#51178=EDGE_CURVE('',#39569,#37015,#32457,.T.);
#51179=EDGE_CURVE('',#38156,#39589,#32458,.T.);
#51180=EDGE_CURVE('',#39570,#37014,#32459,.T.);
#51181=EDGE_CURVE('',#37198,#39588,#32460,.T.);
#51182=EDGE_CURVE('',#39575,#37013,#32461,.T.);
#51183=EDGE_CURVE('',#37199,#39587,#32462,.T.);
#51184=EDGE_CURVE('',#39576,#37012,#32463,.T.);
#51185=EDGE_CURVE('',#37200,#39568,#32464,.T.);
#51186=EDGE_CURVE('',#39577,#38194,#32465,.T.);
#51187=EDGE_CURVE('',#37201,#39571,#32466,.T.);
#51188=EDGE_CURVE('',#39578,#38190,#1296,.T.);
#51189=EDGE_CURVE('',#37202,#39574,#32467,.T.);
#51190=EDGE_CURVE('',#39579,#38189,#32468,.T.);
#51191=EDGE_CURVE('',#37203,#39573,#32469,.T.);
#51192=EDGE_CURVE('',#39580,#38186,#32470,.T.);
#51193=EDGE_CURVE('',#38177,#39572,#32471,.T.);
#51194=EDGE_CURVE('',#39581,#38185,#32472,.T.);
#51195=EDGE_CURVE('',#38178,#39583,#1297,.T.);
#51196=EDGE_CURVE('',#39582,#38182,#32473,.T.);
#51197=EDGE_CURVE('',#39619,#38153,#1298,.T.);
#51198=EDGE_CURVE('',#38148,#39618,#32474,.T.);
#51199=EDGE_CURVE('',#38147,#39617,#32475,.T.);
#51200=EDGE_CURVE('',#39608,#38155,#32476,.T.);
#51201=EDGE_CURVE('',#38144,#39616,#32477,.T.);
#51202=EDGE_CURVE('',#39609,#37021,#32478,.T.);
#51203=EDGE_CURVE('',#38143,#39615,#32479,.T.);
#51204=EDGE_CURVE('',#39610,#37020,#32480,.T.);
#51205=EDGE_CURVE('',#38141,#39614,#1299,.T.);
#51206=EDGE_CURVE('',#38136,#39613,#32481,.T.);
#51207=EDGE_CURVE('',#37551,#39612,#32482,.T.);
#51208=EDGE_CURVE('',#39599,#37019,#32483,.T.);
#51209=EDGE_CURVE('',#37552,#39611,#32484,.T.);
#51210=EDGE_CURVE('',#39600,#37018,#32485,.T.);
#51211=EDGE_CURVE('',#39601,#38174,#32486,.T.);
#51212=EDGE_CURVE('',#39602,#38170,#1300,.T.);
#51213=EDGE_CURVE('',#37196,#39598,#32487,.T.);
#51214=EDGE_CURVE('',#39603,#38169,#32488,.T.);
#51215=EDGE_CURVE('',#37197,#39597,#32489,.T.);
#51216=EDGE_CURVE('',#39604,#38166,#32490,.T.);
#51217=EDGE_CURVE('',#38157,#39596,#32491,.T.);
#51218=EDGE_CURVE('',#39605,#38165,#32492,.T.);
#51219=EDGE_CURVE('',#38158,#39607,#1301,.T.);
#51220=EDGE_CURVE('',#39606,#38162,#32493,.T.);
#51221=EDGE_CURVE('',#39647,#38133,#1302,.T.);
#51222=EDGE_CURVE('',#38128,#39646,#32494,.T.);
#51223=EDGE_CURVE('',#38127,#39645,#32495,.T.);
#51224=EDGE_CURVE('',#39636,#38135,#32496,.T.);
#51225=EDGE_CURVE('',#38124,#39644,#32497,.T.);
#51226=EDGE_CURVE('',#39637,#37027,#32498,.T.);
#51227=EDGE_CURVE('',#38123,#39643,#32499,.T.);
#51228=EDGE_CURVE('',#39638,#37026,#32500,.T.);
#51229=EDGE_CURVE('',#38121,#39642,#1303,.T.);
#51230=EDGE_CURVE('',#39621,#37025,#32501,.T.);
#51231=EDGE_CURVE('',#38116,#39641,#32502,.T.);
#51232=EDGE_CURVE('',#39622,#37024,#32503,.T.);
#51233=EDGE_CURVE('',#37545,#39640,#32504,.T.);
#51234=EDGE_CURVE('',#39627,#37023,#32505,.T.);
#51235=EDGE_CURVE('',#37546,#39639,#32506,.T.);
#51236=EDGE_CURVE('',#39628,#37022,#32507,.T.);
#51237=EDGE_CURVE('',#37547,#39620,#32508,.T.);
#51238=EDGE_CURVE('',#39629,#38154,#32509,.T.);
#51239=EDGE_CURVE('',#37548,#39623,#32510,.T.);
#51240=EDGE_CURVE('',#39630,#38150,#1304,.T.);
#51241=EDGE_CURVE('',#37549,#39626,#32511,.T.);
#51242=EDGE_CURVE('',#39631,#38149,#32512,.T.);
#51243=EDGE_CURVE('',#37550,#39625,#32513,.T.);
#51244=EDGE_CURVE('',#39632,#38146,#32514,.T.);
#51245=EDGE_CURVE('',#38137,#39624,#32515,.T.);
#51246=EDGE_CURVE('',#39633,#38145,#32516,.T.);
#51247=EDGE_CURVE('',#38138,#39635,#1305,.T.);
#51248=EDGE_CURVE('',#39634,#38142,#32517,.T.);
#51249=EDGE_CURVE('',#39675,#38113,#1306,.T.);
#51250=EDGE_CURVE('',#38108,#39674,#32518,.T.);
#51251=EDGE_CURVE('',#38107,#39673,#32519,.T.);
#51252=EDGE_CURVE('',#39664,#38115,#32520,.T.);
#51253=EDGE_CURVE('',#38104,#39672,#32521,.T.);
#51254=EDGE_CURVE('',#39665,#37033,#32522,.T.);
#51255=EDGE_CURVE('',#38103,#39671,#32523,.T.);
#51256=EDGE_CURVE('',#39666,#37032,#32524,.T.);
#51257=EDGE_CURVE('',#38101,#39670,#1307,.T.);
#51258=EDGE_CURVE('',#39649,#37031,#32525,.T.);
#51259=EDGE_CURVE('',#38096,#39669,#32526,.T.);
#51260=EDGE_CURVE('',#39650,#37030,#32527,.T.);
#51261=EDGE_CURVE('',#37539,#39668,#32528,.T.);
#51262=EDGE_CURVE('',#39655,#37029,#32529,.T.);
#51263=EDGE_CURVE('',#37540,#39667,#32530,.T.);
#51264=EDGE_CURVE('',#39656,#37028,#32531,.T.);
#51265=EDGE_CURVE('',#37541,#39648,#32532,.T.);
#51266=EDGE_CURVE('',#39657,#38134,#32533,.T.);
#51267=EDGE_CURVE('',#37542,#39651,#32534,.T.);
#51268=EDGE_CURVE('',#39658,#38130,#1308,.T.);
#51269=EDGE_CURVE('',#37543,#39654,#32535,.T.);
#51270=EDGE_CURVE('',#39659,#38129,#32536,.T.);
#51271=EDGE_CURVE('',#37544,#39653,#32537,.T.);
#51272=EDGE_CURVE('',#39660,#38126,#32538,.T.);
#51273=EDGE_CURVE('',#38117,#39652,#32539,.T.);
#51274=EDGE_CURVE('',#39661,#38125,#32540,.T.);
#51275=EDGE_CURVE('',#38118,#39663,#1309,.T.);
#51276=EDGE_CURVE('',#39662,#38122,#32541,.T.);
#51277=EDGE_CURVE('',#39703,#38093,#1310,.T.);
#51278=EDGE_CURVE('',#38088,#39702,#32542,.T.);
#51279=EDGE_CURVE('',#38087,#39701,#32543,.T.);
#51280=EDGE_CURVE('',#39692,#38095,#32544,.T.);
#51281=EDGE_CURVE('',#38084,#39700,#32545,.T.);
#51282=EDGE_CURVE('',#39693,#37039,#32546,.T.);
#51283=EDGE_CURVE('',#38083,#39699,#32547,.T.);
#51284=EDGE_CURVE('',#39694,#37038,#32548,.T.);
#51285=EDGE_CURVE('',#38081,#39698,#1311,.T.);
#51286=EDGE_CURVE('',#39677,#37037,#32549,.T.);
#51287=EDGE_CURVE('',#38076,#39697,#32550,.T.);
#51288=EDGE_CURVE('',#39678,#37036,#32551,.T.);
#51289=EDGE_CURVE('',#37533,#39696,#32552,.T.);
#51290=EDGE_CURVE('',#39683,#37035,#32553,.T.);
#51291=EDGE_CURVE('',#37534,#39695,#32554,.T.);
#51292=EDGE_CURVE('',#39684,#37034,#32555,.T.);
#51293=EDGE_CURVE('',#37535,#39676,#32556,.T.);
#51294=EDGE_CURVE('',#39685,#38114,#32557,.T.);
#51295=EDGE_CURVE('',#37536,#39679,#32558,.T.);
#51296=EDGE_CURVE('',#39686,#38110,#1312,.T.);
#51297=EDGE_CURVE('',#37537,#39682,#32559,.T.);
#51298=EDGE_CURVE('',#39687,#38109,#32560,.T.);
#51299=EDGE_CURVE('',#37538,#39681,#32561,.T.);
#51300=EDGE_CURVE('',#39688,#38106,#32562,.T.);
#51301=EDGE_CURVE('',#38097,#39680,#32563,.T.);
#51302=EDGE_CURVE('',#39689,#38105,#32564,.T.);
#51303=EDGE_CURVE('',#38098,#39691,#1313,.T.);
#51304=EDGE_CURVE('',#39690,#38102,#32565,.T.);
#51305=EDGE_CURVE('',#39731,#38073,#1314,.T.);
#51306=EDGE_CURVE('',#38068,#39730,#32566,.T.);
#51307=EDGE_CURVE('',#38067,#39729,#32567,.T.);
#51308=EDGE_CURVE('',#39720,#38075,#32568,.T.);
#51309=EDGE_CURVE('',#38064,#39728,#32569,.T.);
#51310=EDGE_CURVE('',#39721,#37045,#32570,.T.);
#51311=EDGE_CURVE('',#38063,#39727,#32571,.T.);
#51312=EDGE_CURVE('',#39722,#37044,#32572,.T.);
#51313=EDGE_CURVE('',#38061,#39726,#1315,.T.);
#51314=EDGE_CURVE('',#39705,#37043,#32573,.T.);
#51315=EDGE_CURVE('',#38056,#39725,#32574,.T.);
#51316=EDGE_CURVE('',#39706,#37042,#32575,.T.);
#51317=EDGE_CURVE('',#37527,#39724,#32576,.T.);
#51318=EDGE_CURVE('',#39711,#37041,#32577,.T.);
#51319=EDGE_CURVE('',#37528,#39723,#32578,.T.);
#51320=EDGE_CURVE('',#39712,#37040,#32579,.T.);
#51321=EDGE_CURVE('',#37529,#39704,#32580,.T.);
#51322=EDGE_CURVE('',#39713,#38094,#32581,.T.);
#51323=EDGE_CURVE('',#37530,#39707,#32582,.T.);
#51324=EDGE_CURVE('',#39714,#38090,#1316,.T.);
#51325=EDGE_CURVE('',#37531,#39710,#32583,.T.);
#51326=EDGE_CURVE('',#39715,#38089,#32584,.T.);
#51327=EDGE_CURVE('',#37532,#39709,#32585,.T.);
#51328=EDGE_CURVE('',#39716,#38086,#32586,.T.);
#51329=EDGE_CURVE('',#38077,#39708,#32587,.T.);
#51330=EDGE_CURVE('',#39717,#38085,#32588,.T.);
#51331=EDGE_CURVE('',#38078,#39719,#1317,.T.);
#51332=EDGE_CURVE('',#39718,#38082,#32589,.T.);
#51333=EDGE_CURVE('',#39759,#38053,#1318,.T.);
#51334=EDGE_CURVE('',#38048,#39758,#32590,.T.);
#51335=EDGE_CURVE('',#38047,#39757,#32591,.T.);
#51336=EDGE_CURVE('',#39748,#38055,#32592,.T.);
#51337=EDGE_CURVE('',#38044,#39756,#32593,.T.);
#51338=EDGE_CURVE('',#39749,#37051,#32594,.T.);
#51339=EDGE_CURVE('',#38043,#39755,#32595,.T.);
#51340=EDGE_CURVE('',#39750,#37050,#32596,.T.);
#51341=EDGE_CURVE('',#38041,#39754,#1319,.T.);
#51342=EDGE_CURVE('',#39733,#37049,#32597,.T.);
#51343=EDGE_CURVE('',#38036,#39753,#32598,.T.);
#51344=EDGE_CURVE('',#39734,#37048,#32599,.T.);
#51345=EDGE_CURVE('',#37521,#39752,#32600,.T.);
#51346=EDGE_CURVE('',#39739,#37047,#32601,.T.);
#51347=EDGE_CURVE('',#37522,#39751,#32602,.T.);
#51348=EDGE_CURVE('',#39740,#37046,#32603,.T.);
#51349=EDGE_CURVE('',#37523,#39732,#32604,.T.);
#51350=EDGE_CURVE('',#39741,#38074,#32605,.T.);
#51351=EDGE_CURVE('',#37524,#39735,#32606,.T.);
#51352=EDGE_CURVE('',#39742,#38070,#1320,.T.);
#51353=EDGE_CURVE('',#37525,#39738,#32607,.T.);
#51354=EDGE_CURVE('',#39743,#38069,#32608,.T.);
#51355=EDGE_CURVE('',#37526,#39737,#32609,.T.);
#51356=EDGE_CURVE('',#39744,#38066,#32610,.T.);
#51357=EDGE_CURVE('',#38057,#39736,#32611,.T.);
#51358=EDGE_CURVE('',#39745,#38065,#32612,.T.);
#51359=EDGE_CURVE('',#38058,#39747,#1321,.T.);
#51360=EDGE_CURVE('',#39746,#38062,#32613,.T.);
#51361=EDGE_CURVE('',#39787,#38033,#1322,.T.);
#51362=EDGE_CURVE('',#38028,#39786,#32614,.T.);
#51363=EDGE_CURVE('',#38027,#39785,#32615,.T.);
#51364=EDGE_CURVE('',#39776,#38035,#32616,.T.);
#51365=EDGE_CURVE('',#38024,#39784,#32617,.T.);
#51366=EDGE_CURVE('',#39777,#37057,#32618,.T.);
#51367=EDGE_CURVE('',#38023,#39783,#32619,.T.);
#51368=EDGE_CURVE('',#39778,#37056,#32620,.T.);
#51369=EDGE_CURVE('',#38021,#39782,#1323,.T.);
#51370=EDGE_CURVE('',#39761,#37055,#32621,.T.);
#51371=EDGE_CURVE('',#38016,#39781,#32622,.T.);
#51372=EDGE_CURVE('',#39762,#37054,#32623,.T.);
#51373=EDGE_CURVE('',#37515,#39780,#32624,.T.);
#51374=EDGE_CURVE('',#39767,#37053,#32625,.T.);
#51375=EDGE_CURVE('',#37516,#39779,#32626,.T.);
#51376=EDGE_CURVE('',#39768,#37052,#32627,.T.);
#51377=EDGE_CURVE('',#37517,#39760,#32628,.T.);
#51378=EDGE_CURVE('',#39769,#38054,#32629,.T.);
#51379=EDGE_CURVE('',#37518,#39763,#32630,.T.);
#51380=EDGE_CURVE('',#39770,#38050,#1324,.T.);
#51381=EDGE_CURVE('',#37519,#39766,#32631,.T.);
#51382=EDGE_CURVE('',#39771,#38049,#32632,.T.);
#51383=EDGE_CURVE('',#37520,#39765,#32633,.T.);
#51384=EDGE_CURVE('',#39772,#38046,#32634,.T.);
#51385=EDGE_CURVE('',#38037,#39764,#32635,.T.);
#51386=EDGE_CURVE('',#39773,#38045,#32636,.T.);
#51387=EDGE_CURVE('',#38038,#39775,#1325,.T.);
#51388=EDGE_CURVE('',#39774,#38042,#32637,.T.);
#51389=EDGE_CURVE('',#39815,#38013,#1326,.T.);
#51390=EDGE_CURVE('',#38008,#39814,#32638,.T.);
#51391=EDGE_CURVE('',#38007,#39813,#32639,.T.);
#51392=EDGE_CURVE('',#39804,#38015,#32640,.T.);
#51393=EDGE_CURVE('',#38004,#39812,#32641,.T.);
#51394=EDGE_CURVE('',#39805,#37063,#32642,.T.);
#51395=EDGE_CURVE('',#38003,#39811,#32643,.T.);
#51396=EDGE_CURVE('',#39806,#37062,#32644,.T.);
#51397=EDGE_CURVE('',#38001,#39810,#1327,.T.);
#51398=EDGE_CURVE('',#39789,#37061,#32645,.T.);
#51399=EDGE_CURVE('',#37996,#39809,#32646,.T.);
#51400=EDGE_CURVE('',#39790,#37060,#32647,.T.);
#51401=EDGE_CURVE('',#37509,#39808,#32648,.T.);
#51402=EDGE_CURVE('',#39795,#37059,#32649,.T.);
#51403=EDGE_CURVE('',#37510,#39807,#32650,.T.);
#51404=EDGE_CURVE('',#39796,#37058,#32651,.T.);
#51405=EDGE_CURVE('',#37511,#39788,#32652,.T.);
#51406=EDGE_CURVE('',#39797,#38034,#32653,.T.);
#51407=EDGE_CURVE('',#37512,#39791,#32654,.T.);
#51408=EDGE_CURVE('',#39798,#38030,#1328,.T.);
#51409=EDGE_CURVE('',#37513,#39794,#32655,.T.);
#51410=EDGE_CURVE('',#39799,#38029,#32656,.T.);
#51411=EDGE_CURVE('',#37514,#39793,#32657,.T.);
#51412=EDGE_CURVE('',#39800,#38026,#32658,.T.);
#51413=EDGE_CURVE('',#38017,#39792,#32659,.T.);
#51414=EDGE_CURVE('',#39801,#38025,#32660,.T.);
#51415=EDGE_CURVE('',#38018,#39803,#1329,.T.);
#51416=EDGE_CURVE('',#39802,#38022,#32661,.T.);
#51417=EDGE_CURVE('',#39843,#37993,#1330,.T.);
#51418=EDGE_CURVE('',#37988,#39842,#32662,.T.);
#51419=EDGE_CURVE('',#37987,#39841,#32663,.T.);
#51420=EDGE_CURVE('',#39832,#37995,#32664,.T.);
#51421=EDGE_CURVE('',#37984,#39840,#32665,.T.);
#51422=EDGE_CURVE('',#39833,#37069,#32666,.T.);
#51423=EDGE_CURVE('',#37983,#39839,#32667,.T.);
#51424=EDGE_CURVE('',#39834,#37068,#32668,.T.);
#51425=EDGE_CURVE('',#37981,#39838,#1331,.T.);
#51426=EDGE_CURVE('',#39817,#37067,#32669,.T.);
#51427=EDGE_CURVE('',#37976,#39837,#32670,.T.);
#51428=EDGE_CURVE('',#39818,#37066,#32671,.T.);
#51429=EDGE_CURVE('',#37503,#39836,#32672,.T.);
#51430=EDGE_CURVE('',#39823,#37065,#32673,.T.);
#51431=EDGE_CURVE('',#37504,#39835,#32674,.T.);
#51432=EDGE_CURVE('',#39824,#37064,#32675,.T.);
#51433=EDGE_CURVE('',#37505,#39816,#32676,.T.);
#51434=EDGE_CURVE('',#39825,#38014,#32677,.T.);
#51435=EDGE_CURVE('',#37506,#39819,#32678,.T.);
#51436=EDGE_CURVE('',#39826,#38010,#1332,.T.);
#51437=EDGE_CURVE('',#37507,#39822,#32679,.T.);
#51438=EDGE_CURVE('',#39827,#38009,#32680,.T.);
#51439=EDGE_CURVE('',#37508,#39821,#32681,.T.);
#51440=EDGE_CURVE('',#39828,#38006,#32682,.T.);
#51441=EDGE_CURVE('',#37997,#39820,#32683,.T.);
#51442=EDGE_CURVE('',#39829,#38005,#32684,.T.);
#51443=EDGE_CURVE('',#37998,#39831,#1333,.T.);
#51444=EDGE_CURVE('',#39830,#38002,#32685,.T.);
#51445=EDGE_CURVE('',#39871,#37973,#1334,.T.);
#51446=EDGE_CURVE('',#37968,#39870,#32686,.T.);
#51447=EDGE_CURVE('',#37967,#39869,#32687,.T.);
#51448=EDGE_CURVE('',#39860,#37975,#32688,.T.);
#51449=EDGE_CURVE('',#37964,#39868,#32689,.T.);
#51450=EDGE_CURVE('',#39861,#37075,#32690,.T.);
#51451=EDGE_CURVE('',#37963,#39867,#32691,.T.);
#51452=EDGE_CURVE('',#39862,#37074,#32692,.T.);
#51453=EDGE_CURVE('',#37961,#39866,#1335,.T.);
#51454=EDGE_CURVE('',#39845,#37073,#32693,.T.);
#51455=EDGE_CURVE('',#37956,#39865,#32694,.T.);
#51456=EDGE_CURVE('',#39846,#37072,#32695,.T.);
#51457=EDGE_CURVE('',#37497,#39864,#32696,.T.);
#51458=EDGE_CURVE('',#39851,#37071,#32697,.T.);
#51459=EDGE_CURVE('',#37498,#39863,#32698,.T.);
#51460=EDGE_CURVE('',#39852,#37070,#32699,.T.);
#51461=EDGE_CURVE('',#37499,#39844,#32700,.T.);
#51462=EDGE_CURVE('',#39853,#37994,#32701,.T.);
#51463=EDGE_CURVE('',#37500,#39847,#32702,.T.);
#51464=EDGE_CURVE('',#39854,#37990,#1336,.T.);
#51465=EDGE_CURVE('',#37501,#39850,#32703,.T.);
#51466=EDGE_CURVE('',#39855,#37989,#32704,.T.);
#51467=EDGE_CURVE('',#37502,#39849,#32705,.T.);
#51468=EDGE_CURVE('',#39856,#37986,#32706,.T.);
#51469=EDGE_CURVE('',#37977,#39848,#32707,.T.);
#51470=EDGE_CURVE('',#39857,#37985,#32708,.T.);
#51471=EDGE_CURVE('',#37978,#39859,#1337,.T.);
#51472=EDGE_CURVE('',#39858,#37982,#32709,.T.);
#51473=EDGE_CURVE('',#39899,#37953,#1338,.T.);
#51474=EDGE_CURVE('',#37948,#39898,#32710,.T.);
#51475=EDGE_CURVE('',#37947,#39897,#32711,.T.);
#51476=EDGE_CURVE('',#39888,#37955,#32712,.T.);
#51477=EDGE_CURVE('',#37944,#39896,#32713,.T.);
#51478=EDGE_CURVE('',#39889,#37081,#32714,.T.);
#51479=EDGE_CURVE('',#37943,#39895,#32715,.T.);
#51480=EDGE_CURVE('',#39890,#37080,#32716,.T.);
#51481=EDGE_CURVE('',#37941,#39894,#1339,.T.);
#51482=EDGE_CURVE('',#39873,#37079,#32717,.T.);
#51483=EDGE_CURVE('',#37936,#39893,#32718,.T.);
#51484=EDGE_CURVE('',#39874,#37078,#32719,.T.);
#51485=EDGE_CURVE('',#37491,#39892,#32720,.T.);
#51486=EDGE_CURVE('',#39879,#37077,#32721,.T.);
#51487=EDGE_CURVE('',#37492,#39891,#32722,.T.);
#51488=EDGE_CURVE('',#39880,#37076,#32723,.T.);
#51489=EDGE_CURVE('',#37493,#39872,#32724,.T.);
#51490=EDGE_CURVE('',#39881,#37974,#32725,.T.);
#51491=EDGE_CURVE('',#37494,#39875,#32726,.T.);
#51492=EDGE_CURVE('',#39882,#37970,#1340,.T.);
#51493=EDGE_CURVE('',#37495,#39878,#32727,.T.);
#51494=EDGE_CURVE('',#39883,#37969,#32728,.T.);
#51495=EDGE_CURVE('',#37496,#39877,#32729,.T.);
#51496=EDGE_CURVE('',#39884,#37966,#32730,.T.);
#51497=EDGE_CURVE('',#37957,#39876,#32731,.T.);
#51498=EDGE_CURVE('',#39885,#37965,#32732,.T.);
#51499=EDGE_CURVE('',#37958,#39887,#1341,.T.);
#51500=EDGE_CURVE('',#39886,#37962,#32733,.T.);
#51501=EDGE_CURVE('',#39927,#37933,#1342,.T.);
#51502=EDGE_CURVE('',#37928,#39926,#32734,.T.);
#51503=EDGE_CURVE('',#37927,#39925,#32735,.T.);
#51504=EDGE_CURVE('',#39916,#37935,#32736,.T.);
#51505=EDGE_CURVE('',#37924,#39924,#32737,.T.);
#51506=EDGE_CURVE('',#39917,#37087,#32738,.T.);
#51507=EDGE_CURVE('',#37923,#39923,#32739,.T.);
#51508=EDGE_CURVE('',#39918,#37086,#32740,.T.);
#51509=EDGE_CURVE('',#37921,#39922,#1343,.T.);
#51510=EDGE_CURVE('',#39901,#37085,#32741,.T.);
#51511=EDGE_CURVE('',#37916,#39921,#32742,.T.);
#51512=EDGE_CURVE('',#39902,#37084,#32743,.T.);
#51513=EDGE_CURVE('',#37485,#39920,#32744,.T.);
#51514=EDGE_CURVE('',#39907,#37083,#32745,.T.);
#51515=EDGE_CURVE('',#37486,#39919,#32746,.T.);
#51516=EDGE_CURVE('',#39908,#37082,#32747,.T.);
#51517=EDGE_CURVE('',#37487,#39900,#32748,.T.);
#51518=EDGE_CURVE('',#39909,#37954,#32749,.T.);
#51519=EDGE_CURVE('',#37488,#39903,#32750,.T.);
#51520=EDGE_CURVE('',#39910,#37950,#1344,.T.);
#51521=EDGE_CURVE('',#37489,#39906,#32751,.T.);
#51522=EDGE_CURVE('',#39911,#37949,#32752,.T.);
#51523=EDGE_CURVE('',#37490,#39905,#32753,.T.);
#51524=EDGE_CURVE('',#39912,#37946,#32754,.T.);
#51525=EDGE_CURVE('',#37937,#39904,#32755,.T.);
#51526=EDGE_CURVE('',#39913,#37945,#32756,.T.);
#51527=EDGE_CURVE('',#37938,#39915,#1345,.T.);
#51528=EDGE_CURVE('',#39914,#37942,#32757,.T.);
#51529=EDGE_CURVE('',#39955,#37913,#1346,.T.);
#51530=EDGE_CURVE('',#37908,#39954,#32758,.T.);
#51531=EDGE_CURVE('',#37907,#39953,#32759,.T.);
#51532=EDGE_CURVE('',#39944,#37915,#32760,.T.);
#51533=EDGE_CURVE('',#37904,#39952,#32761,.T.);
#51534=EDGE_CURVE('',#39945,#37093,#32762,.T.);
#51535=EDGE_CURVE('',#37903,#39951,#32763,.T.);
#51536=EDGE_CURVE('',#39946,#37092,#32764,.T.);
#51537=EDGE_CURVE('',#37901,#39950,#1347,.T.);
#51538=EDGE_CURVE('',#39929,#37091,#32765,.T.);
#51539=EDGE_CURVE('',#37896,#39949,#32766,.T.);
#51540=EDGE_CURVE('',#39930,#37090,#32767,.T.);
#51541=EDGE_CURVE('',#37479,#39948,#32768,.T.);
#51542=EDGE_CURVE('',#39935,#37089,#32769,.T.);
#51543=EDGE_CURVE('',#37480,#39947,#32770,.T.);
#51544=EDGE_CURVE('',#39936,#37088,#32771,.T.);
#51545=EDGE_CURVE('',#37481,#39928,#32772,.T.);
#51546=EDGE_CURVE('',#39937,#37934,#32773,.T.);
#51547=EDGE_CURVE('',#37482,#39931,#32774,.T.);
#51548=EDGE_CURVE('',#39938,#37930,#1348,.T.);
#51549=EDGE_CURVE('',#37483,#39934,#32775,.T.);
#51550=EDGE_CURVE('',#39939,#37929,#32776,.T.);
#51551=EDGE_CURVE('',#37484,#39933,#32777,.T.);
#51552=EDGE_CURVE('',#39940,#37926,#32778,.T.);
#51553=EDGE_CURVE('',#37917,#39932,#32779,.T.);
#51554=EDGE_CURVE('',#39941,#37925,#32780,.T.);
#51555=EDGE_CURVE('',#37918,#39943,#1349,.T.);
#51556=EDGE_CURVE('',#39942,#37922,#32781,.T.);
#51557=EDGE_CURVE('',#39983,#37893,#1350,.T.);
#51558=EDGE_CURVE('',#37888,#39982,#32782,.T.);
#51559=EDGE_CURVE('',#37887,#39981,#32783,.T.);
#51560=EDGE_CURVE('',#39972,#37895,#32784,.T.);
#51561=EDGE_CURVE('',#37884,#39980,#32785,.T.);
#51562=EDGE_CURVE('',#39973,#37099,#32786,.T.);
#51563=EDGE_CURVE('',#37883,#39979,#32787,.T.);
#51564=EDGE_CURVE('',#39974,#37098,#32788,.T.);
#51565=EDGE_CURVE('',#37881,#39978,#1351,.T.);
#51566=EDGE_CURVE('',#39957,#37097,#32789,.T.);
#51567=EDGE_CURVE('',#37876,#39977,#32790,.T.);
#51568=EDGE_CURVE('',#39958,#37096,#32791,.T.);
#51569=EDGE_CURVE('',#37473,#39976,#32792,.T.);
#51570=EDGE_CURVE('',#39963,#37095,#32793,.T.);
#51571=EDGE_CURVE('',#37474,#39975,#32794,.T.);
#51572=EDGE_CURVE('',#39964,#37094,#32795,.T.);
#51573=EDGE_CURVE('',#37475,#39956,#32796,.T.);
#51574=EDGE_CURVE('',#39965,#37914,#32797,.T.);
#51575=EDGE_CURVE('',#37476,#39959,#32798,.T.);
#51576=EDGE_CURVE('',#39966,#37910,#1352,.T.);
#51577=EDGE_CURVE('',#37477,#39962,#32799,.T.);
#51578=EDGE_CURVE('',#39967,#37909,#32800,.T.);
#51579=EDGE_CURVE('',#37478,#39961,#32801,.T.);
#51580=EDGE_CURVE('',#39968,#37906,#32802,.T.);
#51581=EDGE_CURVE('',#37897,#39960,#32803,.T.);
#51582=EDGE_CURVE('',#39969,#37905,#32804,.T.);
#51583=EDGE_CURVE('',#37898,#39971,#1353,.T.);
#51584=EDGE_CURVE('',#39970,#37902,#32805,.T.);
#51585=EDGE_CURVE('',#40011,#37873,#1354,.T.);
#51586=EDGE_CURVE('',#37868,#40010,#32806,.T.);
#51587=EDGE_CURVE('',#37867,#40009,#32807,.T.);
#51588=EDGE_CURVE('',#40000,#37875,#32808,.T.);
#51589=EDGE_CURVE('',#37864,#40008,#32809,.T.);
#51590=EDGE_CURVE('',#40001,#37105,#32810,.T.);
#51591=EDGE_CURVE('',#37863,#40007,#32811,.T.);
#51592=EDGE_CURVE('',#40002,#37104,#32812,.T.);
#51593=EDGE_CURVE('',#37861,#40006,#1355,.T.);
#51594=EDGE_CURVE('',#39985,#37103,#32813,.T.);
#51595=EDGE_CURVE('',#37856,#40005,#32814,.T.);
#51596=EDGE_CURVE('',#39986,#37102,#32815,.T.);
#51597=EDGE_CURVE('',#37467,#40004,#32816,.T.);
#51598=EDGE_CURVE('',#39991,#37101,#32817,.T.);
#51599=EDGE_CURVE('',#37468,#40003,#32818,.T.);
#51600=EDGE_CURVE('',#39992,#37100,#32819,.T.);
#51601=EDGE_CURVE('',#37469,#39984,#32820,.T.);
#51602=EDGE_CURVE('',#39993,#37894,#32821,.T.);
#51603=EDGE_CURVE('',#37470,#39987,#32822,.T.);
#51604=EDGE_CURVE('',#39994,#37890,#1356,.T.);
#51605=EDGE_CURVE('',#37471,#39990,#32823,.T.);
#51606=EDGE_CURVE('',#39995,#37889,#32824,.T.);
#51607=EDGE_CURVE('',#37472,#39989,#32825,.T.);
#51608=EDGE_CURVE('',#39996,#37886,#32826,.T.);
#51609=EDGE_CURVE('',#37877,#39988,#32827,.T.);
#51610=EDGE_CURVE('',#39997,#37885,#32828,.T.);
#51611=EDGE_CURVE('',#37878,#39999,#1357,.T.);
#51612=EDGE_CURVE('',#39998,#37882,#32829,.T.);
#51613=EDGE_CURVE('',#40035,#37853,#1358,.T.);
#51614=EDGE_CURVE('',#37848,#40034,#32830,.T.);
#51615=EDGE_CURVE('',#37847,#40033,#32831,.T.);
#51616=EDGE_CURVE('',#40024,#37855,#32832,.T.);
#51617=EDGE_CURVE('',#37844,#40032,#32833,.T.);
#51618=EDGE_CURVE('',#40025,#37109,#32834,.T.);
#51619=EDGE_CURVE('',#37843,#40031,#32835,.T.);
#51620=EDGE_CURVE('',#40026,#37108,#32836,.T.);
#51621=EDGE_CURVE('',#37841,#40030,#1359,.T.);
#51622=EDGE_CURVE('',#37836,#40029,#32837,.T.);
#51623=EDGE_CURVE('',#37463,#40028,#32838,.T.);
#51624=EDGE_CURVE('',#40015,#37107,#32839,.T.);
#51625=EDGE_CURVE('',#37464,#40027,#32840,.T.);
#51626=EDGE_CURVE('',#40016,#37106,#32841,.T.);
#51627=EDGE_CURVE('',#40017,#37874,#32842,.T.);
#51628=EDGE_CURVE('',#40018,#37870,#1360,.T.);
#51629=EDGE_CURVE('',#37465,#40014,#32843,.T.);
#51630=EDGE_CURVE('',#40019,#37869,#32844,.T.);
#51631=EDGE_CURVE('',#37466,#40013,#32845,.T.);
#51632=EDGE_CURVE('',#40020,#37866,#32846,.T.);
#51633=EDGE_CURVE('',#37857,#40012,#32847,.T.);
#51634=EDGE_CURVE('',#40021,#37865,#32848,.T.);
#51635=EDGE_CURVE('',#37858,#40023,#1361,.T.);
#51636=EDGE_CURVE('',#40022,#37862,#32849,.T.);
#51637=EDGE_CURVE('',#40063,#37833,#1362,.T.);
#51638=EDGE_CURVE('',#37828,#40062,#32850,.T.);
#51639=EDGE_CURVE('',#37827,#40061,#32851,.T.);
#51640=EDGE_CURVE('',#40052,#37835,#32852,.T.);
#51641=EDGE_CURVE('',#37824,#40060,#32853,.T.);
#51642=EDGE_CURVE('',#40053,#37115,#32854,.T.);
#51643=EDGE_CURVE('',#37823,#40059,#32855,.T.);
#51644=EDGE_CURVE('',#40054,#37114,#32856,.T.);
#51645=EDGE_CURVE('',#37821,#40058,#1363,.T.);
#51646=EDGE_CURVE('',#40037,#37113,#32857,.T.);
#51647=EDGE_CURVE('',#37816,#40057,#32858,.T.);
#51648=EDGE_CURVE('',#40038,#37112,#32859,.T.);
#51649=EDGE_CURVE('',#37457,#40056,#32860,.T.);
#51650=EDGE_CURVE('',#40043,#37111,#32861,.T.);
#51651=EDGE_CURVE('',#37458,#40055,#32862,.T.);
#51652=EDGE_CURVE('',#40044,#37110,#32863,.T.);
#51653=EDGE_CURVE('',#37459,#40036,#32864,.T.);
#51654=EDGE_CURVE('',#40045,#37854,#32865,.T.);
#51655=EDGE_CURVE('',#37460,#40039,#32866,.T.);
#51656=EDGE_CURVE('',#40046,#37850,#1364,.T.);
#51657=EDGE_CURVE('',#37461,#40042,#32867,.T.);
#51658=EDGE_CURVE('',#40047,#37849,#32868,.T.);
#51659=EDGE_CURVE('',#37462,#40041,#32869,.T.);
#51660=EDGE_CURVE('',#40048,#37846,#32870,.T.);
#51661=EDGE_CURVE('',#37837,#40040,#32871,.T.);
#51662=EDGE_CURVE('',#40049,#37845,#32872,.T.);
#51663=EDGE_CURVE('',#37838,#40051,#1365,.T.);
#51664=EDGE_CURVE('',#40050,#37842,#32873,.T.);
#51665=EDGE_CURVE('',#40091,#37813,#1366,.T.);
#51666=EDGE_CURVE('',#37808,#40090,#32874,.T.);
#51667=EDGE_CURVE('',#37807,#40089,#32875,.T.);
#51668=EDGE_CURVE('',#40080,#37815,#32876,.T.);
#51669=EDGE_CURVE('',#37804,#40088,#32877,.T.);
#51670=EDGE_CURVE('',#40081,#37121,#32878,.T.);
#51671=EDGE_CURVE('',#37803,#40087,#32879,.T.);
#51672=EDGE_CURVE('',#40082,#37120,#32880,.T.);
#51673=EDGE_CURVE('',#37801,#40086,#1367,.T.);
#51674=EDGE_CURVE('',#40065,#37119,#32881,.T.);
#51675=EDGE_CURVE('',#37796,#40085,#32882,.T.);
#51676=EDGE_CURVE('',#40066,#37118,#32883,.T.);
#51677=EDGE_CURVE('',#37451,#40084,#32884,.T.);
#51678=EDGE_CURVE('',#40071,#37117,#32885,.T.);
#51679=EDGE_CURVE('',#37452,#40083,#32886,.T.);
#51680=EDGE_CURVE('',#40072,#37116,#32887,.T.);
#51681=EDGE_CURVE('',#37453,#40064,#32888,.T.);
#51682=EDGE_CURVE('',#40073,#37834,#32889,.T.);
#51683=EDGE_CURVE('',#37454,#40067,#32890,.T.);
#51684=EDGE_CURVE('',#40074,#37830,#1368,.T.);
#51685=EDGE_CURVE('',#37455,#40070,#32891,.T.);
#51686=EDGE_CURVE('',#40075,#37829,#32892,.T.);
#51687=EDGE_CURVE('',#37456,#40069,#32893,.T.);
#51688=EDGE_CURVE('',#40076,#37826,#32894,.T.);
#51689=EDGE_CURVE('',#37817,#40068,#32895,.T.);
#51690=EDGE_CURVE('',#40077,#37825,#32896,.T.);
#51691=EDGE_CURVE('',#37818,#40079,#1369,.T.);
#51692=EDGE_CURVE('',#40078,#37822,#32897,.T.);
#51693=EDGE_CURVE('',#40119,#37793,#1370,.T.);
#51694=EDGE_CURVE('',#37788,#40118,#32898,.T.);
#51695=EDGE_CURVE('',#37787,#40117,#32899,.T.);
#51696=EDGE_CURVE('',#40108,#37795,#32900,.T.);
#51697=EDGE_CURVE('',#37784,#40116,#32901,.T.);
#51698=EDGE_CURVE('',#40109,#37127,#32902,.T.);
#51699=EDGE_CURVE('',#37783,#40115,#32903,.T.);
#51700=EDGE_CURVE('',#40110,#37126,#32904,.T.);
#51701=EDGE_CURVE('',#37781,#40114,#1371,.T.);
#51702=EDGE_CURVE('',#40093,#37125,#32905,.T.);
#51703=EDGE_CURVE('',#37776,#40113,#32906,.T.);
#51704=EDGE_CURVE('',#40094,#37124,#32907,.T.);
#51705=EDGE_CURVE('',#37445,#40112,#32908,.T.);
#51706=EDGE_CURVE('',#40099,#37123,#32909,.T.);
#51707=EDGE_CURVE('',#37446,#40111,#32910,.T.);
#51708=EDGE_CURVE('',#40100,#37122,#32911,.T.);
#51709=EDGE_CURVE('',#37447,#40092,#32912,.T.);
#51710=EDGE_CURVE('',#40101,#37814,#32913,.T.);
#51711=EDGE_CURVE('',#37448,#40095,#32914,.T.);
#51712=EDGE_CURVE('',#40102,#37810,#1372,.T.);
#51713=EDGE_CURVE('',#37449,#40098,#32915,.T.);
#51714=EDGE_CURVE('',#40103,#37809,#32916,.T.);
#51715=EDGE_CURVE('',#37450,#40097,#32917,.T.);
#51716=EDGE_CURVE('',#40104,#37806,#32918,.T.);
#51717=EDGE_CURVE('',#37797,#40096,#32919,.T.);
#51718=EDGE_CURVE('',#40105,#37805,#32920,.T.);
#51719=EDGE_CURVE('',#37798,#40107,#1373,.T.);
#51720=EDGE_CURVE('',#40106,#37802,#32921,.T.);
#51721=EDGE_CURVE('',#40147,#37773,#1374,.T.);
#51722=EDGE_CURVE('',#37768,#40146,#32922,.T.);
#51723=EDGE_CURVE('',#37767,#40145,#32923,.T.);
#51724=EDGE_CURVE('',#40136,#37775,#32924,.T.);
#51725=EDGE_CURVE('',#37764,#40144,#32925,.T.);
#51726=EDGE_CURVE('',#40137,#37133,#32926,.T.);
#51727=EDGE_CURVE('',#37763,#40143,#32927,.T.);
#51728=EDGE_CURVE('',#40138,#37132,#32928,.T.);
#51729=EDGE_CURVE('',#37761,#40142,#1375,.T.);
#51730=EDGE_CURVE('',#40121,#37131,#32929,.T.);
#51731=EDGE_CURVE('',#37756,#40141,#32930,.T.);
#51732=EDGE_CURVE('',#40122,#37130,#32931,.T.);
#51733=EDGE_CURVE('',#37439,#40140,#32932,.T.);
#51734=EDGE_CURVE('',#40127,#37129,#32933,.T.);
#51735=EDGE_CURVE('',#37440,#40139,#32934,.T.);
#51736=EDGE_CURVE('',#40128,#37128,#32935,.T.);
#51737=EDGE_CURVE('',#37441,#40120,#32936,.T.);
#51738=EDGE_CURVE('',#40129,#37794,#32937,.T.);
#51739=EDGE_CURVE('',#37442,#40123,#32938,.T.);
#51740=EDGE_CURVE('',#40130,#37790,#1376,.T.);
#51741=EDGE_CURVE('',#37443,#40126,#32939,.T.);
#51742=EDGE_CURVE('',#40131,#37789,#32940,.T.);
#51743=EDGE_CURVE('',#37444,#40125,#32941,.T.);
#51744=EDGE_CURVE('',#40132,#37786,#32942,.T.);
#51745=EDGE_CURVE('',#37777,#40124,#32943,.T.);
#51746=EDGE_CURVE('',#40133,#37785,#32944,.T.);
#51747=EDGE_CURVE('',#37778,#40135,#1377,.T.);
#51748=EDGE_CURVE('',#40134,#37782,#32945,.T.);
#51749=EDGE_CURVE('',#40175,#37753,#1378,.T.);
#51750=EDGE_CURVE('',#37748,#40174,#32946,.T.);
#51751=EDGE_CURVE('',#37747,#40173,#32947,.T.);
#51752=EDGE_CURVE('',#40164,#37755,#32948,.T.);
#51753=EDGE_CURVE('',#37744,#40172,#32949,.T.);
#51754=EDGE_CURVE('',#40165,#37139,#32950,.T.);
#51755=EDGE_CURVE('',#37743,#40171,#32951,.T.);
#51756=EDGE_CURVE('',#40166,#37138,#32952,.T.);
#51757=EDGE_CURVE('',#37741,#40170,#1379,.T.);
#51758=EDGE_CURVE('',#40149,#37137,#32953,.T.);
#51759=EDGE_CURVE('',#37736,#40169,#32954,.T.);
#51760=EDGE_CURVE('',#40150,#37136,#32955,.T.);
#51761=EDGE_CURVE('',#37433,#40168,#32956,.T.);
#51762=EDGE_CURVE('',#40155,#37135,#32957,.T.);
#51763=EDGE_CURVE('',#37434,#40167,#32958,.T.);
#51764=EDGE_CURVE('',#40156,#37134,#32959,.T.);
#51765=EDGE_CURVE('',#37435,#40148,#32960,.T.);
#51766=EDGE_CURVE('',#40157,#37774,#32961,.T.);
#51767=EDGE_CURVE('',#37436,#40151,#32962,.T.);
#51768=EDGE_CURVE('',#40158,#37770,#1380,.T.);
#51769=EDGE_CURVE('',#37437,#40154,#32963,.T.);
#51770=EDGE_CURVE('',#40159,#37769,#32964,.T.);
#51771=EDGE_CURVE('',#37438,#40153,#32965,.T.);
#51772=EDGE_CURVE('',#40160,#37766,#32966,.T.);
#51773=EDGE_CURVE('',#37757,#40152,#32967,.T.);
#51774=EDGE_CURVE('',#40161,#37765,#32968,.T.);
#51775=EDGE_CURVE('',#37758,#40163,#1381,.T.);
#51776=EDGE_CURVE('',#40162,#37762,#32969,.T.);
#51777=EDGE_CURVE('',#40203,#37733,#1382,.T.);
#51778=EDGE_CURVE('',#37728,#40202,#32970,.T.);
#51779=EDGE_CURVE('',#37727,#40201,#32971,.T.);
#51780=EDGE_CURVE('',#40192,#37735,#32972,.T.);
#51781=EDGE_CURVE('',#37724,#40200,#32973,.T.);
#51782=EDGE_CURVE('',#40193,#37145,#32974,.T.);
#51783=EDGE_CURVE('',#37723,#40199,#32975,.T.);
#51784=EDGE_CURVE('',#40194,#37144,#32976,.T.);
#51785=EDGE_CURVE('',#37721,#40198,#1383,.T.);
#51786=EDGE_CURVE('',#40177,#37143,#32977,.T.);
#51787=EDGE_CURVE('',#37716,#40197,#32978,.T.);
#51788=EDGE_CURVE('',#40178,#37142,#32979,.T.);
#51789=EDGE_CURVE('',#37427,#40196,#32980,.T.);
#51790=EDGE_CURVE('',#40183,#37141,#32981,.T.);
#51791=EDGE_CURVE('',#37428,#40195,#32982,.T.);
#51792=EDGE_CURVE('',#40184,#37140,#32983,.T.);
#51793=EDGE_CURVE('',#37429,#40176,#32984,.T.);
#51794=EDGE_CURVE('',#40185,#37754,#32985,.T.);
#51795=EDGE_CURVE('',#37430,#40179,#32986,.T.);
#51796=EDGE_CURVE('',#40186,#37750,#1384,.T.);
#51797=EDGE_CURVE('',#37431,#40182,#32987,.T.);
#51798=EDGE_CURVE('',#40187,#37749,#32988,.T.);
#51799=EDGE_CURVE('',#37432,#40181,#32989,.T.);
#51800=EDGE_CURVE('',#40188,#37746,#32990,.T.);
#51801=EDGE_CURVE('',#37737,#40180,#32991,.T.);
#51802=EDGE_CURVE('',#40189,#37745,#32992,.T.);
#51803=EDGE_CURVE('',#37738,#40191,#1385,.T.);
#51804=EDGE_CURVE('',#40190,#37742,#32993,.T.);
#51805=EDGE_CURVE('',#40231,#37713,#1386,.T.);
#51806=EDGE_CURVE('',#37708,#40230,#32994,.T.);
#51807=EDGE_CURVE('',#37707,#40229,#32995,.T.);
#51808=EDGE_CURVE('',#40220,#37715,#32996,.T.);
#51809=EDGE_CURVE('',#37704,#40228,#32997,.T.);
#51810=EDGE_CURVE('',#40221,#37151,#32998,.T.);
#51811=EDGE_CURVE('',#37703,#40227,#32999,.T.);
#51812=EDGE_CURVE('',#40222,#37150,#33000,.T.);
#51813=EDGE_CURVE('',#37701,#40226,#1387,.T.);
#51814=EDGE_CURVE('',#40205,#37149,#33001,.T.);
#51815=EDGE_CURVE('',#37696,#40225,#33002,.T.);
#51816=EDGE_CURVE('',#40206,#37148,#33003,.T.);
#51817=EDGE_CURVE('',#37421,#40224,#33004,.T.);
#51818=EDGE_CURVE('',#40211,#37147,#33005,.T.);
#51819=EDGE_CURVE('',#37422,#40223,#33006,.T.);
#51820=EDGE_CURVE('',#40212,#37146,#33007,.T.);
#51821=EDGE_CURVE('',#37423,#40204,#33008,.T.);
#51822=EDGE_CURVE('',#40213,#37734,#33009,.T.);
#51823=EDGE_CURVE('',#37424,#40207,#33010,.T.);
#51824=EDGE_CURVE('',#40214,#37730,#1388,.T.);
#51825=EDGE_CURVE('',#37425,#40210,#33011,.T.);
#51826=EDGE_CURVE('',#40215,#37729,#33012,.T.);
#51827=EDGE_CURVE('',#37426,#40209,#33013,.T.);
#51828=EDGE_CURVE('',#40216,#37726,#33014,.T.);
#51829=EDGE_CURVE('',#37717,#40208,#33015,.T.);
#51830=EDGE_CURVE('',#40217,#37725,#33016,.T.);
#51831=EDGE_CURVE('',#37718,#40219,#1389,.T.);
#51832=EDGE_CURVE('',#40218,#37722,#33017,.T.);
#51833=EDGE_CURVE('',#40259,#37693,#1390,.T.);
#51834=EDGE_CURVE('',#37688,#40258,#33018,.T.);
#51835=EDGE_CURVE('',#37687,#40257,#33019,.T.);
#51836=EDGE_CURVE('',#40248,#37695,#33020,.T.);
#51837=EDGE_CURVE('',#37684,#40256,#33021,.T.);
#51838=EDGE_CURVE('',#40249,#37157,#33022,.T.);
#51839=EDGE_CURVE('',#37683,#40255,#33023,.T.);
#51840=EDGE_CURVE('',#40250,#37156,#33024,.T.);
#51841=EDGE_CURVE('',#37681,#40254,#1391,.T.);
#51842=EDGE_CURVE('',#40233,#37155,#33025,.T.);
#51843=EDGE_CURVE('',#37676,#40253,#33026,.T.);
#51844=EDGE_CURVE('',#40234,#37154,#33027,.T.);
#51845=EDGE_CURVE('',#37415,#40252,#33028,.T.);
#51846=EDGE_CURVE('',#40239,#37153,#33029,.T.);
#51847=EDGE_CURVE('',#37416,#40251,#33030,.T.);
#51848=EDGE_CURVE('',#40240,#37152,#33031,.T.);
#51849=EDGE_CURVE('',#37417,#40232,#33032,.T.);
#51850=EDGE_CURVE('',#40241,#37714,#33033,.T.);
#51851=EDGE_CURVE('',#37418,#40235,#33034,.T.);
#51852=EDGE_CURVE('',#40242,#37710,#1392,.T.);
#51853=EDGE_CURVE('',#37419,#40238,#33035,.T.);
#51854=EDGE_CURVE('',#40243,#37709,#33036,.T.);
#51855=EDGE_CURVE('',#37420,#40237,#33037,.T.);
#51856=EDGE_CURVE('',#40244,#37706,#33038,.T.);
#51857=EDGE_CURVE('',#37697,#40236,#33039,.T.);
#51858=EDGE_CURVE('',#40245,#37705,#33040,.T.);
#51859=EDGE_CURVE('',#37698,#40247,#1393,.T.);
#51860=EDGE_CURVE('',#40246,#37702,#33041,.T.);
#51861=EDGE_CURVE('',#40287,#37673,#1394,.T.);
#51862=EDGE_CURVE('',#37668,#40286,#33042,.T.);
#51863=EDGE_CURVE('',#37667,#40285,#33043,.T.);
#51864=EDGE_CURVE('',#40276,#37675,#33044,.T.);
#51865=EDGE_CURVE('',#37664,#40284,#33045,.T.);
#51866=EDGE_CURVE('',#40277,#37163,#33046,.T.);
#51867=EDGE_CURVE('',#37663,#40283,#33047,.T.);
#51868=EDGE_CURVE('',#40278,#37162,#33048,.T.);
#51869=EDGE_CURVE('',#37661,#40282,#1395,.T.);
#51870=EDGE_CURVE('',#40261,#37161,#33049,.T.);
#51871=EDGE_CURVE('',#37656,#40281,#33050,.T.);
#51872=EDGE_CURVE('',#40262,#37160,#33051,.T.);
#51873=EDGE_CURVE('',#37409,#40280,#33052,.T.);
#51874=EDGE_CURVE('',#40267,#37159,#33053,.T.);
#51875=EDGE_CURVE('',#37410,#40279,#33054,.T.);
#51876=EDGE_CURVE('',#40268,#37158,#33055,.T.);
#51877=EDGE_CURVE('',#37411,#40260,#33056,.T.);
#51878=EDGE_CURVE('',#40269,#37694,#33057,.T.);
#51879=EDGE_CURVE('',#37412,#40263,#33058,.T.);
#51880=EDGE_CURVE('',#40270,#37690,#1396,.T.);
#51881=EDGE_CURVE('',#37413,#40266,#33059,.T.);
#51882=EDGE_CURVE('',#40271,#37689,#33060,.T.);
#51883=EDGE_CURVE('',#37414,#40265,#33061,.T.);
#51884=EDGE_CURVE('',#40272,#37686,#33062,.T.);
#51885=EDGE_CURVE('',#37677,#40264,#33063,.T.);
#51886=EDGE_CURVE('',#40273,#37685,#33064,.T.);
#51887=EDGE_CURVE('',#37678,#40275,#1397,.T.);
#51888=EDGE_CURVE('',#40274,#37682,#33065,.T.);
#51889=EDGE_CURVE('',#40315,#37653,#1398,.T.);
#51890=EDGE_CURVE('',#37648,#40314,#33066,.T.);
#51891=EDGE_CURVE('',#37647,#40313,#33067,.T.);
#51892=EDGE_CURVE('',#40304,#37655,#33068,.T.);
#51893=EDGE_CURVE('',#37644,#40312,#33069,.T.);
#51894=EDGE_CURVE('',#40305,#37169,#33070,.T.);
#51895=EDGE_CURVE('',#37643,#40311,#33071,.T.);
#51896=EDGE_CURVE('',#40306,#37168,#33072,.T.);
#51897=EDGE_CURVE('',#37641,#40310,#1399,.T.);
#51898=EDGE_CURVE('',#40289,#37167,#33073,.T.);
#51899=EDGE_CURVE('',#37636,#40309,#33074,.T.);
#51900=EDGE_CURVE('',#40290,#37166,#33075,.T.);
#51901=EDGE_CURVE('',#37403,#40308,#33076,.T.);
#51902=EDGE_CURVE('',#40295,#37165,#33077,.T.);
#51903=EDGE_CURVE('',#37404,#40307,#33078,.T.);
#51904=EDGE_CURVE('',#40296,#37164,#33079,.T.);
#51905=EDGE_CURVE('',#37405,#40288,#33080,.T.);
#51906=EDGE_CURVE('',#40297,#37674,#33081,.T.);
#51907=EDGE_CURVE('',#37406,#40291,#33082,.T.);
#51908=EDGE_CURVE('',#40298,#37670,#1400,.T.);
#51909=EDGE_CURVE('',#37407,#40294,#33083,.T.);
#51910=EDGE_CURVE('',#40299,#37669,#33084,.T.);
#51911=EDGE_CURVE('',#37408,#40293,#33085,.T.);
#51912=EDGE_CURVE('',#40300,#37666,#33086,.T.);
#51913=EDGE_CURVE('',#37657,#40292,#33087,.T.);
#51914=EDGE_CURVE('',#40301,#37665,#33088,.T.);
#51915=EDGE_CURVE('',#37658,#40303,#1401,.T.);
#51916=EDGE_CURVE('',#40302,#37662,#33089,.T.);
#51917=EDGE_CURVE('',#40343,#37633,#1402,.T.);
#51918=EDGE_CURVE('',#37628,#40342,#33090,.T.);
#51919=EDGE_CURVE('',#37627,#40341,#33091,.T.);
#51920=EDGE_CURVE('',#40332,#37635,#33092,.T.);
#51921=EDGE_CURVE('',#37624,#40340,#33093,.T.);
#51922=EDGE_CURVE('',#40333,#37175,#33094,.T.);
#51923=EDGE_CURVE('',#37623,#40339,#33095,.T.);
#51924=EDGE_CURVE('',#40334,#37174,#33096,.T.);
#51925=EDGE_CURVE('',#37621,#40338,#1403,.T.);
#51926=EDGE_CURVE('',#40317,#37173,#33097,.T.);
#51927=EDGE_CURVE('',#37616,#40337,#33098,.T.);
#51928=EDGE_CURVE('',#40318,#37172,#33099,.T.);
#51929=EDGE_CURVE('',#37397,#40336,#33100,.T.);
#51930=EDGE_CURVE('',#40323,#37171,#33101,.T.);
#51931=EDGE_CURVE('',#37398,#40335,#33102,.T.);
#51932=EDGE_CURVE('',#40324,#37170,#33103,.T.);
#51933=EDGE_CURVE('',#37399,#40316,#33104,.T.);
#51934=EDGE_CURVE('',#40325,#37654,#33105,.T.);
#51935=EDGE_CURVE('',#37400,#40319,#33106,.T.);
#51936=EDGE_CURVE('',#40326,#37650,#1404,.T.);
#51937=EDGE_CURVE('',#37401,#40322,#33107,.T.);
#51938=EDGE_CURVE('',#40327,#37649,#33108,.T.);
#51939=EDGE_CURVE('',#37402,#40321,#33109,.T.);
#51940=EDGE_CURVE('',#40328,#37646,#33110,.T.);
#51941=EDGE_CURVE('',#37637,#40320,#33111,.T.);
#51942=EDGE_CURVE('',#40329,#37645,#33112,.T.);
#51943=EDGE_CURVE('',#37638,#40331,#1405,.T.);
#51944=EDGE_CURVE('',#40330,#37642,#33113,.T.);
#51945=EDGE_CURVE('',#40371,#37613,#1406,.T.);
#51946=EDGE_CURVE('',#37608,#40370,#33114,.T.);
#51947=EDGE_CURVE('',#37607,#40369,#33115,.T.);
#51948=EDGE_CURVE('',#40360,#37615,#33116,.T.);
#51949=EDGE_CURVE('',#37604,#40368,#33117,.T.);
#51950=EDGE_CURVE('',#40361,#37181,#33118,.T.);
#51951=EDGE_CURVE('',#37603,#40367,#33119,.T.);
#51952=EDGE_CURVE('',#40362,#37180,#33120,.T.);
#51953=EDGE_CURVE('',#37601,#40366,#1407,.T.);
#51954=EDGE_CURVE('',#40345,#37179,#33121,.T.);
#51955=EDGE_CURVE('',#37596,#40365,#33122,.T.);
#51956=EDGE_CURVE('',#40346,#37178,#33123,.T.);
#51957=EDGE_CURVE('',#37391,#40364,#33124,.T.);
#51958=EDGE_CURVE('',#40351,#37177,#33125,.T.);
#51959=EDGE_CURVE('',#37392,#40363,#33126,.T.);
#51960=EDGE_CURVE('',#40352,#37176,#33127,.T.);
#51961=EDGE_CURVE('',#37393,#40344,#33128,.T.);
#51962=EDGE_CURVE('',#40353,#37634,#33129,.T.);
#51963=EDGE_CURVE('',#37394,#40347,#33130,.T.);
#51964=EDGE_CURVE('',#40354,#37630,#1408,.T.);
#51965=EDGE_CURVE('',#37395,#40350,#33131,.T.);
#51966=EDGE_CURVE('',#40355,#37629,#33132,.T.);
#51967=EDGE_CURVE('',#37396,#40349,#33133,.T.);
#51968=EDGE_CURVE('',#40356,#37626,#33134,.T.);
#51969=EDGE_CURVE('',#37617,#40348,#33135,.T.);
#51970=EDGE_CURVE('',#40357,#37625,#33136,.T.);
#51971=EDGE_CURVE('',#37618,#40359,#1409,.T.);
#51972=EDGE_CURVE('',#40358,#37622,#33137,.T.);
#51973=EDGE_CURVE('',#40399,#37593,#1410,.T.);
#51974=EDGE_CURVE('',#37588,#40398,#33138,.T.);
#51975=EDGE_CURVE('',#37587,#40397,#33139,.T.);
#51976=EDGE_CURVE('',#40388,#37595,#33140,.T.);
#51977=EDGE_CURVE('',#37584,#40396,#33141,.T.);
#51978=EDGE_CURVE('',#40389,#37187,#33142,.T.);
#51979=EDGE_CURVE('',#37583,#40395,#33143,.T.);
#51980=EDGE_CURVE('',#40390,#37186,#33144,.T.);
#51981=EDGE_CURVE('',#37581,#40394,#1411,.T.);
#51982=EDGE_CURVE('',#40373,#37185,#33145,.T.);
#51983=EDGE_CURVE('',#37576,#40393,#33146,.T.);
#51984=EDGE_CURVE('',#40374,#37184,#33147,.T.);
#51985=EDGE_CURVE('',#37385,#40392,#33148,.T.);
#51986=EDGE_CURVE('',#40379,#37183,#33149,.T.);
#51987=EDGE_CURVE('',#37386,#40391,#33150,.T.);
#51988=EDGE_CURVE('',#40380,#37182,#33151,.T.);
#51989=EDGE_CURVE('',#37387,#40372,#33152,.T.);
#51990=EDGE_CURVE('',#40381,#37614,#33153,.T.);
#51991=EDGE_CURVE('',#37388,#40375,#33154,.T.);
#51992=EDGE_CURVE('',#40382,#37610,#1412,.T.);
#51993=EDGE_CURVE('',#37389,#40378,#33155,.T.);
#51994=EDGE_CURVE('',#40383,#37609,#33156,.T.);
#51995=EDGE_CURVE('',#37390,#40377,#33157,.T.);
#51996=EDGE_CURVE('',#40384,#37606,#33158,.T.);
#51997=EDGE_CURVE('',#37597,#40376,#33159,.T.);
#51998=EDGE_CURVE('',#40385,#37605,#33160,.T.);
#51999=EDGE_CURVE('',#37598,#40387,#1413,.T.);
#52000=EDGE_CURVE('',#40386,#37602,#33161,.T.);
#52001=EDGE_CURVE('',#40427,#37568,#1414,.T.);
#52002=EDGE_CURVE('',#37570,#40426,#33162,.T.);
#52003=EDGE_CURVE('',#37565,#40425,#33163,.T.);
#52004=EDGE_CURVE('',#40416,#37575,#33164,.T.);
#52005=EDGE_CURVE('',#37566,#40424,#33165,.T.);
#52006=EDGE_CURVE('',#40417,#37193,#33166,.T.);
#52007=EDGE_CURVE('',#37563,#40423,#33167,.T.);
#52008=EDGE_CURVE('',#40418,#37192,#33168,.T.);
#52009=EDGE_CURVE('',#37556,#40422,#1415,.T.);
#52010=EDGE_CURVE('',#40401,#37191,#33169,.T.);
#52011=EDGE_CURVE('',#37558,#40421,#33170,.T.);
#52012=EDGE_CURVE('',#40402,#37190,#33171,.T.);
#52013=EDGE_CURVE('',#37379,#40420,#33172,.T.);
#52014=EDGE_CURVE('',#40407,#37189,#33173,.T.);
#52015=EDGE_CURVE('',#37380,#40419,#33174,.T.);
#52016=EDGE_CURVE('',#40408,#37188,#33175,.T.);
#52017=EDGE_CURVE('',#37381,#40400,#33176,.T.);
#52018=EDGE_CURVE('',#40409,#37594,#33177,.T.);
#52019=EDGE_CURVE('',#37382,#40403,#33178,.T.);
#52020=EDGE_CURVE('',#40410,#37590,#1416,.T.);
#52021=EDGE_CURVE('',#37383,#40406,#33179,.T.);
#52022=EDGE_CURVE('',#40411,#37589,#33180,.T.);
#52023=EDGE_CURVE('',#37384,#40405,#33181,.T.);
#52024=EDGE_CURVE('',#40412,#37586,#33182,.T.);
#52025=EDGE_CURVE('',#37577,#40404,#33183,.T.);
#52026=EDGE_CURVE('',#40413,#37585,#33184,.T.);
#52027=EDGE_CURVE('',#37578,#40415,#1417,.T.);
#52028=EDGE_CURVE('',#40414,#37582,#33185,.T.);
#52029=EDGE_CURVE('',#40428,#40429,#33186,.T.);
#52030=EDGE_CURVE('',#40430,#40428,#33187,.T.);
#52031=EDGE_CURVE('',#40431,#40430,#33188,.T.);
#52032=EDGE_CURVE('',#40431,#40429,#33189,.T.);
#52033=EDGE_CURVE('',#40432,#40433,#33190,.T.);
#52034=EDGE_CURVE('',#40434,#40432,#33191,.T.);
#52035=EDGE_CURVE('',#40435,#40434,#33192,.T.);
#52036=EDGE_CURVE('',#40435,#40433,#33193,.T.);
#52037=EDGE_CURVE('',#40436,#40437,#33194,.T.);
#52038=EDGE_CURVE('',#40438,#40436,#33195,.T.);
#52039=EDGE_CURVE('',#40439,#40438,#33196,.T.);
#52040=EDGE_CURVE('',#40439,#40437,#33197,.T.);
#52041=EDGE_CURVE('',#40440,#40441,#33198,.T.);
#52042=EDGE_CURVE('',#40442,#40440,#33199,.T.);
#52043=EDGE_CURVE('',#40443,#40442,#33200,.T.);
#52044=EDGE_CURVE('',#40443,#40444,#33201,.T.);
#52045=EDGE_CURVE('',#40441,#40444,#33202,.T.);
#52046=EDGE_CURVE('',#40445,#40445,#33203,.T.);
#52047=EDGE_CURVE('',#40445,#40446,#33204,.T.);
#52048=EDGE_CURVE('',#40447,#40446,#33205,.T.);
#52049=EDGE_CURVE('',#40446,#40447,#33206,.T.);
#52050=EDGE_CURVE('',#40448,#40448,#33207,.T.);
#52051=EDGE_CURVE('',#40448,#40449,#33208,.T.);
#52052=EDGE_CURVE('',#40449,#40449,#33209,.T.);
#52053=EDGE_CURVE('',#40450,#40450,#33210,.T.);
#52054=EDGE_CURVE('',#40450,#40451,#33211,.T.);
#52055=EDGE_CURVE('',#40452,#40451,#33212,.T.);
#52056=EDGE_CURVE('',#40451,#40452,#33213,.T.);
#52057=EDGE_CURVE('',#40453,#40453,#33214,.T.);
#52058=EDGE_CURVE('',#40453,#40454,#33215,.T.);
#52059=EDGE_CURVE('',#40454,#40454,#33216,.T.);
#52060=EDGE_CURVE('',#40455,#40455,#33217,.T.);
#52061=EDGE_CURVE('',#40455,#40456,#22034,.T.);
#52062=EDGE_CURVE('',#40456,#40456,#33218,.T.);
#52063=EDGE_CURVE('',#40456,#40453,#22035,.T.);
#52064=EDGE_CURVE('',#40457,#40458,#33219,.T.);
#52065=EDGE_CURVE('',#40458,#40459,#4735,.T.);
#52066=EDGE_CURVE('',#40459,#40460,#22036,.T.);
#52067=EDGE_CURVE('',#40460,#40461,#33220,.T.);
#52068=EDGE_CURVE('',#40461,#40462,#22037,.T.);
#52069=EDGE_CURVE('',#40462,#40463,#4736,.T.);
#52070=EDGE_CURVE('',#40463,#40464,#33221,.T.);
#52071=EDGE_CURVE('',#40464,#40465,#4737,.T.);
#52072=EDGE_CURVE('',#40465,#40466,#22038,.T.);
#52073=EDGE_CURVE('',#40466,#40467,#33222,.T.);
#52074=EDGE_CURVE('',#40467,#40468,#22039,.T.);
#52075=EDGE_CURVE('',#40468,#40469,#4738,.T.);
#52076=EDGE_CURVE('',#40469,#40470,#33223,.T.);
#52077=EDGE_CURVE('',#40470,#40471,#4739,.T.);
#52078=EDGE_CURVE('',#40471,#40472,#22040,.T.);
#52079=EDGE_CURVE('',#40472,#40473,#33224,.T.);
#52080=EDGE_CURVE('',#40473,#40474,#22041,.T.);
#52081=EDGE_CURVE('',#40474,#40475,#4740,.T.);
#52082=EDGE_CURVE('',#40475,#40476,#33225,.T.);
#52083=EDGE_CURVE('',#40476,#40477,#4741,.T.);
#52084=EDGE_CURVE('',#40477,#40478,#22042,.T.);
#52085=EDGE_CURVE('',#40478,#40479,#33226,.T.);
#52086=EDGE_CURVE('',#40479,#40480,#22043,.T.);
#52087=EDGE_CURVE('',#40480,#40481,#4742,.T.);
#52088=EDGE_CURVE('',#40481,#40482,#33227,.T.);
#52089=EDGE_CURVE('',#40482,#40483,#4743,.T.);
#52090=EDGE_CURVE('',#40483,#40484,#22044,.T.);
#52091=EDGE_CURVE('',#40484,#40485,#33228,.T.);
#52092=EDGE_CURVE('',#40485,#40486,#22045,.T.);
#52093=EDGE_CURVE('',#40486,#40487,#4744,.T.);
#52094=EDGE_CURVE('',#40487,#40488,#33229,.T.);
#52095=EDGE_CURVE('',#40488,#40489,#4745,.T.);
#52096=EDGE_CURVE('',#40489,#40490,#22046,.T.);
#52097=EDGE_CURVE('',#40490,#40491,#33230,.T.);
#52098=EDGE_CURVE('',#40491,#40492,#22047,.T.);
#52099=EDGE_CURVE('',#40492,#40493,#4746,.T.);
#52100=EDGE_CURVE('',#40493,#40494,#33231,.T.);
#52101=EDGE_CURVE('',#40494,#40495,#4747,.T.);
#52102=EDGE_CURVE('',#40495,#40496,#22048,.T.);
#52103=EDGE_CURVE('',#40496,#40497,#33232,.T.);
#52104=EDGE_CURVE('',#40497,#40498,#22049,.T.);
#52105=EDGE_CURVE('',#40498,#40499,#4748,.T.);
#52106=EDGE_CURVE('',#40499,#40500,#33233,.T.);
#52107=EDGE_CURVE('',#40500,#40501,#4749,.T.);
#52108=EDGE_CURVE('',#40501,#40502,#22050,.T.);
#52109=EDGE_CURVE('',#40502,#40503,#33234,.T.);
#52110=EDGE_CURVE('',#40503,#40504,#22051,.T.);
#52111=EDGE_CURVE('',#40504,#40505,#4750,.T.);
#52112=EDGE_CURVE('',#40505,#40506,#33235,.T.);
#52113=EDGE_CURVE('',#40506,#40507,#4751,.T.);
#52114=EDGE_CURVE('',#40507,#40508,#22052,.T.);
#52115=EDGE_CURVE('',#40508,#40509,#33236,.T.);
#52116=EDGE_CURVE('',#40509,#40510,#22053,.T.);
#52117=EDGE_CURVE('',#40510,#40511,#4752,.T.);
#52118=EDGE_CURVE('',#40511,#40512,#33237,.T.);
#52119=EDGE_CURVE('',#40512,#40513,#4753,.T.);
#52120=EDGE_CURVE('',#40513,#40514,#22054,.T.);
#52121=EDGE_CURVE('',#40514,#40515,#33238,.T.);
#52122=EDGE_CURVE('',#40515,#40516,#22055,.T.);
#52123=EDGE_CURVE('',#40516,#40517,#4754,.T.);
#52124=EDGE_CURVE('',#40517,#40518,#33239,.T.);
#52125=EDGE_CURVE('',#40518,#40519,#4755,.T.);
#52126=EDGE_CURVE('',#40519,#40520,#22056,.T.);
#52127=EDGE_CURVE('',#40520,#40521,#33240,.T.);
#52128=EDGE_CURVE('',#40521,#40522,#22057,.T.);
#52129=EDGE_CURVE('',#40522,#40523,#4756,.T.);
#52130=EDGE_CURVE('',#40523,#40524,#33241,.T.);
#52131=EDGE_CURVE('',#40524,#40525,#4757,.T.);
#52132=EDGE_CURVE('',#40525,#40526,#22058,.T.);
#52133=EDGE_CURVE('',#40526,#40527,#33242,.T.);
#52134=EDGE_CURVE('',#40527,#40528,#22059,.T.);
#52135=EDGE_CURVE('',#40528,#40529,#4758,.T.);
#52136=EDGE_CURVE('',#40529,#40530,#33243,.T.);
#52137=EDGE_CURVE('',#40530,#40531,#4759,.T.);
#52138=EDGE_CURVE('',#40531,#40532,#22060,.T.);
#52139=EDGE_CURVE('',#40532,#40533,#33244,.T.);
#52140=EDGE_CURVE('',#40533,#40534,#22061,.T.);
#52141=EDGE_CURVE('',#40534,#40535,#4760,.T.);
#52142=EDGE_CURVE('',#40535,#40536,#33245,.T.);
#52143=EDGE_CURVE('',#40536,#40537,#4761,.T.);
#52144=EDGE_CURVE('',#40537,#40538,#22062,.T.);
#52145=EDGE_CURVE('',#40538,#40539,#33246,.T.);
#52146=EDGE_CURVE('',#40539,#40540,#22063,.T.);
#52147=EDGE_CURVE('',#40540,#40541,#4762,.T.);
#52148=EDGE_CURVE('',#40541,#40542,#33247,.T.);
#52149=EDGE_CURVE('',#40542,#40543,#4763,.T.);
#52150=EDGE_CURVE('',#40543,#40544,#22064,.T.);
#52151=EDGE_CURVE('',#40544,#40545,#33248,.T.);
#52152=EDGE_CURVE('',#40545,#40546,#22065,.T.);
#52153=EDGE_CURVE('',#40546,#40547,#4764,.T.);
#52154=EDGE_CURVE('',#40547,#40548,#33249,.T.);
#52155=EDGE_CURVE('',#40548,#40549,#4765,.T.);
#52156=EDGE_CURVE('',#40549,#40550,#22066,.T.);
#52157=EDGE_CURVE('',#40550,#40551,#33250,.T.);
#52158=EDGE_CURVE('',#40551,#40552,#22067,.T.);
#52159=EDGE_CURVE('',#40552,#40553,#4766,.T.);
#52160=EDGE_CURVE('',#40553,#40554,#33251,.T.);
#52161=EDGE_CURVE('',#40554,#40555,#4767,.T.);
#52162=EDGE_CURVE('',#40555,#40556,#22068,.T.);
#52163=EDGE_CURVE('',#40556,#40557,#33252,.T.);
#52164=EDGE_CURVE('',#40557,#40558,#22069,.T.);
#52165=EDGE_CURVE('',#40558,#40559,#4768,.T.);
#52166=EDGE_CURVE('',#40559,#40560,#33253,.T.);
#52167=EDGE_CURVE('',#40560,#40561,#4769,.T.);
#52168=EDGE_CURVE('',#40561,#40562,#22070,.T.);
#52169=EDGE_CURVE('',#40562,#40563,#33254,.T.);
#52170=EDGE_CURVE('',#40563,#40564,#22071,.T.);
#52171=EDGE_CURVE('',#40564,#40565,#4770,.T.);
#52172=EDGE_CURVE('',#40565,#40566,#33255,.T.);
#52173=EDGE_CURVE('',#40566,#40567,#4771,.T.);
#52174=EDGE_CURVE('',#40567,#40568,#22072,.T.);
#52175=EDGE_CURVE('',#40568,#40569,#33256,.T.);
#52176=EDGE_CURVE('',#40569,#40570,#22073,.T.);
#52177=EDGE_CURVE('',#40570,#40571,#4772,.T.);
#52178=EDGE_CURVE('',#40571,#40572,#33257,.T.);
#52179=EDGE_CURVE('',#40572,#40573,#4773,.T.);
#52180=EDGE_CURVE('',#40573,#40574,#22074,.T.);
#52181=EDGE_CURVE('',#40574,#40575,#33258,.T.);
#52182=EDGE_CURVE('',#40575,#40576,#22075,.T.);
#52183=EDGE_CURVE('',#40576,#40577,#4774,.T.);
#52184=EDGE_CURVE('',#40577,#40578,#33259,.T.);
#52185=EDGE_CURVE('',#40578,#40579,#4775,.T.);
#52186=EDGE_CURVE('',#40579,#40580,#22076,.T.);
#52187=EDGE_CURVE('',#40580,#40581,#33260,.T.);
#52188=EDGE_CURVE('',#40581,#40582,#22077,.T.);
#52189=EDGE_CURVE('',#40582,#40583,#4776,.T.);
#52190=EDGE_CURVE('',#40583,#40584,#33261,.T.);
#52191=EDGE_CURVE('',#40584,#40585,#4777,.T.);
#52192=EDGE_CURVE('',#40585,#40586,#22078,.T.);
#52193=EDGE_CURVE('',#40586,#40587,#33262,.T.);
#52194=EDGE_CURVE('',#40587,#40588,#22079,.T.);
#52195=EDGE_CURVE('',#40588,#40589,#4778,.T.);
#52196=EDGE_CURVE('',#40589,#40590,#33263,.T.);
#52197=EDGE_CURVE('',#40590,#40591,#4779,.T.);
#52198=EDGE_CURVE('',#40591,#40592,#22080,.T.);
#52199=EDGE_CURVE('',#40592,#40593,#33264,.T.);
#52200=EDGE_CURVE('',#40593,#40594,#22081,.T.);
#52201=EDGE_CURVE('',#40594,#40595,#4780,.T.);
#52202=EDGE_CURVE('',#40595,#40596,#33265,.T.);
#52203=EDGE_CURVE('',#40596,#40597,#4781,.T.);
#52204=EDGE_CURVE('',#40597,#40598,#22082,.T.);
#52205=EDGE_CURVE('',#40598,#40599,#33266,.T.);
#52206=EDGE_CURVE('',#40599,#40600,#22083,.T.);
#52207=EDGE_CURVE('',#40600,#40601,#4782,.T.);
#52208=EDGE_CURVE('',#40601,#40602,#33267,.T.);
#52209=EDGE_CURVE('',#40602,#40603,#4783,.T.);
#52210=EDGE_CURVE('',#40603,#40604,#22084,.T.);
#52211=EDGE_CURVE('',#40604,#40605,#33268,.T.);
#52212=EDGE_CURVE('',#40605,#40606,#22085,.T.);
#52213=EDGE_CURVE('',#40606,#40607,#4784,.T.);
#52214=EDGE_CURVE('',#40607,#40608,#33269,.T.);
#52215=EDGE_CURVE('',#40608,#40609,#4785,.T.);
#52216=EDGE_CURVE('',#40609,#40610,#22086,.T.);
#52217=EDGE_CURVE('',#40610,#40611,#33270,.T.);
#52218=EDGE_CURVE('',#40611,#40612,#22087,.T.);
#52219=EDGE_CURVE('',#40612,#40613,#4786,.T.);
#52220=EDGE_CURVE('',#40613,#40614,#33271,.T.);
#52221=EDGE_CURVE('',#40614,#40615,#4787,.T.);
#52222=EDGE_CURVE('',#40615,#40616,#22088,.T.);
#52223=EDGE_CURVE('',#40616,#40617,#33272,.T.);
#52224=EDGE_CURVE('',#40617,#40618,#22089,.T.);
#52225=EDGE_CURVE('',#40618,#40619,#4788,.T.);
#52226=EDGE_CURVE('',#40619,#40620,#33273,.T.);
#52227=EDGE_CURVE('',#40620,#40621,#4789,.T.);
#52228=EDGE_CURVE('',#40621,#40622,#22090,.T.);
#52229=EDGE_CURVE('',#40622,#40623,#33274,.T.);
#52230=EDGE_CURVE('',#40623,#40624,#22091,.T.);
#52231=EDGE_CURVE('',#40624,#40625,#4790,.T.);
#52232=EDGE_CURVE('',#40625,#40626,#33275,.T.);
#52233=EDGE_CURVE('',#40626,#40627,#4791,.T.);
#52234=EDGE_CURVE('',#40627,#40628,#22092,.T.);
#52235=EDGE_CURVE('',#40628,#40629,#33276,.T.);
#52236=EDGE_CURVE('',#40629,#40630,#22093,.T.);
#52237=EDGE_CURVE('',#40630,#40631,#4792,.T.);
#52238=EDGE_CURVE('',#40631,#40632,#33277,.T.);
#52239=EDGE_CURVE('',#40632,#40633,#4793,.T.);
#52240=EDGE_CURVE('',#40633,#40634,#22094,.T.);
#52241=EDGE_CURVE('',#40634,#40635,#33278,.T.);
#52242=EDGE_CURVE('',#40635,#40636,#22095,.T.);
#52243=EDGE_CURVE('',#40636,#40440,#4794,.T.);
#52244=EDGE_CURVE('',#40441,#40452,#22096,.T.);
#52245=EDGE_CURVE('',#40444,#40637,#4795,.T.);
#52246=EDGE_CURVE('',#40637,#40638,#22097,.T.);
#52247=EDGE_CURVE('',#40638,#40639,#33279,.T.);
#52248=EDGE_CURVE('',#40639,#40640,#22098,.T.);
#52249=EDGE_CURVE('',#40640,#40641,#4796,.T.);
#52250=EDGE_CURVE('',#40641,#40642,#33280,.T.);
#52251=EDGE_CURVE('',#40642,#40643,#4797,.T.);
#52252=EDGE_CURVE('',#40643,#40644,#22099,.T.);
#52253=EDGE_CURVE('',#40644,#40645,#33281,.T.);
#52254=EDGE_CURVE('',#40645,#40646,#22100,.T.);
#52255=EDGE_CURVE('',#40646,#40647,#4798,.T.);
#52256=EDGE_CURVE('',#40647,#40648,#33282,.T.);
#52257=EDGE_CURVE('',#40648,#40649,#4799,.T.);
#52258=EDGE_CURVE('',#40649,#40650,#22101,.T.);
#52259=EDGE_CURVE('',#40650,#40651,#33283,.T.);
#52260=EDGE_CURVE('',#40651,#40652,#22102,.T.);
#52261=EDGE_CURVE('',#40652,#40653,#4800,.T.);
#52262=EDGE_CURVE('',#40653,#40654,#33284,.T.);
#52263=EDGE_CURVE('',#40654,#40655,#4801,.T.);
#52264=EDGE_CURVE('',#40655,#40656,#22103,.T.);
#52265=EDGE_CURVE('',#40656,#40657,#33285,.T.);
#52266=EDGE_CURVE('',#40657,#40658,#22104,.T.);
#52267=EDGE_CURVE('',#40658,#40659,#4802,.T.);
#52268=EDGE_CURVE('',#40659,#40660,#33286,.T.);
#52269=EDGE_CURVE('',#40660,#40661,#4803,.T.);
#52270=EDGE_CURVE('',#40661,#40662,#22105,.T.);
#52271=EDGE_CURVE('',#40662,#40663,#33287,.T.);
#52272=EDGE_CURVE('',#40663,#40664,#22106,.T.);
#52273=EDGE_CURVE('',#40664,#40665,#4804,.T.);
#52274=EDGE_CURVE('',#40665,#40666,#33288,.T.);
#52275=EDGE_CURVE('',#40666,#40667,#4805,.T.);
#52276=EDGE_CURVE('',#40667,#40668,#22107,.T.);
#52277=EDGE_CURVE('',#40668,#40669,#33289,.T.);
#52278=EDGE_CURVE('',#40669,#40670,#22108,.T.);
#52279=EDGE_CURVE('',#40670,#40671,#4806,.T.);
#52280=EDGE_CURVE('',#40671,#40672,#33290,.T.);
#52281=EDGE_CURVE('',#40672,#40673,#4807,.T.);
#52282=EDGE_CURVE('',#40673,#40674,#22109,.T.);
#52283=EDGE_CURVE('',#40674,#40675,#33291,.T.);
#52284=EDGE_CURVE('',#40675,#40676,#22110,.T.);
#52285=EDGE_CURVE('',#40676,#40677,#4808,.T.);
#52286=EDGE_CURVE('',#40677,#40678,#33292,.T.);
#52287=EDGE_CURVE('',#40678,#40679,#4809,.T.);
#52288=EDGE_CURVE('',#40679,#40680,#22111,.T.);
#52289=EDGE_CURVE('',#40680,#40681,#33293,.T.);
#52290=EDGE_CURVE('',#40681,#40682,#22112,.T.);
#52291=EDGE_CURVE('',#40682,#40683,#4810,.T.);
#52292=EDGE_CURVE('',#40683,#40684,#33294,.T.);
#52293=EDGE_CURVE('',#40684,#40685,#4811,.T.);
#52294=EDGE_CURVE('',#40685,#40686,#22113,.T.);
#52295=EDGE_CURVE('',#40686,#40687,#33295,.T.);
#52296=EDGE_CURVE('',#40687,#40688,#22114,.T.);
#52297=EDGE_CURVE('',#40688,#40689,#4812,.T.);
#52298=EDGE_CURVE('',#40689,#40690,#33296,.T.);
#52299=EDGE_CURVE('',#40690,#40691,#4813,.T.);
#52300=EDGE_CURVE('',#40691,#40692,#22115,.T.);
#52301=EDGE_CURVE('',#40692,#40693,#33297,.T.);
#52302=EDGE_CURVE('',#40693,#40694,#22116,.T.);
#52303=EDGE_CURVE('',#40694,#40695,#4814,.T.);
#52304=EDGE_CURVE('',#40695,#40696,#33298,.T.);
#52305=EDGE_CURVE('',#40696,#40697,#4815,.T.);
#52306=EDGE_CURVE('',#40697,#40698,#22117,.T.);
#52307=EDGE_CURVE('',#40698,#40699,#33299,.T.);
#52308=EDGE_CURVE('',#40699,#40700,#22118,.T.);
#52309=EDGE_CURVE('',#40700,#40701,#4816,.T.);
#52310=EDGE_CURVE('',#40701,#40702,#33300,.T.);
#52311=EDGE_CURVE('',#40702,#40703,#4817,.T.);
#52312=EDGE_CURVE('',#40703,#40704,#22119,.T.);
#52313=EDGE_CURVE('',#40704,#40705,#33301,.T.);
#52314=EDGE_CURVE('',#40705,#40706,#22120,.T.);
#52315=EDGE_CURVE('',#40706,#40707,#4818,.T.);
#52316=EDGE_CURVE('',#40707,#40708,#33302,.T.);
#52317=EDGE_CURVE('',#40708,#40709,#4819,.T.);
#52318=EDGE_CURVE('',#40709,#40710,#22121,.T.);
#52319=EDGE_CURVE('',#40710,#40711,#33303,.T.);
#52320=EDGE_CURVE('',#40711,#40712,#22122,.T.);
#52321=EDGE_CURVE('',#40712,#40713,#4820,.T.);
#52322=EDGE_CURVE('',#40713,#40714,#33304,.T.);
#52323=EDGE_CURVE('',#40714,#40715,#4821,.T.);
#52324=EDGE_CURVE('',#40715,#40716,#22123,.T.);
#52325=EDGE_CURVE('',#40716,#40717,#33305,.T.);
#52326=EDGE_CURVE('',#40717,#40718,#22124,.T.);
#52327=EDGE_CURVE('',#40718,#40719,#4822,.T.);
#52328=EDGE_CURVE('',#40719,#40720,#33306,.T.);
#52329=EDGE_CURVE('',#40720,#40721,#4823,.T.);
#52330=EDGE_CURVE('',#40721,#40722,#22125,.T.);
#52331=EDGE_CURVE('',#40722,#40723,#33307,.T.);
#52332=EDGE_CURVE('',#40723,#40724,#22126,.T.);
#52333=EDGE_CURVE('',#40724,#40432,#4824,.T.);
#52334=EDGE_CURVE('',#40433,#40725,#4825,.T.);
#52335=EDGE_CURVE('',#40725,#40726,#22127,.T.);
#52336=EDGE_CURVE('',#40726,#40727,#33308,.T.);
#52337=EDGE_CURVE('',#40727,#40728,#22128,.T.);
#52338=EDGE_CURVE('',#40728,#40729,#4826,.T.);
#52339=EDGE_CURVE('',#40729,#40730,#33309,.T.);
#52340=EDGE_CURVE('',#40730,#40731,#4827,.T.);
#52341=EDGE_CURVE('',#40731,#40732,#22129,.T.);
#52342=EDGE_CURVE('',#40732,#40733,#33310,.T.);
#52343=EDGE_CURVE('',#40733,#40734,#22130,.T.);
#52344=EDGE_CURVE('',#40734,#40735,#4828,.T.);
#52345=EDGE_CURVE('',#40735,#40736,#33311,.T.);
#52346=EDGE_CURVE('',#40736,#40737,#4829,.T.);
#52347=EDGE_CURVE('',#40737,#40738,#22131,.T.);
#52348=EDGE_CURVE('',#40738,#40739,#33312,.T.);
#52349=EDGE_CURVE('',#40739,#40740,#22132,.T.);
#52350=EDGE_CURVE('',#40740,#40741,#4830,.T.);
#52351=EDGE_CURVE('',#40741,#40742,#33313,.T.);
#52352=EDGE_CURVE('',#40742,#40743,#4831,.T.);
#52353=EDGE_CURVE('',#40743,#40744,#22133,.T.);
#52354=EDGE_CURVE('',#40744,#40745,#33314,.T.);
#52355=EDGE_CURVE('',#40745,#40746,#22134,.T.);
#52356=EDGE_CURVE('',#40746,#40747,#4832,.T.);
#52357=EDGE_CURVE('',#40747,#40748,#33315,.T.);
#52358=EDGE_CURVE('',#40748,#40749,#4833,.T.);
#52359=EDGE_CURVE('',#40749,#40750,#22135,.T.);
#52360=EDGE_CURVE('',#40750,#40751,#33316,.T.);
#52361=EDGE_CURVE('',#40751,#40752,#22136,.T.);
#52362=EDGE_CURVE('',#40752,#40753,#4834,.T.);
#52363=EDGE_CURVE('',#40753,#40754,#33317,.T.);
#52364=EDGE_CURVE('',#40754,#40755,#4835,.T.);
#52365=EDGE_CURVE('',#40755,#40756,#22137,.T.);
#52366=EDGE_CURVE('',#40756,#40757,#33318,.T.);
#52367=EDGE_CURVE('',#40757,#40758,#22138,.T.);
#52368=EDGE_CURVE('',#40758,#40759,#4836,.T.);
#52369=EDGE_CURVE('',#40759,#40760,#33319,.T.);
#52370=EDGE_CURVE('',#40760,#40761,#4837,.T.);
#52371=EDGE_CURVE('',#40761,#40762,#22139,.T.);
#52372=EDGE_CURVE('',#40762,#40763,#33320,.T.);
#52373=EDGE_CURVE('',#40763,#40764,#22140,.T.);
#52374=EDGE_CURVE('',#40764,#40765,#4838,.T.);
#52375=EDGE_CURVE('',#40765,#40766,#33321,.T.);
#52376=EDGE_CURVE('',#40766,#40767,#4839,.T.);
#52377=EDGE_CURVE('',#40767,#40768,#22141,.T.);
#52378=EDGE_CURVE('',#40768,#40769,#33322,.T.);
#52379=EDGE_CURVE('',#40769,#40770,#22142,.T.);
#52380=EDGE_CURVE('',#40770,#40771,#4840,.T.);
#52381=EDGE_CURVE('',#40771,#40772,#33323,.T.);
#52382=EDGE_CURVE('',#40772,#40773,#4841,.T.);
#52383=EDGE_CURVE('',#40773,#40774,#22143,.T.);
#52384=EDGE_CURVE('',#40774,#40775,#33324,.T.);
#52385=EDGE_CURVE('',#40775,#40776,#22144,.T.);
#52386=EDGE_CURVE('',#40776,#40777,#4842,.T.);
#52387=EDGE_CURVE('',#40777,#40778,#33325,.T.);
#52388=EDGE_CURVE('',#40778,#40779,#4843,.T.);
#52389=EDGE_CURVE('',#40779,#40780,#22145,.T.);
#52390=EDGE_CURVE('',#40780,#40781,#33326,.T.);
#52391=EDGE_CURVE('',#40781,#40782,#22146,.T.);
#52392=EDGE_CURVE('',#40782,#40783,#4844,.T.);
#52393=EDGE_CURVE('',#40783,#40784,#33327,.T.);
#52394=EDGE_CURVE('',#40784,#40785,#4845,.T.);
#52395=EDGE_CURVE('',#40785,#40786,#22147,.T.);
#52396=EDGE_CURVE('',#40786,#40787,#33328,.T.);
#52397=EDGE_CURVE('',#40787,#40788,#22148,.T.);
#52398=EDGE_CURVE('',#40788,#40789,#4846,.T.);
#52399=EDGE_CURVE('',#40789,#40790,#33329,.T.);
#52400=EDGE_CURVE('',#40790,#40791,#4847,.T.);
#52401=EDGE_CURVE('',#40791,#40792,#22149,.T.);
#52402=EDGE_CURVE('',#40792,#40793,#33330,.T.);
#52403=EDGE_CURVE('',#40793,#40794,#22150,.T.);
#52404=EDGE_CURVE('',#40794,#40795,#4848,.T.);
#52405=EDGE_CURVE('',#40795,#40796,#33331,.T.);
#52406=EDGE_CURVE('',#40796,#40797,#4849,.T.);
#52407=EDGE_CURVE('',#40797,#40798,#22151,.T.);
#52408=EDGE_CURVE('',#40798,#40799,#33332,.T.);
#52409=EDGE_CURVE('',#40799,#40800,#22152,.T.);
#52410=EDGE_CURVE('',#40800,#40801,#4850,.T.);
#52411=EDGE_CURVE('',#40801,#40802,#33333,.T.);
#52412=EDGE_CURVE('',#40802,#40803,#4851,.T.);
#52413=EDGE_CURVE('',#40803,#40804,#22153,.T.);
#52414=EDGE_CURVE('',#40804,#40805,#33334,.T.);
#52415=EDGE_CURVE('',#40805,#40806,#22154,.T.);
#52416=EDGE_CURVE('',#40806,#40807,#4852,.T.);
#52417=EDGE_CURVE('',#40807,#40808,#33335,.T.);
#52418=EDGE_CURVE('',#40808,#40809,#4853,.T.);
#52419=EDGE_CURVE('',#40809,#40810,#22155,.T.);
#52420=EDGE_CURVE('',#40810,#40811,#33336,.T.);
#52421=EDGE_CURVE('',#40811,#40812,#22156,.T.);
#52422=EDGE_CURVE('',#40812,#40457,#4854,.T.);
#52423=EDGE_CURVE('',#40438,#40813,#4855,.T.);
#52424=EDGE_CURVE('',#40813,#40814,#22157,.T.);
#52425=EDGE_CURVE('',#40814,#40815,#33337,.T.);
#52426=EDGE_CURVE('',#40815,#40816,#22158,.T.);
#52427=EDGE_CURVE('',#40816,#40817,#4856,.T.);
#52428=EDGE_CURVE('',#40817,#40818,#33338,.T.);
#52429=EDGE_CURVE('',#40818,#40819,#4857,.T.);
#52430=EDGE_CURVE('',#40819,#40820,#22159,.T.);
#52431=EDGE_CURVE('',#40820,#40821,#33339,.T.);
#52432=EDGE_CURVE('',#40821,#40822,#22160,.T.);
#52433=EDGE_CURVE('',#40822,#40823,#4858,.T.);
#52434=EDGE_CURVE('',#40823,#40824,#33340,.T.);
#52435=EDGE_CURVE('',#40824,#40825,#4859,.T.);
#52436=EDGE_CURVE('',#40825,#40826,#22161,.T.);
#52437=EDGE_CURVE('',#40826,#40827,#33341,.T.);
#52438=EDGE_CURVE('',#40827,#40828,#22162,.T.);
#52439=EDGE_CURVE('',#40828,#40829,#4860,.T.);
#52440=EDGE_CURVE('',#40829,#40830,#33342,.T.);
#52441=EDGE_CURVE('',#40830,#40831,#4861,.T.);
#52442=EDGE_CURVE('',#40831,#40832,#22163,.T.);
#52443=EDGE_CURVE('',#40832,#40833,#33343,.T.);
#52444=EDGE_CURVE('',#40833,#40834,#22164,.T.);
#52445=EDGE_CURVE('',#40834,#40835,#4862,.T.);
#52446=EDGE_CURVE('',#40835,#40836,#33344,.T.);
#52447=EDGE_CURVE('',#40836,#40837,#4863,.T.);
#52448=EDGE_CURVE('',#40837,#40838,#22165,.T.);
#52449=EDGE_CURVE('',#40838,#40839,#33345,.T.);
#52450=EDGE_CURVE('',#40839,#40840,#22166,.T.);
#52451=EDGE_CURVE('',#40840,#40841,#4864,.T.);
#52452=EDGE_CURVE('',#40841,#40842,#33346,.T.);
#52453=EDGE_CURVE('',#40842,#40843,#4865,.T.);
#52454=EDGE_CURVE('',#40843,#40844,#22167,.T.);
#52455=EDGE_CURVE('',#40844,#40845,#33347,.T.);
#52456=EDGE_CURVE('',#40845,#40846,#22168,.T.);
#52457=EDGE_CURVE('',#40846,#40847,#4866,.T.);
#52458=EDGE_CURVE('',#40847,#40848,#33348,.T.);
#52459=EDGE_CURVE('',#40848,#40849,#4867,.T.);
#52460=EDGE_CURVE('',#40849,#40850,#22169,.T.);
#52461=EDGE_CURVE('',#40850,#40851,#33349,.T.);
#52462=EDGE_CURVE('',#40851,#40852,#22170,.T.);
#52463=EDGE_CURVE('',#40852,#40853,#4868,.T.);
#52464=EDGE_CURVE('',#40853,#40854,#33350,.T.);
#52465=EDGE_CURVE('',#40854,#40855,#4869,.T.);
#52466=EDGE_CURVE('',#40855,#40856,#22171,.T.);
#52467=EDGE_CURVE('',#40856,#40857,#33351,.T.);
#52468=EDGE_CURVE('',#40857,#40858,#22172,.T.);
#52469=EDGE_CURVE('',#40858,#40859,#4870,.T.);
#52470=EDGE_CURVE('',#40859,#40860,#33352,.T.);
#52471=EDGE_CURVE('',#40860,#40861,#4871,.T.);
#52472=EDGE_CURVE('',#40861,#40862,#22173,.T.);
#52473=EDGE_CURVE('',#40862,#40863,#33353,.T.);
#52474=EDGE_CURVE('',#40863,#40864,#22174,.T.);
#52475=EDGE_CURVE('',#40864,#40865,#4872,.T.);
#52476=EDGE_CURVE('',#40865,#40866,#33354,.T.);
#52477=EDGE_CURVE('',#40866,#40867,#4873,.T.);
#52478=EDGE_CURVE('',#40867,#40868,#22175,.T.);
#52479=EDGE_CURVE('',#40868,#40869,#33355,.T.);
#52480=EDGE_CURVE('',#40869,#40870,#22176,.T.);
#52481=EDGE_CURVE('',#40870,#40871,#4874,.T.);
#52482=EDGE_CURVE('',#40871,#40872,#33356,.T.);
#52483=EDGE_CURVE('',#40872,#40873,#4875,.T.);
#52484=EDGE_CURVE('',#40873,#40874,#22177,.T.);
#52485=EDGE_CURVE('',#40874,#40875,#33357,.T.);
#52486=EDGE_CURVE('',#40875,#40876,#22178,.T.);
#52487=EDGE_CURVE('',#40876,#40877,#4876,.T.);
#52488=EDGE_CURVE('',#40877,#40878,#33358,.T.);
#52489=EDGE_CURVE('',#40878,#40879,#4877,.T.);
#52490=EDGE_CURVE('',#40879,#40880,#22179,.T.);
#52491=EDGE_CURVE('',#40880,#40881,#33359,.T.);
#52492=EDGE_CURVE('',#40881,#40882,#22180,.T.);
#52493=EDGE_CURVE('',#40882,#40883,#4878,.T.);
#52494=EDGE_CURVE('',#40883,#40884,#33360,.T.);
#52495=EDGE_CURVE('',#40884,#40885,#4879,.T.);
#52496=EDGE_CURVE('',#40885,#40886,#22181,.T.);
#52497=EDGE_CURVE('',#40886,#40887,#33361,.T.);
#52498=EDGE_CURVE('',#40887,#40888,#22182,.T.);
#52499=EDGE_CURVE('',#40888,#40889,#4880,.T.);
#52500=EDGE_CURVE('',#40889,#40890,#33362,.T.);
#52501=EDGE_CURVE('',#40890,#40891,#4881,.T.);
#52502=EDGE_CURVE('',#40891,#40892,#22183,.T.);
#52503=EDGE_CURVE('',#40892,#40893,#33363,.T.);
#52504=EDGE_CURVE('',#40893,#40894,#22184,.T.);
#52505=EDGE_CURVE('',#40894,#40895,#4882,.T.);
#52506=EDGE_CURVE('',#40895,#40896,#33364,.T.);
#52507=EDGE_CURVE('',#40896,#40897,#4883,.T.);
#52508=EDGE_CURVE('',#40897,#40898,#22185,.T.);
#52509=EDGE_CURVE('',#40898,#40899,#33365,.T.);
#52510=EDGE_CURVE('',#40899,#40900,#22186,.T.);
#52511=EDGE_CURVE('',#40900,#40901,#4884,.T.);
#52512=EDGE_CURVE('',#40901,#40902,#33366,.T.);
#52513=EDGE_CURVE('',#40902,#40903,#4885,.T.);
#52514=EDGE_CURVE('',#40903,#40904,#22187,.T.);
#52515=EDGE_CURVE('',#40904,#40905,#33367,.T.);
#52516=EDGE_CURVE('',#40905,#40906,#22188,.T.);
#52517=EDGE_CURVE('',#40906,#40907,#4886,.T.);
#52518=EDGE_CURVE('',#40907,#40908,#33368,.T.);
#52519=EDGE_CURVE('',#40908,#40909,#4887,.T.);
#52520=EDGE_CURVE('',#40909,#40910,#22189,.T.);
#52521=EDGE_CURVE('',#40910,#40911,#33369,.T.);
#52522=EDGE_CURVE('',#40911,#40912,#22190,.T.);
#52523=EDGE_CURVE('',#40912,#40913,#4888,.T.);
#52524=EDGE_CURVE('',#40913,#40914,#33370,.T.);
#52525=EDGE_CURVE('',#40914,#40915,#4889,.T.);
#52526=EDGE_CURVE('',#40915,#40916,#22191,.T.);
#52527=EDGE_CURVE('',#40916,#40917,#33371,.T.);
#52528=EDGE_CURVE('',#40917,#40918,#22192,.T.);
#52529=EDGE_CURVE('',#40918,#40919,#4890,.T.);
#52530=EDGE_CURVE('',#40919,#40920,#33372,.T.);
#52531=EDGE_CURVE('',#40920,#40921,#4891,.T.);
#52532=EDGE_CURVE('',#40921,#40922,#22193,.T.);
#52533=EDGE_CURVE('',#40922,#40923,#33373,.T.);
#52534=EDGE_CURVE('',#40923,#40924,#22194,.T.);
#52535=EDGE_CURVE('',#40924,#40925,#4892,.T.);
#52536=EDGE_CURVE('',#40925,#40926,#33374,.T.);
#52537=EDGE_CURVE('',#40926,#40927,#4893,.T.);
#52538=EDGE_CURVE('',#40927,#40928,#22195,.T.);
#52539=EDGE_CURVE('',#40928,#40929,#33375,.T.);
#52540=EDGE_CURVE('',#40929,#40930,#22196,.T.);
#52541=EDGE_CURVE('',#40930,#40931,#4894,.T.);
#52542=EDGE_CURVE('',#40931,#40932,#33376,.T.);
#52543=EDGE_CURVE('',#40932,#40933,#4895,.T.);
#52544=EDGE_CURVE('',#40933,#40934,#22197,.T.);
#52545=EDGE_CURVE('',#40934,#40935,#33377,.T.);
#52546=EDGE_CURVE('',#40935,#40936,#22198,.T.);
#52547=EDGE_CURVE('',#40936,#40937,#4896,.T.);
#52548=EDGE_CURVE('',#40937,#40938,#33378,.T.);
#52549=EDGE_CURVE('',#40938,#40939,#4897,.T.);
#52550=EDGE_CURVE('',#40939,#40940,#22199,.T.);
#52551=EDGE_CURVE('',#40940,#40941,#33379,.T.);
#52552=EDGE_CURVE('',#40941,#40942,#22200,.T.);
#52553=EDGE_CURVE('',#40942,#40943,#4898,.T.);
#52554=EDGE_CURVE('',#40943,#40944,#33380,.T.);
#52555=EDGE_CURVE('',#40944,#40945,#4899,.T.);
#52556=EDGE_CURVE('',#40945,#40946,#22201,.T.);
#52557=EDGE_CURVE('',#40946,#40947,#33381,.T.);
#52558=EDGE_CURVE('',#40947,#40948,#22202,.T.);
#52559=EDGE_CURVE('',#40948,#40949,#4900,.T.);
#52560=EDGE_CURVE('',#40949,#40950,#33382,.T.);
#52561=EDGE_CURVE('',#40950,#40951,#4901,.T.);
#52562=EDGE_CURVE('',#40951,#40952,#22203,.T.);
#52563=EDGE_CURVE('',#40952,#40953,#33383,.T.);
#52564=EDGE_CURVE('',#40953,#40954,#22204,.T.);
#52565=EDGE_CURVE('',#40954,#40955,#4902,.T.);
#52566=EDGE_CURVE('',#40955,#40956,#33384,.T.);
#52567=EDGE_CURVE('',#40956,#40957,#4903,.T.);
#52568=EDGE_CURVE('',#40957,#40958,#22205,.T.);
#52569=EDGE_CURVE('',#40958,#40959,#33385,.T.);
#52570=EDGE_CURVE('',#40959,#40960,#22206,.T.);
#52571=EDGE_CURVE('',#40960,#40961,#4904,.T.);
#52572=EDGE_CURVE('',#40961,#40962,#33386,.T.);
#52573=EDGE_CURVE('',#40962,#40963,#4905,.T.);
#52574=EDGE_CURVE('',#40963,#40964,#22207,.T.);
#52575=EDGE_CURVE('',#40964,#40965,#33387,.T.);
#52576=EDGE_CURVE('',#40965,#40966,#22208,.T.);
#52577=EDGE_CURVE('',#40966,#40967,#4906,.T.);
#52578=EDGE_CURVE('',#40967,#40968,#33388,.T.);
#52579=EDGE_CURVE('',#40968,#40969,#4907,.T.);
#52580=EDGE_CURVE('',#40969,#40970,#22209,.T.);
#52581=EDGE_CURVE('',#40970,#40971,#33389,.T.);
#52582=EDGE_CURVE('',#40971,#40972,#22210,.T.);
#52583=EDGE_CURVE('',#40972,#40973,#4908,.T.);
#52584=EDGE_CURVE('',#40973,#40974,#33390,.T.);
#52585=EDGE_CURVE('',#40974,#40975,#4909,.T.);
#52586=EDGE_CURVE('',#40975,#40976,#22211,.T.);
#52587=EDGE_CURVE('',#40976,#40977,#33391,.T.);
#52588=EDGE_CURVE('',#40977,#40978,#22212,.T.);
#52589=EDGE_CURVE('',#40978,#40979,#4910,.T.);
#52590=EDGE_CURVE('',#40979,#40980,#33392,.T.);
#52591=EDGE_CURVE('',#40980,#40981,#4911,.T.);
#52592=EDGE_CURVE('',#40981,#40982,#22213,.T.);
#52593=EDGE_CURVE('',#40982,#40983,#33393,.T.);
#52594=EDGE_CURVE('',#40983,#40984,#22214,.T.);
#52595=EDGE_CURVE('',#40984,#40985,#4912,.T.);
#52596=EDGE_CURVE('',#40985,#40986,#33394,.T.);
#52597=EDGE_CURVE('',#40986,#40987,#4913,.T.);
#52598=EDGE_CURVE('',#40987,#40988,#22215,.T.);
#52599=EDGE_CURVE('',#40988,#40989,#33395,.T.);
#52600=EDGE_CURVE('',#40989,#40990,#22216,.T.);
#52601=EDGE_CURVE('',#40990,#40991,#4914,.T.);
#52602=EDGE_CURVE('',#40991,#40992,#33396,.T.);
#52603=EDGE_CURVE('',#40992,#40448,#22217,.T.);
#52604=EDGE_CURVE('',#40992,#40993,#33397,.T.);
#52605=EDGE_CURVE('',#40993,#40994,#4915,.T.);
#52606=EDGE_CURVE('',#40994,#40995,#22218,.T.);
#52607=EDGE_CURVE('',#40995,#40996,#33398,.T.);
#52608=EDGE_CURVE('',#40996,#40997,#22219,.T.);
#52609=EDGE_CURVE('',#40997,#40998,#4916,.T.);
#52610=EDGE_CURVE('',#40998,#40999,#33399,.T.);
#52611=EDGE_CURVE('',#40999,#41000,#4917,.T.);
#52612=EDGE_CURVE('',#41000,#41001,#22220,.T.);
#52613=EDGE_CURVE('',#41001,#41002,#33400,.T.);
#52614=EDGE_CURVE('',#41002,#41003,#22221,.T.);
#52615=EDGE_CURVE('',#41003,#41004,#4918,.T.);
#52616=EDGE_CURVE('',#41004,#41005,#33401,.T.);
#52617=EDGE_CURVE('',#41005,#41006,#4919,.T.);
#52618=EDGE_CURVE('',#41006,#41007,#22222,.T.);
#52619=EDGE_CURVE('',#41007,#41008,#33402,.T.);
#52620=EDGE_CURVE('',#41008,#41009,#22223,.T.);
#52621=EDGE_CURVE('',#41009,#41010,#4920,.T.);
#52622=EDGE_CURVE('',#41010,#41011,#33403,.T.);
#52623=EDGE_CURVE('',#41011,#41012,#4921,.T.);
#52624=EDGE_CURVE('',#41012,#41013,#22224,.T.);
#52625=EDGE_CURVE('',#41013,#41014,#33404,.T.);
#52626=EDGE_CURVE('',#41014,#41015,#22225,.T.);
#52627=EDGE_CURVE('',#41015,#41016,#4922,.T.);
#52628=EDGE_CURVE('',#41016,#41017,#33405,.T.);
#52629=EDGE_CURVE('',#41017,#41018,#4923,.T.);
#52630=EDGE_CURVE('',#41018,#41019,#22226,.T.);
#52631=EDGE_CURVE('',#41019,#41020,#33406,.T.);
#52632=EDGE_CURVE('',#41020,#41021,#22227,.T.);
#52633=EDGE_CURVE('',#41021,#41022,#4924,.T.);
#52634=EDGE_CURVE('',#41022,#41023,#33407,.T.);
#52635=EDGE_CURVE('',#41023,#41024,#4925,.T.);
#52636=EDGE_CURVE('',#41024,#41025,#22228,.T.);
#52637=EDGE_CURVE('',#41025,#41026,#33408,.T.);
#52638=EDGE_CURVE('',#41026,#41027,#22229,.T.);
#52639=EDGE_CURVE('',#41027,#41028,#4926,.T.);
#52640=EDGE_CURVE('',#41028,#41029,#33409,.T.);
#52641=EDGE_CURVE('',#41029,#41030,#4927,.T.);
#52642=EDGE_CURVE('',#41030,#41031,#22230,.T.);
#52643=EDGE_CURVE('',#41031,#41032,#33410,.T.);
#52644=EDGE_CURVE('',#41032,#41033,#22231,.T.);
#52645=EDGE_CURVE('',#41033,#41034,#4928,.T.);
#52646=EDGE_CURVE('',#41034,#41035,#33411,.T.);
#52647=EDGE_CURVE('',#41035,#41036,#4929,.T.);
#52648=EDGE_CURVE('',#41036,#41037,#22232,.T.);
#52649=EDGE_CURVE('',#41037,#41038,#33412,.T.);
#52650=EDGE_CURVE('',#41038,#41039,#22233,.T.);
#52651=EDGE_CURVE('',#41039,#41040,#4930,.T.);
#52652=EDGE_CURVE('',#41040,#41041,#33413,.T.);
#52653=EDGE_CURVE('',#41041,#41042,#4931,.T.);
#52654=EDGE_CURVE('',#41042,#41043,#22234,.T.);
#52655=EDGE_CURVE('',#41043,#41044,#33414,.T.);
#52656=EDGE_CURVE('',#41044,#41045,#22235,.T.);
#52657=EDGE_CURVE('',#41045,#41046,#4932,.T.);
#52658=EDGE_CURVE('',#41046,#41047,#33415,.T.);
#52659=EDGE_CURVE('',#41047,#41048,#4933,.T.);
#52660=EDGE_CURVE('',#41048,#41049,#22236,.T.);
#52661=EDGE_CURVE('',#41049,#41050,#33416,.T.);
#52662=EDGE_CURVE('',#41050,#41051,#22237,.T.);
#52663=EDGE_CURVE('',#41051,#41052,#4934,.T.);
#52664=EDGE_CURVE('',#41052,#41053,#33417,.T.);
#52665=EDGE_CURVE('',#41053,#41054,#4935,.T.);
#52666=EDGE_CURVE('',#41054,#41055,#22238,.T.);
#52667=EDGE_CURVE('',#41055,#41056,#33418,.T.);
#52668=EDGE_CURVE('',#41056,#41057,#22239,.T.);
#52669=EDGE_CURVE('',#41057,#41058,#4936,.T.);
#52670=EDGE_CURVE('',#41058,#41059,#33419,.T.);
#52671=EDGE_CURVE('',#41059,#41060,#4937,.T.);
#52672=EDGE_CURVE('',#41060,#41061,#22240,.T.);
#52673=EDGE_CURVE('',#41061,#41062,#33420,.T.);
#52674=EDGE_CURVE('',#41062,#41063,#22241,.T.);
#52675=EDGE_CURVE('',#41063,#41064,#4938,.T.);
#52676=EDGE_CURVE('',#41064,#41065,#33421,.T.);
#52677=EDGE_CURVE('',#41065,#41066,#4939,.T.);
#52678=EDGE_CURVE('',#41066,#41067,#22242,.T.);
#52679=EDGE_CURVE('',#41067,#41068,#33422,.T.);
#52680=EDGE_CURVE('',#41068,#41069,#22243,.T.);
#52681=EDGE_CURVE('',#41069,#41070,#4940,.T.);
#52682=EDGE_CURVE('',#41070,#41071,#33423,.T.);
#52683=EDGE_CURVE('',#41071,#41072,#4941,.T.);
#52684=EDGE_CURVE('',#41072,#41073,#22244,.T.);
#52685=EDGE_CURVE('',#41073,#41074,#33424,.T.);
#52686=EDGE_CURVE('',#41074,#41075,#22245,.T.);
#52687=EDGE_CURVE('',#41075,#41076,#4942,.T.);
#52688=EDGE_CURVE('',#41076,#41077,#33425,.T.);
#52689=EDGE_CURVE('',#41077,#41078,#4943,.T.);
#52690=EDGE_CURVE('',#41078,#41079,#22246,.T.);
#52691=EDGE_CURVE('',#41079,#41080,#33426,.T.);
#52692=EDGE_CURVE('',#41080,#41081,#22247,.T.);
#52693=EDGE_CURVE('',#41081,#40431,#4944,.T.);
#52694=EDGE_CURVE('',#40430,#41082,#4945,.T.);
#52695=EDGE_CURVE('',#41082,#41083,#22248,.T.);
#52696=EDGE_CURVE('',#41083,#41084,#33427,.T.);
#52697=EDGE_CURVE('',#41084,#41085,#22249,.T.);
#52698=EDGE_CURVE('',#41085,#41086,#4946,.T.);
#52699=EDGE_CURVE('',#41086,#41087,#33428,.T.);
#52700=EDGE_CURVE('',#41087,#41088,#4947,.T.);
#52701=EDGE_CURVE('',#41088,#41089,#22250,.T.);
#52702=EDGE_CURVE('',#41089,#41090,#33429,.T.);
#52703=EDGE_CURVE('',#41090,#41091,#22251,.T.);
#52704=EDGE_CURVE('',#41091,#41092,#4948,.T.);
#52705=EDGE_CURVE('',#41092,#41093,#33430,.T.);
#52706=EDGE_CURVE('',#41093,#41094,#4949,.T.);
#52707=EDGE_CURVE('',#41094,#41095,#22252,.T.);
#52708=EDGE_CURVE('',#41095,#41096,#33431,.T.);
#52709=EDGE_CURVE('',#41096,#41097,#22253,.T.);
#52710=EDGE_CURVE('',#41097,#41098,#4950,.T.);
#52711=EDGE_CURVE('',#41098,#41099,#33432,.T.);
#52712=EDGE_CURVE('',#41099,#41100,#4951,.T.);
#52713=EDGE_CURVE('',#41100,#41101,#22254,.T.);
#52714=EDGE_CURVE('',#41101,#41102,#33433,.T.);
#52715=EDGE_CURVE('',#41102,#41103,#22255,.T.);
#52716=EDGE_CURVE('',#41103,#41104,#4952,.T.);
#52717=EDGE_CURVE('',#41104,#41105,#33434,.T.);
#52718=EDGE_CURVE('',#41105,#41106,#4953,.T.);
#52719=EDGE_CURVE('',#41106,#41107,#22256,.T.);
#52720=EDGE_CURVE('',#41107,#41108,#33435,.T.);
#52721=EDGE_CURVE('',#41108,#41109,#22257,.T.);
#52722=EDGE_CURVE('',#41109,#41110,#4954,.T.);
#52723=EDGE_CURVE('',#41110,#41111,#33436,.T.);
#52724=EDGE_CURVE('',#41111,#41112,#4955,.T.);
#52725=EDGE_CURVE('',#41112,#41113,#22258,.T.);
#52726=EDGE_CURVE('',#41113,#41114,#33437,.T.);
#52727=EDGE_CURVE('',#41114,#41115,#22259,.T.);
#52728=EDGE_CURVE('',#41115,#41116,#4956,.T.);
#52729=EDGE_CURVE('',#41116,#41117,#33438,.T.);
#52730=EDGE_CURVE('',#41117,#41118,#4957,.T.);
#52731=EDGE_CURVE('',#41118,#41119,#22260,.T.);
#52732=EDGE_CURVE('',#41119,#41120,#33439,.T.);
#52733=EDGE_CURVE('',#41120,#41121,#22261,.T.);
#52734=EDGE_CURVE('',#41121,#41122,#4958,.T.);
#52735=EDGE_CURVE('',#41122,#41123,#33440,.T.);
#52736=EDGE_CURVE('',#41123,#41124,#4959,.T.);
#52737=EDGE_CURVE('',#41124,#41125,#22262,.T.);
#52738=EDGE_CURVE('',#41125,#41126,#33441,.T.);
#52739=EDGE_CURVE('',#41126,#41127,#22263,.T.);
#52740=EDGE_CURVE('',#41127,#41128,#4960,.T.);
#52741=EDGE_CURVE('',#41128,#41129,#33442,.T.);
#52742=EDGE_CURVE('',#41129,#41130,#4961,.T.);
#52743=EDGE_CURVE('',#41130,#41131,#22264,.T.);
#52744=EDGE_CURVE('',#41131,#41132,#33443,.T.);
#52745=EDGE_CURVE('',#41132,#41133,#22265,.T.);
#52746=EDGE_CURVE('',#41133,#41134,#4962,.T.);
#52747=EDGE_CURVE('',#41134,#41135,#33444,.T.);
#52748=EDGE_CURVE('',#41135,#41136,#4963,.T.);
#52749=EDGE_CURVE('',#41136,#41137,#22266,.T.);
#52750=EDGE_CURVE('',#41137,#41138,#33445,.T.);
#52751=EDGE_CURVE('',#41138,#41139,#22267,.T.);
#52752=EDGE_CURVE('',#41139,#41140,#4964,.T.);
#52753=EDGE_CURVE('',#41140,#41141,#33446,.T.);
#52754=EDGE_CURVE('',#41141,#41142,#4965,.T.);
#52755=EDGE_CURVE('',#41142,#41143,#22268,.T.);
#52756=EDGE_CURVE('',#41143,#41144,#33447,.T.);
#52757=EDGE_CURVE('',#41144,#41145,#22269,.T.);
#52758=EDGE_CURVE('',#41145,#41146,#4966,.T.);
#52759=EDGE_CURVE('',#41146,#41147,#33448,.T.);
#52760=EDGE_CURVE('',#41147,#41148,#4967,.T.);
#52761=EDGE_CURVE('',#41148,#41149,#22270,.T.);
#52762=EDGE_CURVE('',#41149,#41150,#33449,.T.);
#52763=EDGE_CURVE('',#41150,#41151,#22271,.T.);
#52764=EDGE_CURVE('',#41151,#41152,#4968,.T.);
#52765=EDGE_CURVE('',#41152,#41153,#33450,.T.);
#52766=EDGE_CURVE('',#41153,#41154,#4969,.T.);
#52767=EDGE_CURVE('',#41154,#41155,#22272,.T.);
#52768=EDGE_CURVE('',#41155,#41156,#33451,.T.);
#52769=EDGE_CURVE('',#41156,#41157,#22273,.T.);
#52770=EDGE_CURVE('',#41157,#41158,#4970,.T.);
#52771=EDGE_CURVE('',#41158,#41159,#33452,.T.);
#52772=EDGE_CURVE('',#41159,#41160,#4971,.T.);
#52773=EDGE_CURVE('',#41160,#41161,#22274,.T.);
#52774=EDGE_CURVE('',#41161,#41162,#33453,.T.);
#52775=EDGE_CURVE('',#41162,#41163,#22275,.T.);
#52776=EDGE_CURVE('',#41163,#41164,#4972,.T.);
#52777=EDGE_CURVE('',#41164,#41165,#33454,.T.);
#52778=EDGE_CURVE('',#41165,#41166,#4973,.T.);
#52779=EDGE_CURVE('',#41166,#41167,#22276,.T.);
#52780=EDGE_CURVE('',#41167,#41168,#33455,.T.);
#52781=EDGE_CURVE('',#41168,#41169,#22277,.T.);
#52782=EDGE_CURVE('',#41169,#40439,#4974,.T.);
#52783=EDGE_CURVE('',#41170,#41171,#33456,.T.);
#52784=EDGE_CURVE('',#41171,#40447,#22278,.T.);
#52785=EDGE_CURVE('',#41171,#41170,#33457,.T.);
#52786=EDGE_CURVE('',#41170,#41172,#22279,.T.);
#52787=EDGE_CURVE('',#41172,#41172,#33458,.T.);
#52788=EDGE_CURVE('',#41173,#41174,#33459,.T.);
#52789=EDGE_CURVE('',#41173,#41175,#22280,.T.);
#52790=EDGE_CURVE('',#41175,#41176,#33460,.T.);
#52791=EDGE_CURVE('',#41176,#41177,#22281,.T.);
#52792=EDGE_CURVE('',#41178,#41177,#33461,.T.);
#52793=EDGE_CURVE('',#41174,#41178,#33462,.T.);
#52794=EDGE_CURVE('',#41179,#41180,#33463,.T.);
#52795=EDGE_CURVE('',#41180,#41174,#22282,.T.);
#52796=EDGE_CURVE('',#41178,#41179,#22283,.T.);
#52797=EDGE_CURVE('',#41181,#41182,#33464,.T.);
#52798=EDGE_CURVE('',#41182,#41183,#22284,.T.);
#52799=EDGE_CURVE('',#41183,#41184,#33465,.T.);
#52800=EDGE_CURVE('',#41184,#41181,#22285,.T.);
#52801=EDGE_CURVE('',#41185,#41186,#33466,.T.);
#52802=EDGE_CURVE('',#41185,#41187,#22286,.T.);
#52803=EDGE_CURVE('',#41187,#41188,#33467,.T.);
#52804=EDGE_CURVE('',#41188,#41189,#22287,.T.);
#52805=EDGE_CURVE('',#41190,#41189,#33468,.T.);
#52806=EDGE_CURVE('',#41186,#41190,#33469,.T.);
#52807=EDGE_CURVE('',#41191,#41192,#33470,.T.);
#52808=EDGE_CURVE('',#41192,#41186,#22288,.T.);
#52809=EDGE_CURVE('',#41190,#41191,#22289,.T.);
#52810=EDGE_CURVE('',#41175,#40996,#33471,.T.);
#52811=EDGE_CURVE('',#40995,#41176,#33472,.T.);
#52812=EDGE_CURVE('',#40810,#41192,#1418,.T.);
#52813=EDGE_CURVE('',#41191,#40811,#1419,.T.);
#52814=EDGE_CURVE('',#41187,#41182,#1420,.T.);
#52815=EDGE_CURVE('',#41181,#41188,#1421,.T.);
#52816=EDGE_CURVE('',#41183,#41180,#1422,.T.);
#52817=EDGE_CURVE('',#41179,#41184,#1423,.T.);
#52818=EDGE_CURVE('',#41193,#41194,#33473,.T.);
#52819=EDGE_CURVE('',#41194,#41195,#22290,.T.);
#52820=EDGE_CURVE('',#41196,#41195,#33474,.T.);
#52821=EDGE_CURVE('',#41197,#41196,#33475,.T.);
#52822=EDGE_CURVE('',#41198,#41197,#33476,.T.);
#52823=EDGE_CURVE('',#41198,#41193,#22291,.T.);
#52824=EDGE_CURVE('',#41196,#41199,#22292,.T.);
#52825=EDGE_CURVE('',#41199,#41200,#33477,.T.);
#52826=EDGE_CURVE('',#41200,#41197,#22293,.T.);
#52827=EDGE_CURVE('',#41201,#41202,#33478,.T.);
#52828=EDGE_CURVE('',#41202,#41203,#22294,.T.);
#52829=EDGE_CURVE('',#41203,#41204,#33479,.T.);
#52830=EDGE_CURVE('',#41204,#41201,#22295,.T.);
#52831=EDGE_CURVE('',#41205,#41206,#33480,.T.);
#52832=EDGE_CURVE('',#41206,#41207,#22296,.T.);
#52833=EDGE_CURVE('',#41208,#41207,#33481,.T.);
#52834=EDGE_CURVE('',#41209,#41208,#33482,.T.);
#52835=EDGE_CURVE('',#41210,#41209,#33483,.T.);
#52836=EDGE_CURVE('',#41210,#41205,#22297,.T.);
#52837=EDGE_CURVE('',#41208,#41211,#22298,.T.);
#52838=EDGE_CURVE('',#41211,#41212,#33484,.T.);
#52839=EDGE_CURVE('',#41212,#41209,#22299,.T.);
#52840=EDGE_CURVE('',#41001,#41194,#33485,.T.);
#52841=EDGE_CURVE('',#41193,#41002,#33486,.T.);
#52842=EDGE_CURVE('',#41211,#40805,#1424,.T.);
#52843=EDGE_CURVE('',#40804,#41212,#1425,.T.);
#52844=EDGE_CURVE('',#41203,#41206,#1426,.T.);
#52845=EDGE_CURVE('',#41205,#41204,#1427,.T.);
#52846=EDGE_CURVE('',#41199,#41202,#1428,.T.);
#52847=EDGE_CURVE('',#41201,#41200,#1429,.T.);
#52848=EDGE_CURVE('',#41213,#41214,#33487,.T.);
#52849=EDGE_CURVE('',#41214,#41215,#22300,.T.);
#52850=EDGE_CURVE('',#41216,#41215,#33488,.T.);
#52851=EDGE_CURVE('',#41217,#41216,#33489,.T.);
#52852=EDGE_CURVE('',#41218,#41217,#33490,.T.);
#52853=EDGE_CURVE('',#41218,#41213,#22301,.T.);
#52854=EDGE_CURVE('',#41216,#41219,#22302,.T.);
#52855=EDGE_CURVE('',#41219,#41220,#33491,.T.);
#52856=EDGE_CURVE('',#41220,#41217,#22303,.T.);
#52857=EDGE_CURVE('',#41221,#41222,#33492,.T.);
#52858=EDGE_CURVE('',#41222,#41223,#22304,.T.);
#52859=EDGE_CURVE('',#41223,#41224,#33493,.T.);
#52860=EDGE_CURVE('',#41224,#41221,#22305,.T.);
#52861=EDGE_CURVE('',#41225,#41226,#33494,.T.);
#52862=EDGE_CURVE('',#41226,#41227,#22306,.T.);
#52863=EDGE_CURVE('',#41228,#41227,#33495,.T.);
#52864=EDGE_CURVE('',#41229,#41228,#33496,.T.);
#52865=EDGE_CURVE('',#41230,#41229,#33497,.T.);
#52866=EDGE_CURVE('',#41230,#41225,#22307,.T.);
#52867=EDGE_CURVE('',#41228,#41231,#22308,.T.);
#52868=EDGE_CURVE('',#41231,#41232,#33498,.T.);
#52869=EDGE_CURVE('',#41232,#41229,#22309,.T.);
#52870=EDGE_CURVE('',#41007,#41214,#33499,.T.);
#52871=EDGE_CURVE('',#41213,#41008,#33500,.T.);
#52872=EDGE_CURVE('',#41231,#40799,#1430,.T.);
#52873=EDGE_CURVE('',#40798,#41232,#1431,.T.);
#52874=EDGE_CURVE('',#41223,#41226,#1432,.T.);
#52875=EDGE_CURVE('',#41225,#41224,#1433,.T.);
#52876=EDGE_CURVE('',#41219,#41222,#1434,.T.);
#52877=EDGE_CURVE('',#41221,#41220,#1435,.T.);
#52878=EDGE_CURVE('',#41233,#41234,#33501,.T.);
#52879=EDGE_CURVE('',#41234,#41235,#22310,.T.);
#52880=EDGE_CURVE('',#41236,#41235,#33502,.T.);
#52881=EDGE_CURVE('',#41237,#41236,#33503,.T.);
#52882=EDGE_CURVE('',#41238,#41237,#33504,.T.);
#52883=EDGE_CURVE('',#41238,#41233,#22311,.T.);
#52884=EDGE_CURVE('',#41236,#41239,#22312,.T.);
#52885=EDGE_CURVE('',#41239,#41240,#33505,.T.);
#52886=EDGE_CURVE('',#41240,#41237,#22313,.T.);
#52887=EDGE_CURVE('',#41241,#41242,#33506,.T.);
#52888=EDGE_CURVE('',#41242,#41243,#22314,.T.);
#52889=EDGE_CURVE('',#41243,#41244,#33507,.T.);
#52890=EDGE_CURVE('',#41244,#41241,#22315,.T.);
#52891=EDGE_CURVE('',#41245,#41246,#33508,.T.);
#52892=EDGE_CURVE('',#41246,#41247,#22316,.T.);
#52893=EDGE_CURVE('',#41248,#41247,#33509,.T.);
#52894=EDGE_CURVE('',#41249,#41248,#33510,.T.);
#52895=EDGE_CURVE('',#41250,#41249,#33511,.T.);
#52896=EDGE_CURVE('',#41250,#41245,#22317,.T.);
#52897=EDGE_CURVE('',#41248,#41251,#22318,.T.);
#52898=EDGE_CURVE('',#41251,#41252,#33512,.T.);
#52899=EDGE_CURVE('',#41252,#41249,#22319,.T.);
#52900=EDGE_CURVE('',#41013,#41234,#33513,.T.);
#52901=EDGE_CURVE('',#41233,#41014,#33514,.T.);
#52902=EDGE_CURVE('',#41251,#40793,#1436,.T.);
#52903=EDGE_CURVE('',#40792,#41252,#1437,.T.);
#52904=EDGE_CURVE('',#41243,#41246,#1438,.T.);
#52905=EDGE_CURVE('',#41245,#41244,#1439,.T.);
#52906=EDGE_CURVE('',#41239,#41242,#1440,.T.);
#52907=EDGE_CURVE('',#41241,#41240,#1441,.T.);
#52908=EDGE_CURVE('',#41253,#41254,#33515,.T.);
#52909=EDGE_CURVE('',#41254,#41255,#22320,.T.);
#52910=EDGE_CURVE('',#41256,#41255,#33516,.T.);
#52911=EDGE_CURVE('',#41257,#41256,#33517,.T.);
#52912=EDGE_CURVE('',#41258,#41257,#33518,.T.);
#52913=EDGE_CURVE('',#41258,#41253,#22321,.T.);
#52914=EDGE_CURVE('',#41256,#41259,#22322,.T.);
#52915=EDGE_CURVE('',#41259,#41260,#33519,.T.);
#52916=EDGE_CURVE('',#41260,#41257,#22323,.T.);
#52917=EDGE_CURVE('',#41261,#41262,#33520,.T.);
#52918=EDGE_CURVE('',#41262,#41263,#22324,.T.);
#52919=EDGE_CURVE('',#41263,#41264,#33521,.T.);
#52920=EDGE_CURVE('',#41264,#41261,#22325,.T.);
#52921=EDGE_CURVE('',#41265,#41266,#33522,.T.);
#52922=EDGE_CURVE('',#41266,#41267,#22326,.T.);
#52923=EDGE_CURVE('',#41268,#41267,#33523,.T.);
#52924=EDGE_CURVE('',#41269,#41268,#33524,.T.);
#52925=EDGE_CURVE('',#41270,#41269,#33525,.T.);
#52926=EDGE_CURVE('',#41270,#41265,#22327,.T.);
#52927=EDGE_CURVE('',#41268,#41271,#22328,.T.);
#52928=EDGE_CURVE('',#41271,#41272,#33526,.T.);
#52929=EDGE_CURVE('',#41272,#41269,#22329,.T.);
#52930=EDGE_CURVE('',#41019,#41254,#33527,.T.);
#52931=EDGE_CURVE('',#41253,#41020,#33528,.T.);
#52932=EDGE_CURVE('',#41271,#40787,#1442,.T.);
#52933=EDGE_CURVE('',#40786,#41272,#1443,.T.);
#52934=EDGE_CURVE('',#41263,#41266,#1444,.T.);
#52935=EDGE_CURVE('',#41265,#41264,#1445,.T.);
#52936=EDGE_CURVE('',#41259,#41262,#1446,.T.);
#52937=EDGE_CURVE('',#41261,#41260,#1447,.T.);
#52938=EDGE_CURVE('',#41273,#41274,#33529,.T.);
#52939=EDGE_CURVE('',#41274,#41275,#22330,.T.);
#52940=EDGE_CURVE('',#41276,#41275,#33530,.T.);
#52941=EDGE_CURVE('',#41277,#41276,#33531,.T.);
#52942=EDGE_CURVE('',#41278,#41277,#33532,.T.);
#52943=EDGE_CURVE('',#41278,#41273,#22331,.T.);
#52944=EDGE_CURVE('',#41276,#41279,#22332,.T.);
#52945=EDGE_CURVE('',#41279,#41280,#33533,.T.);
#52946=EDGE_CURVE('',#41280,#41277,#22333,.T.);
#52947=EDGE_CURVE('',#41281,#41282,#33534,.T.);
#52948=EDGE_CURVE('',#41282,#41283,#22334,.T.);
#52949=EDGE_CURVE('',#41283,#41284,#33535,.T.);
#52950=EDGE_CURVE('',#41284,#41281,#22335,.T.);
#52951=EDGE_CURVE('',#41285,#41286,#33536,.T.);
#52952=EDGE_CURVE('',#41286,#41287,#22336,.T.);
#52953=EDGE_CURVE('',#41288,#41287,#33537,.T.);
#52954=EDGE_CURVE('',#41289,#41288,#33538,.T.);
#52955=EDGE_CURVE('',#41290,#41289,#33539,.T.);
#52956=EDGE_CURVE('',#41290,#41285,#22337,.T.);
#52957=EDGE_CURVE('',#41288,#41291,#22338,.T.);
#52958=EDGE_CURVE('',#41291,#41292,#33540,.T.);
#52959=EDGE_CURVE('',#41292,#41289,#22339,.T.);
#52960=EDGE_CURVE('',#41025,#41274,#33541,.T.);
#52961=EDGE_CURVE('',#41273,#41026,#33542,.T.);
#52962=EDGE_CURVE('',#41291,#40781,#1448,.T.);
#52963=EDGE_CURVE('',#40780,#41292,#1449,.T.);
#52964=EDGE_CURVE('',#41283,#41286,#1450,.T.);
#52965=EDGE_CURVE('',#41285,#41284,#1451,.T.);
#52966=EDGE_CURVE('',#41279,#41282,#1452,.T.);
#52967=EDGE_CURVE('',#41281,#41280,#1453,.T.);
#52968=EDGE_CURVE('',#41293,#41294,#33543,.T.);
#52969=EDGE_CURVE('',#41294,#41295,#22340,.T.);
#52970=EDGE_CURVE('',#41296,#41295,#33544,.T.);
#52971=EDGE_CURVE('',#41297,#41296,#33545,.T.);
#52972=EDGE_CURVE('',#41298,#41297,#33546,.T.);
#52973=EDGE_CURVE('',#41298,#41293,#22341,.T.);
#52974=EDGE_CURVE('',#41296,#41299,#22342,.T.);
#52975=EDGE_CURVE('',#41299,#41300,#33547,.T.);
#52976=EDGE_CURVE('',#41300,#41297,#22343,.T.);
#52977=EDGE_CURVE('',#41301,#41302,#33548,.T.);
#52978=EDGE_CURVE('',#41302,#41303,#22344,.T.);
#52979=EDGE_CURVE('',#41303,#41304,#33549,.T.);
#52980=EDGE_CURVE('',#41304,#41301,#22345,.T.);
#52981=EDGE_CURVE('',#41305,#41306,#33550,.T.);
#52982=EDGE_CURVE('',#41306,#41307,#22346,.T.);
#52983=EDGE_CURVE('',#41308,#41307,#33551,.T.);
#52984=EDGE_CURVE('',#41309,#41308,#33552,.T.);
#52985=EDGE_CURVE('',#41310,#41309,#33553,.T.);
#52986=EDGE_CURVE('',#41310,#41305,#22347,.T.);
#52987=EDGE_CURVE('',#41308,#41311,#22348,.T.);
#52988=EDGE_CURVE('',#41311,#41312,#33554,.T.);
#52989=EDGE_CURVE('',#41312,#41309,#22349,.T.);
#52990=EDGE_CURVE('',#41031,#41294,#33555,.T.);
#52991=EDGE_CURVE('',#41293,#41032,#33556,.T.);
#52992=EDGE_CURVE('',#41311,#40775,#1454,.T.);
#52993=EDGE_CURVE('',#40774,#41312,#1455,.T.);
#52994=EDGE_CURVE('',#41303,#41306,#1456,.T.);
#52995=EDGE_CURVE('',#41305,#41304,#1457,.T.);
#52996=EDGE_CURVE('',#41299,#41302,#1458,.T.);
#52997=EDGE_CURVE('',#41301,#41300,#1459,.T.);
#52998=EDGE_CURVE('',#41313,#41314,#33557,.T.);
#52999=EDGE_CURVE('',#41314,#41315,#22350,.T.);
#53000=EDGE_CURVE('',#41316,#41315,#33558,.T.);
#53001=EDGE_CURVE('',#41317,#41316,#33559,.T.);
#53002=EDGE_CURVE('',#41318,#41317,#33560,.T.);
#53003=EDGE_CURVE('',#41318,#41313,#22351,.T.);
#53004=EDGE_CURVE('',#41316,#41319,#22352,.T.);
#53005=EDGE_CURVE('',#41319,#41320,#33561,.T.);
#53006=EDGE_CURVE('',#41320,#41317,#22353,.T.);
#53007=EDGE_CURVE('',#41321,#41322,#33562,.T.);
#53008=EDGE_CURVE('',#41322,#41323,#22354,.T.);
#53009=EDGE_CURVE('',#41323,#41324,#33563,.T.);
#53010=EDGE_CURVE('',#41324,#41321,#22355,.T.);
#53011=EDGE_CURVE('',#41325,#41326,#33564,.T.);
#53012=EDGE_CURVE('',#41326,#41327,#22356,.T.);
#53013=EDGE_CURVE('',#41328,#41327,#33565,.T.);
#53014=EDGE_CURVE('',#41329,#41328,#33566,.T.);
#53015=EDGE_CURVE('',#41330,#41329,#33567,.T.);
#53016=EDGE_CURVE('',#41330,#41325,#22357,.T.);
#53017=EDGE_CURVE('',#41328,#41331,#22358,.T.);
#53018=EDGE_CURVE('',#41331,#41332,#33568,.T.);
#53019=EDGE_CURVE('',#41332,#41329,#22359,.T.);
#53020=EDGE_CURVE('',#41037,#41314,#33569,.T.);
#53021=EDGE_CURVE('',#41313,#41038,#33570,.T.);
#53022=EDGE_CURVE('',#41331,#40769,#1460,.T.);
#53023=EDGE_CURVE('',#40768,#41332,#1461,.T.);
#53024=EDGE_CURVE('',#41323,#41326,#1462,.T.);
#53025=EDGE_CURVE('',#41325,#41324,#1463,.T.);
#53026=EDGE_CURVE('',#41319,#41322,#1464,.T.);
#53027=EDGE_CURVE('',#41321,#41320,#1465,.T.);
#53028=EDGE_CURVE('',#41333,#41334,#33571,.T.);
#53029=EDGE_CURVE('',#41334,#41335,#22360,.T.);
#53030=EDGE_CURVE('',#41336,#41335,#33572,.T.);
#53031=EDGE_CURVE('',#41337,#41336,#33573,.T.);
#53032=EDGE_CURVE('',#41338,#41337,#33574,.T.);
#53033=EDGE_CURVE('',#41338,#41333,#22361,.T.);
#53034=EDGE_CURVE('',#41336,#41339,#22362,.T.);
#53035=EDGE_CURVE('',#41339,#41340,#33575,.T.);
#53036=EDGE_CURVE('',#41340,#41337,#22363,.T.);
#53037=EDGE_CURVE('',#41341,#41342,#33576,.T.);
#53038=EDGE_CURVE('',#41342,#41343,#22364,.T.);
#53039=EDGE_CURVE('',#41343,#41344,#33577,.T.);
#53040=EDGE_CURVE('',#41344,#41341,#22365,.T.);
#53041=EDGE_CURVE('',#41345,#41346,#33578,.T.);
#53042=EDGE_CURVE('',#41346,#41347,#22366,.T.);
#53043=EDGE_CURVE('',#41348,#41347,#33579,.T.);
#53044=EDGE_CURVE('',#41349,#41348,#33580,.T.);
#53045=EDGE_CURVE('',#41350,#41349,#33581,.T.);
#53046=EDGE_CURVE('',#41350,#41345,#22367,.T.);
#53047=EDGE_CURVE('',#41348,#41351,#22368,.T.);
#53048=EDGE_CURVE('',#41351,#41352,#33582,.T.);
#53049=EDGE_CURVE('',#41352,#41349,#22369,.T.);
#53050=EDGE_CURVE('',#41043,#41334,#33583,.T.);
#53051=EDGE_CURVE('',#41333,#41044,#33584,.T.);
#53052=EDGE_CURVE('',#41351,#40763,#1466,.T.);
#53053=EDGE_CURVE('',#40762,#41352,#1467,.T.);
#53054=EDGE_CURVE('',#41343,#41346,#1468,.T.);
#53055=EDGE_CURVE('',#41345,#41344,#1469,.T.);
#53056=EDGE_CURVE('',#41339,#41342,#1470,.T.);
#53057=EDGE_CURVE('',#41341,#41340,#1471,.T.);
#53058=EDGE_CURVE('',#41353,#41354,#33585,.T.);
#53059=EDGE_CURVE('',#41354,#41355,#22370,.T.);
#53060=EDGE_CURVE('',#41356,#41355,#33586,.T.);
#53061=EDGE_CURVE('',#41357,#41356,#33587,.T.);
#53062=EDGE_CURVE('',#41358,#41357,#33588,.T.);
#53063=EDGE_CURVE('',#41358,#41353,#22371,.T.);
#53064=EDGE_CURVE('',#41356,#41359,#22372,.T.);
#53065=EDGE_CURVE('',#41359,#41360,#33589,.T.);
#53066=EDGE_CURVE('',#41360,#41357,#22373,.T.);
#53067=EDGE_CURVE('',#41361,#41362,#33590,.T.);
#53068=EDGE_CURVE('',#41362,#41363,#22374,.T.);
#53069=EDGE_CURVE('',#41363,#41364,#33591,.T.);
#53070=EDGE_CURVE('',#41364,#41361,#22375,.T.);
#53071=EDGE_CURVE('',#41365,#41366,#33592,.T.);
#53072=EDGE_CURVE('',#41366,#41367,#22376,.T.);
#53073=EDGE_CURVE('',#41368,#41367,#33593,.T.);
#53074=EDGE_CURVE('',#41369,#41368,#33594,.T.);
#53075=EDGE_CURVE('',#41370,#41369,#33595,.T.);
#53076=EDGE_CURVE('',#41370,#41365,#22377,.T.);
#53077=EDGE_CURVE('',#41368,#41371,#22378,.T.);
#53078=EDGE_CURVE('',#41371,#41372,#33596,.T.);
#53079=EDGE_CURVE('',#41372,#41369,#22379,.T.);
#53080=EDGE_CURVE('',#41049,#41354,#33597,.T.);
#53081=EDGE_CURVE('',#41353,#41050,#33598,.T.);
#53082=EDGE_CURVE('',#41371,#40757,#1472,.T.);
#53083=EDGE_CURVE('',#40756,#41372,#1473,.T.);
#53084=EDGE_CURVE('',#41363,#41366,#1474,.T.);
#53085=EDGE_CURVE('',#41365,#41364,#1475,.T.);
#53086=EDGE_CURVE('',#41359,#41362,#1476,.T.);
#53087=EDGE_CURVE('',#41361,#41360,#1477,.T.);
#53088=EDGE_CURVE('',#41373,#41374,#33599,.T.);
#53089=EDGE_CURVE('',#41374,#41375,#22380,.T.);
#53090=EDGE_CURVE('',#41376,#41375,#33600,.T.);
#53091=EDGE_CURVE('',#41377,#41376,#33601,.T.);
#53092=EDGE_CURVE('',#41378,#41377,#33602,.T.);
#53093=EDGE_CURVE('',#41378,#41373,#22381,.T.);
#53094=EDGE_CURVE('',#41376,#41379,#22382,.T.);
#53095=EDGE_CURVE('',#41379,#41380,#33603,.T.);
#53096=EDGE_CURVE('',#41380,#41377,#22383,.T.);
#53097=EDGE_CURVE('',#41381,#41382,#33604,.T.);
#53098=EDGE_CURVE('',#41382,#41383,#22384,.T.);
#53099=EDGE_CURVE('',#41383,#41384,#33605,.T.);
#53100=EDGE_CURVE('',#41384,#41381,#22385,.T.);
#53101=EDGE_CURVE('',#41385,#41386,#33606,.T.);
#53102=EDGE_CURVE('',#41386,#41387,#22386,.T.);
#53103=EDGE_CURVE('',#41388,#41387,#33607,.T.);
#53104=EDGE_CURVE('',#41389,#41388,#33608,.T.);
#53105=EDGE_CURVE('',#41390,#41389,#33609,.T.);
#53106=EDGE_CURVE('',#41390,#41385,#22387,.T.);
#53107=EDGE_CURVE('',#41388,#41391,#22388,.T.);
#53108=EDGE_CURVE('',#41391,#41392,#33610,.T.);
#53109=EDGE_CURVE('',#41392,#41389,#22389,.T.);
#53110=EDGE_CURVE('',#41055,#41374,#33611,.T.);
#53111=EDGE_CURVE('',#41373,#41056,#33612,.T.);
#53112=EDGE_CURVE('',#41391,#40751,#1478,.T.);
#53113=EDGE_CURVE('',#40750,#41392,#1479,.T.);
#53114=EDGE_CURVE('',#41383,#41386,#1480,.T.);
#53115=EDGE_CURVE('',#41385,#41384,#1481,.T.);
#53116=EDGE_CURVE('',#41379,#41382,#1482,.T.);
#53117=EDGE_CURVE('',#41381,#41380,#1483,.T.);
#53118=EDGE_CURVE('',#41393,#41394,#33613,.T.);
#53119=EDGE_CURVE('',#41394,#41395,#22390,.T.);
#53120=EDGE_CURVE('',#41396,#41395,#33614,.T.);
#53121=EDGE_CURVE('',#41397,#41396,#33615,.T.);
#53122=EDGE_CURVE('',#41398,#41397,#33616,.T.);
#53123=EDGE_CURVE('',#41398,#41393,#22391,.T.);
#53124=EDGE_CURVE('',#41396,#41399,#22392,.T.);
#53125=EDGE_CURVE('',#41399,#41400,#33617,.T.);
#53126=EDGE_CURVE('',#41400,#41397,#22393,.T.);
#53127=EDGE_CURVE('',#41401,#41402,#33618,.T.);
#53128=EDGE_CURVE('',#41402,#41403,#22394,.T.);
#53129=EDGE_CURVE('',#41403,#41404,#33619,.T.);
#53130=EDGE_CURVE('',#41404,#41401,#22395,.T.);
#53131=EDGE_CURVE('',#41405,#41406,#33620,.T.);
#53132=EDGE_CURVE('',#41406,#41407,#22396,.T.);
#53133=EDGE_CURVE('',#41408,#41407,#33621,.T.);
#53134=EDGE_CURVE('',#41409,#41408,#33622,.T.);
#53135=EDGE_CURVE('',#41410,#41409,#33623,.T.);
#53136=EDGE_CURVE('',#41410,#41405,#22397,.T.);
#53137=EDGE_CURVE('',#41408,#41411,#22398,.T.);
#53138=EDGE_CURVE('',#41411,#41412,#33624,.T.);
#53139=EDGE_CURVE('',#41412,#41409,#22399,.T.);
#53140=EDGE_CURVE('',#41061,#41394,#33625,.T.);
#53141=EDGE_CURVE('',#41393,#41062,#33626,.T.);
#53142=EDGE_CURVE('',#41411,#40745,#1484,.T.);
#53143=EDGE_CURVE('',#40744,#41412,#1485,.T.);
#53144=EDGE_CURVE('',#41403,#41406,#1486,.T.);
#53145=EDGE_CURVE('',#41405,#41404,#1487,.T.);
#53146=EDGE_CURVE('',#41399,#41402,#1488,.T.);
#53147=EDGE_CURVE('',#41401,#41400,#1489,.T.);
#53148=EDGE_CURVE('',#41413,#41414,#33627,.T.);
#53149=EDGE_CURVE('',#41414,#41415,#22400,.T.);
#53150=EDGE_CURVE('',#41416,#41415,#33628,.T.);
#53151=EDGE_CURVE('',#41417,#41416,#33629,.T.);
#53152=EDGE_CURVE('',#41418,#41417,#33630,.T.);
#53153=EDGE_CURVE('',#41418,#41413,#22401,.T.);
#53154=EDGE_CURVE('',#41416,#41419,#22402,.T.);
#53155=EDGE_CURVE('',#41419,#41420,#33631,.T.);
#53156=EDGE_CURVE('',#41420,#41417,#22403,.T.);
#53157=EDGE_CURVE('',#41421,#41422,#33632,.T.);
#53158=EDGE_CURVE('',#41422,#41423,#22404,.T.);
#53159=EDGE_CURVE('',#41423,#41424,#33633,.T.);
#53160=EDGE_CURVE('',#41424,#41421,#22405,.T.);
#53161=EDGE_CURVE('',#41425,#41426,#33634,.T.);
#53162=EDGE_CURVE('',#41426,#41427,#22406,.T.);
#53163=EDGE_CURVE('',#41428,#41427,#33635,.T.);
#53164=EDGE_CURVE('',#41429,#41428,#33636,.T.);
#53165=EDGE_CURVE('',#41430,#41429,#33637,.T.);
#53166=EDGE_CURVE('',#41430,#41425,#22407,.T.);
#53167=EDGE_CURVE('',#41428,#41431,#22408,.T.);
#53168=EDGE_CURVE('',#41431,#41432,#33638,.T.);
#53169=EDGE_CURVE('',#41432,#41429,#22409,.T.);
#53170=EDGE_CURVE('',#41067,#41414,#33639,.T.);
#53171=EDGE_CURVE('',#41413,#41068,#33640,.T.);
#53172=EDGE_CURVE('',#41431,#40739,#1490,.T.);
#53173=EDGE_CURVE('',#40738,#41432,#1491,.T.);
#53174=EDGE_CURVE('',#41423,#41426,#1492,.T.);
#53175=EDGE_CURVE('',#41425,#41424,#1493,.T.);
#53176=EDGE_CURVE('',#41419,#41422,#1494,.T.);
#53177=EDGE_CURVE('',#41421,#41420,#1495,.T.);
#53178=EDGE_CURVE('',#41433,#41434,#33641,.T.);
#53179=EDGE_CURVE('',#41434,#41435,#22410,.T.);
#53180=EDGE_CURVE('',#41436,#41435,#33642,.T.);
#53181=EDGE_CURVE('',#41437,#41436,#33643,.T.);
#53182=EDGE_CURVE('',#41438,#41437,#33644,.T.);
#53183=EDGE_CURVE('',#41438,#41433,#22411,.T.);
#53184=EDGE_CURVE('',#41436,#41439,#22412,.T.);
#53185=EDGE_CURVE('',#41439,#41440,#33645,.T.);
#53186=EDGE_CURVE('',#41440,#41437,#22413,.T.);
#53187=EDGE_CURVE('',#41441,#41442,#33646,.T.);
#53188=EDGE_CURVE('',#41442,#41443,#22414,.T.);
#53189=EDGE_CURVE('',#41443,#41444,#33647,.T.);
#53190=EDGE_CURVE('',#41444,#41441,#22415,.T.);
#53191=EDGE_CURVE('',#41445,#41446,#33648,.T.);
#53192=EDGE_CURVE('',#41446,#41447,#22416,.T.);
#53193=EDGE_CURVE('',#41448,#41447,#33649,.T.);
#53194=EDGE_CURVE('',#41449,#41448,#33650,.T.);
#53195=EDGE_CURVE('',#41450,#41449,#33651,.T.);
#53196=EDGE_CURVE('',#41450,#41445,#22417,.T.);
#53197=EDGE_CURVE('',#41448,#41451,#22418,.T.);
#53198=EDGE_CURVE('',#41451,#41452,#33652,.T.);
#53199=EDGE_CURVE('',#41452,#41449,#22419,.T.);
#53200=EDGE_CURVE('',#41073,#41434,#33653,.T.);
#53201=EDGE_CURVE('',#41433,#41074,#33654,.T.);
#53202=EDGE_CURVE('',#41451,#40733,#1496,.T.);
#53203=EDGE_CURVE('',#40732,#41452,#1497,.T.);
#53204=EDGE_CURVE('',#41443,#41446,#1498,.T.);
#53205=EDGE_CURVE('',#41445,#41444,#1499,.T.);
#53206=EDGE_CURVE('',#41439,#41442,#1500,.T.);
#53207=EDGE_CURVE('',#41441,#41440,#1501,.T.);
#53208=EDGE_CURVE('',#41453,#41454,#33655,.T.);
#53209=EDGE_CURVE('',#41454,#41455,#22420,.T.);
#53210=EDGE_CURVE('',#41456,#41455,#33656,.T.);
#53211=EDGE_CURVE('',#41457,#41456,#33657,.T.);
#53212=EDGE_CURVE('',#41458,#41457,#33658,.T.);
#53213=EDGE_CURVE('',#41458,#41453,#22421,.T.);
#53214=EDGE_CURVE('',#41456,#41459,#22422,.T.);
#53215=EDGE_CURVE('',#41459,#41460,#33659,.T.);
#53216=EDGE_CURVE('',#41460,#41457,#22423,.T.);
#53217=EDGE_CURVE('',#41461,#41462,#33660,.T.);
#53218=EDGE_CURVE('',#41462,#41463,#22424,.T.);
#53219=EDGE_CURVE('',#41463,#41464,#33661,.T.);
#53220=EDGE_CURVE('',#41464,#41461,#22425,.T.);
#53221=EDGE_CURVE('',#41465,#41466,#33662,.T.);
#53222=EDGE_CURVE('',#41466,#41467,#22426,.T.);
#53223=EDGE_CURVE('',#41468,#41467,#33663,.T.);
#53224=EDGE_CURVE('',#41469,#41468,#33664,.T.);
#53225=EDGE_CURVE('',#41470,#41469,#33665,.T.);
#53226=EDGE_CURVE('',#41470,#41465,#22427,.T.);
#53227=EDGE_CURVE('',#41468,#41471,#22428,.T.);
#53228=EDGE_CURVE('',#41471,#41472,#33666,.T.);
#53229=EDGE_CURVE('',#41472,#41469,#22429,.T.);
#53230=EDGE_CURVE('',#41079,#41454,#33667,.T.);
#53231=EDGE_CURVE('',#41453,#41080,#33668,.T.);
#53232=EDGE_CURVE('',#41471,#40727,#1502,.T.);
#53233=EDGE_CURVE('',#40726,#41472,#1503,.T.);
#53234=EDGE_CURVE('',#41463,#41466,#1504,.T.);
#53235=EDGE_CURVE('',#41465,#41464,#1505,.T.);
#53236=EDGE_CURVE('',#41459,#41462,#1506,.T.);
#53237=EDGE_CURVE('',#41461,#41460,#1507,.T.);
#53238=EDGE_CURVE('',#41473,#41474,#33669,.T.);
#53239=EDGE_CURVE('',#41474,#41475,#22430,.T.);
#53240=EDGE_CURVE('',#41476,#41475,#33670,.T.);
#53241=EDGE_CURVE('',#41477,#41476,#33671,.T.);
#53242=EDGE_CURVE('',#41478,#41477,#33672,.T.);
#53243=EDGE_CURVE('',#41478,#41473,#22431,.T.);
#53244=EDGE_CURVE('',#41476,#41479,#22432,.T.);
#53245=EDGE_CURVE('',#41479,#41480,#33673,.T.);
#53246=EDGE_CURVE('',#41480,#41477,#22433,.T.);
#53247=EDGE_CURVE('',#41481,#41482,#33674,.T.);
#53248=EDGE_CURVE('',#41482,#41483,#22434,.T.);
#53249=EDGE_CURVE('',#41483,#41484,#33675,.T.);
#53250=EDGE_CURVE('',#41484,#41481,#22435,.T.);
#53251=EDGE_CURVE('',#41485,#41486,#33676,.T.);
#53252=EDGE_CURVE('',#41486,#41487,#22436,.T.);
#53253=EDGE_CURVE('',#41488,#41487,#33677,.T.);
#53254=EDGE_CURVE('',#41489,#41488,#33678,.T.);
#53255=EDGE_CURVE('',#41490,#41489,#33679,.T.);
#53256=EDGE_CURVE('',#41490,#41485,#22437,.T.);
#53257=EDGE_CURVE('',#41488,#41491,#22438,.T.);
#53258=EDGE_CURVE('',#41491,#41492,#33680,.T.);
#53259=EDGE_CURVE('',#41492,#41489,#22439,.T.);
#53260=EDGE_CURVE('',#41083,#41474,#33681,.T.);
#53261=EDGE_CURVE('',#41473,#41084,#33682,.T.);
#53262=EDGE_CURVE('',#41491,#40723,#1508,.T.);
#53263=EDGE_CURVE('',#40722,#41492,#1509,.T.);
#53264=EDGE_CURVE('',#41483,#41486,#1510,.T.);
#53265=EDGE_CURVE('',#41485,#41484,#1511,.T.);
#53266=EDGE_CURVE('',#41479,#41482,#1512,.T.);
#53267=EDGE_CURVE('',#41481,#41480,#1513,.T.);
#53268=EDGE_CURVE('',#41493,#41494,#33683,.T.);
#53269=EDGE_CURVE('',#41494,#41495,#22440,.T.);
#53270=EDGE_CURVE('',#41496,#41495,#33684,.T.);
#53271=EDGE_CURVE('',#41497,#41496,#33685,.T.);
#53272=EDGE_CURVE('',#41498,#41497,#33686,.T.);
#53273=EDGE_CURVE('',#41498,#41493,#22441,.T.);
#53274=EDGE_CURVE('',#41496,#41499,#22442,.T.);
#53275=EDGE_CURVE('',#41499,#41500,#33687,.T.);
#53276=EDGE_CURVE('',#41500,#41497,#22443,.T.);
#53277=EDGE_CURVE('',#41501,#41502,#33688,.T.);
#53278=EDGE_CURVE('',#41502,#41503,#22444,.T.);
#53279=EDGE_CURVE('',#41503,#41504,#33689,.T.);
#53280=EDGE_CURVE('',#41504,#41501,#22445,.T.);
#53281=EDGE_CURVE('',#41505,#41506,#33690,.T.);
#53282=EDGE_CURVE('',#41506,#41507,#22446,.T.);
#53283=EDGE_CURVE('',#41508,#41507,#33691,.T.);
#53284=EDGE_CURVE('',#41509,#41508,#33692,.T.);
#53285=EDGE_CURVE('',#41510,#41509,#33693,.T.);
#53286=EDGE_CURVE('',#41510,#41505,#22447,.T.);
#53287=EDGE_CURVE('',#41508,#41511,#22448,.T.);
#53288=EDGE_CURVE('',#41511,#41512,#33694,.T.);
#53289=EDGE_CURVE('',#41512,#41509,#22449,.T.);
#53290=EDGE_CURVE('',#41089,#41494,#33695,.T.);
#53291=EDGE_CURVE('',#41493,#41090,#33696,.T.);
#53292=EDGE_CURVE('',#41511,#40717,#1514,.T.);
#53293=EDGE_CURVE('',#40716,#41512,#1515,.T.);
#53294=EDGE_CURVE('',#41503,#41506,#1516,.T.);
#53295=EDGE_CURVE('',#41505,#41504,#1517,.T.);
#53296=EDGE_CURVE('',#41499,#41502,#1518,.T.);
#53297=EDGE_CURVE('',#41501,#41500,#1519,.T.);
#53298=EDGE_CURVE('',#41513,#41514,#33697,.T.);
#53299=EDGE_CURVE('',#41514,#41515,#22450,.T.);
#53300=EDGE_CURVE('',#41516,#41515,#33698,.T.);
#53301=EDGE_CURVE('',#41517,#41516,#33699,.T.);
#53302=EDGE_CURVE('',#41518,#41517,#33700,.T.);
#53303=EDGE_CURVE('',#41518,#41513,#22451,.T.);
#53304=EDGE_CURVE('',#41516,#41519,#22452,.T.);
#53305=EDGE_CURVE('',#41519,#41520,#33701,.T.);
#53306=EDGE_CURVE('',#41520,#41517,#22453,.T.);
#53307=EDGE_CURVE('',#41521,#41522,#33702,.T.);
#53308=EDGE_CURVE('',#41522,#41523,#22454,.T.);
#53309=EDGE_CURVE('',#41523,#41524,#33703,.T.);
#53310=EDGE_CURVE('',#41524,#41521,#22455,.T.);
#53311=EDGE_CURVE('',#41525,#41526,#33704,.T.);
#53312=EDGE_CURVE('',#41526,#41527,#22456,.T.);
#53313=EDGE_CURVE('',#41528,#41527,#33705,.T.);
#53314=EDGE_CURVE('',#41529,#41528,#33706,.T.);
#53315=EDGE_CURVE('',#41530,#41529,#33707,.T.);
#53316=EDGE_CURVE('',#41530,#41525,#22457,.T.);
#53317=EDGE_CURVE('',#41528,#41531,#22458,.T.);
#53318=EDGE_CURVE('',#41531,#41532,#33708,.T.);
#53319=EDGE_CURVE('',#41532,#41529,#22459,.T.);
#53320=EDGE_CURVE('',#41095,#41514,#33709,.T.);
#53321=EDGE_CURVE('',#41513,#41096,#33710,.T.);
#53322=EDGE_CURVE('',#41531,#40711,#1520,.T.);
#53323=EDGE_CURVE('',#40710,#41532,#1521,.T.);
#53324=EDGE_CURVE('',#41523,#41526,#1522,.T.);
#53325=EDGE_CURVE('',#41525,#41524,#1523,.T.);
#53326=EDGE_CURVE('',#41519,#41522,#1524,.T.);
#53327=EDGE_CURVE('',#41521,#41520,#1525,.T.);
#53328=EDGE_CURVE('',#41533,#41534,#33711,.T.);
#53329=EDGE_CURVE('',#41534,#41535,#22460,.T.);
#53330=EDGE_CURVE('',#41536,#41535,#33712,.T.);
#53331=EDGE_CURVE('',#41537,#41536,#33713,.T.);
#53332=EDGE_CURVE('',#41538,#41537,#33714,.T.);
#53333=EDGE_CURVE('',#41538,#41533,#22461,.T.);
#53334=EDGE_CURVE('',#41536,#41539,#22462,.T.);
#53335=EDGE_CURVE('',#41539,#41540,#33715,.T.);
#53336=EDGE_CURVE('',#41540,#41537,#22463,.T.);
#53337=EDGE_CURVE('',#41541,#41542,#33716,.T.);
#53338=EDGE_CURVE('',#41542,#41543,#22464,.T.);
#53339=EDGE_CURVE('',#41543,#41544,#33717,.T.);
#53340=EDGE_CURVE('',#41544,#41541,#22465,.T.);
#53341=EDGE_CURVE('',#41545,#41546,#33718,.T.);
#53342=EDGE_CURVE('',#41546,#41547,#22466,.T.);
#53343=EDGE_CURVE('',#41548,#41547,#33719,.T.);
#53344=EDGE_CURVE('',#41549,#41548,#33720,.T.);
#53345=EDGE_CURVE('',#41550,#41549,#33721,.T.);
#53346=EDGE_CURVE('',#41550,#41545,#22467,.T.);
#53347=EDGE_CURVE('',#41548,#41551,#22468,.T.);
#53348=EDGE_CURVE('',#41551,#41552,#33722,.T.);
#53349=EDGE_CURVE('',#41552,#41549,#22469,.T.);
#53350=EDGE_CURVE('',#41101,#41534,#33723,.T.);
#53351=EDGE_CURVE('',#41533,#41102,#33724,.T.);
#53352=EDGE_CURVE('',#41551,#40705,#1526,.T.);
#53353=EDGE_CURVE('',#40704,#41552,#1527,.T.);
#53354=EDGE_CURVE('',#41543,#41546,#1528,.T.);
#53355=EDGE_CURVE('',#41545,#41544,#1529,.T.);
#53356=EDGE_CURVE('',#41539,#41542,#1530,.T.);
#53357=EDGE_CURVE('',#41541,#41540,#1531,.T.);
#53358=EDGE_CURVE('',#41553,#41554,#33725,.T.);
#53359=EDGE_CURVE('',#41554,#41555,#22470,.T.);
#53360=EDGE_CURVE('',#41556,#41555,#33726,.T.);
#53361=EDGE_CURVE('',#41557,#41556,#33727,.T.);
#53362=EDGE_CURVE('',#41558,#41557,#33728,.T.);
#53363=EDGE_CURVE('',#41558,#41553,#22471,.T.);
#53364=EDGE_CURVE('',#41556,#41559,#22472,.T.);
#53365=EDGE_CURVE('',#41559,#41560,#33729,.T.);
#53366=EDGE_CURVE('',#41560,#41557,#22473,.T.);
#53367=EDGE_CURVE('',#41561,#41562,#33730,.T.);
#53368=EDGE_CURVE('',#41562,#41563,#22474,.T.);
#53369=EDGE_CURVE('',#41563,#41564,#33731,.T.);
#53370=EDGE_CURVE('',#41564,#41561,#22475,.T.);
#53371=EDGE_CURVE('',#41565,#41566,#33732,.T.);
#53372=EDGE_CURVE('',#41566,#41567,#22476,.T.);
#53373=EDGE_CURVE('',#41568,#41567,#33733,.T.);
#53374=EDGE_CURVE('',#41569,#41568,#33734,.T.);
#53375=EDGE_CURVE('',#41570,#41569,#33735,.T.);
#53376=EDGE_CURVE('',#41570,#41565,#22477,.T.);
#53377=EDGE_CURVE('',#41568,#41571,#22478,.T.);
#53378=EDGE_CURVE('',#41571,#41572,#33736,.T.);
#53379=EDGE_CURVE('',#41572,#41569,#22479,.T.);
#53380=EDGE_CURVE('',#41107,#41554,#33737,.T.);
#53381=EDGE_CURVE('',#41553,#41108,#33738,.T.);
#53382=EDGE_CURVE('',#41571,#40699,#1532,.T.);
#53383=EDGE_CURVE('',#40698,#41572,#1533,.T.);
#53384=EDGE_CURVE('',#41563,#41566,#1534,.T.);
#53385=EDGE_CURVE('',#41565,#41564,#1535,.T.);
#53386=EDGE_CURVE('',#41559,#41562,#1536,.T.);
#53387=EDGE_CURVE('',#41561,#41560,#1537,.T.);
#53388=EDGE_CURVE('',#41573,#41574,#33739,.T.);
#53389=EDGE_CURVE('',#41574,#41575,#22480,.T.);
#53390=EDGE_CURVE('',#41576,#41575,#33740,.T.);
#53391=EDGE_CURVE('',#41577,#41576,#33741,.T.);
#53392=EDGE_CURVE('',#41578,#41577,#33742,.T.);
#53393=EDGE_CURVE('',#41578,#41573,#22481,.T.);
#53394=EDGE_CURVE('',#41576,#41579,#22482,.T.);
#53395=EDGE_CURVE('',#41579,#41580,#33743,.T.);
#53396=EDGE_CURVE('',#41580,#41577,#22483,.T.);
#53397=EDGE_CURVE('',#41581,#41582,#33744,.T.);
#53398=EDGE_CURVE('',#41582,#41583,#22484,.T.);
#53399=EDGE_CURVE('',#41583,#41584,#33745,.T.);
#53400=EDGE_CURVE('',#41584,#41581,#22485,.T.);
#53401=EDGE_CURVE('',#41585,#41586,#33746,.T.);
#53402=EDGE_CURVE('',#41586,#41587,#22486,.T.);
#53403=EDGE_CURVE('',#41588,#41587,#33747,.T.);
#53404=EDGE_CURVE('',#41589,#41588,#33748,.T.);
#53405=EDGE_CURVE('',#41590,#41589,#33749,.T.);
#53406=EDGE_CURVE('',#41590,#41585,#22487,.T.);
#53407=EDGE_CURVE('',#41588,#41591,#22488,.T.);
#53408=EDGE_CURVE('',#41591,#41592,#33750,.T.);
#53409=EDGE_CURVE('',#41592,#41589,#22489,.T.);
#53410=EDGE_CURVE('',#41113,#41574,#33751,.T.);
#53411=EDGE_CURVE('',#41573,#41114,#33752,.T.);
#53412=EDGE_CURVE('',#41591,#40693,#1538,.T.);
#53413=EDGE_CURVE('',#40692,#41592,#1539,.T.);
#53414=EDGE_CURVE('',#41583,#41586,#1540,.T.);
#53415=EDGE_CURVE('',#41585,#41584,#1541,.T.);
#53416=EDGE_CURVE('',#41579,#41582,#1542,.T.);
#53417=EDGE_CURVE('',#41581,#41580,#1543,.T.);
#53418=EDGE_CURVE('',#41593,#41594,#33753,.T.);
#53419=EDGE_CURVE('',#41594,#41595,#22490,.T.);
#53420=EDGE_CURVE('',#41596,#41595,#33754,.T.);
#53421=EDGE_CURVE('',#41597,#41596,#33755,.T.);
#53422=EDGE_CURVE('',#41598,#41597,#33756,.T.);
#53423=EDGE_CURVE('',#41598,#41593,#22491,.T.);
#53424=EDGE_CURVE('',#41596,#41599,#22492,.T.);
#53425=EDGE_CURVE('',#41599,#41600,#33757,.T.);
#53426=EDGE_CURVE('',#41600,#41597,#22493,.T.);
#53427=EDGE_CURVE('',#41601,#41602,#33758,.T.);
#53428=EDGE_CURVE('',#41602,#41603,#22494,.T.);
#53429=EDGE_CURVE('',#41603,#41604,#33759,.T.);
#53430=EDGE_CURVE('',#41604,#41601,#22495,.T.);
#53431=EDGE_CURVE('',#41605,#41606,#33760,.T.);
#53432=EDGE_CURVE('',#41606,#41607,#22496,.T.);
#53433=EDGE_CURVE('',#41608,#41607,#33761,.T.);
#53434=EDGE_CURVE('',#41609,#41608,#33762,.T.);
#53435=EDGE_CURVE('',#41610,#41609,#33763,.T.);
#53436=EDGE_CURVE('',#41610,#41605,#22497,.T.);
#53437=EDGE_CURVE('',#41608,#41611,#22498,.T.);
#53438=EDGE_CURVE('',#41611,#41612,#33764,.T.);
#53439=EDGE_CURVE('',#41612,#41609,#22499,.T.);
#53440=EDGE_CURVE('',#41119,#41594,#33765,.T.);
#53441=EDGE_CURVE('',#41593,#41120,#33766,.T.);
#53442=EDGE_CURVE('',#41611,#40687,#1544,.T.);
#53443=EDGE_CURVE('',#40686,#41612,#1545,.T.);
#53444=EDGE_CURVE('',#41603,#41606,#1546,.T.);
#53445=EDGE_CURVE('',#41605,#41604,#1547,.T.);
#53446=EDGE_CURVE('',#41599,#41602,#1548,.T.);
#53447=EDGE_CURVE('',#41601,#41600,#1549,.T.);
#53448=EDGE_CURVE('',#41613,#41614,#33767,.T.);
#53449=EDGE_CURVE('',#41614,#41615,#22500,.T.);
#53450=EDGE_CURVE('',#41616,#41615,#33768,.T.);
#53451=EDGE_CURVE('',#41617,#41616,#33769,.T.);
#53452=EDGE_CURVE('',#41618,#41617,#33770,.T.);
#53453=EDGE_CURVE('',#41618,#41613,#22501,.T.);
#53454=EDGE_CURVE('',#41616,#41619,#22502,.T.);
#53455=EDGE_CURVE('',#41619,#41620,#33771,.T.);
#53456=EDGE_CURVE('',#41620,#41617,#22503,.T.);
#53457=EDGE_CURVE('',#41621,#41622,#33772,.T.);
#53458=EDGE_CURVE('',#41622,#41623,#22504,.T.);
#53459=EDGE_CURVE('',#41623,#41624,#33773,.T.);
#53460=EDGE_CURVE('',#41624,#41621,#22505,.T.);
#53461=EDGE_CURVE('',#41625,#41626,#33774,.T.);
#53462=EDGE_CURVE('',#41626,#41627,#22506,.T.);
#53463=EDGE_CURVE('',#41628,#41627,#33775,.T.);
#53464=EDGE_CURVE('',#41629,#41628,#33776,.T.);
#53465=EDGE_CURVE('',#41630,#41629,#33777,.T.);
#53466=EDGE_CURVE('',#41630,#41625,#22507,.T.);
#53467=EDGE_CURVE('',#41628,#41631,#22508,.T.);
#53468=EDGE_CURVE('',#41631,#41632,#33778,.T.);
#53469=EDGE_CURVE('',#41632,#41629,#22509,.T.);
#53470=EDGE_CURVE('',#41125,#41614,#33779,.T.);
#53471=EDGE_CURVE('',#41613,#41126,#33780,.T.);
#53472=EDGE_CURVE('',#41631,#40681,#1550,.T.);
#53473=EDGE_CURVE('',#40680,#41632,#1551,.T.);
#53474=EDGE_CURVE('',#41623,#41626,#1552,.T.);
#53475=EDGE_CURVE('',#41625,#41624,#1553,.T.);
#53476=EDGE_CURVE('',#41619,#41622,#1554,.T.);
#53477=EDGE_CURVE('',#41621,#41620,#1555,.T.);
#53478=EDGE_CURVE('',#41633,#41634,#33781,.T.);
#53479=EDGE_CURVE('',#41634,#41635,#22510,.T.);
#53480=EDGE_CURVE('',#41636,#41635,#33782,.T.);
#53481=EDGE_CURVE('',#41637,#41636,#33783,.T.);
#53482=EDGE_CURVE('',#41638,#41637,#33784,.T.);
#53483=EDGE_CURVE('',#41638,#41633,#22511,.T.);
#53484=EDGE_CURVE('',#41636,#41639,#22512,.T.);
#53485=EDGE_CURVE('',#41639,#41640,#33785,.T.);
#53486=EDGE_CURVE('',#41640,#41637,#22513,.T.);
#53487=EDGE_CURVE('',#41641,#41642,#33786,.T.);
#53488=EDGE_CURVE('',#41642,#41643,#22514,.T.);
#53489=EDGE_CURVE('',#41643,#41644,#33787,.T.);
#53490=EDGE_CURVE('',#41644,#41641,#22515,.T.);
#53491=EDGE_CURVE('',#41645,#41646,#33788,.T.);
#53492=EDGE_CURVE('',#41646,#41647,#22516,.T.);
#53493=EDGE_CURVE('',#41648,#41647,#33789,.T.);
#53494=EDGE_CURVE('',#41649,#41648,#33790,.T.);
#53495=EDGE_CURVE('',#41650,#41649,#33791,.T.);
#53496=EDGE_CURVE('',#41650,#41645,#22517,.T.);
#53497=EDGE_CURVE('',#41648,#41651,#22518,.T.);
#53498=EDGE_CURVE('',#41651,#41652,#33792,.T.);
#53499=EDGE_CURVE('',#41652,#41649,#22519,.T.);
#53500=EDGE_CURVE('',#41131,#41634,#33793,.T.);
#53501=EDGE_CURVE('',#41633,#41132,#33794,.T.);
#53502=EDGE_CURVE('',#41651,#40675,#1556,.T.);
#53503=EDGE_CURVE('',#40674,#41652,#1557,.T.);
#53504=EDGE_CURVE('',#41643,#41646,#1558,.T.);
#53505=EDGE_CURVE('',#41645,#41644,#1559,.T.);
#53506=EDGE_CURVE('',#41639,#41642,#1560,.T.);
#53507=EDGE_CURVE('',#41641,#41640,#1561,.T.);
#53508=EDGE_CURVE('',#41653,#41654,#33795,.T.);
#53509=EDGE_CURVE('',#41654,#41655,#22520,.T.);
#53510=EDGE_CURVE('',#41656,#41655,#33796,.T.);
#53511=EDGE_CURVE('',#41657,#41656,#33797,.T.);
#53512=EDGE_CURVE('',#41658,#41657,#33798,.T.);
#53513=EDGE_CURVE('',#41658,#41653,#22521,.T.);
#53514=EDGE_CURVE('',#41656,#41659,#22522,.T.);
#53515=EDGE_CURVE('',#41659,#41660,#33799,.T.);
#53516=EDGE_CURVE('',#41660,#41657,#22523,.T.);
#53517=EDGE_CURVE('',#41661,#41662,#33800,.T.);
#53518=EDGE_CURVE('',#41662,#41663,#22524,.T.);
#53519=EDGE_CURVE('',#41663,#41664,#33801,.T.);
#53520=EDGE_CURVE('',#41664,#41661,#22525,.T.);
#53521=EDGE_CURVE('',#41665,#41666,#33802,.T.);
#53522=EDGE_CURVE('',#41666,#41667,#22526,.T.);
#53523=EDGE_CURVE('',#41668,#41667,#33803,.T.);
#53524=EDGE_CURVE('',#41669,#41668,#33804,.T.);
#53525=EDGE_CURVE('',#41670,#41669,#33805,.T.);
#53526=EDGE_CURVE('',#41670,#41665,#22527,.T.);
#53527=EDGE_CURVE('',#41668,#41671,#22528,.T.);
#53528=EDGE_CURVE('',#41671,#41672,#33806,.T.);
#53529=EDGE_CURVE('',#41672,#41669,#22529,.T.);
#53530=EDGE_CURVE('',#41137,#41654,#33807,.T.);
#53531=EDGE_CURVE('',#41653,#41138,#33808,.T.);
#53532=EDGE_CURVE('',#41671,#40669,#1562,.T.);
#53533=EDGE_CURVE('',#40668,#41672,#1563,.T.);
#53534=EDGE_CURVE('',#41663,#41666,#1564,.T.);
#53535=EDGE_CURVE('',#41665,#41664,#1565,.T.);
#53536=EDGE_CURVE('',#41659,#41662,#1566,.T.);
#53537=EDGE_CURVE('',#41661,#41660,#1567,.T.);
#53538=EDGE_CURVE('',#41673,#41674,#33809,.T.);
#53539=EDGE_CURVE('',#41674,#41675,#22530,.T.);
#53540=EDGE_CURVE('',#41676,#41675,#33810,.T.);
#53541=EDGE_CURVE('',#41677,#41676,#33811,.T.);
#53542=EDGE_CURVE('',#41678,#41677,#33812,.T.);
#53543=EDGE_CURVE('',#41678,#41673,#22531,.T.);
#53544=EDGE_CURVE('',#41676,#41679,#22532,.T.);
#53545=EDGE_CURVE('',#41679,#41680,#33813,.T.);
#53546=EDGE_CURVE('',#41680,#41677,#22533,.T.);
#53547=EDGE_CURVE('',#41681,#41682,#33814,.T.);
#53548=EDGE_CURVE('',#41682,#41683,#22534,.T.);
#53549=EDGE_CURVE('',#41683,#41684,#33815,.T.);
#53550=EDGE_CURVE('',#41684,#41681,#22535,.T.);
#53551=EDGE_CURVE('',#41685,#41686,#33816,.T.);
#53552=EDGE_CURVE('',#41686,#41687,#22536,.T.);
#53553=EDGE_CURVE('',#41688,#41687,#33817,.T.);
#53554=EDGE_CURVE('',#41689,#41688,#33818,.T.);
#53555=EDGE_CURVE('',#41690,#41689,#33819,.T.);
#53556=EDGE_CURVE('',#41690,#41685,#22537,.T.);
#53557=EDGE_CURVE('',#41688,#41691,#22538,.T.);
#53558=EDGE_CURVE('',#41691,#41692,#33820,.T.);
#53559=EDGE_CURVE('',#41692,#41689,#22539,.T.);
#53560=EDGE_CURVE('',#41143,#41674,#33821,.T.);
#53561=EDGE_CURVE('',#41673,#41144,#33822,.T.);
#53562=EDGE_CURVE('',#41691,#40663,#1568,.T.);
#53563=EDGE_CURVE('',#40662,#41692,#1569,.T.);
#53564=EDGE_CURVE('',#41683,#41686,#1570,.T.);
#53565=EDGE_CURVE('',#41685,#41684,#1571,.T.);
#53566=EDGE_CURVE('',#41679,#41682,#1572,.T.);
#53567=EDGE_CURVE('',#41681,#41680,#1573,.T.);
#53568=EDGE_CURVE('',#41693,#41694,#33823,.T.);
#53569=EDGE_CURVE('',#41694,#41695,#22540,.T.);
#53570=EDGE_CURVE('',#41696,#41695,#33824,.T.);
#53571=EDGE_CURVE('',#41697,#41696,#33825,.T.);
#53572=EDGE_CURVE('',#41698,#41697,#33826,.T.);
#53573=EDGE_CURVE('',#41698,#41693,#22541,.T.);
#53574=EDGE_CURVE('',#41696,#41699,#22542,.T.);
#53575=EDGE_CURVE('',#41699,#41700,#33827,.T.);
#53576=EDGE_CURVE('',#41700,#41697,#22543,.T.);
#53577=EDGE_CURVE('',#41701,#41702,#33828,.T.);
#53578=EDGE_CURVE('',#41702,#41703,#22544,.T.);
#53579=EDGE_CURVE('',#41703,#41704,#33829,.T.);
#53580=EDGE_CURVE('',#41704,#41701,#22545,.T.);
#53581=EDGE_CURVE('',#41705,#41706,#33830,.T.);
#53582=EDGE_CURVE('',#41706,#41707,#22546,.T.);
#53583=EDGE_CURVE('',#41708,#41707,#33831,.T.);
#53584=EDGE_CURVE('',#41709,#41708,#33832,.T.);
#53585=EDGE_CURVE('',#41710,#41709,#33833,.T.);
#53586=EDGE_CURVE('',#41710,#41705,#22547,.T.);
#53587=EDGE_CURVE('',#41708,#41711,#22548,.T.);
#53588=EDGE_CURVE('',#41711,#41712,#33834,.T.);
#53589=EDGE_CURVE('',#41712,#41709,#22549,.T.);
#53590=EDGE_CURVE('',#41149,#41694,#33835,.T.);
#53591=EDGE_CURVE('',#41693,#41150,#33836,.T.);
#53592=EDGE_CURVE('',#41711,#40657,#1574,.T.);
#53593=EDGE_CURVE('',#40656,#41712,#1575,.T.);
#53594=EDGE_CURVE('',#41703,#41706,#1576,.T.);
#53595=EDGE_CURVE('',#41705,#41704,#1577,.T.);
#53596=EDGE_CURVE('',#41699,#41702,#1578,.T.);
#53597=EDGE_CURVE('',#41701,#41700,#1579,.T.);
#53598=EDGE_CURVE('',#41713,#41714,#33837,.T.);
#53599=EDGE_CURVE('',#41714,#41715,#22550,.T.);
#53600=EDGE_CURVE('',#41716,#41715,#33838,.T.);
#53601=EDGE_CURVE('',#41717,#41716,#33839,.T.);
#53602=EDGE_CURVE('',#41718,#41717,#33840,.T.);
#53603=EDGE_CURVE('',#41718,#41713,#22551,.T.);
#53604=EDGE_CURVE('',#41716,#41719,#22552,.T.);
#53605=EDGE_CURVE('',#41719,#41720,#33841,.T.);
#53606=EDGE_CURVE('',#41720,#41717,#22553,.T.);
#53607=EDGE_CURVE('',#41721,#41722,#33842,.T.);
#53608=EDGE_CURVE('',#41722,#41723,#22554,.T.);
#53609=EDGE_CURVE('',#41723,#41724,#33843,.T.);
#53610=EDGE_CURVE('',#41724,#41721,#22555,.T.);
#53611=EDGE_CURVE('',#41725,#41726,#33844,.T.);
#53612=EDGE_CURVE('',#41726,#41727,#22556,.T.);
#53613=EDGE_CURVE('',#41728,#41727,#33845,.T.);
#53614=EDGE_CURVE('',#41729,#41728,#33846,.T.);
#53615=EDGE_CURVE('',#41730,#41729,#33847,.T.);
#53616=EDGE_CURVE('',#41730,#41725,#22557,.T.);
#53617=EDGE_CURVE('',#41728,#41731,#22558,.T.);
#53618=EDGE_CURVE('',#41731,#41732,#33848,.T.);
#53619=EDGE_CURVE('',#41732,#41729,#22559,.T.);
#53620=EDGE_CURVE('',#41155,#41714,#33849,.T.);
#53621=EDGE_CURVE('',#41713,#41156,#33850,.T.);
#53622=EDGE_CURVE('',#41731,#40651,#1580,.T.);
#53623=EDGE_CURVE('',#40650,#41732,#1581,.T.);
#53624=EDGE_CURVE('',#41723,#41726,#1582,.T.);
#53625=EDGE_CURVE('',#41725,#41724,#1583,.T.);
#53626=EDGE_CURVE('',#41719,#41722,#1584,.T.);
#53627=EDGE_CURVE('',#41721,#41720,#1585,.T.);
#53628=EDGE_CURVE('',#41733,#41734,#33851,.T.);
#53629=EDGE_CURVE('',#41734,#41735,#22560,.T.);
#53630=EDGE_CURVE('',#41736,#41735,#33852,.T.);
#53631=EDGE_CURVE('',#41737,#41736,#33853,.T.);
#53632=EDGE_CURVE('',#41738,#41737,#33854,.T.);
#53633=EDGE_CURVE('',#41738,#41733,#22561,.T.);
#53634=EDGE_CURVE('',#41736,#41739,#22562,.T.);
#53635=EDGE_CURVE('',#41739,#41740,#33855,.T.);
#53636=EDGE_CURVE('',#41740,#41737,#22563,.T.);
#53637=EDGE_CURVE('',#41741,#41742,#33856,.T.);
#53638=EDGE_CURVE('',#41742,#41743,#22564,.T.);
#53639=EDGE_CURVE('',#41743,#41744,#33857,.T.);
#53640=EDGE_CURVE('',#41744,#41741,#22565,.T.);
#53641=EDGE_CURVE('',#41745,#41746,#33858,.T.);
#53642=EDGE_CURVE('',#41746,#41747,#22566,.T.);
#53643=EDGE_CURVE('',#41748,#41747,#33859,.T.);
#53644=EDGE_CURVE('',#41749,#41748,#33860,.T.);
#53645=EDGE_CURVE('',#41750,#41749,#33861,.T.);
#53646=EDGE_CURVE('',#41750,#41745,#22567,.T.);
#53647=EDGE_CURVE('',#41748,#41751,#22568,.T.);
#53648=EDGE_CURVE('',#41751,#41752,#33862,.T.);
#53649=EDGE_CURVE('',#41752,#41749,#22569,.T.);
#53650=EDGE_CURVE('',#41161,#41734,#33863,.T.);
#53651=EDGE_CURVE('',#41733,#41162,#33864,.T.);
#53652=EDGE_CURVE('',#41751,#40645,#1586,.T.);
#53653=EDGE_CURVE('',#40644,#41752,#1587,.T.);
#53654=EDGE_CURVE('',#41743,#41746,#1588,.T.);
#53655=EDGE_CURVE('',#41745,#41744,#1589,.T.);
#53656=EDGE_CURVE('',#41739,#41742,#1590,.T.);
#53657=EDGE_CURVE('',#41741,#41740,#1591,.T.);
#53658=EDGE_CURVE('',#41753,#41754,#33865,.T.);
#53659=EDGE_CURVE('',#41754,#41755,#22570,.T.);
#53660=EDGE_CURVE('',#41756,#41755,#33866,.T.);
#53661=EDGE_CURVE('',#41757,#41756,#33867,.T.);
#53662=EDGE_CURVE('',#41758,#41757,#33868,.T.);
#53663=EDGE_CURVE('',#41758,#41753,#22571,.T.);
#53664=EDGE_CURVE('',#41756,#41759,#22572,.T.);
#53665=EDGE_CURVE('',#41759,#41760,#33869,.T.);
#53666=EDGE_CURVE('',#41760,#41757,#22573,.T.);
#53667=EDGE_CURVE('',#41761,#41762,#33870,.T.);
#53668=EDGE_CURVE('',#41762,#41763,#22574,.T.);
#53669=EDGE_CURVE('',#41763,#41764,#33871,.T.);
#53670=EDGE_CURVE('',#41764,#41761,#22575,.T.);
#53671=EDGE_CURVE('',#41765,#41766,#33872,.T.);
#53672=EDGE_CURVE('',#41766,#41767,#22576,.T.);
#53673=EDGE_CURVE('',#41768,#41767,#33873,.T.);
#53674=EDGE_CURVE('',#41769,#41768,#33874,.T.);
#53675=EDGE_CURVE('',#41770,#41769,#33875,.T.);
#53676=EDGE_CURVE('',#41770,#41765,#22577,.T.);
#53677=EDGE_CURVE('',#41768,#41771,#22578,.T.);
#53678=EDGE_CURVE('',#41771,#41772,#33876,.T.);
#53679=EDGE_CURVE('',#41772,#41769,#22579,.T.);
#53680=EDGE_CURVE('',#41167,#41754,#33877,.T.);
#53681=EDGE_CURVE('',#41753,#41168,#33878,.T.);
#53682=EDGE_CURVE('',#41771,#40639,#1592,.T.);
#53683=EDGE_CURVE('',#40638,#41772,#1593,.T.);
#53684=EDGE_CURVE('',#41763,#41766,#1594,.T.);
#53685=EDGE_CURVE('',#41765,#41764,#1595,.T.);
#53686=EDGE_CURVE('',#41759,#41762,#1596,.T.);
#53687=EDGE_CURVE('',#41761,#41760,#1597,.T.);
#53688=EDGE_CURVE('',#41773,#41774,#33879,.T.);
#53689=EDGE_CURVE('',#41774,#41775,#22580,.T.);
#53690=EDGE_CURVE('',#41776,#41775,#33880,.T.);
#53691=EDGE_CURVE('',#41777,#41776,#33881,.T.);
#53692=EDGE_CURVE('',#41778,#41777,#33882,.T.);
#53693=EDGE_CURVE('',#41778,#41773,#22581,.T.);
#53694=EDGE_CURVE('',#41776,#41779,#22582,.T.);
#53695=EDGE_CURVE('',#41779,#41780,#33883,.T.);
#53696=EDGE_CURVE('',#41780,#41777,#22583,.T.);
#53697=EDGE_CURVE('',#41781,#41782,#33884,.T.);
#53698=EDGE_CURVE('',#41782,#41783,#22584,.T.);
#53699=EDGE_CURVE('',#41783,#41784,#33885,.T.);
#53700=EDGE_CURVE('',#41784,#41781,#22585,.T.);
#53701=EDGE_CURVE('',#41785,#41786,#33886,.T.);
#53702=EDGE_CURVE('',#41786,#41787,#22586,.T.);
#53703=EDGE_CURVE('',#41788,#41787,#33887,.T.);
#53704=EDGE_CURVE('',#41789,#41788,#33888,.T.);
#53705=EDGE_CURVE('',#41790,#41789,#33889,.T.);
#53706=EDGE_CURVE('',#41790,#41785,#22587,.T.);
#53707=EDGE_CURVE('',#41788,#41791,#22588,.T.);
#53708=EDGE_CURVE('',#41791,#41792,#33890,.T.);
#53709=EDGE_CURVE('',#41792,#41789,#22589,.T.);
#53710=EDGE_CURVE('',#40814,#41774,#33891,.T.);
#53711=EDGE_CURVE('',#41773,#40815,#33892,.T.);
#53712=EDGE_CURVE('',#41791,#40635,#1598,.T.);
#53713=EDGE_CURVE('',#40634,#41792,#1599,.T.);
#53714=EDGE_CURVE('',#41783,#41786,#1600,.T.);
#53715=EDGE_CURVE('',#41785,#41784,#1601,.T.);
#53716=EDGE_CURVE('',#41779,#41782,#1602,.T.);
#53717=EDGE_CURVE('',#41781,#41780,#1603,.T.);
#53718=EDGE_CURVE('',#41793,#41794,#33893,.T.);
#53719=EDGE_CURVE('',#41794,#41795,#22590,.T.);
#53720=EDGE_CURVE('',#41796,#41795,#33894,.T.);
#53721=EDGE_CURVE('',#41797,#41796,#33895,.T.);
#53722=EDGE_CURVE('',#41798,#41797,#33896,.T.);
#53723=EDGE_CURVE('',#41798,#41793,#22591,.T.);
#53724=EDGE_CURVE('',#41796,#41799,#22592,.T.);
#53725=EDGE_CURVE('',#41799,#41800,#33897,.T.);
#53726=EDGE_CURVE('',#41800,#41797,#22593,.T.);
#53727=EDGE_CURVE('',#41801,#41802,#33898,.T.);
#53728=EDGE_CURVE('',#41802,#41803,#22594,.T.);
#53729=EDGE_CURVE('',#41803,#41804,#33899,.T.);
#53730=EDGE_CURVE('',#41804,#41801,#22595,.T.);
#53731=EDGE_CURVE('',#41805,#41806,#33900,.T.);
#53732=EDGE_CURVE('',#41806,#41807,#22596,.T.);
#53733=EDGE_CURVE('',#41808,#41807,#33901,.T.);
#53734=EDGE_CURVE('',#41809,#41808,#33902,.T.);
#53735=EDGE_CURVE('',#41810,#41809,#33903,.T.);
#53736=EDGE_CURVE('',#41810,#41805,#22597,.T.);
#53737=EDGE_CURVE('',#41808,#41811,#22598,.T.);
#53738=EDGE_CURVE('',#41811,#41812,#33904,.T.);
#53739=EDGE_CURVE('',#41812,#41809,#22599,.T.);
#53740=EDGE_CURVE('',#40820,#41794,#33905,.T.);
#53741=EDGE_CURVE('',#41793,#40821,#33906,.T.);
#53742=EDGE_CURVE('',#41811,#40629,#1604,.T.);
#53743=EDGE_CURVE('',#40628,#41812,#1605,.T.);
#53744=EDGE_CURVE('',#41803,#41806,#1606,.T.);
#53745=EDGE_CURVE('',#41805,#41804,#1607,.T.);
#53746=EDGE_CURVE('',#41799,#41802,#1608,.T.);
#53747=EDGE_CURVE('',#41801,#41800,#1609,.T.);
#53748=EDGE_CURVE('',#41813,#41814,#33907,.T.);
#53749=EDGE_CURVE('',#41814,#41815,#22600,.T.);
#53750=EDGE_CURVE('',#41816,#41815,#33908,.T.);
#53751=EDGE_CURVE('',#41817,#41816,#33909,.T.);
#53752=EDGE_CURVE('',#41818,#41817,#33910,.T.);
#53753=EDGE_CURVE('',#41818,#41813,#22601,.T.);
#53754=EDGE_CURVE('',#41816,#41819,#22602,.T.);
#53755=EDGE_CURVE('',#41819,#41820,#33911,.T.);
#53756=EDGE_CURVE('',#41820,#41817,#22603,.T.);
#53757=EDGE_CURVE('',#41821,#41822,#33912,.T.);
#53758=EDGE_CURVE('',#41822,#41823,#22604,.T.);
#53759=EDGE_CURVE('',#41823,#41824,#33913,.T.);
#53760=EDGE_CURVE('',#41824,#41821,#22605,.T.);
#53761=EDGE_CURVE('',#41825,#41826,#33914,.T.);
#53762=EDGE_CURVE('',#41826,#41827,#22606,.T.);
#53763=EDGE_CURVE('',#41828,#41827,#33915,.T.);
#53764=EDGE_CURVE('',#41829,#41828,#33916,.T.);
#53765=EDGE_CURVE('',#41830,#41829,#33917,.T.);
#53766=EDGE_CURVE('',#41830,#41825,#22607,.T.);
#53767=EDGE_CURVE('',#41828,#41831,#22608,.T.);
#53768=EDGE_CURVE('',#41831,#41832,#33918,.T.);
#53769=EDGE_CURVE('',#41832,#41829,#22609,.T.);
#53770=EDGE_CURVE('',#40826,#41814,#33919,.T.);
#53771=EDGE_CURVE('',#41813,#40827,#33920,.T.);
#53772=EDGE_CURVE('',#41831,#40623,#1610,.T.);
#53773=EDGE_CURVE('',#40622,#41832,#1611,.T.);
#53774=EDGE_CURVE('',#41823,#41826,#1612,.T.);
#53775=EDGE_CURVE('',#41825,#41824,#1613,.T.);
#53776=EDGE_CURVE('',#41819,#41822,#1614,.T.);
#53777=EDGE_CURVE('',#41821,#41820,#1615,.T.);
#53778=EDGE_CURVE('',#41833,#41834,#33921,.T.);
#53779=EDGE_CURVE('',#41834,#41835,#22610,.T.);
#53780=EDGE_CURVE('',#41836,#41835,#33922,.T.);
#53781=EDGE_CURVE('',#41837,#41836,#33923,.T.);
#53782=EDGE_CURVE('',#41838,#41837,#33924,.T.);
#53783=EDGE_CURVE('',#41838,#41833,#22611,.T.);
#53784=EDGE_CURVE('',#41836,#41839,#22612,.T.);
#53785=EDGE_CURVE('',#41839,#41840,#33925,.T.);
#53786=EDGE_CURVE('',#41840,#41837,#22613,.T.);
#53787=EDGE_CURVE('',#41841,#41842,#33926,.T.);
#53788=EDGE_CURVE('',#41842,#41843,#22614,.T.);
#53789=EDGE_CURVE('',#41843,#41844,#33927,.T.);
#53790=EDGE_CURVE('',#41844,#41841,#22615,.T.);
#53791=EDGE_CURVE('',#41845,#41846,#33928,.T.);
#53792=EDGE_CURVE('',#41846,#41847,#22616,.T.);
#53793=EDGE_CURVE('',#41848,#41847,#33929,.T.);
#53794=EDGE_CURVE('',#41849,#41848,#33930,.T.);
#53795=EDGE_CURVE('',#41850,#41849,#33931,.T.);
#53796=EDGE_CURVE('',#41850,#41845,#22617,.T.);
#53797=EDGE_CURVE('',#41848,#41851,#22618,.T.);
#53798=EDGE_CURVE('',#41851,#41852,#33932,.T.);
#53799=EDGE_CURVE('',#41852,#41849,#22619,.T.);
#53800=EDGE_CURVE('',#40832,#41834,#33933,.T.);
#53801=EDGE_CURVE('',#41833,#40833,#33934,.T.);
#53802=EDGE_CURVE('',#41851,#40617,#1616,.T.);
#53803=EDGE_CURVE('',#40616,#41852,#1617,.T.);
#53804=EDGE_CURVE('',#41843,#41846,#1618,.T.);
#53805=EDGE_CURVE('',#41845,#41844,#1619,.T.);
#53806=EDGE_CURVE('',#41839,#41842,#1620,.T.);
#53807=EDGE_CURVE('',#41841,#41840,#1621,.T.);
#53808=EDGE_CURVE('',#41853,#41854,#33935,.T.);
#53809=EDGE_CURVE('',#41854,#41855,#22620,.T.);
#53810=EDGE_CURVE('',#41856,#41855,#33936,.T.);
#53811=EDGE_CURVE('',#41857,#41856,#33937,.T.);
#53812=EDGE_CURVE('',#41858,#41857,#33938,.T.);
#53813=EDGE_CURVE('',#41858,#41853,#22621,.T.);
#53814=EDGE_CURVE('',#41856,#41859,#22622,.T.);
#53815=EDGE_CURVE('',#41859,#41860,#33939,.T.);
#53816=EDGE_CURVE('',#41860,#41857,#22623,.T.);
#53817=EDGE_CURVE('',#41861,#41862,#33940,.T.);
#53818=EDGE_CURVE('',#41862,#41863,#22624,.T.);
#53819=EDGE_CURVE('',#41863,#41864,#33941,.T.);
#53820=EDGE_CURVE('',#41864,#41861,#22625,.T.);
#53821=EDGE_CURVE('',#41865,#41866,#33942,.T.);
#53822=EDGE_CURVE('',#41866,#41867,#22626,.T.);
#53823=EDGE_CURVE('',#41868,#41867,#33943,.T.);
#53824=EDGE_CURVE('',#41869,#41868,#33944,.T.);
#53825=EDGE_CURVE('',#41870,#41869,#33945,.T.);
#53826=EDGE_CURVE('',#41870,#41865,#22627,.T.);
#53827=EDGE_CURVE('',#41868,#41871,#22628,.T.);
#53828=EDGE_CURVE('',#41871,#41872,#33946,.T.);
#53829=EDGE_CURVE('',#41872,#41869,#22629,.T.);
#53830=EDGE_CURVE('',#40838,#41854,#33947,.T.);
#53831=EDGE_CURVE('',#41853,#40839,#33948,.T.);
#53832=EDGE_CURVE('',#41871,#40611,#1622,.T.);
#53833=EDGE_CURVE('',#40610,#41872,#1623,.T.);
#53834=EDGE_CURVE('',#41863,#41866,#1624,.T.);
#53835=EDGE_CURVE('',#41865,#41864,#1625,.T.);
#53836=EDGE_CURVE('',#41859,#41862,#1626,.T.);
#53837=EDGE_CURVE('',#41861,#41860,#1627,.T.);
#53838=EDGE_CURVE('',#41873,#41874,#33949,.T.);
#53839=EDGE_CURVE('',#41874,#41875,#22630,.T.);
#53840=EDGE_CURVE('',#41876,#41875,#33950,.T.);
#53841=EDGE_CURVE('',#41877,#41876,#33951,.T.);
#53842=EDGE_CURVE('',#41878,#41877,#33952,.T.);
#53843=EDGE_CURVE('',#41878,#41873,#22631,.T.);
#53844=EDGE_CURVE('',#41876,#41879,#22632,.T.);
#53845=EDGE_CURVE('',#41879,#41880,#33953,.T.);
#53846=EDGE_CURVE('',#41880,#41877,#22633,.T.);
#53847=EDGE_CURVE('',#41881,#41882,#33954,.T.);
#53848=EDGE_CURVE('',#41882,#41883,#22634,.T.);
#53849=EDGE_CURVE('',#41883,#41884,#33955,.T.);
#53850=EDGE_CURVE('',#41884,#41881,#22635,.T.);
#53851=EDGE_CURVE('',#41885,#41886,#33956,.T.);
#53852=EDGE_CURVE('',#41886,#41887,#22636,.T.);
#53853=EDGE_CURVE('',#41888,#41887,#33957,.T.);
#53854=EDGE_CURVE('',#41889,#41888,#33958,.T.);
#53855=EDGE_CURVE('',#41890,#41889,#33959,.T.);
#53856=EDGE_CURVE('',#41890,#41885,#22637,.T.);
#53857=EDGE_CURVE('',#41888,#41891,#22638,.T.);
#53858=EDGE_CURVE('',#41891,#41892,#33960,.T.);
#53859=EDGE_CURVE('',#41892,#41889,#22639,.T.);
#53860=EDGE_CURVE('',#40844,#41874,#33961,.T.);
#53861=EDGE_CURVE('',#41873,#40845,#33962,.T.);
#53862=EDGE_CURVE('',#41891,#40605,#1628,.T.);
#53863=EDGE_CURVE('',#40604,#41892,#1629,.T.);
#53864=EDGE_CURVE('',#41883,#41886,#1630,.T.);
#53865=EDGE_CURVE('',#41885,#41884,#1631,.T.);
#53866=EDGE_CURVE('',#41879,#41882,#1632,.T.);
#53867=EDGE_CURVE('',#41881,#41880,#1633,.T.);
#53868=EDGE_CURVE('',#41893,#41894,#33963,.T.);
#53869=EDGE_CURVE('',#41894,#41895,#22640,.T.);
#53870=EDGE_CURVE('',#41896,#41895,#33964,.T.);
#53871=EDGE_CURVE('',#41897,#41896,#33965,.T.);
#53872=EDGE_CURVE('',#41898,#41897,#33966,.T.);
#53873=EDGE_CURVE('',#41898,#41893,#22641,.T.);
#53874=EDGE_CURVE('',#41896,#41899,#22642,.T.);
#53875=EDGE_CURVE('',#41899,#41900,#33967,.T.);
#53876=EDGE_CURVE('',#41900,#41897,#22643,.T.);
#53877=EDGE_CURVE('',#41901,#41902,#33968,.T.);
#53878=EDGE_CURVE('',#41902,#41903,#22644,.T.);
#53879=EDGE_CURVE('',#41903,#41904,#33969,.T.);
#53880=EDGE_CURVE('',#41904,#41901,#22645,.T.);
#53881=EDGE_CURVE('',#41905,#41906,#33970,.T.);
#53882=EDGE_CURVE('',#41906,#41907,#22646,.T.);
#53883=EDGE_CURVE('',#41908,#41907,#33971,.T.);
#53884=EDGE_CURVE('',#41909,#41908,#33972,.T.);
#53885=EDGE_CURVE('',#41910,#41909,#33973,.T.);
#53886=EDGE_CURVE('',#41910,#41905,#22647,.T.);
#53887=EDGE_CURVE('',#41908,#41911,#22648,.T.);
#53888=EDGE_CURVE('',#41911,#41912,#33974,.T.);
#53889=EDGE_CURVE('',#41912,#41909,#22649,.T.);
#53890=EDGE_CURVE('',#40850,#41894,#33975,.T.);
#53891=EDGE_CURVE('',#41893,#40851,#33976,.T.);
#53892=EDGE_CURVE('',#41911,#40599,#1634,.T.);
#53893=EDGE_CURVE('',#40598,#41912,#1635,.T.);
#53894=EDGE_CURVE('',#41903,#41906,#1636,.T.);
#53895=EDGE_CURVE('',#41905,#41904,#1637,.T.);
#53896=EDGE_CURVE('',#41899,#41902,#1638,.T.);
#53897=EDGE_CURVE('',#41901,#41900,#1639,.T.);
#53898=EDGE_CURVE('',#41913,#41914,#33977,.T.);
#53899=EDGE_CURVE('',#41914,#41915,#22650,.T.);
#53900=EDGE_CURVE('',#41916,#41915,#33978,.T.);
#53901=EDGE_CURVE('',#41917,#41916,#33979,.T.);
#53902=EDGE_CURVE('',#41918,#41917,#33980,.T.);
#53903=EDGE_CURVE('',#41918,#41913,#22651,.T.);
#53904=EDGE_CURVE('',#41916,#41919,#22652,.T.);
#53905=EDGE_CURVE('',#41919,#41920,#33981,.T.);
#53906=EDGE_CURVE('',#41920,#41917,#22653,.T.);
#53907=EDGE_CURVE('',#41921,#41922,#33982,.T.);
#53908=EDGE_CURVE('',#41922,#41923,#22654,.T.);
#53909=EDGE_CURVE('',#41923,#41924,#33983,.T.);
#53910=EDGE_CURVE('',#41924,#41921,#22655,.T.);
#53911=EDGE_CURVE('',#41925,#41926,#33984,.T.);
#53912=EDGE_CURVE('',#41926,#41927,#22656,.T.);
#53913=EDGE_CURVE('',#41928,#41927,#33985,.T.);
#53914=EDGE_CURVE('',#41929,#41928,#33986,.T.);
#53915=EDGE_CURVE('',#41930,#41929,#33987,.T.);
#53916=EDGE_CURVE('',#41930,#41925,#22657,.T.);
#53917=EDGE_CURVE('',#41928,#41931,#22658,.T.);
#53918=EDGE_CURVE('',#41931,#41932,#33988,.T.);
#53919=EDGE_CURVE('',#41932,#41929,#22659,.T.);
#53920=EDGE_CURVE('',#40856,#41914,#33989,.T.);
#53921=EDGE_CURVE('',#41913,#40857,#33990,.T.);
#53922=EDGE_CURVE('',#41931,#40593,#1640,.T.);
#53923=EDGE_CURVE('',#40592,#41932,#1641,.T.);
#53924=EDGE_CURVE('',#41923,#41926,#1642,.T.);
#53925=EDGE_CURVE('',#41925,#41924,#1643,.T.);
#53926=EDGE_CURVE('',#41919,#41922,#1644,.T.);
#53927=EDGE_CURVE('',#41921,#41920,#1645,.T.);
#53928=EDGE_CURVE('',#41933,#41934,#33991,.T.);
#53929=EDGE_CURVE('',#41934,#41935,#22660,.T.);
#53930=EDGE_CURVE('',#41936,#41935,#33992,.T.);
#53931=EDGE_CURVE('',#41937,#41936,#33993,.T.);
#53932=EDGE_CURVE('',#41938,#41937,#33994,.T.);
#53933=EDGE_CURVE('',#41938,#41933,#22661,.T.);
#53934=EDGE_CURVE('',#41936,#41939,#22662,.T.);
#53935=EDGE_CURVE('',#41939,#41940,#33995,.T.);
#53936=EDGE_CURVE('',#41940,#41937,#22663,.T.);
#53937=EDGE_CURVE('',#41941,#41942,#33996,.T.);
#53938=EDGE_CURVE('',#41942,#41943,#22664,.T.);
#53939=EDGE_CURVE('',#41943,#41944,#33997,.T.);
#53940=EDGE_CURVE('',#41944,#41941,#22665,.T.);
#53941=EDGE_CURVE('',#41945,#41946,#33998,.T.);
#53942=EDGE_CURVE('',#41946,#41947,#22666,.T.);
#53943=EDGE_CURVE('',#41948,#41947,#33999,.T.);
#53944=EDGE_CURVE('',#41949,#41948,#34000,.T.);
#53945=EDGE_CURVE('',#41950,#41949,#34001,.T.);
#53946=EDGE_CURVE('',#41950,#41945,#22667,.T.);
#53947=EDGE_CURVE('',#41948,#41951,#22668,.T.);
#53948=EDGE_CURVE('',#41951,#41952,#34002,.T.);
#53949=EDGE_CURVE('',#41952,#41949,#22669,.T.);
#53950=EDGE_CURVE('',#40862,#41934,#34003,.T.);
#53951=EDGE_CURVE('',#41933,#40863,#34004,.T.);
#53952=EDGE_CURVE('',#41951,#40587,#1646,.T.);
#53953=EDGE_CURVE('',#40586,#41952,#1647,.T.);
#53954=EDGE_CURVE('',#41943,#41946,#1648,.T.);
#53955=EDGE_CURVE('',#41945,#41944,#1649,.T.);
#53956=EDGE_CURVE('',#41939,#41942,#1650,.T.);
#53957=EDGE_CURVE('',#41941,#41940,#1651,.T.);
#53958=EDGE_CURVE('',#41953,#41954,#34005,.T.);
#53959=EDGE_CURVE('',#41954,#41955,#22670,.T.);
#53960=EDGE_CURVE('',#41956,#41955,#34006,.T.);
#53961=EDGE_CURVE('',#41957,#41956,#34007,.T.);
#53962=EDGE_CURVE('',#41958,#41957,#34008,.T.);
#53963=EDGE_CURVE('',#41958,#41953,#22671,.T.);
#53964=EDGE_CURVE('',#41956,#41959,#22672,.T.);
#53965=EDGE_CURVE('',#41959,#41960,#34009,.T.);
#53966=EDGE_CURVE('',#41960,#41957,#22673,.T.);
#53967=EDGE_CURVE('',#41961,#41962,#34010,.T.);
#53968=EDGE_CURVE('',#41962,#41963,#22674,.T.);
#53969=EDGE_CURVE('',#41963,#41964,#34011,.T.);
#53970=EDGE_CURVE('',#41964,#41961,#22675,.T.);
#53971=EDGE_CURVE('',#41965,#41966,#34012,.T.);
#53972=EDGE_CURVE('',#41966,#41967,#22676,.T.);
#53973=EDGE_CURVE('',#41968,#41967,#34013,.T.);
#53974=EDGE_CURVE('',#41969,#41968,#34014,.T.);
#53975=EDGE_CURVE('',#41970,#41969,#34015,.T.);
#53976=EDGE_CURVE('',#41970,#41965,#22677,.T.);
#53977=EDGE_CURVE('',#41968,#41971,#22678,.T.);
#53978=EDGE_CURVE('',#41971,#41972,#34016,.T.);
#53979=EDGE_CURVE('',#41972,#41969,#22679,.T.);
#53980=EDGE_CURVE('',#40868,#41954,#34017,.T.);
#53981=EDGE_CURVE('',#41953,#40869,#34018,.T.);
#53982=EDGE_CURVE('',#41971,#40581,#1652,.T.);
#53983=EDGE_CURVE('',#40580,#41972,#1653,.T.);
#53984=EDGE_CURVE('',#41963,#41966,#1654,.T.);
#53985=EDGE_CURVE('',#41965,#41964,#1655,.T.);
#53986=EDGE_CURVE('',#41959,#41962,#1656,.T.);
#53987=EDGE_CURVE('',#41961,#41960,#1657,.T.);
#53988=EDGE_CURVE('',#41973,#41974,#34019,.T.);
#53989=EDGE_CURVE('',#41974,#41975,#22680,.T.);
#53990=EDGE_CURVE('',#41976,#41975,#34020,.T.);
#53991=EDGE_CURVE('',#41977,#41976,#34021,.T.);
#53992=EDGE_CURVE('',#41978,#41977,#34022,.T.);
#53993=EDGE_CURVE('',#41978,#41973,#22681,.T.);
#53994=EDGE_CURVE('',#41976,#41979,#22682,.T.);
#53995=EDGE_CURVE('',#41979,#41980,#34023,.T.);
#53996=EDGE_CURVE('',#41980,#41977,#22683,.T.);
#53997=EDGE_CURVE('',#41981,#41982,#34024,.T.);
#53998=EDGE_CURVE('',#41982,#41983,#22684,.T.);
#53999=EDGE_CURVE('',#41983,#41984,#34025,.T.);
#54000=EDGE_CURVE('',#41984,#41981,#22685,.T.);
#54001=EDGE_CURVE('',#41985,#41986,#34026,.T.);
#54002=EDGE_CURVE('',#41986,#41987,#22686,.T.);
#54003=EDGE_CURVE('',#41988,#41987,#34027,.T.);
#54004=EDGE_CURVE('',#41989,#41988,#34028,.T.);
#54005=EDGE_CURVE('',#41990,#41989,#34029,.T.);
#54006=EDGE_CURVE('',#41990,#41985,#22687,.T.);
#54007=EDGE_CURVE('',#41988,#41991,#22688,.T.);
#54008=EDGE_CURVE('',#41991,#41992,#34030,.T.);
#54009=EDGE_CURVE('',#41992,#41989,#22689,.T.);
#54010=EDGE_CURVE('',#40874,#41974,#34031,.T.);
#54011=EDGE_CURVE('',#41973,#40875,#34032,.T.);
#54012=EDGE_CURVE('',#41991,#40575,#1658,.T.);
#54013=EDGE_CURVE('',#40574,#41992,#1659,.T.);
#54014=EDGE_CURVE('',#41983,#41986,#1660,.T.);
#54015=EDGE_CURVE('',#41985,#41984,#1661,.T.);
#54016=EDGE_CURVE('',#41979,#41982,#1662,.T.);
#54017=EDGE_CURVE('',#41981,#41980,#1663,.T.);
#54018=EDGE_CURVE('',#41993,#41994,#34033,.T.);
#54019=EDGE_CURVE('',#41994,#41995,#22690,.T.);
#54020=EDGE_CURVE('',#41996,#41995,#34034,.T.);
#54021=EDGE_CURVE('',#41997,#41996,#34035,.T.);
#54022=EDGE_CURVE('',#41998,#41997,#34036,.T.);
#54023=EDGE_CURVE('',#41998,#41993,#22691,.T.);
#54024=EDGE_CURVE('',#41996,#41999,#22692,.T.);
#54025=EDGE_CURVE('',#41999,#42000,#34037,.T.);
#54026=EDGE_CURVE('',#42000,#41997,#22693,.T.);
#54027=EDGE_CURVE('',#42001,#42002,#34038,.T.);
#54028=EDGE_CURVE('',#42002,#42003,#22694,.T.);
#54029=EDGE_CURVE('',#42003,#42004,#34039,.T.);
#54030=EDGE_CURVE('',#42004,#42001,#22695,.T.);
#54031=EDGE_CURVE('',#42005,#42006,#34040,.T.);
#54032=EDGE_CURVE('',#42006,#42007,#22696,.T.);
#54033=EDGE_CURVE('',#42008,#42007,#34041,.T.);
#54034=EDGE_CURVE('',#42009,#42008,#34042,.T.);
#54035=EDGE_CURVE('',#42010,#42009,#34043,.T.);
#54036=EDGE_CURVE('',#42010,#42005,#22697,.T.);
#54037=EDGE_CURVE('',#42008,#42011,#22698,.T.);
#54038=EDGE_CURVE('',#42011,#42012,#34044,.T.);
#54039=EDGE_CURVE('',#42012,#42009,#22699,.T.);
#54040=EDGE_CURVE('',#40880,#41994,#34045,.T.);
#54041=EDGE_CURVE('',#41993,#40881,#34046,.T.);
#54042=EDGE_CURVE('',#42011,#40569,#1664,.T.);
#54043=EDGE_CURVE('',#40568,#42012,#1665,.T.);
#54044=EDGE_CURVE('',#42003,#42006,#1666,.T.);
#54045=EDGE_CURVE('',#42005,#42004,#1667,.T.);
#54046=EDGE_CURVE('',#41999,#42002,#1668,.T.);
#54047=EDGE_CURVE('',#42001,#42000,#1669,.T.);
#54048=EDGE_CURVE('',#42013,#42014,#34047,.T.);
#54049=EDGE_CURVE('',#42014,#42015,#22700,.T.);
#54050=EDGE_CURVE('',#42016,#42015,#34048,.T.);
#54051=EDGE_CURVE('',#42017,#42016,#34049,.T.);
#54052=EDGE_CURVE('',#42018,#42017,#34050,.T.);
#54053=EDGE_CURVE('',#42018,#42013,#22701,.T.);
#54054=EDGE_CURVE('',#42016,#42019,#22702,.T.);
#54055=EDGE_CURVE('',#42019,#42020,#34051,.T.);
#54056=EDGE_CURVE('',#42020,#42017,#22703,.T.);
#54057=EDGE_CURVE('',#42021,#42022,#34052,.T.);
#54058=EDGE_CURVE('',#42022,#42023,#22704,.T.);
#54059=EDGE_CURVE('',#42023,#42024,#34053,.T.);
#54060=EDGE_CURVE('',#42024,#42021,#22705,.T.);
#54061=EDGE_CURVE('',#42025,#42026,#34054,.T.);
#54062=EDGE_CURVE('',#42026,#42027,#22706,.T.);
#54063=EDGE_CURVE('',#42028,#42027,#34055,.T.);
#54064=EDGE_CURVE('',#42029,#42028,#34056,.T.);
#54065=EDGE_CURVE('',#42030,#42029,#34057,.T.);
#54066=EDGE_CURVE('',#42030,#42025,#22707,.T.);
#54067=EDGE_CURVE('',#42028,#42031,#22708,.T.);
#54068=EDGE_CURVE('',#42031,#42032,#34058,.T.);
#54069=EDGE_CURVE('',#42032,#42029,#22709,.T.);
#54070=EDGE_CURVE('',#40886,#42014,#34059,.T.);
#54071=EDGE_CURVE('',#42013,#40887,#34060,.T.);
#54072=EDGE_CURVE('',#42031,#40563,#1670,.T.);
#54073=EDGE_CURVE('',#40562,#42032,#1671,.T.);
#54074=EDGE_CURVE('',#42023,#42026,#1672,.T.);
#54075=EDGE_CURVE('',#42025,#42024,#1673,.T.);
#54076=EDGE_CURVE('',#42019,#42022,#1674,.T.);
#54077=EDGE_CURVE('',#42021,#42020,#1675,.T.);
#54078=EDGE_CURVE('',#42033,#42034,#34061,.T.);
#54079=EDGE_CURVE('',#42034,#42035,#22710,.T.);
#54080=EDGE_CURVE('',#42036,#42035,#34062,.T.);
#54081=EDGE_CURVE('',#42037,#42036,#34063,.T.);
#54082=EDGE_CURVE('',#42038,#42037,#34064,.T.);
#54083=EDGE_CURVE('',#42038,#42033,#22711,.T.);
#54084=EDGE_CURVE('',#42036,#42039,#22712,.T.);
#54085=EDGE_CURVE('',#42039,#42040,#34065,.T.);
#54086=EDGE_CURVE('',#42040,#42037,#22713,.T.);
#54087=EDGE_CURVE('',#42041,#42042,#34066,.T.);
#54088=EDGE_CURVE('',#42042,#42043,#22714,.T.);
#54089=EDGE_CURVE('',#42043,#42044,#34067,.T.);
#54090=EDGE_CURVE('',#42044,#42041,#22715,.T.);
#54091=EDGE_CURVE('',#42045,#42046,#34068,.T.);
#54092=EDGE_CURVE('',#42046,#42047,#22716,.T.);
#54093=EDGE_CURVE('',#42048,#42047,#34069,.T.);
#54094=EDGE_CURVE('',#42049,#42048,#34070,.T.);
#54095=EDGE_CURVE('',#42050,#42049,#34071,.T.);
#54096=EDGE_CURVE('',#42050,#42045,#22717,.T.);
#54097=EDGE_CURVE('',#42048,#42051,#22718,.T.);
#54098=EDGE_CURVE('',#42051,#42052,#34072,.T.);
#54099=EDGE_CURVE('',#42052,#42049,#22719,.T.);
#54100=EDGE_CURVE('',#40892,#42034,#34073,.T.);
#54101=EDGE_CURVE('',#42033,#40893,#34074,.T.);
#54102=EDGE_CURVE('',#42051,#40557,#1676,.T.);
#54103=EDGE_CURVE('',#40556,#42052,#1677,.T.);
#54104=EDGE_CURVE('',#42043,#42046,#1678,.T.);
#54105=EDGE_CURVE('',#42045,#42044,#1679,.T.);
#54106=EDGE_CURVE('',#42039,#42042,#1680,.T.);
#54107=EDGE_CURVE('',#42041,#42040,#1681,.T.);
#54108=EDGE_CURVE('',#42053,#42054,#34075,.T.);
#54109=EDGE_CURVE('',#42054,#42055,#22720,.T.);
#54110=EDGE_CURVE('',#42056,#42055,#34076,.T.);
#54111=EDGE_CURVE('',#42057,#42056,#34077,.T.);
#54112=EDGE_CURVE('',#42058,#42057,#34078,.T.);
#54113=EDGE_CURVE('',#42058,#42053,#22721,.T.);
#54114=EDGE_CURVE('',#42056,#42059,#22722,.T.);
#54115=EDGE_CURVE('',#42059,#42060,#34079,.T.);
#54116=EDGE_CURVE('',#42060,#42057,#22723,.T.);
#54117=EDGE_CURVE('',#42061,#42062,#34080,.T.);
#54118=EDGE_CURVE('',#42062,#42063,#22724,.T.);
#54119=EDGE_CURVE('',#42063,#42064,#34081,.T.);
#54120=EDGE_CURVE('',#42064,#42061,#22725,.T.);
#54121=EDGE_CURVE('',#42065,#42066,#34082,.T.);
#54122=EDGE_CURVE('',#42066,#42067,#22726,.T.);
#54123=EDGE_CURVE('',#42068,#42067,#34083,.T.);
#54124=EDGE_CURVE('',#42069,#42068,#34084,.T.);
#54125=EDGE_CURVE('',#42070,#42069,#34085,.T.);
#54126=EDGE_CURVE('',#42070,#42065,#22727,.T.);
#54127=EDGE_CURVE('',#42068,#42071,#22728,.T.);
#54128=EDGE_CURVE('',#42071,#42072,#34086,.T.);
#54129=EDGE_CURVE('',#42072,#42069,#22729,.T.);
#54130=EDGE_CURVE('',#40898,#42054,#34087,.T.);
#54131=EDGE_CURVE('',#42053,#40899,#34088,.T.);
#54132=EDGE_CURVE('',#42071,#40551,#1682,.T.);
#54133=EDGE_CURVE('',#40550,#42072,#1683,.T.);
#54134=EDGE_CURVE('',#42063,#42066,#1684,.T.);
#54135=EDGE_CURVE('',#42065,#42064,#1685,.T.);
#54136=EDGE_CURVE('',#42059,#42062,#1686,.T.);
#54137=EDGE_CURVE('',#42061,#42060,#1687,.T.);
#54138=EDGE_CURVE('',#42073,#42074,#34089,.T.);
#54139=EDGE_CURVE('',#42074,#42075,#22730,.T.);
#54140=EDGE_CURVE('',#42076,#42075,#34090,.T.);
#54141=EDGE_CURVE('',#42077,#42076,#34091,.T.);
#54142=EDGE_CURVE('',#42078,#42077,#34092,.T.);
#54143=EDGE_CURVE('',#42078,#42073,#22731,.T.);
#54144=EDGE_CURVE('',#42076,#42079,#22732,.T.);
#54145=EDGE_CURVE('',#42079,#42080,#34093,.T.);
#54146=EDGE_CURVE('',#42080,#42077,#22733,.T.);
#54147=EDGE_CURVE('',#42081,#42082,#34094,.T.);
#54148=EDGE_CURVE('',#42082,#42083,#22734,.T.);
#54149=EDGE_CURVE('',#42083,#42084,#34095,.T.);
#54150=EDGE_CURVE('',#42084,#42081,#22735,.T.);
#54151=EDGE_CURVE('',#42085,#42086,#34096,.T.);
#54152=EDGE_CURVE('',#42086,#42087,#22736,.T.);
#54153=EDGE_CURVE('',#42088,#42087,#34097,.T.);
#54154=EDGE_CURVE('',#42089,#42088,#34098,.T.);
#54155=EDGE_CURVE('',#42090,#42089,#34099,.T.);
#54156=EDGE_CURVE('',#42090,#42085,#22737,.T.);
#54157=EDGE_CURVE('',#42088,#42091,#22738,.T.);
#54158=EDGE_CURVE('',#42091,#42092,#34100,.T.);
#54159=EDGE_CURVE('',#42092,#42089,#22739,.T.);
#54160=EDGE_CURVE('',#40904,#42074,#34101,.T.);
#54161=EDGE_CURVE('',#42073,#40905,#34102,.T.);
#54162=EDGE_CURVE('',#42091,#40545,#1688,.T.);
#54163=EDGE_CURVE('',#40544,#42092,#1689,.T.);
#54164=EDGE_CURVE('',#42083,#42086,#1690,.T.);
#54165=EDGE_CURVE('',#42085,#42084,#1691,.T.);
#54166=EDGE_CURVE('',#42079,#42082,#1692,.T.);
#54167=EDGE_CURVE('',#42081,#42080,#1693,.T.);
#54168=EDGE_CURVE('',#42093,#42094,#34103,.T.);
#54169=EDGE_CURVE('',#42094,#42095,#22740,.T.);
#54170=EDGE_CURVE('',#42096,#42095,#34104,.T.);
#54171=EDGE_CURVE('',#42097,#42096,#34105,.T.);
#54172=EDGE_CURVE('',#42098,#42097,#34106,.T.);
#54173=EDGE_CURVE('',#42098,#42093,#22741,.T.);
#54174=EDGE_CURVE('',#42096,#42099,#22742,.T.);
#54175=EDGE_CURVE('',#42099,#42100,#34107,.T.);
#54176=EDGE_CURVE('',#42100,#42097,#22743,.T.);
#54177=EDGE_CURVE('',#42101,#42102,#34108,.T.);
#54178=EDGE_CURVE('',#42102,#42103,#22744,.T.);
#54179=EDGE_CURVE('',#42103,#42104,#34109,.T.);
#54180=EDGE_CURVE('',#42104,#42101,#22745,.T.);
#54181=EDGE_CURVE('',#42105,#42106,#34110,.T.);
#54182=EDGE_CURVE('',#42106,#42107,#22746,.T.);
#54183=EDGE_CURVE('',#42108,#42107,#34111,.T.);
#54184=EDGE_CURVE('',#42109,#42108,#34112,.T.);
#54185=EDGE_CURVE('',#42110,#42109,#34113,.T.);
#54186=EDGE_CURVE('',#42110,#42105,#22747,.T.);
#54187=EDGE_CURVE('',#42108,#42111,#22748,.T.);
#54188=EDGE_CURVE('',#42111,#42112,#34114,.T.);
#54189=EDGE_CURVE('',#42112,#42109,#22749,.T.);
#54190=EDGE_CURVE('',#40910,#42094,#34115,.T.);
#54191=EDGE_CURVE('',#42093,#40911,#34116,.T.);
#54192=EDGE_CURVE('',#42111,#40539,#1694,.T.);
#54193=EDGE_CURVE('',#40538,#42112,#1695,.T.);
#54194=EDGE_CURVE('',#42103,#42106,#1696,.T.);
#54195=EDGE_CURVE('',#42105,#42104,#1697,.T.);
#54196=EDGE_CURVE('',#42099,#42102,#1698,.T.);
#54197=EDGE_CURVE('',#42101,#42100,#1699,.T.);
#54198=EDGE_CURVE('',#42113,#42114,#34117,.T.);
#54199=EDGE_CURVE('',#42114,#42115,#22750,.T.);
#54200=EDGE_CURVE('',#42116,#42115,#34118,.T.);
#54201=EDGE_CURVE('',#42117,#42116,#34119,.T.);
#54202=EDGE_CURVE('',#42118,#42117,#34120,.T.);
#54203=EDGE_CURVE('',#42118,#42113,#22751,.T.);
#54204=EDGE_CURVE('',#42116,#42119,#22752,.T.);
#54205=EDGE_CURVE('',#42119,#42120,#34121,.T.);
#54206=EDGE_CURVE('',#42120,#42117,#22753,.T.);
#54207=EDGE_CURVE('',#42121,#42122,#34122,.T.);
#54208=EDGE_CURVE('',#42122,#42123,#22754,.T.);
#54209=EDGE_CURVE('',#42123,#42124,#34123,.T.);
#54210=EDGE_CURVE('',#42124,#42121,#22755,.T.);
#54211=EDGE_CURVE('',#42125,#42126,#34124,.T.);
#54212=EDGE_CURVE('',#42126,#42127,#22756,.T.);
#54213=EDGE_CURVE('',#42128,#42127,#34125,.T.);
#54214=EDGE_CURVE('',#42129,#42128,#34126,.T.);
#54215=EDGE_CURVE('',#42130,#42129,#34127,.T.);
#54216=EDGE_CURVE('',#42130,#42125,#22757,.T.);
#54217=EDGE_CURVE('',#42128,#42131,#22758,.T.);
#54218=EDGE_CURVE('',#42131,#42132,#34128,.T.);
#54219=EDGE_CURVE('',#42132,#42129,#22759,.T.);
#54220=EDGE_CURVE('',#40916,#42114,#34129,.T.);
#54221=EDGE_CURVE('',#42113,#40917,#34130,.T.);
#54222=EDGE_CURVE('',#42131,#40533,#1700,.T.);
#54223=EDGE_CURVE('',#40532,#42132,#1701,.T.);
#54224=EDGE_CURVE('',#42123,#42126,#1702,.T.);
#54225=EDGE_CURVE('',#42125,#42124,#1703,.T.);
#54226=EDGE_CURVE('',#42119,#42122,#1704,.T.);
#54227=EDGE_CURVE('',#42121,#42120,#1705,.T.);
#54228=EDGE_CURVE('',#42133,#42134,#34131,.T.);
#54229=EDGE_CURVE('',#42134,#42135,#22760,.T.);
#54230=EDGE_CURVE('',#42136,#42135,#34132,.T.);
#54231=EDGE_CURVE('',#42137,#42136,#34133,.T.);
#54232=EDGE_CURVE('',#42138,#42137,#34134,.T.);
#54233=EDGE_CURVE('',#42138,#42133,#22761,.T.);
#54234=EDGE_CURVE('',#42136,#42139,#22762,.T.);
#54235=EDGE_CURVE('',#42139,#42140,#34135,.T.);
#54236=EDGE_CURVE('',#42140,#42137,#22763,.T.);
#54237=EDGE_CURVE('',#42141,#42142,#34136,.T.);
#54238=EDGE_CURVE('',#42142,#42143,#22764,.T.);
#54239=EDGE_CURVE('',#42143,#42144,#34137,.T.);
#54240=EDGE_CURVE('',#42144,#42141,#22765,.T.);
#54241=EDGE_CURVE('',#42145,#42146,#34138,.T.);
#54242=EDGE_CURVE('',#42146,#42147,#22766,.T.);
#54243=EDGE_CURVE('',#42148,#42147,#34139,.T.);
#54244=EDGE_CURVE('',#42149,#42148,#34140,.T.);
#54245=EDGE_CURVE('',#42150,#42149,#34141,.T.);
#54246=EDGE_CURVE('',#42150,#42145,#22767,.T.);
#54247=EDGE_CURVE('',#42148,#42151,#22768,.T.);
#54248=EDGE_CURVE('',#42151,#42152,#34142,.T.);
#54249=EDGE_CURVE('',#42152,#42149,#22769,.T.);
#54250=EDGE_CURVE('',#40922,#42134,#34143,.T.);
#54251=EDGE_CURVE('',#42133,#40923,#34144,.T.);
#54252=EDGE_CURVE('',#42151,#40527,#1706,.T.);
#54253=EDGE_CURVE('',#40526,#42152,#1707,.T.);
#54254=EDGE_CURVE('',#42143,#42146,#1708,.T.);
#54255=EDGE_CURVE('',#42145,#42144,#1709,.T.);
#54256=EDGE_CURVE('',#42139,#42142,#1710,.T.);
#54257=EDGE_CURVE('',#42141,#42140,#1711,.T.);
#54258=EDGE_CURVE('',#42153,#42154,#34145,.T.);
#54259=EDGE_CURVE('',#42154,#42155,#22770,.T.);
#54260=EDGE_CURVE('',#42156,#42155,#34146,.T.);
#54261=EDGE_CURVE('',#42157,#42156,#34147,.T.);
#54262=EDGE_CURVE('',#42158,#42157,#34148,.T.);
#54263=EDGE_CURVE('',#42158,#42153,#22771,.T.);
#54264=EDGE_CURVE('',#42156,#42159,#22772,.T.);
#54265=EDGE_CURVE('',#42159,#42160,#34149,.T.);
#54266=EDGE_CURVE('',#42160,#42157,#22773,.T.);
#54267=EDGE_CURVE('',#42161,#42162,#34150,.T.);
#54268=EDGE_CURVE('',#42162,#42163,#22774,.T.);
#54269=EDGE_CURVE('',#42163,#42164,#34151,.T.);
#54270=EDGE_CURVE('',#42164,#42161,#22775,.T.);
#54271=EDGE_CURVE('',#42165,#42166,#34152,.T.);
#54272=EDGE_CURVE('',#42166,#42167,#22776,.T.);
#54273=EDGE_CURVE('',#42168,#42167,#34153,.T.);
#54274=EDGE_CURVE('',#42169,#42168,#34154,.T.);
#54275=EDGE_CURVE('',#42170,#42169,#34155,.T.);
#54276=EDGE_CURVE('',#42170,#42165,#22777,.T.);
#54277=EDGE_CURVE('',#42168,#42171,#22778,.T.);
#54278=EDGE_CURVE('',#42171,#42172,#34156,.T.);
#54279=EDGE_CURVE('',#42172,#42169,#22779,.T.);
#54280=EDGE_CURVE('',#40928,#42154,#34157,.T.);
#54281=EDGE_CURVE('',#42153,#40929,#34158,.T.);
#54282=EDGE_CURVE('',#42171,#40521,#1712,.T.);
#54283=EDGE_CURVE('',#40520,#42172,#1713,.T.);
#54284=EDGE_CURVE('',#42163,#42166,#1714,.T.);
#54285=EDGE_CURVE('',#42165,#42164,#1715,.T.);
#54286=EDGE_CURVE('',#42159,#42162,#1716,.T.);
#54287=EDGE_CURVE('',#42161,#42160,#1717,.T.);
#54288=EDGE_CURVE('',#42173,#42174,#34159,.T.);
#54289=EDGE_CURVE('',#42174,#42175,#22780,.T.);
#54290=EDGE_CURVE('',#42176,#42175,#34160,.T.);
#54291=EDGE_CURVE('',#42177,#42176,#34161,.T.);
#54292=EDGE_CURVE('',#42178,#42177,#34162,.T.);
#54293=EDGE_CURVE('',#42178,#42173,#22781,.T.);
#54294=EDGE_CURVE('',#42176,#42179,#22782,.T.);
#54295=EDGE_CURVE('',#42179,#42180,#34163,.T.);
#54296=EDGE_CURVE('',#42180,#42177,#22783,.T.);
#54297=EDGE_CURVE('',#42181,#42182,#34164,.T.);
#54298=EDGE_CURVE('',#42182,#42183,#22784,.T.);
#54299=EDGE_CURVE('',#42183,#42184,#34165,.T.);
#54300=EDGE_CURVE('',#42184,#42181,#22785,.T.);
#54301=EDGE_CURVE('',#42185,#42186,#34166,.T.);
#54302=EDGE_CURVE('',#42186,#42187,#22786,.T.);
#54303=EDGE_CURVE('',#42188,#42187,#34167,.T.);
#54304=EDGE_CURVE('',#42189,#42188,#34168,.T.);
#54305=EDGE_CURVE('',#42190,#42189,#34169,.T.);
#54306=EDGE_CURVE('',#42190,#42185,#22787,.T.);
#54307=EDGE_CURVE('',#42188,#42191,#22788,.T.);
#54308=EDGE_CURVE('',#42191,#42192,#34170,.T.);
#54309=EDGE_CURVE('',#42192,#42189,#22789,.T.);
#54310=EDGE_CURVE('',#40934,#42174,#34171,.T.);
#54311=EDGE_CURVE('',#42173,#40935,#34172,.T.);
#54312=EDGE_CURVE('',#42191,#40515,#1718,.T.);
#54313=EDGE_CURVE('',#40514,#42192,#1719,.T.);
#54314=EDGE_CURVE('',#42183,#42186,#1720,.T.);
#54315=EDGE_CURVE('',#42185,#42184,#1721,.T.);
#54316=EDGE_CURVE('',#42179,#42182,#1722,.T.);
#54317=EDGE_CURVE('',#42181,#42180,#1723,.T.);
#54318=EDGE_CURVE('',#42193,#42194,#34173,.T.);
#54319=EDGE_CURVE('',#42194,#42195,#22790,.T.);
#54320=EDGE_CURVE('',#42196,#42195,#34174,.T.);
#54321=EDGE_CURVE('',#42197,#42196,#34175,.T.);
#54322=EDGE_CURVE('',#42198,#42197,#34176,.T.);
#54323=EDGE_CURVE('',#42198,#42193,#22791,.T.);
#54324=EDGE_CURVE('',#42196,#42199,#22792,.T.);
#54325=EDGE_CURVE('',#42199,#42200,#34177,.T.);
#54326=EDGE_CURVE('',#42200,#42197,#22793,.T.);
#54327=EDGE_CURVE('',#42201,#42202,#34178,.T.);
#54328=EDGE_CURVE('',#42202,#42203,#22794,.T.);
#54329=EDGE_CURVE('',#42203,#42204,#34179,.T.);
#54330=EDGE_CURVE('',#42204,#42201,#22795,.T.);
#54331=EDGE_CURVE('',#42205,#42206,#34180,.T.);
#54332=EDGE_CURVE('',#42206,#42207,#22796,.T.);
#54333=EDGE_CURVE('',#42208,#42207,#34181,.T.);
#54334=EDGE_CURVE('',#42209,#42208,#34182,.T.);
#54335=EDGE_CURVE('',#42210,#42209,#34183,.T.);
#54336=EDGE_CURVE('',#42210,#42205,#22797,.T.);
#54337=EDGE_CURVE('',#42208,#42211,#22798,.T.);
#54338=EDGE_CURVE('',#42211,#42212,#34184,.T.);
#54339=EDGE_CURVE('',#42212,#42209,#22799,.T.);
#54340=EDGE_CURVE('',#40940,#42194,#34185,.T.);
#54341=EDGE_CURVE('',#42193,#40941,#34186,.T.);
#54342=EDGE_CURVE('',#42211,#40509,#1724,.T.);
#54343=EDGE_CURVE('',#40508,#42212,#1725,.T.);
#54344=EDGE_CURVE('',#42203,#42206,#1726,.T.);
#54345=EDGE_CURVE('',#42205,#42204,#1727,.T.);
#54346=EDGE_CURVE('',#42199,#42202,#1728,.T.);
#54347=EDGE_CURVE('',#42201,#42200,#1729,.T.);
#54348=EDGE_CURVE('',#42213,#42214,#34187,.T.);
#54349=EDGE_CURVE('',#42214,#42215,#22800,.T.);
#54350=EDGE_CURVE('',#42216,#42215,#34188,.T.);
#54351=EDGE_CURVE('',#42217,#42216,#34189,.T.);
#54352=EDGE_CURVE('',#42218,#42217,#34190,.T.);
#54353=EDGE_CURVE('',#42218,#42213,#22801,.T.);
#54354=EDGE_CURVE('',#42216,#42219,#22802,.T.);
#54355=EDGE_CURVE('',#42219,#42220,#34191,.T.);
#54356=EDGE_CURVE('',#42220,#42217,#22803,.T.);
#54357=EDGE_CURVE('',#42221,#42222,#34192,.T.);
#54358=EDGE_CURVE('',#42222,#42223,#22804,.T.);
#54359=EDGE_CURVE('',#42223,#42224,#34193,.T.);
#54360=EDGE_CURVE('',#42224,#42221,#22805,.T.);
#54361=EDGE_CURVE('',#42225,#42226,#34194,.T.);
#54362=EDGE_CURVE('',#42226,#42227,#22806,.T.);
#54363=EDGE_CURVE('',#42228,#42227,#34195,.T.);
#54364=EDGE_CURVE('',#42229,#42228,#34196,.T.);
#54365=EDGE_CURVE('',#42230,#42229,#34197,.T.);
#54366=EDGE_CURVE('',#42230,#42225,#22807,.T.);
#54367=EDGE_CURVE('',#42228,#42231,#22808,.T.);
#54368=EDGE_CURVE('',#42231,#42232,#34198,.T.);
#54369=EDGE_CURVE('',#42232,#42229,#22809,.T.);
#54370=EDGE_CURVE('',#40946,#42214,#34199,.T.);
#54371=EDGE_CURVE('',#42213,#40947,#34200,.T.);
#54372=EDGE_CURVE('',#42231,#40503,#1730,.T.);
#54373=EDGE_CURVE('',#40502,#42232,#1731,.T.);
#54374=EDGE_CURVE('',#42223,#42226,#1732,.T.);
#54375=EDGE_CURVE('',#42225,#42224,#1733,.T.);
#54376=EDGE_CURVE('',#42219,#42222,#1734,.T.);
#54377=EDGE_CURVE('',#42221,#42220,#1735,.T.);
#54378=EDGE_CURVE('',#42233,#42234,#34201,.T.);
#54379=EDGE_CURVE('',#42234,#42235,#22810,.T.);
#54380=EDGE_CURVE('',#42236,#42235,#34202,.T.);
#54381=EDGE_CURVE('',#42237,#42236,#34203,.T.);
#54382=EDGE_CURVE('',#42238,#42237,#34204,.T.);
#54383=EDGE_CURVE('',#42238,#42233,#22811,.T.);
#54384=EDGE_CURVE('',#42236,#42239,#22812,.T.);
#54385=EDGE_CURVE('',#42239,#42240,#34205,.T.);
#54386=EDGE_CURVE('',#42240,#42237,#22813,.T.);
#54387=EDGE_CURVE('',#42241,#42242,#34206,.T.);
#54388=EDGE_CURVE('',#42242,#42243,#22814,.T.);
#54389=EDGE_CURVE('',#42243,#42244,#34207,.T.);
#54390=EDGE_CURVE('',#42244,#42241,#22815,.T.);
#54391=EDGE_CURVE('',#42245,#42246,#34208,.T.);
#54392=EDGE_CURVE('',#42246,#42247,#22816,.T.);
#54393=EDGE_CURVE('',#42248,#42247,#34209,.T.);
#54394=EDGE_CURVE('',#42249,#42248,#34210,.T.);
#54395=EDGE_CURVE('',#42250,#42249,#34211,.T.);
#54396=EDGE_CURVE('',#42250,#42245,#22817,.T.);
#54397=EDGE_CURVE('',#42248,#42251,#22818,.T.);
#54398=EDGE_CURVE('',#42251,#42252,#34212,.T.);
#54399=EDGE_CURVE('',#42252,#42249,#22819,.T.);
#54400=EDGE_CURVE('',#40952,#42234,#34213,.T.);
#54401=EDGE_CURVE('',#42233,#40953,#34214,.T.);
#54402=EDGE_CURVE('',#42251,#40497,#1736,.T.);
#54403=EDGE_CURVE('',#40496,#42252,#1737,.T.);
#54404=EDGE_CURVE('',#42243,#42246,#1738,.T.);
#54405=EDGE_CURVE('',#42245,#42244,#1739,.T.);
#54406=EDGE_CURVE('',#42239,#42242,#1740,.T.);
#54407=EDGE_CURVE('',#42241,#42240,#1741,.T.);
#54408=EDGE_CURVE('',#42253,#42254,#34215,.T.);
#54409=EDGE_CURVE('',#42254,#42255,#22820,.T.);
#54410=EDGE_CURVE('',#42256,#42255,#34216,.T.);
#54411=EDGE_CURVE('',#42257,#42256,#34217,.T.);
#54412=EDGE_CURVE('',#42258,#42257,#34218,.T.);
#54413=EDGE_CURVE('',#42258,#42253,#22821,.T.);
#54414=EDGE_CURVE('',#42256,#42259,#22822,.T.);
#54415=EDGE_CURVE('',#42259,#42260,#34219,.T.);
#54416=EDGE_CURVE('',#42260,#42257,#22823,.T.);
#54417=EDGE_CURVE('',#42261,#42262,#34220,.T.);
#54418=EDGE_CURVE('',#42262,#42263,#22824,.T.);
#54419=EDGE_CURVE('',#42263,#42264,#34221,.T.);
#54420=EDGE_CURVE('',#42264,#42261,#22825,.T.);
#54421=EDGE_CURVE('',#42265,#42266,#34222,.T.);
#54422=EDGE_CURVE('',#42266,#42267,#22826,.T.);
#54423=EDGE_CURVE('',#42268,#42267,#34223,.T.);
#54424=EDGE_CURVE('',#42269,#42268,#34224,.T.);
#54425=EDGE_CURVE('',#42270,#42269,#34225,.T.);
#54426=EDGE_CURVE('',#42270,#42265,#22827,.T.);
#54427=EDGE_CURVE('',#42268,#42271,#22828,.T.);
#54428=EDGE_CURVE('',#42271,#42272,#34226,.T.);
#54429=EDGE_CURVE('',#42272,#42269,#22829,.T.);
#54430=EDGE_CURVE('',#40958,#42254,#34227,.T.);
#54431=EDGE_CURVE('',#42253,#40959,#34228,.T.);
#54432=EDGE_CURVE('',#42271,#40491,#1742,.T.);
#54433=EDGE_CURVE('',#40490,#42272,#1743,.T.);
#54434=EDGE_CURVE('',#42263,#42266,#1744,.T.);
#54435=EDGE_CURVE('',#42265,#42264,#1745,.T.);
#54436=EDGE_CURVE('',#42259,#42262,#1746,.T.);
#54437=EDGE_CURVE('',#42261,#42260,#1747,.T.);
#54438=EDGE_CURVE('',#42273,#42274,#34229,.T.);
#54439=EDGE_CURVE('',#42274,#42275,#22830,.T.);
#54440=EDGE_CURVE('',#42276,#42275,#34230,.T.);
#54441=EDGE_CURVE('',#42277,#42276,#34231,.T.);
#54442=EDGE_CURVE('',#42278,#42277,#34232,.T.);
#54443=EDGE_CURVE('',#42278,#42273,#22831,.T.);
#54444=EDGE_CURVE('',#42276,#42279,#22832,.T.);
#54445=EDGE_CURVE('',#42279,#42280,#34233,.T.);
#54446=EDGE_CURVE('',#42280,#42277,#22833,.T.);
#54447=EDGE_CURVE('',#42281,#42282,#34234,.T.);
#54448=EDGE_CURVE('',#42282,#42283,#22834,.T.);
#54449=EDGE_CURVE('',#42283,#42284,#34235,.T.);
#54450=EDGE_CURVE('',#42284,#42281,#22835,.T.);
#54451=EDGE_CURVE('',#42285,#42286,#34236,.T.);
#54452=EDGE_CURVE('',#42286,#42287,#22836,.T.);
#54453=EDGE_CURVE('',#42288,#42287,#34237,.T.);
#54454=EDGE_CURVE('',#42289,#42288,#34238,.T.);
#54455=EDGE_CURVE('',#42290,#42289,#34239,.T.);
#54456=EDGE_CURVE('',#42290,#42285,#22837,.T.);
#54457=EDGE_CURVE('',#42288,#42291,#22838,.T.);
#54458=EDGE_CURVE('',#42291,#42292,#34240,.T.);
#54459=EDGE_CURVE('',#42292,#42289,#22839,.T.);
#54460=EDGE_CURVE('',#40964,#42274,#34241,.T.);
#54461=EDGE_CURVE('',#42273,#40965,#34242,.T.);
#54462=EDGE_CURVE('',#42291,#40485,#1748,.T.);
#54463=EDGE_CURVE('',#40484,#42292,#1749,.T.);
#54464=EDGE_CURVE('',#42283,#42286,#1750,.T.);
#54465=EDGE_CURVE('',#42285,#42284,#1751,.T.);
#54466=EDGE_CURVE('',#42279,#42282,#1752,.T.);
#54467=EDGE_CURVE('',#42281,#42280,#1753,.T.);
#54468=EDGE_CURVE('',#42293,#42294,#34243,.T.);
#54469=EDGE_CURVE('',#42294,#42295,#22840,.T.);
#54470=EDGE_CURVE('',#42296,#42295,#34244,.T.);
#54471=EDGE_CURVE('',#42297,#42296,#34245,.T.);
#54472=EDGE_CURVE('',#42298,#42297,#34246,.T.);
#54473=EDGE_CURVE('',#42298,#42293,#22841,.T.);
#54474=EDGE_CURVE('',#42296,#42299,#22842,.T.);
#54475=EDGE_CURVE('',#42299,#42300,#34247,.T.);
#54476=EDGE_CURVE('',#42300,#42297,#22843,.T.);
#54477=EDGE_CURVE('',#42301,#42302,#34248,.T.);
#54478=EDGE_CURVE('',#42302,#42303,#22844,.T.);
#54479=EDGE_CURVE('',#42303,#42304,#34249,.T.);
#54480=EDGE_CURVE('',#42304,#42301,#22845,.T.);
#54481=EDGE_CURVE('',#42305,#42306,#34250,.T.);
#54482=EDGE_CURVE('',#42306,#42307,#22846,.T.);
#54483=EDGE_CURVE('',#42308,#42307,#34251,.T.);
#54484=EDGE_CURVE('',#42309,#42308,#34252,.T.);
#54485=EDGE_CURVE('',#42310,#42309,#34253,.T.);
#54486=EDGE_CURVE('',#42310,#42305,#22847,.T.);
#54487=EDGE_CURVE('',#42308,#42311,#22848,.T.);
#54488=EDGE_CURVE('',#42311,#42312,#34254,.T.);
#54489=EDGE_CURVE('',#42312,#42309,#22849,.T.);
#54490=EDGE_CURVE('',#40970,#42294,#34255,.T.);
#54491=EDGE_CURVE('',#42293,#40971,#34256,.T.);
#54492=EDGE_CURVE('',#42311,#40479,#1754,.T.);
#54493=EDGE_CURVE('',#40478,#42312,#1755,.T.);
#54494=EDGE_CURVE('',#42303,#42306,#1756,.T.);
#54495=EDGE_CURVE('',#42305,#42304,#1757,.T.);
#54496=EDGE_CURVE('',#42299,#42302,#1758,.T.);
#54497=EDGE_CURVE('',#42301,#42300,#1759,.T.);
#54498=EDGE_CURVE('',#42313,#42314,#34257,.T.);
#54499=EDGE_CURVE('',#42314,#42315,#22850,.T.);
#54500=EDGE_CURVE('',#42316,#42315,#34258,.T.);
#54501=EDGE_CURVE('',#42317,#42316,#34259,.T.);
#54502=EDGE_CURVE('',#42318,#42317,#34260,.T.);
#54503=EDGE_CURVE('',#42318,#42313,#22851,.T.);
#54504=EDGE_CURVE('',#42316,#42319,#22852,.T.);
#54505=EDGE_CURVE('',#42319,#42320,#34261,.T.);
#54506=EDGE_CURVE('',#42320,#42317,#22853,.T.);
#54507=EDGE_CURVE('',#42321,#42322,#34262,.T.);
#54508=EDGE_CURVE('',#42322,#42323,#22854,.T.);
#54509=EDGE_CURVE('',#42323,#42324,#34263,.T.);
#54510=EDGE_CURVE('',#42324,#42321,#22855,.T.);
#54511=EDGE_CURVE('',#42325,#42326,#34264,.T.);
#54512=EDGE_CURVE('',#42326,#42327,#22856,.T.);
#54513=EDGE_CURVE('',#42328,#42327,#34265,.T.);
#54514=EDGE_CURVE('',#42329,#42328,#34266,.T.);
#54515=EDGE_CURVE('',#42330,#42329,#34267,.T.);
#54516=EDGE_CURVE('',#42330,#42325,#22857,.T.);
#54517=EDGE_CURVE('',#42328,#42331,#22858,.T.);
#54518=EDGE_CURVE('',#42331,#42332,#34268,.T.);
#54519=EDGE_CURVE('',#42332,#42329,#22859,.T.);
#54520=EDGE_CURVE('',#40976,#42314,#34269,.T.);
#54521=EDGE_CURVE('',#42313,#40977,#34270,.T.);
#54522=EDGE_CURVE('',#42331,#40473,#1760,.T.);
#54523=EDGE_CURVE('',#40472,#42332,#1761,.T.);
#54524=EDGE_CURVE('',#42323,#42326,#1762,.T.);
#54525=EDGE_CURVE('',#42325,#42324,#1763,.T.);
#54526=EDGE_CURVE('',#42319,#42322,#1764,.T.);
#54527=EDGE_CURVE('',#42321,#42320,#1765,.T.);
#54528=EDGE_CURVE('',#42333,#42334,#34271,.T.);
#54529=EDGE_CURVE('',#42334,#42335,#22860,.T.);
#54530=EDGE_CURVE('',#42336,#42335,#34272,.T.);
#54531=EDGE_CURVE('',#42337,#42336,#34273,.T.);
#54532=EDGE_CURVE('',#42338,#42337,#34274,.T.);
#54533=EDGE_CURVE('',#42338,#42333,#22861,.T.);
#54534=EDGE_CURVE('',#42336,#42339,#22862,.T.);
#54535=EDGE_CURVE('',#42339,#42340,#34275,.T.);
#54536=EDGE_CURVE('',#42340,#42337,#22863,.T.);
#54537=EDGE_CURVE('',#42341,#42342,#34276,.T.);
#54538=EDGE_CURVE('',#42342,#42343,#22864,.T.);
#54539=EDGE_CURVE('',#42343,#42344,#34277,.T.);
#54540=EDGE_CURVE('',#42344,#42341,#22865,.T.);
#54541=EDGE_CURVE('',#42345,#42346,#34278,.T.);
#54542=EDGE_CURVE('',#42346,#42347,#22866,.T.);
#54543=EDGE_CURVE('',#42348,#42347,#34279,.T.);
#54544=EDGE_CURVE('',#42349,#42348,#34280,.T.);
#54545=EDGE_CURVE('',#42350,#42349,#34281,.T.);
#54546=EDGE_CURVE('',#42350,#42345,#22867,.T.);
#54547=EDGE_CURVE('',#42348,#42351,#22868,.T.);
#54548=EDGE_CURVE('',#42351,#42352,#34282,.T.);
#54549=EDGE_CURVE('',#42352,#42349,#22869,.T.);
#54550=EDGE_CURVE('',#40982,#42334,#34283,.T.);
#54551=EDGE_CURVE('',#42333,#40983,#34284,.T.);
#54552=EDGE_CURVE('',#42351,#40467,#1766,.T.);
#54553=EDGE_CURVE('',#40466,#42352,#1767,.T.);
#54554=EDGE_CURVE('',#42343,#42346,#1768,.T.);
#54555=EDGE_CURVE('',#42345,#42344,#1769,.T.);
#54556=EDGE_CURVE('',#42339,#42342,#1770,.T.);
#54557=EDGE_CURVE('',#42341,#42340,#1771,.T.);
#54558=EDGE_CURVE('',#42353,#42354,#34285,.T.);
#54559=EDGE_CURVE('',#42354,#42355,#22870,.T.);
#54560=EDGE_CURVE('',#42356,#42355,#34286,.T.);
#54561=EDGE_CURVE('',#42357,#42356,#34287,.T.);
#54562=EDGE_CURVE('',#42358,#42357,#34288,.T.);
#54563=EDGE_CURVE('',#42358,#42353,#22871,.T.);
#54564=EDGE_CURVE('',#42356,#42359,#22872,.T.);
#54565=EDGE_CURVE('',#42359,#42360,#34289,.T.);
#54566=EDGE_CURVE('',#42360,#42357,#22873,.T.);
#54567=EDGE_CURVE('',#42361,#42362,#34290,.T.);
#54568=EDGE_CURVE('',#42362,#42363,#22874,.T.);
#54569=EDGE_CURVE('',#42363,#42364,#34291,.T.);
#54570=EDGE_CURVE('',#42364,#42361,#22875,.T.);
#54571=EDGE_CURVE('',#42365,#42366,#34292,.T.);
#54572=EDGE_CURVE('',#42366,#42367,#22876,.T.);
#54573=EDGE_CURVE('',#42368,#42367,#34293,.T.);
#54574=EDGE_CURVE('',#42369,#42368,#34294,.T.);
#54575=EDGE_CURVE('',#42370,#42369,#34295,.T.);
#54576=EDGE_CURVE('',#42370,#42365,#22877,.T.);
#54577=EDGE_CURVE('',#42368,#42371,#22878,.T.);
#54578=EDGE_CURVE('',#42371,#42372,#34296,.T.);
#54579=EDGE_CURVE('',#42372,#42369,#22879,.T.);
#54580=EDGE_CURVE('',#40988,#42354,#34297,.T.);
#54581=EDGE_CURVE('',#42353,#40989,#34298,.T.);
#54582=EDGE_CURVE('',#42371,#40461,#1772,.T.);
#54583=EDGE_CURVE('',#40460,#42372,#1773,.T.);
#54584=EDGE_CURVE('',#42363,#42366,#1774,.T.);
#54585=EDGE_CURVE('',#42365,#42364,#1775,.T.);
#54586=EDGE_CURVE('',#42359,#42362,#1776,.T.);
#54587=EDGE_CURVE('',#42361,#42360,#1777,.T.);
#54588=EDGE_CURVE('',#42373,#42374,#22880,.T.);
#54589=EDGE_CURVE('',#42374,#42375,#34299,.T.);
#54590=EDGE_CURVE('',#42375,#42376,#22881,.T.);
#54591=EDGE_CURVE('',#42376,#42373,#34300,.T.);
#54592=EDGE_CURVE('',#42377,#42378,#1778,.T.);
#54593=EDGE_CURVE('',#42378,#42379,#22882,.T.);
#54594=EDGE_CURVE('',#42379,#42380,#22883,.T.);
#54595=EDGE_CURVE('',#42380,#42381,#22884,.T.);
#54596=EDGE_CURVE('',#42381,#42382,#1779,.T.);
#54597=EDGE_CURVE('',#42382,#42383,#22885,.T.);
#54598=EDGE_CURVE('',#42383,#42384,#22886,.T.);
#54599=EDGE_CURVE('',#42384,#42385,#1780,.T.);
#54600=EDGE_CURVE('',#42385,#42386,#22887,.T.);
#54601=EDGE_CURVE('',#42386,#42387,#1781,.T.);
#54602=EDGE_CURVE('',#42387,#42388,#22888,.T.);
#54603=EDGE_CURVE('',#42388,#42377,#22889,.T.);
#54604=EDGE_CURVE('',#42389,#42390,#1782,.T.);
#54605=EDGE_CURVE('',#42390,#42391,#22890,.T.);
#54606=EDGE_CURVE('',#42391,#42392,#22891,.T.);
#54607=EDGE_CURVE('',#42392,#42393,#22892,.T.);
#54608=EDGE_CURVE('',#42393,#42394,#1783,.T.);
#54609=EDGE_CURVE('',#42394,#42395,#22893,.T.);
#54610=EDGE_CURVE('',#42395,#42396,#22894,.T.);
#54611=EDGE_CURVE('',#42396,#42397,#1784,.T.);
#54612=EDGE_CURVE('',#42397,#42398,#22895,.T.);
#54613=EDGE_CURVE('',#42398,#42399,#1785,.T.);
#54614=EDGE_CURVE('',#42399,#42400,#22896,.T.);
#54615=EDGE_CURVE('',#42400,#42389,#22897,.T.);
#54616=EDGE_CURVE('',#42391,#42374,#4975,.T.);
#54617=EDGE_CURVE('',#42373,#42392,#4976,.T.);
#54618=EDGE_CURVE('',#42375,#42380,#4977,.T.);
#54619=EDGE_CURVE('',#42379,#42376,#4978,.T.);
#54620=EDGE_CURVE('',#42400,#42370,#1786,.T.);
#54621=EDGE_CURVE('',#42365,#42399,#34301,.T.);
#54622=EDGE_CURVE('',#42364,#42398,#34302,.T.);
#54623=EDGE_CURVE('',#42389,#42372,#34303,.T.);
#54624=EDGE_CURVE('',#42361,#42397,#34304,.T.);
#54625=EDGE_CURVE('',#42390,#40460,#34305,.T.);
#54626=EDGE_CURVE('',#42360,#42396,#34306,.T.);
#54627=EDGE_CURVE('',#42391,#40459,#34307,.T.);
#54628=EDGE_CURVE('',#42358,#42395,#1787,.T.);
#54629=EDGE_CURVE('',#42374,#40458,#34308,.T.);
#54630=EDGE_CURVE('',#42353,#42394,#34309,.T.);
#54631=EDGE_CURVE('',#42375,#40457,#34310,.T.);
#54632=EDGE_CURVE('',#40989,#42393,#34311,.T.);
#54633=EDGE_CURVE('',#42380,#40812,#34312,.T.);
#54634=EDGE_CURVE('',#40990,#42392,#34313,.T.);
#54635=EDGE_CURVE('',#42381,#40811,#34314,.T.);
#54636=EDGE_CURVE('',#40991,#42373,#34315,.T.);
#54637=EDGE_CURVE('',#42382,#41191,#34316,.T.);
#54638=EDGE_CURVE('',#40993,#42376,#34317,.T.);
#54639=EDGE_CURVE('',#42383,#41189,#1788,.T.);
#54640=EDGE_CURVE('',#40994,#42379,#34318,.T.);
#54641=EDGE_CURVE('',#42384,#41188,#34319,.T.);
#54642=EDGE_CURVE('',#40995,#42378,#34320,.T.);
#54643=EDGE_CURVE('',#42385,#41181,#34321,.T.);
#54644=EDGE_CURVE('',#41176,#42377,#34322,.T.);
#54645=EDGE_CURVE('',#42386,#41184,#34323,.T.);
#54646=EDGE_CURVE('',#41177,#42388,#1789,.T.);
#54647=EDGE_CURVE('',#42387,#41179,#34324,.T.);
#54648=EDGE_CURVE('',#42401,#42402,#22898,.T.);
#54649=EDGE_CURVE('',#42402,#42403,#34325,.T.);
#54650=EDGE_CURVE('',#42403,#42404,#22899,.T.);
#54651=EDGE_CURVE('',#42404,#42401,#34326,.T.);
#54652=EDGE_CURVE('',#42405,#42406,#1790,.T.);
#54653=EDGE_CURVE('',#42406,#42407,#22900,.T.);
#54654=EDGE_CURVE('',#42407,#42408,#22901,.T.);
#54655=EDGE_CURVE('',#42408,#42409,#22902,.T.);
#54656=EDGE_CURVE('',#42409,#42410,#1791,.T.);
#54657=EDGE_CURVE('',#42410,#42411,#22903,.T.);
#54658=EDGE_CURVE('',#42411,#42412,#22904,.T.);
#54659=EDGE_CURVE('',#42412,#42413,#1792,.T.);
#54660=EDGE_CURVE('',#42413,#42414,#22905,.T.);
#54661=EDGE_CURVE('',#42414,#42415,#1793,.T.);
#54662=EDGE_CURVE('',#42415,#42416,#22906,.T.);
#54663=EDGE_CURVE('',#42416,#42405,#22907,.T.);
#54664=EDGE_CURVE('',#42417,#42418,#1794,.T.);
#54665=EDGE_CURVE('',#42418,#42419,#22908,.T.);
#54666=EDGE_CURVE('',#42419,#42420,#22909,.T.);
#54667=EDGE_CURVE('',#42420,#42421,#22910,.T.);
#54668=EDGE_CURVE('',#42421,#42422,#1795,.T.);
#54669=EDGE_CURVE('',#42422,#42423,#22911,.T.);
#54670=EDGE_CURVE('',#42423,#42424,#22912,.T.);
#54671=EDGE_CURVE('',#42424,#42425,#1796,.T.);
#54672=EDGE_CURVE('',#42425,#42426,#22913,.T.);
#54673=EDGE_CURVE('',#42426,#42427,#1797,.T.);
#54674=EDGE_CURVE('',#42427,#42428,#22914,.T.);
#54675=EDGE_CURVE('',#42428,#42417,#22915,.T.);
#54676=EDGE_CURVE('',#42429,#42430,#22916,.T.);
#54677=EDGE_CURVE('',#42430,#42431,#34327,.T.);
#54678=EDGE_CURVE('',#42431,#42432,#22917,.T.);
#54679=EDGE_CURVE('',#42432,#42429,#34328,.T.);
#54680=EDGE_CURVE('',#42433,#42434,#1798,.T.);
#54681=EDGE_CURVE('',#42434,#42435,#22918,.T.);
#54682=EDGE_CURVE('',#42435,#42436,#22919,.T.);
#54683=EDGE_CURVE('',#42436,#42437,#22920,.T.);
#54684=EDGE_CURVE('',#42437,#42438,#1799,.T.);
#54685=EDGE_CURVE('',#42438,#42439,#22921,.T.);
#54686=EDGE_CURVE('',#42439,#42440,#22922,.T.);
#54687=EDGE_CURVE('',#42440,#42441,#1800,.T.);
#54688=EDGE_CURVE('',#42441,#42442,#22923,.T.);
#54689=EDGE_CURVE('',#42442,#42443,#1801,.T.);
#54690=EDGE_CURVE('',#42443,#42444,#22924,.T.);
#54691=EDGE_CURVE('',#42444,#42433,#22925,.T.);
#54692=EDGE_CURVE('',#42445,#42446,#1802,.T.);
#54693=EDGE_CURVE('',#42446,#42447,#22926,.T.);
#54694=EDGE_CURVE('',#42447,#42448,#22927,.T.);
#54695=EDGE_CURVE('',#42448,#42449,#22928,.T.);
#54696=EDGE_CURVE('',#42449,#42450,#1803,.T.);
#54697=EDGE_CURVE('',#42450,#42451,#22929,.T.);
#54698=EDGE_CURVE('',#42451,#42452,#22930,.T.);
#54699=EDGE_CURVE('',#42452,#42453,#1804,.T.);
#54700=EDGE_CURVE('',#42453,#42454,#22931,.T.);
#54701=EDGE_CURVE('',#42454,#42455,#1805,.T.);
#54702=EDGE_CURVE('',#42455,#42456,#22932,.T.);
#54703=EDGE_CURVE('',#42456,#42445,#22933,.T.);
#54704=EDGE_CURVE('',#42457,#42458,#22934,.T.);
#54705=EDGE_CURVE('',#42458,#42459,#34329,.T.);
#54706=EDGE_CURVE('',#42459,#42460,#22935,.T.);
#54707=EDGE_CURVE('',#42460,#42457,#34330,.T.);
#54708=EDGE_CURVE('',#42461,#42462,#1806,.T.);
#54709=EDGE_CURVE('',#42462,#42463,#22936,.T.);
#54710=EDGE_CURVE('',#42463,#42464,#22937,.T.);
#54711=EDGE_CURVE('',#42464,#42465,#22938,.T.);
#54712=EDGE_CURVE('',#42465,#42466,#1807,.T.);
#54713=EDGE_CURVE('',#42466,#42467,#22939,.T.);
#54714=EDGE_CURVE('',#42467,#42468,#22940,.T.);
#54715=EDGE_CURVE('',#42468,#42469,#1808,.T.);
#54716=EDGE_CURVE('',#42469,#42470,#22941,.T.);
#54717=EDGE_CURVE('',#42470,#42471,#1809,.T.);
#54718=EDGE_CURVE('',#42471,#42472,#22942,.T.);
#54719=EDGE_CURVE('',#42472,#42461,#22943,.T.);
#54720=EDGE_CURVE('',#42473,#42474,#1810,.T.);
#54721=EDGE_CURVE('',#42474,#42475,#22944,.T.);
#54722=EDGE_CURVE('',#42475,#42476,#22945,.T.);
#54723=EDGE_CURVE('',#42476,#42477,#22946,.T.);
#54724=EDGE_CURVE('',#42477,#42478,#1811,.T.);
#54725=EDGE_CURVE('',#42478,#42479,#22947,.T.);
#54726=EDGE_CURVE('',#42479,#42480,#22948,.T.);
#54727=EDGE_CURVE('',#42480,#42481,#1812,.T.);
#54728=EDGE_CURVE('',#42481,#42482,#22949,.T.);
#54729=EDGE_CURVE('',#42482,#42483,#1813,.T.);
#54730=EDGE_CURVE('',#42483,#42484,#22950,.T.);
#54731=EDGE_CURVE('',#42484,#42473,#22951,.T.);
#54732=EDGE_CURVE('',#42485,#42486,#22952,.T.);
#54733=EDGE_CURVE('',#42486,#42487,#34331,.T.);
#54734=EDGE_CURVE('',#42487,#42488,#22953,.T.);
#54735=EDGE_CURVE('',#42488,#42485,#34332,.T.);
#54736=EDGE_CURVE('',#42489,#42490,#1814,.T.);
#54737=EDGE_CURVE('',#42490,#42491,#22954,.T.);
#54738=EDGE_CURVE('',#42491,#42492,#22955,.T.);
#54739=EDGE_CURVE('',#42492,#42493,#22956,.T.);
#54740=EDGE_CURVE('',#42493,#42494,#1815,.T.);
#54741=EDGE_CURVE('',#42494,#42495,#22957,.T.);
#54742=EDGE_CURVE('',#42495,#42496,#22958,.T.);
#54743=EDGE_CURVE('',#42496,#42497,#1816,.T.);
#54744=EDGE_CURVE('',#42497,#42498,#22959,.T.);
#54745=EDGE_CURVE('',#42498,#42499,#1817,.T.);
#54746=EDGE_CURVE('',#42499,#42500,#22960,.T.);
#54747=EDGE_CURVE('',#42500,#42489,#22961,.T.);
#54748=EDGE_CURVE('',#42501,#42502,#1818,.T.);
#54749=EDGE_CURVE('',#42502,#42503,#22962,.T.);
#54750=EDGE_CURVE('',#42503,#42504,#22963,.T.);
#54751=EDGE_CURVE('',#42504,#42505,#22964,.T.);
#54752=EDGE_CURVE('',#42505,#42506,#1819,.T.);
#54753=EDGE_CURVE('',#42506,#42507,#22965,.T.);
#54754=EDGE_CURVE('',#42507,#42508,#22966,.T.);
#54755=EDGE_CURVE('',#42508,#42509,#1820,.T.);
#54756=EDGE_CURVE('',#42509,#42510,#22967,.T.);
#54757=EDGE_CURVE('',#42510,#42511,#1821,.T.);
#54758=EDGE_CURVE('',#42511,#42512,#22968,.T.);
#54759=EDGE_CURVE('',#42512,#42501,#22969,.T.);
#54760=EDGE_CURVE('',#42513,#42514,#22970,.T.);
#54761=EDGE_CURVE('',#42514,#42515,#34333,.T.);
#54762=EDGE_CURVE('',#42515,#42516,#22971,.T.);
#54763=EDGE_CURVE('',#42516,#42513,#34334,.T.);
#54764=EDGE_CURVE('',#42517,#42518,#1822,.T.);
#54765=EDGE_CURVE('',#42518,#42519,#22972,.T.);
#54766=EDGE_CURVE('',#42519,#42520,#22973,.T.);
#54767=EDGE_CURVE('',#42520,#42521,#22974,.T.);
#54768=EDGE_CURVE('',#42521,#42522,#1823,.T.);
#54769=EDGE_CURVE('',#42522,#42523,#22975,.T.);
#54770=EDGE_CURVE('',#42523,#42524,#22976,.T.);
#54771=EDGE_CURVE('',#42524,#42525,#1824,.T.);
#54772=EDGE_CURVE('',#42525,#42526,#22977,.T.);
#54773=EDGE_CURVE('',#42526,#42527,#1825,.T.);
#54774=EDGE_CURVE('',#42527,#42528,#22978,.T.);
#54775=EDGE_CURVE('',#42528,#42517,#22979,.T.);
#54776=EDGE_CURVE('',#42529,#42530,#1826,.T.);
#54777=EDGE_CURVE('',#42530,#42531,#22980,.T.);
#54778=EDGE_CURVE('',#42531,#42532,#22981,.T.);
#54779=EDGE_CURVE('',#42532,#42533,#22982,.T.);
#54780=EDGE_CURVE('',#42533,#42534,#1827,.T.);
#54781=EDGE_CURVE('',#42534,#42535,#22983,.T.);
#54782=EDGE_CURVE('',#42535,#42536,#22984,.T.);
#54783=EDGE_CURVE('',#42536,#42537,#1828,.T.);
#54784=EDGE_CURVE('',#42537,#42538,#22985,.T.);
#54785=EDGE_CURVE('',#42538,#42539,#1829,.T.);
#54786=EDGE_CURVE('',#42539,#42540,#22986,.T.);
#54787=EDGE_CURVE('',#42540,#42529,#22987,.T.);
#54788=EDGE_CURVE('',#42541,#42542,#22988,.T.);
#54789=EDGE_CURVE('',#42542,#42543,#34335,.T.);
#54790=EDGE_CURVE('',#42543,#42544,#22989,.T.);
#54791=EDGE_CURVE('',#42544,#42541,#34336,.T.);
#54792=EDGE_CURVE('',#42545,#42546,#1830,.T.);
#54793=EDGE_CURVE('',#42546,#42547,#22990,.T.);
#54794=EDGE_CURVE('',#42547,#42548,#22991,.T.);
#54795=EDGE_CURVE('',#42548,#42549,#22992,.T.);
#54796=EDGE_CURVE('',#42549,#42550,#1831,.T.);
#54797=EDGE_CURVE('',#42550,#42551,#22993,.T.);
#54798=EDGE_CURVE('',#42551,#42552,#22994,.T.);
#54799=EDGE_CURVE('',#42552,#42553,#1832,.T.);
#54800=EDGE_CURVE('',#42553,#42554,#22995,.T.);
#54801=EDGE_CURVE('',#42554,#42555,#1833,.T.);
#54802=EDGE_CURVE('',#42555,#42556,#22996,.T.);
#54803=EDGE_CURVE('',#42556,#42545,#22997,.T.);
#54804=EDGE_CURVE('',#42557,#42558,#1834,.T.);
#54805=EDGE_CURVE('',#42558,#42559,#22998,.T.);
#54806=EDGE_CURVE('',#42559,#42560,#22999,.T.);
#54807=EDGE_CURVE('',#42560,#42561,#23000,.T.);
#54808=EDGE_CURVE('',#42561,#42562,#1835,.T.);
#54809=EDGE_CURVE('',#42562,#42563,#23001,.T.);
#54810=EDGE_CURVE('',#42563,#42564,#23002,.T.);
#54811=EDGE_CURVE('',#42564,#42565,#1836,.T.);
#54812=EDGE_CURVE('',#42565,#42566,#23003,.T.);
#54813=EDGE_CURVE('',#42566,#42567,#1837,.T.);
#54814=EDGE_CURVE('',#42567,#42568,#23004,.T.);
#54815=EDGE_CURVE('',#42568,#42557,#23005,.T.);
#54816=EDGE_CURVE('',#42569,#42570,#23006,.T.);
#54817=EDGE_CURVE('',#42570,#42571,#34337,.T.);
#54818=EDGE_CURVE('',#42571,#42572,#23007,.T.);
#54819=EDGE_CURVE('',#42572,#42569,#34338,.T.);
#54820=EDGE_CURVE('',#42573,#42574,#1838,.T.);
#54821=EDGE_CURVE('',#42574,#42575,#23008,.T.);
#54822=EDGE_CURVE('',#42575,#42576,#23009,.T.);
#54823=EDGE_CURVE('',#42576,#42577,#23010,.T.);
#54824=EDGE_CURVE('',#42577,#42578,#1839,.T.);
#54825=EDGE_CURVE('',#42578,#42579,#23011,.T.);
#54826=EDGE_CURVE('',#42579,#42580,#23012,.T.);
#54827=EDGE_CURVE('',#42580,#42581,#1840,.T.);
#54828=EDGE_CURVE('',#42581,#42582,#23013,.T.);
#54829=EDGE_CURVE('',#42582,#42583,#1841,.T.);
#54830=EDGE_CURVE('',#42583,#42584,#23014,.T.);
#54831=EDGE_CURVE('',#42584,#42573,#23015,.T.);
#54832=EDGE_CURVE('',#42585,#42586,#1842,.T.);
#54833=EDGE_CURVE('',#42586,#42587,#23016,.T.);
#54834=EDGE_CURVE('',#42587,#42588,#23017,.T.);
#54835=EDGE_CURVE('',#42588,#42589,#23018,.T.);
#54836=EDGE_CURVE('',#42589,#42590,#1843,.T.);
#54837=EDGE_CURVE('',#42590,#42591,#23019,.T.);
#54838=EDGE_CURVE('',#42591,#42592,#23020,.T.);
#54839=EDGE_CURVE('',#42592,#42593,#1844,.T.);
#54840=EDGE_CURVE('',#42593,#42594,#23021,.T.);
#54841=EDGE_CURVE('',#42594,#42595,#1845,.T.);
#54842=EDGE_CURVE('',#42595,#42596,#23022,.T.);
#54843=EDGE_CURVE('',#42596,#42585,#23023,.T.);
#54844=EDGE_CURVE('',#42597,#42598,#23024,.T.);
#54845=EDGE_CURVE('',#42598,#42599,#34339,.T.);
#54846=EDGE_CURVE('',#42599,#42600,#23025,.T.);
#54847=EDGE_CURVE('',#42600,#42597,#34340,.T.);
#54848=EDGE_CURVE('',#42601,#42602,#1846,.T.);
#54849=EDGE_CURVE('',#42602,#42603,#23026,.T.);
#54850=EDGE_CURVE('',#42603,#42604,#23027,.T.);
#54851=EDGE_CURVE('',#42604,#42605,#23028,.T.);
#54852=EDGE_CURVE('',#42605,#42606,#1847,.T.);
#54853=EDGE_CURVE('',#42606,#42607,#23029,.T.);
#54854=EDGE_CURVE('',#42607,#42608,#23030,.T.);
#54855=EDGE_CURVE('',#42608,#42609,#1848,.T.);
#54856=EDGE_CURVE('',#42609,#42610,#23031,.T.);
#54857=EDGE_CURVE('',#42610,#42611,#1849,.T.);
#54858=EDGE_CURVE('',#42611,#42612,#23032,.T.);
#54859=EDGE_CURVE('',#42612,#42601,#23033,.T.);
#54860=EDGE_CURVE('',#42613,#42614,#1850,.T.);
#54861=EDGE_CURVE('',#42614,#42615,#23034,.T.);
#54862=EDGE_CURVE('',#42615,#42616,#23035,.T.);
#54863=EDGE_CURVE('',#42616,#42617,#23036,.T.);
#54864=EDGE_CURVE('',#42617,#42618,#1851,.T.);
#54865=EDGE_CURVE('',#42618,#42619,#23037,.T.);
#54866=EDGE_CURVE('',#42619,#42620,#23038,.T.);
#54867=EDGE_CURVE('',#42620,#42621,#1852,.T.);
#54868=EDGE_CURVE('',#42621,#42622,#23039,.T.);
#54869=EDGE_CURVE('',#42622,#42623,#1853,.T.);
#54870=EDGE_CURVE('',#42623,#42624,#23040,.T.);
#54871=EDGE_CURVE('',#42624,#42613,#23041,.T.);
#54872=EDGE_CURVE('',#42625,#42626,#23042,.T.);
#54873=EDGE_CURVE('',#42626,#42627,#34341,.T.);
#54874=EDGE_CURVE('',#42627,#42628,#23043,.T.);
#54875=EDGE_CURVE('',#42628,#42625,#34342,.T.);
#54876=EDGE_CURVE('',#42629,#42630,#1854,.T.);
#54877=EDGE_CURVE('',#42630,#42631,#23044,.T.);
#54878=EDGE_CURVE('',#42631,#42632,#23045,.T.);
#54879=EDGE_CURVE('',#42632,#42633,#23046,.T.);
#54880=EDGE_CURVE('',#42633,#42634,#1855,.T.);
#54881=EDGE_CURVE('',#42634,#42635,#23047,.T.);
#54882=EDGE_CURVE('',#42635,#42636,#23048,.T.);
#54883=EDGE_CURVE('',#42636,#42637,#1856,.T.);
#54884=EDGE_CURVE('',#42637,#42638,#23049,.T.);
#54885=EDGE_CURVE('',#42638,#42639,#1857,.T.);
#54886=EDGE_CURVE('',#42639,#42640,#23050,.T.);
#54887=EDGE_CURVE('',#42640,#42629,#23051,.T.);
#54888=EDGE_CURVE('',#42641,#42642,#1858,.T.);
#54889=EDGE_CURVE('',#42642,#42643,#23052,.T.);
#54890=EDGE_CURVE('',#42643,#42644,#23053,.T.);
#54891=EDGE_CURVE('',#42644,#42645,#23054,.T.);
#54892=EDGE_CURVE('',#42645,#42646,#1859,.T.);
#54893=EDGE_CURVE('',#42646,#42647,#23055,.T.);
#54894=EDGE_CURVE('',#42647,#42648,#23056,.T.);
#54895=EDGE_CURVE('',#42648,#42649,#1860,.T.);
#54896=EDGE_CURVE('',#42649,#42650,#23057,.T.);
#54897=EDGE_CURVE('',#42650,#42651,#1861,.T.);
#54898=EDGE_CURVE('',#42651,#42652,#23058,.T.);
#54899=EDGE_CURVE('',#42652,#42641,#23059,.T.);
#54900=EDGE_CURVE('',#42653,#42654,#23060,.T.);
#54901=EDGE_CURVE('',#42654,#42655,#34343,.T.);
#54902=EDGE_CURVE('',#42655,#42656,#23061,.T.);
#54903=EDGE_CURVE('',#42656,#42653,#34344,.T.);
#54904=EDGE_CURVE('',#42657,#42658,#1862,.T.);
#54905=EDGE_CURVE('',#42658,#42659,#23062,.T.);
#54906=EDGE_CURVE('',#42659,#42660,#23063,.T.);
#54907=EDGE_CURVE('',#42660,#42661,#23064,.T.);
#54908=EDGE_CURVE('',#42661,#42662,#1863,.T.);
#54909=EDGE_CURVE('',#42662,#42663,#23065,.T.);
#54910=EDGE_CURVE('',#42663,#42664,#23066,.T.);
#54911=EDGE_CURVE('',#42664,#42665,#1864,.T.);
#54912=EDGE_CURVE('',#42665,#42666,#23067,.T.);
#54913=EDGE_CURVE('',#42666,#42667,#1865,.T.);
#54914=EDGE_CURVE('',#42667,#42668,#23068,.T.);
#54915=EDGE_CURVE('',#42668,#42657,#23069,.T.);
#54916=EDGE_CURVE('',#42669,#42670,#1866,.T.);
#54917=EDGE_CURVE('',#42670,#42671,#23070,.T.);
#54918=EDGE_CURVE('',#42671,#42672,#23071,.T.);
#54919=EDGE_CURVE('',#42672,#42673,#23072,.T.);
#54920=EDGE_CURVE('',#42673,#42674,#1867,.T.);
#54921=EDGE_CURVE('',#42674,#42675,#23073,.T.);
#54922=EDGE_CURVE('',#42675,#42676,#23074,.T.);
#54923=EDGE_CURVE('',#42676,#42677,#1868,.T.);
#54924=EDGE_CURVE('',#42677,#42678,#23075,.T.);
#54925=EDGE_CURVE('',#42678,#42679,#1869,.T.);
#54926=EDGE_CURVE('',#42679,#42680,#23076,.T.);
#54927=EDGE_CURVE('',#42680,#42669,#23077,.T.);
#54928=EDGE_CURVE('',#42681,#42682,#23078,.T.);
#54929=EDGE_CURVE('',#42682,#42683,#34345,.T.);
#54930=EDGE_CURVE('',#42683,#42684,#23079,.T.);
#54931=EDGE_CURVE('',#42684,#42681,#34346,.T.);
#54932=EDGE_CURVE('',#42685,#42686,#1870,.T.);
#54933=EDGE_CURVE('',#42686,#42687,#23080,.T.);
#54934=EDGE_CURVE('',#42687,#42688,#23081,.T.);
#54935=EDGE_CURVE('',#42688,#42689,#23082,.T.);
#54936=EDGE_CURVE('',#42689,#42690,#1871,.T.);
#54937=EDGE_CURVE('',#42690,#42691,#23083,.T.);
#54938=EDGE_CURVE('',#42691,#42692,#23084,.T.);
#54939=EDGE_CURVE('',#42692,#42693,#1872,.T.);
#54940=EDGE_CURVE('',#42693,#42694,#23085,.T.);
#54941=EDGE_CURVE('',#42694,#42695,#1873,.T.);
#54942=EDGE_CURVE('',#42695,#42696,#23086,.T.);
#54943=EDGE_CURVE('',#42696,#42685,#23087,.T.);
#54944=EDGE_CURVE('',#42697,#42698,#1874,.T.);
#54945=EDGE_CURVE('',#42698,#42699,#23088,.T.);
#54946=EDGE_CURVE('',#42699,#42700,#23089,.T.);
#54947=EDGE_CURVE('',#42700,#42701,#23090,.T.);
#54948=EDGE_CURVE('',#42701,#42702,#1875,.T.);
#54949=EDGE_CURVE('',#42702,#42703,#23091,.T.);
#54950=EDGE_CURVE('',#42703,#42704,#23092,.T.);
#54951=EDGE_CURVE('',#42704,#42705,#1876,.T.);
#54952=EDGE_CURVE('',#42705,#42706,#23093,.T.);
#54953=EDGE_CURVE('',#42706,#42707,#1877,.T.);
#54954=EDGE_CURVE('',#42707,#42708,#23094,.T.);
#54955=EDGE_CURVE('',#42708,#42697,#23095,.T.);
#54956=EDGE_CURVE('',#42709,#42710,#23096,.T.);
#54957=EDGE_CURVE('',#42710,#42711,#34347,.T.);
#54958=EDGE_CURVE('',#42711,#42712,#23097,.T.);
#54959=EDGE_CURVE('',#42712,#42709,#34348,.T.);
#54960=EDGE_CURVE('',#42713,#42714,#1878,.T.);
#54961=EDGE_CURVE('',#42714,#42715,#23098,.T.);
#54962=EDGE_CURVE('',#42715,#42716,#23099,.T.);
#54963=EDGE_CURVE('',#42716,#42717,#23100,.T.);
#54964=EDGE_CURVE('',#42717,#42718,#1879,.T.);
#54965=EDGE_CURVE('',#42718,#42719,#23101,.T.);
#54966=EDGE_CURVE('',#42719,#42720,#23102,.T.);
#54967=EDGE_CURVE('',#42720,#42721,#1880,.T.);
#54968=EDGE_CURVE('',#42721,#42722,#23103,.T.);
#54969=EDGE_CURVE('',#42722,#42723,#1881,.T.);
#54970=EDGE_CURVE('',#42723,#42724,#23104,.T.);
#54971=EDGE_CURVE('',#42724,#42713,#23105,.T.);
#54972=EDGE_CURVE('',#42725,#42726,#1882,.T.);
#54973=EDGE_CURVE('',#42726,#42727,#23106,.T.);
#54974=EDGE_CURVE('',#42727,#42728,#23107,.T.);
#54975=EDGE_CURVE('',#42728,#42729,#23108,.T.);
#54976=EDGE_CURVE('',#42729,#42730,#1883,.T.);
#54977=EDGE_CURVE('',#42730,#42731,#23109,.T.);
#54978=EDGE_CURVE('',#42731,#42732,#23110,.T.);
#54979=EDGE_CURVE('',#42732,#42733,#1884,.T.);
#54980=EDGE_CURVE('',#42733,#42734,#23111,.T.);
#54981=EDGE_CURVE('',#42734,#42735,#1885,.T.);
#54982=EDGE_CURVE('',#42735,#42736,#23112,.T.);
#54983=EDGE_CURVE('',#42736,#42725,#23113,.T.);
#54984=EDGE_CURVE('',#42737,#42738,#23114,.T.);
#54985=EDGE_CURVE('',#42738,#42739,#34349,.T.);
#54986=EDGE_CURVE('',#42739,#42740,#23115,.T.);
#54987=EDGE_CURVE('',#42740,#42737,#34350,.T.);
#54988=EDGE_CURVE('',#42741,#42742,#1886,.T.);
#54989=EDGE_CURVE('',#42742,#42743,#23116,.T.);
#54990=EDGE_CURVE('',#42743,#42744,#23117,.T.);
#54991=EDGE_CURVE('',#42744,#42745,#23118,.T.);
#54992=EDGE_CURVE('',#42745,#42746,#1887,.T.);
#54993=EDGE_CURVE('',#42746,#42747,#23119,.T.);
#54994=EDGE_CURVE('',#42747,#42748,#23120,.T.);
#54995=EDGE_CURVE('',#42748,#42749,#1888,.T.);
#54996=EDGE_CURVE('',#42749,#42750,#23121,.T.);
#54997=EDGE_CURVE('',#42750,#42751,#1889,.T.);
#54998=EDGE_CURVE('',#42751,#42752,#23122,.T.);
#54999=EDGE_CURVE('',#42752,#42741,#23123,.T.);
#55000=EDGE_CURVE('',#42753,#42754,#1890,.T.);
#55001=EDGE_CURVE('',#42754,#42755,#23124,.T.);
#55002=EDGE_CURVE('',#42755,#42756,#23125,.T.);
#55003=EDGE_CURVE('',#42756,#42757,#23126,.T.);
#55004=EDGE_CURVE('',#42757,#42758,#1891,.T.);
#55005=EDGE_CURVE('',#42758,#42759,#23127,.T.);
#55006=EDGE_CURVE('',#42759,#42760,#23128,.T.);
#55007=EDGE_CURVE('',#42760,#42761,#1892,.T.);
#55008=EDGE_CURVE('',#42761,#42762,#23129,.T.);
#55009=EDGE_CURVE('',#42762,#42763,#1893,.T.);
#55010=EDGE_CURVE('',#42763,#42764,#23130,.T.);
#55011=EDGE_CURVE('',#42764,#42753,#23131,.T.);
#55012=EDGE_CURVE('',#42765,#42766,#23132,.T.);
#55013=EDGE_CURVE('',#42766,#42767,#34351,.T.);
#55014=EDGE_CURVE('',#42767,#42768,#23133,.T.);
#55015=EDGE_CURVE('',#42768,#42765,#34352,.T.);
#55016=EDGE_CURVE('',#42769,#42770,#1894,.T.);
#55017=EDGE_CURVE('',#42770,#42771,#23134,.T.);
#55018=EDGE_CURVE('',#42771,#42772,#23135,.T.);
#55019=EDGE_CURVE('',#42772,#42773,#23136,.T.);
#55020=EDGE_CURVE('',#42773,#42774,#1895,.T.);
#55021=EDGE_CURVE('',#42774,#42775,#23137,.T.);
#55022=EDGE_CURVE('',#42775,#42776,#23138,.T.);
#55023=EDGE_CURVE('',#42776,#42777,#1896,.T.);
#55024=EDGE_CURVE('',#42777,#42778,#23139,.T.);
#55025=EDGE_CURVE('',#42778,#42779,#1897,.T.);
#55026=EDGE_CURVE('',#42779,#42780,#23140,.T.);
#55027=EDGE_CURVE('',#42780,#42769,#23141,.T.);
#55028=EDGE_CURVE('',#42781,#42782,#1898,.T.);
#55029=EDGE_CURVE('',#42782,#42783,#23142,.T.);
#55030=EDGE_CURVE('',#42783,#42784,#23143,.T.);
#55031=EDGE_CURVE('',#42784,#42785,#23144,.T.);
#55032=EDGE_CURVE('',#42785,#42786,#1899,.T.);
#55033=EDGE_CURVE('',#42786,#42787,#23145,.T.);
#55034=EDGE_CURVE('',#42787,#42788,#23146,.T.);
#55035=EDGE_CURVE('',#42788,#42789,#1900,.T.);
#55036=EDGE_CURVE('',#42789,#42790,#23147,.T.);
#55037=EDGE_CURVE('',#42790,#42791,#1901,.T.);
#55038=EDGE_CURVE('',#42791,#42792,#23148,.T.);
#55039=EDGE_CURVE('',#42792,#42781,#23149,.T.);
#55040=EDGE_CURVE('',#42793,#42794,#23150,.T.);
#55041=EDGE_CURVE('',#42794,#42795,#34353,.T.);
#55042=EDGE_CURVE('',#42795,#42796,#23151,.T.);
#55043=EDGE_CURVE('',#42796,#42793,#34354,.T.);
#55044=EDGE_CURVE('',#42797,#42798,#1902,.T.);
#55045=EDGE_CURVE('',#42798,#42799,#23152,.T.);
#55046=EDGE_CURVE('',#42799,#42800,#23153,.T.);
#55047=EDGE_CURVE('',#42800,#42801,#23154,.T.);
#55048=EDGE_CURVE('',#42801,#42802,#1903,.T.);
#55049=EDGE_CURVE('',#42802,#42803,#23155,.T.);
#55050=EDGE_CURVE('',#42803,#42804,#23156,.T.);
#55051=EDGE_CURVE('',#42804,#42805,#1904,.T.);
#55052=EDGE_CURVE('',#42805,#42806,#23157,.T.);
#55053=EDGE_CURVE('',#42806,#42807,#1905,.T.);
#55054=EDGE_CURVE('',#42807,#42808,#23158,.T.);
#55055=EDGE_CURVE('',#42808,#42797,#23159,.T.);
#55056=EDGE_CURVE('',#42809,#42810,#1906,.T.);
#55057=EDGE_CURVE('',#42810,#42811,#23160,.T.);
#55058=EDGE_CURVE('',#42811,#42812,#23161,.T.);
#55059=EDGE_CURVE('',#42812,#42813,#23162,.T.);
#55060=EDGE_CURVE('',#42813,#42814,#1907,.T.);
#55061=EDGE_CURVE('',#42814,#42815,#23163,.T.);
#55062=EDGE_CURVE('',#42815,#42816,#23164,.T.);
#55063=EDGE_CURVE('',#42816,#42817,#1908,.T.);
#55064=EDGE_CURVE('',#42817,#42818,#23165,.T.);
#55065=EDGE_CURVE('',#42818,#42819,#1909,.T.);
#55066=EDGE_CURVE('',#42819,#42820,#23166,.T.);
#55067=EDGE_CURVE('',#42820,#42809,#23167,.T.);
#55068=EDGE_CURVE('',#42821,#42822,#23168,.T.);
#55069=EDGE_CURVE('',#42822,#42823,#34355,.T.);
#55070=EDGE_CURVE('',#42823,#42824,#23169,.T.);
#55071=EDGE_CURVE('',#42824,#42821,#34356,.T.);
#55072=EDGE_CURVE('',#42825,#42826,#1910,.T.);
#55073=EDGE_CURVE('',#42826,#42827,#23170,.T.);
#55074=EDGE_CURVE('',#42827,#42828,#23171,.T.);
#55075=EDGE_CURVE('',#42828,#42829,#23172,.T.);
#55076=EDGE_CURVE('',#42829,#42830,#1911,.T.);
#55077=EDGE_CURVE('',#42830,#42831,#23173,.T.);
#55078=EDGE_CURVE('',#42831,#42832,#23174,.T.);
#55079=EDGE_CURVE('',#42832,#42833,#1912,.T.);
#55080=EDGE_CURVE('',#42833,#42834,#23175,.T.);
#55081=EDGE_CURVE('',#42834,#42835,#1913,.T.);
#55082=EDGE_CURVE('',#42835,#42836,#23176,.T.);
#55083=EDGE_CURVE('',#42836,#42825,#23177,.T.);
#55084=EDGE_CURVE('',#42837,#42838,#1914,.T.);
#55085=EDGE_CURVE('',#42838,#42839,#23178,.T.);
#55086=EDGE_CURVE('',#42839,#42840,#23179,.T.);
#55087=EDGE_CURVE('',#42840,#42841,#23180,.T.);
#55088=EDGE_CURVE('',#42841,#42842,#1915,.T.);
#55089=EDGE_CURVE('',#42842,#42843,#23181,.T.);
#55090=EDGE_CURVE('',#42843,#42844,#23182,.T.);
#55091=EDGE_CURVE('',#42844,#42845,#1916,.T.);
#55092=EDGE_CURVE('',#42845,#42846,#23183,.T.);
#55093=EDGE_CURVE('',#42846,#42847,#1917,.T.);
#55094=EDGE_CURVE('',#42847,#42848,#23184,.T.);
#55095=EDGE_CURVE('',#42848,#42837,#23185,.T.);
#55096=EDGE_CURVE('',#42849,#42850,#23186,.T.);
#55097=EDGE_CURVE('',#42850,#42851,#34357,.T.);
#55098=EDGE_CURVE('',#42851,#42852,#23187,.T.);
#55099=EDGE_CURVE('',#42852,#42849,#34358,.T.);
#55100=EDGE_CURVE('',#42853,#42854,#1918,.T.);
#55101=EDGE_CURVE('',#42854,#42855,#23188,.T.);
#55102=EDGE_CURVE('',#42855,#42856,#23189,.T.);
#55103=EDGE_CURVE('',#42856,#42857,#23190,.T.);
#55104=EDGE_CURVE('',#42857,#42858,#1919,.T.);
#55105=EDGE_CURVE('',#42858,#42859,#23191,.T.);
#55106=EDGE_CURVE('',#42859,#42860,#23192,.T.);
#55107=EDGE_CURVE('',#42860,#42861,#1920,.T.);
#55108=EDGE_CURVE('',#42861,#42862,#23193,.T.);
#55109=EDGE_CURVE('',#42862,#42863,#1921,.T.);
#55110=EDGE_CURVE('',#42863,#42864,#23194,.T.);
#55111=EDGE_CURVE('',#42864,#42853,#23195,.T.);
#55112=EDGE_CURVE('',#42865,#42866,#1922,.T.);
#55113=EDGE_CURVE('',#42866,#42867,#23196,.T.);
#55114=EDGE_CURVE('',#42867,#42868,#23197,.T.);
#55115=EDGE_CURVE('',#42868,#42869,#23198,.T.);
#55116=EDGE_CURVE('',#42869,#42870,#1923,.T.);
#55117=EDGE_CURVE('',#42870,#42871,#23199,.T.);
#55118=EDGE_CURVE('',#42871,#42872,#23200,.T.);
#55119=EDGE_CURVE('',#42872,#42873,#1924,.T.);
#55120=EDGE_CURVE('',#42873,#42874,#23201,.T.);
#55121=EDGE_CURVE('',#42874,#42875,#1925,.T.);
#55122=EDGE_CURVE('',#42875,#42876,#23202,.T.);
#55123=EDGE_CURVE('',#42876,#42865,#23203,.T.);
#55124=EDGE_CURVE('',#42877,#42878,#23204,.T.);
#55125=EDGE_CURVE('',#42878,#42879,#34359,.T.);
#55126=EDGE_CURVE('',#42879,#42880,#23205,.T.);
#55127=EDGE_CURVE('',#42880,#42877,#34360,.T.);
#55128=EDGE_CURVE('',#42881,#42882,#1926,.T.);
#55129=EDGE_CURVE('',#42882,#42883,#23206,.T.);
#55130=EDGE_CURVE('',#42883,#42884,#23207,.T.);
#55131=EDGE_CURVE('',#42884,#42885,#23208,.T.);
#55132=EDGE_CURVE('',#42885,#42886,#1927,.T.);
#55133=EDGE_CURVE('',#42886,#42887,#23209,.T.);
#55134=EDGE_CURVE('',#42887,#42888,#23210,.T.);
#55135=EDGE_CURVE('',#42888,#42889,#1928,.T.);
#55136=EDGE_CURVE('',#42889,#42890,#23211,.T.);
#55137=EDGE_CURVE('',#42890,#42891,#1929,.T.);
#55138=EDGE_CURVE('',#42891,#42892,#23212,.T.);
#55139=EDGE_CURVE('',#42892,#42881,#23213,.T.);
#55140=EDGE_CURVE('',#42893,#42894,#1930,.T.);
#55141=EDGE_CURVE('',#42894,#42895,#23214,.T.);
#55142=EDGE_CURVE('',#42895,#42896,#23215,.T.);
#55143=EDGE_CURVE('',#42896,#42897,#23216,.T.);
#55144=EDGE_CURVE('',#42897,#42898,#1931,.T.);
#55145=EDGE_CURVE('',#42898,#42899,#23217,.T.);
#55146=EDGE_CURVE('',#42899,#42900,#23218,.T.);
#55147=EDGE_CURVE('',#42900,#42901,#1932,.T.);
#55148=EDGE_CURVE('',#42901,#42902,#23219,.T.);
#55149=EDGE_CURVE('',#42902,#42903,#1933,.T.);
#55150=EDGE_CURVE('',#42903,#42904,#23220,.T.);
#55151=EDGE_CURVE('',#42904,#42893,#23221,.T.);
#55152=EDGE_CURVE('',#42905,#42906,#23222,.T.);
#55153=EDGE_CURVE('',#42906,#42907,#34361,.T.);
#55154=EDGE_CURVE('',#42907,#42908,#23223,.T.);
#55155=EDGE_CURVE('',#42908,#42905,#34362,.T.);
#55156=EDGE_CURVE('',#42909,#42910,#1934,.T.);
#55157=EDGE_CURVE('',#42910,#42911,#23224,.T.);
#55158=EDGE_CURVE('',#42911,#42912,#23225,.T.);
#55159=EDGE_CURVE('',#42912,#42913,#23226,.T.);
#55160=EDGE_CURVE('',#42913,#42914,#1935,.T.);
#55161=EDGE_CURVE('',#42914,#42915,#23227,.T.);
#55162=EDGE_CURVE('',#42915,#42916,#23228,.T.);
#55163=EDGE_CURVE('',#42916,#42917,#1936,.T.);
#55164=EDGE_CURVE('',#42917,#42918,#23229,.T.);
#55165=EDGE_CURVE('',#42918,#42919,#1937,.T.);
#55166=EDGE_CURVE('',#42919,#42920,#23230,.T.);
#55167=EDGE_CURVE('',#42920,#42909,#23231,.T.);
#55168=EDGE_CURVE('',#42921,#42922,#1938,.T.);
#55169=EDGE_CURVE('',#42922,#42923,#23232,.T.);
#55170=EDGE_CURVE('',#42923,#42924,#23233,.T.);
#55171=EDGE_CURVE('',#42924,#42925,#23234,.T.);
#55172=EDGE_CURVE('',#42925,#42926,#1939,.T.);
#55173=EDGE_CURVE('',#42926,#42927,#23235,.T.);
#55174=EDGE_CURVE('',#42927,#42928,#23236,.T.);
#55175=EDGE_CURVE('',#42928,#42929,#1940,.T.);
#55176=EDGE_CURVE('',#42929,#42930,#23237,.T.);
#55177=EDGE_CURVE('',#42930,#42931,#1941,.T.);
#55178=EDGE_CURVE('',#42931,#42932,#23238,.T.);
#55179=EDGE_CURVE('',#42932,#42921,#23239,.T.);
#55180=EDGE_CURVE('',#42933,#42934,#23240,.T.);
#55181=EDGE_CURVE('',#42934,#42935,#34363,.T.);
#55182=EDGE_CURVE('',#42935,#42936,#23241,.T.);
#55183=EDGE_CURVE('',#42936,#42933,#34364,.T.);
#55184=EDGE_CURVE('',#42937,#42938,#1942,.T.);
#55185=EDGE_CURVE('',#42938,#42939,#23242,.T.);
#55186=EDGE_CURVE('',#42939,#42940,#23243,.T.);
#55187=EDGE_CURVE('',#42940,#42941,#23244,.T.);
#55188=EDGE_CURVE('',#42941,#42942,#1943,.T.);
#55189=EDGE_CURVE('',#42942,#42943,#23245,.T.);
#55190=EDGE_CURVE('',#42943,#42944,#23246,.T.);
#55191=EDGE_CURVE('',#42944,#42945,#1944,.T.);
#55192=EDGE_CURVE('',#42945,#42946,#23247,.T.);
#55193=EDGE_CURVE('',#42946,#42947,#1945,.T.);
#55194=EDGE_CURVE('',#42947,#42948,#23248,.T.);
#55195=EDGE_CURVE('',#42948,#42937,#23249,.T.);
#55196=EDGE_CURVE('',#42949,#42950,#1946,.T.);
#55197=EDGE_CURVE('',#42950,#42951,#23250,.T.);
#55198=EDGE_CURVE('',#42951,#42952,#23251,.T.);
#55199=EDGE_CURVE('',#42952,#42953,#23252,.T.);
#55200=EDGE_CURVE('',#42953,#42954,#1947,.T.);
#55201=EDGE_CURVE('',#42954,#42955,#23253,.T.);
#55202=EDGE_CURVE('',#42955,#42956,#23254,.T.);
#55203=EDGE_CURVE('',#42956,#42957,#1948,.T.);
#55204=EDGE_CURVE('',#42957,#42958,#23255,.T.);
#55205=EDGE_CURVE('',#42958,#42959,#1949,.T.);
#55206=EDGE_CURVE('',#42959,#42960,#23256,.T.);
#55207=EDGE_CURVE('',#42960,#42949,#23257,.T.);
#55208=EDGE_CURVE('',#42961,#42962,#23258,.T.);
#55209=EDGE_CURVE('',#42962,#42963,#34365,.T.);
#55210=EDGE_CURVE('',#42963,#42964,#23259,.T.);
#55211=EDGE_CURVE('',#42964,#42961,#34366,.T.);
#55212=EDGE_CURVE('',#42965,#42966,#1950,.T.);
#55213=EDGE_CURVE('',#42966,#42967,#23260,.T.);
#55214=EDGE_CURVE('',#42967,#42968,#23261,.T.);
#55215=EDGE_CURVE('',#42968,#42969,#23262,.T.);
#55216=EDGE_CURVE('',#42969,#42970,#1951,.T.);
#55217=EDGE_CURVE('',#42970,#42971,#23263,.T.);
#55218=EDGE_CURVE('',#42971,#42972,#23264,.T.);
#55219=EDGE_CURVE('',#42972,#42973,#1952,.T.);
#55220=EDGE_CURVE('',#42973,#42974,#23265,.T.);
#55221=EDGE_CURVE('',#42974,#42975,#1953,.T.);
#55222=EDGE_CURVE('',#42975,#42976,#23266,.T.);
#55223=EDGE_CURVE('',#42976,#42965,#23267,.T.);
#55224=EDGE_CURVE('',#42977,#42978,#1954,.T.);
#55225=EDGE_CURVE('',#42978,#42979,#23268,.T.);
#55226=EDGE_CURVE('',#42979,#42980,#23269,.T.);
#55227=EDGE_CURVE('',#42980,#42981,#23270,.T.);
#55228=EDGE_CURVE('',#42981,#42982,#1955,.T.);
#55229=EDGE_CURVE('',#42982,#42983,#23271,.T.);
#55230=EDGE_CURVE('',#42983,#42984,#23272,.T.);
#55231=EDGE_CURVE('',#42984,#42985,#1956,.T.);
#55232=EDGE_CURVE('',#42985,#42986,#23273,.T.);
#55233=EDGE_CURVE('',#42986,#42987,#1957,.T.);
#55234=EDGE_CURVE('',#42987,#42988,#23274,.T.);
#55235=EDGE_CURVE('',#42988,#42977,#23275,.T.);
#55236=EDGE_CURVE('',#42989,#42990,#23276,.T.);
#55237=EDGE_CURVE('',#42990,#42991,#34367,.T.);
#55238=EDGE_CURVE('',#42991,#42992,#23277,.T.);
#55239=EDGE_CURVE('',#42992,#42989,#34368,.T.);
#55240=EDGE_CURVE('',#42993,#42994,#1958,.T.);
#55241=EDGE_CURVE('',#42994,#42995,#23278,.T.);
#55242=EDGE_CURVE('',#42995,#42996,#23279,.T.);
#55243=EDGE_CURVE('',#42996,#42997,#23280,.T.);
#55244=EDGE_CURVE('',#42997,#42998,#1959,.T.);
#55245=EDGE_CURVE('',#42998,#42999,#23281,.T.);
#55246=EDGE_CURVE('',#42999,#43000,#23282,.T.);
#55247=EDGE_CURVE('',#43000,#43001,#1960,.T.);
#55248=EDGE_CURVE('',#43001,#43002,#23283,.T.);
#55249=EDGE_CURVE('',#43002,#43003,#1961,.T.);
#55250=EDGE_CURVE('',#43003,#43004,#23284,.T.);
#55251=EDGE_CURVE('',#43004,#42993,#23285,.T.);
#55252=EDGE_CURVE('',#43005,#43006,#1962,.T.);
#55253=EDGE_CURVE('',#43006,#43007,#23286,.T.);
#55254=EDGE_CURVE('',#43007,#43008,#23287,.T.);
#55255=EDGE_CURVE('',#43008,#43009,#23288,.T.);
#55256=EDGE_CURVE('',#43009,#43010,#1963,.T.);
#55257=EDGE_CURVE('',#43010,#43011,#23289,.T.);
#55258=EDGE_CURVE('',#43011,#43012,#23290,.T.);
#55259=EDGE_CURVE('',#43012,#43013,#1964,.T.);
#55260=EDGE_CURVE('',#43013,#43014,#23291,.T.);
#55261=EDGE_CURVE('',#43014,#43015,#1965,.T.);
#55262=EDGE_CURVE('',#43015,#43016,#23292,.T.);
#55263=EDGE_CURVE('',#43016,#43005,#23293,.T.);
#55264=EDGE_CURVE('',#43017,#43018,#23294,.T.);
#55265=EDGE_CURVE('',#43018,#43019,#34369,.T.);
#55266=EDGE_CURVE('',#43019,#43020,#23295,.T.);
#55267=EDGE_CURVE('',#43020,#43017,#34370,.T.);
#55268=EDGE_CURVE('',#43021,#43022,#1966,.T.);
#55269=EDGE_CURVE('',#43022,#43023,#23296,.T.);
#55270=EDGE_CURVE('',#43023,#43024,#23297,.T.);
#55271=EDGE_CURVE('',#43024,#43025,#23298,.T.);
#55272=EDGE_CURVE('',#43025,#43026,#1967,.T.);
#55273=EDGE_CURVE('',#43026,#43027,#23299,.T.);
#55274=EDGE_CURVE('',#43027,#43028,#23300,.T.);
#55275=EDGE_CURVE('',#43028,#43029,#1968,.T.);
#55276=EDGE_CURVE('',#43029,#43030,#23301,.T.);
#55277=EDGE_CURVE('',#43030,#43031,#1969,.T.);
#55278=EDGE_CURVE('',#43031,#43032,#23302,.T.);
#55279=EDGE_CURVE('',#43032,#43021,#23303,.T.);
#55280=EDGE_CURVE('',#43033,#43034,#1970,.T.);
#55281=EDGE_CURVE('',#43034,#43035,#23304,.T.);
#55282=EDGE_CURVE('',#43035,#43036,#23305,.T.);
#55283=EDGE_CURVE('',#43036,#43037,#23306,.T.);
#55284=EDGE_CURVE('',#43037,#43038,#1971,.T.);
#55285=EDGE_CURVE('',#43038,#43039,#23307,.T.);
#55286=EDGE_CURVE('',#43039,#43040,#23308,.T.);
#55287=EDGE_CURVE('',#43040,#43041,#1972,.T.);
#55288=EDGE_CURVE('',#43041,#43042,#23309,.T.);
#55289=EDGE_CURVE('',#43042,#43043,#1973,.T.);
#55290=EDGE_CURVE('',#43043,#43044,#23310,.T.);
#55291=EDGE_CURVE('',#43044,#43033,#23311,.T.);
#55292=EDGE_CURVE('',#43045,#43046,#23312,.T.);
#55293=EDGE_CURVE('',#43046,#43047,#34371,.T.);
#55294=EDGE_CURVE('',#43047,#43048,#23313,.T.);
#55295=EDGE_CURVE('',#43048,#43045,#34372,.T.);
#55296=EDGE_CURVE('',#43049,#43050,#1974,.T.);
#55297=EDGE_CURVE('',#43050,#43051,#23314,.T.);
#55298=EDGE_CURVE('',#43051,#43052,#23315,.T.);
#55299=EDGE_CURVE('',#43052,#43053,#23316,.T.);
#55300=EDGE_CURVE('',#43053,#43054,#1975,.T.);
#55301=EDGE_CURVE('',#43054,#43055,#23317,.T.);
#55302=EDGE_CURVE('',#43055,#43056,#23318,.T.);
#55303=EDGE_CURVE('',#43056,#43057,#1976,.T.);
#55304=EDGE_CURVE('',#43057,#43058,#23319,.T.);
#55305=EDGE_CURVE('',#43058,#43059,#1977,.T.);
#55306=EDGE_CURVE('',#43059,#43060,#23320,.T.);
#55307=EDGE_CURVE('',#43060,#43049,#23321,.T.);
#55308=EDGE_CURVE('',#43061,#43062,#1978,.T.);
#55309=EDGE_CURVE('',#43062,#43063,#23322,.T.);
#55310=EDGE_CURVE('',#43063,#43064,#23323,.T.);
#55311=EDGE_CURVE('',#43064,#43065,#23324,.T.);
#55312=EDGE_CURVE('',#43065,#43066,#1979,.T.);
#55313=EDGE_CURVE('',#43066,#43067,#23325,.T.);
#55314=EDGE_CURVE('',#43067,#43068,#23326,.T.);
#55315=EDGE_CURVE('',#43068,#43069,#1980,.T.);
#55316=EDGE_CURVE('',#43069,#43070,#23327,.T.);
#55317=EDGE_CURVE('',#43070,#43071,#1981,.T.);
#55318=EDGE_CURVE('',#43071,#43072,#23328,.T.);
#55319=EDGE_CURVE('',#43072,#43061,#23329,.T.);
#55320=EDGE_CURVE('',#43073,#43074,#23330,.T.);
#55321=EDGE_CURVE('',#43074,#43075,#34373,.T.);
#55322=EDGE_CURVE('',#43075,#43076,#23331,.T.);
#55323=EDGE_CURVE('',#43076,#43073,#34374,.T.);
#55324=EDGE_CURVE('',#43077,#43078,#1982,.T.);
#55325=EDGE_CURVE('',#43078,#43079,#23332,.T.);
#55326=EDGE_CURVE('',#43079,#43080,#23333,.T.);
#55327=EDGE_CURVE('',#43080,#43081,#23334,.T.);
#55328=EDGE_CURVE('',#43081,#43082,#1983,.T.);
#55329=EDGE_CURVE('',#43082,#43083,#23335,.T.);
#55330=EDGE_CURVE('',#43083,#43084,#23336,.T.);
#55331=EDGE_CURVE('',#43084,#43085,#1984,.T.);
#55332=EDGE_CURVE('',#43085,#43086,#23337,.T.);
#55333=EDGE_CURVE('',#43086,#43087,#1985,.T.);
#55334=EDGE_CURVE('',#43087,#43088,#23338,.T.);
#55335=EDGE_CURVE('',#43088,#43077,#23339,.T.);
#55336=EDGE_CURVE('',#43089,#43090,#1986,.T.);
#55337=EDGE_CURVE('',#43090,#43091,#23340,.T.);
#55338=EDGE_CURVE('',#43091,#43092,#23341,.T.);
#55339=EDGE_CURVE('',#43092,#43093,#23342,.T.);
#55340=EDGE_CURVE('',#43093,#43094,#1987,.T.);
#55341=EDGE_CURVE('',#43094,#43095,#23343,.T.);
#55342=EDGE_CURVE('',#43095,#43096,#23344,.T.);
#55343=EDGE_CURVE('',#43096,#43097,#1988,.T.);
#55344=EDGE_CURVE('',#43097,#43098,#23345,.T.);
#55345=EDGE_CURVE('',#43098,#43099,#1989,.T.);
#55346=EDGE_CURVE('',#43099,#43100,#23346,.T.);
#55347=EDGE_CURVE('',#43100,#43089,#23347,.T.);
#55348=EDGE_CURVE('',#43101,#43102,#23348,.T.);
#55349=EDGE_CURVE('',#43102,#43103,#34375,.T.);
#55350=EDGE_CURVE('',#43103,#43104,#23349,.T.);
#55351=EDGE_CURVE('',#43104,#43101,#34376,.T.);
#55352=EDGE_CURVE('',#43105,#43106,#1990,.T.);
#55353=EDGE_CURVE('',#43106,#43107,#23350,.T.);
#55354=EDGE_CURVE('',#43107,#43108,#23351,.T.);
#55355=EDGE_CURVE('',#43108,#43109,#23352,.T.);
#55356=EDGE_CURVE('',#43109,#43110,#1991,.T.);
#55357=EDGE_CURVE('',#43110,#43111,#23353,.T.);
#55358=EDGE_CURVE('',#43111,#43112,#23354,.T.);
#55359=EDGE_CURVE('',#43112,#43113,#1992,.T.);
#55360=EDGE_CURVE('',#43113,#43114,#23355,.T.);
#55361=EDGE_CURVE('',#43114,#43115,#1993,.T.);
#55362=EDGE_CURVE('',#43115,#43116,#23356,.T.);
#55363=EDGE_CURVE('',#43116,#43105,#23357,.T.);
#55364=EDGE_CURVE('',#43117,#43118,#1994,.T.);
#55365=EDGE_CURVE('',#43118,#43119,#23358,.T.);
#55366=EDGE_CURVE('',#43119,#43120,#23359,.T.);
#55367=EDGE_CURVE('',#43120,#43121,#23360,.T.);
#55368=EDGE_CURVE('',#43121,#43122,#1995,.T.);
#55369=EDGE_CURVE('',#43122,#43123,#23361,.T.);
#55370=EDGE_CURVE('',#43123,#43124,#23362,.T.);
#55371=EDGE_CURVE('',#43124,#43125,#1996,.T.);
#55372=EDGE_CURVE('',#43125,#43126,#23363,.T.);
#55373=EDGE_CURVE('',#43126,#43127,#1997,.T.);
#55374=EDGE_CURVE('',#43127,#43128,#23364,.T.);
#55375=EDGE_CURVE('',#43128,#43117,#23365,.T.);
#55376=EDGE_CURVE('',#43129,#43130,#23366,.T.);
#55377=EDGE_CURVE('',#43130,#43131,#34377,.T.);
#55378=EDGE_CURVE('',#43131,#43132,#23367,.T.);
#55379=EDGE_CURVE('',#43132,#43129,#34378,.T.);
#55380=EDGE_CURVE('',#43133,#43134,#1998,.T.);
#55381=EDGE_CURVE('',#43134,#43135,#23368,.T.);
#55382=EDGE_CURVE('',#43135,#43136,#23369,.T.);
#55383=EDGE_CURVE('',#43136,#43137,#23370,.T.);
#55384=EDGE_CURVE('',#43137,#43138,#1999,.T.);
#55385=EDGE_CURVE('',#43138,#43139,#23371,.T.);
#55386=EDGE_CURVE('',#43139,#43140,#23372,.T.);
#55387=EDGE_CURVE('',#43140,#43141,#2000,.T.);
#55388=EDGE_CURVE('',#43141,#43142,#23373,.T.);
#55389=EDGE_CURVE('',#43142,#43143,#2001,.T.);
#55390=EDGE_CURVE('',#43143,#43144,#23374,.T.);
#55391=EDGE_CURVE('',#43144,#43133,#23375,.T.);
#55392=EDGE_CURVE('',#43145,#43146,#2002,.T.);
#55393=EDGE_CURVE('',#43146,#43147,#23376,.T.);
#55394=EDGE_CURVE('',#43147,#43148,#23377,.T.);
#55395=EDGE_CURVE('',#43148,#43149,#23378,.T.);
#55396=EDGE_CURVE('',#43149,#43150,#2003,.T.);
#55397=EDGE_CURVE('',#43150,#43151,#23379,.T.);
#55398=EDGE_CURVE('',#43151,#43152,#23380,.T.);
#55399=EDGE_CURVE('',#43152,#43153,#2004,.T.);
#55400=EDGE_CURVE('',#43153,#43154,#23381,.T.);
#55401=EDGE_CURVE('',#43154,#43155,#2005,.T.);
#55402=EDGE_CURVE('',#43155,#43156,#23382,.T.);
#55403=EDGE_CURVE('',#43156,#43145,#23383,.T.);
#55404=EDGE_CURVE('',#43157,#43158,#23384,.T.);
#55405=EDGE_CURVE('',#43158,#43159,#34379,.T.);
#55406=EDGE_CURVE('',#43159,#43160,#23385,.T.);
#55407=EDGE_CURVE('',#43160,#43157,#34380,.T.);
#55408=EDGE_CURVE('',#43161,#43162,#2006,.T.);
#55409=EDGE_CURVE('',#43162,#43163,#23386,.T.);
#55410=EDGE_CURVE('',#43163,#43164,#23387,.T.);
#55411=EDGE_CURVE('',#43164,#43165,#23388,.T.);
#55412=EDGE_CURVE('',#43165,#43166,#2007,.T.);
#55413=EDGE_CURVE('',#43166,#43167,#23389,.T.);
#55414=EDGE_CURVE('',#43167,#43168,#23390,.T.);
#55415=EDGE_CURVE('',#43168,#43169,#2008,.T.);
#55416=EDGE_CURVE('',#43169,#43170,#23391,.T.);
#55417=EDGE_CURVE('',#43170,#43171,#2009,.T.);
#55418=EDGE_CURVE('',#43171,#43172,#23392,.T.);
#55419=EDGE_CURVE('',#43172,#43161,#23393,.T.);
#55420=EDGE_CURVE('',#43173,#43174,#2010,.T.);
#55421=EDGE_CURVE('',#43174,#43175,#23394,.T.);
#55422=EDGE_CURVE('',#43175,#43176,#23395,.T.);
#55423=EDGE_CURVE('',#43176,#43177,#23396,.T.);
#55424=EDGE_CURVE('',#43177,#43178,#2011,.T.);
#55425=EDGE_CURVE('',#43178,#43179,#23397,.T.);
#55426=EDGE_CURVE('',#43179,#43180,#23398,.T.);
#55427=EDGE_CURVE('',#43180,#43181,#2012,.T.);
#55428=EDGE_CURVE('',#43181,#43182,#23399,.T.);
#55429=EDGE_CURVE('',#43182,#43183,#2013,.T.);
#55430=EDGE_CURVE('',#43183,#43184,#23400,.T.);
#55431=EDGE_CURVE('',#43184,#43173,#23401,.T.);
#55432=EDGE_CURVE('',#43185,#43186,#23402,.T.);
#55433=EDGE_CURVE('',#43186,#43187,#34381,.T.);
#55434=EDGE_CURVE('',#43187,#43188,#23403,.T.);
#55435=EDGE_CURVE('',#43188,#43185,#34382,.T.);
#55436=EDGE_CURVE('',#43189,#43190,#2014,.T.);
#55437=EDGE_CURVE('',#43190,#43191,#23404,.T.);
#55438=EDGE_CURVE('',#43191,#43192,#23405,.T.);
#55439=EDGE_CURVE('',#43192,#43193,#23406,.T.);
#55440=EDGE_CURVE('',#43193,#43194,#2015,.T.);
#55441=EDGE_CURVE('',#43194,#43195,#23407,.T.);
#55442=EDGE_CURVE('',#43195,#43196,#23408,.T.);
#55443=EDGE_CURVE('',#43196,#43197,#2016,.T.);
#55444=EDGE_CURVE('',#43197,#43198,#23409,.T.);
#55445=EDGE_CURVE('',#43198,#43199,#2017,.T.);
#55446=EDGE_CURVE('',#43199,#43200,#23410,.T.);
#55447=EDGE_CURVE('',#43200,#43189,#23411,.T.);
#55448=EDGE_CURVE('',#43201,#43202,#2018,.T.);
#55449=EDGE_CURVE('',#43202,#43203,#23412,.T.);
#55450=EDGE_CURVE('',#43203,#43204,#23413,.T.);
#55451=EDGE_CURVE('',#43204,#43205,#23414,.T.);
#55452=EDGE_CURVE('',#43205,#43206,#2019,.T.);
#55453=EDGE_CURVE('',#43206,#43207,#23415,.T.);
#55454=EDGE_CURVE('',#43207,#43208,#23416,.T.);
#55455=EDGE_CURVE('',#43208,#43209,#2020,.T.);
#55456=EDGE_CURVE('',#43209,#43210,#23417,.T.);
#55457=EDGE_CURVE('',#43210,#43211,#2021,.T.);
#55458=EDGE_CURVE('',#43211,#43212,#23418,.T.);
#55459=EDGE_CURVE('',#43212,#43201,#23419,.T.);
#55460=EDGE_CURVE('',#40437,#40443,#23420,.T.);
#55461=EDGE_CURVE('',#40442,#40436,#23421,.T.);
#55462=EDGE_CURVE('',#43213,#43214,#2022,.T.);
#55463=EDGE_CURVE('',#43214,#43215,#23422,.T.);
#55464=EDGE_CURVE('',#43215,#43216,#23423,.T.);
#55465=EDGE_CURVE('',#43216,#43217,#23424,.T.);
#55466=EDGE_CURVE('',#43217,#43218,#2023,.T.);
#55467=EDGE_CURVE('',#43218,#43219,#23425,.T.);
#55468=EDGE_CURVE('',#43219,#43220,#23426,.T.);
#55469=EDGE_CURVE('',#43220,#43221,#2024,.T.);
#55470=EDGE_CURVE('',#43221,#43222,#23427,.T.);
#55471=EDGE_CURVE('',#43222,#43223,#2025,.T.);
#55472=EDGE_CURVE('',#43223,#43224,#23428,.T.);
#55473=EDGE_CURVE('',#43224,#43213,#23429,.T.);
#55474=EDGE_CURVE('',#43225,#43226,#2026,.T.);
#55475=EDGE_CURVE('',#43226,#43227,#23430,.T.);
#55476=EDGE_CURVE('',#43227,#43228,#23431,.T.);
#55477=EDGE_CURVE('',#43228,#43229,#23432,.T.);
#55478=EDGE_CURVE('',#43229,#43230,#2027,.T.);
#55479=EDGE_CURVE('',#43230,#43231,#23433,.T.);
#55480=EDGE_CURVE('',#43231,#43232,#23434,.T.);
#55481=EDGE_CURVE('',#43232,#43233,#2028,.T.);
#55482=EDGE_CURVE('',#43233,#43234,#23435,.T.);
#55483=EDGE_CURVE('',#43234,#43235,#2029,.T.);
#55484=EDGE_CURVE('',#43235,#43236,#23436,.T.);
#55485=EDGE_CURVE('',#43236,#43225,#23437,.T.);
#55486=EDGE_CURVE('',#43237,#43238,#23438,.T.);
#55487=EDGE_CURVE('',#43238,#43239,#34383,.T.);
#55488=EDGE_CURVE('',#43239,#43240,#23439,.T.);
#55489=EDGE_CURVE('',#43240,#43237,#34384,.T.);
#55490=EDGE_CURVE('',#43241,#43242,#2030,.T.);
#55491=EDGE_CURVE('',#43242,#43243,#23440,.T.);
#55492=EDGE_CURVE('',#43243,#43244,#23441,.T.);
#55493=EDGE_CURVE('',#43244,#43245,#23442,.T.);
#55494=EDGE_CURVE('',#43245,#43246,#2031,.T.);
#55495=EDGE_CURVE('',#43246,#43247,#23443,.T.);
#55496=EDGE_CURVE('',#43247,#43248,#23444,.T.);
#55497=EDGE_CURVE('',#43248,#43249,#2032,.T.);
#55498=EDGE_CURVE('',#43249,#43250,#23445,.T.);
#55499=EDGE_CURVE('',#43250,#43251,#2033,.T.);
#55500=EDGE_CURVE('',#43251,#43252,#23446,.T.);
#55501=EDGE_CURVE('',#43252,#43241,#23447,.T.);
#55502=EDGE_CURVE('',#43253,#43254,#2034,.T.);
#55503=EDGE_CURVE('',#43254,#43255,#23448,.T.);
#55504=EDGE_CURVE('',#43255,#43256,#23449,.T.);
#55505=EDGE_CURVE('',#43256,#43257,#23450,.T.);
#55506=EDGE_CURVE('',#43257,#43258,#2035,.T.);
#55507=EDGE_CURVE('',#43258,#43259,#23451,.T.);
#55508=EDGE_CURVE('',#43259,#43260,#23452,.T.);
#55509=EDGE_CURVE('',#43260,#43261,#2036,.T.);
#55510=EDGE_CURVE('',#43261,#43262,#23453,.T.);
#55511=EDGE_CURVE('',#43262,#43263,#2037,.T.);
#55512=EDGE_CURVE('',#43263,#43264,#23454,.T.);
#55513=EDGE_CURVE('',#43264,#43253,#23455,.T.);
#55514=EDGE_CURVE('',#43265,#43266,#23456,.T.);
#55515=EDGE_CURVE('',#43266,#43267,#34385,.T.);
#55516=EDGE_CURVE('',#43267,#43268,#23457,.T.);
#55517=EDGE_CURVE('',#43268,#43265,#34386,.T.);
#55518=EDGE_CURVE('',#43269,#43270,#2038,.T.);
#55519=EDGE_CURVE('',#43270,#43271,#23458,.T.);
#55520=EDGE_CURVE('',#43271,#43272,#23459,.T.);
#55521=EDGE_CURVE('',#43272,#43273,#23460,.T.);
#55522=EDGE_CURVE('',#43273,#43274,#2039,.T.);
#55523=EDGE_CURVE('',#43274,#43275,#23461,.T.);
#55524=EDGE_CURVE('',#43275,#43276,#23462,.T.);
#55525=EDGE_CURVE('',#43276,#43277,#2040,.T.);
#55526=EDGE_CURVE('',#43277,#43278,#23463,.T.);
#55527=EDGE_CURVE('',#43278,#43279,#2041,.T.);
#55528=EDGE_CURVE('',#43279,#43280,#23464,.T.);
#55529=EDGE_CURVE('',#43280,#43269,#23465,.T.);
#55530=EDGE_CURVE('',#43281,#43282,#2042,.T.);
#55531=EDGE_CURVE('',#43282,#43283,#23466,.T.);
#55532=EDGE_CURVE('',#43283,#43284,#23467,.T.);
#55533=EDGE_CURVE('',#43284,#43285,#23468,.T.);
#55534=EDGE_CURVE('',#43285,#43286,#2043,.T.);
#55535=EDGE_CURVE('',#43286,#43287,#23469,.T.);
#55536=EDGE_CURVE('',#43287,#43288,#23470,.T.);
#55537=EDGE_CURVE('',#43288,#43289,#2044,.T.);
#55538=EDGE_CURVE('',#43289,#43290,#23471,.T.);
#55539=EDGE_CURVE('',#43290,#43291,#2045,.T.);
#55540=EDGE_CURVE('',#43291,#43292,#23472,.T.);
#55541=EDGE_CURVE('',#43292,#43281,#23473,.T.);
#55542=EDGE_CURVE('',#43293,#43294,#23474,.T.);
#55543=EDGE_CURVE('',#43294,#43295,#34387,.T.);
#55544=EDGE_CURVE('',#43295,#43296,#23475,.T.);
#55545=EDGE_CURVE('',#43296,#43293,#34388,.T.);
#55546=EDGE_CURVE('',#43297,#43298,#2046,.T.);
#55547=EDGE_CURVE('',#43298,#43299,#23476,.T.);
#55548=EDGE_CURVE('',#43299,#43300,#23477,.T.);
#55549=EDGE_CURVE('',#43300,#43301,#23478,.T.);
#55550=EDGE_CURVE('',#43301,#43302,#2047,.T.);
#55551=EDGE_CURVE('',#43302,#43303,#23479,.T.);
#55552=EDGE_CURVE('',#43303,#43304,#23480,.T.);
#55553=EDGE_CURVE('',#43304,#43305,#2048,.T.);
#55554=EDGE_CURVE('',#43305,#43306,#23481,.T.);
#55555=EDGE_CURVE('',#43306,#43307,#2049,.T.);
#55556=EDGE_CURVE('',#43307,#43308,#23482,.T.);
#55557=EDGE_CURVE('',#43308,#43297,#23483,.T.);
#55558=EDGE_CURVE('',#43309,#43310,#2050,.T.);
#55559=EDGE_CURVE('',#43310,#43311,#23484,.T.);
#55560=EDGE_CURVE('',#43311,#43312,#23485,.T.);
#55561=EDGE_CURVE('',#43312,#43313,#23486,.T.);
#55562=EDGE_CURVE('',#43313,#43314,#2051,.T.);
#55563=EDGE_CURVE('',#43314,#43315,#23487,.T.);
#55564=EDGE_CURVE('',#43315,#43316,#23488,.T.);
#55565=EDGE_CURVE('',#43316,#43317,#2052,.T.);
#55566=EDGE_CURVE('',#43317,#43318,#23489,.T.);
#55567=EDGE_CURVE('',#43318,#43319,#2053,.T.);
#55568=EDGE_CURVE('',#43319,#43320,#23490,.T.);
#55569=EDGE_CURVE('',#43320,#43309,#23491,.T.);
#55570=EDGE_CURVE('',#43321,#43322,#23492,.T.);
#55571=EDGE_CURVE('',#43322,#43323,#34389,.T.);
#55572=EDGE_CURVE('',#43323,#43324,#23493,.T.);
#55573=EDGE_CURVE('',#43324,#43321,#34390,.T.);
#55574=EDGE_CURVE('',#43325,#43326,#2054,.T.);
#55575=EDGE_CURVE('',#43326,#43327,#23494,.T.);
#55576=EDGE_CURVE('',#43327,#43328,#23495,.T.);
#55577=EDGE_CURVE('',#43328,#43329,#23496,.T.);
#55578=EDGE_CURVE('',#43329,#43330,#2055,.T.);
#55579=EDGE_CURVE('',#43330,#43331,#23497,.T.);
#55580=EDGE_CURVE('',#43331,#43332,#23498,.T.);
#55581=EDGE_CURVE('',#43332,#43333,#2056,.T.);
#55582=EDGE_CURVE('',#43333,#43334,#23499,.T.);
#55583=EDGE_CURVE('',#43334,#43335,#2057,.T.);
#55584=EDGE_CURVE('',#43335,#43336,#23500,.T.);
#55585=EDGE_CURVE('',#43336,#43325,#23501,.T.);
#55586=EDGE_CURVE('',#43337,#43338,#2058,.T.);
#55587=EDGE_CURVE('',#43338,#43339,#23502,.T.);
#55588=EDGE_CURVE('',#43339,#43340,#23503,.T.);
#55589=EDGE_CURVE('',#43340,#43341,#23504,.T.);
#55590=EDGE_CURVE('',#43341,#43342,#2059,.T.);
#55591=EDGE_CURVE('',#43342,#43343,#23505,.T.);
#55592=EDGE_CURVE('',#43343,#43344,#23506,.T.);
#55593=EDGE_CURVE('',#43344,#43345,#2060,.T.);
#55594=EDGE_CURVE('',#43345,#43346,#23507,.T.);
#55595=EDGE_CURVE('',#43346,#43347,#2061,.T.);
#55596=EDGE_CURVE('',#43347,#43348,#23508,.T.);
#55597=EDGE_CURVE('',#43348,#43337,#23509,.T.);
#55598=EDGE_CURVE('',#43349,#43350,#23510,.T.);
#55599=EDGE_CURVE('',#43350,#43351,#34391,.T.);
#55600=EDGE_CURVE('',#43351,#43352,#23511,.T.);
#55601=EDGE_CURVE('',#43352,#43349,#34392,.T.);
#55602=EDGE_CURVE('',#43353,#43354,#2062,.T.);
#55603=EDGE_CURVE('',#43354,#43355,#23512,.T.);
#55604=EDGE_CURVE('',#43355,#43356,#23513,.T.);
#55605=EDGE_CURVE('',#43356,#43357,#23514,.T.);
#55606=EDGE_CURVE('',#43357,#43358,#2063,.T.);
#55607=EDGE_CURVE('',#43358,#43359,#23515,.T.);
#55608=EDGE_CURVE('',#43359,#43360,#23516,.T.);
#55609=EDGE_CURVE('',#43360,#43361,#2064,.T.);
#55610=EDGE_CURVE('',#43361,#43362,#23517,.T.);
#55611=EDGE_CURVE('',#43362,#43363,#2065,.T.);
#55612=EDGE_CURVE('',#43363,#43364,#23518,.T.);
#55613=EDGE_CURVE('',#43364,#43353,#23519,.T.);
#55614=EDGE_CURVE('',#43365,#43366,#2066,.T.);
#55615=EDGE_CURVE('',#43366,#43367,#23520,.T.);
#55616=EDGE_CURVE('',#43367,#43368,#23521,.T.);
#55617=EDGE_CURVE('',#43368,#43369,#23522,.T.);
#55618=EDGE_CURVE('',#43369,#43370,#2067,.T.);
#55619=EDGE_CURVE('',#43370,#43371,#23523,.T.);
#55620=EDGE_CURVE('',#43371,#43372,#23524,.T.);
#55621=EDGE_CURVE('',#43372,#43373,#2068,.T.);
#55622=EDGE_CURVE('',#43373,#43374,#23525,.T.);
#55623=EDGE_CURVE('',#43374,#43375,#2069,.T.);
#55624=EDGE_CURVE('',#43375,#43376,#23526,.T.);
#55625=EDGE_CURVE('',#43376,#43365,#23527,.T.);
#55626=EDGE_CURVE('',#43377,#43378,#23528,.T.);
#55627=EDGE_CURVE('',#43378,#43379,#34393,.T.);
#55628=EDGE_CURVE('',#43379,#43380,#23529,.T.);
#55629=EDGE_CURVE('',#43380,#43377,#34394,.T.);
#55630=EDGE_CURVE('',#43381,#43382,#2070,.T.);
#55631=EDGE_CURVE('',#43382,#43383,#23530,.T.);
#55632=EDGE_CURVE('',#43383,#43384,#23531,.T.);
#55633=EDGE_CURVE('',#43384,#43385,#23532,.T.);
#55634=EDGE_CURVE('',#43385,#43386,#2071,.T.);
#55635=EDGE_CURVE('',#43386,#43387,#23533,.T.);
#55636=EDGE_CURVE('',#43387,#43388,#23534,.T.);
#55637=EDGE_CURVE('',#43388,#43389,#2072,.T.);
#55638=EDGE_CURVE('',#43389,#43390,#23535,.T.);
#55639=EDGE_CURVE('',#43390,#43391,#2073,.T.);
#55640=EDGE_CURVE('',#43391,#43392,#23536,.T.);
#55641=EDGE_CURVE('',#43392,#43381,#23537,.T.);
#55642=EDGE_CURVE('',#43393,#43394,#2074,.T.);
#55643=EDGE_CURVE('',#43394,#43395,#23538,.T.);
#55644=EDGE_CURVE('',#43395,#43396,#23539,.T.);
#55645=EDGE_CURVE('',#43396,#43397,#23540,.T.);
#55646=EDGE_CURVE('',#43397,#43398,#2075,.T.);
#55647=EDGE_CURVE('',#43398,#43399,#23541,.T.);
#55648=EDGE_CURVE('',#43399,#43400,#23542,.T.);
#55649=EDGE_CURVE('',#43400,#43401,#2076,.T.);
#55650=EDGE_CURVE('',#43401,#43402,#23543,.T.);
#55651=EDGE_CURVE('',#43402,#43403,#2077,.T.);
#55652=EDGE_CURVE('',#43403,#43404,#23544,.T.);
#55653=EDGE_CURVE('',#43404,#43393,#23545,.T.);
#55654=EDGE_CURVE('',#43405,#43406,#23546,.T.);
#55655=EDGE_CURVE('',#43406,#43407,#34395,.T.);
#55656=EDGE_CURVE('',#43407,#43408,#23547,.T.);
#55657=EDGE_CURVE('',#43408,#43405,#34396,.T.);
#55658=EDGE_CURVE('',#43409,#43410,#2078,.T.);
#55659=EDGE_CURVE('',#43410,#43411,#23548,.T.);
#55660=EDGE_CURVE('',#43411,#43412,#23549,.T.);
#55661=EDGE_CURVE('',#43412,#43413,#23550,.T.);
#55662=EDGE_CURVE('',#43413,#43414,#2079,.T.);
#55663=EDGE_CURVE('',#43414,#43415,#23551,.T.);
#55664=EDGE_CURVE('',#43415,#43416,#23552,.T.);
#55665=EDGE_CURVE('',#43416,#43417,#2080,.T.);
#55666=EDGE_CURVE('',#43417,#43418,#23553,.T.);
#55667=EDGE_CURVE('',#43418,#43419,#2081,.T.);
#55668=EDGE_CURVE('',#43419,#43420,#23554,.T.);
#55669=EDGE_CURVE('',#43420,#43409,#23555,.T.);
#55670=EDGE_CURVE('',#43421,#43422,#2082,.T.);
#55671=EDGE_CURVE('',#43422,#43423,#23556,.T.);
#55672=EDGE_CURVE('',#43423,#43424,#23557,.T.);
#55673=EDGE_CURVE('',#43424,#43425,#23558,.T.);
#55674=EDGE_CURVE('',#43425,#43426,#2083,.T.);
#55675=EDGE_CURVE('',#43426,#43427,#23559,.T.);
#55676=EDGE_CURVE('',#43427,#43428,#23560,.T.);
#55677=EDGE_CURVE('',#43428,#43429,#2084,.T.);
#55678=EDGE_CURVE('',#43429,#43430,#23561,.T.);
#55679=EDGE_CURVE('',#43430,#43431,#2085,.T.);
#55680=EDGE_CURVE('',#43431,#43432,#23562,.T.);
#55681=EDGE_CURVE('',#43432,#43421,#23563,.T.);
#55682=EDGE_CURVE('',#43433,#43434,#23564,.T.);
#55683=EDGE_CURVE('',#43434,#43435,#34397,.T.);
#55684=EDGE_CURVE('',#43435,#43436,#23565,.T.);
#55685=EDGE_CURVE('',#43436,#43433,#34398,.T.);
#55686=EDGE_CURVE('',#43437,#43438,#2086,.T.);
#55687=EDGE_CURVE('',#43438,#43439,#23566,.T.);
#55688=EDGE_CURVE('',#43439,#43440,#23567,.T.);
#55689=EDGE_CURVE('',#43440,#43441,#23568,.T.);
#55690=EDGE_CURVE('',#43441,#43442,#2087,.T.);
#55691=EDGE_CURVE('',#43442,#43443,#23569,.T.);
#55692=EDGE_CURVE('',#43443,#43444,#23570,.T.);
#55693=EDGE_CURVE('',#43444,#43445,#2088,.T.);
#55694=EDGE_CURVE('',#43445,#43446,#23571,.T.);
#55695=EDGE_CURVE('',#43446,#43447,#2089,.T.);
#55696=EDGE_CURVE('',#43447,#43448,#23572,.T.);
#55697=EDGE_CURVE('',#43448,#43437,#23573,.T.);
#55698=EDGE_CURVE('',#43449,#43450,#2090,.T.);
#55699=EDGE_CURVE('',#43450,#43451,#23574,.T.);
#55700=EDGE_CURVE('',#43451,#43452,#23575,.T.);
#55701=EDGE_CURVE('',#43452,#43453,#23576,.T.);
#55702=EDGE_CURVE('',#43453,#43454,#2091,.T.);
#55703=EDGE_CURVE('',#43454,#43455,#23577,.T.);
#55704=EDGE_CURVE('',#43455,#43456,#23578,.T.);
#55705=EDGE_CURVE('',#43456,#43457,#2092,.T.);
#55706=EDGE_CURVE('',#43457,#43458,#23579,.T.);
#55707=EDGE_CURVE('',#43458,#43459,#2093,.T.);
#55708=EDGE_CURVE('',#43459,#43460,#23580,.T.);
#55709=EDGE_CURVE('',#43460,#43449,#23581,.T.);
#55710=EDGE_CURVE('',#43461,#43462,#23582,.T.);
#55711=EDGE_CURVE('',#43462,#43463,#34399,.T.);
#55712=EDGE_CURVE('',#43463,#43464,#23583,.T.);
#55713=EDGE_CURVE('',#43464,#43461,#34400,.T.);
#55714=EDGE_CURVE('',#43465,#43466,#2094,.T.);
#55715=EDGE_CURVE('',#43466,#43467,#23584,.T.);
#55716=EDGE_CURVE('',#43467,#43468,#23585,.T.);
#55717=EDGE_CURVE('',#43468,#43469,#23586,.T.);
#55718=EDGE_CURVE('',#43469,#43470,#2095,.T.);
#55719=EDGE_CURVE('',#43470,#43471,#23587,.T.);
#55720=EDGE_CURVE('',#43471,#43472,#23588,.T.);
#55721=EDGE_CURVE('',#43472,#43473,#2096,.T.);
#55722=EDGE_CURVE('',#43473,#43474,#23589,.T.);
#55723=EDGE_CURVE('',#43474,#43475,#2097,.T.);
#55724=EDGE_CURVE('',#43475,#43476,#23590,.T.);
#55725=EDGE_CURVE('',#43476,#43465,#23591,.T.);
#55726=EDGE_CURVE('',#43477,#43478,#2098,.T.);
#55727=EDGE_CURVE('',#43478,#43479,#23592,.T.);
#55728=EDGE_CURVE('',#43479,#43480,#23593,.T.);
#55729=EDGE_CURVE('',#43480,#43481,#23594,.T.);
#55730=EDGE_CURVE('',#43481,#43482,#2099,.T.);
#55731=EDGE_CURVE('',#43482,#43483,#23595,.T.);
#55732=EDGE_CURVE('',#43483,#43484,#23596,.T.);
#55733=EDGE_CURVE('',#43484,#43485,#2100,.T.);
#55734=EDGE_CURVE('',#43485,#43486,#23597,.T.);
#55735=EDGE_CURVE('',#43486,#43487,#2101,.T.);
#55736=EDGE_CURVE('',#43487,#43488,#23598,.T.);
#55737=EDGE_CURVE('',#43488,#43477,#23599,.T.);
#55738=EDGE_CURVE('',#43489,#43490,#23600,.T.);
#55739=EDGE_CURVE('',#43490,#43491,#34401,.T.);
#55740=EDGE_CURVE('',#43491,#43492,#23601,.T.);
#55741=EDGE_CURVE('',#43492,#43489,#34402,.T.);
#55742=EDGE_CURVE('',#43493,#43494,#2102,.T.);
#55743=EDGE_CURVE('',#43494,#43495,#23602,.T.);
#55744=EDGE_CURVE('',#43495,#43496,#23603,.T.);
#55745=EDGE_CURVE('',#43496,#43497,#23604,.T.);
#55746=EDGE_CURVE('',#43497,#43498,#2103,.T.);
#55747=EDGE_CURVE('',#43498,#43499,#23605,.T.);
#55748=EDGE_CURVE('',#43499,#43500,#23606,.T.);
#55749=EDGE_CURVE('',#43500,#43501,#2104,.T.);
#55750=EDGE_CURVE('',#43501,#43502,#23607,.T.);
#55751=EDGE_CURVE('',#43502,#43503,#2105,.T.);
#55752=EDGE_CURVE('',#43503,#43504,#23608,.T.);
#55753=EDGE_CURVE('',#43504,#43493,#23609,.T.);
#55754=EDGE_CURVE('',#43505,#43506,#2106,.T.);
#55755=EDGE_CURVE('',#43506,#43507,#23610,.T.);
#55756=EDGE_CURVE('',#43507,#43508,#23611,.T.);
#55757=EDGE_CURVE('',#43508,#43509,#23612,.T.);
#55758=EDGE_CURVE('',#43509,#43510,#2107,.T.);
#55759=EDGE_CURVE('',#43510,#43511,#23613,.T.);
#55760=EDGE_CURVE('',#43511,#43512,#23614,.T.);
#55761=EDGE_CURVE('',#43512,#43513,#2108,.T.);
#55762=EDGE_CURVE('',#43513,#43514,#23615,.T.);
#55763=EDGE_CURVE('',#43514,#43515,#2109,.T.);
#55764=EDGE_CURVE('',#43515,#43516,#23616,.T.);
#55765=EDGE_CURVE('',#43516,#43505,#23617,.T.);
#55766=EDGE_CURVE('',#43517,#43518,#23618,.T.);
#55767=EDGE_CURVE('',#43518,#43519,#34403,.T.);
#55768=EDGE_CURVE('',#43519,#43520,#23619,.T.);
#55769=EDGE_CURVE('',#43520,#43517,#34404,.T.);
#55770=EDGE_CURVE('',#43521,#43522,#2110,.T.);
#55771=EDGE_CURVE('',#43522,#43523,#23620,.T.);
#55772=EDGE_CURVE('',#43523,#43524,#23621,.T.);
#55773=EDGE_CURVE('',#43524,#43525,#23622,.T.);
#55774=EDGE_CURVE('',#43525,#43526,#2111,.T.);
#55775=EDGE_CURVE('',#43526,#43527,#23623,.T.);
#55776=EDGE_CURVE('',#43527,#43528,#23624,.T.);
#55777=EDGE_CURVE('',#43528,#43529,#2112,.T.);
#55778=EDGE_CURVE('',#43529,#43530,#23625,.T.);
#55779=EDGE_CURVE('',#43530,#43531,#2113,.T.);
#55780=EDGE_CURVE('',#43531,#43532,#23626,.T.);
#55781=EDGE_CURVE('',#43532,#43521,#23627,.T.);
#55782=EDGE_CURVE('',#43533,#43534,#2114,.T.);
#55783=EDGE_CURVE('',#43534,#43535,#23628,.T.);
#55784=EDGE_CURVE('',#43535,#43536,#23629,.T.);
#55785=EDGE_CURVE('',#43536,#43537,#23630,.T.);
#55786=EDGE_CURVE('',#43537,#43538,#2115,.T.);
#55787=EDGE_CURVE('',#43538,#43539,#23631,.T.);
#55788=EDGE_CURVE('',#43539,#43540,#23632,.T.);
#55789=EDGE_CURVE('',#43540,#43541,#2116,.T.);
#55790=EDGE_CURVE('',#43541,#43542,#23633,.T.);
#55791=EDGE_CURVE('',#43542,#43543,#2117,.T.);
#55792=EDGE_CURVE('',#43543,#43544,#23634,.T.);
#55793=EDGE_CURVE('',#43544,#43533,#23635,.T.);
#55794=EDGE_CURVE('',#43545,#43546,#23636,.T.);
#55795=EDGE_CURVE('',#43546,#43547,#34405,.T.);
#55796=EDGE_CURVE('',#43547,#43548,#23637,.T.);
#55797=EDGE_CURVE('',#43548,#43545,#34406,.T.);
#55798=EDGE_CURVE('',#43549,#43550,#2118,.T.);
#55799=EDGE_CURVE('',#43550,#43551,#23638,.T.);
#55800=EDGE_CURVE('',#43551,#43552,#23639,.T.);
#55801=EDGE_CURVE('',#43552,#43553,#23640,.T.);
#55802=EDGE_CURVE('',#43553,#43554,#2119,.T.);
#55803=EDGE_CURVE('',#43554,#43555,#23641,.T.);
#55804=EDGE_CURVE('',#43555,#43556,#23642,.T.);
#55805=EDGE_CURVE('',#43556,#43557,#2120,.T.);
#55806=EDGE_CURVE('',#43557,#43558,#23643,.T.);
#55807=EDGE_CURVE('',#43558,#43559,#2121,.T.);
#55808=EDGE_CURVE('',#43559,#43560,#23644,.T.);
#55809=EDGE_CURVE('',#43560,#43549,#23645,.T.);
#55810=EDGE_CURVE('',#43561,#43562,#2122,.T.);
#55811=EDGE_CURVE('',#43562,#43563,#23646,.T.);
#55812=EDGE_CURVE('',#43563,#43564,#23647,.T.);
#55813=EDGE_CURVE('',#43564,#43565,#23648,.T.);
#55814=EDGE_CURVE('',#43565,#43566,#2123,.T.);
#55815=EDGE_CURVE('',#43566,#43567,#23649,.T.);
#55816=EDGE_CURVE('',#43567,#43568,#23650,.T.);
#55817=EDGE_CURVE('',#43568,#43569,#2124,.T.);
#55818=EDGE_CURVE('',#43569,#43570,#23651,.T.);
#55819=EDGE_CURVE('',#43570,#43571,#2125,.T.);
#55820=EDGE_CURVE('',#43571,#43572,#23652,.T.);
#55821=EDGE_CURVE('',#43572,#43561,#23653,.T.);
#55822=EDGE_CURVE('',#43573,#43574,#23654,.T.);
#55823=EDGE_CURVE('',#43574,#43575,#34407,.T.);
#55824=EDGE_CURVE('',#43575,#43576,#23655,.T.);
#55825=EDGE_CURVE('',#43576,#43573,#34408,.T.);
#55826=EDGE_CURVE('',#43577,#43578,#2126,.T.);
#55827=EDGE_CURVE('',#43578,#43579,#23656,.T.);
#55828=EDGE_CURVE('',#43579,#43580,#23657,.T.);
#55829=EDGE_CURVE('',#43580,#43581,#23658,.T.);
#55830=EDGE_CURVE('',#43581,#43582,#2127,.T.);
#55831=EDGE_CURVE('',#43582,#43583,#23659,.T.);
#55832=EDGE_CURVE('',#43583,#43584,#23660,.T.);
#55833=EDGE_CURVE('',#43584,#43585,#2128,.T.);
#55834=EDGE_CURVE('',#43585,#43586,#23661,.T.);
#55835=EDGE_CURVE('',#43586,#43587,#2129,.T.);
#55836=EDGE_CURVE('',#43587,#43588,#23662,.T.);
#55837=EDGE_CURVE('',#43588,#43577,#23663,.T.);
#55838=EDGE_CURVE('',#43589,#43590,#2130,.T.);
#55839=EDGE_CURVE('',#43590,#43591,#23664,.T.);
#55840=EDGE_CURVE('',#43591,#43592,#23665,.T.);
#55841=EDGE_CURVE('',#43592,#43593,#23666,.T.);
#55842=EDGE_CURVE('',#43593,#43594,#2131,.T.);
#55843=EDGE_CURVE('',#43594,#43595,#23667,.T.);
#55844=EDGE_CURVE('',#43595,#43596,#23668,.T.);
#55845=EDGE_CURVE('',#43596,#43597,#2132,.T.);
#55846=EDGE_CURVE('',#43597,#43598,#23669,.T.);
#55847=EDGE_CURVE('',#43598,#43599,#2133,.T.);
#55848=EDGE_CURVE('',#43599,#43600,#23670,.T.);
#55849=EDGE_CURVE('',#43600,#43589,#23671,.T.);
#55850=EDGE_CURVE('',#43601,#43602,#23672,.T.);
#55851=EDGE_CURVE('',#43602,#43603,#34409,.T.);
#55852=EDGE_CURVE('',#43603,#43604,#23673,.T.);
#55853=EDGE_CURVE('',#43604,#43601,#34410,.T.);
#55854=EDGE_CURVE('',#43605,#43606,#2134,.T.);
#55855=EDGE_CURVE('',#43606,#43607,#23674,.T.);
#55856=EDGE_CURVE('',#43607,#43608,#23675,.T.);
#55857=EDGE_CURVE('',#43608,#43609,#23676,.T.);
#55858=EDGE_CURVE('',#43609,#43610,#2135,.T.);
#55859=EDGE_CURVE('',#43610,#43611,#23677,.T.);
#55860=EDGE_CURVE('',#43611,#43612,#23678,.T.);
#55861=EDGE_CURVE('',#43612,#43613,#2136,.T.);
#55862=EDGE_CURVE('',#43613,#43614,#23679,.T.);
#55863=EDGE_CURVE('',#43614,#43615,#2137,.T.);
#55864=EDGE_CURVE('',#43615,#43616,#23680,.T.);
#55865=EDGE_CURVE('',#43616,#43605,#23681,.T.);
#55866=EDGE_CURVE('',#43617,#43618,#2138,.T.);
#55867=EDGE_CURVE('',#43618,#43619,#23682,.T.);
#55868=EDGE_CURVE('',#43619,#43620,#23683,.T.);
#55869=EDGE_CURVE('',#43620,#43621,#23684,.T.);
#55870=EDGE_CURVE('',#43621,#43622,#2139,.T.);
#55871=EDGE_CURVE('',#43622,#43623,#23685,.T.);
#55872=EDGE_CURVE('',#43623,#43624,#23686,.T.);
#55873=EDGE_CURVE('',#43624,#43625,#2140,.T.);
#55874=EDGE_CURVE('',#43625,#43626,#23687,.T.);
#55875=EDGE_CURVE('',#43626,#43627,#2141,.T.);
#55876=EDGE_CURVE('',#43627,#43628,#23688,.T.);
#55877=EDGE_CURVE('',#43628,#43617,#23689,.T.);
#55878=EDGE_CURVE('',#40429,#40435,#23690,.T.);
#55879=EDGE_CURVE('',#40434,#40428,#23691,.T.);
#55880=EDGE_CURVE('',#43629,#43630,#2142,.T.);
#55881=EDGE_CURVE('',#43630,#43631,#23692,.T.);
#55882=EDGE_CURVE('',#43631,#43632,#23693,.T.);
#55883=EDGE_CURVE('',#43632,#43633,#23694,.T.);
#55884=EDGE_CURVE('',#43633,#43634,#2143,.T.);
#55885=EDGE_CURVE('',#43634,#43635,#23695,.T.);
#55886=EDGE_CURVE('',#43635,#43636,#23696,.T.);
#55887=EDGE_CURVE('',#43636,#43637,#2144,.T.);
#55888=EDGE_CURVE('',#43637,#43638,#23697,.T.);
#55889=EDGE_CURVE('',#43638,#43639,#2145,.T.);
#55890=EDGE_CURVE('',#43639,#43640,#23698,.T.);
#55891=EDGE_CURVE('',#43640,#43629,#23699,.T.);
#55892=EDGE_CURVE('',#43641,#43642,#2146,.T.);
#55893=EDGE_CURVE('',#43642,#43643,#23700,.T.);
#55894=EDGE_CURVE('',#43643,#43644,#23701,.T.);
#55895=EDGE_CURVE('',#43644,#43645,#23702,.T.);
#55896=EDGE_CURVE('',#43645,#43646,#2147,.T.);
#55897=EDGE_CURVE('',#43646,#43647,#23703,.T.);
#55898=EDGE_CURVE('',#43647,#43648,#23704,.T.);
#55899=EDGE_CURVE('',#43648,#43649,#2148,.T.);
#55900=EDGE_CURVE('',#43649,#43650,#23705,.T.);
#55901=EDGE_CURVE('',#43650,#43651,#2149,.T.);
#55902=EDGE_CURVE('',#43651,#43652,#23706,.T.);
#55903=EDGE_CURVE('',#43652,#43641,#23707,.T.);
#55904=EDGE_CURVE('',#43653,#43654,#23708,.T.);
#55905=EDGE_CURVE('',#43654,#43655,#34411,.T.);
#55906=EDGE_CURVE('',#43655,#43656,#23709,.T.);
#55907=EDGE_CURVE('',#43656,#43653,#34412,.T.);
#55908=EDGE_CURVE('',#43657,#43658,#2150,.T.);
#55909=EDGE_CURVE('',#43658,#43659,#23710,.T.);
#55910=EDGE_CURVE('',#43659,#43660,#23711,.T.);
#55911=EDGE_CURVE('',#43660,#43661,#23712,.T.);
#55912=EDGE_CURVE('',#43661,#43662,#2151,.T.);
#55913=EDGE_CURVE('',#43662,#43663,#23713,.T.);
#55914=EDGE_CURVE('',#43663,#43664,#23714,.T.);
#55915=EDGE_CURVE('',#43664,#43665,#2152,.T.);
#55916=EDGE_CURVE('',#43665,#43666,#23715,.T.);
#55917=EDGE_CURVE('',#43666,#43667,#2153,.T.);
#55918=EDGE_CURVE('',#43667,#43668,#23716,.T.);
#55919=EDGE_CURVE('',#43668,#43657,#23717,.T.);
#55920=EDGE_CURVE('',#43669,#43670,#2154,.T.);
#55921=EDGE_CURVE('',#43670,#43671,#23718,.T.);
#55922=EDGE_CURVE('',#43671,#43672,#23719,.T.);
#55923=EDGE_CURVE('',#43672,#43673,#23720,.T.);
#55924=EDGE_CURVE('',#43673,#43674,#2155,.T.);
#55925=EDGE_CURVE('',#43674,#43675,#23721,.T.);
#55926=EDGE_CURVE('',#43675,#43676,#23722,.T.);
#55927=EDGE_CURVE('',#43676,#43677,#2156,.T.);
#55928=EDGE_CURVE('',#43677,#43678,#23723,.T.);
#55929=EDGE_CURVE('',#43678,#43679,#2157,.T.);
#55930=EDGE_CURVE('',#43679,#43680,#23724,.T.);
#55931=EDGE_CURVE('',#43680,#43669,#23725,.T.);
#55932=EDGE_CURVE('',#43681,#43682,#23726,.T.);
#55933=EDGE_CURVE('',#43682,#43683,#34413,.T.);
#55934=EDGE_CURVE('',#43683,#43684,#23727,.T.);
#55935=EDGE_CURVE('',#43684,#43681,#34414,.T.);
#55936=EDGE_CURVE('',#43685,#43686,#2158,.T.);
#55937=EDGE_CURVE('',#43686,#43687,#23728,.T.);
#55938=EDGE_CURVE('',#43687,#43688,#23729,.T.);
#55939=EDGE_CURVE('',#43688,#43689,#23730,.T.);
#55940=EDGE_CURVE('',#43689,#43690,#2159,.T.);
#55941=EDGE_CURVE('',#43690,#43691,#23731,.T.);
#55942=EDGE_CURVE('',#43691,#43692,#23732,.T.);
#55943=EDGE_CURVE('',#43692,#43693,#2160,.T.);
#55944=EDGE_CURVE('',#43693,#43694,#23733,.T.);
#55945=EDGE_CURVE('',#43694,#43695,#2161,.T.);
#55946=EDGE_CURVE('',#43695,#43696,#23734,.T.);
#55947=EDGE_CURVE('',#43696,#43685,#23735,.T.);
#55948=EDGE_CURVE('',#43697,#43698,#2162,.T.);
#55949=EDGE_CURVE('',#43698,#43699,#23736,.T.);
#55950=EDGE_CURVE('',#43699,#43700,#23737,.T.);
#55951=EDGE_CURVE('',#43700,#43701,#23738,.T.);
#55952=EDGE_CURVE('',#43701,#43702,#2163,.T.);
#55953=EDGE_CURVE('',#43702,#43703,#23739,.T.);
#55954=EDGE_CURVE('',#43703,#43704,#23740,.T.);
#55955=EDGE_CURVE('',#43704,#43705,#2164,.T.);
#55956=EDGE_CURVE('',#43705,#43706,#23741,.T.);
#55957=EDGE_CURVE('',#43706,#43707,#2165,.T.);
#55958=EDGE_CURVE('',#43707,#43708,#23742,.T.);
#55959=EDGE_CURVE('',#43708,#43697,#23743,.T.);
#55960=EDGE_CURVE('',#43709,#43710,#23744,.T.);
#55961=EDGE_CURVE('',#43710,#43711,#34415,.T.);
#55962=EDGE_CURVE('',#43711,#43712,#23745,.T.);
#55963=EDGE_CURVE('',#43712,#43709,#34416,.T.);
#55964=EDGE_CURVE('',#43713,#43714,#2166,.T.);
#55965=EDGE_CURVE('',#43714,#43715,#23746,.T.);
#55966=EDGE_CURVE('',#43715,#43716,#23747,.T.);
#55967=EDGE_CURVE('',#43716,#43717,#23748,.T.);
#55968=EDGE_CURVE('',#43717,#43718,#2167,.T.);
#55969=EDGE_CURVE('',#43718,#43719,#23749,.T.);
#55970=EDGE_CURVE('',#43719,#43720,#23750,.T.);
#55971=EDGE_CURVE('',#43720,#43721,#2168,.T.);
#55972=EDGE_CURVE('',#43721,#43722,#23751,.T.);
#55973=EDGE_CURVE('',#43722,#43723,#2169,.T.);
#55974=EDGE_CURVE('',#43723,#43724,#23752,.T.);
#55975=EDGE_CURVE('',#43724,#43713,#23753,.T.);
#55976=EDGE_CURVE('',#43725,#43726,#2170,.T.);
#55977=EDGE_CURVE('',#43726,#43727,#23754,.T.);
#55978=EDGE_CURVE('',#43727,#43728,#23755,.T.);
#55979=EDGE_CURVE('',#43728,#43729,#23756,.T.);
#55980=EDGE_CURVE('',#43729,#43730,#2171,.T.);
#55981=EDGE_CURVE('',#43730,#43731,#23757,.T.);
#55982=EDGE_CURVE('',#43731,#43732,#23758,.T.);
#55983=EDGE_CURVE('',#43732,#43733,#2172,.T.);
#55984=EDGE_CURVE('',#43733,#43734,#23759,.T.);
#55985=EDGE_CURVE('',#43734,#43735,#2173,.T.);
#55986=EDGE_CURVE('',#43735,#43736,#23760,.T.);
#55987=EDGE_CURVE('',#43736,#43725,#23761,.T.);
#55988=EDGE_CURVE('',#43737,#43738,#23762,.T.);
#55989=EDGE_CURVE('',#43738,#43739,#34417,.T.);
#55990=EDGE_CURVE('',#43739,#43740,#23763,.T.);
#55991=EDGE_CURVE('',#43740,#43737,#34418,.T.);
#55992=EDGE_CURVE('',#43741,#43742,#2174,.T.);
#55993=EDGE_CURVE('',#43742,#43743,#23764,.T.);
#55994=EDGE_CURVE('',#43743,#43744,#23765,.T.);
#55995=EDGE_CURVE('',#43744,#43745,#23766,.T.);
#55996=EDGE_CURVE('',#43745,#43746,#2175,.T.);
#55997=EDGE_CURVE('',#43746,#43747,#23767,.T.);
#55998=EDGE_CURVE('',#43747,#43748,#23768,.T.);
#55999=EDGE_CURVE('',#43748,#43749,#2176,.T.);
#56000=EDGE_CURVE('',#43749,#43750,#23769,.T.);
#56001=EDGE_CURVE('',#43750,#43751,#2177,.T.);
#56002=EDGE_CURVE('',#43751,#43752,#23770,.T.);
#56003=EDGE_CURVE('',#43752,#43741,#23771,.T.);
#56004=EDGE_CURVE('',#43753,#43754,#2178,.T.);
#56005=EDGE_CURVE('',#43754,#43755,#23772,.T.);
#56006=EDGE_CURVE('',#43755,#43756,#23773,.T.);
#56007=EDGE_CURVE('',#43756,#43757,#23774,.T.);
#56008=EDGE_CURVE('',#43757,#43758,#2179,.T.);
#56009=EDGE_CURVE('',#43758,#43759,#23775,.T.);
#56010=EDGE_CURVE('',#43759,#43760,#23776,.T.);
#56011=EDGE_CURVE('',#43760,#43761,#2180,.T.);
#56012=EDGE_CURVE('',#43761,#43762,#23777,.T.);
#56013=EDGE_CURVE('',#43762,#43763,#2181,.T.);
#56014=EDGE_CURVE('',#43763,#43764,#23778,.T.);
#56015=EDGE_CURVE('',#43764,#43753,#23779,.T.);
#56016=EDGE_CURVE('',#43765,#43766,#23780,.T.);
#56017=EDGE_CURVE('',#43766,#43767,#34419,.T.);
#56018=EDGE_CURVE('',#43767,#43768,#23781,.T.);
#56019=EDGE_CURVE('',#43768,#43765,#34420,.T.);
#56020=EDGE_CURVE('',#43769,#43770,#2182,.T.);
#56021=EDGE_CURVE('',#43770,#43771,#23782,.T.);
#56022=EDGE_CURVE('',#43771,#43772,#23783,.T.);
#56023=EDGE_CURVE('',#43772,#43773,#23784,.T.);
#56024=EDGE_CURVE('',#43773,#43774,#2183,.T.);
#56025=EDGE_CURVE('',#43774,#43775,#23785,.T.);
#56026=EDGE_CURVE('',#43775,#43776,#23786,.T.);
#56027=EDGE_CURVE('',#43776,#43777,#2184,.T.);
#56028=EDGE_CURVE('',#43777,#43778,#23787,.T.);
#56029=EDGE_CURVE('',#43778,#43779,#2185,.T.);
#56030=EDGE_CURVE('',#43779,#43780,#23788,.T.);
#56031=EDGE_CURVE('',#43780,#43769,#23789,.T.);
#56032=EDGE_CURVE('',#43781,#43782,#2186,.T.);
#56033=EDGE_CURVE('',#43782,#43783,#23790,.T.);
#56034=EDGE_CURVE('',#43783,#43784,#23791,.T.);
#56035=EDGE_CURVE('',#43784,#43785,#23792,.T.);
#56036=EDGE_CURVE('',#43785,#43786,#2187,.T.);
#56037=EDGE_CURVE('',#43786,#43787,#23793,.T.);
#56038=EDGE_CURVE('',#43787,#43788,#23794,.T.);
#56039=EDGE_CURVE('',#43788,#43789,#2188,.T.);
#56040=EDGE_CURVE('',#43789,#43790,#23795,.T.);
#56041=EDGE_CURVE('',#43790,#43791,#2189,.T.);
#56042=EDGE_CURVE('',#43791,#43792,#23796,.T.);
#56043=EDGE_CURVE('',#43792,#43781,#23797,.T.);
#56044=EDGE_CURVE('',#43793,#43794,#23798,.T.);
#56045=EDGE_CURVE('',#43794,#43795,#34421,.T.);
#56046=EDGE_CURVE('',#43795,#43796,#23799,.T.);
#56047=EDGE_CURVE('',#43796,#43793,#34422,.T.);
#56048=EDGE_CURVE('',#43797,#43798,#2190,.T.);
#56049=EDGE_CURVE('',#43798,#43799,#23800,.T.);
#56050=EDGE_CURVE('',#43799,#43800,#23801,.T.);
#56051=EDGE_CURVE('',#43800,#43801,#23802,.T.);
#56052=EDGE_CURVE('',#43801,#43802,#2191,.T.);
#56053=EDGE_CURVE('',#43802,#43803,#23803,.T.);
#56054=EDGE_CURVE('',#43803,#43804,#23804,.T.);
#56055=EDGE_CURVE('',#43804,#43805,#2192,.T.);
#56056=EDGE_CURVE('',#43805,#43806,#23805,.T.);
#56057=EDGE_CURVE('',#43806,#43807,#2193,.T.);
#56058=EDGE_CURVE('',#43807,#43808,#23806,.T.);
#56059=EDGE_CURVE('',#43808,#43797,#23807,.T.);
#56060=EDGE_CURVE('',#43809,#43810,#2194,.T.);
#56061=EDGE_CURVE('',#43810,#43811,#23808,.T.);
#56062=EDGE_CURVE('',#43811,#43812,#23809,.T.);
#56063=EDGE_CURVE('',#43812,#43813,#23810,.T.);
#56064=EDGE_CURVE('',#43813,#43814,#2195,.T.);
#56065=EDGE_CURVE('',#43814,#43815,#23811,.T.);
#56066=EDGE_CURVE('',#43815,#43816,#23812,.T.);
#56067=EDGE_CURVE('',#43816,#43817,#2196,.T.);
#56068=EDGE_CURVE('',#43817,#43818,#23813,.T.);
#56069=EDGE_CURVE('',#43818,#43819,#2197,.T.);
#56070=EDGE_CURVE('',#43819,#43820,#23814,.T.);
#56071=EDGE_CURVE('',#43820,#43809,#23815,.T.);
#56072=EDGE_CURVE('',#43821,#43822,#23816,.T.);
#56073=EDGE_CURVE('',#43822,#43823,#34423,.T.);
#56074=EDGE_CURVE('',#43823,#43824,#23817,.T.);
#56075=EDGE_CURVE('',#43824,#43821,#34424,.T.);
#56076=EDGE_CURVE('',#43825,#43826,#2198,.T.);
#56077=EDGE_CURVE('',#43826,#43827,#23818,.T.);
#56078=EDGE_CURVE('',#43827,#43828,#23819,.T.);
#56079=EDGE_CURVE('',#43828,#43829,#23820,.T.);
#56080=EDGE_CURVE('',#43829,#43830,#2199,.T.);
#56081=EDGE_CURVE('',#43830,#43831,#23821,.T.);
#56082=EDGE_CURVE('',#43831,#43832,#23822,.T.);
#56083=EDGE_CURVE('',#43832,#43833,#2200,.T.);
#56084=EDGE_CURVE('',#43833,#43834,#23823,.T.);
#56085=EDGE_CURVE('',#43834,#43835,#2201,.T.);
#56086=EDGE_CURVE('',#43835,#43836,#23824,.T.);
#56087=EDGE_CURVE('',#43836,#43825,#23825,.T.);
#56088=EDGE_CURVE('',#43837,#43838,#2202,.T.);
#56089=EDGE_CURVE('',#43838,#43839,#23826,.T.);
#56090=EDGE_CURVE('',#43839,#43840,#23827,.T.);
#56091=EDGE_CURVE('',#43840,#43841,#23828,.T.);
#56092=EDGE_CURVE('',#43841,#43842,#2203,.T.);
#56093=EDGE_CURVE('',#43842,#43843,#23829,.T.);
#56094=EDGE_CURVE('',#43843,#43844,#23830,.T.);
#56095=EDGE_CURVE('',#43844,#43845,#2204,.T.);
#56096=EDGE_CURVE('',#43845,#43846,#23831,.T.);
#56097=EDGE_CURVE('',#43846,#43847,#2205,.T.);
#56098=EDGE_CURVE('',#43847,#43848,#23832,.T.);
#56099=EDGE_CURVE('',#43848,#43837,#23833,.T.);
#56100=EDGE_CURVE('',#43849,#43850,#23834,.T.);
#56101=EDGE_CURVE('',#43850,#43851,#34425,.T.);
#56102=EDGE_CURVE('',#43851,#43852,#23835,.T.);
#56103=EDGE_CURVE('',#43852,#43849,#34426,.T.);
#56104=EDGE_CURVE('',#43853,#43854,#2206,.T.);
#56105=EDGE_CURVE('',#43854,#43855,#23836,.T.);
#56106=EDGE_CURVE('',#43855,#43856,#23837,.T.);
#56107=EDGE_CURVE('',#43856,#43857,#23838,.T.);
#56108=EDGE_CURVE('',#43857,#43858,#2207,.T.);
#56109=EDGE_CURVE('',#43858,#43859,#23839,.T.);
#56110=EDGE_CURVE('',#43859,#43860,#23840,.T.);
#56111=EDGE_CURVE('',#43860,#43861,#2208,.T.);
#56112=EDGE_CURVE('',#43861,#43862,#23841,.T.);
#56113=EDGE_CURVE('',#43862,#43863,#2209,.T.);
#56114=EDGE_CURVE('',#43863,#43864,#23842,.T.);
#56115=EDGE_CURVE('',#43864,#43853,#23843,.T.);
#56116=EDGE_CURVE('',#43865,#43866,#2210,.T.);
#56117=EDGE_CURVE('',#43866,#43867,#23844,.T.);
#56118=EDGE_CURVE('',#43867,#43868,#23845,.T.);
#56119=EDGE_CURVE('',#43868,#43869,#23846,.T.);
#56120=EDGE_CURVE('',#43869,#43870,#2211,.T.);
#56121=EDGE_CURVE('',#43870,#43871,#23847,.T.);
#56122=EDGE_CURVE('',#43871,#43872,#23848,.T.);
#56123=EDGE_CURVE('',#43872,#43873,#2212,.T.);
#56124=EDGE_CURVE('',#43873,#43874,#23849,.T.);
#56125=EDGE_CURVE('',#43874,#43875,#2213,.T.);
#56126=EDGE_CURVE('',#43875,#43876,#23850,.T.);
#56127=EDGE_CURVE('',#43876,#43865,#23851,.T.);
#56128=EDGE_CURVE('',#43877,#43878,#23852,.T.);
#56129=EDGE_CURVE('',#43878,#43879,#34427,.T.);
#56130=EDGE_CURVE('',#43879,#43880,#23853,.T.);
#56131=EDGE_CURVE('',#43880,#43877,#34428,.T.);
#56132=EDGE_CURVE('',#43881,#43882,#2214,.T.);
#56133=EDGE_CURVE('',#43882,#43883,#23854,.T.);
#56134=EDGE_CURVE('',#43883,#43884,#23855,.T.);
#56135=EDGE_CURVE('',#43884,#43885,#23856,.T.);
#56136=EDGE_CURVE('',#43885,#43886,#2215,.T.);
#56137=EDGE_CURVE('',#43886,#43887,#23857,.T.);
#56138=EDGE_CURVE('',#43887,#43888,#23858,.T.);
#56139=EDGE_CURVE('',#43888,#43889,#2216,.T.);
#56140=EDGE_CURVE('',#43889,#43890,#23859,.T.);
#56141=EDGE_CURVE('',#43890,#43891,#2217,.T.);
#56142=EDGE_CURVE('',#43891,#43892,#23860,.T.);
#56143=EDGE_CURVE('',#43892,#43881,#23861,.T.);
#56144=EDGE_CURVE('',#43893,#43894,#2218,.T.);
#56145=EDGE_CURVE('',#43894,#43895,#23862,.T.);
#56146=EDGE_CURVE('',#43895,#43896,#23863,.T.);
#56147=EDGE_CURVE('',#43896,#43897,#23864,.T.);
#56148=EDGE_CURVE('',#43897,#43898,#2219,.T.);
#56149=EDGE_CURVE('',#43898,#43899,#23865,.T.);
#56150=EDGE_CURVE('',#43899,#43900,#23866,.T.);
#56151=EDGE_CURVE('',#43900,#43901,#2220,.T.);
#56152=EDGE_CURVE('',#43901,#43902,#23867,.T.);
#56153=EDGE_CURVE('',#43902,#43903,#2221,.T.);
#56154=EDGE_CURVE('',#43903,#43904,#23868,.T.);
#56155=EDGE_CURVE('',#43904,#43893,#23869,.T.);
#56156=EDGE_CURVE('',#43905,#43906,#23870,.T.);
#56157=EDGE_CURVE('',#43906,#43907,#34429,.T.);
#56158=EDGE_CURVE('',#43907,#43908,#23871,.T.);
#56159=EDGE_CURVE('',#43908,#43905,#34430,.T.);
#56160=EDGE_CURVE('',#43909,#43910,#2222,.T.);
#56161=EDGE_CURVE('',#43910,#43911,#23872,.T.);
#56162=EDGE_CURVE('',#43911,#43912,#23873,.T.);
#56163=EDGE_CURVE('',#43912,#43913,#23874,.T.);
#56164=EDGE_CURVE('',#43913,#43914,#2223,.T.);
#56165=EDGE_CURVE('',#43914,#43915,#23875,.T.);
#56166=EDGE_CURVE('',#43915,#43916,#23876,.T.);
#56167=EDGE_CURVE('',#43916,#43917,#2224,.T.);
#56168=EDGE_CURVE('',#43917,#43918,#23877,.T.);
#56169=EDGE_CURVE('',#43918,#43919,#2225,.T.);
#56170=EDGE_CURVE('',#43919,#43920,#23878,.T.);
#56171=EDGE_CURVE('',#43920,#43909,#23879,.T.);
#56172=EDGE_CURVE('',#43921,#43922,#2226,.T.);
#56173=EDGE_CURVE('',#43922,#43923,#23880,.T.);
#56174=EDGE_CURVE('',#43923,#43924,#23881,.T.);
#56175=EDGE_CURVE('',#43924,#43925,#23882,.T.);
#56176=EDGE_CURVE('',#43925,#43926,#2227,.T.);
#56177=EDGE_CURVE('',#43926,#43927,#23883,.T.);
#56178=EDGE_CURVE('',#43927,#43928,#23884,.T.);
#56179=EDGE_CURVE('',#43928,#43929,#2228,.T.);
#56180=EDGE_CURVE('',#43929,#43930,#23885,.T.);
#56181=EDGE_CURVE('',#43930,#43931,#2229,.T.);
#56182=EDGE_CURVE('',#43931,#43932,#23886,.T.);
#56183=EDGE_CURVE('',#43932,#43921,#23887,.T.);
#56184=EDGE_CURVE('',#43933,#43934,#23888,.T.);
#56185=EDGE_CURVE('',#43934,#43935,#34431,.T.);
#56186=EDGE_CURVE('',#43935,#43936,#23889,.T.);
#56187=EDGE_CURVE('',#43936,#43933,#34432,.T.);
#56188=EDGE_CURVE('',#43937,#43938,#2230,.T.);
#56189=EDGE_CURVE('',#43938,#43939,#23890,.T.);
#56190=EDGE_CURVE('',#43939,#43940,#23891,.T.);
#56191=EDGE_CURVE('',#43940,#43941,#23892,.T.);
#56192=EDGE_CURVE('',#43941,#43942,#2231,.T.);
#56193=EDGE_CURVE('',#43942,#43943,#23893,.T.);
#56194=EDGE_CURVE('',#43943,#43944,#23894,.T.);
#56195=EDGE_CURVE('',#43944,#43945,#2232,.T.);
#56196=EDGE_CURVE('',#43945,#43946,#23895,.T.);
#56197=EDGE_CURVE('',#43946,#43947,#2233,.T.);
#56198=EDGE_CURVE('',#43947,#43948,#23896,.T.);
#56199=EDGE_CURVE('',#43948,#43937,#23897,.T.);
#56200=EDGE_CURVE('',#43949,#43950,#2234,.T.);
#56201=EDGE_CURVE('',#43950,#43951,#23898,.T.);
#56202=EDGE_CURVE('',#43951,#43952,#23899,.T.);
#56203=EDGE_CURVE('',#43952,#43953,#23900,.T.);
#56204=EDGE_CURVE('',#43953,#43954,#2235,.T.);
#56205=EDGE_CURVE('',#43954,#43955,#23901,.T.);
#56206=EDGE_CURVE('',#43955,#43956,#23902,.T.);
#56207=EDGE_CURVE('',#43956,#43957,#2236,.T.);
#56208=EDGE_CURVE('',#43957,#43958,#23903,.T.);
#56209=EDGE_CURVE('',#43958,#43959,#2237,.T.);
#56210=EDGE_CURVE('',#43959,#43960,#23904,.T.);
#56211=EDGE_CURVE('',#43960,#43949,#23905,.T.);
#56212=EDGE_CURVE('',#43961,#43962,#23906,.T.);
#56213=EDGE_CURVE('',#43962,#43963,#34433,.T.);
#56214=EDGE_CURVE('',#43963,#43964,#23907,.T.);
#56215=EDGE_CURVE('',#43964,#43961,#34434,.T.);
#56216=EDGE_CURVE('',#43965,#43966,#2238,.T.);
#56217=EDGE_CURVE('',#43966,#43967,#23908,.T.);
#56218=EDGE_CURVE('',#43967,#43968,#23909,.T.);
#56219=EDGE_CURVE('',#43968,#43969,#23910,.T.);
#56220=EDGE_CURVE('',#43969,#43970,#2239,.T.);
#56221=EDGE_CURVE('',#43970,#43971,#23911,.T.);
#56222=EDGE_CURVE('',#43971,#43972,#23912,.T.);
#56223=EDGE_CURVE('',#43972,#43973,#2240,.T.);
#56224=EDGE_CURVE('',#43973,#43974,#23913,.T.);
#56225=EDGE_CURVE('',#43974,#43975,#2241,.T.);
#56226=EDGE_CURVE('',#43975,#43976,#23914,.T.);
#56227=EDGE_CURVE('',#43976,#43965,#23915,.T.);
#56228=EDGE_CURVE('',#43977,#43978,#2242,.T.);
#56229=EDGE_CURVE('',#43978,#43979,#23916,.T.);
#56230=EDGE_CURVE('',#43979,#43980,#23917,.T.);
#56231=EDGE_CURVE('',#43980,#43981,#23918,.T.);
#56232=EDGE_CURVE('',#43981,#43982,#2243,.T.);
#56233=EDGE_CURVE('',#43982,#43983,#23919,.T.);
#56234=EDGE_CURVE('',#43983,#43984,#23920,.T.);
#56235=EDGE_CURVE('',#43984,#43985,#2244,.T.);
#56236=EDGE_CURVE('',#43985,#43986,#23921,.T.);
#56237=EDGE_CURVE('',#43986,#43987,#2245,.T.);
#56238=EDGE_CURVE('',#43987,#43988,#23922,.T.);
#56239=EDGE_CURVE('',#43988,#43977,#23923,.T.);
#56240=EDGE_CURVE('',#43989,#43990,#23924,.T.);
#56241=EDGE_CURVE('',#43990,#43991,#34435,.T.);
#56242=EDGE_CURVE('',#43991,#43992,#23925,.T.);
#56243=EDGE_CURVE('',#43992,#43989,#34436,.T.);
#56244=EDGE_CURVE('',#43993,#43994,#2246,.T.);
#56245=EDGE_CURVE('',#43994,#43995,#23926,.T.);
#56246=EDGE_CURVE('',#43995,#43996,#23927,.T.);
#56247=EDGE_CURVE('',#43996,#43997,#23928,.T.);
#56248=EDGE_CURVE('',#43997,#43998,#2247,.T.);
#56249=EDGE_CURVE('',#43998,#43999,#23929,.T.);
#56250=EDGE_CURVE('',#43999,#44000,#23930,.T.);
#56251=EDGE_CURVE('',#44000,#44001,#2248,.T.);
#56252=EDGE_CURVE('',#44001,#44002,#23931,.T.);
#56253=EDGE_CURVE('',#44002,#44003,#2249,.T.);
#56254=EDGE_CURVE('',#44003,#44004,#23932,.T.);
#56255=EDGE_CURVE('',#44004,#43993,#23933,.T.);
#56256=EDGE_CURVE('',#44005,#44006,#2250,.T.);
#56257=EDGE_CURVE('',#44006,#44007,#23934,.T.);
#56258=EDGE_CURVE('',#44007,#44008,#23935,.T.);
#56259=EDGE_CURVE('',#44008,#44009,#23936,.T.);
#56260=EDGE_CURVE('',#44009,#44010,#2251,.T.);
#56261=EDGE_CURVE('',#44010,#44011,#23937,.T.);
#56262=EDGE_CURVE('',#44011,#44012,#23938,.T.);
#56263=EDGE_CURVE('',#44012,#44013,#2252,.T.);
#56264=EDGE_CURVE('',#44013,#44014,#23939,.T.);
#56265=EDGE_CURVE('',#44014,#44015,#2253,.T.);
#56266=EDGE_CURVE('',#44015,#44016,#23940,.T.);
#56267=EDGE_CURVE('',#44016,#44005,#23941,.T.);
#56268=EDGE_CURVE('',#44017,#44018,#23942,.T.);
#56269=EDGE_CURVE('',#44018,#44019,#34437,.T.);
#56270=EDGE_CURVE('',#44019,#44020,#23943,.T.);
#56271=EDGE_CURVE('',#44020,#44017,#34438,.T.);
#56272=EDGE_CURVE('',#44021,#44022,#2254,.T.);
#56273=EDGE_CURVE('',#44022,#44023,#23944,.T.);
#56274=EDGE_CURVE('',#44023,#44024,#23945,.T.);
#56275=EDGE_CURVE('',#44024,#44025,#23946,.T.);
#56276=EDGE_CURVE('',#44025,#44026,#2255,.T.);
#56277=EDGE_CURVE('',#44026,#44027,#23947,.T.);
#56278=EDGE_CURVE('',#44027,#44028,#23948,.T.);
#56279=EDGE_CURVE('',#44028,#44029,#2256,.T.);
#56280=EDGE_CURVE('',#44029,#44030,#23949,.T.);
#56281=EDGE_CURVE('',#44030,#44031,#2257,.T.);
#56282=EDGE_CURVE('',#44031,#44032,#23950,.T.);
#56283=EDGE_CURVE('',#44032,#44021,#23951,.T.);
#56284=EDGE_CURVE('',#44033,#44034,#2258,.T.);
#56285=EDGE_CURVE('',#44034,#44035,#23952,.T.);
#56286=EDGE_CURVE('',#44035,#44036,#23953,.T.);
#56287=EDGE_CURVE('',#44036,#44037,#23954,.T.);
#56288=EDGE_CURVE('',#44037,#44038,#2259,.T.);
#56289=EDGE_CURVE('',#44038,#44039,#23955,.T.);
#56290=EDGE_CURVE('',#44039,#44040,#23956,.T.);
#56291=EDGE_CURVE('',#44040,#44041,#2260,.T.);
#56292=EDGE_CURVE('',#44041,#44042,#23957,.T.);
#56293=EDGE_CURVE('',#44042,#44043,#2261,.T.);
#56294=EDGE_CURVE('',#44043,#44044,#23958,.T.);
#56295=EDGE_CURVE('',#44044,#44033,#23959,.T.);
#56296=EDGE_CURVE('',#42419,#42402,#4979,.T.);
#56297=EDGE_CURVE('',#42401,#42420,#4980,.T.);
#56298=EDGE_CURVE('',#42403,#42408,#4981,.T.);
#56299=EDGE_CURVE('',#42407,#42404,#4982,.T.);
#56300=EDGE_CURVE('',#42447,#42430,#4983,.T.);
#56301=EDGE_CURVE('',#42429,#42448,#4984,.T.);
#56302=EDGE_CURVE('',#42431,#42436,#4985,.T.);
#56303=EDGE_CURVE('',#42435,#42432,#4986,.T.);
#56304=EDGE_CURVE('',#42475,#42458,#4987,.T.);
#56305=EDGE_CURVE('',#42457,#42476,#4988,.T.);
#56306=EDGE_CURVE('',#42459,#42464,#4989,.T.);
#56307=EDGE_CURVE('',#42463,#42460,#4990,.T.);
#56308=EDGE_CURVE('',#42503,#42486,#4991,.T.);
#56309=EDGE_CURVE('',#42485,#42504,#4992,.T.);
#56310=EDGE_CURVE('',#42487,#42492,#4993,.T.);
#56311=EDGE_CURVE('',#42491,#42488,#4994,.T.);
#56312=EDGE_CURVE('',#42531,#42514,#4995,.T.);
#56313=EDGE_CURVE('',#42513,#42532,#4996,.T.);
#56314=EDGE_CURVE('',#42515,#42520,#4997,.T.);
#56315=EDGE_CURVE('',#42519,#42516,#4998,.T.);
#56316=EDGE_CURVE('',#42559,#42542,#4999,.T.);
#56317=EDGE_CURVE('',#42541,#42560,#5000,.T.);
#56318=EDGE_CURVE('',#42543,#42548,#5001,.T.);
#56319=EDGE_CURVE('',#42547,#42544,#5002,.T.);
#56320=EDGE_CURVE('',#42587,#42570,#5003,.T.);
#56321=EDGE_CURVE('',#42569,#42588,#5004,.T.);
#56322=EDGE_CURVE('',#42571,#42576,#5005,.T.);
#56323=EDGE_CURVE('',#42575,#42572,#5006,.T.);
#56324=EDGE_CURVE('',#42615,#42598,#5007,.T.);
#56325=EDGE_CURVE('',#42597,#42616,#5008,.T.);
#56326=EDGE_CURVE('',#42599,#42604,#5009,.T.);
#56327=EDGE_CURVE('',#42603,#42600,#5010,.T.);
#56328=EDGE_CURVE('',#42643,#42626,#5011,.T.);
#56329=EDGE_CURVE('',#42625,#42644,#5012,.T.);
#56330=EDGE_CURVE('',#42627,#42632,#5013,.T.);
#56331=EDGE_CURVE('',#42631,#42628,#5014,.T.);
#56332=EDGE_CURVE('',#42671,#42654,#5015,.T.);
#56333=EDGE_CURVE('',#42653,#42672,#5016,.T.);
#56334=EDGE_CURVE('',#42655,#42660,#5017,.T.);
#56335=EDGE_CURVE('',#42659,#42656,#5018,.T.);
#56336=EDGE_CURVE('',#42699,#42682,#5019,.T.);
#56337=EDGE_CURVE('',#42681,#42700,#5020,.T.);
#56338=EDGE_CURVE('',#42683,#42688,#5021,.T.);
#56339=EDGE_CURVE('',#42687,#42684,#5022,.T.);
#56340=EDGE_CURVE('',#42727,#42710,#5023,.T.);
#56341=EDGE_CURVE('',#42709,#42728,#5024,.T.);
#56342=EDGE_CURVE('',#42711,#42716,#5025,.T.);
#56343=EDGE_CURVE('',#42715,#42712,#5026,.T.);
#56344=EDGE_CURVE('',#42755,#42738,#5027,.T.);
#56345=EDGE_CURVE('',#42737,#42756,#5028,.T.);
#56346=EDGE_CURVE('',#42739,#42744,#5029,.T.);
#56347=EDGE_CURVE('',#42743,#42740,#5030,.T.);
#56348=EDGE_CURVE('',#42783,#42766,#5031,.T.);
#56349=EDGE_CURVE('',#42765,#42784,#5032,.T.);
#56350=EDGE_CURVE('',#42767,#42772,#5033,.T.);
#56351=EDGE_CURVE('',#42771,#42768,#5034,.T.);
#56352=EDGE_CURVE('',#42811,#42794,#5035,.T.);
#56353=EDGE_CURVE('',#42793,#42812,#5036,.T.);
#56354=EDGE_CURVE('',#42795,#42800,#5037,.T.);
#56355=EDGE_CURVE('',#42799,#42796,#5038,.T.);
#56356=EDGE_CURVE('',#42839,#42822,#5039,.T.);
#56357=EDGE_CURVE('',#42821,#42840,#5040,.T.);
#56358=EDGE_CURVE('',#42823,#42828,#5041,.T.);
#56359=EDGE_CURVE('',#42827,#42824,#5042,.T.);
#56360=EDGE_CURVE('',#42867,#42850,#5043,.T.);
#56361=EDGE_CURVE('',#42849,#42868,#5044,.T.);
#56362=EDGE_CURVE('',#42851,#42856,#5045,.T.);
#56363=EDGE_CURVE('',#42855,#42852,#5046,.T.);
#56364=EDGE_CURVE('',#42895,#42878,#5047,.T.);
#56365=EDGE_CURVE('',#42877,#42896,#5048,.T.);
#56366=EDGE_CURVE('',#42879,#42884,#5049,.T.);
#56367=EDGE_CURVE('',#42883,#42880,#5050,.T.);
#56368=EDGE_CURVE('',#42923,#42906,#5051,.T.);
#56369=EDGE_CURVE('',#42905,#42924,#5052,.T.);
#56370=EDGE_CURVE('',#42907,#42912,#5053,.T.);
#56371=EDGE_CURVE('',#42911,#42908,#5054,.T.);
#56372=EDGE_CURVE('',#42951,#42934,#5055,.T.);
#56373=EDGE_CURVE('',#42933,#42952,#5056,.T.);
#56374=EDGE_CURVE('',#42935,#42940,#5057,.T.);
#56375=EDGE_CURVE('',#42939,#42936,#5058,.T.);
#56376=EDGE_CURVE('',#42979,#42962,#5059,.T.);
#56377=EDGE_CURVE('',#42961,#42980,#5060,.T.);
#56378=EDGE_CURVE('',#42963,#42968,#5061,.T.);
#56379=EDGE_CURVE('',#42967,#42964,#5062,.T.);
#56380=EDGE_CURVE('',#43007,#42990,#5063,.T.);
#56381=EDGE_CURVE('',#42989,#43008,#5064,.T.);
#56382=EDGE_CURVE('',#42991,#42996,#5065,.T.);
#56383=EDGE_CURVE('',#42995,#42992,#5066,.T.);
#56384=EDGE_CURVE('',#43035,#43018,#5067,.T.);
#56385=EDGE_CURVE('',#43017,#43036,#5068,.T.);
#56386=EDGE_CURVE('',#43019,#43024,#5069,.T.);
#56387=EDGE_CURVE('',#43023,#43020,#5070,.T.);
#56388=EDGE_CURVE('',#43063,#43046,#5071,.T.);
#56389=EDGE_CURVE('',#43045,#43064,#5072,.T.);
#56390=EDGE_CURVE('',#43047,#43052,#5073,.T.);
#56391=EDGE_CURVE('',#43051,#43048,#5074,.T.);
#56392=EDGE_CURVE('',#43091,#43074,#5075,.T.);
#56393=EDGE_CURVE('',#43073,#43092,#5076,.T.);
#56394=EDGE_CURVE('',#43075,#43080,#5077,.T.);
#56395=EDGE_CURVE('',#43079,#43076,#5078,.T.);
#56396=EDGE_CURVE('',#43119,#43102,#5079,.T.);
#56397=EDGE_CURVE('',#43101,#43120,#5080,.T.);
#56398=EDGE_CURVE('',#43103,#43108,#5081,.T.);
#56399=EDGE_CURVE('',#43107,#43104,#5082,.T.);
#56400=EDGE_CURVE('',#43147,#43130,#5083,.T.);
#56401=EDGE_CURVE('',#43129,#43148,#5084,.T.);
#56402=EDGE_CURVE('',#43131,#43136,#5085,.T.);
#56403=EDGE_CURVE('',#43135,#43132,#5086,.T.);
#56404=EDGE_CURVE('',#43175,#43158,#5087,.T.);
#56405=EDGE_CURVE('',#43157,#43176,#5088,.T.);
#56406=EDGE_CURVE('',#43159,#43164,#5089,.T.);
#56407=EDGE_CURVE('',#43163,#43160,#5090,.T.);
#56408=EDGE_CURVE('',#43203,#43186,#5091,.T.);
#56409=EDGE_CURVE('',#43185,#43204,#5092,.T.);
#56410=EDGE_CURVE('',#43187,#43192,#5093,.T.);
#56411=EDGE_CURVE('',#43191,#43188,#5094,.T.);
#56412=EDGE_CURVE('',#43227,#40443,#5095,.T.);
#56413=EDGE_CURVE('',#40437,#43228,#5096,.T.);
#56414=EDGE_CURVE('',#40442,#43216,#5097,.T.);
#56415=EDGE_CURVE('',#43215,#40436,#5098,.T.);
#56416=EDGE_CURVE('',#43255,#43238,#5099,.T.);
#56417=EDGE_CURVE('',#43237,#43256,#5100,.T.);
#56418=EDGE_CURVE('',#43239,#43244,#5101,.T.);
#56419=EDGE_CURVE('',#43243,#43240,#5102,.T.);
#56420=EDGE_CURVE('',#43283,#43266,#5103,.T.);
#56421=EDGE_CURVE('',#43265,#43284,#5104,.T.);
#56422=EDGE_CURVE('',#43267,#43272,#5105,.T.);
#56423=EDGE_CURVE('',#43271,#43268,#5106,.T.);
#56424=EDGE_CURVE('',#43311,#43294,#5107,.T.);
#56425=EDGE_CURVE('',#43293,#43312,#5108,.T.);
#56426=EDGE_CURVE('',#43295,#43300,#5109,.T.);
#56427=EDGE_CURVE('',#43299,#43296,#5110,.T.);
#56428=EDGE_CURVE('',#43339,#43322,#5111,.T.);
#56429=EDGE_CURVE('',#43321,#43340,#5112,.T.);
#56430=EDGE_CURVE('',#43323,#43328,#5113,.T.);
#56431=EDGE_CURVE('',#43327,#43324,#5114,.T.);
#56432=EDGE_CURVE('',#43367,#43350,#5115,.T.);
#56433=EDGE_CURVE('',#43349,#43368,#5116,.T.);
#56434=EDGE_CURVE('',#43351,#43356,#5117,.T.);
#56435=EDGE_CURVE('',#43355,#43352,#5118,.T.);
#56436=EDGE_CURVE('',#43395,#43378,#5119,.T.);
#56437=EDGE_CURVE('',#43377,#43396,#5120,.T.);
#56438=EDGE_CURVE('',#43379,#43384,#5121,.T.);
#56439=EDGE_CURVE('',#43383,#43380,#5122,.T.);
#56440=EDGE_CURVE('',#43423,#43406,#5123,.T.);
#56441=EDGE_CURVE('',#43405,#43424,#5124,.T.);
#56442=EDGE_CURVE('',#43407,#43412,#5125,.T.);
#56443=EDGE_CURVE('',#43411,#43408,#5126,.T.);
#56444=EDGE_CURVE('',#43451,#43434,#5127,.T.);
#56445=EDGE_CURVE('',#43433,#43452,#5128,.T.);
#56446=EDGE_CURVE('',#43435,#43440,#5129,.T.);
#56447=EDGE_CURVE('',#43439,#43436,#5130,.T.);
#56448=EDGE_CURVE('',#43479,#43462,#5131,.T.);
#56449=EDGE_CURVE('',#43461,#43480,#5132,.T.);
#56450=EDGE_CURVE('',#43463,#43468,#5133,.T.);
#56451=EDGE_CURVE('',#43467,#43464,#5134,.T.);
#56452=EDGE_CURVE('',#43507,#43490,#5135,.T.);
#56453=EDGE_CURVE('',#43489,#43508,#5136,.T.);
#56454=EDGE_CURVE('',#43491,#43496,#5137,.T.);
#56455=EDGE_CURVE('',#43495,#43492,#5138,.T.);
#56456=EDGE_CURVE('',#43535,#43518,#5139,.T.);
#56457=EDGE_CURVE('',#43517,#43536,#5140,.T.);
#56458=EDGE_CURVE('',#43519,#43524,#5141,.T.);
#56459=EDGE_CURVE('',#43523,#43520,#5142,.T.);
#56460=EDGE_CURVE('',#43563,#43546,#5143,.T.);
#56461=EDGE_CURVE('',#43545,#43564,#5144,.T.);
#56462=EDGE_CURVE('',#43547,#43552,#5145,.T.);
#56463=EDGE_CURVE('',#43551,#43548,#5146,.T.);
#56464=EDGE_CURVE('',#43591,#43574,#5147,.T.);
#56465=EDGE_CURVE('',#43573,#43592,#5148,.T.);
#56466=EDGE_CURVE('',#43575,#43580,#5149,.T.);
#56467=EDGE_CURVE('',#43579,#43576,#5150,.T.);
#56468=EDGE_CURVE('',#43619,#43602,#5151,.T.);
#56469=EDGE_CURVE('',#43601,#43620,#5152,.T.);
#56470=EDGE_CURVE('',#43603,#43608,#5153,.T.);
#56471=EDGE_CURVE('',#43607,#43604,#5154,.T.);
#56472=EDGE_CURVE('',#43643,#40435,#5155,.T.);
#56473=EDGE_CURVE('',#40429,#43644,#5156,.T.);
#56474=EDGE_CURVE('',#40434,#43632,#5157,.T.);
#56475=EDGE_CURVE('',#43631,#40428,#5158,.T.);
#56476=EDGE_CURVE('',#43671,#43654,#5159,.T.);
#56477=EDGE_CURVE('',#43653,#43672,#5160,.T.);
#56478=EDGE_CURVE('',#43655,#43660,#5161,.T.);
#56479=EDGE_CURVE('',#43659,#43656,#5162,.T.);
#56480=EDGE_CURVE('',#43699,#43682,#5163,.T.);
#56481=EDGE_CURVE('',#43681,#43700,#5164,.T.);
#56482=EDGE_CURVE('',#43683,#43688,#5165,.T.);
#56483=EDGE_CURVE('',#43687,#43684,#5166,.T.);
#56484=EDGE_CURVE('',#43727,#43710,#5167,.T.);
#56485=EDGE_CURVE('',#43709,#43728,#5168,.T.);
#56486=EDGE_CURVE('',#43711,#43716,#5169,.T.);
#56487=EDGE_CURVE('',#43715,#43712,#5170,.T.);
#56488=EDGE_CURVE('',#43755,#43738,#5171,.T.);
#56489=EDGE_CURVE('',#43737,#43756,#5172,.T.);
#56490=EDGE_CURVE('',#43739,#43744,#5173,.T.);
#56491=EDGE_CURVE('',#43743,#43740,#5174,.T.);
#56492=EDGE_CURVE('',#43783,#43766,#5175,.T.);
#56493=EDGE_CURVE('',#43765,#43784,#5176,.T.);
#56494=EDGE_CURVE('',#43767,#43772,#5177,.T.);
#56495=EDGE_CURVE('',#43771,#43768,#5178,.T.);
#56496=EDGE_CURVE('',#43811,#43794,#5179,.T.);
#56497=EDGE_CURVE('',#43793,#43812,#5180,.T.);
#56498=EDGE_CURVE('',#43795,#43800,#5181,.T.);
#56499=EDGE_CURVE('',#43799,#43796,#5182,.T.);
#56500=EDGE_CURVE('',#43839,#43822,#5183,.T.);
#56501=EDGE_CURVE('',#43821,#43840,#5184,.T.);
#56502=EDGE_CURVE('',#43823,#43828,#5185,.T.);
#56503=EDGE_CURVE('',#43827,#43824,#5186,.T.);
#56504=EDGE_CURVE('',#43867,#43850,#5187,.T.);
#56505=EDGE_CURVE('',#43849,#43868,#5188,.T.);
#56506=EDGE_CURVE('',#43851,#43856,#5189,.T.);
#56507=EDGE_CURVE('',#43855,#43852,#5190,.T.);
#56508=EDGE_CURVE('',#43895,#43878,#5191,.T.);
#56509=EDGE_CURVE('',#43877,#43896,#5192,.T.);
#56510=EDGE_CURVE('',#43879,#43884,#5193,.T.);
#56511=EDGE_CURVE('',#43883,#43880,#5194,.T.);
#56512=EDGE_CURVE('',#43923,#43906,#5195,.T.);
#56513=EDGE_CURVE('',#43905,#43924,#5196,.T.);
#56514=EDGE_CURVE('',#43907,#43912,#5197,.T.);
#56515=EDGE_CURVE('',#43911,#43908,#5198,.T.);
#56516=EDGE_CURVE('',#43951,#43934,#5199,.T.);
#56517=EDGE_CURVE('',#43933,#43952,#5200,.T.);
#56518=EDGE_CURVE('',#43935,#43940,#5201,.T.);
#56519=EDGE_CURVE('',#43939,#43936,#5202,.T.);
#56520=EDGE_CURVE('',#43979,#43962,#5203,.T.);
#56521=EDGE_CURVE('',#43961,#43980,#5204,.T.);
#56522=EDGE_CURVE('',#43963,#43968,#5205,.T.);
#56523=EDGE_CURVE('',#43967,#43964,#5206,.T.);
#56524=EDGE_CURVE('',#44007,#43990,#5207,.T.);
#56525=EDGE_CURVE('',#43989,#44008,#5208,.T.);
#56526=EDGE_CURVE('',#43991,#43996,#5209,.T.);
#56527=EDGE_CURVE('',#43995,#43992,#5210,.T.);
#56528=EDGE_CURVE('',#44035,#44018,#5211,.T.);
#56529=EDGE_CURVE('',#44017,#44036,#5212,.T.);
#56530=EDGE_CURVE('',#44019,#44024,#5213,.T.);
#56531=EDGE_CURVE('',#44023,#44020,#5214,.T.);
#56532=EDGE_CURVE('',#42428,#42350,#2262,.T.);
#56533=EDGE_CURVE('',#42345,#42427,#34439,.T.);
#56534=EDGE_CURVE('',#42344,#42426,#34440,.T.);
#56535=EDGE_CURVE('',#42417,#42352,#34441,.T.);
#56536=EDGE_CURVE('',#42341,#42425,#34442,.T.);
#56537=EDGE_CURVE('',#42418,#40466,#34443,.T.);
#56538=EDGE_CURVE('',#42340,#42424,#34444,.T.);
#56539=EDGE_CURVE('',#42419,#40465,#34445,.T.);
#56540=EDGE_CURVE('',#42338,#42423,#2263,.T.);
#56541=EDGE_CURVE('',#42402,#40464,#34446,.T.);
#56542=EDGE_CURVE('',#42333,#42422,#34447,.T.);
#56543=EDGE_CURVE('',#42403,#40463,#34448,.T.);
#56544=EDGE_CURVE('',#40983,#42421,#34449,.T.);
#56545=EDGE_CURVE('',#42408,#40462,#34450,.T.);
#56546=EDGE_CURVE('',#40984,#42420,#34451,.T.);
#56547=EDGE_CURVE('',#42409,#40461,#34452,.T.);
#56548=EDGE_CURVE('',#40985,#42401,#34453,.T.);
#56549=EDGE_CURVE('',#42410,#42371,#34454,.T.);
#56550=EDGE_CURVE('',#40986,#42404,#34455,.T.);
#56551=EDGE_CURVE('',#42411,#42367,#2264,.T.);
#56552=EDGE_CURVE('',#40987,#42407,#34456,.T.);
#56553=EDGE_CURVE('',#42412,#42366,#34457,.T.);
#56554=EDGE_CURVE('',#40988,#42406,#34458,.T.);
#56555=EDGE_CURVE('',#42413,#42363,#34459,.T.);
#56556=EDGE_CURVE('',#42354,#42405,#34460,.T.);
#56557=EDGE_CURVE('',#42414,#42362,#34461,.T.);
#56558=EDGE_CURVE('',#42355,#42416,#2265,.T.);
#56559=EDGE_CURVE('',#42415,#42359,#34462,.T.);
#56560=EDGE_CURVE('',#42456,#42330,#2266,.T.);
#56561=EDGE_CURVE('',#42325,#42455,#34463,.T.);
#56562=EDGE_CURVE('',#42324,#42454,#34464,.T.);
#56563=EDGE_CURVE('',#42445,#42332,#34465,.T.);
#56564=EDGE_CURVE('',#42321,#42453,#34466,.T.);
#56565=EDGE_CURVE('',#42446,#40472,#34467,.T.);
#56566=EDGE_CURVE('',#42320,#42452,#34468,.T.);
#56567=EDGE_CURVE('',#42447,#40471,#34469,.T.);
#56568=EDGE_CURVE('',#42318,#42451,#2267,.T.);
#56569=EDGE_CURVE('',#42430,#40470,#34470,.T.);
#56570=EDGE_CURVE('',#42313,#42450,#34471,.T.);
#56571=EDGE_CURVE('',#42431,#40469,#34472,.T.);
#56572=EDGE_CURVE('',#40977,#42449,#34473,.T.);
#56573=EDGE_CURVE('',#42436,#40468,#34474,.T.);
#56574=EDGE_CURVE('',#40978,#42448,#34475,.T.);
#56575=EDGE_CURVE('',#42437,#40467,#34476,.T.);
#56576=EDGE_CURVE('',#40979,#42429,#34477,.T.);
#56577=EDGE_CURVE('',#42438,#42351,#34478,.T.);
#56578=EDGE_CURVE('',#40980,#42432,#34479,.T.);
#56579=EDGE_CURVE('',#42439,#42347,#2268,.T.);
#56580=EDGE_CURVE('',#40981,#42435,#34480,.T.);
#56581=EDGE_CURVE('',#42440,#42346,#34481,.T.);
#56582=EDGE_CURVE('',#40982,#42434,#34482,.T.);
#56583=EDGE_CURVE('',#42441,#42343,#34483,.T.);
#56584=EDGE_CURVE('',#42334,#42433,#34484,.T.);
#56585=EDGE_CURVE('',#42442,#42342,#34485,.T.);
#56586=EDGE_CURVE('',#42335,#42444,#2269,.T.);
#56587=EDGE_CURVE('',#42443,#42339,#34486,.T.);
#56588=EDGE_CURVE('',#42484,#42310,#2270,.T.);
#56589=EDGE_CURVE('',#42305,#42483,#34487,.T.);
#56590=EDGE_CURVE('',#42304,#42482,#34488,.T.);
#56591=EDGE_CURVE('',#42473,#42312,#34489,.T.);
#56592=EDGE_CURVE('',#42301,#42481,#34490,.T.);
#56593=EDGE_CURVE('',#42474,#40478,#34491,.T.);
#56594=EDGE_CURVE('',#42300,#42480,#34492,.T.);
#56595=EDGE_CURVE('',#42475,#40477,#34493,.T.);
#56596=EDGE_CURVE('',#42298,#42479,#2271,.T.);
#56597=EDGE_CURVE('',#42458,#40476,#34494,.T.);
#56598=EDGE_CURVE('',#42293,#42478,#34495,.T.);
#56599=EDGE_CURVE('',#42459,#40475,#34496,.T.);
#56600=EDGE_CURVE('',#40971,#42477,#34497,.T.);
#56601=EDGE_CURVE('',#42464,#40474,#34498,.T.);
#56602=EDGE_CURVE('',#40972,#42476,#34499,.T.);
#56603=EDGE_CURVE('',#42465,#40473,#34500,.T.);
#56604=EDGE_CURVE('',#40973,#42457,#34501,.T.);
#56605=EDGE_CURVE('',#42466,#42331,#34502,.T.);
#56606=EDGE_CURVE('',#40974,#42460,#34503,.T.);
#56607=EDGE_CURVE('',#42467,#42327,#2272,.T.);
#56608=EDGE_CURVE('',#40975,#42463,#34504,.T.);
#56609=EDGE_CURVE('',#42468,#42326,#34505,.T.);
#56610=EDGE_CURVE('',#40976,#42462,#34506,.T.);
#56611=EDGE_CURVE('',#42469,#42323,#34507,.T.);
#56612=EDGE_CURVE('',#42314,#42461,#34508,.T.);
#56613=EDGE_CURVE('',#42470,#42322,#34509,.T.);
#56614=EDGE_CURVE('',#42315,#42472,#2273,.T.);
#56615=EDGE_CURVE('',#42471,#42319,#34510,.T.);
#56616=EDGE_CURVE('',#42512,#42290,#2274,.T.);
#56617=EDGE_CURVE('',#42285,#42511,#34511,.T.);
#56618=EDGE_CURVE('',#42284,#42510,#34512,.T.);
#56619=EDGE_CURVE('',#42501,#42292,#34513,.T.);
#56620=EDGE_CURVE('',#42281,#42509,#34514,.T.);
#56621=EDGE_CURVE('',#42502,#40484,#34515,.T.);
#56622=EDGE_CURVE('',#42280,#42508,#34516,.T.);
#56623=EDGE_CURVE('',#42503,#40483,#34517,.T.);
#56624=EDGE_CURVE('',#42278,#42507,#2275,.T.);
#56625=EDGE_CURVE('',#42486,#40482,#34518,.T.);
#56626=EDGE_CURVE('',#42273,#42506,#34519,.T.);
#56627=EDGE_CURVE('',#42487,#40481,#34520,.T.);
#56628=EDGE_CURVE('',#40965,#42505,#34521,.T.);
#56629=EDGE_CURVE('',#42492,#40480,#34522,.T.);
#56630=EDGE_CURVE('',#40966,#42504,#34523,.T.);
#56631=EDGE_CURVE('',#42493,#40479,#34524,.T.);
#56632=EDGE_CURVE('',#40967,#42485,#34525,.T.);
#56633=EDGE_CURVE('',#42494,#42311,#34526,.T.);
#56634=EDGE_CURVE('',#40968,#42488,#34527,.T.);
#56635=EDGE_CURVE('',#42495,#42307,#2276,.T.);
#56636=EDGE_CURVE('',#40969,#42491,#34528,.T.);
#56637=EDGE_CURVE('',#42496,#42306,#34529,.T.);
#56638=EDGE_CURVE('',#40970,#42490,#34530,.T.);
#56639=EDGE_CURVE('',#42497,#42303,#34531,.T.);
#56640=EDGE_CURVE('',#42294,#42489,#34532,.T.);
#56641=EDGE_CURVE('',#42498,#42302,#34533,.T.);
#56642=EDGE_CURVE('',#42295,#42500,#2277,.T.);
#56643=EDGE_CURVE('',#42499,#42299,#34534,.T.);
#56644=EDGE_CURVE('',#42540,#42270,#2278,.T.);
#56645=EDGE_CURVE('',#42265,#42539,#34535,.T.);
#56646=EDGE_CURVE('',#42264,#42538,#34536,.T.);
#56647=EDGE_CURVE('',#42529,#42272,#34537,.T.);
#56648=EDGE_CURVE('',#42261,#42537,#34538,.T.);
#56649=EDGE_CURVE('',#42530,#40490,#34539,.T.);
#56650=EDGE_CURVE('',#42260,#42536,#34540,.T.);
#56651=EDGE_CURVE('',#42531,#40489,#34541,.T.);
#56652=EDGE_CURVE('',#42258,#42535,#2279,.T.);
#56653=EDGE_CURVE('',#42514,#40488,#34542,.T.);
#56654=EDGE_CURVE('',#42253,#42534,#34543,.T.);
#56655=EDGE_CURVE('',#42515,#40487,#34544,.T.);
#56656=EDGE_CURVE('',#40959,#42533,#34545,.T.);
#56657=EDGE_CURVE('',#42520,#40486,#34546,.T.);
#56658=EDGE_CURVE('',#40960,#42532,#34547,.T.);
#56659=EDGE_CURVE('',#42521,#40485,#34548,.T.);
#56660=EDGE_CURVE('',#40961,#42513,#34549,.T.);
#56661=EDGE_CURVE('',#42522,#42291,#34550,.T.);
#56662=EDGE_CURVE('',#40962,#42516,#34551,.T.);
#56663=EDGE_CURVE('',#42523,#42287,#2280,.T.);
#56664=EDGE_CURVE('',#40963,#42519,#34552,.T.);
#56665=EDGE_CURVE('',#42524,#42286,#34553,.T.);
#56666=EDGE_CURVE('',#40964,#42518,#34554,.T.);
#56667=EDGE_CURVE('',#42525,#42283,#34555,.T.);
#56668=EDGE_CURVE('',#42274,#42517,#34556,.T.);
#56669=EDGE_CURVE('',#42526,#42282,#34557,.T.);
#56670=EDGE_CURVE('',#42275,#42528,#2281,.T.);
#56671=EDGE_CURVE('',#42527,#42279,#34558,.T.);
#56672=EDGE_CURVE('',#42568,#42250,#2282,.T.);
#56673=EDGE_CURVE('',#42245,#42567,#34559,.T.);
#56674=EDGE_CURVE('',#42244,#42566,#34560,.T.);
#56675=EDGE_CURVE('',#42557,#42252,#34561,.T.);
#56676=EDGE_CURVE('',#42241,#42565,#34562,.T.);
#56677=EDGE_CURVE('',#42558,#40496,#34563,.T.);
#56678=EDGE_CURVE('',#42240,#42564,#34564,.T.);
#56679=EDGE_CURVE('',#42559,#40495,#34565,.T.);
#56680=EDGE_CURVE('',#42238,#42563,#2283,.T.);
#56681=EDGE_CURVE('',#42542,#40494,#34566,.T.);
#56682=EDGE_CURVE('',#42233,#42562,#34567,.T.);
#56683=EDGE_CURVE('',#42543,#40493,#34568,.T.);
#56684=EDGE_CURVE('',#40953,#42561,#34569,.T.);
#56685=EDGE_CURVE('',#42548,#40492,#34570,.T.);
#56686=EDGE_CURVE('',#40954,#42560,#34571,.T.);
#56687=EDGE_CURVE('',#42549,#40491,#34572,.T.);
#56688=EDGE_CURVE('',#40955,#42541,#34573,.T.);
#56689=EDGE_CURVE('',#42550,#42271,#34574,.T.);
#56690=EDGE_CURVE('',#40956,#42544,#34575,.T.);
#56691=EDGE_CURVE('',#42551,#42267,#2284,.T.);
#56692=EDGE_CURVE('',#40957,#42547,#34576,.T.);
#56693=EDGE_CURVE('',#42552,#42266,#34577,.T.);
#56694=EDGE_CURVE('',#40958,#42546,#34578,.T.);
#56695=EDGE_CURVE('',#42553,#42263,#34579,.T.);
#56696=EDGE_CURVE('',#42254,#42545,#34580,.T.);
#56697=EDGE_CURVE('',#42554,#42262,#34581,.T.);
#56698=EDGE_CURVE('',#42255,#42556,#2285,.T.);
#56699=EDGE_CURVE('',#42555,#42259,#34582,.T.);
#56700=EDGE_CURVE('',#42596,#42230,#2286,.T.);
#56701=EDGE_CURVE('',#42225,#42595,#34583,.T.);
#56702=EDGE_CURVE('',#42224,#42594,#34584,.T.);
#56703=EDGE_CURVE('',#42585,#42232,#34585,.T.);
#56704=EDGE_CURVE('',#42221,#42593,#34586,.T.);
#56705=EDGE_CURVE('',#42586,#40502,#34587,.T.);
#56706=EDGE_CURVE('',#42220,#42592,#34588,.T.);
#56707=EDGE_CURVE('',#42587,#40501,#34589,.T.);
#56708=EDGE_CURVE('',#42218,#42591,#2287,.T.);
#56709=EDGE_CURVE('',#42570,#40500,#34590,.T.);
#56710=EDGE_CURVE('',#42213,#42590,#34591,.T.);
#56711=EDGE_CURVE('',#42571,#40499,#34592,.T.);
#56712=EDGE_CURVE('',#40947,#42589,#34593,.T.);
#56713=EDGE_CURVE('',#42576,#40498,#34594,.T.);
#56714=EDGE_CURVE('',#40948,#42588,#34595,.T.);
#56715=EDGE_CURVE('',#42577,#40497,#34596,.T.);
#56716=EDGE_CURVE('',#40949,#42569,#34597,.T.);
#56717=EDGE_CURVE('',#42578,#42251,#34598,.T.);
#56718=EDGE_CURVE('',#40950,#42572,#34599,.T.);
#56719=EDGE_CURVE('',#42579,#42247,#2288,.T.);
#56720=EDGE_CURVE('',#40951,#42575,#34600,.T.);
#56721=EDGE_CURVE('',#42580,#42246,#34601,.T.);
#56722=EDGE_CURVE('',#40952,#42574,#34602,.T.);
#56723=EDGE_CURVE('',#42581,#42243,#34603,.T.);
#56724=EDGE_CURVE('',#42234,#42573,#34604,.T.);
#56725=EDGE_CURVE('',#42582,#42242,#34605,.T.);
#56726=EDGE_CURVE('',#42235,#42584,#2289,.T.);
#56727=EDGE_CURVE('',#42583,#42239,#34606,.T.);
#56728=EDGE_CURVE('',#42624,#42210,#2290,.T.);
#56729=EDGE_CURVE('',#42205,#42623,#34607,.T.);
#56730=EDGE_CURVE('',#42204,#42622,#34608,.T.);
#56731=EDGE_CURVE('',#42613,#42212,#34609,.T.);
#56732=EDGE_CURVE('',#42201,#42621,#34610,.T.);
#56733=EDGE_CURVE('',#42614,#40508,#34611,.T.);
#56734=EDGE_CURVE('',#42200,#42620,#34612,.T.);
#56735=EDGE_CURVE('',#42615,#40507,#34613,.T.);
#56736=EDGE_CURVE('',#42198,#42619,#2291,.T.);
#56737=EDGE_CURVE('',#42598,#40506,#34614,.T.);
#56738=EDGE_CURVE('',#42193,#42618,#34615,.T.);
#56739=EDGE_CURVE('',#42599,#40505,#34616,.T.);
#56740=EDGE_CURVE('',#40941,#42617,#34617,.T.);
#56741=EDGE_CURVE('',#42604,#40504,#34618,.T.);
#56742=EDGE_CURVE('',#40942,#42616,#34619,.T.);
#56743=EDGE_CURVE('',#42605,#40503,#34620,.T.);
#56744=EDGE_CURVE('',#40943,#42597,#34621,.T.);
#56745=EDGE_CURVE('',#42606,#42231,#34622,.T.);
#56746=EDGE_CURVE('',#40944,#42600,#34623,.T.);
#56747=EDGE_CURVE('',#42607,#42227,#2292,.T.);
#56748=EDGE_CURVE('',#40945,#42603,#34624,.T.);
#56749=EDGE_CURVE('',#42608,#42226,#34625,.T.);
#56750=EDGE_CURVE('',#40946,#42602,#34626,.T.);
#56751=EDGE_CURVE('',#42609,#42223,#34627,.T.);
#56752=EDGE_CURVE('',#42214,#42601,#34628,.T.);
#56753=EDGE_CURVE('',#42610,#42222,#34629,.T.);
#56754=EDGE_CURVE('',#42215,#42612,#2293,.T.);
#56755=EDGE_CURVE('',#42611,#42219,#34630,.T.);
#56756=EDGE_CURVE('',#42652,#42190,#2294,.T.);
#56757=EDGE_CURVE('',#42185,#42651,#34631,.T.);
#56758=EDGE_CURVE('',#42184,#42650,#34632,.T.);
#56759=EDGE_CURVE('',#42641,#42192,#34633,.T.);
#56760=EDGE_CURVE('',#42181,#42649,#34634,.T.);
#56761=EDGE_CURVE('',#42642,#40514,#34635,.T.);
#56762=EDGE_CURVE('',#42180,#42648,#34636,.T.);
#56763=EDGE_CURVE('',#42643,#40513,#34637,.T.);
#56764=EDGE_CURVE('',#42178,#42647,#2295,.T.);
#56765=EDGE_CURVE('',#42626,#40512,#34638,.T.);
#56766=EDGE_CURVE('',#42173,#42646,#34639,.T.);
#56767=EDGE_CURVE('',#42627,#40511,#34640,.T.);
#56768=EDGE_CURVE('',#40935,#42645,#34641,.T.);
#56769=EDGE_CURVE('',#42632,#40510,#34642,.T.);
#56770=EDGE_CURVE('',#40936,#42644,#34643,.T.);
#56771=EDGE_CURVE('',#42633,#40509,#34644,.T.);
#56772=EDGE_CURVE('',#40937,#42625,#34645,.T.);
#56773=EDGE_CURVE('',#42634,#42211,#34646,.T.);
#56774=EDGE_CURVE('',#40938,#42628,#34647,.T.);
#56775=EDGE_CURVE('',#42635,#42207,#2296,.T.);
#56776=EDGE_CURVE('',#40939,#42631,#34648,.T.);
#56777=EDGE_CURVE('',#42636,#42206,#34649,.T.);
#56778=EDGE_CURVE('',#40940,#42630,#34650,.T.);
#56779=EDGE_CURVE('',#42637,#42203,#34651,.T.);
#56780=EDGE_CURVE('',#42194,#42629,#34652,.T.);
#56781=EDGE_CURVE('',#42638,#42202,#34653,.T.);
#56782=EDGE_CURVE('',#42195,#42640,#2297,.T.);
#56783=EDGE_CURVE('',#42639,#42199,#34654,.T.);
#56784=EDGE_CURVE('',#42680,#42170,#2298,.T.);
#56785=EDGE_CURVE('',#42165,#42679,#34655,.T.);
#56786=EDGE_CURVE('',#42164,#42678,#34656,.T.);
#56787=EDGE_CURVE('',#42669,#42172,#34657,.T.);
#56788=EDGE_CURVE('',#42161,#42677,#34658,.T.);
#56789=EDGE_CURVE('',#42670,#40520,#34659,.T.);
#56790=EDGE_CURVE('',#42160,#42676,#34660,.T.);
#56791=EDGE_CURVE('',#42671,#40519,#34661,.T.);
#56792=EDGE_CURVE('',#42158,#42675,#2299,.T.);
#56793=EDGE_CURVE('',#42654,#40518,#34662,.T.);
#56794=EDGE_CURVE('',#42153,#42674,#34663,.T.);
#56795=EDGE_CURVE('',#42655,#40517,#34664,.T.);
#56796=EDGE_CURVE('',#40929,#42673,#34665,.T.);
#56797=EDGE_CURVE('',#42660,#40516,#34666,.T.);
#56798=EDGE_CURVE('',#40930,#42672,#34667,.T.);
#56799=EDGE_CURVE('',#42661,#40515,#34668,.T.);
#56800=EDGE_CURVE('',#40931,#42653,#34669,.T.);
#56801=EDGE_CURVE('',#42662,#42191,#34670,.T.);
#56802=EDGE_CURVE('',#40932,#42656,#34671,.T.);
#56803=EDGE_CURVE('',#42663,#42187,#2300,.T.);
#56804=EDGE_CURVE('',#40933,#42659,#34672,.T.);
#56805=EDGE_CURVE('',#42664,#42186,#34673,.T.);
#56806=EDGE_CURVE('',#40934,#42658,#34674,.T.);
#56807=EDGE_CURVE('',#42665,#42183,#34675,.T.);
#56808=EDGE_CURVE('',#42174,#42657,#34676,.T.);
#56809=EDGE_CURVE('',#42666,#42182,#34677,.T.);
#56810=EDGE_CURVE('',#42175,#42668,#2301,.T.);
#56811=EDGE_CURVE('',#42667,#42179,#34678,.T.);
#56812=EDGE_CURVE('',#42708,#42150,#2302,.T.);
#56813=EDGE_CURVE('',#42145,#42707,#34679,.T.);
#56814=EDGE_CURVE('',#42144,#42706,#34680,.T.);
#56815=EDGE_CURVE('',#42697,#42152,#34681,.T.);
#56816=EDGE_CURVE('',#42141,#42705,#34682,.T.);
#56817=EDGE_CURVE('',#42698,#40526,#34683,.T.);
#56818=EDGE_CURVE('',#42140,#42704,#34684,.T.);
#56819=EDGE_CURVE('',#42699,#40525,#34685,.T.);
#56820=EDGE_CURVE('',#42138,#42703,#2303,.T.);
#56821=EDGE_CURVE('',#42682,#40524,#34686,.T.);
#56822=EDGE_CURVE('',#42133,#42702,#34687,.T.);
#56823=EDGE_CURVE('',#42683,#40523,#34688,.T.);
#56824=EDGE_CURVE('',#40923,#42701,#34689,.T.);
#56825=EDGE_CURVE('',#42688,#40522,#34690,.T.);
#56826=EDGE_CURVE('',#40924,#42700,#34691,.T.);
#56827=EDGE_CURVE('',#42689,#40521,#34692,.T.);
#56828=EDGE_CURVE('',#40925,#42681,#34693,.T.);
#56829=EDGE_CURVE('',#42690,#42171,#34694,.T.);
#56830=EDGE_CURVE('',#40926,#42684,#34695,.T.);
#56831=EDGE_CURVE('',#42691,#42167,#2304,.T.);
#56832=EDGE_CURVE('',#40927,#42687,#34696,.T.);
#56833=EDGE_CURVE('',#42692,#42166,#34697,.T.);
#56834=EDGE_CURVE('',#40928,#42686,#34698,.T.);
#56835=EDGE_CURVE('',#42693,#42163,#34699,.T.);
#56836=EDGE_CURVE('',#42154,#42685,#34700,.T.);
#56837=EDGE_CURVE('',#42694,#42162,#34701,.T.);
#56838=EDGE_CURVE('',#42155,#42696,#2305,.T.);
#56839=EDGE_CURVE('',#42695,#42159,#34702,.T.);
#56840=EDGE_CURVE('',#42736,#42130,#2306,.T.);
#56841=EDGE_CURVE('',#42125,#42735,#34703,.T.);
#56842=EDGE_CURVE('',#42124,#42734,#34704,.T.);
#56843=EDGE_CURVE('',#42725,#42132,#34705,.T.);
#56844=EDGE_CURVE('',#42121,#42733,#34706,.T.);
#56845=EDGE_CURVE('',#42726,#40532,#34707,.T.);
#56846=EDGE_CURVE('',#42120,#42732,#34708,.T.);
#56847=EDGE_CURVE('',#42727,#40531,#34709,.T.);
#56848=EDGE_CURVE('',#42118,#42731,#2307,.T.);
#56849=EDGE_CURVE('',#42710,#40530,#34710,.T.);
#56850=EDGE_CURVE('',#42113,#42730,#34711,.T.);
#56851=EDGE_CURVE('',#42711,#40529,#34712,.T.);
#56852=EDGE_CURVE('',#40917,#42729,#34713,.T.);
#56853=EDGE_CURVE('',#42716,#40528,#34714,.T.);
#56854=EDGE_CURVE('',#40918,#42728,#34715,.T.);
#56855=EDGE_CURVE('',#42717,#40527,#34716,.T.);
#56856=EDGE_CURVE('',#40919,#42709,#34717,.T.);
#56857=EDGE_CURVE('',#42718,#42151,#34718,.T.);
#56858=EDGE_CURVE('',#40920,#42712,#34719,.T.);
#56859=EDGE_CURVE('',#42719,#42147,#2308,.T.);
#56860=EDGE_CURVE('',#40921,#42715,#34720,.T.);
#56861=EDGE_CURVE('',#42720,#42146,#34721,.T.);
#56862=EDGE_CURVE('',#40922,#42714,#34722,.T.);
#56863=EDGE_CURVE('',#42721,#42143,#34723,.T.);
#56864=EDGE_CURVE('',#42134,#42713,#34724,.T.);
#56865=EDGE_CURVE('',#42722,#42142,#34725,.T.);
#56866=EDGE_CURVE('',#42135,#42724,#2309,.T.);
#56867=EDGE_CURVE('',#42723,#42139,#34726,.T.);
#56868=EDGE_CURVE('',#42764,#42110,#2310,.T.);
#56869=EDGE_CURVE('',#42105,#42763,#34727,.T.);
#56870=EDGE_CURVE('',#42104,#42762,#34728,.T.);
#56871=EDGE_CURVE('',#42753,#42112,#34729,.T.);
#56872=EDGE_CURVE('',#42101,#42761,#34730,.T.);
#56873=EDGE_CURVE('',#42754,#40538,#34731,.T.);
#56874=EDGE_CURVE('',#42100,#42760,#34732,.T.);
#56875=EDGE_CURVE('',#42755,#40537,#34733,.T.);
#56876=EDGE_CURVE('',#42098,#42759,#2311,.T.);
#56877=EDGE_CURVE('',#42738,#40536,#34734,.T.);
#56878=EDGE_CURVE('',#42093,#42758,#34735,.T.);
#56879=EDGE_CURVE('',#42739,#40535,#34736,.T.);
#56880=EDGE_CURVE('',#40911,#42757,#34737,.T.);
#56881=EDGE_CURVE('',#42744,#40534,#34738,.T.);
#56882=EDGE_CURVE('',#40912,#42756,#34739,.T.);
#56883=EDGE_CURVE('',#42745,#40533,#34740,.T.);
#56884=EDGE_CURVE('',#40913,#42737,#34741,.T.);
#56885=EDGE_CURVE('',#42746,#42131,#34742,.T.);
#56886=EDGE_CURVE('',#40914,#42740,#34743,.T.);
#56887=EDGE_CURVE('',#42747,#42127,#2312,.T.);
#56888=EDGE_CURVE('',#40915,#42743,#34744,.T.);
#56889=EDGE_CURVE('',#42748,#42126,#34745,.T.);
#56890=EDGE_CURVE('',#40916,#42742,#34746,.T.);
#56891=EDGE_CURVE('',#42749,#42123,#34747,.T.);
#56892=EDGE_CURVE('',#42114,#42741,#34748,.T.);
#56893=EDGE_CURVE('',#42750,#42122,#34749,.T.);
#56894=EDGE_CURVE('',#42115,#42752,#2313,.T.);
#56895=EDGE_CURVE('',#42751,#42119,#34750,.T.);
#56896=EDGE_CURVE('',#42792,#42090,#2314,.T.);
#56897=EDGE_CURVE('',#42085,#42791,#34751,.T.);
#56898=EDGE_CURVE('',#42084,#42790,#34752,.T.);
#56899=EDGE_CURVE('',#42781,#42092,#34753,.T.);
#56900=EDGE_CURVE('',#42081,#42789,#34754,.T.);
#56901=EDGE_CURVE('',#42782,#40544,#34755,.T.);
#56902=EDGE_CURVE('',#42080,#42788,#34756,.T.);
#56903=EDGE_CURVE('',#42783,#40543,#34757,.T.);
#56904=EDGE_CURVE('',#42078,#42787,#2315,.T.);
#56905=EDGE_CURVE('',#42766,#40542,#34758,.T.);
#56906=EDGE_CURVE('',#42073,#42786,#34759,.T.);
#56907=EDGE_CURVE('',#42767,#40541,#34760,.T.);
#56908=EDGE_CURVE('',#40905,#42785,#34761,.T.);
#56909=EDGE_CURVE('',#42772,#40540,#34762,.T.);
#56910=EDGE_CURVE('',#40906,#42784,#34763,.T.);
#56911=EDGE_CURVE('',#42773,#40539,#34764,.T.);
#56912=EDGE_CURVE('',#40907,#42765,#34765,.T.);
#56913=EDGE_CURVE('',#42774,#42111,#34766,.T.);
#56914=EDGE_CURVE('',#40908,#42768,#34767,.T.);
#56915=EDGE_CURVE('',#42775,#42107,#2316,.T.);
#56916=EDGE_CURVE('',#40909,#42771,#34768,.T.);
#56917=EDGE_CURVE('',#42776,#42106,#34769,.T.);
#56918=EDGE_CURVE('',#40910,#42770,#34770,.T.);
#56919=EDGE_CURVE('',#42777,#42103,#34771,.T.);
#56920=EDGE_CURVE('',#42094,#42769,#34772,.T.);
#56921=EDGE_CURVE('',#42778,#42102,#34773,.T.);
#56922=EDGE_CURVE('',#42095,#42780,#2317,.T.);
#56923=EDGE_CURVE('',#42779,#42099,#34774,.T.);
#56924=EDGE_CURVE('',#42820,#42070,#2318,.T.);
#56925=EDGE_CURVE('',#42065,#42819,#34775,.T.);
#56926=EDGE_CURVE('',#42064,#42818,#34776,.T.);
#56927=EDGE_CURVE('',#42809,#42072,#34777,.T.);
#56928=EDGE_CURVE('',#42061,#42817,#34778,.T.);
#56929=EDGE_CURVE('',#42810,#40550,#34779,.T.);
#56930=EDGE_CURVE('',#42060,#42816,#34780,.T.);
#56931=EDGE_CURVE('',#42811,#40549,#34781,.T.);
#56932=EDGE_CURVE('',#42058,#42815,#2319,.T.);
#56933=EDGE_CURVE('',#42794,#40548,#34782,.T.);
#56934=EDGE_CURVE('',#42053,#42814,#34783,.T.);
#56935=EDGE_CURVE('',#42795,#40547,#34784,.T.);
#56936=EDGE_CURVE('',#40899,#42813,#34785,.T.);
#56937=EDGE_CURVE('',#42800,#40546,#34786,.T.);
#56938=EDGE_CURVE('',#40900,#42812,#34787,.T.);
#56939=EDGE_CURVE('',#42801,#40545,#34788,.T.);
#56940=EDGE_CURVE('',#40901,#42793,#34789,.T.);
#56941=EDGE_CURVE('',#42802,#42091,#34790,.T.);
#56942=EDGE_CURVE('',#40902,#42796,#34791,.T.);
#56943=EDGE_CURVE('',#42803,#42087,#2320,.T.);
#56944=EDGE_CURVE('',#40903,#42799,#34792,.T.);
#56945=EDGE_CURVE('',#42804,#42086,#34793,.T.);
#56946=EDGE_CURVE('',#40904,#42798,#34794,.T.);
#56947=EDGE_CURVE('',#42805,#42083,#34795,.T.);
#56948=EDGE_CURVE('',#42074,#42797,#34796,.T.);
#56949=EDGE_CURVE('',#42806,#42082,#34797,.T.);
#56950=EDGE_CURVE('',#42075,#42808,#2321,.T.);
#56951=EDGE_CURVE('',#42807,#42079,#34798,.T.);
#56952=EDGE_CURVE('',#42848,#42050,#2322,.T.);
#56953=EDGE_CURVE('',#42045,#42847,#34799,.T.);
#56954=EDGE_CURVE('',#42044,#42846,#34800,.T.);
#56955=EDGE_CURVE('',#42837,#42052,#34801,.T.);
#56956=EDGE_CURVE('',#42041,#42845,#34802,.T.);
#56957=EDGE_CURVE('',#42838,#40556,#34803,.T.);
#56958=EDGE_CURVE('',#42040,#42844,#34804,.T.);
#56959=EDGE_CURVE('',#42839,#40555,#34805,.T.);
#56960=EDGE_CURVE('',#42038,#42843,#2323,.T.);
#56961=EDGE_CURVE('',#42822,#40554,#34806,.T.);
#56962=EDGE_CURVE('',#42033,#42842,#34807,.T.);
#56963=EDGE_CURVE('',#42823,#40553,#34808,.T.);
#56964=EDGE_CURVE('',#40893,#42841,#34809,.T.);
#56965=EDGE_CURVE('',#42828,#40552,#34810,.T.);
#56966=EDGE_CURVE('',#40894,#42840,#34811,.T.);
#56967=EDGE_CURVE('',#42829,#40551,#34812,.T.);
#56968=EDGE_CURVE('',#40895,#42821,#34813,.T.);
#56969=EDGE_CURVE('',#42830,#42071,#34814,.T.);
#56970=EDGE_CURVE('',#40896,#42824,#34815,.T.);
#56971=EDGE_CURVE('',#42831,#42067,#2324,.T.);
#56972=EDGE_CURVE('',#40897,#42827,#34816,.T.);
#56973=EDGE_CURVE('',#42832,#42066,#34817,.T.);
#56974=EDGE_CURVE('',#40898,#42826,#34818,.T.);
#56975=EDGE_CURVE('',#42833,#42063,#34819,.T.);
#56976=EDGE_CURVE('',#42054,#42825,#34820,.T.);
#56977=EDGE_CURVE('',#42834,#42062,#34821,.T.);
#56978=EDGE_CURVE('',#42055,#42836,#2325,.T.);
#56979=EDGE_CURVE('',#42835,#42059,#34822,.T.);
#56980=EDGE_CURVE('',#42876,#42030,#2326,.T.);
#56981=EDGE_CURVE('',#42025,#42875,#34823,.T.);
#56982=EDGE_CURVE('',#42024,#42874,#34824,.T.);
#56983=EDGE_CURVE('',#42865,#42032,#34825,.T.);
#56984=EDGE_CURVE('',#42021,#42873,#34826,.T.);
#56985=EDGE_CURVE('',#42866,#40562,#34827,.T.);
#56986=EDGE_CURVE('',#42020,#42872,#34828,.T.);
#56987=EDGE_CURVE('',#42867,#40561,#34829,.T.);
#56988=EDGE_CURVE('',#42018,#42871,#2327,.T.);
#56989=EDGE_CURVE('',#42850,#40560,#34830,.T.);
#56990=EDGE_CURVE('',#42013,#42870,#34831,.T.);
#56991=EDGE_CURVE('',#42851,#40559,#34832,.T.);
#56992=EDGE_CURVE('',#40887,#42869,#34833,.T.);
#56993=EDGE_CURVE('',#42856,#40558,#34834,.T.);
#56994=EDGE_CURVE('',#40888,#42868,#34835,.T.);
#56995=EDGE_CURVE('',#42857,#40557,#34836,.T.);
#56996=EDGE_CURVE('',#40889,#42849,#34837,.T.);
#56997=EDGE_CURVE('',#42858,#42051,#34838,.T.);
#56998=EDGE_CURVE('',#40890,#42852,#34839,.T.);
#56999=EDGE_CURVE('',#42859,#42047,#2328,.T.);
#57000=EDGE_CURVE('',#40891,#42855,#34840,.T.);
#57001=EDGE_CURVE('',#42860,#42046,#34841,.T.);
#57002=EDGE_CURVE('',#40892,#42854,#34842,.T.);
#57003=EDGE_CURVE('',#42861,#42043,#34843,.T.);
#57004=EDGE_CURVE('',#42034,#42853,#34844,.T.);
#57005=EDGE_CURVE('',#42862,#42042,#34845,.T.);
#57006=EDGE_CURVE('',#42035,#42864,#2329,.T.);
#57007=EDGE_CURVE('',#42863,#42039,#34846,.T.);
#57008=EDGE_CURVE('',#42904,#42010,#2330,.T.);
#57009=EDGE_CURVE('',#42005,#42903,#34847,.T.);
#57010=EDGE_CURVE('',#42004,#42902,#34848,.T.);
#57011=EDGE_CURVE('',#42893,#42012,#34849,.T.);
#57012=EDGE_CURVE('',#42001,#42901,#34850,.T.);
#57013=EDGE_CURVE('',#42894,#40568,#34851,.T.);
#57014=EDGE_CURVE('',#42000,#42900,#34852,.T.);
#57015=EDGE_CURVE('',#42895,#40567,#34853,.T.);
#57016=EDGE_CURVE('',#41998,#42899,#2331,.T.);
#57017=EDGE_CURVE('',#42878,#40566,#34854,.T.);
#57018=EDGE_CURVE('',#41993,#42898,#34855,.T.);
#57019=EDGE_CURVE('',#42879,#40565,#34856,.T.);
#57020=EDGE_CURVE('',#40881,#42897,#34857,.T.);
#57021=EDGE_CURVE('',#42884,#40564,#34858,.T.);
#57022=EDGE_CURVE('',#40882,#42896,#34859,.T.);
#57023=EDGE_CURVE('',#42885,#40563,#34860,.T.);
#57024=EDGE_CURVE('',#40883,#42877,#34861,.T.);
#57025=EDGE_CURVE('',#42886,#42031,#34862,.T.);
#57026=EDGE_CURVE('',#40884,#42880,#34863,.T.);
#57027=EDGE_CURVE('',#42887,#42027,#2332,.T.);
#57028=EDGE_CURVE('',#40885,#42883,#34864,.T.);
#57029=EDGE_CURVE('',#42888,#42026,#34865,.T.);
#57030=EDGE_CURVE('',#40886,#42882,#34866,.T.);
#57031=EDGE_CURVE('',#42889,#42023,#34867,.T.);
#57032=EDGE_CURVE('',#42014,#42881,#34868,.T.);
#57033=EDGE_CURVE('',#42890,#42022,#34869,.T.);
#57034=EDGE_CURVE('',#42015,#42892,#2333,.T.);
#57035=EDGE_CURVE('',#42891,#42019,#34870,.T.);
#57036=EDGE_CURVE('',#42932,#41990,#2334,.T.);
#57037=EDGE_CURVE('',#41985,#42931,#34871,.T.);
#57038=EDGE_CURVE('',#41984,#42930,#34872,.T.);
#57039=EDGE_CURVE('',#42921,#41992,#34873,.T.);
#57040=EDGE_CURVE('',#41981,#42929,#34874,.T.);
#57041=EDGE_CURVE('',#42922,#40574,#34875,.T.);
#57042=EDGE_CURVE('',#41980,#42928,#34876,.T.);
#57043=EDGE_CURVE('',#42923,#40573,#34877,.T.);
#57044=EDGE_CURVE('',#41978,#42927,#2335,.T.);
#57045=EDGE_CURVE('',#42906,#40572,#34878,.T.);
#57046=EDGE_CURVE('',#41973,#42926,#34879,.T.);
#57047=EDGE_CURVE('',#42907,#40571,#34880,.T.);
#57048=EDGE_CURVE('',#40875,#42925,#34881,.T.);
#57049=EDGE_CURVE('',#42912,#40570,#34882,.T.);
#57050=EDGE_CURVE('',#40876,#42924,#34883,.T.);
#57051=EDGE_CURVE('',#42913,#40569,#34884,.T.);
#57052=EDGE_CURVE('',#40877,#42905,#34885,.T.);
#57053=EDGE_CURVE('',#42914,#42011,#34886,.T.);
#57054=EDGE_CURVE('',#40878,#42908,#34887,.T.);
#57055=EDGE_CURVE('',#42915,#42007,#2336,.T.);
#57056=EDGE_CURVE('',#40879,#42911,#34888,.T.);
#57057=EDGE_CURVE('',#42916,#42006,#34889,.T.);
#57058=EDGE_CURVE('',#40880,#42910,#34890,.T.);
#57059=EDGE_CURVE('',#42917,#42003,#34891,.T.);
#57060=EDGE_CURVE('',#41994,#42909,#34892,.T.);
#57061=EDGE_CURVE('',#42918,#42002,#34893,.T.);
#57062=EDGE_CURVE('',#41995,#42920,#2337,.T.);
#57063=EDGE_CURVE('',#42919,#41999,#34894,.T.);
#57064=EDGE_CURVE('',#42960,#41970,#2338,.T.);
#57065=EDGE_CURVE('',#41965,#42959,#34895,.T.);
#57066=EDGE_CURVE('',#41964,#42958,#34896,.T.);
#57067=EDGE_CURVE('',#42949,#41972,#34897,.T.);
#57068=EDGE_CURVE('',#41961,#42957,#34898,.T.);
#57069=EDGE_CURVE('',#42950,#40580,#34899,.T.);
#57070=EDGE_CURVE('',#41960,#42956,#34900,.T.);
#57071=EDGE_CURVE('',#42951,#40579,#34901,.T.);
#57072=EDGE_CURVE('',#41958,#42955,#2339,.T.);
#57073=EDGE_CURVE('',#42934,#40578,#34902,.T.);
#57074=EDGE_CURVE('',#41953,#42954,#34903,.T.);
#57075=EDGE_CURVE('',#42935,#40577,#34904,.T.);
#57076=EDGE_CURVE('',#40869,#42953,#34905,.T.);
#57077=EDGE_CURVE('',#42940,#40576,#34906,.T.);
#57078=EDGE_CURVE('',#40870,#42952,#34907,.T.);
#57079=EDGE_CURVE('',#42941,#40575,#34908,.T.);
#57080=EDGE_CURVE('',#40871,#42933,#34909,.T.);
#57081=EDGE_CURVE('',#42942,#41991,#34910,.T.);
#57082=EDGE_CURVE('',#40872,#42936,#34911,.T.);
#57083=EDGE_CURVE('',#42943,#41987,#2340,.T.);
#57084=EDGE_CURVE('',#40873,#42939,#34912,.T.);
#57085=EDGE_CURVE('',#42944,#41986,#34913,.T.);
#57086=EDGE_CURVE('',#40874,#42938,#34914,.T.);
#57087=EDGE_CURVE('',#42945,#41983,#34915,.T.);
#57088=EDGE_CURVE('',#41974,#42937,#34916,.T.);
#57089=EDGE_CURVE('',#42946,#41982,#34917,.T.);
#57090=EDGE_CURVE('',#41975,#42948,#2341,.T.);
#57091=EDGE_CURVE('',#42947,#41979,#34918,.T.);
#57092=EDGE_CURVE('',#42988,#41950,#2342,.T.);
#57093=EDGE_CURVE('',#41945,#42987,#34919,.T.);
#57094=EDGE_CURVE('',#41944,#42986,#34920,.T.);
#57095=EDGE_CURVE('',#42977,#41952,#34921,.T.);
#57096=EDGE_CURVE('',#41941,#42985,#34922,.T.);
#57097=EDGE_CURVE('',#42978,#40586,#34923,.T.);
#57098=EDGE_CURVE('',#41940,#42984,#34924,.T.);
#57099=EDGE_CURVE('',#42979,#40585,#34925,.T.);
#57100=EDGE_CURVE('',#41938,#42983,#2343,.T.);
#57101=EDGE_CURVE('',#42962,#40584,#34926,.T.);
#57102=EDGE_CURVE('',#41933,#42982,#34927,.T.);
#57103=EDGE_CURVE('',#42963,#40583,#34928,.T.);
#57104=EDGE_CURVE('',#40863,#42981,#34929,.T.);
#57105=EDGE_CURVE('',#42968,#40582,#34930,.T.);
#57106=EDGE_CURVE('',#40864,#42980,#34931,.T.);
#57107=EDGE_CURVE('',#42969,#40581,#34932,.T.);
#57108=EDGE_CURVE('',#40865,#42961,#34933,.T.);
#57109=EDGE_CURVE('',#42970,#41971,#34934,.T.);
#57110=EDGE_CURVE('',#40866,#42964,#34935,.T.);
#57111=EDGE_CURVE('',#42971,#41967,#2344,.T.);
#57112=EDGE_CURVE('',#40867,#42967,#34936,.T.);
#57113=EDGE_CURVE('',#42972,#41966,#34937,.T.);
#57114=EDGE_CURVE('',#40868,#42966,#34938,.T.);
#57115=EDGE_CURVE('',#42973,#41963,#34939,.T.);
#57116=EDGE_CURVE('',#41954,#42965,#34940,.T.);
#57117=EDGE_CURVE('',#42974,#41962,#34941,.T.);
#57118=EDGE_CURVE('',#41955,#42976,#2345,.T.);
#57119=EDGE_CURVE('',#42975,#41959,#34942,.T.);
#57120=EDGE_CURVE('',#43016,#41930,#2346,.T.);
#57121=EDGE_CURVE('',#41925,#43015,#34943,.T.);
#57122=EDGE_CURVE('',#41924,#43014,#34944,.T.);
#57123=EDGE_CURVE('',#43005,#41932,#34945,.T.);
#57124=EDGE_CURVE('',#41921,#43013,#34946,.T.);
#57125=EDGE_CURVE('',#43006,#40592,#34947,.T.);
#57126=EDGE_CURVE('',#41920,#43012,#34948,.T.);
#57127=EDGE_CURVE('',#43007,#40591,#34949,.T.);
#57128=EDGE_CURVE('',#41918,#43011,#2347,.T.);
#57129=EDGE_CURVE('',#42990,#40590,#34950,.T.);
#57130=EDGE_CURVE('',#41913,#43010,#34951,.T.);
#57131=EDGE_CURVE('',#42991,#40589,#34952,.T.);
#57132=EDGE_CURVE('',#40857,#43009,#34953,.T.);
#57133=EDGE_CURVE('',#42996,#40588,#34954,.T.);
#57134=EDGE_CURVE('',#40858,#43008,#34955,.T.);
#57135=EDGE_CURVE('',#42997,#40587,#34956,.T.);
#57136=EDGE_CURVE('',#40859,#42989,#34957,.T.);
#57137=EDGE_CURVE('',#42998,#41951,#34958,.T.);
#57138=EDGE_CURVE('',#40860,#42992,#34959,.T.);
#57139=EDGE_CURVE('',#42999,#41947,#2348,.T.);
#57140=EDGE_CURVE('',#40861,#42995,#34960,.T.);
#57141=EDGE_CURVE('',#43000,#41946,#34961,.T.);
#57142=EDGE_CURVE('',#40862,#42994,#34962,.T.);
#57143=EDGE_CURVE('',#43001,#41943,#34963,.T.);
#57144=EDGE_CURVE('',#41934,#42993,#34964,.T.);
#57145=EDGE_CURVE('',#43002,#41942,#34965,.T.);
#57146=EDGE_CURVE('',#41935,#43004,#2349,.T.);
#57147=EDGE_CURVE('',#43003,#41939,#34966,.T.);
#57148=EDGE_CURVE('',#43044,#41910,#2350,.T.);
#57149=EDGE_CURVE('',#41905,#43043,#34967,.T.);
#57150=EDGE_CURVE('',#41904,#43042,#34968,.T.);
#57151=EDGE_CURVE('',#43033,#41912,#34969,.T.);
#57152=EDGE_CURVE('',#41901,#43041,#34970,.T.);
#57153=EDGE_CURVE('',#43034,#40598,#34971,.T.);
#57154=EDGE_CURVE('',#41900,#43040,#34972,.T.);
#57155=EDGE_CURVE('',#43035,#40597,#34973,.T.);
#57156=EDGE_CURVE('',#41898,#43039,#2351,.T.);
#57157=EDGE_CURVE('',#43018,#40596,#34974,.T.);
#57158=EDGE_CURVE('',#41893,#43038,#34975,.T.);
#57159=EDGE_CURVE('',#43019,#40595,#34976,.T.);
#57160=EDGE_CURVE('',#40851,#43037,#34977,.T.);
#57161=EDGE_CURVE('',#43024,#40594,#34978,.T.);
#57162=EDGE_CURVE('',#40852,#43036,#34979,.T.);
#57163=EDGE_CURVE('',#43025,#40593,#34980,.T.);
#57164=EDGE_CURVE('',#40853,#43017,#34981,.T.);
#57165=EDGE_CURVE('',#43026,#41931,#34982,.T.);
#57166=EDGE_CURVE('',#40854,#43020,#34983,.T.);
#57167=EDGE_CURVE('',#43027,#41927,#2352,.T.);
#57168=EDGE_CURVE('',#40855,#43023,#34984,.T.);
#57169=EDGE_CURVE('',#43028,#41926,#34985,.T.);
#57170=EDGE_CURVE('',#40856,#43022,#34986,.T.);
#57171=EDGE_CURVE('',#43029,#41923,#34987,.T.);
#57172=EDGE_CURVE('',#41914,#43021,#34988,.T.);
#57173=EDGE_CURVE('',#43030,#41922,#34989,.T.);
#57174=EDGE_CURVE('',#41915,#43032,#2353,.T.);
#57175=EDGE_CURVE('',#43031,#41919,#34990,.T.);
#57176=EDGE_CURVE('',#43072,#41890,#2354,.T.);
#57177=EDGE_CURVE('',#41885,#43071,#34991,.T.);
#57178=EDGE_CURVE('',#41884,#43070,#34992,.T.);
#57179=EDGE_CURVE('',#43061,#41892,#34993,.T.);
#57180=EDGE_CURVE('',#41881,#43069,#34994,.T.);
#57181=EDGE_CURVE('',#43062,#40604,#34995,.T.);
#57182=EDGE_CURVE('',#41880,#43068,#34996,.T.);
#57183=EDGE_CURVE('',#43063,#40603,#34997,.T.);
#57184=EDGE_CURVE('',#41878,#43067,#2355,.T.);
#57185=EDGE_CURVE('',#43046,#40602,#34998,.T.);
#57186=EDGE_CURVE('',#41873,#43066,#34999,.T.);
#57187=EDGE_CURVE('',#43047,#40601,#35000,.T.);
#57188=EDGE_CURVE('',#40845,#43065,#35001,.T.);
#57189=EDGE_CURVE('',#43052,#40600,#35002,.T.);
#57190=EDGE_CURVE('',#40846,#43064,#35003,.T.);
#57191=EDGE_CURVE('',#43053,#40599,#35004,.T.);
#57192=EDGE_CURVE('',#40847,#43045,#35005,.T.);
#57193=EDGE_CURVE('',#43054,#41911,#35006,.T.);
#57194=EDGE_CURVE('',#40848,#43048,#35007,.T.);
#57195=EDGE_CURVE('',#43055,#41907,#2356,.T.);
#57196=EDGE_CURVE('',#40849,#43051,#35008,.T.);
#57197=EDGE_CURVE('',#43056,#41906,#35009,.T.);
#57198=EDGE_CURVE('',#40850,#43050,#35010,.T.);
#57199=EDGE_CURVE('',#43057,#41903,#35011,.T.);
#57200=EDGE_CURVE('',#41894,#43049,#35012,.T.);
#57201=EDGE_CURVE('',#43058,#41902,#35013,.T.);
#57202=EDGE_CURVE('',#41895,#43060,#2357,.T.);
#57203=EDGE_CURVE('',#43059,#41899,#35014,.T.);
#57204=EDGE_CURVE('',#43100,#41870,#2358,.T.);
#57205=EDGE_CURVE('',#41865,#43099,#35015,.T.);
#57206=EDGE_CURVE('',#41864,#43098,#35016,.T.);
#57207=EDGE_CURVE('',#43089,#41872,#35017,.T.);
#57208=EDGE_CURVE('',#41861,#43097,#35018,.T.);
#57209=EDGE_CURVE('',#43090,#40610,#35019,.T.);
#57210=EDGE_CURVE('',#41860,#43096,#35020,.T.);
#57211=EDGE_CURVE('',#43091,#40609,#35021,.T.);
#57212=EDGE_CURVE('',#41858,#43095,#2359,.T.);
#57213=EDGE_CURVE('',#43074,#40608,#35022,.T.);
#57214=EDGE_CURVE('',#41853,#43094,#35023,.T.);
#57215=EDGE_CURVE('',#43075,#40607,#35024,.T.);
#57216=EDGE_CURVE('',#40839,#43093,#35025,.T.);
#57217=EDGE_CURVE('',#43080,#40606,#35026,.T.);
#57218=EDGE_CURVE('',#40840,#43092,#35027,.T.);
#57219=EDGE_CURVE('',#43081,#40605,#35028,.T.);
#57220=EDGE_CURVE('',#40841,#43073,#35029,.T.);
#57221=EDGE_CURVE('',#43082,#41891,#35030,.T.);
#57222=EDGE_CURVE('',#40842,#43076,#35031,.T.);
#57223=EDGE_CURVE('',#43083,#41887,#2360,.T.);
#57224=EDGE_CURVE('',#40843,#43079,#35032,.T.);
#57225=EDGE_CURVE('',#43084,#41886,#35033,.T.);
#57226=EDGE_CURVE('',#40844,#43078,#35034,.T.);
#57227=EDGE_CURVE('',#43085,#41883,#35035,.T.);
#57228=EDGE_CURVE('',#41874,#43077,#35036,.T.);
#57229=EDGE_CURVE('',#43086,#41882,#35037,.T.);
#57230=EDGE_CURVE('',#41875,#43088,#2361,.T.);
#57231=EDGE_CURVE('',#43087,#41879,#35038,.T.);
#57232=EDGE_CURVE('',#43128,#41850,#2362,.T.);
#57233=EDGE_CURVE('',#41845,#43127,#35039,.T.);
#57234=EDGE_CURVE('',#41844,#43126,#35040,.T.);
#57235=EDGE_CURVE('',#43117,#41852,#35041,.T.);
#57236=EDGE_CURVE('',#41841,#43125,#35042,.T.);
#57237=EDGE_CURVE('',#43118,#40616,#35043,.T.);
#57238=EDGE_CURVE('',#41840,#43124,#35044,.T.);
#57239=EDGE_CURVE('',#43119,#40615,#35045,.T.);
#57240=EDGE_CURVE('',#41838,#43123,#2363,.T.);
#57241=EDGE_CURVE('',#43102,#40614,#35046,.T.);
#57242=EDGE_CURVE('',#41833,#43122,#35047,.T.);
#57243=EDGE_CURVE('',#43103,#40613,#35048,.T.);
#57244=EDGE_CURVE('',#40833,#43121,#35049,.T.);
#57245=EDGE_CURVE('',#43108,#40612,#35050,.T.);
#57246=EDGE_CURVE('',#40834,#43120,#35051,.T.);
#57247=EDGE_CURVE('',#43109,#40611,#35052,.T.);
#57248=EDGE_CURVE('',#40835,#43101,#35053,.T.);
#57249=EDGE_CURVE('',#43110,#41871,#35054,.T.);
#57250=EDGE_CURVE('',#40836,#43104,#35055,.T.);
#57251=EDGE_CURVE('',#43111,#41867,#2364,.T.);
#57252=EDGE_CURVE('',#40837,#43107,#35056,.T.);
#57253=EDGE_CURVE('',#43112,#41866,#35057,.T.);
#57254=EDGE_CURVE('',#40838,#43106,#35058,.T.);
#57255=EDGE_CURVE('',#43113,#41863,#35059,.T.);
#57256=EDGE_CURVE('',#41854,#43105,#35060,.T.);
#57257=EDGE_CURVE('',#43114,#41862,#35061,.T.);
#57258=EDGE_CURVE('',#41855,#43116,#2365,.T.);
#57259=EDGE_CURVE('',#43115,#41859,#35062,.T.);
#57260=EDGE_CURVE('',#43156,#41830,#2366,.T.);
#57261=EDGE_CURVE('',#41825,#43155,#35063,.T.);
#57262=EDGE_CURVE('',#41824,#43154,#35064,.T.);
#57263=EDGE_CURVE('',#43145,#41832,#35065,.T.);
#57264=EDGE_CURVE('',#41821,#43153,#35066,.T.);
#57265=EDGE_CURVE('',#43146,#40622,#35067,.T.);
#57266=EDGE_CURVE('',#41820,#43152,#35068,.T.);
#57267=EDGE_CURVE('',#43147,#40621,#35069,.T.);
#57268=EDGE_CURVE('',#41818,#43151,#2367,.T.);
#57269=EDGE_CURVE('',#43130,#40620,#35070,.T.);
#57270=EDGE_CURVE('',#41813,#43150,#35071,.T.);
#57271=EDGE_CURVE('',#43131,#40619,#35072,.T.);
#57272=EDGE_CURVE('',#40827,#43149,#35073,.T.);
#57273=EDGE_CURVE('',#43136,#40618,#35074,.T.);
#57274=EDGE_CURVE('',#40828,#43148,#35075,.T.);
#57275=EDGE_CURVE('',#43137,#40617,#35076,.T.);
#57276=EDGE_CURVE('',#40829,#43129,#35077,.T.);
#57277=EDGE_CURVE('',#43138,#41851,#35078,.T.);
#57278=EDGE_CURVE('',#40830,#43132,#35079,.T.);
#57279=EDGE_CURVE('',#43139,#41847,#2368,.T.);
#57280=EDGE_CURVE('',#40831,#43135,#35080,.T.);
#57281=EDGE_CURVE('',#43140,#41846,#35081,.T.);
#57282=EDGE_CURVE('',#40832,#43134,#35082,.T.);
#57283=EDGE_CURVE('',#43141,#41843,#35083,.T.);
#57284=EDGE_CURVE('',#41834,#43133,#35084,.T.);
#57285=EDGE_CURVE('',#43142,#41842,#35085,.T.);
#57286=EDGE_CURVE('',#41835,#43144,#2369,.T.);
#57287=EDGE_CURVE('',#43143,#41839,#35086,.T.);
#57288=EDGE_CURVE('',#43184,#41810,#2370,.T.);
#57289=EDGE_CURVE('',#41805,#43183,#35087,.T.);
#57290=EDGE_CURVE('',#41804,#43182,#35088,.T.);
#57291=EDGE_CURVE('',#43173,#41812,#35089,.T.);
#57292=EDGE_CURVE('',#41801,#43181,#35090,.T.);
#57293=EDGE_CURVE('',#43174,#40628,#35091,.T.);
#57294=EDGE_CURVE('',#41800,#43180,#35092,.T.);
#57295=EDGE_CURVE('',#43175,#40627,#35093,.T.);
#57296=EDGE_CURVE('',#41798,#43179,#2371,.T.);
#57297=EDGE_CURVE('',#43158,#40626,#35094,.T.);
#57298=EDGE_CURVE('',#41793,#43178,#35095,.T.);
#57299=EDGE_CURVE('',#43159,#40625,#35096,.T.);
#57300=EDGE_CURVE('',#40821,#43177,#35097,.T.);
#57301=EDGE_CURVE('',#43164,#40624,#35098,.T.);
#57302=EDGE_CURVE('',#40822,#43176,#35099,.T.);
#57303=EDGE_CURVE('',#43165,#40623,#35100,.T.);
#57304=EDGE_CURVE('',#40823,#43157,#35101,.T.);
#57305=EDGE_CURVE('',#43166,#41831,#35102,.T.);
#57306=EDGE_CURVE('',#40824,#43160,#35103,.T.);
#57307=EDGE_CURVE('',#43167,#41827,#2372,.T.);
#57308=EDGE_CURVE('',#40825,#43163,#35104,.T.);
#57309=EDGE_CURVE('',#43168,#41826,#35105,.T.);
#57310=EDGE_CURVE('',#40826,#43162,#35106,.T.);
#57311=EDGE_CURVE('',#43169,#41823,#35107,.T.);
#57312=EDGE_CURVE('',#41814,#43161,#35108,.T.);
#57313=EDGE_CURVE('',#43170,#41822,#35109,.T.);
#57314=EDGE_CURVE('',#41815,#43172,#2373,.T.);
#57315=EDGE_CURVE('',#43171,#41819,#35110,.T.);
#57316=EDGE_CURVE('',#43212,#41790,#2374,.T.);
#57317=EDGE_CURVE('',#41785,#43211,#35111,.T.);
#57318=EDGE_CURVE('',#41784,#43210,#35112,.T.);
#57319=EDGE_CURVE('',#43201,#41792,#35113,.T.);
#57320=EDGE_CURVE('',#41781,#43209,#35114,.T.);
#57321=EDGE_CURVE('',#43202,#40634,#35115,.T.);
#57322=EDGE_CURVE('',#41780,#43208,#35116,.T.);
#57323=EDGE_CURVE('',#43203,#40633,#35117,.T.);
#57324=EDGE_CURVE('',#41778,#43207,#2375,.T.);
#57325=EDGE_CURVE('',#43186,#40632,#35118,.T.);
#57326=EDGE_CURVE('',#41773,#43206,#35119,.T.);
#57327=EDGE_CURVE('',#43187,#40631,#35120,.T.);
#57328=EDGE_CURVE('',#40815,#43205,#35121,.T.);
#57329=EDGE_CURVE('',#43192,#40630,#35122,.T.);
#57330=EDGE_CURVE('',#40816,#43204,#35123,.T.);
#57331=EDGE_CURVE('',#43193,#40629,#35124,.T.);
#57332=EDGE_CURVE('',#40817,#43185,#35125,.T.);
#57333=EDGE_CURVE('',#43194,#41811,#35126,.T.);
#57334=EDGE_CURVE('',#40818,#43188,#35127,.T.);
#57335=EDGE_CURVE('',#43195,#41807,#2376,.T.);
#57336=EDGE_CURVE('',#40819,#43191,#35128,.T.);
#57337=EDGE_CURVE('',#43196,#41806,#35129,.T.);
#57338=EDGE_CURVE('',#40820,#43190,#35130,.T.);
#57339=EDGE_CURVE('',#43197,#41803,#35131,.T.);
#57340=EDGE_CURVE('',#41794,#43189,#35132,.T.);
#57341=EDGE_CURVE('',#43198,#41802,#35133,.T.);
#57342=EDGE_CURVE('',#41795,#43200,#2377,.T.);
#57343=EDGE_CURVE('',#43199,#41799,#35134,.T.);
#57344=EDGE_CURVE('',#43236,#41770,#2378,.T.);
#57345=EDGE_CURVE('',#41765,#43235,#35135,.T.);
#57346=EDGE_CURVE('',#41764,#43234,#35136,.T.);
#57347=EDGE_CURVE('',#43225,#41772,#35137,.T.);
#57348=EDGE_CURVE('',#41761,#43233,#35138,.T.);
#57349=EDGE_CURVE('',#43226,#40638,#35139,.T.);
#57350=EDGE_CURVE('',#41760,#43232,#35140,.T.);
#57351=EDGE_CURVE('',#43227,#40637,#35141,.T.);
#57352=EDGE_CURVE('',#41758,#43231,#2379,.T.);
#57353=EDGE_CURVE('',#41753,#43230,#35142,.T.);
#57354=EDGE_CURVE('',#41168,#43229,#35143,.T.);
#57355=EDGE_CURVE('',#43216,#40636,#35144,.T.);
#57356=EDGE_CURVE('',#41169,#43228,#35145,.T.);
#57357=EDGE_CURVE('',#43217,#40635,#35146,.T.);
#57358=EDGE_CURVE('',#43218,#41791,#35147,.T.);
#57359=EDGE_CURVE('',#43219,#41787,#2380,.T.);
#57360=EDGE_CURVE('',#40813,#43215,#35148,.T.);
#57361=EDGE_CURVE('',#43220,#41786,#35149,.T.);
#57362=EDGE_CURVE('',#40814,#43214,#35150,.T.);
#57363=EDGE_CURVE('',#43221,#41783,#35151,.T.);
#57364=EDGE_CURVE('',#41774,#43213,#35152,.T.);
#57365=EDGE_CURVE('',#43222,#41782,#35153,.T.);
#57366=EDGE_CURVE('',#41775,#43224,#2381,.T.);
#57367=EDGE_CURVE('',#43223,#41779,#35154,.T.);
#57368=EDGE_CURVE('',#43264,#41750,#2382,.T.);
#57369=EDGE_CURVE('',#41745,#43263,#35155,.T.);
#57370=EDGE_CURVE('',#41744,#43262,#35156,.T.);
#57371=EDGE_CURVE('',#43253,#41752,#35157,.T.);
#57372=EDGE_CURVE('',#41741,#43261,#35158,.T.);
#57373=EDGE_CURVE('',#43254,#40644,#35159,.T.);
#57374=EDGE_CURVE('',#41740,#43260,#35160,.T.);
#57375=EDGE_CURVE('',#43255,#40643,#35161,.T.);
#57376=EDGE_CURVE('',#41738,#43259,#2383,.T.);
#57377=EDGE_CURVE('',#43238,#40642,#35162,.T.);
#57378=EDGE_CURVE('',#41733,#43258,#35163,.T.);
#57379=EDGE_CURVE('',#43239,#40641,#35164,.T.);
#57380=EDGE_CURVE('',#41162,#43257,#35165,.T.);
#57381=EDGE_CURVE('',#43244,#40640,#35166,.T.);
#57382=EDGE_CURVE('',#41163,#43256,#35167,.T.);
#57383=EDGE_CURVE('',#43245,#40639,#35168,.T.);
#57384=EDGE_CURVE('',#41164,#43237,#35169,.T.);
#57385=EDGE_CURVE('',#43246,#41771,#35170,.T.);
#57386=EDGE_CURVE('',#41165,#43240,#35171,.T.);
#57387=EDGE_CURVE('',#43247,#41767,#2384,.T.);
#57388=EDGE_CURVE('',#41166,#43243,#35172,.T.);
#57389=EDGE_CURVE('',#43248,#41766,#35173,.T.);
#57390=EDGE_CURVE('',#41167,#43242,#35174,.T.);
#57391=EDGE_CURVE('',#43249,#41763,#35175,.T.);
#57392=EDGE_CURVE('',#41754,#43241,#35176,.T.);
#57393=EDGE_CURVE('',#43250,#41762,#35177,.T.);
#57394=EDGE_CURVE('',#41755,#43252,#2385,.T.);
#57395=EDGE_CURVE('',#43251,#41759,#35178,.T.);
#57396=EDGE_CURVE('',#43292,#41730,#2386,.T.);
#57397=EDGE_CURVE('',#41725,#43291,#35179,.T.);
#57398=EDGE_CURVE('',#41724,#43290,#35180,.T.);
#57399=EDGE_CURVE('',#43281,#41732,#35181,.T.);
#57400=EDGE_CURVE('',#41721,#43289,#35182,.T.);
#57401=EDGE_CURVE('',#43282,#40650,#35183,.T.);
#57402=EDGE_CURVE('',#41720,#43288,#35184,.T.);
#57403=EDGE_CURVE('',#43283,#40649,#35185,.T.);
#57404=EDGE_CURVE('',#41718,#43287,#2387,.T.);
#57405=EDGE_CURVE('',#43266,#40648,#35186,.T.);
#57406=EDGE_CURVE('',#41713,#43286,#35187,.T.);
#57407=EDGE_CURVE('',#43267,#40647,#35188,.T.);
#57408=EDGE_CURVE('',#41156,#43285,#35189,.T.);
#57409=EDGE_CURVE('',#43272,#40646,#35190,.T.);
#57410=EDGE_CURVE('',#41157,#43284,#35191,.T.);
#57411=EDGE_CURVE('',#43273,#40645,#35192,.T.);
#57412=EDGE_CURVE('',#41158,#43265,#35193,.T.);
#57413=EDGE_CURVE('',#43274,#41751,#35194,.T.);
#57414=EDGE_CURVE('',#41159,#43268,#35195,.T.);
#57415=EDGE_CURVE('',#43275,#41747,#2388,.T.);
#57416=EDGE_CURVE('',#41160,#43271,#35196,.T.);
#57417=EDGE_CURVE('',#43276,#41746,#35197,.T.);
#57418=EDGE_CURVE('',#41161,#43270,#35198,.T.);
#57419=EDGE_CURVE('',#43277,#41743,#35199,.T.);
#57420=EDGE_CURVE('',#41734,#43269,#35200,.T.);
#57421=EDGE_CURVE('',#43278,#41742,#35201,.T.);
#57422=EDGE_CURVE('',#41735,#43280,#2389,.T.);
#57423=EDGE_CURVE('',#43279,#41739,#35202,.T.);
#57424=EDGE_CURVE('',#43320,#41710,#2390,.T.);
#57425=EDGE_CURVE('',#41705,#43319,#35203,.T.);
#57426=EDGE_CURVE('',#41704,#43318,#35204,.T.);
#57427=EDGE_CURVE('',#43309,#41712,#35205,.T.);
#57428=EDGE_CURVE('',#41701,#43317,#35206,.T.);
#57429=EDGE_CURVE('',#43310,#40656,#35207,.T.);
#57430=EDGE_CURVE('',#41700,#43316,#35208,.T.);
#57431=EDGE_CURVE('',#43311,#40655,#35209,.T.);
#57432=EDGE_CURVE('',#41698,#43315,#2391,.T.);
#57433=EDGE_CURVE('',#43294,#40654,#35210,.T.);
#57434=EDGE_CURVE('',#41693,#43314,#35211,.T.);
#57435=EDGE_CURVE('',#43295,#40653,#35212,.T.);
#57436=EDGE_CURVE('',#41150,#43313,#35213,.T.);
#57437=EDGE_CURVE('',#43300,#40652,#35214,.T.);
#57438=EDGE_CURVE('',#41151,#43312,#35215,.T.);
#57439=EDGE_CURVE('',#43301,#40651,#35216,.T.);
#57440=EDGE_CURVE('',#41152,#43293,#35217,.T.);
#57441=EDGE_CURVE('',#43302,#41731,#35218,.T.);
#57442=EDGE_CURVE('',#41153,#43296,#35219,.T.);
#57443=EDGE_CURVE('',#43303,#41727,#2392,.T.);
#57444=EDGE_CURVE('',#41154,#43299,#35220,.T.);
#57445=EDGE_CURVE('',#43304,#41726,#35221,.T.);
#57446=EDGE_CURVE('',#41155,#43298,#35222,.T.);
#57447=EDGE_CURVE('',#43305,#41723,#35223,.T.);
#57448=EDGE_CURVE('',#41714,#43297,#35224,.T.);
#57449=EDGE_CURVE('',#43306,#41722,#35225,.T.);
#57450=EDGE_CURVE('',#41715,#43308,#2393,.T.);
#57451=EDGE_CURVE('',#43307,#41719,#35226,.T.);
#57452=EDGE_CURVE('',#43348,#41690,#2394,.T.);
#57453=EDGE_CURVE('',#41685,#43347,#35227,.T.);
#57454=EDGE_CURVE('',#41684,#43346,#35228,.T.);
#57455=EDGE_CURVE('',#43337,#41692,#35229,.T.);
#57456=EDGE_CURVE('',#41681,#43345,#35230,.T.);
#57457=EDGE_CURVE('',#43338,#40662,#35231,.T.);
#57458=EDGE_CURVE('',#41680,#43344,#35232,.T.);
#57459=EDGE_CURVE('',#43339,#40661,#35233,.T.);
#57460=EDGE_CURVE('',#41678,#43343,#2395,.T.);
#57461=EDGE_CURVE('',#43322,#40660,#35234,.T.);
#57462=EDGE_CURVE('',#41673,#43342,#35235,.T.);
#57463=EDGE_CURVE('',#43323,#40659,#35236,.T.);
#57464=EDGE_CURVE('',#41144,#43341,#35237,.T.);
#57465=EDGE_CURVE('',#43328,#40658,#35238,.T.);
#57466=EDGE_CURVE('',#41145,#43340,#35239,.T.);
#57467=EDGE_CURVE('',#43329,#40657,#35240,.T.);
#57468=EDGE_CURVE('',#41146,#43321,#35241,.T.);
#57469=EDGE_CURVE('',#43330,#41711,#35242,.T.);
#57470=EDGE_CURVE('',#41147,#43324,#35243,.T.);
#57471=EDGE_CURVE('',#43331,#41707,#2396,.T.);
#57472=EDGE_CURVE('',#41148,#43327,#35244,.T.);
#57473=EDGE_CURVE('',#43332,#41706,#35245,.T.);
#57474=EDGE_CURVE('',#41149,#43326,#35246,.T.);
#57475=EDGE_CURVE('',#43333,#41703,#35247,.T.);
#57476=EDGE_CURVE('',#41694,#43325,#35248,.T.);
#57477=EDGE_CURVE('',#43334,#41702,#35249,.T.);
#57478=EDGE_CURVE('',#41695,#43336,#2397,.T.);
#57479=EDGE_CURVE('',#43335,#41699,#35250,.T.);
#57480=EDGE_CURVE('',#43376,#41670,#2398,.T.);
#57481=EDGE_CURVE('',#41665,#43375,#35251,.T.);
#57482=EDGE_CURVE('',#41664,#43374,#35252,.T.);
#57483=EDGE_CURVE('',#43365,#41672,#35253,.T.);
#57484=EDGE_CURVE('',#41661,#43373,#35254,.T.);
#57485=EDGE_CURVE('',#43366,#40668,#35255,.T.);
#57486=EDGE_CURVE('',#41660,#43372,#35256,.T.);
#57487=EDGE_CURVE('',#43367,#40667,#35257,.T.);
#57488=EDGE_CURVE('',#41658,#43371,#2399,.T.);
#57489=EDGE_CURVE('',#43350,#40666,#35258,.T.);
#57490=EDGE_CURVE('',#41653,#43370,#35259,.T.);
#57491=EDGE_CURVE('',#43351,#40665,#35260,.T.);
#57492=EDGE_CURVE('',#41138,#43369,#35261,.T.);
#57493=EDGE_CURVE('',#43356,#40664,#35262,.T.);
#57494=EDGE_CURVE('',#41139,#43368,#35263,.T.);
#57495=EDGE_CURVE('',#43357,#40663,#35264,.T.);
#57496=EDGE_CURVE('',#41140,#43349,#35265,.T.);
#57497=EDGE_CURVE('',#43358,#41691,#35266,.T.);
#57498=EDGE_CURVE('',#41141,#43352,#35267,.T.);
#57499=EDGE_CURVE('',#43359,#41687,#2400,.T.);
#57500=EDGE_CURVE('',#41142,#43355,#35268,.T.);
#57501=EDGE_CURVE('',#43360,#41686,#35269,.T.);
#57502=EDGE_CURVE('',#41143,#43354,#35270,.T.);
#57503=EDGE_CURVE('',#43361,#41683,#35271,.T.);
#57504=EDGE_CURVE('',#41674,#43353,#35272,.T.);
#57505=EDGE_CURVE('',#43362,#41682,#35273,.T.);
#57506=EDGE_CURVE('',#41675,#43364,#2401,.T.);
#57507=EDGE_CURVE('',#43363,#41679,#35274,.T.);
#57508=EDGE_CURVE('',#43404,#41650,#2402,.T.);
#57509=EDGE_CURVE('',#41645,#43403,#35275,.T.);
#57510=EDGE_CURVE('',#41644,#43402,#35276,.T.);
#57511=EDGE_CURVE('',#43393,#41652,#35277,.T.);
#57512=EDGE_CURVE('',#41641,#43401,#35278,.T.);
#57513=EDGE_CURVE('',#43394,#40674,#35279,.T.);
#57514=EDGE_CURVE('',#41640,#43400,#35280,.T.);
#57515=EDGE_CURVE('',#43395,#40673,#35281,.T.);
#57516=EDGE_CURVE('',#41638,#43399,#2403,.T.);
#57517=EDGE_CURVE('',#43378,#40672,#35282,.T.);
#57518=EDGE_CURVE('',#41633,#43398,#35283,.T.);
#57519=EDGE_CURVE('',#43379,#40671,#35284,.T.);
#57520=EDGE_CURVE('',#41132,#43397,#35285,.T.);
#57521=EDGE_CURVE('',#43384,#40670,#35286,.T.);
#57522=EDGE_CURVE('',#41133,#43396,#35287,.T.);
#57523=EDGE_CURVE('',#43385,#40669,#35288,.T.);
#57524=EDGE_CURVE('',#41134,#43377,#35289,.T.);
#57525=EDGE_CURVE('',#43386,#41671,#35290,.T.);
#57526=EDGE_CURVE('',#41135,#43380,#35291,.T.);
#57527=EDGE_CURVE('',#43387,#41667,#2404,.T.);
#57528=EDGE_CURVE('',#41136,#43383,#35292,.T.);
#57529=EDGE_CURVE('',#43388,#41666,#35293,.T.);
#57530=EDGE_CURVE('',#41137,#43382,#35294,.T.);
#57531=EDGE_CURVE('',#43389,#41663,#35295,.T.);
#57532=EDGE_CURVE('',#41654,#43381,#35296,.T.);
#57533=EDGE_CURVE('',#43390,#41662,#35297,.T.);
#57534=EDGE_CURVE('',#41655,#43392,#2405,.T.);
#57535=EDGE_CURVE('',#43391,#41659,#35298,.T.);
#57536=EDGE_CURVE('',#43432,#41630,#2406,.T.);
#57537=EDGE_CURVE('',#41625,#43431,#35299,.T.);
#57538=EDGE_CURVE('',#41624,#43430,#35300,.T.);
#57539=EDGE_CURVE('',#43421,#41632,#35301,.T.);
#57540=EDGE_CURVE('',#41621,#43429,#35302,.T.);
#57541=EDGE_CURVE('',#43422,#40680,#35303,.T.);
#57542=EDGE_CURVE('',#41620,#43428,#35304,.T.);
#57543=EDGE_CURVE('',#43423,#40679,#35305,.T.);
#57544=EDGE_CURVE('',#41618,#43427,#2407,.T.);
#57545=EDGE_CURVE('',#43406,#40678,#35306,.T.);
#57546=EDGE_CURVE('',#41613,#43426,#35307,.T.);
#57547=EDGE_CURVE('',#43407,#40677,#35308,.T.);
#57548=EDGE_CURVE('',#41126,#43425,#35309,.T.);
#57549=EDGE_CURVE('',#43412,#40676,#35310,.T.);
#57550=EDGE_CURVE('',#41127,#43424,#35311,.T.);
#57551=EDGE_CURVE('',#43413,#40675,#35312,.T.);
#57552=EDGE_CURVE('',#41128,#43405,#35313,.T.);
#57553=EDGE_CURVE('',#43414,#41651,#35314,.T.);
#57554=EDGE_CURVE('',#41129,#43408,#35315,.T.);
#57555=EDGE_CURVE('',#43415,#41647,#2408,.T.);
#57556=EDGE_CURVE('',#41130,#43411,#35316,.T.);
#57557=EDGE_CURVE('',#43416,#41646,#35317,.T.);
#57558=EDGE_CURVE('',#41131,#43410,#35318,.T.);
#57559=EDGE_CURVE('',#43417,#41643,#35319,.T.);
#57560=EDGE_CURVE('',#41634,#43409,#35320,.T.);
#57561=EDGE_CURVE('',#43418,#41642,#35321,.T.);
#57562=EDGE_CURVE('',#41635,#43420,#2409,.T.);
#57563=EDGE_CURVE('',#43419,#41639,#35322,.T.);
#57564=EDGE_CURVE('',#43460,#41610,#2410,.T.);
#57565=EDGE_CURVE('',#41605,#43459,#35323,.T.);
#57566=EDGE_CURVE('',#41604,#43458,#35324,.T.);
#57567=EDGE_CURVE('',#43449,#41612,#35325,.T.);
#57568=EDGE_CURVE('',#41601,#43457,#35326,.T.);
#57569=EDGE_CURVE('',#43450,#40686,#35327,.T.);
#57570=EDGE_CURVE('',#41600,#43456,#35328,.T.);
#57571=EDGE_CURVE('',#43451,#40685,#35329,.T.);
#57572=EDGE_CURVE('',#41598,#43455,#2411,.T.);
#57573=EDGE_CURVE('',#43434,#40684,#35330,.T.);
#57574=EDGE_CURVE('',#41593,#43454,#35331,.T.);
#57575=EDGE_CURVE('',#43435,#40683,#35332,.T.);
#57576=EDGE_CURVE('',#41120,#43453,#35333,.T.);
#57577=EDGE_CURVE('',#43440,#40682,#35334,.T.);
#57578=EDGE_CURVE('',#41121,#43452,#35335,.T.);
#57579=EDGE_CURVE('',#43441,#40681,#35336,.T.);
#57580=EDGE_CURVE('',#41122,#43433,#35337,.T.);
#57581=EDGE_CURVE('',#43442,#41631,#35338,.T.);
#57582=EDGE_CURVE('',#41123,#43436,#35339,.T.);
#57583=EDGE_CURVE('',#43443,#41627,#2412,.T.);
#57584=EDGE_CURVE('',#41124,#43439,#35340,.T.);
#57585=EDGE_CURVE('',#43444,#41626,#35341,.T.);
#57586=EDGE_CURVE('',#41125,#43438,#35342,.T.);
#57587=EDGE_CURVE('',#43445,#41623,#35343,.T.);
#57588=EDGE_CURVE('',#41614,#43437,#35344,.T.);
#57589=EDGE_CURVE('',#43446,#41622,#35345,.T.);
#57590=EDGE_CURVE('',#41615,#43448,#2413,.T.);
#57591=EDGE_CURVE('',#43447,#41619,#35346,.T.);
#57592=EDGE_CURVE('',#43488,#41590,#2414,.T.);
#57593=EDGE_CURVE('',#41585,#43487,#35347,.T.);
#57594=EDGE_CURVE('',#41584,#43486,#35348,.T.);
#57595=EDGE_CURVE('',#43477,#41592,#35349,.T.);
#57596=EDGE_CURVE('',#41581,#43485,#35350,.T.);
#57597=EDGE_CURVE('',#43478,#40692,#35351,.T.);
#57598=EDGE_CURVE('',#41580,#43484,#35352,.T.);
#57599=EDGE_CURVE('',#43479,#40691,#35353,.T.);
#57600=EDGE_CURVE('',#41578,#43483,#2415,.T.);
#57601=EDGE_CURVE('',#43462,#40690,#35354,.T.);
#57602=EDGE_CURVE('',#41573,#43482,#35355,.T.);
#57603=EDGE_CURVE('',#43463,#40689,#35356,.T.);
#57604=EDGE_CURVE('',#41114,#43481,#35357,.T.);
#57605=EDGE_CURVE('',#43468,#40688,#35358,.T.);
#57606=EDGE_CURVE('',#41115,#43480,#35359,.T.);
#57607=EDGE_CURVE('',#43469,#40687,#35360,.T.);
#57608=EDGE_CURVE('',#41116,#43461,#35361,.T.);
#57609=EDGE_CURVE('',#43470,#41611,#35362,.T.);
#57610=EDGE_CURVE('',#41117,#43464,#35363,.T.);
#57611=EDGE_CURVE('',#43471,#41607,#2416,.T.);
#57612=EDGE_CURVE('',#41118,#43467,#35364,.T.);
#57613=EDGE_CURVE('',#43472,#41606,#35365,.T.);
#57614=EDGE_CURVE('',#41119,#43466,#35366,.T.);
#57615=EDGE_CURVE('',#43473,#41603,#35367,.T.);
#57616=EDGE_CURVE('',#41594,#43465,#35368,.T.);
#57617=EDGE_CURVE('',#43474,#41602,#35369,.T.);
#57618=EDGE_CURVE('',#41595,#43476,#2417,.T.);
#57619=EDGE_CURVE('',#43475,#41599,#35370,.T.);
#57620=EDGE_CURVE('',#43516,#41570,#2418,.T.);
#57621=EDGE_CURVE('',#41565,#43515,#35371,.T.);
#57622=EDGE_CURVE('',#41564,#43514,#35372,.T.);
#57623=EDGE_CURVE('',#43505,#41572,#35373,.T.);
#57624=EDGE_CURVE('',#41561,#43513,#35374,.T.);
#57625=EDGE_CURVE('',#43506,#40698,#35375,.T.);
#57626=EDGE_CURVE('',#41560,#43512,#35376,.T.);
#57627=EDGE_CURVE('',#43507,#40697,#35377,.T.);
#57628=EDGE_CURVE('',#41558,#43511,#2419,.T.);
#57629=EDGE_CURVE('',#43490,#40696,#35378,.T.);
#57630=EDGE_CURVE('',#41553,#43510,#35379,.T.);
#57631=EDGE_CURVE('',#43491,#40695,#35380,.T.);
#57632=EDGE_CURVE('',#41108,#43509,#35381,.T.);
#57633=EDGE_CURVE('',#43496,#40694,#35382,.T.);
#57634=EDGE_CURVE('',#41109,#43508,#35383,.T.);
#57635=EDGE_CURVE('',#43497,#40693,#35384,.T.);
#57636=EDGE_CURVE('',#41110,#43489,#35385,.T.);
#57637=EDGE_CURVE('',#43498,#41591,#35386,.T.);
#57638=EDGE_CURVE('',#41111,#43492,#35387,.T.);
#57639=EDGE_CURVE('',#43499,#41587,#2420,.T.);
#57640=EDGE_CURVE('',#41112,#43495,#35388,.T.);
#57641=EDGE_CURVE('',#43500,#41586,#35389,.T.);
#57642=EDGE_CURVE('',#41113,#43494,#35390,.T.);
#57643=EDGE_CURVE('',#43501,#41583,#35391,.T.);
#57644=EDGE_CURVE('',#41574,#43493,#35392,.T.);
#57645=EDGE_CURVE('',#43502,#41582,#35393,.T.);
#57646=EDGE_CURVE('',#41575,#43504,#2421,.T.);
#57647=EDGE_CURVE('',#43503,#41579,#35394,.T.);
#57648=EDGE_CURVE('',#43544,#41550,#2422,.T.);
#57649=EDGE_CURVE('',#41545,#43543,#35395,.T.);
#57650=EDGE_CURVE('',#41544,#43542,#35396,.T.);
#57651=EDGE_CURVE('',#43533,#41552,#35397,.T.);
#57652=EDGE_CURVE('',#41541,#43541,#35398,.T.);
#57653=EDGE_CURVE('',#43534,#40704,#35399,.T.);
#57654=EDGE_CURVE('',#41540,#43540,#35400,.T.);
#57655=EDGE_CURVE('',#43535,#40703,#35401,.T.);
#57656=EDGE_CURVE('',#41538,#43539,#2423,.T.);
#57657=EDGE_CURVE('',#43518,#40702,#35402,.T.);
#57658=EDGE_CURVE('',#41533,#43538,#35403,.T.);
#57659=EDGE_CURVE('',#43519,#40701,#35404,.T.);
#57660=EDGE_CURVE('',#41102,#43537,#35405,.T.);
#57661=EDGE_CURVE('',#43524,#40700,#35406,.T.);
#57662=EDGE_CURVE('',#41103,#43536,#35407,.T.);
#57663=EDGE_CURVE('',#43525,#40699,#35408,.T.);
#57664=EDGE_CURVE('',#41104,#43517,#35409,.T.);
#57665=EDGE_CURVE('',#43526,#41571,#35410,.T.);
#57666=EDGE_CURVE('',#41105,#43520,#35411,.T.);
#57667=EDGE_CURVE('',#43527,#41567,#2424,.T.);
#57668=EDGE_CURVE('',#41106,#43523,#35412,.T.);
#57669=EDGE_CURVE('',#43528,#41566,#35413,.T.);
#57670=EDGE_CURVE('',#41107,#43522,#35414,.T.);
#57671=EDGE_CURVE('',#43529,#41563,#35415,.T.);
#57672=EDGE_CURVE('',#41554,#43521,#35416,.T.);
#57673=EDGE_CURVE('',#43530,#41562,#35417,.T.);
#57674=EDGE_CURVE('',#41555,#43532,#2425,.T.);
#57675=EDGE_CURVE('',#43531,#41559,#35418,.T.);
#57676=EDGE_CURVE('',#43572,#41530,#2426,.T.);
#57677=EDGE_CURVE('',#41525,#43571,#35419,.T.);
#57678=EDGE_CURVE('',#41524,#43570,#35420,.T.);
#57679=EDGE_CURVE('',#43561,#41532,#35421,.T.);
#57680=EDGE_CURVE('',#41521,#43569,#35422,.T.);
#57681=EDGE_CURVE('',#43562,#40710,#35423,.T.);
#57682=EDGE_CURVE('',#41520,#43568,#35424,.T.);
#57683=EDGE_CURVE('',#43563,#40709,#35425,.T.);
#57684=EDGE_CURVE('',#41518,#43567,#2427,.T.);
#57685=EDGE_CURVE('',#43546,#40708,#35426,.T.);
#57686=EDGE_CURVE('',#41513,#43566,#35427,.T.);
#57687=EDGE_CURVE('',#43547,#40707,#35428,.T.);
#57688=EDGE_CURVE('',#41096,#43565,#35429,.T.);
#57689=EDGE_CURVE('',#43552,#40706,#35430,.T.);
#57690=EDGE_CURVE('',#41097,#43564,#35431,.T.);
#57691=EDGE_CURVE('',#43553,#40705,#35432,.T.);
#57692=EDGE_CURVE('',#41098,#43545,#35433,.T.);
#57693=EDGE_CURVE('',#43554,#41551,#35434,.T.);
#57694=EDGE_CURVE('',#41099,#43548,#35435,.T.);
#57695=EDGE_CURVE('',#43555,#41547,#2428,.T.);
#57696=EDGE_CURVE('',#41100,#43551,#35436,.T.);
#57697=EDGE_CURVE('',#43556,#41546,#35437,.T.);
#57698=EDGE_CURVE('',#41101,#43550,#35438,.T.);
#57699=EDGE_CURVE('',#43557,#41543,#35439,.T.);
#57700=EDGE_CURVE('',#41534,#43549,#35440,.T.);
#57701=EDGE_CURVE('',#43558,#41542,#35441,.T.);
#57702=EDGE_CURVE('',#41535,#43560,#2429,.T.);
#57703=EDGE_CURVE('',#43559,#41539,#35442,.T.);
#57704=EDGE_CURVE('',#43600,#41510,#2430,.T.);
#57705=EDGE_CURVE('',#41505,#43599,#35443,.T.);
#57706=EDGE_CURVE('',#41504,#43598,#35444,.T.);
#57707=EDGE_CURVE('',#43589,#41512,#35445,.T.);
#57708=EDGE_CURVE('',#41501,#43597,#35446,.T.);
#57709=EDGE_CURVE('',#43590,#40716,#35447,.T.);
#57710=EDGE_CURVE('',#41500,#43596,#35448,.T.);
#57711=EDGE_CURVE('',#43591,#40715,#35449,.T.);
#57712=EDGE_CURVE('',#41498,#43595,#2431,.T.);
#57713=EDGE_CURVE('',#43574,#40714,#35450,.T.);
#57714=EDGE_CURVE('',#41493,#43594,#35451,.T.);
#57715=EDGE_CURVE('',#43575,#40713,#35452,.T.);
#57716=EDGE_CURVE('',#41090,#43593,#35453,.T.);
#57717=EDGE_CURVE('',#43580,#40712,#35454,.T.);
#57718=EDGE_CURVE('',#41091,#43592,#35455,.T.);
#57719=EDGE_CURVE('',#43581,#40711,#35456,.T.);
#57720=EDGE_CURVE('',#41092,#43573,#35457,.T.);
#57721=EDGE_CURVE('',#43582,#41531,#35458,.T.);
#57722=EDGE_CURVE('',#41093,#43576,#35459,.T.);
#57723=EDGE_CURVE('',#43583,#41527,#2432,.T.);
#57724=EDGE_CURVE('',#41094,#43579,#35460,.T.);
#57725=EDGE_CURVE('',#43584,#41526,#35461,.T.);
#57726=EDGE_CURVE('',#41095,#43578,#35462,.T.);
#57727=EDGE_CURVE('',#43585,#41523,#35463,.T.);
#57728=EDGE_CURVE('',#41514,#43577,#35464,.T.);
#57729=EDGE_CURVE('',#43586,#41522,#35465,.T.);
#57730=EDGE_CURVE('',#41515,#43588,#2433,.T.);
#57731=EDGE_CURVE('',#43587,#41519,#35466,.T.);
#57732=EDGE_CURVE('',#43628,#41490,#2434,.T.);
#57733=EDGE_CURVE('',#41485,#43627,#35467,.T.);
#57734=EDGE_CURVE('',#41484,#43626,#35468,.T.);
#57735=EDGE_CURVE('',#43617,#41492,#35469,.T.);
#57736=EDGE_CURVE('',#41481,#43625,#35470,.T.);
#57737=EDGE_CURVE('',#43618,#40722,#35471,.T.);
#57738=EDGE_CURVE('',#41480,#43624,#35472,.T.);
#57739=EDGE_CURVE('',#43619,#40721,#35473,.T.);
#57740=EDGE_CURVE('',#41478,#43623,#2435,.T.);
#57741=EDGE_CURVE('',#43602,#40720,#35474,.T.);
#57742=EDGE_CURVE('',#41473,#43622,#35475,.T.);
#57743=EDGE_CURVE('',#43603,#40719,#35476,.T.);
#57744=EDGE_CURVE('',#41084,#43621,#35477,.T.);
#57745=EDGE_CURVE('',#43608,#40718,#35478,.T.);
#57746=EDGE_CURVE('',#41085,#43620,#35479,.T.);
#57747=EDGE_CURVE('',#43609,#40717,#35480,.T.);
#57748=EDGE_CURVE('',#41086,#43601,#35481,.T.);
#57749=EDGE_CURVE('',#43610,#41511,#35482,.T.);
#57750=EDGE_CURVE('',#41087,#43604,#35483,.T.);
#57751=EDGE_CURVE('',#43611,#41507,#2436,.T.);
#57752=EDGE_CURVE('',#41088,#43607,#35484,.T.);
#57753=EDGE_CURVE('',#43612,#41506,#35485,.T.);
#57754=EDGE_CURVE('',#41089,#43606,#35486,.T.);
#57755=EDGE_CURVE('',#43613,#41503,#35487,.T.);
#57756=EDGE_CURVE('',#41494,#43605,#35488,.T.);
#57757=EDGE_CURVE('',#43614,#41502,#35489,.T.);
#57758=EDGE_CURVE('',#41495,#43616,#2437,.T.);
#57759=EDGE_CURVE('',#43615,#41499,#35490,.T.);
#57760=EDGE_CURVE('',#43652,#41470,#2438,.T.);
#57761=EDGE_CURVE('',#41465,#43651,#35491,.T.);
#57762=EDGE_CURVE('',#41464,#43650,#35492,.T.);
#57763=EDGE_CURVE('',#43641,#41472,#35493,.T.);
#57764=EDGE_CURVE('',#41461,#43649,#35494,.T.);
#57765=EDGE_CURVE('',#43642,#40726,#35495,.T.);
#57766=EDGE_CURVE('',#41460,#43648,#35496,.T.);
#57767=EDGE_CURVE('',#43643,#40725,#35497,.T.);
#57768=EDGE_CURVE('',#41458,#43647,#2439,.T.);
#57769=EDGE_CURVE('',#41453,#43646,#35498,.T.);
#57770=EDGE_CURVE('',#41080,#43645,#35499,.T.);
#57771=EDGE_CURVE('',#43632,#40724,#35500,.T.);
#57772=EDGE_CURVE('',#41081,#43644,#35501,.T.);
#57773=EDGE_CURVE('',#43633,#40723,#35502,.T.);
#57774=EDGE_CURVE('',#43634,#41491,#35503,.T.);
#57775=EDGE_CURVE('',#43635,#41487,#2440,.T.);
#57776=EDGE_CURVE('',#41082,#43631,#35504,.T.);
#57777=EDGE_CURVE('',#43636,#41486,#35505,.T.);
#57778=EDGE_CURVE('',#41083,#43630,#35506,.T.);
#57779=EDGE_CURVE('',#43637,#41483,#35507,.T.);
#57780=EDGE_CURVE('',#41474,#43629,#35508,.T.);
#57781=EDGE_CURVE('',#43638,#41482,#35509,.T.);
#57782=EDGE_CURVE('',#41475,#43640,#2441,.T.);
#57783=EDGE_CURVE('',#43639,#41479,#35510,.T.);
#57784=EDGE_CURVE('',#43680,#41450,#2442,.T.);
#57785=EDGE_CURVE('',#41445,#43679,#35511,.T.);
#57786=EDGE_CURVE('',#41444,#43678,#35512,.T.);
#57787=EDGE_CURVE('',#43669,#41452,#35513,.T.);
#57788=EDGE_CURVE('',#41441,#43677,#35514,.T.);
#57789=EDGE_CURVE('',#43670,#40732,#35515,.T.);
#57790=EDGE_CURVE('',#41440,#43676,#35516,.T.);
#57791=EDGE_CURVE('',#43671,#40731,#35517,.T.);
#57792=EDGE_CURVE('',#41438,#43675,#2443,.T.);
#57793=EDGE_CURVE('',#43654,#40730,#35518,.T.);
#57794=EDGE_CURVE('',#41433,#43674,#35519,.T.);
#57795=EDGE_CURVE('',#43655,#40729,#35520,.T.);
#57796=EDGE_CURVE('',#41074,#43673,#35521,.T.);
#57797=EDGE_CURVE('',#43660,#40728,#35522,.T.);
#57798=EDGE_CURVE('',#41075,#43672,#35523,.T.);
#57799=EDGE_CURVE('',#43661,#40727,#35524,.T.);
#57800=EDGE_CURVE('',#41076,#43653,#35525,.T.);
#57801=EDGE_CURVE('',#43662,#41471,#35526,.T.);
#57802=EDGE_CURVE('',#41077,#43656,#35527,.T.);
#57803=EDGE_CURVE('',#43663,#41467,#2444,.T.);
#57804=EDGE_CURVE('',#41078,#43659,#35528,.T.);
#57805=EDGE_CURVE('',#43664,#41466,#35529,.T.);
#57806=EDGE_CURVE('',#41079,#43658,#35530,.T.);
#57807=EDGE_CURVE('',#43665,#41463,#35531,.T.);
#57808=EDGE_CURVE('',#41454,#43657,#35532,.T.);
#57809=EDGE_CURVE('',#43666,#41462,#35533,.T.);
#57810=EDGE_CURVE('',#41455,#43668,#2445,.T.);
#57811=EDGE_CURVE('',#43667,#41459,#35534,.T.);
#57812=EDGE_CURVE('',#43708,#41430,#2446,.T.);
#57813=EDGE_CURVE('',#41425,#43707,#35535,.T.);
#57814=EDGE_CURVE('',#41424,#43706,#35536,.T.);
#57815=EDGE_CURVE('',#43697,#41432,#35537,.T.);
#57816=EDGE_CURVE('',#41421,#43705,#35538,.T.);
#57817=EDGE_CURVE('',#43698,#40738,#35539,.T.);
#57818=EDGE_CURVE('',#41420,#43704,#35540,.T.);
#57819=EDGE_CURVE('',#43699,#40737,#35541,.T.);
#57820=EDGE_CURVE('',#41418,#43703,#2447,.T.);
#57821=EDGE_CURVE('',#43682,#40736,#35542,.T.);
#57822=EDGE_CURVE('',#41413,#43702,#35543,.T.);
#57823=EDGE_CURVE('',#43683,#40735,#35544,.T.);
#57824=EDGE_CURVE('',#41068,#43701,#35545,.T.);
#57825=EDGE_CURVE('',#43688,#40734,#35546,.T.);
#57826=EDGE_CURVE('',#41069,#43700,#35547,.T.);
#57827=EDGE_CURVE('',#43689,#40733,#35548,.T.);
#57828=EDGE_CURVE('',#41070,#43681,#35549,.T.);
#57829=EDGE_CURVE('',#43690,#41451,#35550,.T.);
#57830=EDGE_CURVE('',#41071,#43684,#35551,.T.);
#57831=EDGE_CURVE('',#43691,#41447,#2448,.T.);
#57832=EDGE_CURVE('',#41072,#43687,#35552,.T.);
#57833=EDGE_CURVE('',#43692,#41446,#35553,.T.);
#57834=EDGE_CURVE('',#41073,#43686,#35554,.T.);
#57835=EDGE_CURVE('',#43693,#41443,#35555,.T.);
#57836=EDGE_CURVE('',#41434,#43685,#35556,.T.);
#57837=EDGE_CURVE('',#43694,#41442,#35557,.T.);
#57838=EDGE_CURVE('',#41435,#43696,#2449,.T.);
#57839=EDGE_CURVE('',#43695,#41439,#35558,.T.);
#57840=EDGE_CURVE('',#43736,#41410,#2450,.T.);
#57841=EDGE_CURVE('',#41405,#43735,#35559,.T.);
#57842=EDGE_CURVE('',#41404,#43734,#35560,.T.);
#57843=EDGE_CURVE('',#43725,#41412,#35561,.T.);
#57844=EDGE_CURVE('',#41401,#43733,#35562,.T.);
#57845=EDGE_CURVE('',#43726,#40744,#35563,.T.);
#57846=EDGE_CURVE('',#41400,#43732,#35564,.T.);
#57847=EDGE_CURVE('',#43727,#40743,#35565,.T.);
#57848=EDGE_CURVE('',#41398,#43731,#2451,.T.);
#57849=EDGE_CURVE('',#43710,#40742,#35566,.T.);
#57850=EDGE_CURVE('',#41393,#43730,#35567,.T.);
#57851=EDGE_CURVE('',#43711,#40741,#35568,.T.);
#57852=EDGE_CURVE('',#41062,#43729,#35569,.T.);
#57853=EDGE_CURVE('',#43716,#40740,#35570,.T.);
#57854=EDGE_CURVE('',#41063,#43728,#35571,.T.);
#57855=EDGE_CURVE('',#43717,#40739,#35572,.T.);
#57856=EDGE_CURVE('',#41064,#43709,#35573,.T.);
#57857=EDGE_CURVE('',#43718,#41431,#35574,.T.);
#57858=EDGE_CURVE('',#41065,#43712,#35575,.T.);
#57859=EDGE_CURVE('',#43719,#41427,#2452,.T.);
#57860=EDGE_CURVE('',#41066,#43715,#35576,.T.);
#57861=EDGE_CURVE('',#43720,#41426,#35577,.T.);
#57862=EDGE_CURVE('',#41067,#43714,#35578,.T.);
#57863=EDGE_CURVE('',#43721,#41423,#35579,.T.);
#57864=EDGE_CURVE('',#41414,#43713,#35580,.T.);
#57865=EDGE_CURVE('',#43722,#41422,#35581,.T.);
#57866=EDGE_CURVE('',#41415,#43724,#2453,.T.);
#57867=EDGE_CURVE('',#43723,#41419,#35582,.T.);
#57868=EDGE_CURVE('',#43764,#41390,#2454,.T.);
#57869=EDGE_CURVE('',#41385,#43763,#35583,.T.);
#57870=EDGE_CURVE('',#41384,#43762,#35584,.T.);
#57871=EDGE_CURVE('',#43753,#41392,#35585,.T.);
#57872=EDGE_CURVE('',#41381,#43761,#35586,.T.);
#57873=EDGE_CURVE('',#43754,#40750,#35587,.T.);
#57874=EDGE_CURVE('',#41380,#43760,#35588,.T.);
#57875=EDGE_CURVE('',#43755,#40749,#35589,.T.);
#57876=EDGE_CURVE('',#41378,#43759,#2455,.T.);
#57877=EDGE_CURVE('',#43738,#40748,#35590,.T.);
#57878=EDGE_CURVE('',#41373,#43758,#35591,.T.);
#57879=EDGE_CURVE('',#43739,#40747,#35592,.T.);
#57880=EDGE_CURVE('',#41056,#43757,#35593,.T.);
#57881=EDGE_CURVE('',#43744,#40746,#35594,.T.);
#57882=EDGE_CURVE('',#41057,#43756,#35595,.T.);
#57883=EDGE_CURVE('',#43745,#40745,#35596,.T.);
#57884=EDGE_CURVE('',#41058,#43737,#35597,.T.);
#57885=EDGE_CURVE('',#43746,#41411,#35598,.T.);
#57886=EDGE_CURVE('',#41059,#43740,#35599,.T.);
#57887=EDGE_CURVE('',#43747,#41407,#2456,.T.);
#57888=EDGE_CURVE('',#41060,#43743,#35600,.T.);
#57889=EDGE_CURVE('',#43748,#41406,#35601,.T.);
#57890=EDGE_CURVE('',#41061,#43742,#35602,.T.);
#57891=EDGE_CURVE('',#43749,#41403,#35603,.T.);
#57892=EDGE_CURVE('',#41394,#43741,#35604,.T.);
#57893=EDGE_CURVE('',#43750,#41402,#35605,.T.);
#57894=EDGE_CURVE('',#41395,#43752,#2457,.T.);
#57895=EDGE_CURVE('',#43751,#41399,#35606,.T.);
#57896=EDGE_CURVE('',#43792,#41370,#2458,.T.);
#57897=EDGE_CURVE('',#41365,#43791,#35607,.T.);
#57898=EDGE_CURVE('',#41364,#43790,#35608,.T.);
#57899=EDGE_CURVE('',#43781,#41372,#35609,.T.);
#57900=EDGE_CURVE('',#41361,#43789,#35610,.T.);
#57901=EDGE_CURVE('',#43782,#40756,#35611,.T.);
#57902=EDGE_CURVE('',#41360,#43788,#35612,.T.);
#57903=EDGE_CURVE('',#43783,#40755,#35613,.T.);
#57904=EDGE_CURVE('',#41358,#43787,#2459,.T.);
#57905=EDGE_CURVE('',#43766,#40754,#35614,.T.);
#57906=EDGE_CURVE('',#41353,#43786,#35615,.T.);
#57907=EDGE_CURVE('',#43767,#40753,#35616,.T.);
#57908=EDGE_CURVE('',#41050,#43785,#35617,.T.);
#57909=EDGE_CURVE('',#43772,#40752,#35618,.T.);
#57910=EDGE_CURVE('',#41051,#43784,#35619,.T.);
#57911=EDGE_CURVE('',#43773,#40751,#35620,.T.);
#57912=EDGE_CURVE('',#41052,#43765,#35621,.T.);
#57913=EDGE_CURVE('',#43774,#41391,#35622,.T.);
#57914=EDGE_CURVE('',#41053,#43768,#35623,.T.);
#57915=EDGE_CURVE('',#43775,#41387,#2460,.T.);
#57916=EDGE_CURVE('',#41054,#43771,#35624,.T.);
#57917=EDGE_CURVE('',#43776,#41386,#35625,.T.);
#57918=EDGE_CURVE('',#41055,#43770,#35626,.T.);
#57919=EDGE_CURVE('',#43777,#41383,#35627,.T.);
#57920=EDGE_CURVE('',#41374,#43769,#35628,.T.);
#57921=EDGE_CURVE('',#43778,#41382,#35629,.T.);
#57922=EDGE_CURVE('',#41375,#43780,#2461,.T.);
#57923=EDGE_CURVE('',#43779,#41379,#35630,.T.);
#57924=EDGE_CURVE('',#43820,#41350,#2462,.T.);
#57925=EDGE_CURVE('',#41345,#43819,#35631,.T.);
#57926=EDGE_CURVE('',#41344,#43818,#35632,.T.);
#57927=EDGE_CURVE('',#43809,#41352,#35633,.T.);
#57928=EDGE_CURVE('',#41341,#43817,#35634,.T.);
#57929=EDGE_CURVE('',#43810,#40762,#35635,.T.);
#57930=EDGE_CURVE('',#41340,#43816,#35636,.T.);
#57931=EDGE_CURVE('',#43811,#40761,#35637,.T.);
#57932=EDGE_CURVE('',#41338,#43815,#2463,.T.);
#57933=EDGE_CURVE('',#43794,#40760,#35638,.T.);
#57934=EDGE_CURVE('',#41333,#43814,#35639,.T.);
#57935=EDGE_CURVE('',#43795,#40759,#35640,.T.);
#57936=EDGE_CURVE('',#41044,#43813,#35641,.T.);
#57937=EDGE_CURVE('',#43800,#40758,#35642,.T.);
#57938=EDGE_CURVE('',#41045,#43812,#35643,.T.);
#57939=EDGE_CURVE('',#43801,#40757,#35644,.T.);
#57940=EDGE_CURVE('',#41046,#43793,#35645,.T.);
#57941=EDGE_CURVE('',#43802,#41371,#35646,.T.);
#57942=EDGE_CURVE('',#41047,#43796,#35647,.T.);
#57943=EDGE_CURVE('',#43803,#41367,#2464,.T.);
#57944=EDGE_CURVE('',#41048,#43799,#35648,.T.);
#57945=EDGE_CURVE('',#43804,#41366,#35649,.T.);
#57946=EDGE_CURVE('',#41049,#43798,#35650,.T.);
#57947=EDGE_CURVE('',#43805,#41363,#35651,.T.);
#57948=EDGE_CURVE('',#41354,#43797,#35652,.T.);
#57949=EDGE_CURVE('',#43806,#41362,#35653,.T.);
#57950=EDGE_CURVE('',#41355,#43808,#2465,.T.);
#57951=EDGE_CURVE('',#43807,#41359,#35654,.T.);
#57952=EDGE_CURVE('',#43848,#41330,#2466,.T.);
#57953=EDGE_CURVE('',#41325,#43847,#35655,.T.);
#57954=EDGE_CURVE('',#41324,#43846,#35656,.T.);
#57955=EDGE_CURVE('',#43837,#41332,#35657,.T.);
#57956=EDGE_CURVE('',#41321,#43845,#35658,.T.);
#57957=EDGE_CURVE('',#43838,#40768,#35659,.T.);
#57958=EDGE_CURVE('',#41320,#43844,#35660,.T.);
#57959=EDGE_CURVE('',#43839,#40767,#35661,.T.);
#57960=EDGE_CURVE('',#41318,#43843,#2467,.T.);
#57961=EDGE_CURVE('',#43822,#40766,#35662,.T.);
#57962=EDGE_CURVE('',#41313,#43842,#35663,.T.);
#57963=EDGE_CURVE('',#43823,#40765,#35664,.T.);
#57964=EDGE_CURVE('',#41038,#43841,#35665,.T.);
#57965=EDGE_CURVE('',#43828,#40764,#35666,.T.);
#57966=EDGE_CURVE('',#41039,#43840,#35667,.T.);
#57967=EDGE_CURVE('',#43829,#40763,#35668,.T.);
#57968=EDGE_CURVE('',#41040,#43821,#35669,.T.);
#57969=EDGE_CURVE('',#43830,#41351,#35670,.T.);
#57970=EDGE_CURVE('',#41041,#43824,#35671,.T.);
#57971=EDGE_CURVE('',#43831,#41347,#2468,.T.);
#57972=EDGE_CURVE('',#41042,#43827,#35672,.T.);
#57973=EDGE_CURVE('',#43832,#41346,#35673,.T.);
#57974=EDGE_CURVE('',#41043,#43826,#35674,.T.);
#57975=EDGE_CURVE('',#43833,#41343,#35675,.T.);
#57976=EDGE_CURVE('',#41334,#43825,#35676,.T.);
#57977=EDGE_CURVE('',#43834,#41342,#35677,.T.);
#57978=EDGE_CURVE('',#41335,#43836,#2469,.T.);
#57979=EDGE_CURVE('',#43835,#41339,#35678,.T.);
#57980=EDGE_CURVE('',#43876,#41310,#2470,.T.);
#57981=EDGE_CURVE('',#41305,#43875,#35679,.T.);
#57982=EDGE_CURVE('',#41304,#43874,#35680,.T.);
#57983=EDGE_CURVE('',#43865,#41312,#35681,.T.);
#57984=EDGE_CURVE('',#41301,#43873,#35682,.T.);
#57985=EDGE_CURVE('',#43866,#40774,#35683,.T.);
#57986=EDGE_CURVE('',#41300,#43872,#35684,.T.);
#57987=EDGE_CURVE('',#43867,#40773,#35685,.T.);
#57988=EDGE_CURVE('',#41298,#43871,#2471,.T.);
#57989=EDGE_CURVE('',#43850,#40772,#35686,.T.);
#57990=EDGE_CURVE('',#41293,#43870,#35687,.T.);
#57991=EDGE_CURVE('',#43851,#40771,#35688,.T.);
#57992=EDGE_CURVE('',#41032,#43869,#35689,.T.);
#57993=EDGE_CURVE('',#43856,#40770,#35690,.T.);
#57994=EDGE_CURVE('',#41033,#43868,#35691,.T.);
#57995=EDGE_CURVE('',#43857,#40769,#35692,.T.);
#57996=EDGE_CURVE('',#41034,#43849,#35693,.T.);
#57997=EDGE_CURVE('',#43858,#41331,#35694,.T.);
#57998=EDGE_CURVE('',#41035,#43852,#35695,.T.);
#57999=EDGE_CURVE('',#43859,#41327,#2472,.T.);
#58000=EDGE_CURVE('',#41036,#43855,#35696,.T.);
#58001=EDGE_CURVE('',#43860,#41326,#35697,.T.);
#58002=EDGE_CURVE('',#41037,#43854,#35698,.T.);
#58003=EDGE_CURVE('',#43861,#41323,#35699,.T.);
#58004=EDGE_CURVE('',#41314,#43853,#35700,.T.);
#58005=EDGE_CURVE('',#43862,#41322,#35701,.T.);
#58006=EDGE_CURVE('',#41315,#43864,#2473,.T.);
#58007=EDGE_CURVE('',#43863,#41319,#35702,.T.);
#58008=EDGE_CURVE('',#43904,#41290,#2474,.T.);
#58009=EDGE_CURVE('',#41285,#43903,#35703,.T.);
#58010=EDGE_CURVE('',#41284,#43902,#35704,.T.);
#58011=EDGE_CURVE('',#43893,#41292,#35705,.T.);
#58012=EDGE_CURVE('',#41281,#43901,#35706,.T.);
#58013=EDGE_CURVE('',#43894,#40780,#35707,.T.);
#58014=EDGE_CURVE('',#41280,#43900,#35708,.T.);
#58015=EDGE_CURVE('',#43895,#40779,#35709,.T.);
#58016=EDGE_CURVE('',#41278,#43899,#2475,.T.);
#58017=EDGE_CURVE('',#43878,#40778,#35710,.T.);
#58018=EDGE_CURVE('',#41273,#43898,#35711,.T.);
#58019=EDGE_CURVE('',#43879,#40777,#35712,.T.);
#58020=EDGE_CURVE('',#41026,#43897,#35713,.T.);
#58021=EDGE_CURVE('',#43884,#40776,#35714,.T.);
#58022=EDGE_CURVE('',#41027,#43896,#35715,.T.);
#58023=EDGE_CURVE('',#43885,#40775,#35716,.T.);
#58024=EDGE_CURVE('',#41028,#43877,#35717,.T.);
#58025=EDGE_CURVE('',#43886,#41311,#35718,.T.);
#58026=EDGE_CURVE('',#41029,#43880,#35719,.T.);
#58027=EDGE_CURVE('',#43887,#41307,#2476,.T.);
#58028=EDGE_CURVE('',#41030,#43883,#35720,.T.);
#58029=EDGE_CURVE('',#43888,#41306,#35721,.T.);
#58030=EDGE_CURVE('',#41031,#43882,#35722,.T.);
#58031=EDGE_CURVE('',#43889,#41303,#35723,.T.);
#58032=EDGE_CURVE('',#41294,#43881,#35724,.T.);
#58033=EDGE_CURVE('',#43890,#41302,#35725,.T.);
#58034=EDGE_CURVE('',#41295,#43892,#2477,.T.);
#58035=EDGE_CURVE('',#43891,#41299,#35726,.T.);
#58036=EDGE_CURVE('',#43932,#41270,#2478,.T.);
#58037=EDGE_CURVE('',#41265,#43931,#35727,.T.);
#58038=EDGE_CURVE('',#41264,#43930,#35728,.T.);
#58039=EDGE_CURVE('',#43921,#41272,#35729,.T.);
#58040=EDGE_CURVE('',#41261,#43929,#35730,.T.);
#58041=EDGE_CURVE('',#43922,#40786,#35731,.T.);
#58042=EDGE_CURVE('',#41260,#43928,#35732,.T.);
#58043=EDGE_CURVE('',#43923,#40785,#35733,.T.);
#58044=EDGE_CURVE('',#41258,#43927,#2479,.T.);
#58045=EDGE_CURVE('',#43906,#40784,#35734,.T.);
#58046=EDGE_CURVE('',#41253,#43926,#35735,.T.);
#58047=EDGE_CURVE('',#43907,#40783,#35736,.T.);
#58048=EDGE_CURVE('',#41020,#43925,#35737,.T.);
#58049=EDGE_CURVE('',#43912,#40782,#35738,.T.);
#58050=EDGE_CURVE('',#41021,#43924,#35739,.T.);
#58051=EDGE_CURVE('',#43913,#40781,#35740,.T.);
#58052=EDGE_CURVE('',#41022,#43905,#35741,.T.);
#58053=EDGE_CURVE('',#43914,#41291,#35742,.T.);
#58054=EDGE_CURVE('',#41023,#43908,#35743,.T.);
#58055=EDGE_CURVE('',#43915,#41287,#2480,.T.);
#58056=EDGE_CURVE('',#41024,#43911,#35744,.T.);
#58057=EDGE_CURVE('',#43916,#41286,#35745,.T.);
#58058=EDGE_CURVE('',#41025,#43910,#35746,.T.);
#58059=EDGE_CURVE('',#43917,#41283,#35747,.T.);
#58060=EDGE_CURVE('',#41274,#43909,#35748,.T.);
#58061=EDGE_CURVE('',#43918,#41282,#35749,.T.);
#58062=EDGE_CURVE('',#41275,#43920,#2481,.T.);
#58063=EDGE_CURVE('',#43919,#41279,#35750,.T.);
#58064=EDGE_CURVE('',#43960,#41250,#2482,.T.);
#58065=EDGE_CURVE('',#41245,#43959,#35751,.T.);
#58066=EDGE_CURVE('',#41244,#43958,#35752,.T.);
#58067=EDGE_CURVE('',#43949,#41252,#35753,.T.);
#58068=EDGE_CURVE('',#41241,#43957,#35754,.T.);
#58069=EDGE_CURVE('',#43950,#40792,#35755,.T.);
#58070=EDGE_CURVE('',#41240,#43956,#35756,.T.);
#58071=EDGE_CURVE('',#43951,#40791,#35757,.T.);
#58072=EDGE_CURVE('',#41238,#43955,#2483,.T.);
#58073=EDGE_CURVE('',#43934,#40790,#35758,.T.);
#58074=EDGE_CURVE('',#41233,#43954,#35759,.T.);
#58075=EDGE_CURVE('',#43935,#40789,#35760,.T.);
#58076=EDGE_CURVE('',#41014,#43953,#35761,.T.);
#58077=EDGE_CURVE('',#43940,#40788,#35762,.T.);
#58078=EDGE_CURVE('',#41015,#43952,#35763,.T.);
#58079=EDGE_CURVE('',#43941,#40787,#35764,.T.);
#58080=EDGE_CURVE('',#41016,#43933,#35765,.T.);
#58081=EDGE_CURVE('',#43942,#41271,#35766,.T.);
#58082=EDGE_CURVE('',#41017,#43936,#35767,.T.);
#58083=EDGE_CURVE('',#43943,#41267,#2484,.T.);
#58084=EDGE_CURVE('',#41018,#43939,#35768,.T.);
#58085=EDGE_CURVE('',#43944,#41266,#35769,.T.);
#58086=EDGE_CURVE('',#41019,#43938,#35770,.T.);
#58087=EDGE_CURVE('',#43945,#41263,#35771,.T.);
#58088=EDGE_CURVE('',#41254,#43937,#35772,.T.);
#58089=EDGE_CURVE('',#43946,#41262,#35773,.T.);
#58090=EDGE_CURVE('',#41255,#43948,#2485,.T.);
#58091=EDGE_CURVE('',#43947,#41259,#35774,.T.);
#58092=EDGE_CURVE('',#43988,#41230,#2486,.T.);
#58093=EDGE_CURVE('',#41225,#43987,#35775,.T.);
#58094=EDGE_CURVE('',#41224,#43986,#35776,.T.);
#58095=EDGE_CURVE('',#43977,#41232,#35777,.T.);
#58096=EDGE_CURVE('',#41221,#43985,#35778,.T.);
#58097=EDGE_CURVE('',#43978,#40798,#35779,.T.);
#58098=EDGE_CURVE('',#41220,#43984,#35780,.T.);
#58099=EDGE_CURVE('',#43979,#40797,#35781,.T.);
#58100=EDGE_CURVE('',#41218,#43983,#2487,.T.);
#58101=EDGE_CURVE('',#43962,#40796,#35782,.T.);
#58102=EDGE_CURVE('',#41213,#43982,#35783,.T.);
#58103=EDGE_CURVE('',#43963,#40795,#35784,.T.);
#58104=EDGE_CURVE('',#41008,#43981,#35785,.T.);
#58105=EDGE_CURVE('',#43968,#40794,#35786,.T.);
#58106=EDGE_CURVE('',#41009,#43980,#35787,.T.);
#58107=EDGE_CURVE('',#43969,#40793,#35788,.T.);
#58108=EDGE_CURVE('',#41010,#43961,#35789,.T.);
#58109=EDGE_CURVE('',#43970,#41251,#35790,.T.);
#58110=EDGE_CURVE('',#41011,#43964,#35791,.T.);
#58111=EDGE_CURVE('',#43971,#41247,#2488,.T.);
#58112=EDGE_CURVE('',#41012,#43967,#35792,.T.);
#58113=EDGE_CURVE('',#43972,#41246,#35793,.T.);
#58114=EDGE_CURVE('',#41013,#43966,#35794,.T.);
#58115=EDGE_CURVE('',#43973,#41243,#35795,.T.);
#58116=EDGE_CURVE('',#41234,#43965,#35796,.T.);
#58117=EDGE_CURVE('',#43974,#41242,#35797,.T.);
#58118=EDGE_CURVE('',#41235,#43976,#2489,.T.);
#58119=EDGE_CURVE('',#43975,#41239,#35798,.T.);
#58120=EDGE_CURVE('',#44016,#41210,#2490,.T.);
#58121=EDGE_CURVE('',#41205,#44015,#35799,.T.);
#58122=EDGE_CURVE('',#41204,#44014,#35800,.T.);
#58123=EDGE_CURVE('',#44005,#41212,#35801,.T.);
#58124=EDGE_CURVE('',#41201,#44013,#35802,.T.);
#58125=EDGE_CURVE('',#44006,#40804,#35803,.T.);
#58126=EDGE_CURVE('',#41200,#44012,#35804,.T.);
#58127=EDGE_CURVE('',#44007,#40803,#35805,.T.);
#58128=EDGE_CURVE('',#41198,#44011,#2491,.T.);
#58129=EDGE_CURVE('',#43990,#40802,#35806,.T.);
#58130=EDGE_CURVE('',#41193,#44010,#35807,.T.);
#58131=EDGE_CURVE('',#43991,#40801,#35808,.T.);
#58132=EDGE_CURVE('',#41002,#44009,#35809,.T.);
#58133=EDGE_CURVE('',#43996,#40800,#35810,.T.);
#58134=EDGE_CURVE('',#41003,#44008,#35811,.T.);
#58135=EDGE_CURVE('',#43997,#40799,#35812,.T.);
#58136=EDGE_CURVE('',#41004,#43989,#35813,.T.);
#58137=EDGE_CURVE('',#43998,#41231,#35814,.T.);
#58138=EDGE_CURVE('',#41005,#43992,#35815,.T.);
#58139=EDGE_CURVE('',#43999,#41227,#2492,.T.);
#58140=EDGE_CURVE('',#41006,#43995,#35816,.T.);
#58141=EDGE_CURVE('',#44000,#41226,#35817,.T.);
#58142=EDGE_CURVE('',#41007,#43994,#35818,.T.);
#58143=EDGE_CURVE('',#44001,#41223,#35819,.T.);
#58144=EDGE_CURVE('',#41214,#43993,#35820,.T.);
#58145=EDGE_CURVE('',#44002,#41222,#35821,.T.);
#58146=EDGE_CURVE('',#41215,#44004,#2493,.T.);
#58147=EDGE_CURVE('',#44003,#41219,#35822,.T.);
#58148=EDGE_CURVE('',#44044,#41185,#2494,.T.);
#58149=EDGE_CURVE('',#41187,#44043,#35823,.T.);
#58150=EDGE_CURVE('',#41182,#44042,#35824,.T.);
#58151=EDGE_CURVE('',#44033,#41192,#35825,.T.);
#58152=EDGE_CURVE('',#41183,#44041,#35826,.T.);
#58153=EDGE_CURVE('',#44034,#40810,#35827,.T.);
#58154=EDGE_CURVE('',#41180,#44040,#35828,.T.);
#58155=EDGE_CURVE('',#44035,#40809,#35829,.T.);
#58156=EDGE_CURVE('',#41173,#44039,#2495,.T.);
#58157=EDGE_CURVE('',#44018,#40808,#35830,.T.);
#58158=EDGE_CURVE('',#41175,#44038,#35831,.T.);
#58159=EDGE_CURVE('',#44019,#40807,#35832,.T.);
#58160=EDGE_CURVE('',#40996,#44037,#35833,.T.);
#58161=EDGE_CURVE('',#44024,#40806,#35834,.T.);
#58162=EDGE_CURVE('',#40997,#44036,#35835,.T.);
#58163=EDGE_CURVE('',#44025,#40805,#35836,.T.);
#58164=EDGE_CURVE('',#40998,#44017,#35837,.T.);
#58165=EDGE_CURVE('',#44026,#41211,#35838,.T.);
#58166=EDGE_CURVE('',#40999,#44020,#35839,.T.);
#58167=EDGE_CURVE('',#44027,#41207,#2496,.T.);
#58168=EDGE_CURVE('',#41000,#44023,#35840,.T.);
#58169=EDGE_CURVE('',#44028,#41206,#35841,.T.);
#58170=EDGE_CURVE('',#41001,#44022,#35842,.T.);
#58171=EDGE_CURVE('',#44029,#41203,#35843,.T.);
#58172=EDGE_CURVE('',#41194,#44021,#35844,.T.);
#58173=EDGE_CURVE('',#44030,#41202,#35845,.T.);
#58174=EDGE_CURVE('',#41195,#44032,#2497,.T.);
#58175=EDGE_CURVE('',#44031,#41199,#35846,.T.);
#58176=EDGE_CURVE('',#44045,#44045,#35847,.T.);
#58177=EDGE_CURVE('',#44045,#44046,#35848,.T.);
#58178=EDGE_CURVE('',#44046,#44046,#35849,.T.);
#58179=EDGE_CURVE('',#44047,#44047,#35850,.T.);
#58180=EDGE_CURVE('',#44047,#44048,#35851,.T.);
#58181=EDGE_CURVE('',#44048,#44048,#35852,.T.);
#58182=EDGE_CURVE('',#44049,#44049,#35853,.T.);
#58183=EDGE_CURVE('',#44049,#44050,#35854,.T.);
#58184=EDGE_CURVE('',#44051,#44050,#35855,.T.);
#58185=EDGE_CURVE('',#44050,#44051,#35856,.T.);
#58186=EDGE_CURVE('',#44052,#44052,#35857,.T.);
#58187=EDGE_CURVE('',#44052,#44045,#23960,.T.);
#58188=EDGE_CURVE('',#44048,#44051,#23961,.T.);
#58189=EDGE_CURVE('',#44053,#44053,#35858,.T.);
#58190=EDGE_CURVE('',#44053,#44054,#23962,.T.);
#58191=EDGE_CURVE('',#44054,#44054,#35859,.T.);
#58192=EDGE_CURVE('',#44055,#44055,#35860,.T.);
#58193=EDGE_CURVE('',#44055,#44056,#35861,.T.);
#58194=EDGE_CURVE('',#44056,#44056,#35862,.T.);
#58195=EDGE_CURVE('',#44057,#44057,#35863,.T.);
#58196=EDGE_CURVE('',#44057,#44058,#35864,.T.);
#58197=EDGE_CURVE('',#44058,#44058,#35865,.T.);
#58198=EDGE_CURVE('',#44059,#44059,#35866,.T.);
#58199=EDGE_CURVE('',#44059,#44055,#23963,.T.);
#58200=EDGE_CURVE('',#44058,#44060,#23964,.T.);
#58201=EDGE_CURVE('',#44060,#44060,#35867,.T.);
#58202=EDGE_CURVE('',#44061,#44061,#35868,.T.);
#58203=EDGE_CURVE('',#44061,#44062,#35869,.T.);
#58204=EDGE_CURVE('',#44062,#44062,#35870,.T.);
#58205=EDGE_CURVE('',#44063,#44064,#35871,.T.);
#58206=EDGE_CURVE('',#44065,#44063,#35872,.T.);
#58207=EDGE_CURVE('',#44066,#44065,#35873,.T.);
#58208=EDGE_CURVE('',#44066,#44064,#35874,.T.);
#58209=EDGE_CURVE('',#44067,#44068,#35875,.T.);
#58210=EDGE_CURVE('',#44067,#44069,#35876,.T.);
#58211=EDGE_CURVE('',#44070,#44069,#35877,.T.);
#58212=EDGE_CURVE('',#44068,#44070,#35878,.T.);
#58213=EDGE_CURVE('',#44071,#44072,#35879,.T.);
#58214=EDGE_CURVE('',#44071,#44073,#35880,.T.);
#58215=EDGE_CURVE('',#44074,#44073,#35881,.T.);
#58216=EDGE_CURVE('',#44072,#44074,#35882,.T.);
#58217=EDGE_CURVE('',#44075,#44076,#35883,.T.);
#58218=EDGE_CURVE('',#44075,#44077,#35884,.T.);
#58219=EDGE_CURVE('',#44078,#44077,#35885,.T.);
#58220=EDGE_CURVE('',#44076,#44078,#35886,.T.);
#58221=EDGE_CURVE('',#44079,#44080,#35887,.T.);
#58222=EDGE_CURVE('',#44081,#44079,#35888,.T.);
#58223=EDGE_CURVE('',#44082,#44081,#35889,.T.);
#58224=EDGE_CURVE('',#44080,#44082,#35890,.T.);
#58225=EDGE_CURVE('',#44083,#44084,#35891,.T.);
#58226=EDGE_CURVE('',#44083,#44085,#35892,.T.);
#58227=EDGE_CURVE('',#44086,#44085,#35893,.T.);
#58228=EDGE_CURVE('',#44084,#44086,#35894,.T.);
#58229=EDGE_CURVE('',#44085,#44087,#35895,.T.);
#58230=EDGE_CURVE('',#44088,#44083,#35896,.T.);
#58231=EDGE_CURVE('',#44088,#44087,#35897,.T.);
#58232=EDGE_CURVE('',#44089,#44088,#35898,.T.);
#58233=EDGE_CURVE('',#44090,#44089,#35899,.T.);
#58234=EDGE_CURVE('',#44087,#44090,#35900,.T.);
#58235=EDGE_CURVE('',#44091,#44077,#23965,.T.);
#58236=EDGE_CURVE('',#44092,#44091,#35901,.T.);
#58237=EDGE_CURVE('',#44092,#44093,#5215,.T.);
#58238=EDGE_CURVE('',#44093,#44094,#5216,.T.);
#58239=EDGE_CURVE('',#44078,#44094,#23966,.T.);
#58240=EDGE_CURVE('',#44095,#44081,#23967,.T.);
#58241=EDGE_CURVE('',#44095,#44096,#5217,.T.);
#58242=EDGE_CURVE('',#44096,#44097,#5218,.T.);
#58243=EDGE_CURVE('',#44098,#44097,#35902,.T.);
#58244=EDGE_CURVE('',#44082,#44098,#23968,.T.);
#58245=EDGE_CURVE('',#44099,#44100,#35903,.T.);
#58246=EDGE_CURVE('',#44099,#44091,#5219,.T.);
#58247=EDGE_CURVE('',#44098,#44091,#35904,.T.);
#58248=EDGE_CURVE('',#44098,#44100,#5220,.T.);
#58249=EDGE_CURVE('',#44101,#44101,#35905,.T.);
#58250=EDGE_CURVE('',#44101,#44102,#23969,.T.);
#58251=EDGE_CURVE('',#44102,#44102,#35906,.T.);
#58252=EDGE_CURVE('',#44103,#44103,#35907,.T.);
#58253=EDGE_CURVE('',#44103,#44104,#23970,.T.);
#58254=EDGE_CURVE('',#44104,#44104,#35908,.T.);
#58255=EDGE_CURVE('',#44105,#44105,#35909,.T.);
#58256=EDGE_CURVE('',#44105,#44106,#23971,.T.);
#58257=EDGE_CURVE('',#44106,#44106,#35910,.T.);
#58258=EDGE_CURVE('',#44107,#44107,#35911,.T.);
#58259=EDGE_CURVE('',#44107,#44108,#23972,.T.);
#58260=EDGE_CURVE('',#44108,#44108,#35912,.T.);
#58261=EDGE_CURVE('',#44109,#44109,#35913,.T.);
#58262=EDGE_CURVE('',#44109,#44110,#23973,.T.);
#58263=EDGE_CURVE('',#44110,#44110,#35914,.T.);
#58264=EDGE_CURVE('',#44087,#44111,#23974,.T.);
#58265=EDGE_CURVE('',#44111,#44112,#35915,.T.);
#58266=EDGE_CURVE('',#44112,#44085,#23975,.T.);
#58267=EDGE_CURVE('',#44064,#44113,#5221,.T.);
#58268=EDGE_CURVE('',#44113,#44114,#35916,.T.);
#58269=EDGE_CURVE('',#44114,#44115,#5222,.T.);
#58270=EDGE_CURVE('',#44115,#44116,#5223,.T.);
#58271=EDGE_CURVE('',#44116,#44117,#35917,.T.);
#58272=EDGE_CURVE('',#44117,#44118,#5224,.T.);
#58273=EDGE_CURVE('',#44118,#44099,#5225,.T.);
#58274=EDGE_CURVE('',#44100,#44119,#5226,.T.);
#58275=EDGE_CURVE('',#44119,#44120,#5227,.T.);
#58276=EDGE_CURVE('',#44120,#44121,#35918,.T.);
#58277=EDGE_CURVE('',#44121,#44122,#5228,.T.);
#58278=EDGE_CURVE('',#44122,#44123,#5229,.T.);
#58279=EDGE_CURVE('',#44123,#44124,#35919,.T.);
#58280=EDGE_CURVE('',#44124,#44125,#5230,.T.);
#58281=EDGE_CURVE('',#44125,#44126,#5231,.T.);
#58282=EDGE_CURVE('',#44126,#44127,#35920,.T.);
#58283=EDGE_CURVE('',#44127,#44128,#5232,.T.);
#58284=EDGE_CURVE('',#44128,#44129,#5233,.T.);
#58285=EDGE_CURVE('',#44129,#44130,#35921,.T.);
#58286=EDGE_CURVE('',#44130,#44131,#5234,.T.);
#58287=EDGE_CURVE('',#44131,#44132,#5235,.T.);
#58288=EDGE_CURVE('',#44132,#44133,#35922,.T.);
#58289=EDGE_CURVE('',#44133,#44134,#5236,.T.);
#58290=EDGE_CURVE('',#44134,#44135,#5237,.T.);
#58291=EDGE_CURVE('',#44135,#44136,#35923,.T.);
#58292=EDGE_CURVE('',#44136,#44063,#5238,.T.);
#58293=EDGE_CURVE('',#44137,#44138,#35924,.T.);
#58294=EDGE_CURVE('',#44139,#44138,#23976,.T.);
#58295=EDGE_CURVE('',#44139,#44140,#35925,.T.);
#58296=EDGE_CURVE('',#44140,#44141,#5239,.T.);
#58297=EDGE_CURVE('',#44141,#44142,#23977,.T.);
#58298=EDGE_CURVE('',#44143,#44142,#35926,.T.);
#58299=EDGE_CURVE('',#44144,#44143,#23978,.T.);
#58300=EDGE_CURVE('',#44144,#44145,#5240,.T.);
#58301=EDGE_CURVE('',#44145,#44146,#35927,.T.);
#58302=EDGE_CURVE('',#44146,#44137,#23979,.T.);
#58303=EDGE_CURVE('',#44147,#44148,#35928,.T.);
#58304=EDGE_CURVE('',#44149,#44148,#23980,.T.);
#58305=EDGE_CURVE('',#44149,#44150,#35929,.T.);
#58306=EDGE_CURVE('',#44150,#44151,#5241,.T.);
#58307=EDGE_CURVE('',#44151,#44152,#23981,.T.);
#58308=EDGE_CURVE('',#44153,#44152,#35930,.T.);
#58309=EDGE_CURVE('',#44154,#44153,#23982,.T.);
#58310=EDGE_CURVE('',#44154,#44155,#5242,.T.);
#58311=EDGE_CURVE('',#44155,#44156,#35931,.T.);
#58312=EDGE_CURVE('',#44156,#44147,#23983,.T.);
#58313=EDGE_CURVE('',#44157,#44158,#23984,.T.);
#58314=EDGE_CURVE('',#44157,#44154,#23985,.T.);
#58315=EDGE_CURVE('',#44158,#44153,#23986,.T.);
#58316=EDGE_CURVE('',#44151,#44144,#23987,.T.);
#58317=EDGE_CURVE('',#44152,#44143,#23988,.T.);
#58318=EDGE_CURVE('',#44159,#44160,#23989,.T.);
#58319=EDGE_CURVE('',#44159,#44161,#23990,.T.);
#58320=EDGE_CURVE('',#44161,#44162,#23991,.T.);
#58321=EDGE_CURVE('',#44160,#44162,#23992,.T.);
#58322=EDGE_CURVE('',#44163,#44067,#23993,.T.);
#58323=EDGE_CURVE('',#44164,#44068,#23994,.T.);
#58324=EDGE_CURVE('',#44164,#44165,#35932,.T.);
#58325=EDGE_CURVE('',#44165,#44157,#5243,.T.);
#58326=EDGE_CURVE('',#44162,#44158,#35933,.T.);
#58327=EDGE_CURVE('',#44161,#44166,#5244,.T.);
#58328=EDGE_CURVE('',#44166,#44163,#35934,.T.);
#58329=EDGE_CURVE('',#44167,#44071,#23995,.T.);
#58330=EDGE_CURVE('',#44168,#44072,#23996,.T.);
#58331=EDGE_CURVE('',#44168,#44169,#35935,.T.);
#58332=EDGE_CURVE('',#44169,#44159,#5245,.T.);
#58333=EDGE_CURVE('',#44170,#44160,#35936,.T.);
#58334=EDGE_CURVE('',#44171,#44170,#23997,.T.);
#58335=EDGE_CURVE('',#44171,#44172,#5246,.T.);
#58336=EDGE_CURVE('',#44172,#44167,#35937,.T.);
#58337=EDGE_CURVE('',#44173,#44174,#5247,.T.);
#58338=EDGE_CURVE('',#44174,#44171,#23998,.T.);
#58339=EDGE_CURVE('',#44142,#44170,#23999,.T.);
#58340=EDGE_CURVE('',#44141,#44173,#24000,.T.);
#58341=EDGE_CURVE('',#44175,#44176,#24001,.T.);
#58342=EDGE_CURVE('',#44175,#44177,#35938,.T.);
#58343=EDGE_CURVE('',#44177,#44178,#24002,.T.);
#58344=EDGE_CURVE('',#44176,#44178,#35939,.T.);
#58345=EDGE_CURVE('',#44177,#44179,#24003,.T.);
#58346=EDGE_CURVE('',#44179,#44180,#24004,.T.);
#58347=EDGE_CURVE('',#44178,#44180,#24005,.T.);
#58348=EDGE_CURVE('',#44179,#44181,#35940,.T.);
#58349=EDGE_CURVE('',#44181,#44182,#24006,.T.);
#58350=EDGE_CURVE('',#44180,#44182,#35941,.T.);
#58351=EDGE_CURVE('',#44181,#44183,#24007,.T.);
#58352=EDGE_CURVE('',#44183,#44184,#24008,.T.);
#58353=EDGE_CURVE('',#44182,#44184,#24009,.T.);
#58354=EDGE_CURVE('',#44183,#44185,#35942,.T.);
#58355=EDGE_CURVE('',#44185,#44186,#24010,.T.);
#58356=EDGE_CURVE('',#44184,#44186,#35943,.T.);
#58357=EDGE_CURVE('',#44185,#44187,#24011,.T.);
#58358=EDGE_CURVE('',#44187,#44188,#24012,.T.);
#58359=EDGE_CURVE('',#44186,#44188,#24013,.T.);
#58360=EDGE_CURVE('',#44187,#44189,#35944,.T.);
#58361=EDGE_CURVE('',#44189,#44190,#24014,.T.);
#58362=EDGE_CURVE('',#44188,#44190,#35945,.T.);
#58363=EDGE_CURVE('',#44189,#44175,#24015,.T.);
#58364=EDGE_CURVE('',#44190,#44176,#24016,.T.);
#58365=EDGE_CURVE('',#44065,#44191,#5248,.T.);
#58366=EDGE_CURVE('',#44191,#44192,#24017,.T.);
#58367=EDGE_CURVE('',#44192,#44193,#35946,.T.);
#58368=EDGE_CURVE('',#44193,#44194,#24018,.T.);
#58369=EDGE_CURVE('',#44194,#44066,#5249,.T.);
#58370=EDGE_CURVE('',#44195,#44196,#5250,.T.);
#58371=EDGE_CURVE('',#44196,#44197,#24019,.T.);
#58372=EDGE_CURVE('',#44198,#44197,#24020,.T.);
#58373=EDGE_CURVE('',#44198,#44199,#5251,.T.);
#58374=EDGE_CURVE('',#44199,#44200,#5252,.T.);
#58375=EDGE_CURVE('',#44200,#44201,#5253,.T.);
#58376=EDGE_CURVE('',#44201,#44202,#24021,.T.);
#58377=EDGE_CURVE('',#44202,#44195,#35947,.T.);
#58378=EDGE_CURVE('',#44203,#44204,#24022,.T.);
#58379=EDGE_CURVE('',#44204,#44205,#24023,.T.);
#58380=EDGE_CURVE('',#44205,#44206,#5254,.T.);
#58381=EDGE_CURVE('',#44206,#44207,#35948,.T.);
#58382=EDGE_CURVE('',#44207,#44208,#24024,.T.);
#58383=EDGE_CURVE('',#44208,#44209,#5255,.T.);
#58384=EDGE_CURVE('',#44209,#44210,#5256,.T.);
#58385=EDGE_CURVE('',#44210,#44203,#5257,.T.);
#58386=EDGE_CURVE('',#44197,#44204,#35949,.T.);
#58387=EDGE_CURVE('',#44203,#44198,#5258,.T.);
#58388=EDGE_CURVE('',#44199,#44210,#5259,.T.);
#58389=EDGE_CURVE('',#44209,#44211,#5260,.T.);
#58390=EDGE_CURVE('',#44211,#44212,#5261,.T.);
#58391=EDGE_CURVE('',#44212,#44200,#5262,.T.);
#58392=EDGE_CURVE('',#44213,#44214,#35950,.T.);
#58393=EDGE_CURVE('',#44214,#44215,#24025,.T.);
#58394=EDGE_CURVE('',#44215,#44216,#35951,.T.);
#58395=EDGE_CURVE('',#44216,#44213,#24026,.T.);
#58396=EDGE_CURVE('',#44172,#44217,#24027,.T.);
#58397=EDGE_CURVE('',#44217,#44218,#5263,.T.);
#58398=EDGE_CURVE('',#44218,#44214,#35952,.T.);
#58399=EDGE_CURVE('',#44213,#44219,#35953,.T.);
#58400=EDGE_CURVE('',#44167,#44219,#24028,.T.);
#58401=EDGE_CURVE('',#44220,#44221,#35954,.T.);
#58402=EDGE_CURVE('',#44221,#44222,#5264,.T.);
#58403=EDGE_CURVE('',#44222,#44140,#24029,.T.);
#58404=EDGE_CURVE('',#44223,#44139,#24030,.T.);
#58405=EDGE_CURVE('',#44223,#44224,#35955,.T.);
#58406=EDGE_CURVE('',#44220,#44224,#35956,.T.);
#58407=EDGE_CURVE('',#44225,#44226,#35957,.T.);
#58408=EDGE_CURVE('',#44226,#44220,#24031,.T.);
#58409=EDGE_CURVE('',#44224,#44225,#24032,.T.);
#58410=EDGE_CURVE('',#44227,#44228,#24033,.T.);
#58411=EDGE_CURVE('',#44228,#44229,#35958,.T.);
#58412=EDGE_CURVE('',#44229,#44230,#24034,.T.);
#58413=EDGE_CURVE('',#44230,#44227,#35959,.T.);
#58414=EDGE_CURVE('',#44077,#44082,#35960,.T.);
#58415=EDGE_CURVE('',#44231,#44232,#24035,.T.);
#58416=EDGE_CURVE('',#44232,#44233,#35961,.T.);
#58417=EDGE_CURVE('',#44233,#44234,#24036,.T.);
#58418=EDGE_CURVE('',#44234,#44231,#35962,.T.);
#58419=EDGE_CURVE('',#44235,#44236,#24037,.T.);
#58420=EDGE_CURVE('',#44236,#44237,#35963,.T.);
#58421=EDGE_CURVE('',#44237,#44238,#24038,.T.);
#58422=EDGE_CURVE('',#44238,#44235,#35964,.T.);
#58423=EDGE_CURVE('',#44069,#44239,#24039,.T.);
#58424=EDGE_CURVE('',#44239,#44240,#35965,.T.);
#58425=EDGE_CURVE('',#44240,#44070,#24040,.T.);
#58426=EDGE_CURVE('',#44073,#44241,#24041,.T.);
#58427=EDGE_CURVE('',#44241,#44242,#35966,.T.);
#58428=EDGE_CURVE('',#44242,#44074,#24042,.T.);
#58429=EDGE_CURVE('',#44219,#44243,#24043,.T.);
#58430=EDGE_CURVE('',#44243,#44244,#5265,.T.);
#58431=EDGE_CURVE('',#44244,#44245,#5266,.T.);
#58432=EDGE_CURVE('',#44245,#44071,#24044,.T.);
#58433=EDGE_CURVE('',#44138,#44246,#24045,.T.);
#58434=EDGE_CURVE('',#44246,#44247,#5267,.T.);
#58435=EDGE_CURVE('',#44247,#44248,#5268,.T.);
#58436=EDGE_CURVE('',#44248,#44223,#24046,.T.);
#58437=EDGE_CURVE('',#44094,#44249,#5269,.T.);
#58438=EDGE_CURVE('',#44249,#44250,#5270,.T.);
#58439=EDGE_CURVE('',#44250,#44137,#24047,.T.);
#58440=EDGE_CURVE('',#44146,#44078,#24048,.T.);
#58441=EDGE_CURVE('',#44251,#44252,#35967,.T.);
#58442=EDGE_CURVE('',#44252,#44253,#24049,.T.);
#58443=EDGE_CURVE('',#44253,#44254,#35968,.T.);
#58444=EDGE_CURVE('',#44254,#44079,#24050,.T.);
#58445=EDGE_CURVE('',#44080,#44075,#35969,.T.);
#58446=EDGE_CURVE('',#44076,#44251,#24051,.T.);
#58447=EDGE_CURVE('',#44148,#44255,#24052,.T.);
#58448=EDGE_CURVE('',#44255,#44256,#5271,.T.);
#58449=EDGE_CURVE('',#44256,#44095,#5272,.T.);
#58450=EDGE_CURVE('',#44081,#44149,#24053,.T.);
#58451=EDGE_CURVE('',#44257,#44258,#24054,.T.);
#58452=EDGE_CURVE('',#44258,#44259,#5273,.T.);
#58453=EDGE_CURVE('',#44259,#44260,#5274,.T.);
#58454=EDGE_CURVE('',#44260,#44147,#24055,.T.);
#58455=EDGE_CURVE('',#44156,#44257,#24056,.T.);
#58456=EDGE_CURVE('',#44261,#44262,#35970,.T.);
#58457=EDGE_CURVE('',#44262,#44263,#24057,.T.);
#58458=EDGE_CURVE('',#44263,#44264,#35971,.T.);
#58459=EDGE_CURVE('',#44264,#44265,#24058,.T.);
#58460=EDGE_CURVE('',#44265,#44266,#35972,.T.);
#58461=EDGE_CURVE('',#44266,#44267,#35973,.T.);
#58462=EDGE_CURVE('',#44267,#44268,#35974,.T.);
#58463=EDGE_CURVE('',#44268,#44261,#24059,.T.);
#58464=EDGE_CURVE('',#44068,#44269,#24060,.T.);
#58465=EDGE_CURVE('',#44269,#44270,#5275,.T.);
#58466=EDGE_CURVE('',#44270,#44271,#5276,.T.);
#58467=EDGE_CURVE('',#44271,#44272,#24061,.T.);
#58468=EDGE_CURVE('',#44272,#44164,#24062,.T.);
#58469=EDGE_CURVE('',#44086,#44273,#24063,.T.);
#58470=EDGE_CURVE('',#44273,#44274,#5277,.T.);
#58471=EDGE_CURVE('',#44274,#44275,#5278,.T.);
#58472=EDGE_CURVE('',#44275,#44067,#24064,.T.);
#58473=EDGE_CURVE('',#44163,#44086,#24065,.T.);
#58474=EDGE_CURVE('',#44276,#44277,#35975,.T.);
#58475=EDGE_CURVE('',#44277,#44278,#24066,.T.);
#58476=EDGE_CURVE('',#44278,#44279,#35976,.T.);
#58477=EDGE_CURVE('',#44279,#44089,#24067,.T.);
#58478=EDGE_CURVE('',#44084,#44276,#24068,.T.);
#58479=EDGE_CURVE('',#44072,#44280,#24069,.T.);
#58480=EDGE_CURVE('',#44280,#44281,#2498,.T.);
#58481=EDGE_CURVE('',#44281,#44090,#24070,.T.);
#58482=EDGE_CURVE('',#44090,#44168,#24071,.T.);
#58483=EDGE_CURVE('',#44215,#44136,#35977,.T.);
#58484=EDGE_CURVE('',#44135,#44216,#5279,.T.);
#58485=EDGE_CURVE('',#44113,#44226,#35978,.T.);
#58486=EDGE_CURVE('',#44225,#44114,#5280,.T.);
#58487=EDGE_CURVE('',#44123,#44235,#5281,.T.);
#58488=EDGE_CURVE('',#44238,#44124,#5282,.T.);
#58489=EDGE_CURVE('',#44129,#44112,#5283,.T.);
#58490=EDGE_CURVE('',#44111,#44130,#5284,.T.);
#58491=EDGE_CURVE('',#44282,#44235,#35979,.T.);
#58492=EDGE_CURVE('',#44282,#44258,#5285,.T.);
#58493=EDGE_CURVE('',#44257,#44236,#35980,.T.);
#58494=EDGE_CURVE('',#44123,#44283,#5286,.T.);
#58495=EDGE_CURVE('',#44283,#44282,#5287,.T.);
#58496=EDGE_CURVE('',#44271,#44284,#5288,.T.);
#58497=EDGE_CURVE('',#44238,#44284,#35981,.T.);
#58498=EDGE_CURVE('',#44237,#44272,#35982,.T.);
#58499=EDGE_CURVE('',#44284,#44285,#5289,.T.);
#58500=EDGE_CURVE('',#44285,#44124,#5290,.T.);
#58501=EDGE_CURVE('',#44286,#44112,#35983,.T.);
#58502=EDGE_CURVE('',#44286,#44273,#5291,.T.);
#58503=EDGE_CURVE('',#44129,#44287,#5292,.T.);
#58504=EDGE_CURVE('',#44287,#44286,#5293,.T.);
#58505=EDGE_CURVE('',#44281,#44288,#5294,.T.);
#58506=EDGE_CURVE('',#44288,#44289,#5295,.T.);
#58507=EDGE_CURVE('',#44111,#44289,#35984,.T.);
#58508=EDGE_CURVE('',#44289,#44290,#5296,.T.);
#58509=EDGE_CURVE('',#44290,#44130,#5297,.T.);
#58510=EDGE_CURVE('',#44291,#44216,#35985,.T.);
#58511=EDGE_CURVE('',#44291,#44243,#5298,.T.);
#58512=EDGE_CURVE('',#44135,#44292,#5299,.T.);
#58513=EDGE_CURVE('',#44292,#44291,#5300,.T.);
#58514=EDGE_CURVE('',#44248,#44293,#5301,.T.);
#58515=EDGE_CURVE('',#44225,#44293,#35986,.T.);
#58516=EDGE_CURVE('',#44293,#44294,#5302,.T.);
#58517=EDGE_CURVE('',#44294,#44114,#5303,.T.);
#58518=EDGE_CURVE('',#44097,#44295,#5304,.T.);
#58519=EDGE_CURVE('',#44295,#44100,#5305,.T.);
#58520=EDGE_CURVE('',#44099,#44296,#5306,.T.);
#58521=EDGE_CURVE('',#44296,#44092,#5307,.T.);
#58522=EDGE_CURVE('',#44266,#44237,#35987,.T.);
#58523=EDGE_CURVE('',#44272,#44265,#35988,.T.);
#58524=EDGE_CURVE('',#44164,#44264,#35989,.T.);
#58525=EDGE_CURVE('',#44267,#44236,#35990,.T.);
#58526=EDGE_CURVE('',#44165,#44263,#35991,.T.);
#58527=EDGE_CURVE('',#44268,#44257,#35992,.T.);
#58528=EDGE_CURVE('',#44157,#44263,#5308,.T.);
#58529=EDGE_CURVE('',#44261,#44156,#35993,.T.);
#58530=EDGE_CURVE('',#44154,#44262,#5309,.T.);
#58531=EDGE_CURVE('',#44262,#44155,#35994,.T.);
#58532=EDGE_CURVE('',#44168,#44279,#35995,.T.);
#58533=EDGE_CURVE('',#44169,#44278,#35996,.T.);
#58534=EDGE_CURVE('',#44159,#44278,#5310,.T.);
#58535=EDGE_CURVE('',#44276,#44163,#35997,.T.);
#58536=EDGE_CURVE('',#44161,#44277,#5311,.T.);
#58537=EDGE_CURVE('',#44277,#44166,#35998,.T.);
#58538=EDGE_CURVE('',#44149,#44254,#35999,.T.);
#58539=EDGE_CURVE('',#44150,#44253,#36000,.T.);
#58540=EDGE_CURVE('',#44151,#44253,#5312,.T.);
#58541=EDGE_CURVE('',#44251,#44146,#36001,.T.);
#58542=EDGE_CURVE('',#44144,#44252,#5313,.T.);
#58543=EDGE_CURVE('',#44252,#44145,#36002,.T.);
#58544=EDGE_CURVE('',#44222,#44173,#36003,.T.);
#58545=EDGE_CURVE('',#44211,#44174,#36004,.T.);
#58546=EDGE_CURVE('',#44173,#44212,#36005,.T.);
#58547=EDGE_CURVE('',#44174,#44217,#36006,.T.);
#58548=EDGE_CURVE('',#44250,#44228,#5314,.T.);
#58549=EDGE_CURVE('',#44137,#44227,#36007,.T.);
#58550=EDGE_CURVE('',#44138,#44230,#36008,.T.);
#58551=EDGE_CURVE('',#44229,#44246,#5315,.T.);
#58552=EDGE_CURVE('',#44245,#44241,#5316,.T.);
#58553=EDGE_CURVE('',#44242,#44280,#5317,.T.);
#58554=EDGE_CURVE('',#44275,#44239,#5318,.T.);
#58555=EDGE_CURVE('',#44240,#44269,#5319,.T.);
#58556=EDGE_CURVE('',#44260,#44232,#5320,.T.);
#58557=EDGE_CURVE('',#44147,#44231,#36009,.T.);
#58558=EDGE_CURVE('',#44148,#44234,#36010,.T.);
#58559=EDGE_CURVE('',#44233,#44255,#5321,.T.);
#58560=EDGE_CURVE('',#44259,#44297,#5322,.T.);
#58561=EDGE_CURVE('',#44297,#44122,#5323,.T.);
#58562=EDGE_CURVE('',#44232,#44121,#36011,.T.);
#58563=EDGE_CURVE('',#44233,#44120,#36012,.T.);
#58564=EDGE_CURVE('',#44119,#44298,#5324,.T.);
#58565=EDGE_CURVE('',#44298,#44256,#5325,.T.);
#58566=EDGE_CURVE('',#44274,#44299,#5326,.T.);
#58567=EDGE_CURVE('',#44299,#44128,#5327,.T.);
#58568=EDGE_CURVE('',#44239,#44127,#36013,.T.);
#58569=EDGE_CURVE('',#44240,#44126,#36014,.T.);
#58570=EDGE_CURVE('',#44125,#44300,#5328,.T.);
#58571=EDGE_CURVE('',#44300,#44270,#5329,.T.);
#58572=EDGE_CURVE('',#44244,#44301,#5330,.T.);
#58573=EDGE_CURVE('',#44301,#44134,#5331,.T.);
#58574=EDGE_CURVE('',#44241,#44133,#36015,.T.);
#58575=EDGE_CURVE('',#44242,#44132,#36016,.T.);
#58576=EDGE_CURVE('',#44131,#44302,#5332,.T.);
#58577=EDGE_CURVE('',#44302,#44303,#5333,.T.);
#58578=EDGE_CURVE('',#44303,#44280,#2499,.T.);
#58579=EDGE_CURVE('',#44115,#44304,#5334,.T.);
#58580=EDGE_CURVE('',#44304,#44247,#5335,.T.);
#58581=EDGE_CURVE('',#44116,#44229,#36017,.T.);
#58582=EDGE_CURVE('',#44117,#44228,#36018,.T.);
#58583=EDGE_CURVE('',#44249,#44305,#5336,.T.);
#58584=EDGE_CURVE('',#44305,#44118,#5337,.T.);
#58585=EDGE_CURVE('',#44205,#44063,#5338,.T.);
#58586=EDGE_CURVE('',#44206,#44136,#36019,.T.);
#58587=EDGE_CURVE('',#44207,#44215,#36020,.T.);
#58588=EDGE_CURVE('',#44218,#44208,#5339,.T.);
#58589=EDGE_CURVE('',#44064,#44196,#5340,.T.);
#58590=EDGE_CURVE('',#44113,#44195,#36021,.T.);
#58591=EDGE_CURVE('',#44226,#44202,#36022,.T.);
#58592=EDGE_CURVE('',#44201,#44221,#5341,.T.);
#58593=EDGE_CURVE('',#44211,#44217,#36023,.T.);
#58594=EDGE_CURVE('',#44222,#44212,#36024,.T.);
#58595=EDGE_CURVE('',#44281,#44303,#5342,.T.);
#58596=EDGE_CURVE('',#44288,#44303,#36025,.T.);
#58597=EDGE_CURVE('',#44289,#44302,#36026,.T.);
#58598=EDGE_CURVE('',#44290,#44131,#36027,.T.);
#58599=EDGE_CURVE('',#44301,#44291,#36028,.T.);
#58600=EDGE_CURVE('',#44134,#44292,#36029,.T.);
#58601=EDGE_CURVE('',#44293,#44304,#36030,.T.);
#58602=EDGE_CURVE('',#44294,#44115,#36031,.T.);
#58603=EDGE_CURVE('',#44305,#44092,#36032,.T.);
#58604=EDGE_CURVE('',#44118,#44296,#36033,.T.);
#58605=EDGE_CURVE('',#44097,#44298,#36034,.T.);
#58606=EDGE_CURVE('',#44295,#44119,#36035,.T.);
#58607=EDGE_CURVE('',#44297,#44282,#36036,.T.);
#58608=EDGE_CURVE('',#44122,#44283,#36037,.T.);
#58609=EDGE_CURVE('',#44125,#44285,#36038,.T.);
#58610=EDGE_CURVE('',#44300,#44284,#36039,.T.);
#58611=EDGE_CURVE('',#44299,#44286,#36040,.T.);
#58612=EDGE_CURVE('',#44128,#44287,#36041,.T.);
#58613=EDGE_CURVE('',#44196,#44194,#36042,.T.);
#58614=EDGE_CURVE('',#44197,#44193,#5343,.T.);
#58615=EDGE_CURVE('',#44191,#44205,#36043,.T.);
#58616=EDGE_CURVE('',#44204,#44192,#5344,.T.);
#58617=EDGE_CURVE('',#44306,#44307,#36044,.T.);
#58618=EDGE_CURVE('',#44308,#44309,#36045,.T.);
#58619=EDGE_CURVE('',#44308,#44310,#36046,.T.);
#58620=EDGE_CURVE('',#44310,#44310,#36047,.T.);
#58621=EDGE_CURVE('',#44309,#44308,#36048,.T.);
#58622=EDGE_CURVE('',#44311,#44312,#36049,.T.);
#58623=EDGE_CURVE('',#44311,#44313,#36050,.T.);
#58624=EDGE_CURVE('',#44313,#44313,#36051,.T.);
#58625=EDGE_CURVE('',#44312,#44311,#36052,.T.);
#58626=EDGE_CURVE('',#44314,#44315,#5345,.T.);
#58627=EDGE_CURVE('',#44314,#44316,#36053,.T.);
#58628=EDGE_CURVE('',#44317,#44316,#5346,.T.);
#58629=EDGE_CURVE('',#44318,#44317,#36054,.T.);
#58630=EDGE_CURVE('',#44319,#44318,#36055,.T.);
#58631=EDGE_CURVE('',#44315,#44319,#5347,.T.);
#58632=EDGE_CURVE('',#44320,#44318,#5348,.T.);
#58633=EDGE_CURVE('',#44316,#44320,#5349,.T.);
#58634=EDGE_CURVE('',#44321,#44321,#36056,.T.);
#58635=EDGE_CURVE('',#44321,#44322,#24072,.T.);
#58636=EDGE_CURVE('',#44322,#44314,#36057,.T.);
#58637=EDGE_CURVE('',#44319,#44322,#5350,.T.);
#58638=EDGE_CURVE('',#44312,#44309,#24073,.T.);
#58639=EDGE_CURVE('',#44323,#44310,#36058,.T.);
#58640=EDGE_CURVE('',#44324,#44325,#36059,.T.);
#58641=EDGE_CURVE('',#44324,#44326,#36060,.T.);
#58642=EDGE_CURVE('',#44326,#44326,#36061,.T.);
#58643=EDGE_CURVE('',#44325,#44324,#36062,.T.);
#58644=EDGE_CURVE('',#44327,#44327,#36063,.T.);
#58645=EDGE_CURVE('',#44327,#44328,#36064,.T.);
#58646=EDGE_CURVE('',#44329,#44328,#36065,.T.);
#58647=EDGE_CURVE('',#44328,#44329,#36066,.T.);
#58648=EDGE_CURVE('',#44330,#44330,#5351,.T.);
#58649=EDGE_CURVE('',#44330,#44331,#24074,.T.);
#58650=EDGE_CURVE('',#44331,#44332,#5352,.T.);
#58651=EDGE_CURVE('',#44332,#44331,#5353,.T.);
#58652=EDGE_CURVE('',#44333,#44333,#36067,.T.);
#58653=EDGE_CURVE('',#44333,#44325,#24075,.T.);
#58654=EDGE_CURVE('',#44329,#44334,#24076,.T.);
#58655=EDGE_CURVE('',#44334,#44334,#36068,.T.);
#58656=EDGE_CURVE('',#44335,#44335,#36069,.T.);
#58657=EDGE_CURVE('',#44335,#44336,#36070,.T.);
#58658=EDGE_CURVE('',#44336,#44336,#36071,.T.);
#58659=EDGE_CURVE('',#44337,#44337,#36072,.T.);
#58660=EDGE_CURVE('',#44337,#44338,#36073,.T.);
#58661=EDGE_CURVE('',#44339,#44338,#36074,.T.);
#58662=EDGE_CURVE('',#44338,#44339,#36075,.T.);
#58663=EDGE_CURVE('',#44340,#44341,#36076,.T.);
#58664=EDGE_CURVE('',#44341,#44340,#36077,.T.);
#58665=EDGE_CURVE('',#44341,#44342,#36078,.T.);
#58666=EDGE_CURVE('',#44342,#44342,#36079,.T.);
#58667=EDGE_CURVE('',#44343,#44343,#36080,.T.);
#58668=EDGE_CURVE('',#44343,#44344,#36081,.T.);
#58669=EDGE_CURVE('',#44344,#44344,#36082,.T.);
#58670=EDGE_CURVE('',#44345,#44345,#36083,.T.);
#58671=EDGE_CURVE('',#44345,#44346,#36084,.T.);
#58672=EDGE_CURVE('',#44346,#44346,#36085,.T.);
#58673=EDGE_CURVE('',#44347,#44347,#36086,.T.);
#58674=EDGE_CURVE('',#44347,#44348,#24077,.T.);
#58675=EDGE_CURVE('',#44348,#44348,#36087,.T.);
#58676=EDGE_CURVE('',#44336,#44343,#24078,.T.);
#58677=EDGE_CURVE('',#44346,#44347,#24079,.T.);
#58678=EDGE_CURVE('',#44349,#44349,#36088,.T.);
#58679=EDGE_CURVE('',#44349,#44339,#24080,.T.);
#58680=EDGE_CURVE('',#44340,#44350,#24081,.T.);
#58681=EDGE_CURVE('',#44350,#44350,#36089,.T.);
#58682=EDGE_CURVE('',#44351,#44351,#36090,.T.);
#58683=EDGE_CURVE('',#44351,#44352,#24082,.T.);
#58684=EDGE_CURVE('',#44352,#44352,#36091,.T.);
#58685=EDGE_CURVE('',#44353,#44354,#24083,.T.);
#58686=EDGE_CURVE('',#44353,#44355,#4109,.T.);
#58687=EDGE_CURVE('',#44355,#44356,#2500,.T.);
#58688=EDGE_CURVE('',#44354,#44356,#4110,.T.);
#58689=EDGE_CURVE('',#44357,#44358,#24084,.T.);
#58690=EDGE_CURVE('',#44357,#44353,#4111,.T.);
#58691=EDGE_CURVE('',#44358,#44354,#4112,.T.);
#58692=EDGE_CURVE('',#44359,#44360,#24085,.T.);
#58693=EDGE_CURVE('',#44359,#44357,#4113,.T.);
#58694=EDGE_CURVE('',#44360,#44358,#4114,.T.);
#58695=EDGE_CURVE('',#44361,#44362,#24086,.T.);
#58696=EDGE_CURVE('',#44361,#44359,#4115,.T.);
#58697=EDGE_CURVE('',#44362,#44360,#4116,.T.);
#58698=EDGE_CURVE('',#44363,#44364,#24087,.T.);
#58699=EDGE_CURVE('',#44363,#44361,#4117,.T.);
#58700=EDGE_CURVE('',#44364,#44362,#4118,.T.);
#58701=EDGE_CURVE('',#44365,#44366,#24088,.T.);
#58702=EDGE_CURVE('',#44365,#44363,#4119,.T.);
#58703=EDGE_CURVE('',#44366,#44364,#4120,.T.);
#58704=EDGE_CURVE('',#44367,#44368,#24089,.T.);
#58705=EDGE_CURVE('',#44369,#44367,#5354,.F.);
#58706=EDGE_CURVE('',#44369,#44368,#36092,.T.);
#58707=EDGE_CURVE('',#44370,#44371,#24090,.T.);
#58708=EDGE_CURVE('',#44367,#44370,#5355,.F.);
#58709=EDGE_CURVE('',#44368,#44372,#36093,.T.);
#58710=EDGE_CURVE('',#44371,#44372,#5356,.F.);
#58711=EDGE_CURVE('',#44373,#44374,#24091,.T.);
#58712=EDGE_CURVE('',#44370,#44373,#5357,.F.);
#58713=EDGE_CURVE('',#44374,#44371,#5358,.F.);
#58714=EDGE_CURVE('',#44375,#44376,#24092,.T.);
#58715=EDGE_CURVE('',#44373,#44375,#5359,.F.);
#58716=EDGE_CURVE('',#44376,#44374,#5360,.F.);
#58717=EDGE_CURVE('',#44377,#44378,#24093,.T.);
#58718=EDGE_CURVE('',#44375,#44377,#5361,.F.);
#58719=EDGE_CURVE('',#44378,#44376,#5362,.F.);
#58720=EDGE_CURVE('',#44379,#44380,#24094,.T.);
#58721=EDGE_CURVE('',#44377,#44379,#5363,.F.);
#58722=EDGE_CURVE('',#44380,#44378,#5364,.F.);
#58723=EDGE_CURVE('',#44381,#44382,#24095,.T.);
#58724=EDGE_CURVE('',#44379,#44381,#5365,.F.);
#58725=EDGE_CURVE('',#44382,#44380,#5366,.F.);
#58726=EDGE_CURVE('',#44383,#44384,#24096,.T.);
#58727=EDGE_CURVE('',#44383,#44385,#36094,.T.);
#58728=EDGE_CURVE('',#44381,#44385,#5367,.F.);
#58729=EDGE_CURVE('',#44384,#44382,#5368,.F.);
#58730=EDGE_CURVE('',#44386,#44369,#36095,.T.);
#58731=EDGE_CURVE('',#44387,#44386,#36096,.T.);
#58732=EDGE_CURVE('',#44372,#44387,#36097,.T.);
#58733=EDGE_CURVE('',#44368,#44388,#24097,.T.);
#58734=EDGE_CURVE('',#44388,#44388,#36098,.T.);
#58735=EDGE_CURVE('',#44389,#44390,#36099,.T.);
#58736=EDGE_CURVE('',#44356,#44389,#36100,.T.);
#58737=EDGE_CURVE('',#44385,#44355,#36101,.T.);
#58738=EDGE_CURVE('',#44390,#44383,#36102,.T.);
#58739=EDGE_CURVE('',#44390,#44391,#24098,.T.);
#58740=EDGE_CURVE('',#44391,#44391,#36103,.T.);
#58741=EDGE_CURVE('',#44389,#44384,#5369,.F.);
#58742=EDGE_CURVE('',#44392,#44393,#36104,.T.);
#58743=EDGE_CURVE('',#44394,#44392,#36105,.T.);
#58744=EDGE_CURVE('',#44395,#44394,#36106,.T.);
#58745=EDGE_CURVE('',#44396,#44395,#36107,.T.);
#58746=EDGE_CURVE('',#44397,#44396,#36108,.T.);
#58747=EDGE_CURVE('',#44393,#44397,#36109,.T.);
#58748=EDGE_CURVE('',#44392,#44393,#4121,.T.);
#58749=EDGE_CURVE('',#44393,#44397,#4122,.T.);
#58750=EDGE_CURVE('',#44397,#44396,#4123,.T.);
#58751=EDGE_CURVE('',#44396,#44395,#4124,.T.);
#58752=EDGE_CURVE('',#44395,#44394,#4125,.T.);
#58753=EDGE_CURVE('',#44394,#44392,#4126,.T.);
#58754=EDGE_CURVE('',#44398,#44399,#24099,.T.);
#58755=EDGE_CURVE('',#44399,#44400,#24100,.T.);
#58756=EDGE_CURVE('',#44400,#44401,#24101,.T.);
#58757=EDGE_CURVE('',#44401,#44402,#24102,.T.);
#58758=EDGE_CURVE('',#44402,#44403,#24103,.T.);
#58759=EDGE_CURVE('',#44403,#44398,#24104,.T.);
#58760=EDGE_CURVE('',#44399,#44392,#24105,.T.);
#58761=EDGE_CURVE('',#44400,#44393,#24106,.T.);
#58762=EDGE_CURVE('',#44401,#44397,#24107,.T.);
#58763=EDGE_CURVE('',#44402,#44396,#24108,.T.);
#58764=EDGE_CURVE('',#44403,#44395,#24109,.T.);
#58765=EDGE_CURVE('',#44398,#44394,#24110,.T.);
#58766=EDGE_CURVE('',#44387,#44366,#4127,.T.);
#58767=EDGE_CURVE('',#44386,#44365,#4128,.T.);
#58768=EDGE_CURVE('',#44404,#44405,#24111,.T.);
#58769=EDGE_CURVE('',#44404,#44406,#4129,.T.);
#58770=EDGE_CURVE('',#44406,#44407,#36110,.T.);
#58771=EDGE_CURVE('',#44405,#44407,#4130,.T.);
#58772=EDGE_CURVE('',#44408,#44409,#24112,.T.);
#58773=EDGE_CURVE('',#44408,#44404,#4131,.T.);
#58774=EDGE_CURVE('',#44409,#44405,#4132,.T.);
#58775=EDGE_CURVE('',#44410,#44411,#24113,.T.);
#58776=EDGE_CURVE('',#44410,#44408,#4133,.T.);
#58777=EDGE_CURVE('',#44411,#44409,#4134,.T.);
#58778=EDGE_CURVE('',#44412,#44413,#24114,.T.);
#58779=EDGE_CURVE('',#44412,#44410,#4135,.T.);
#58780=EDGE_CURVE('',#44413,#44411,#4136,.T.);
#58781=EDGE_CURVE('',#44414,#44415,#24115,.T.);
#58782=EDGE_CURVE('',#44414,#44412,#4137,.T.);
#58783=EDGE_CURVE('',#44415,#44413,#4138,.T.);
#58784=EDGE_CURVE('',#44416,#44417,#24116,.T.);
#58785=EDGE_CURVE('',#44416,#44414,#4139,.T.);
#58786=EDGE_CURVE('',#44417,#44415,#4140,.T.);
#58787=EDGE_CURVE('',#44418,#44419,#24117,.T.);
#58788=EDGE_CURVE('',#44420,#44418,#5370,.F.);
#58789=EDGE_CURVE('',#44420,#44419,#36111,.T.);
#58790=EDGE_CURVE('',#44421,#44422,#24118,.T.);
#58791=EDGE_CURVE('',#44418,#44421,#5371,.F.);
#58792=EDGE_CURVE('',#44419,#44423,#36112,.T.);
#58793=EDGE_CURVE('',#44422,#44423,#5372,.F.);
#58794=EDGE_CURVE('',#44424,#44425,#24119,.T.);
#58795=EDGE_CURVE('',#44421,#44424,#5373,.F.);
#58796=EDGE_CURVE('',#44425,#44422,#5374,.F.);
#58797=EDGE_CURVE('',#44426,#44427,#24120,.T.);
#58798=EDGE_CURVE('',#44424,#44426,#5375,.F.);
#58799=EDGE_CURVE('',#44427,#44425,#5376,.F.);
#58800=EDGE_CURVE('',#44428,#44429,#24121,.T.);
#58801=EDGE_CURVE('',#44426,#44428,#5377,.F.);
#58802=EDGE_CURVE('',#44429,#44427,#5378,.F.);
#58803=EDGE_CURVE('',#44430,#44431,#24122,.T.);
#58804=EDGE_CURVE('',#44428,#44430,#5379,.F.);
#58805=EDGE_CURVE('',#44431,#44429,#5380,.F.);
#58806=EDGE_CURVE('',#44432,#44433,#24123,.T.);
#58807=EDGE_CURVE('',#44430,#44432,#5381,.F.);
#58808=EDGE_CURVE('',#44433,#44431,#5382,.F.);
#58809=EDGE_CURVE('',#44434,#44435,#24124,.T.);
#58810=EDGE_CURVE('',#44434,#44436,#36113,.T.);
#58811=EDGE_CURVE('',#44432,#44436,#5383,.F.);
#58812=EDGE_CURVE('',#44435,#44433,#5384,.F.);
#58813=EDGE_CURVE('',#44437,#44420,#36114,.T.);
#58814=EDGE_CURVE('',#44438,#44437,#36115,.T.);
#58815=EDGE_CURVE('',#44423,#44438,#36116,.T.);
#58816=EDGE_CURVE('',#44419,#44439,#24125,.T.);
#58817=EDGE_CURVE('',#44439,#44439,#36117,.T.);
#58818=EDGE_CURVE('',#44440,#44441,#36118,.T.);
#58819=EDGE_CURVE('',#44407,#44440,#36119,.T.);
#58820=EDGE_CURVE('',#44436,#44406,#36120,.T.);
#58821=EDGE_CURVE('',#44441,#44434,#36121,.T.);
#58822=EDGE_CURVE('',#44441,#44442,#24126,.T.);
#58823=EDGE_CURVE('',#44442,#44442,#36122,.T.);
#58824=EDGE_CURVE('',#44440,#44435,#5385,.F.);
#58825=EDGE_CURVE('',#44443,#44444,#36123,.T.);
#58826=EDGE_CURVE('',#44445,#44443,#36124,.T.);
#58827=EDGE_CURVE('',#44446,#44445,#36125,.T.);
#58828=EDGE_CURVE('',#44447,#44446,#36126,.T.);
#58829=EDGE_CURVE('',#44448,#44447,#36127,.T.);
#58830=EDGE_CURVE('',#44444,#44448,#36128,.T.);
#58831=EDGE_CURVE('',#44443,#44444,#4141,.T.);
#58832=EDGE_CURVE('',#44444,#44448,#4142,.T.);
#58833=EDGE_CURVE('',#44448,#44447,#4143,.T.);
#58834=EDGE_CURVE('',#44447,#44446,#4144,.T.);
#58835=EDGE_CURVE('',#44446,#44445,#4145,.T.);
#58836=EDGE_CURVE('',#44445,#44443,#4146,.T.);
#58837=EDGE_CURVE('',#44449,#44450,#24127,.T.);
#58838=EDGE_CURVE('',#44450,#44451,#24128,.T.);
#58839=EDGE_CURVE('',#44451,#44452,#24129,.T.);
#58840=EDGE_CURVE('',#44452,#44453,#24130,.T.);
#58841=EDGE_CURVE('',#44453,#44454,#24131,.T.);
#58842=EDGE_CURVE('',#44454,#44449,#24132,.T.);
#58843=EDGE_CURVE('',#44450,#44443,#24133,.T.);
#58844=EDGE_CURVE('',#44451,#44444,#24134,.T.);
#58845=EDGE_CURVE('',#44452,#44448,#24135,.T.);
#58846=EDGE_CURVE('',#44453,#44447,#24136,.T.);
#58847=EDGE_CURVE('',#44454,#44446,#24137,.T.);
#58848=EDGE_CURVE('',#44449,#44445,#24138,.T.);
#58849=EDGE_CURVE('',#44438,#44417,#4147,.T.);
#58850=EDGE_CURVE('',#44437,#44416,#4148,.T.);
#58851=EDGE_CURVE('',#44455,#44455,#36129,.T.);
#58852=EDGE_CURVE('',#44455,#44456,#24139,.T.);
#58853=EDGE_CURVE('',#44456,#44456,#36130,.T.);
#58854=EDGE_CURVE('',#44457,#44458,#36131,.T.);
#58855=EDGE_CURVE('',#44458,#44457,#36132,.T.);
#58856=EDGE_CURVE('',#44458,#44459,#24140,.T.);
#58857=EDGE_CURVE('',#44459,#44459,#36133,.T.);
#58858=EDGE_CURVE('',#44460,#44460,#36134,.T.);
#58859=EDGE_CURVE('',#44460,#44461,#24141,.T.);
#58860=EDGE_CURVE('',#44461,#44461,#36135,.T.);
#58861=EDGE_CURVE('',#44462,#44463,#36136,.T.);
#58862=EDGE_CURVE('',#44463,#44462,#36137,.T.);
#58863=EDGE_CURVE('',#44463,#44464,#24142,.T.);
#58864=EDGE_CURVE('',#44464,#44464,#36138,.T.);
#58865=EDGE_CURVE('',#44462,#44465,#24143,.T.);
#58866=EDGE_CURVE('',#44466,#44465,#5386,.T.);
#58867=EDGE_CURVE('',#44466,#44460,#24144,.T.);
#58868=EDGE_CURVE('',#44465,#44466,#5387,.T.);
#58869=EDGE_CURVE('',#44467,#44468,#5388,.T.);
#58870=EDGE_CURVE('',#44468,#44467,#5389,.T.);
#58871=EDGE_CURVE('',#44468,#44469,#24145,.T.);
#58872=EDGE_CURVE('',#44469,#44469,#5390,.T.);
#58873=EDGE_CURVE('',#44466,#44470,#24146,.T.);
#58874=EDGE_CURVE('',#44471,#44470,#5391,.T.);
#58875=EDGE_CURVE('',#44470,#44471,#5392,.T.);
#58876=EDGE_CURVE('',#44457,#44470,#24147,.T.);
#58877=EDGE_CURVE('',#44471,#44455,#24148,.T.);
#58878=EDGE_CURVE('',#44472,#44472,#36139,.T.);
#58879=EDGE_CURVE('',#44472,#44473,#24149,.T.);
#58880=EDGE_CURVE('',#44473,#44473,#36140,.T.);
#58881=EDGE_CURVE('',#44474,#44474,#36141,.T.);
#58882=EDGE_CURVE('',#44474,#44475,#24150,.T.);
#58883=EDGE_CURVE('',#44475,#44475,#36142,.T.);
#58884=EDGE_CURVE('',#44476,#44476,#36143,.T.);
#58885=EDGE_CURVE('',#44476,#44477,#36144,.T.);
#58886=EDGE_CURVE('',#44478,#44477,#36145,.T.);
#58887=EDGE_CURVE('',#44477,#44478,#36146,.T.);
#58888=EDGE_CURVE('',#44479,#44479,#36147,.T.);
#58889=EDGE_CURVE('',#44479,#44478,#24151,.T.);
#58890=EDGE_CURVE('',#44480,#44481,#36148,.T.);
#58891=EDGE_CURVE('',#44482,#44481,#24152,.T.);
#58892=EDGE_CURVE('',#44482,#44483,#36149,.T.);
#58893=EDGE_CURVE('',#44483,#44480,#24153,.T.);
#58894=EDGE_CURVE('',#44484,#44484,#36150,.T.);
#58895=EDGE_CURVE('',#44484,#44485,#24154,.T.);
#58896=EDGE_CURVE('',#44485,#44485,#36151,.T.);
#58897=EDGE_CURVE('',#44486,#44486,#36152,.T.);
#58898=EDGE_CURVE('',#44486,#44487,#24155,.T.);
#58899=EDGE_CURVE('',#44487,#44487,#36153,.T.);
#58900=EDGE_CURVE('',#44488,#44488,#36154,.T.);
#58901=EDGE_CURVE('',#44488,#44489,#24156,.T.);
#58902=EDGE_CURVE('',#44489,#44489,#36155,.T.);
#58903=EDGE_CURVE('',#44490,#44490,#36156,.T.);
#58904=EDGE_CURVE('',#44490,#44491,#24157,.T.);
#58905=EDGE_CURVE('',#44491,#44491,#36157,.T.);
#58906=EDGE_CURVE('',#44492,#44492,#36158,.T.);
#58907=EDGE_CURVE('',#44492,#44493,#24158,.T.);
#58908=EDGE_CURVE('',#44493,#44493,#36159,.T.);
#58909=EDGE_CURVE('',#44494,#44494,#36160,.T.);
#58910=EDGE_CURVE('',#44494,#44495,#24159,.T.);
#58911=EDGE_CURVE('',#44495,#44495,#36161,.T.);
#58912=EDGE_CURVE('',#44496,#44496,#36162,.T.);
#58913=EDGE_CURVE('',#44496,#44497,#24160,.T.);
#58914=EDGE_CURVE('',#44497,#44497,#36163,.T.);
#58915=EDGE_CURVE('',#44498,#44498,#36164,.T.);
#58916=EDGE_CURVE('',#44498,#44499,#24161,.T.);
#58917=EDGE_CURVE('',#44499,#44499,#36165,.T.);
#58918=EDGE_CURVE('',#44500,#44500,#36166,.T.);
#58919=EDGE_CURVE('',#44500,#44501,#24162,.T.);
#58920=EDGE_CURVE('',#44501,#44501,#36167,.T.);
#58921=EDGE_CURVE('',#44502,#44502,#36168,.T.);
#58922=EDGE_CURVE('',#44502,#44503,#24163,.T.);
#58923=EDGE_CURVE('',#44503,#44503,#36169,.T.);
#58924=EDGE_CURVE('',#44504,#44505,#24164,.T.);
#58925=EDGE_CURVE('',#44505,#44506,#36170,.T.);
#58926=EDGE_CURVE('',#44507,#44506,#24165,.T.);
#58927=EDGE_CURVE('',#44504,#44507,#36171,.T.);
#58928=EDGE_CURVE('',#44506,#44508,#24166,.T.);
#58929=EDGE_CURVE('',#44509,#44508,#24167,.T.);
#58930=EDGE_CURVE('',#44507,#44509,#24168,.T.);
#58931=EDGE_CURVE('',#44508,#44510,#36172,.T.);
#58932=EDGE_CURVE('',#44511,#44510,#24169,.T.);
#58933=EDGE_CURVE('',#44509,#44511,#36173,.T.);
#58934=EDGE_CURVE('',#44510,#44512,#24170,.T.);
#58935=EDGE_CURVE('',#44513,#44512,#24171,.T.);
#58936=EDGE_CURVE('',#44511,#44513,#24172,.T.);
#58937=EDGE_CURVE('',#44512,#44514,#36174,.T.);
#58938=EDGE_CURVE('',#44515,#44514,#24173,.T.);
#58939=EDGE_CURVE('',#44513,#44515,#36175,.T.);
#58940=EDGE_CURVE('',#44514,#44516,#24174,.T.);
#58941=EDGE_CURVE('',#44517,#44516,#24175,.T.);
#58942=EDGE_CURVE('',#44515,#44517,#24176,.T.);
#58943=EDGE_CURVE('',#44516,#44518,#36176,.T.);
#58944=EDGE_CURVE('',#44519,#44518,#24177,.T.);
#58945=EDGE_CURVE('',#44517,#44519,#36177,.T.);
#58946=EDGE_CURVE('',#44518,#44505,#24178,.T.);
#58947=EDGE_CURVE('',#44519,#44504,#24179,.T.);
#58948=EDGE_CURVE('',#44520,#44521,#24180,.T.);
#58949=EDGE_CURVE('',#44521,#44522,#36178,.T.);
#58950=EDGE_CURVE('',#44522,#44523,#24181,.T.);
#58951=EDGE_CURVE('',#44523,#44524,#36179,.T.);
#58952=EDGE_CURVE('',#44524,#44525,#24182,.T.);
#58953=EDGE_CURVE('',#44525,#44526,#36180,.T.);
#58954=EDGE_CURVE('',#44526,#44527,#24183,.T.);
#58955=EDGE_CURVE('',#44527,#44520,#36181,.T.);
#58956=EDGE_CURVE('',#44528,#44529,#36182,.T.);
#58957=EDGE_CURVE('',#44530,#44528,#24184,.T.);
#58958=EDGE_CURVE('',#44531,#44530,#36183,.T.);
#58959=EDGE_CURVE('',#44532,#44531,#24185,.T.);
#58960=EDGE_CURVE('',#44533,#44532,#36184,.T.);
#58961=EDGE_CURVE('',#44534,#44533,#24186,.T.);
#58962=EDGE_CURVE('',#44535,#44534,#36185,.T.);
#58963=EDGE_CURVE('',#44529,#44535,#24187,.T.);
#58964=EDGE_CURVE('',#44536,#44529,#24188,.T.);
#58965=EDGE_CURVE('',#44537,#44536,#36186,.T.);
#58966=EDGE_CURVE('',#44537,#44528,#24189,.T.);
#58967=EDGE_CURVE('',#44538,#44535,#24190,.T.);
#58968=EDGE_CURVE('',#44536,#44538,#24191,.T.);
#58969=EDGE_CURVE('',#44539,#44534,#24192,.T.);
#58970=EDGE_CURVE('',#44538,#44539,#36187,.T.);
#58971=EDGE_CURVE('',#44540,#44533,#24193,.T.);
#58972=EDGE_CURVE('',#44539,#44540,#24194,.T.);
#58973=EDGE_CURVE('',#44541,#44532,#24195,.T.);
#58974=EDGE_CURVE('',#44540,#44541,#36188,.T.);
#58975=EDGE_CURVE('',#44542,#44531,#24196,.T.);
#58976=EDGE_CURVE('',#44541,#44542,#24197,.T.);
#58977=EDGE_CURVE('',#44543,#44530,#24198,.T.);
#58978=EDGE_CURVE('',#44542,#44543,#36189,.T.);
#58979=EDGE_CURVE('',#44543,#44537,#24199,.T.);
#58980=EDGE_CURVE('',#44526,#44512,#36190,.T.);
#58981=EDGE_CURVE('',#44514,#44525,#36191,.T.);
#58982=EDGE_CURVE('',#44516,#44524,#36192,.T.);
#58983=EDGE_CURVE('',#44527,#44510,#36193,.T.);
#58984=EDGE_CURVE('',#44518,#44523,#36194,.T.);
#58985=EDGE_CURVE('',#44520,#44508,#36195,.T.);
#58986=EDGE_CURVE('',#44505,#44522,#36196,.T.);
#58987=EDGE_CURVE('',#44521,#44506,#36197,.T.);
#58988=EDGE_CURVE('',#44544,#44545,#24200,.T.);
#58989=EDGE_CURVE('',#44545,#44546,#36198,.T.);
#58990=EDGE_CURVE('',#44547,#44546,#24201,.T.);
#58991=EDGE_CURVE('',#44547,#44544,#36199,.T.);
#58992=EDGE_CURVE('',#44545,#44548,#24202,.T.);
#58993=EDGE_CURVE('',#44548,#44549,#36200,.T.);
#58994=EDGE_CURVE('',#44549,#44481,#24203,.T.);
#58995=EDGE_CURVE('',#44550,#44480,#24204,.T.);
#58996=EDGE_CURVE('',#44551,#44550,#36201,.T.);
#58997=EDGE_CURVE('',#44546,#44551,#24205,.T.);
#58998=EDGE_CURVE('',#44552,#44550,#24206,.T.);
#58999=EDGE_CURVE('',#44553,#44552,#36202,.T.);
#59000=EDGE_CURVE('',#44553,#44551,#24207,.T.);
#59001=EDGE_CURVE('',#44547,#44553,#24208,.T.);
#59002=EDGE_CURVE('',#44552,#44483,#24209,.T.);
#59003=EDGE_CURVE('',#44554,#44482,#24210,.T.);
#59004=EDGE_CURVE('',#44555,#44554,#36203,.T.);
#59005=EDGE_CURVE('',#44544,#44555,#24211,.T.);
#59006=EDGE_CURVE('',#44555,#44548,#24212,.T.);
#59007=EDGE_CURVE('',#44554,#44549,#24213,.T.);
#59008=EDGE_CURVE('',#44556,#44557,#5393,.T.);
#59009=EDGE_CURVE('',#44558,#44556,#4149,.T.);
#59010=EDGE_CURVE('',#44558,#44559,#24214,.T.);
#59011=EDGE_CURVE('',#44559,#44557,#4150,.T.);
#59012=EDGE_CURVE('',#44560,#44556,#24215,.T.);
#59013=EDGE_CURVE('',#44561,#44560,#4151,.T.);
#59014=EDGE_CURVE('',#44561,#44558,#24216,.T.);
#59015=EDGE_CURVE('',#44562,#44560,#5394,.T.);
#59016=EDGE_CURVE('',#44563,#44562,#4152,.T.);
#59017=EDGE_CURVE('',#44563,#44561,#24217,.T.);
#59018=EDGE_CURVE('',#44557,#44562,#24218,.T.);
#59019=EDGE_CURVE('',#44559,#44563,#24219,.T.);
#59020=EDGE_CURVE('',#44564,#44565,#5395,.T.);
#59021=EDGE_CURVE('',#44566,#44564,#4153,.T.);
#59022=EDGE_CURVE('',#44566,#44567,#24220,.T.);
#59023=EDGE_CURVE('',#44567,#44565,#4154,.T.);
#59024=EDGE_CURVE('',#44568,#44564,#24221,.T.);
#59025=EDGE_CURVE('',#44569,#44568,#4155,.T.);
#59026=EDGE_CURVE('',#44569,#44566,#24222,.T.);
#59027=EDGE_CURVE('',#44570,#44568,#5396,.T.);
#59028=EDGE_CURVE('',#44571,#44570,#4156,.T.);
#59029=EDGE_CURVE('',#44571,#44569,#24223,.T.);
#59030=EDGE_CURVE('',#44565,#44570,#24224,.T.);
#59031=EDGE_CURVE('',#44567,#44571,#24225,.T.);
#59032=EDGE_CURVE('',#44572,#44572,#36204,.T.);
#59033=EDGE_CURVE('',#44572,#44573,#24226,.T.);
#59034=EDGE_CURVE('',#44573,#44573,#36205,.T.);
#59035=EDGE_CURVE('',#44574,#44572,#24227,.T.);
#59036=EDGE_CURVE('',#44575,#44575,#5397,.T.);
#59037=EDGE_CURVE('',#44575,#44576,#24228,.T.);
#59038=EDGE_CURVE('',#44576,#44576,#36206,.T.);
#59039=EDGE_CURVE('',#44577,#44578,#5398,.T.);
#59040=EDGE_CURVE('',#44578,#44579,#5399,.T.);
#59041=EDGE_CURVE('',#44579,#44580,#5400,.T.);
#59042=EDGE_CURVE('',#44580,#44577,#5401,.T.);
#59043=EDGE_CURVE('',#44581,#44582,#5402,.T.);
#59044=EDGE_CURVE('',#44581,#44583,#24229,.T.);
#59045=EDGE_CURVE('',#44583,#44583,#36207,.T.);
#59046=EDGE_CURVE('',#44582,#44581,#5403,.T.);
#59047=EDGE_CURVE('',#44584,#44585,#5404,.T.);
#59048=EDGE_CURVE('',#44585,#44586,#5405,.T.);
#59049=EDGE_CURVE('',#44586,#44587,#5406,.T.);
#59050=EDGE_CURVE('',#44587,#44584,#5407,.T.);
#59051=EDGE_CURVE('',#44588,#44589,#5408,.T.);
#59052=EDGE_CURVE('',#44589,#44590,#24230,.T.);
#59053=EDGE_CURVE('',#44590,#44590,#36208,.T.);
#59054=EDGE_CURVE('',#44589,#44588,#5409,.T.);
#59055=EDGE_CURVE('',#44591,#44592,#5410,.T.);
#59056=EDGE_CURVE('',#44593,#44591,#5411,.T.);
#59057=EDGE_CURVE('',#44594,#44593,#5412,.T.);
#59058=EDGE_CURVE('',#44592,#44594,#5413,.T.);
#59059=EDGE_CURVE('',#44595,#44596,#5414,.T.);
#59060=EDGE_CURVE('',#44596,#44597,#24231,.T.);
#59061=EDGE_CURVE('',#44597,#44597,#36209,.T.);
#59062=EDGE_CURVE('',#44596,#44595,#5415,.T.);
#59063=EDGE_CURVE('',#44598,#44599,#5416,.T.);
#59064=EDGE_CURVE('',#44600,#44598,#5417,.T.);
#59065=EDGE_CURVE('',#44601,#44600,#5418,.T.);
#59066=EDGE_CURVE('',#44599,#44601,#5419,.T.);
#59067=EDGE_CURVE('',#44602,#44603,#5420,.T.);
#59068=EDGE_CURVE('',#44602,#44604,#24232,.T.);
#59069=EDGE_CURVE('',#44604,#44604,#36210,.T.);
#59070=EDGE_CURVE('',#44603,#44602,#5421,.T.);
#59071=EDGE_CURVE('',#44605,#44606,#5422,.T.);
#59072=EDGE_CURVE('',#44606,#44607,#5423,.T.);
#59073=EDGE_CURVE('',#44607,#44608,#5424,.T.);
#59074=EDGE_CURVE('',#44608,#44605,#5425,.T.);
#59075=EDGE_CURVE('',#44609,#44610,#5426,.T.);
#59076=EDGE_CURVE('',#44611,#44609,#5427,.T.);
#59077=EDGE_CURVE('',#44612,#44611,#5428,.T.);
#59078=EDGE_CURVE('',#44610,#44612,#5429,.T.);
#59079=EDGE_CURVE('',#44613,#44614,#5430,.T.);
#59080=EDGE_CURVE('',#44614,#44615,#24233,.T.);
#59081=EDGE_CURVE('',#44615,#44615,#36211,.T.);
#59082=EDGE_CURVE('',#44614,#44613,#5431,.T.);
#59083=EDGE_CURVE('',#44616,#44617,#5432,.T.);
#59084=EDGE_CURVE('',#44617,#44618,#5433,.T.);
#59085=EDGE_CURVE('',#44618,#44619,#5434,.T.);
#59086=EDGE_CURVE('',#44619,#44616,#5435,.T.);
#59087=EDGE_CURVE('',#44620,#44621,#5436,.T.);
#59088=EDGE_CURVE('',#44622,#44620,#5437,.T.);
#59089=EDGE_CURVE('',#44623,#44622,#5438,.T.);
#59090=EDGE_CURVE('',#44621,#44623,#5439,.T.);
#59091=EDGE_CURVE('',#44582,#44596,#36212,.T.);
#59092=EDGE_CURVE('',#44595,#44602,#24234,.T.);
#59093=EDGE_CURVE('',#44603,#44589,#24235,.T.);
#59094=EDGE_CURVE('',#44588,#44624,#24236,.T.);
#59095=EDGE_CURVE('',#44624,#44624,#36213,.T.);
#59096=EDGE_CURVE('',#44596,#44582,#36214,.T.);
#59097=EDGE_CURVE('',#44578,#44618,#4157,.T.);
#59098=EDGE_CURVE('',#44579,#44617,#4158,.T.);
#59099=EDGE_CURVE('',#44580,#44616,#4159,.T.);
#59100=EDGE_CURVE('',#44577,#44619,#4160,.T.);
#59101=EDGE_CURVE('',#44625,#44626,#5440,.T.);
#59102=EDGE_CURVE('',#44627,#44625,#24237,.T.);
#59103=EDGE_CURVE('',#44627,#44628,#5441,.T.);
#59104=EDGE_CURVE('',#44628,#44625,#5442,.T.);
#59105=EDGE_CURVE('',#44629,#44625,#24238,.T.);
#59106=EDGE_CURVE('',#44626,#44629,#5443,.T.);
#59107=EDGE_CURVE('',#44626,#44629,#36215,.T.);
#59108=EDGE_CURVE('',#44627,#44628,#36216,.T.);
#59109=EDGE_CURVE('',#44620,#44585,#4161,.T.);
#59110=EDGE_CURVE('',#44621,#44586,#4162,.T.);
#59111=EDGE_CURVE('',#44622,#44584,#4163,.T.);
#59112=EDGE_CURVE('',#44623,#44587,#4164,.T.);
#59113=EDGE_CURVE('',#44591,#44610,#4165,.T.);
#59114=EDGE_CURVE('',#44592,#44609,#4166,.T.);
#59115=EDGE_CURVE('',#44593,#44612,#4167,.T.);
#59116=EDGE_CURVE('',#44594,#44611,#4168,.T.);
#59117=EDGE_CURVE('',#44608,#44598,#4169,.T.);
#59118=EDGE_CURVE('',#44605,#44599,#4170,.T.);
#59119=EDGE_CURVE('',#44607,#44600,#4171,.T.);
#59120=EDGE_CURVE('',#44606,#44601,#4172,.T.);
#59121=EDGE_CURVE('',#44630,#44631,#24239,.T.);
#59122=EDGE_CURVE('',#44632,#44630,#5444,.T.);
#59123=EDGE_CURVE('',#44631,#44632,#5445,.T.);
#59124=EDGE_CURVE('',#44633,#44631,#24240,.T.);
#59125=EDGE_CURVE('',#44633,#44634,#5446,.T.);
#59126=EDGE_CURVE('',#44634,#44631,#5447,.T.);
#59127=EDGE_CURVE('',#44634,#44633,#36217,.T.);
#59128=EDGE_CURVE('',#44630,#44632,#36218,.T.);
#59129=EDGE_CURVE('',#44635,#44636,#24241,.T.);
#59130=EDGE_CURVE('',#44635,#44637,#5448,.T.);
#59131=EDGE_CURVE('',#44637,#44636,#5449,.T.);
#59132=EDGE_CURVE('',#44637,#44635,#36219,.T.);
#59133=EDGE_CURVE('',#44638,#44639,#5450,.T.);
#59134=EDGE_CURVE('',#44639,#44640,#5451,.T.);
#59135=EDGE_CURVE('',#44638,#44640,#24242,.T.);
#59136=EDGE_CURVE('',#44638,#44639,#36220,.T.);
#59137=EDGE_CURVE('',#44641,#44642,#5452,.T.);
#59138=EDGE_CURVE('',#44643,#44641,#24243,.T.);
#59139=EDGE_CURVE('',#44642,#44643,#5453,.T.);
#59140=EDGE_CURVE('',#44642,#44643,#36221,.T.);
#59141=EDGE_CURVE('',#44644,#44645,#5454,.T.);
#59142=EDGE_CURVE('',#44646,#44644,#24244,.T.);
#59143=EDGE_CURVE('',#44645,#44646,#5455,.T.);
#59144=EDGE_CURVE('',#44646,#44645,#36222,.T.);
#59145=EDGE_CURVE('',#44647,#44648,#24245,.T.);
#59146=EDGE_CURVE('',#44649,#44647,#24246,.T.);
#59147=EDGE_CURVE('',#44650,#44649,#24247,.T.);
#59148=EDGE_CURVE('',#44648,#44650,#24248,.T.);
#59149=EDGE_CURVE('',#44651,#44652,#24249,.T.);
#59150=EDGE_CURVE('',#44652,#44653,#36223,.T.);
#59151=EDGE_CURVE('',#44654,#44653,#24250,.T.);
#59152=EDGE_CURVE('',#44655,#44654,#24251,.T.);
#59153=EDGE_CURVE('',#44656,#44655,#24252,.T.);
#59154=EDGE_CURVE('',#44656,#44651,#36224,.T.);
#59155=EDGE_CURVE('',#44657,#44658,#24253,.T.);
#59156=EDGE_CURVE('',#44658,#44659,#24254,.T.);
#59157=EDGE_CURVE('',#44659,#44660,#24255,.T.);
#59158=EDGE_CURVE('',#44661,#44660,#24256,.T.);
#59159=EDGE_CURVE('',#44661,#44649,#24257,.T.);
#59160=EDGE_CURVE('',#44662,#44647,#24258,.T.);
#59161=EDGE_CURVE('',#44657,#44662,#24259,.T.);
#59162=EDGE_CURVE('',#44663,#44664,#24260,.T.);
#59163=EDGE_CURVE('',#44664,#44665,#24261,.T.);
#59164=EDGE_CURVE('',#44665,#44666,#24262,.T.);
#59165=EDGE_CURVE('',#44663,#44666,#24263,.T.);
#59166=EDGE_CURVE('',#44667,#44668,#24264,.T.);
#59167=EDGE_CURVE('',#44668,#44669,#24265,.T.);
#59168=EDGE_CURVE('',#44669,#44670,#24266,.T.);
#59169=EDGE_CURVE('',#44671,#44670,#24267,.T.);
#59170=EDGE_CURVE('',#44671,#44648,#24268,.T.);
#59171=EDGE_CURVE('',#44672,#44650,#24269,.T.);
#59172=EDGE_CURVE('',#44667,#44672,#24270,.T.);
#59173=EDGE_CURVE('',#44673,#44674,#24271,.T.);
#59174=EDGE_CURVE('',#44674,#44675,#24272,.T.);
#59175=EDGE_CURVE('',#44675,#44676,#24273,.T.);
#59176=EDGE_CURVE('',#44673,#44676,#24274,.T.);
#59177=EDGE_CURVE('',#44677,#44678,#24275,.T.);
#59178=EDGE_CURVE('',#44678,#44679,#36225,.T.);
#59179=EDGE_CURVE('',#44679,#44680,#24276,.T.);
#59180=EDGE_CURVE('',#44680,#44681,#36226,.T.);
#59181=EDGE_CURVE('',#44681,#44682,#24277,.T.);
#59182=EDGE_CURVE('',#44682,#44683,#36227,.T.);
#59183=EDGE_CURVE('',#44683,#44684,#24278,.T.);
#59184=EDGE_CURVE('',#44684,#44677,#36228,.T.);
#59185=EDGE_CURVE('',#44685,#44686,#24279,.T.);
#59186=EDGE_CURVE('',#44686,#44687,#36229,.T.);
#59187=EDGE_CURVE('',#44687,#44688,#24280,.T.);
#59188=EDGE_CURVE('',#44688,#44689,#36230,.T.);
#59189=EDGE_CURVE('',#44689,#44690,#24281,.T.);
#59190=EDGE_CURVE('',#44690,#44691,#36231,.T.);
#59191=EDGE_CURVE('',#44691,#44692,#24282,.T.);
#59192=EDGE_CURVE('',#44692,#44685,#36232,.T.);
#59193=EDGE_CURVE('',#44693,#44694,#24283,.T.);
#59194=EDGE_CURVE('',#44694,#44695,#24284,.T.);
#59195=EDGE_CURVE('',#44695,#44696,#24285,.T.);
#59196=EDGE_CURVE('',#44696,#44693,#24286,.T.);
#59197=EDGE_CURVE('',#44697,#44698,#24287,.T.);
#59198=EDGE_CURVE('',#44698,#44699,#24288,.T.);
#59199=EDGE_CURVE('',#44699,#44700,#24289,.T.);
#59200=EDGE_CURVE('',#44700,#44697,#24290,.T.);
#59201=EDGE_CURVE('',#44701,#44702,#24291,.T.);
#59202=EDGE_CURVE('',#44702,#44703,#24292,.T.);
#59203=EDGE_CURVE('',#44703,#44704,#24293,.T.);
#59204=EDGE_CURVE('',#44704,#44701,#24294,.T.);
#59205=EDGE_CURVE('',#44705,#44706,#24295,.T.);
#59206=EDGE_CURVE('',#44706,#44707,#24296,.T.);
#59207=EDGE_CURVE('',#44707,#44708,#24297,.T.);
#59208=EDGE_CURVE('',#44708,#44705,#24298,.T.);
#59209=EDGE_CURVE('',#44659,#44674,#36233,.T.);
#59210=EDGE_CURVE('',#44660,#44673,#36234,.T.);
#59211=EDGE_CURVE('',#44669,#44664,#36235,.T.);
#59212=EDGE_CURVE('',#44670,#44663,#36236,.T.);
#59213=EDGE_CURVE('',#44665,#44658,#36237,.T.);
#59214=EDGE_CURVE('',#44666,#44657,#36238,.T.);
#59215=EDGE_CURVE('',#44675,#44668,#36239,.T.);
#59216=EDGE_CURVE('',#44676,#44667,#36240,.T.);
#59217=EDGE_CURVE('',#44658,#44682,#36241,.T.);
#59218=EDGE_CURVE('',#44683,#44665,#36242,.T.);
#59219=EDGE_CURVE('',#44684,#44664,#36243,.T.);
#59220=EDGE_CURVE('',#44659,#44681,#36244,.T.);
#59221=EDGE_CURVE('',#44677,#44669,#36245,.T.);
#59222=EDGE_CURVE('',#44674,#44680,#36246,.T.);
#59223=EDGE_CURVE('',#44678,#44668,#36247,.T.);
#59224=EDGE_CURVE('',#44675,#44679,#36248,.T.);
#59225=EDGE_CURVE('',#44707,#44694,#36249,.T.);
#59226=EDGE_CURVE('',#44693,#44709,#36250,.T.);
#59227=EDGE_CURVE('',#44709,#44708,#5456,.T.);
#59228=EDGE_CURVE('',#44703,#44706,#36251,.T.);
#59229=EDGE_CURVE('',#44705,#44710,#5457,.T.);
#59230=EDGE_CURVE('',#44710,#44704,#36252,.T.);
#59231=EDGE_CURVE('',#44695,#44700,#36253,.T.);
#59232=EDGE_CURVE('',#44699,#44711,#5458,.T.);
#59233=EDGE_CURVE('',#44711,#44696,#36254,.T.);
#59234=EDGE_CURVE('',#44697,#44702,#36255,.T.);
#59235=EDGE_CURVE('',#44701,#44712,#36256,.T.);
#59236=EDGE_CURVE('',#44712,#44698,#5459,.T.);
#59237=EDGE_CURVE('',#44713,#44654,#24299,.T.);
#59238=EDGE_CURVE('',#44714,#44713,#24300,.T.);
#59239=EDGE_CURVE('',#44714,#44655,#24301,.T.);
#59240=EDGE_CURVE('',#44653,#44715,#24302,.T.);
#59241=EDGE_CURVE('',#44715,#44716,#24303,.T.);
#59242=EDGE_CURVE('',#44716,#44717,#24304,.T.);
#59243=EDGE_CURVE('',#44717,#44718,#24305,.T.);
#59244=EDGE_CURVE('',#44719,#44718,#24306,.T.);
#59245=EDGE_CURVE('',#44713,#44719,#24307,.T.);
#59246=EDGE_CURVE('',#44718,#44720,#24308,.T.);
#59247=EDGE_CURVE('',#44721,#44720,#24309,.T.);
#59248=EDGE_CURVE('',#44719,#44721,#24310,.T.);
#59249=EDGE_CURVE('',#44720,#44722,#24311,.T.);
#59250=EDGE_CURVE('',#44722,#44723,#24312,.T.);
#59251=EDGE_CURVE('',#44723,#44724,#24313,.T.);
#59252=EDGE_CURVE('',#44724,#44656,#24314,.T.);
#59253=EDGE_CURVE('',#44721,#44714,#24315,.T.);
#59254=EDGE_CURVE('',#44725,#44726,#24316,.T.);
#59255=EDGE_CURVE('',#44726,#44722,#36257,.T.);
#59256=EDGE_CURVE('',#44717,#44725,#36258,.T.);
#59257=EDGE_CURVE('',#44706,#44690,#36259,.T.);
#59258=EDGE_CURVE('',#44691,#44703,#36260,.T.);
#59259=EDGE_CURVE('',#44692,#44702,#36261,.T.);
#59260=EDGE_CURVE('',#44707,#44689,#36262,.T.);
#59261=EDGE_CURVE('',#44685,#44697,#36263,.T.);
#59262=EDGE_CURVE('',#44694,#44688,#36264,.T.);
#59263=EDGE_CURVE('',#44686,#44700,#36265,.T.);
#59264=EDGE_CURVE('',#44695,#44687,#36266,.T.);
#59265=EDGE_CURVE('',#44704,#44726,#36267,.T.);
#59266=EDGE_CURVE('',#44722,#44710,#36268,.T.);
#59267=EDGE_CURVE('',#44723,#44705,#36269,.T.);
#59268=EDGE_CURVE('',#44701,#44725,#36270,.T.);
#59269=EDGE_CURVE('',#44724,#44708,#36271,.T.);
#59270=EDGE_CURVE('',#44712,#44717,#36272,.T.);
#59271=EDGE_CURVE('',#44656,#44709,#36273,.T.);
#59272=EDGE_CURVE('',#44698,#44716,#36274,.T.);
#59273=EDGE_CURVE('',#44651,#44693,#36275,.T.);
#59274=EDGE_CURVE('',#44699,#44715,#36276,.T.);
#59275=EDGE_CURVE('',#44652,#44696,#36277,.T.);
#59276=EDGE_CURVE('',#44711,#44653,#36278,.T.);
#59277=EDGE_CURVE('',#44727,#44728,#24317,.T.);
#59278=EDGE_CURVE('',#44729,#44727,#24318,.T.);
#59279=EDGE_CURVE('',#44730,#44729,#24319,.T.);
#59280=EDGE_CURVE('',#44728,#44730,#24320,.T.);
#59281=EDGE_CURVE('',#44731,#44728,#24321,.T.);
#59282=EDGE_CURVE('',#44732,#44731,#24322,.T.);
#59283=EDGE_CURVE('',#44732,#44727,#24323,.T.);
#59284=EDGE_CURVE('',#44733,#44730,#24324,.T.);
#59285=EDGE_CURVE('',#44731,#44733,#24325,.T.);
#59286=EDGE_CURVE('',#44734,#44729,#24326,.T.);
#59287=EDGE_CURVE('',#44733,#44734,#24327,.T.);
#59288=EDGE_CURVE('',#44734,#44732,#24328,.T.);
#59289=EDGE_CURVE('',#44672,#44661,#24329,.T.);
#59290=EDGE_CURVE('',#44662,#44671,#24330,.T.);
#59291=EDGE_CURVE('',#44735,#44736,#36279,.T.);
#59292=EDGE_CURVE('',#44736,#44737,#24331,.T.);
#59293=EDGE_CURVE('',#44738,#44737,#36280,.T.);
#59294=EDGE_CURVE('',#44735,#44738,#24332,.T.);
#59295=EDGE_CURVE('',#44739,#44740,#36281,.T.);
#59296=EDGE_CURVE('',#44740,#44741,#24333,.T.);
#59297=EDGE_CURVE('',#44741,#44742,#36282,.T.);
#59298=EDGE_CURVE('',#44742,#44743,#24334,.T.);
#59299=EDGE_CURVE('',#44743,#44744,#36283,.T.);
#59300=EDGE_CURVE('',#44744,#44745,#24335,.T.);
#59301=EDGE_CURVE('',#44745,#44746,#36284,.T.);
#59302=EDGE_CURVE('',#44746,#44747,#24336,.T.);
#59303=EDGE_CURVE('',#44747,#44748,#36285,.T.);
#59304=EDGE_CURVE('',#44748,#44749,#24337,.T.);
#59305=EDGE_CURVE('',#44749,#44750,#36286,.T.);
#59306=EDGE_CURVE('',#44750,#44751,#24338,.T.);
#59307=EDGE_CURVE('',#44751,#44752,#36287,.T.);
#59308=EDGE_CURVE('',#44752,#44738,#24339,.T.);
#59309=EDGE_CURVE('',#44737,#44739,#24340,.T.);
#59310=EDGE_CURVE('',#44736,#44753,#24341,.T.);
#59311=EDGE_CURVE('',#44753,#44739,#24342,.T.);
#59312=EDGE_CURVE('',#44754,#44752,#24343,.T.);
#59313=EDGE_CURVE('',#44754,#44735,#24344,.T.);
#59314=EDGE_CURVE('',#44755,#44751,#24345,.T.);
#59315=EDGE_CURVE('',#44755,#44754,#36288,.T.);
#59316=EDGE_CURVE('',#44756,#44750,#24346,.T.);
#59317=EDGE_CURVE('',#44756,#44755,#24347,.T.);
#59318=EDGE_CURVE('',#44757,#44749,#24348,.T.);
#59319=EDGE_CURVE('',#44757,#44756,#36289,.T.);
#59320=EDGE_CURVE('',#44758,#44748,#24349,.T.);
#59321=EDGE_CURVE('',#44758,#44757,#24350,.T.);
#59322=EDGE_CURVE('',#44759,#44747,#24351,.T.);
#59323=EDGE_CURVE('',#44759,#44758,#36290,.T.);
#59324=EDGE_CURVE('',#44760,#44746,#24352,.T.);
#59325=EDGE_CURVE('',#44760,#44759,#24353,.T.);
#59326=EDGE_CURVE('',#44761,#44745,#24354,.T.);
#59327=EDGE_CURVE('',#44761,#44760,#36291,.T.);
#59328=EDGE_CURVE('',#44762,#44744,#24355,.T.);
#59329=EDGE_CURVE('',#44762,#44761,#24356,.T.);
#59330=EDGE_CURVE('',#44763,#44743,#24357,.T.);
#59331=EDGE_CURVE('',#44763,#44762,#36292,.T.);
#59332=EDGE_CURVE('',#44764,#44742,#24358,.T.);
#59333=EDGE_CURVE('',#44764,#44763,#24359,.T.);
#59334=EDGE_CURVE('',#44765,#44741,#24360,.T.);
#59335=EDGE_CURVE('',#44765,#44764,#36293,.T.);
#59336=EDGE_CURVE('',#44766,#44740,#24361,.T.);
#59337=EDGE_CURVE('',#44766,#44765,#24362,.T.);
#59338=EDGE_CURVE('',#44753,#44766,#36294,.T.);
#59339=EDGE_CURVE('',#44767,#44768,#36295,.T.);
#59340=EDGE_CURVE('',#44768,#44769,#24363,.T.);
#59341=EDGE_CURVE('',#44769,#44770,#36296,.T.);
#59342=EDGE_CURVE('',#44770,#44771,#24364,.T.);
#59343=EDGE_CURVE('',#44771,#44772,#36297,.T.);
#59344=EDGE_CURVE('',#44772,#44773,#24365,.T.);
#59345=EDGE_CURVE('',#44773,#44774,#36298,.T.);
#59346=EDGE_CURVE('',#44774,#44767,#24366,.T.);
#59347=EDGE_CURVE('',#44775,#44774,#24367,.T.);
#59348=EDGE_CURVE('',#44775,#44776,#24368,.T.);
#59349=EDGE_CURVE('',#44776,#44767,#24369,.T.);
#59350=EDGE_CURVE('',#44777,#44773,#24370,.T.);
#59351=EDGE_CURVE('',#44777,#44775,#36299,.T.);
#59352=EDGE_CURVE('',#44778,#44772,#24371,.T.);
#59353=EDGE_CURVE('',#44778,#44777,#24372,.T.);
#59354=EDGE_CURVE('',#44779,#44771,#24373,.T.);
#59355=EDGE_CURVE('',#44779,#44778,#36300,.T.);
#59356=EDGE_CURVE('',#44780,#44770,#24374,.T.);
#59357=EDGE_CURVE('',#44780,#44779,#24375,.T.);
#59358=EDGE_CURVE('',#44781,#44769,#24376,.T.);
#59359=EDGE_CURVE('',#44781,#44780,#36301,.T.);
#59360=EDGE_CURVE('',#44782,#44768,#24377,.T.);
#59361=EDGE_CURVE('',#44782,#44781,#24378,.T.);
#59362=EDGE_CURVE('',#44776,#44782,#36302,.T.);
#59363=EDGE_CURVE('',#44783,#44784,#36303,.T.);
#59364=EDGE_CURVE('',#44784,#44785,#24379,.T.);
#59365=EDGE_CURVE('',#44785,#44786,#36304,.T.);
#59366=EDGE_CURVE('',#44786,#44787,#24380,.T.);
#59367=EDGE_CURVE('',#44787,#44788,#36305,.T.);
#59368=EDGE_CURVE('',#44788,#44789,#24381,.T.);
#59369=EDGE_CURVE('',#44789,#44790,#36306,.T.);
#59370=EDGE_CURVE('',#44790,#44791,#24382,.T.);
#59371=EDGE_CURVE('',#44791,#44792,#24383,.T.);
#59372=EDGE_CURVE('',#44792,#44793,#24384,.T.);
#59373=EDGE_CURVE('',#44793,#44794,#36307,.T.);
#59374=EDGE_CURVE('',#44794,#44795,#24385,.T.);
#59375=EDGE_CURVE('',#44795,#44796,#36308,.T.);
#59376=EDGE_CURVE('',#44796,#44797,#24386,.T.);
#59377=EDGE_CURVE('',#44797,#44798,#36309,.T.);
#59378=EDGE_CURVE('',#44798,#44799,#24387,.T.);
#59379=EDGE_CURVE('',#44799,#44800,#36310,.T.);
#59380=EDGE_CURVE('',#44800,#44801,#24388,.T.);
#59381=EDGE_CURVE('',#44801,#44802,#36311,.T.);
#59382=EDGE_CURVE('',#44802,#44803,#24389,.T.);
#59383=EDGE_CURVE('',#44803,#44804,#36312,.T.);
#59384=EDGE_CURVE('',#44804,#44805,#24390,.T.);
#59385=EDGE_CURVE('',#44805,#44806,#24391,.T.);
#59386=EDGE_CURVE('',#44806,#44807,#24392,.T.);
#59387=EDGE_CURVE('',#44807,#44808,#36313,.T.);
#59388=EDGE_CURVE('',#44808,#44809,#24393,.T.);
#59389=EDGE_CURVE('',#44809,#44810,#36314,.T.);
#59390=EDGE_CURVE('',#44810,#44811,#24394,.T.);
#59391=EDGE_CURVE('',#44811,#44812,#36315,.T.);
#59392=EDGE_CURVE('',#44812,#44813,#24395,.T.);
#59393=EDGE_CURVE('',#44813,#44814,#36316,.T.);
#59394=EDGE_CURVE('',#44814,#44815,#24396,.T.);
#59395=EDGE_CURVE('',#44815,#44816,#36317,.T.);
#59396=EDGE_CURVE('',#44816,#44817,#24397,.T.);
#59397=EDGE_CURVE('',#44817,#44818,#36318,.T.);
#59398=EDGE_CURVE('',#44818,#44819,#24398,.T.);
#59399=EDGE_CURVE('',#44819,#44820,#24399,.T.);
#59400=EDGE_CURVE('',#44820,#44821,#24400,.T.);
#59401=EDGE_CURVE('',#44821,#44822,#36319,.T.);
#59402=EDGE_CURVE('',#44822,#44823,#24401,.T.);
#59403=EDGE_CURVE('',#44823,#44824,#36320,.T.);
#59404=EDGE_CURVE('',#44824,#44825,#24402,.T.);
#59405=EDGE_CURVE('',#44825,#44826,#36321,.T.);
#59406=EDGE_CURVE('',#44826,#44827,#24403,.T.);
#59407=EDGE_CURVE('',#44827,#44828,#36322,.T.);
#59408=EDGE_CURVE('',#44828,#44829,#24404,.T.);
#59409=EDGE_CURVE('',#44829,#44830,#36323,.T.);
#59410=EDGE_CURVE('',#44830,#44831,#24405,.T.);
#59411=EDGE_CURVE('',#44831,#44832,#36324,.T.);
#59412=EDGE_CURVE('',#44832,#44833,#24406,.T.);
#59413=EDGE_CURVE('',#44833,#44834,#24407,.T.);
#59414=EDGE_CURVE('',#44834,#44835,#24408,.T.);
#59415=EDGE_CURVE('',#44835,#44836,#36325,.T.);
#59416=EDGE_CURVE('',#44836,#44837,#24409,.T.);
#59417=EDGE_CURVE('',#44837,#44838,#36326,.T.);
#59418=EDGE_CURVE('',#44838,#44783,#24410,.T.);
#59419=EDGE_CURVE('',#44839,#44840,#36327,.T.);
#59420=EDGE_CURVE('',#44841,#44839,#24411,.T.);
#59421=EDGE_CURVE('',#44842,#44841,#36328,.T.);
#59422=EDGE_CURVE('',#44843,#44842,#24412,.T.);
#59423=EDGE_CURVE('',#44844,#44843,#36329,.T.);
#59424=EDGE_CURVE('',#44845,#44844,#24413,.T.);
#59425=EDGE_CURVE('',#44846,#44845,#36330,.T.);
#59426=EDGE_CURVE('',#44847,#44846,#24414,.T.);
#59427=EDGE_CURVE('',#44848,#44847,#24415,.T.);
#59428=EDGE_CURVE('',#44849,#44848,#24416,.T.);
#59429=EDGE_CURVE('',#44850,#44849,#36331,.T.);
#59430=EDGE_CURVE('',#44851,#44850,#24417,.T.);
#59431=EDGE_CURVE('',#44852,#44851,#36332,.T.);
#59432=EDGE_CURVE('',#44853,#44852,#24418,.T.);
#59433=EDGE_CURVE('',#44854,#44853,#36333,.T.);
#59434=EDGE_CURVE('',#44855,#44854,#24419,.T.);
#59435=EDGE_CURVE('',#44856,#44855,#36334,.T.);
#59436=EDGE_CURVE('',#44857,#44856,#24420,.T.);
#59437=EDGE_CURVE('',#44858,#44857,#36335,.T.);
#59438=EDGE_CURVE('',#44859,#44858,#24421,.T.);
#59439=EDGE_CURVE('',#44860,#44859,#36336,.T.);
#59440=EDGE_CURVE('',#44861,#44860,#24422,.T.);
#59441=EDGE_CURVE('',#44862,#44861,#24423,.T.);
#59442=EDGE_CURVE('',#44863,#44862,#24424,.T.);
#59443=EDGE_CURVE('',#44864,#44863,#36337,.T.);
#59444=EDGE_CURVE('',#44865,#44864,#24425,.T.);
#59445=EDGE_CURVE('',#44866,#44865,#36338,.T.);
#59446=EDGE_CURVE('',#44867,#44866,#24426,.T.);
#59447=EDGE_CURVE('',#44868,#44867,#36339,.T.);
#59448=EDGE_CURVE('',#44869,#44868,#24427,.T.);
#59449=EDGE_CURVE('',#44870,#44869,#36340,.T.);
#59450=EDGE_CURVE('',#44871,#44870,#24428,.T.);
#59451=EDGE_CURVE('',#44872,#44871,#36341,.T.);
#59452=EDGE_CURVE('',#44873,#44872,#24429,.T.);
#59453=EDGE_CURVE('',#44874,#44873,#36342,.T.);
#59454=EDGE_CURVE('',#44875,#44874,#24430,.T.);
#59455=EDGE_CURVE('',#44876,#44875,#24431,.T.);
#59456=EDGE_CURVE('',#44877,#44876,#24432,.T.);
#59457=EDGE_CURVE('',#44878,#44877,#36343,.T.);
#59458=EDGE_CURVE('',#44879,#44878,#24433,.T.);
#59459=EDGE_CURVE('',#44880,#44879,#36344,.T.);
#59460=EDGE_CURVE('',#44881,#44880,#24434,.T.);
#59461=EDGE_CURVE('',#44882,#44881,#36345,.T.);
#59462=EDGE_CURVE('',#44883,#44882,#24435,.T.);
#59463=EDGE_CURVE('',#44884,#44883,#36346,.T.);
#59464=EDGE_CURVE('',#44885,#44884,#24436,.T.);
#59465=EDGE_CURVE('',#44886,#44885,#36347,.T.);
#59466=EDGE_CURVE('',#44887,#44886,#24437,.T.);
#59467=EDGE_CURVE('',#44888,#44887,#36348,.T.);
#59468=EDGE_CURVE('',#44889,#44888,#24438,.T.);
#59469=EDGE_CURVE('',#44890,#44889,#24439,.T.);
#59470=EDGE_CURVE('',#44891,#44890,#24440,.T.);
#59471=EDGE_CURVE('',#44892,#44891,#36349,.T.);
#59472=EDGE_CURVE('',#44893,#44892,#24441,.T.);
#59473=EDGE_CURVE('',#44894,#44893,#36350,.T.);
#59474=EDGE_CURVE('',#44840,#44894,#24442,.T.);
#59475=EDGE_CURVE('',#44783,#44842,#24443,.T.);
#59476=EDGE_CURVE('',#44784,#44841,#24444,.T.);
#59477=EDGE_CURVE('',#44838,#44843,#24445,.T.);
#59478=EDGE_CURVE('',#44837,#44844,#24446,.T.);
#59479=EDGE_CURVE('',#44836,#44845,#24447,.T.);
#59480=EDGE_CURVE('',#44835,#44846,#24448,.T.);
#59481=EDGE_CURVE('',#44834,#44847,#24449,.T.);
#59482=EDGE_CURVE('',#44833,#44848,#24450,.T.);
#59483=EDGE_CURVE('',#44832,#44849,#24451,.T.);
#59484=EDGE_CURVE('',#44831,#44850,#24452,.T.);
#59485=EDGE_CURVE('',#44830,#44851,#24453,.T.);
#59486=EDGE_CURVE('',#44829,#44852,#24454,.T.);
#59487=EDGE_CURVE('',#44828,#44853,#24455,.T.);
#59488=EDGE_CURVE('',#44827,#44854,#24456,.T.);
#59489=EDGE_CURVE('',#44826,#44855,#24457,.T.);
#59490=EDGE_CURVE('',#44825,#44856,#24458,.T.);
#59491=EDGE_CURVE('',#44824,#44857,#24459,.T.);
#59492=EDGE_CURVE('',#44823,#44858,#24460,.T.);
#59493=EDGE_CURVE('',#44822,#44859,#24461,.T.);
#59494=EDGE_CURVE('',#44821,#44860,#24462,.T.);
#59495=EDGE_CURVE('',#44820,#44861,#24463,.T.);
#59496=EDGE_CURVE('',#44819,#44862,#24464,.T.);
#59497=EDGE_CURVE('',#44818,#44863,#24465,.T.);
#59498=EDGE_CURVE('',#44817,#44864,#24466,.T.);
#59499=EDGE_CURVE('',#44816,#44865,#24467,.T.);
#59500=EDGE_CURVE('',#44815,#44866,#24468,.T.);
#59501=EDGE_CURVE('',#44814,#44867,#24469,.T.);
#59502=EDGE_CURVE('',#44813,#44868,#24470,.T.);
#59503=EDGE_CURVE('',#44812,#44869,#24471,.T.);
#59504=EDGE_CURVE('',#44811,#44870,#24472,.T.);
#59505=EDGE_CURVE('',#44810,#44871,#24473,.T.);
#59506=EDGE_CURVE('',#44809,#44872,#24474,.T.);
#59507=EDGE_CURVE('',#44808,#44873,#24475,.T.);
#59508=EDGE_CURVE('',#44807,#44874,#24476,.T.);
#59509=EDGE_CURVE('',#44806,#44875,#24477,.T.);
#59510=EDGE_CURVE('',#44805,#44876,#24478,.T.);
#59511=EDGE_CURVE('',#44804,#44877,#24479,.T.);
#59512=EDGE_CURVE('',#44803,#44878,#24480,.T.);
#59513=EDGE_CURVE('',#44802,#44879,#24481,.T.);
#59514=EDGE_CURVE('',#44801,#44880,#24482,.T.);
#59515=EDGE_CURVE('',#44800,#44881,#24483,.T.);
#59516=EDGE_CURVE('',#44799,#44882,#24484,.T.);
#59517=EDGE_CURVE('',#44798,#44883,#24485,.T.);
#59518=EDGE_CURVE('',#44797,#44884,#24486,.T.);
#59519=EDGE_CURVE('',#44796,#44885,#24487,.T.);
#59520=EDGE_CURVE('',#44795,#44886,#24488,.T.);
#59521=EDGE_CURVE('',#44794,#44887,#24489,.T.);
#59522=EDGE_CURVE('',#44793,#44888,#24490,.T.);
#59523=EDGE_CURVE('',#44792,#44889,#24491,.T.);
#59524=EDGE_CURVE('',#44791,#44890,#24492,.T.);
#59525=EDGE_CURVE('',#44790,#44891,#24493,.T.);
#59526=EDGE_CURVE('',#44789,#44892,#24494,.T.);
#59527=EDGE_CURVE('',#44788,#44893,#24495,.T.);
#59528=EDGE_CURVE('',#44787,#44894,#24496,.T.);
#59529=EDGE_CURVE('',#44786,#44840,#24497,.T.);
#59530=EDGE_CURVE('',#44785,#44839,#24498,.T.);
#59531=EDGE_CURVE('',#44895,#44896,#36351,.T.);
#59532=EDGE_CURVE('',#44896,#44897,#24499,.T.);
#59533=EDGE_CURVE('',#44898,#44897,#36352,.T.);
#59534=EDGE_CURVE('',#44895,#44898,#24500,.T.);
#59535=EDGE_CURVE('',#44899,#44900,#36353,.T.);
#59536=EDGE_CURVE('',#44900,#44901,#24501,.T.);
#59537=EDGE_CURVE('',#44901,#44902,#36354,.T.);
#59538=EDGE_CURVE('',#44902,#44903,#24502,.T.);
#59539=EDGE_CURVE('',#44903,#44904,#36355,.T.);
#59540=EDGE_CURVE('',#44904,#44898,#24503,.T.);
#59541=EDGE_CURVE('',#44897,#44905,#24504,.T.);
#59542=EDGE_CURVE('',#44905,#44906,#36356,.T.);
#59543=EDGE_CURVE('',#44906,#44907,#24505,.T.);
#59544=EDGE_CURVE('',#44907,#44908,#36357,.T.);
#59545=EDGE_CURVE('',#44908,#44909,#24506,.T.);
#59546=EDGE_CURVE('',#44909,#44910,#36358,.T.);
#59547=EDGE_CURVE('',#44910,#44911,#24507,.T.);
#59548=EDGE_CURVE('',#44911,#44912,#36359,.T.);
#59549=EDGE_CURVE('',#44912,#44899,#24508,.T.);
#59550=EDGE_CURVE('',#44913,#44912,#24509,.T.);
#59551=EDGE_CURVE('',#44913,#44914,#24510,.T.);
#59552=EDGE_CURVE('',#44914,#44899,#24511,.T.);
#59553=EDGE_CURVE('',#44915,#44911,#24512,.T.);
#59554=EDGE_CURVE('',#44915,#44913,#36360,.T.);
#59555=EDGE_CURVE('',#44916,#44910,#24513,.T.);
#59556=EDGE_CURVE('',#44916,#44915,#24514,.T.);
#59557=EDGE_CURVE('',#44917,#44909,#24515,.T.);
#59558=EDGE_CURVE('',#44917,#44916,#36361,.T.);
#59559=EDGE_CURVE('',#44918,#44908,#24516,.T.);
#59560=EDGE_CURVE('',#44918,#44917,#24517,.T.);
#59561=EDGE_CURVE('',#44919,#44907,#24518,.T.);
#59562=EDGE_CURVE('',#44919,#44918,#36362,.T.);
#59563=EDGE_CURVE('',#44920,#44906,#24519,.T.);
#59564=EDGE_CURVE('',#44920,#44919,#24520,.T.);
#59565=EDGE_CURVE('',#44921,#44905,#24521,.T.);
#59566=EDGE_CURVE('',#44921,#44920,#36363,.T.);
#59567=EDGE_CURVE('',#44896,#44921,#24522,.T.);
#59568=EDGE_CURVE('',#44922,#44904,#24523,.T.);
#59569=EDGE_CURVE('',#44922,#44895,#24524,.T.);
#59570=EDGE_CURVE('',#44923,#44903,#24525,.T.);
#59571=EDGE_CURVE('',#44923,#44922,#36364,.T.);
#59572=EDGE_CURVE('',#44924,#44902,#24526,.T.);
#59573=EDGE_CURVE('',#44924,#44923,#24527,.T.);
#59574=EDGE_CURVE('',#44925,#44901,#24528,.T.);
#59575=EDGE_CURVE('',#44925,#44924,#36365,.T.);
#59576=EDGE_CURVE('',#44926,#44900,#24529,.T.);
#59577=EDGE_CURVE('',#44926,#44925,#24530,.T.);
#59578=EDGE_CURVE('',#44914,#44926,#36366,.T.);
#59579=EDGE_CURVE('',#44927,#44928,#36367,.T.);
#59580=EDGE_CURVE('',#44928,#44929,#24531,.T.);
#59581=EDGE_CURVE('',#44929,#44930,#36368,.T.);
#59582=EDGE_CURVE('',#44930,#44931,#24532,.T.);
#59583=EDGE_CURVE('',#44931,#44932,#36369,.T.);
#59584=EDGE_CURVE('',#44932,#44933,#24533,.T.);
#59585=EDGE_CURVE('',#44933,#44934,#36370,.T.);
#59586=EDGE_CURVE('',#44934,#44927,#24534,.T.);
#59587=EDGE_CURVE('',#44935,#44934,#24535,.T.);
#59588=EDGE_CURVE('',#44935,#44936,#24536,.T.);
#59589=EDGE_CURVE('',#44936,#44927,#24537,.T.);
#59590=EDGE_CURVE('',#44937,#44933,#24538,.T.);
#59591=EDGE_CURVE('',#44937,#44935,#36371,.T.);
#59592=EDGE_CURVE('',#44938,#44932,#24539,.T.);
#59593=EDGE_CURVE('',#44938,#44937,#24540,.T.);
#59594=EDGE_CURVE('',#44939,#44931,#24541,.T.);
#59595=EDGE_CURVE('',#44939,#44938,#36372,.T.);
#59596=EDGE_CURVE('',#44940,#44930,#24542,.T.);
#59597=EDGE_CURVE('',#44940,#44939,#24543,.T.);
#59598=EDGE_CURVE('',#44941,#44929,#24544,.T.);
#59599=EDGE_CURVE('',#44941,#44940,#36373,.T.);
#59600=EDGE_CURVE('',#44942,#44928,#24545,.T.);
#59601=EDGE_CURVE('',#44942,#44941,#24546,.T.);
#59602=EDGE_CURVE('',#44936,#44942,#36374,.T.);
#59603=EDGE_CURVE('',#44943,#44944,#36375,.T.);
#59604=EDGE_CURVE('',#44944,#44945,#24547,.T.);
#59605=EDGE_CURVE('',#44946,#44945,#36376,.T.);
#59606=EDGE_CURVE('',#44943,#44946,#24548,.T.);
#59607=EDGE_CURVE('',#44947,#44948,#36377,.T.);
#59608=EDGE_CURVE('',#44948,#44946,#24549,.T.);
#59609=EDGE_CURVE('',#44945,#44949,#24550,.T.);
#59610=EDGE_CURVE('',#44949,#44950,#36378,.T.);
#59611=EDGE_CURVE('',#44950,#44951,#24551,.T.);
#59612=EDGE_CURVE('',#44951,#44952,#36379,.T.);
#59613=EDGE_CURVE('',#44952,#44953,#24552,.T.);
#59614=EDGE_CURVE('',#44953,#44954,#36380,.T.);
#59615=EDGE_CURVE('',#44954,#44955,#24553,.T.);
#59616=EDGE_CURVE('',#44955,#44956,#36381,.T.);
#59617=EDGE_CURVE('',#44956,#44957,#24554,.T.);
#59618=EDGE_CURVE('',#44957,#44958,#36382,.T.);
#59619=EDGE_CURVE('',#44958,#44959,#24555,.T.);
#59620=EDGE_CURVE('',#44959,#44960,#36383,.T.);
#59621=EDGE_CURVE('',#44960,#44947,#24556,.T.);
#59622=EDGE_CURVE('',#44961,#44960,#24557,.T.);
#59623=EDGE_CURVE('',#44961,#44962,#24558,.T.);
#59624=EDGE_CURVE('',#44962,#44947,#24559,.T.);
#59625=EDGE_CURVE('',#44963,#44959,#24560,.T.);
#59626=EDGE_CURVE('',#44963,#44961,#36384,.T.);
#59627=EDGE_CURVE('',#44964,#44958,#24561,.T.);
#59628=EDGE_CURVE('',#44964,#44963,#24562,.T.);
#59629=EDGE_CURVE('',#44965,#44957,#24563,.T.);
#59630=EDGE_CURVE('',#44965,#44964,#36385,.T.);
#59631=EDGE_CURVE('',#44966,#44956,#24564,.T.);
#59632=EDGE_CURVE('',#44966,#44965,#24565,.T.);
#59633=EDGE_CURVE('',#44967,#44955,#24566,.T.);
#59634=EDGE_CURVE('',#44967,#44966,#36386,.T.);
#59635=EDGE_CURVE('',#44968,#44954,#24567,.T.);
#59636=EDGE_CURVE('',#44968,#44967,#24568,.T.);
#59637=EDGE_CURVE('',#44969,#44953,#24569,.T.);
#59638=EDGE_CURVE('',#44969,#44968,#36387,.T.);
#59639=EDGE_CURVE('',#44970,#44952,#24570,.T.);
#59640=EDGE_CURVE('',#44970,#44969,#24571,.T.);
#59641=EDGE_CURVE('',#44971,#44951,#24572,.T.);
#59642=EDGE_CURVE('',#44971,#44970,#36388,.T.);
#59643=EDGE_CURVE('',#44972,#44950,#24573,.T.);
#59644=EDGE_CURVE('',#44972,#44971,#24574,.T.);
#59645=EDGE_CURVE('',#44973,#44949,#24575,.T.);
#59646=EDGE_CURVE('',#44973,#44972,#36389,.T.);
#59647=EDGE_CURVE('',#44944,#44973,#24576,.T.);
#59648=EDGE_CURVE('',#44974,#44948,#24577,.T.);
#59649=EDGE_CURVE('',#44974,#44943,#24578,.T.);
#59650=EDGE_CURVE('',#44962,#44974,#36390,.T.);
#59651=EDGE_CURVE('',#44975,#44976,#36391,.T.);
#59652=EDGE_CURVE('',#44976,#44977,#24579,.T.);
#59653=EDGE_CURVE('',#44977,#44978,#36392,.T.);
#59654=EDGE_CURVE('',#44978,#44979,#24580,.T.);
#59655=EDGE_CURVE('',#44979,#44980,#36393,.T.);
#59656=EDGE_CURVE('',#44980,#44981,#24581,.T.);
#59657=EDGE_CURVE('',#44981,#44982,#36394,.T.);
#59658=EDGE_CURVE('',#44982,#44975,#24582,.T.);
#59659=EDGE_CURVE('',#44983,#44982,#24583,.T.);
#59660=EDGE_CURVE('',#44983,#44984,#24584,.T.);
#59661=EDGE_CURVE('',#44984,#44975,#24585,.T.);
#59662=EDGE_CURVE('',#44985,#44981,#24586,.T.);
#59663=EDGE_CURVE('',#44985,#44983,#36395,.T.);
#59664=EDGE_CURVE('',#44986,#44980,#24587,.T.);
#59665=EDGE_CURVE('',#44986,#44985,#24588,.T.);
#59666=EDGE_CURVE('',#44987,#44979,#24589,.T.);
#59667=EDGE_CURVE('',#44987,#44986,#36396,.T.);
#59668=EDGE_CURVE('',#44988,#44978,#24590,.T.);
#59669=EDGE_CURVE('',#44988,#44987,#24591,.T.);
#59670=EDGE_CURVE('',#44989,#44977,#24592,.T.);
#59671=EDGE_CURVE('',#44989,#44988,#36397,.T.);
#59672=EDGE_CURVE('',#44990,#44976,#24593,.T.);
#59673=EDGE_CURVE('',#44990,#44989,#24594,.T.);
#59674=EDGE_CURVE('',#44984,#44990,#36398,.T.);
#59675=EDGE_CURVE('',#44991,#44992,#36399,.T.);
#59676=EDGE_CURVE('',#44992,#44993,#24595,.T.);
#59677=EDGE_CURVE('',#44994,#44993,#36400,.T.);
#59678=EDGE_CURVE('',#44991,#44994,#24596,.T.);
#59679=EDGE_CURVE('',#44995,#44996,#36401,.T.);
#59680=EDGE_CURVE('',#44996,#44994,#24597,.T.);
#59681=EDGE_CURVE('',#44993,#44997,#24598,.T.);
#59682=EDGE_CURVE('',#44997,#44998,#36402,.T.);
#59683=EDGE_CURVE('',#44998,#44999,#24599,.T.);
#59684=EDGE_CURVE('',#44999,#45000,#36403,.T.);
#59685=EDGE_CURVE('',#45000,#45001,#24600,.T.);
#59686=EDGE_CURVE('',#45001,#45002,#36404,.T.);
#59687=EDGE_CURVE('',#45002,#45003,#24601,.T.);
#59688=EDGE_CURVE('',#45003,#45004,#36405,.T.);
#59689=EDGE_CURVE('',#45004,#45005,#24602,.T.);
#59690=EDGE_CURVE('',#45005,#45006,#36406,.T.);
#59691=EDGE_CURVE('',#45006,#45007,#24603,.T.);
#59692=EDGE_CURVE('',#45007,#45008,#36407,.T.);
#59693=EDGE_CURVE('',#45008,#44995,#24604,.T.);
#59694=EDGE_CURVE('',#45009,#45008,#24605,.T.);
#59695=EDGE_CURVE('',#45009,#45010,#24606,.T.);
#59696=EDGE_CURVE('',#45010,#44995,#24607,.T.);
#59697=EDGE_CURVE('',#45011,#45007,#24608,.T.);
#59698=EDGE_CURVE('',#45011,#45009,#36408,.T.);
#59699=EDGE_CURVE('',#45012,#45006,#24609,.T.);
#59700=EDGE_CURVE('',#45012,#45011,#24610,.T.);
#59701=EDGE_CURVE('',#45013,#45005,#24611,.T.);
#59702=EDGE_CURVE('',#45013,#45012,#36409,.T.);
#59703=EDGE_CURVE('',#45014,#45004,#24612,.T.);
#59704=EDGE_CURVE('',#45014,#45013,#24613,.T.);
#59705=EDGE_CURVE('',#45015,#45003,#24614,.T.);
#59706=EDGE_CURVE('',#45015,#45014,#36410,.T.);
#59707=EDGE_CURVE('',#45016,#45002,#24615,.T.);
#59708=EDGE_CURVE('',#45016,#45015,#24616,.T.);
#59709=EDGE_CURVE('',#45017,#45001,#24617,.T.);
#59710=EDGE_CURVE('',#45017,#45016,#36411,.T.);
#59711=EDGE_CURVE('',#45018,#45000,#24618,.T.);
#59712=EDGE_CURVE('',#45018,#45017,#24619,.T.);
#59713=EDGE_CURVE('',#45019,#44999,#24620,.T.);
#59714=EDGE_CURVE('',#45019,#45018,#36412,.T.);
#59715=EDGE_CURVE('',#45020,#44998,#24621,.T.);
#59716=EDGE_CURVE('',#45020,#45019,#24622,.T.);
#59717=EDGE_CURVE('',#45021,#44997,#24623,.T.);
#59718=EDGE_CURVE('',#45021,#45020,#36413,.T.);
#59719=EDGE_CURVE('',#44992,#45021,#24624,.T.);
#59720=EDGE_CURVE('',#45022,#44996,#24625,.T.);
#59721=EDGE_CURVE('',#45022,#44991,#24626,.T.);
#59722=EDGE_CURVE('',#45010,#45022,#36414,.T.);
#59723=EDGE_CURVE('',#45023,#45024,#36415,.T.);
#59724=EDGE_CURVE('',#45024,#45025,#24627,.T.);
#59725=EDGE_CURVE('',#45025,#45026,#36416,.T.);
#59726=EDGE_CURVE('',#45026,#45027,#24628,.T.);
#59727=EDGE_CURVE('',#45027,#45028,#36417,.T.);
#59728=EDGE_CURVE('',#45028,#45029,#24629,.T.);
#59729=EDGE_CURVE('',#45029,#45030,#36418,.T.);
#59730=EDGE_CURVE('',#45030,#45023,#24630,.T.);
#59731=EDGE_CURVE('',#45031,#45030,#24631,.T.);
#59732=EDGE_CURVE('',#45031,#45032,#24632,.T.);
#59733=EDGE_CURVE('',#45032,#45023,#24633,.T.);
#59734=EDGE_CURVE('',#45033,#45029,#24634,.T.);
#59735=EDGE_CURVE('',#45033,#45031,#36419,.T.);
#59736=EDGE_CURVE('',#45034,#45028,#24635,.T.);
#59737=EDGE_CURVE('',#45034,#45033,#24636,.T.);
#59738=EDGE_CURVE('',#45035,#45027,#24637,.T.);
#59739=EDGE_CURVE('',#45035,#45034,#36420,.T.);
#59740=EDGE_CURVE('',#45036,#45026,#24638,.T.);
#59741=EDGE_CURVE('',#45036,#45035,#24639,.T.);
#59742=EDGE_CURVE('',#45037,#45025,#24640,.T.);
#59743=EDGE_CURVE('',#45037,#45036,#36421,.T.);
#59744=EDGE_CURVE('',#45038,#45024,#24641,.T.);
#59745=EDGE_CURVE('',#45038,#45037,#24642,.T.);
#59746=EDGE_CURVE('',#45032,#45038,#36422,.T.);
#59747=EDGE_CURVE('',#45039,#45040,#24643,.T.);
#59748=EDGE_CURVE('',#45039,#45041,#24644,.T.);
#59749=EDGE_CURVE('',#45041,#45042,#24645,.T.);
#59750=EDGE_CURVE('',#45042,#45040,#24646,.T.);
#59751=EDGE_CURVE('',#45043,#45044,#24647,.T.);
#59752=EDGE_CURVE('',#45043,#45045,#24648,.T.);
#59753=EDGE_CURVE('',#45045,#45046,#24649,.T.);
#59754=EDGE_CURVE('',#45044,#45046,#24650,.T.);
#59755=EDGE_CURVE('',#45047,#45048,#24651,.T.);
#59756=EDGE_CURVE('',#45047,#45049,#24652,.T.);
#59757=EDGE_CURVE('',#45049,#45050,#24653,.T.);
#59758=EDGE_CURVE('',#45048,#45050,#24654,.T.);
#59759=EDGE_CURVE('',#45048,#45051,#24655,.T.);
#59760=EDGE_CURVE('',#45050,#45052,#24656,.T.);
#59761=EDGE_CURVE('',#45051,#45052,#24657,.T.);
#59762=EDGE_CURVE('',#45051,#45053,#24658,.T.);
#59763=EDGE_CURVE('',#45052,#45054,#24659,.T.);
#59764=EDGE_CURVE('',#45053,#45054,#24660,.T.);
#59765=EDGE_CURVE('',#45053,#45055,#36423,.T.);
#59766=EDGE_CURVE('',#45054,#45056,#36424,.T.);
#59767=EDGE_CURVE('',#45055,#45056,#24661,.T.);
#59768=EDGE_CURVE('',#45055,#45057,#24662,.T.);
#59769=EDGE_CURVE('',#45056,#45058,#24663,.T.);
#59770=EDGE_CURVE('',#45057,#45058,#24664,.T.);
#59771=EDGE_CURVE('',#45057,#45059,#36425,.T.);
#59772=EDGE_CURVE('',#45058,#45060,#36426,.T.);
#59773=EDGE_CURVE('',#45059,#45060,#24665,.T.);
#59774=EDGE_CURVE('',#45059,#45061,#24666,.T.);
#59775=EDGE_CURVE('',#45060,#45062,#24667,.T.);
#59776=EDGE_CURVE('',#45061,#45062,#24668,.T.);
#59777=EDGE_CURVE('',#45061,#45063,#36427,.T.);
#59778=EDGE_CURVE('',#45062,#45064,#36428,.T.);
#59779=EDGE_CURVE('',#45063,#45064,#24669,.T.);
#59780=EDGE_CURVE('',#45063,#45065,#24670,.T.);
#59781=EDGE_CURVE('',#45064,#45066,#24671,.T.);
#59782=EDGE_CURVE('',#45065,#45066,#24672,.T.);
#59783=EDGE_CURVE('',#45065,#45067,#36429,.T.);
#59784=EDGE_CURVE('',#45066,#45068,#36430,.T.);
#59785=EDGE_CURVE('',#45067,#45068,#24673,.T.);
#59786=EDGE_CURVE('',#45067,#45069,#24674,.T.);
#59787=EDGE_CURVE('',#45068,#45070,#24675,.T.);
#59788=EDGE_CURVE('',#45069,#45070,#24676,.T.);
#59789=EDGE_CURVE('',#45069,#45071,#24677,.T.);
#59790=EDGE_CURVE('',#45070,#45072,#24678,.T.);
#59791=EDGE_CURVE('',#45071,#45072,#24679,.T.);
#59792=EDGE_CURVE('',#45071,#45073,#24680,.T.);
#59793=EDGE_CURVE('',#45072,#45074,#24681,.T.);
#59794=EDGE_CURVE('',#45073,#45074,#24682,.T.);
#59795=EDGE_CURVE('',#45073,#45075,#24683,.T.);
#59796=EDGE_CURVE('',#45074,#45076,#24684,.T.);
#59797=EDGE_CURVE('',#45075,#45076,#24685,.T.);
#59798=EDGE_CURVE('',#45077,#45078,#24686,.T.);
#59799=EDGE_CURVE('',#45077,#45079,#24687,.T.);
#59800=EDGE_CURVE('',#45079,#45080,#24688,.T.);
#59801=EDGE_CURVE('',#45078,#45080,#24689,.T.);
#59802=EDGE_CURVE('',#45078,#45081,#24690,.T.);
#59803=EDGE_CURVE('',#45080,#45082,#24691,.T.);
#59804=EDGE_CURVE('',#45081,#45082,#24692,.T.);
#59805=EDGE_CURVE('',#45081,#45083,#24693,.T.);
#59806=EDGE_CURVE('',#45082,#45084,#24694,.T.);
#59807=EDGE_CURVE('',#45083,#45084,#24695,.T.);
#59808=EDGE_CURVE('',#45083,#45085,#24696,.T.);
#59809=EDGE_CURVE('',#45084,#45086,#24697,.T.);
#59810=EDGE_CURVE('',#45085,#45086,#24698,.T.);
#59811=EDGE_CURVE('',#45085,#45087,#36431,.T.);
#59812=EDGE_CURVE('',#45086,#45088,#36432,.T.);
#59813=EDGE_CURVE('',#45087,#45088,#24699,.T.);
#59814=EDGE_CURVE('',#45087,#45089,#24700,.T.);
#59815=EDGE_CURVE('',#45088,#45090,#24701,.T.);
#59816=EDGE_CURVE('',#45089,#45090,#24702,.T.);
#59817=EDGE_CURVE('',#45089,#45091,#36433,.T.);
#59818=EDGE_CURVE('',#45090,#45092,#36434,.T.);
#59819=EDGE_CURVE('',#45091,#45092,#24703,.T.);
#59820=EDGE_CURVE('',#45091,#45093,#24704,.T.);
#59821=EDGE_CURVE('',#45092,#45094,#24705,.T.);
#59822=EDGE_CURVE('',#45093,#45094,#24706,.T.);
#59823=EDGE_CURVE('',#45093,#45095,#36435,.T.);
#59824=EDGE_CURVE('',#45094,#45096,#36436,.T.);
#59825=EDGE_CURVE('',#45095,#45096,#24707,.T.);
#59826=EDGE_CURVE('',#45095,#45097,#24708,.T.);
#59827=EDGE_CURVE('',#45096,#45098,#24709,.T.);
#59828=EDGE_CURVE('',#45097,#45098,#24710,.T.);
#59829=EDGE_CURVE('',#45097,#45099,#36437,.T.);
#59830=EDGE_CURVE('',#45098,#45100,#36438,.T.);
#59831=EDGE_CURVE('',#45099,#45100,#24711,.T.);
#59832=EDGE_CURVE('',#45099,#45101,#24712,.T.);
#59833=EDGE_CURVE('',#45100,#45102,#24713,.T.);
#59834=EDGE_CURVE('',#45101,#45102,#24714,.T.);
#59835=EDGE_CURVE('',#45101,#45103,#24715,.T.);
#59836=EDGE_CURVE('',#45102,#45104,#24716,.T.);
#59837=EDGE_CURVE('',#45103,#45104,#24717,.T.);
#59838=EDGE_CURVE('',#45103,#45105,#24718,.T.);
#59839=EDGE_CURVE('',#45104,#45106,#24719,.T.);
#59840=EDGE_CURVE('',#45105,#45106,#24720,.T.);
#59841=EDGE_CURVE('',#45105,#45107,#24721,.T.);
#59842=EDGE_CURVE('',#45106,#45108,#24722,.T.);
#59843=EDGE_CURVE('',#45107,#45108,#24723,.T.);
#59844=EDGE_CURVE('',#45107,#45109,#36439,.T.);
#59845=EDGE_CURVE('',#45108,#45110,#36440,.T.);
#59846=EDGE_CURVE('',#45109,#45110,#24724,.T.);
#59847=EDGE_CURVE('',#45109,#45111,#24725,.T.);
#59848=EDGE_CURVE('',#45110,#45112,#24726,.T.);
#59849=EDGE_CURVE('',#45111,#45112,#24727,.T.);
#59850=EDGE_CURVE('',#45111,#45113,#36441,.T.);
#59851=EDGE_CURVE('',#45112,#45114,#36442,.T.);
#59852=EDGE_CURVE('',#45113,#45114,#24728,.T.);
#59853=EDGE_CURVE('',#45113,#45115,#24729,.T.);
#59854=EDGE_CURVE('',#45114,#45116,#24730,.T.);
#59855=EDGE_CURVE('',#45115,#45116,#24731,.T.);
#59856=EDGE_CURVE('',#45115,#45039,#36443,.T.);
#59857=EDGE_CURVE('',#45116,#45041,#36444,.T.);
#59858=EDGE_CURVE('',#45117,#45118,#24732,.T.);
#59859=EDGE_CURVE('',#45117,#45119,#24733,.T.);
#59860=EDGE_CURVE('',#45119,#45120,#24734,.T.);
#59861=EDGE_CURVE('',#45118,#45120,#24735,.T.);
#59862=EDGE_CURVE('',#45118,#45121,#36445,.T.);
#59863=EDGE_CURVE('',#45120,#45122,#36446,.T.);
#59864=EDGE_CURVE('',#45121,#45122,#24736,.T.);
#59865=EDGE_CURVE('',#45121,#45123,#24737,.T.);
#59866=EDGE_CURVE('',#45122,#45124,#24738,.T.);
#59867=EDGE_CURVE('',#45123,#45124,#24739,.T.);
#59868=EDGE_CURVE('',#45123,#45125,#24740,.T.);
#59869=EDGE_CURVE('',#45124,#45126,#24741,.T.);
#59870=EDGE_CURVE('',#45125,#45126,#24742,.T.);
#59871=EDGE_CURVE('',#45125,#45127,#24743,.T.);
#59872=EDGE_CURVE('',#45126,#45128,#24744,.T.);
#59873=EDGE_CURVE('',#45127,#45128,#24745,.T.);
#59874=EDGE_CURVE('',#45127,#45129,#24746,.T.);
#59875=EDGE_CURVE('',#45128,#45130,#24747,.T.);
#59876=EDGE_CURVE('',#45129,#45130,#24748,.T.);
#59877=EDGE_CURVE('',#45129,#45131,#36447,.T.);
#59878=EDGE_CURVE('',#45130,#45132,#36448,.T.);
#59879=EDGE_CURVE('',#45131,#45132,#24749,.T.);
#59880=EDGE_CURVE('',#45131,#45133,#24750,.T.);
#59881=EDGE_CURVE('',#45132,#45134,#24751,.T.);
#59882=EDGE_CURVE('',#45133,#45134,#24752,.T.);
#59883=EDGE_CURVE('',#45133,#45135,#24753,.T.);
#59884=EDGE_CURVE('',#45134,#45136,#24754,.T.);
#59885=EDGE_CURVE('',#45135,#45136,#24755,.T.);
#59886=EDGE_CURVE('',#45135,#45137,#24756,.T.);
#59887=EDGE_CURVE('',#45136,#45138,#24757,.T.);
#59888=EDGE_CURVE('',#45137,#45138,#24758,.T.);
#59889=EDGE_CURVE('',#45137,#45139,#24759,.T.);
#59890=EDGE_CURVE('',#45138,#45140,#24760,.T.);
#59891=EDGE_CURVE('',#45139,#45140,#24761,.T.);
#59892=EDGE_CURVE('',#45139,#45141,#36449,.T.);
#59893=EDGE_CURVE('',#45140,#45142,#36450,.T.);
#59894=EDGE_CURVE('',#45141,#45142,#24762,.T.);
#59895=EDGE_CURVE('',#45141,#45143,#24763,.T.);
#59896=EDGE_CURVE('',#45142,#45144,#24764,.T.);
#59897=EDGE_CURVE('',#45144,#45143,#24765,.T.);
#59898=EDGE_CURVE('',#45044,#45145,#36451,.T.);
#59899=EDGE_CURVE('',#45046,#45146,#36452,.T.);
#59900=EDGE_CURVE('',#45145,#45146,#24766,.T.);
#59901=EDGE_CURVE('',#45145,#45147,#24767,.T.);
#59902=EDGE_CURVE('',#45146,#45148,#24768,.T.);
#59903=EDGE_CURVE('',#45147,#45148,#24769,.T.);
#59904=EDGE_CURVE('',#45147,#45149,#36453,.T.);
#59905=EDGE_CURVE('',#45148,#45150,#36454,.T.);
#59906=EDGE_CURVE('',#45149,#45150,#24770,.T.);
#59907=EDGE_CURVE('',#45149,#45151,#24771,.T.);
#59908=EDGE_CURVE('',#45150,#45152,#24772,.T.);
#59909=EDGE_CURVE('',#45151,#45152,#24773,.T.);
#59910=EDGE_CURVE('',#45151,#45153,#36455,.T.);
#59911=EDGE_CURVE('',#45152,#45154,#36456,.T.);
#59912=EDGE_CURVE('',#45153,#45154,#24774,.T.);
#59913=EDGE_CURVE('',#45153,#45047,#24775,.T.);
#59914=EDGE_CURVE('',#45154,#45049,#24776,.T.);
#59915=EDGE_CURVE('',#45155,#45156,#24777,.T.);
#59916=EDGE_CURVE('',#45155,#45157,#24778,.T.);
#59917=EDGE_CURVE('',#45157,#45158,#24779,.T.);
#59918=EDGE_CURVE('',#45156,#45158,#24780,.T.);
#59919=EDGE_CURVE('',#45156,#45159,#24781,.T.);
#59920=EDGE_CURVE('',#45158,#45160,#24782,.T.);
#59921=EDGE_CURVE('',#45159,#45160,#24783,.T.);
#59922=EDGE_CURVE('',#45159,#45161,#24784,.T.);
#59923=EDGE_CURVE('',#45160,#45162,#24785,.T.);
#59924=EDGE_CURVE('',#45161,#45162,#24786,.T.);
#59925=EDGE_CURVE('',#45161,#45163,#36457,.T.);
#59926=EDGE_CURVE('',#45162,#45164,#36458,.T.);
#59927=EDGE_CURVE('',#45163,#45164,#24787,.T.);
#59928=EDGE_CURVE('',#45163,#45165,#24788,.T.);
#59929=EDGE_CURVE('',#45164,#45166,#24789,.T.);
#59930=EDGE_CURVE('',#45165,#45166,#24790,.T.);
#59931=EDGE_CURVE('',#45165,#45167,#36459,.T.);
#59932=EDGE_CURVE('',#45166,#45168,#36460,.T.);
#59933=EDGE_CURVE('',#45167,#45168,#24791,.T.);
#59934=EDGE_CURVE('',#45167,#45169,#24792,.T.);
#59935=EDGE_CURVE('',#45168,#45170,#24793,.T.);
#59936=EDGE_CURVE('',#45169,#45170,#24794,.T.);
#59937=EDGE_CURVE('',#45169,#45171,#36461,.T.);
#59938=EDGE_CURVE('',#45170,#45172,#36462,.T.);
#59939=EDGE_CURVE('',#45171,#45172,#24795,.T.);
#59940=EDGE_CURVE('',#45171,#45173,#24796,.T.);
#59941=EDGE_CURVE('',#45172,#45174,#24797,.T.);
#59942=EDGE_CURVE('',#45173,#45174,#24798,.T.);
#59943=EDGE_CURVE('',#45173,#45175,#36463,.T.);
#59944=EDGE_CURVE('',#45174,#45176,#36464,.T.);
#59945=EDGE_CURVE('',#45175,#45176,#24799,.T.);
#59946=EDGE_CURVE('',#45175,#45177,#24800,.T.);
#59947=EDGE_CURVE('',#45176,#45178,#24801,.T.);
#59948=EDGE_CURVE('',#45177,#45178,#24802,.T.);
#59949=EDGE_CURVE('',#45177,#45179,#24803,.T.);
#59950=EDGE_CURVE('',#45178,#45180,#24804,.T.);
#59951=EDGE_CURVE('',#45179,#45180,#24805,.T.);
#59952=EDGE_CURVE('',#45179,#45077,#24806,.T.);
#59953=EDGE_CURVE('',#45180,#45079,#24807,.T.);
#59954=EDGE_CURVE('',#45181,#45182,#24808,.T.);
#59955=EDGE_CURVE('',#45181,#45183,#24809,.T.);
#59956=EDGE_CURVE('',#45183,#45184,#24810,.T.);
#59957=EDGE_CURVE('',#45182,#45184,#24811,.T.);
#59958=EDGE_CURVE('',#45182,#45185,#24812,.T.);
#59959=EDGE_CURVE('',#45184,#45186,#24813,.T.);
#59960=EDGE_CURVE('',#45185,#45186,#24814,.T.);
#59961=EDGE_CURVE('',#45185,#45187,#24815,.T.);
#59962=EDGE_CURVE('',#45186,#45188,#24816,.T.);
#59963=EDGE_CURVE('',#45187,#45188,#24817,.T.);
#59964=EDGE_CURVE('',#45187,#45189,#24818,.T.);
#59965=EDGE_CURVE('',#45188,#45190,#24819,.T.);
#59966=EDGE_CURVE('',#45189,#45190,#24820,.T.);
#59967=EDGE_CURVE('',#45189,#45191,#36465,.T.);
#59968=EDGE_CURVE('',#45190,#45192,#36466,.T.);
#59969=EDGE_CURVE('',#45191,#45192,#24821,.T.);
#59970=EDGE_CURVE('',#45191,#45193,#24822,.T.);
#59971=EDGE_CURVE('',#45192,#45194,#24823,.T.);
#59972=EDGE_CURVE('',#45193,#45194,#24824,.T.);
#59973=EDGE_CURVE('',#45193,#45195,#36467,.T.);
#59974=EDGE_CURVE('',#45194,#45196,#36468,.T.);
#59975=EDGE_CURVE('',#45195,#45196,#24825,.T.);
#59976=EDGE_CURVE('',#45195,#45197,#24826,.T.);
#59977=EDGE_CURVE('',#45196,#45198,#24827,.T.);
#59978=EDGE_CURVE('',#45197,#45198,#24828,.T.);
#59979=EDGE_CURVE('',#45197,#45199,#36469,.T.);
#59980=EDGE_CURVE('',#45198,#45200,#36470,.T.);
#59981=EDGE_CURVE('',#45199,#45200,#24829,.T.);
#59982=EDGE_CURVE('',#45199,#45201,#24830,.T.);
#59983=EDGE_CURVE('',#45200,#45202,#24831,.T.);
#59984=EDGE_CURVE('',#45201,#45202,#24832,.T.);
#59985=EDGE_CURVE('',#45201,#45203,#36471,.T.);
#59986=EDGE_CURVE('',#45202,#45204,#36472,.T.);
#59987=EDGE_CURVE('',#45203,#45204,#24833,.T.);
#59988=EDGE_CURVE('',#45203,#45205,#24834,.T.);
#59989=EDGE_CURVE('',#45204,#45206,#24835,.T.);
#59990=EDGE_CURVE('',#45205,#45206,#24836,.T.);
#59991=EDGE_CURVE('',#45205,#45207,#24837,.T.);
#59992=EDGE_CURVE('',#45206,#45208,#24838,.T.);
#59993=EDGE_CURVE('',#45207,#45208,#24839,.T.);
#59994=EDGE_CURVE('',#45207,#45209,#24840,.T.);
#59995=EDGE_CURVE('',#45208,#45210,#24841,.T.);
#59996=EDGE_CURVE('',#45209,#45210,#24842,.T.);
#59997=EDGE_CURVE('',#45209,#45211,#24843,.T.);
#59998=EDGE_CURVE('',#45210,#45212,#24844,.T.);
#59999=EDGE_CURVE('',#45211,#45212,#24845,.T.);
#60000=EDGE_CURVE('',#45211,#45213,#36473,.T.);
#60001=EDGE_CURVE('',#45212,#45214,#36474,.T.);
#60002=EDGE_CURVE('',#45213,#45214,#24846,.T.);
#60003=EDGE_CURVE('',#45213,#45215,#24847,.T.);
#60004=EDGE_CURVE('',#45214,#45216,#24848,.T.);
#60005=EDGE_CURVE('',#45215,#45216,#24849,.T.);
#60006=EDGE_CURVE('',#45215,#45217,#36475,.T.);
#60007=EDGE_CURVE('',#45216,#45218,#36476,.T.);
#60008=EDGE_CURVE('',#45217,#45218,#24850,.T.);
#60009=EDGE_CURVE('',#45217,#45219,#24851,.T.);
#60010=EDGE_CURVE('',#45218,#45220,#24852,.T.);
#60011=EDGE_CURVE('',#45219,#45220,#24853,.T.);
#60012=EDGE_CURVE('',#45219,#45221,#36477,.T.);
#60013=EDGE_CURVE('',#45220,#45222,#36478,.T.);
#60014=EDGE_CURVE('',#45221,#45222,#24854,.T.);
#60015=EDGE_CURVE('',#45221,#45223,#24855,.T.);
#60016=EDGE_CURVE('',#45222,#45224,#24856,.T.);
#60017=EDGE_CURVE('',#45223,#45224,#24857,.T.);
#60018=EDGE_CURVE('',#45223,#45225,#36479,.T.);
#60019=EDGE_CURVE('',#45224,#45226,#36480,.T.);
#60020=EDGE_CURVE('',#45225,#45226,#24858,.T.);
#60021=EDGE_CURVE('',#45225,#45227,#24859,.T.);
#60022=EDGE_CURVE('',#45226,#45228,#24860,.T.);
#60023=EDGE_CURVE('',#45227,#45228,#24861,.T.);
#60024=EDGE_CURVE('',#45227,#45229,#24862,.T.);
#60025=EDGE_CURVE('',#45228,#45230,#24863,.T.);
#60026=EDGE_CURVE('',#45229,#45230,#24864,.T.);
#60027=EDGE_CURVE('',#45229,#45231,#24865,.T.);
#60028=EDGE_CURVE('',#45230,#45232,#24866,.T.);
#60029=EDGE_CURVE('',#45231,#45232,#24867,.T.);
#60030=EDGE_CURVE('',#45231,#45233,#24868,.T.);
#60031=EDGE_CURVE('',#45232,#45234,#24869,.T.);
#60032=EDGE_CURVE('',#45233,#45234,#24870,.T.);
#60033=EDGE_CURVE('',#45233,#45235,#36481,.T.);
#60034=EDGE_CURVE('',#45234,#45236,#36482,.T.);
#60035=EDGE_CURVE('',#45235,#45236,#24871,.T.);
#60036=EDGE_CURVE('',#45235,#45237,#24872,.T.);
#60037=EDGE_CURVE('',#45236,#45238,#24873,.T.);
#60038=EDGE_CURVE('',#45237,#45238,#24874,.T.);
#60039=EDGE_CURVE('',#45237,#45239,#24875,.T.);
#60040=EDGE_CURVE('',#45238,#45240,#24876,.T.);
#60041=EDGE_CURVE('',#45239,#45240,#24877,.T.);
#60042=EDGE_CURVE('',#45239,#45241,#24878,.T.);
#60043=EDGE_CURVE('',#45240,#45242,#24879,.T.);
#60044=EDGE_CURVE('',#45241,#45242,#24880,.T.);
#60045=EDGE_CURVE('',#45241,#45243,#24881,.T.);
#60046=EDGE_CURVE('',#45242,#45244,#24882,.T.);
#60047=EDGE_CURVE('',#45243,#45244,#24883,.T.);
#60048=EDGE_CURVE('',#45243,#45245,#36483,.T.);
#60049=EDGE_CURVE('',#45244,#45246,#36484,.T.);
#60050=EDGE_CURVE('',#45245,#45246,#24884,.T.);
#60051=EDGE_CURVE('',#45245,#45247,#24885,.T.);
#60052=EDGE_CURVE('',#45246,#45248,#24886,.T.);
#60053=EDGE_CURVE('',#45247,#45248,#24887,.T.);
#60054=EDGE_CURVE('',#45247,#45249,#36485,.T.);
#60055=EDGE_CURVE('',#45248,#45250,#36486,.T.);
#60056=EDGE_CURVE('',#45249,#45250,#24888,.T.);
#60057=EDGE_CURVE('',#45249,#45251,#24889,.T.);
#60058=EDGE_CURVE('',#45250,#45252,#24890,.T.);
#60059=EDGE_CURVE('',#45251,#45252,#24891,.T.);
#60060=EDGE_CURVE('',#45251,#45253,#36487,.T.);
#60061=EDGE_CURVE('',#45252,#45254,#36488,.T.);
#60062=EDGE_CURVE('',#45253,#45254,#24892,.T.);
#60063=EDGE_CURVE('',#45253,#45255,#24893,.T.);
#60064=EDGE_CURVE('',#45254,#45256,#24894,.T.);
#60065=EDGE_CURVE('',#45255,#45256,#24895,.T.);
#60066=EDGE_CURVE('',#45255,#45257,#36489,.T.);
#60067=EDGE_CURVE('',#45256,#45258,#36490,.T.);
#60068=EDGE_CURVE('',#45257,#45258,#24896,.T.);
#60069=EDGE_CURVE('',#45257,#45155,#24897,.T.);
#60070=EDGE_CURVE('',#45258,#45157,#24898,.T.);
#60071=EDGE_CURVE('',#45259,#45260,#24899,.T.);
#60072=EDGE_CURVE('',#45259,#45261,#24900,.T.);
#60073=EDGE_CURVE('',#45261,#45262,#24901,.T.);
#60074=EDGE_CURVE('',#45260,#45262,#24902,.T.);
#60075=EDGE_CURVE('',#45260,#45263,#24903,.T.);
#60076=EDGE_CURVE('',#45262,#45264,#24904,.T.);
#60077=EDGE_CURVE('',#45263,#45264,#24905,.T.);
#60078=EDGE_CURVE('',#45263,#45265,#24906,.T.);
#60079=EDGE_CURVE('',#45264,#45266,#24907,.T.);
#60080=EDGE_CURVE('',#45265,#45266,#24908,.T.);
#60081=EDGE_CURVE('',#45265,#45267,#36491,.T.);
#60082=EDGE_CURVE('',#45266,#45268,#36492,.T.);
#60083=EDGE_CURVE('',#45267,#45268,#24909,.T.);
#60084=EDGE_CURVE('',#45267,#45269,#24910,.T.);
#60085=EDGE_CURVE('',#45268,#45270,#24911,.T.);
#60086=EDGE_CURVE('',#45269,#45270,#24912,.T.);
#60087=EDGE_CURVE('',#45269,#45271,#36493,.T.);
#60088=EDGE_CURVE('',#45270,#45272,#36494,.T.);
#60089=EDGE_CURVE('',#45271,#45272,#24913,.T.);
#60090=EDGE_CURVE('',#45271,#45273,#24914,.T.);
#60091=EDGE_CURVE('',#45272,#45274,#24915,.T.);
#60092=EDGE_CURVE('',#45273,#45274,#24916,.T.);
#60093=EDGE_CURVE('',#45273,#45275,#36495,.T.);
#60094=EDGE_CURVE('',#45274,#45276,#36496,.T.);
#60095=EDGE_CURVE('',#45275,#45276,#24917,.T.);
#60096=EDGE_CURVE('',#45275,#45277,#24918,.T.);
#60097=EDGE_CURVE('',#45276,#45278,#24919,.T.);
#60098=EDGE_CURVE('',#45277,#45278,#24920,.T.);
#60099=EDGE_CURVE('',#45277,#45279,#36497,.T.);
#60100=EDGE_CURVE('',#45278,#45280,#36498,.T.);
#60101=EDGE_CURVE('',#45279,#45280,#24921,.T.);
#60102=EDGE_CURVE('',#45279,#45281,#24922,.T.);
#60103=EDGE_CURVE('',#45280,#45282,#24923,.T.);
#60104=EDGE_CURVE('',#45281,#45282,#24924,.T.);
#60105=EDGE_CURVE('',#45281,#45283,#24925,.T.);
#60106=EDGE_CURVE('',#45282,#45284,#24926,.T.);
#60107=EDGE_CURVE('',#45283,#45284,#24927,.T.);
#60108=EDGE_CURVE('',#45283,#45181,#24928,.T.);
#60109=EDGE_CURVE('',#45284,#45183,#24929,.T.);
#60110=EDGE_CURVE('',#45285,#45286,#24930,.T.);
#60111=EDGE_CURVE('',#45285,#45287,#24931,.T.);
#60112=EDGE_CURVE('',#45287,#45288,#24932,.T.);
#60113=EDGE_CURVE('',#45286,#45288,#24933,.T.);
#60114=EDGE_CURVE('',#45286,#45289,#24934,.T.);
#60115=EDGE_CURVE('',#45288,#45290,#24935,.T.);
#60116=EDGE_CURVE('',#45289,#45290,#24936,.T.);
#60117=EDGE_CURVE('',#45289,#45291,#24937,.T.);
#60118=EDGE_CURVE('',#45290,#45292,#24938,.T.);
#60119=EDGE_CURVE('',#45291,#45292,#24939,.T.);
#60120=EDGE_CURVE('',#45291,#45293,#24940,.T.);
#60121=EDGE_CURVE('',#45292,#45294,#24941,.T.);
#60122=EDGE_CURVE('',#45293,#45294,#24942,.T.);
#60123=EDGE_CURVE('',#45293,#45295,#36499,.T.);
#60124=EDGE_CURVE('',#45294,#45296,#36500,.T.);
#60125=EDGE_CURVE('',#45295,#45296,#24943,.T.);
#60126=EDGE_CURVE('',#45295,#45297,#24944,.T.);
#60127=EDGE_CURVE('',#45296,#45298,#24945,.T.);
#60128=EDGE_CURVE('',#45297,#45298,#24946,.T.);
#60129=EDGE_CURVE('',#45297,#45299,#36501,.T.);
#60130=EDGE_CURVE('',#45298,#45300,#36502,.T.);
#60131=EDGE_CURVE('',#45299,#45300,#24947,.T.);
#60132=EDGE_CURVE('',#45299,#45301,#24948,.T.);
#60133=EDGE_CURVE('',#45300,#45302,#24949,.T.);
#60134=EDGE_CURVE('',#45301,#45302,#24950,.T.);
#60135=EDGE_CURVE('',#45301,#45303,#36503,.T.);
#60136=EDGE_CURVE('',#45302,#45304,#36504,.T.);
#60137=EDGE_CURVE('',#45303,#45304,#24951,.T.);
#60138=EDGE_CURVE('',#45303,#45305,#24952,.T.);
#60139=EDGE_CURVE('',#45304,#45306,#24953,.T.);
#60140=EDGE_CURVE('',#45305,#45306,#24954,.T.);
#60141=EDGE_CURVE('',#45305,#45307,#36505,.T.);
#60142=EDGE_CURVE('',#45306,#45308,#36506,.T.);
#60143=EDGE_CURVE('',#45307,#45308,#24955,.T.);
#60144=EDGE_CURVE('',#45307,#45309,#24956,.T.);
#60145=EDGE_CURVE('',#45308,#45310,#24957,.T.);
#60146=EDGE_CURVE('',#45309,#45310,#24958,.T.);
#60147=EDGE_CURVE('',#45309,#45311,#24959,.T.);
#60148=EDGE_CURVE('',#45310,#45312,#24960,.T.);
#60149=EDGE_CURVE('',#45311,#45312,#24961,.T.);
#60150=EDGE_CURVE('',#45311,#45313,#24962,.T.);
#60151=EDGE_CURVE('',#45312,#45314,#24963,.T.);
#60152=EDGE_CURVE('',#45313,#45314,#24964,.T.);
#60153=EDGE_CURVE('',#45313,#45315,#24965,.T.);
#60154=EDGE_CURVE('',#45314,#45316,#24966,.T.);
#60155=EDGE_CURVE('',#45315,#45316,#24967,.T.);
#60156=EDGE_CURVE('',#45315,#45317,#36507,.T.);
#60157=EDGE_CURVE('',#45316,#45318,#36508,.T.);
#60158=EDGE_CURVE('',#45317,#45318,#24968,.T.);
#60159=EDGE_CURVE('',#45317,#45319,#24969,.T.);
#60160=EDGE_CURVE('',#45318,#45320,#24970,.T.);
#60161=EDGE_CURVE('',#45319,#45320,#24971,.T.);
#60162=EDGE_CURVE('',#45319,#45321,#36509,.T.);
#60163=EDGE_CURVE('',#45320,#45322,#36510,.T.);
#60164=EDGE_CURVE('',#45321,#45322,#24972,.T.);
#60165=EDGE_CURVE('',#45321,#45323,#24973,.T.);
#60166=EDGE_CURVE('',#45322,#45324,#24974,.T.);
#60167=EDGE_CURVE('',#45323,#45324,#24975,.T.);
#60168=EDGE_CURVE('',#45323,#45325,#36511,.T.);
#60169=EDGE_CURVE('',#45324,#45326,#36512,.T.);
#60170=EDGE_CURVE('',#45325,#45326,#24976,.T.);
#60171=EDGE_CURVE('',#45325,#45327,#24977,.T.);
#60172=EDGE_CURVE('',#45326,#45328,#24978,.T.);
#60173=EDGE_CURVE('',#45327,#45328,#24979,.T.);
#60174=EDGE_CURVE('',#45327,#45329,#36513,.T.);
#60175=EDGE_CURVE('',#45328,#45330,#36514,.T.);
#60176=EDGE_CURVE('',#45329,#45330,#24980,.T.);
#60177=EDGE_CURVE('',#45329,#45331,#24981,.T.);
#60178=EDGE_CURVE('',#45330,#45332,#24982,.T.);
#60179=EDGE_CURVE('',#45331,#45332,#24983,.T.);
#60180=EDGE_CURVE('',#45331,#45333,#24984,.T.);
#60181=EDGE_CURVE('',#45332,#45334,#24985,.T.);
#60182=EDGE_CURVE('',#45333,#45334,#24986,.T.);
#60183=EDGE_CURVE('',#45333,#45335,#24987,.T.);
#60184=EDGE_CURVE('',#45334,#45336,#24988,.T.);
#60185=EDGE_CURVE('',#45335,#45336,#24989,.T.);
#60186=EDGE_CURVE('',#45335,#45337,#24990,.T.);
#60187=EDGE_CURVE('',#45336,#45338,#24991,.T.);
#60188=EDGE_CURVE('',#45337,#45338,#24992,.T.);
#60189=EDGE_CURVE('',#45337,#45339,#36515,.T.);
#60190=EDGE_CURVE('',#45338,#45340,#36516,.T.);
#60191=EDGE_CURVE('',#45339,#45340,#24993,.T.);
#60192=EDGE_CURVE('',#45339,#45341,#24994,.T.);
#60193=EDGE_CURVE('',#45340,#45342,#24995,.T.);
#60194=EDGE_CURVE('',#45341,#45342,#24996,.T.);
#60195=EDGE_CURVE('',#45341,#45343,#24997,.T.);
#60196=EDGE_CURVE('',#45342,#45344,#24998,.T.);
#60197=EDGE_CURVE('',#45343,#45344,#24999,.T.);
#60198=EDGE_CURVE('',#45343,#45345,#25000,.T.);
#60199=EDGE_CURVE('',#45344,#45346,#25001,.T.);
#60200=EDGE_CURVE('',#45345,#45346,#25002,.T.);
#60201=EDGE_CURVE('',#45345,#45347,#25003,.T.);
#60202=EDGE_CURVE('',#45346,#45348,#25004,.T.);
#60203=EDGE_CURVE('',#45347,#45348,#25005,.T.);
#60204=EDGE_CURVE('',#45347,#45349,#36517,.T.);
#60205=EDGE_CURVE('',#45348,#45350,#36518,.T.);
#60206=EDGE_CURVE('',#45349,#45350,#25006,.T.);
#60207=EDGE_CURVE('',#45349,#45351,#25007,.T.);
#60208=EDGE_CURVE('',#45350,#45352,#25008,.T.);
#60209=EDGE_CURVE('',#45351,#45352,#25009,.T.);
#60210=EDGE_CURVE('',#45351,#45353,#36519,.T.);
#60211=EDGE_CURVE('',#45352,#45354,#36520,.T.);
#60212=EDGE_CURVE('',#45353,#45354,#25010,.T.);
#60213=EDGE_CURVE('',#45353,#45355,#25011,.T.);
#60214=EDGE_CURVE('',#45354,#45356,#25012,.T.);
#60215=EDGE_CURVE('',#45355,#45356,#25013,.T.);
#60216=EDGE_CURVE('',#45355,#45357,#36521,.T.);
#60217=EDGE_CURVE('',#45356,#45358,#36522,.T.);
#60218=EDGE_CURVE('',#45357,#45358,#25014,.T.);
#60219=EDGE_CURVE('',#45357,#45359,#25015,.T.);
#60220=EDGE_CURVE('',#45358,#45360,#25016,.T.);
#60221=EDGE_CURVE('',#45359,#45360,#25017,.T.);
#60222=EDGE_CURVE('',#45359,#45361,#36523,.T.);
#60223=EDGE_CURVE('',#45360,#45362,#36524,.T.);
#60224=EDGE_CURVE('',#45361,#45362,#25018,.T.);
#60225=EDGE_CURVE('',#45361,#45259,#25019,.T.);
#60226=EDGE_CURVE('',#45362,#45261,#25020,.T.);
#60227=EDGE_CURVE('',#45363,#45364,#25021,.T.);
#60228=EDGE_CURVE('',#45363,#45365,#25022,.T.);
#60229=EDGE_CURVE('',#45365,#45366,#25023,.T.);
#60230=EDGE_CURVE('',#45364,#45366,#25024,.T.);
#60231=EDGE_CURVE('',#45364,#45367,#25025,.T.);
#60232=EDGE_CURVE('',#45366,#45368,#25026,.T.);
#60233=EDGE_CURVE('',#45367,#45368,#25027,.T.);
#60234=EDGE_CURVE('',#45367,#45369,#25028,.T.);
#60235=EDGE_CURVE('',#45368,#45370,#25029,.T.);
#60236=EDGE_CURVE('',#45369,#45370,#25030,.T.);
#60237=EDGE_CURVE('',#45369,#45371,#36525,.T.);
#60238=EDGE_CURVE('',#45370,#45372,#36526,.T.);
#60239=EDGE_CURVE('',#45371,#45372,#25031,.T.);
#60240=EDGE_CURVE('',#45371,#45373,#25032,.T.);
#60241=EDGE_CURVE('',#45372,#45374,#25033,.T.);
#60242=EDGE_CURVE('',#45373,#45374,#25034,.T.);
#60243=EDGE_CURVE('',#45373,#45375,#36527,.T.);
#60244=EDGE_CURVE('',#45374,#45376,#36528,.T.);
#60245=EDGE_CURVE('',#45375,#45376,#25035,.T.);
#60246=EDGE_CURVE('',#45375,#45377,#25036,.T.);
#60247=EDGE_CURVE('',#45376,#45378,#25037,.T.);
#60248=EDGE_CURVE('',#45377,#45378,#25038,.T.);
#60249=EDGE_CURVE('',#45377,#45379,#36529,.T.);
#60250=EDGE_CURVE('',#45378,#45380,#36530,.T.);
#60251=EDGE_CURVE('',#45379,#45380,#25039,.T.);
#60252=EDGE_CURVE('',#45379,#45381,#25040,.T.);
#60253=EDGE_CURVE('',#45380,#45382,#25041,.T.);
#60254=EDGE_CURVE('',#45381,#45382,#25042,.T.);
#60255=EDGE_CURVE('',#45381,#45383,#36531,.T.);
#60256=EDGE_CURVE('',#45382,#45384,#36532,.T.);
#60257=EDGE_CURVE('',#45383,#45384,#25043,.T.);
#60258=EDGE_CURVE('',#45383,#45385,#25044,.T.);
#60259=EDGE_CURVE('',#45384,#45386,#25045,.T.);
#60260=EDGE_CURVE('',#45385,#45386,#25046,.T.);
#60261=EDGE_CURVE('',#45385,#45387,#25047,.T.);
#60262=EDGE_CURVE('',#45386,#45388,#25048,.T.);
#60263=EDGE_CURVE('',#45387,#45388,#25049,.T.);
#60264=EDGE_CURVE('',#45387,#45285,#25050,.T.);
#60265=EDGE_CURVE('',#45388,#45287,#25051,.T.);
#60266=EDGE_CURVE('',#45075,#45389,#25052,.T.);
#60267=EDGE_CURVE('',#45076,#45390,#25053,.T.);
#60268=EDGE_CURVE('',#45389,#45390,#25054,.T.);
#60269=EDGE_CURVE('',#45389,#45391,#25055,.T.);
#60270=EDGE_CURVE('',#45390,#45392,#25056,.T.);
#60271=EDGE_CURVE('',#45391,#45392,#25057,.T.);
#60272=EDGE_CURVE('',#45391,#45393,#25058,.T.);
#60273=EDGE_CURVE('',#45392,#45394,#25059,.T.);
#60274=EDGE_CURVE('',#45393,#45394,#25060,.T.);
#60275=EDGE_CURVE('',#45393,#45395,#36533,.T.);
#60276=EDGE_CURVE('',#45394,#45396,#36534,.T.);
#60277=EDGE_CURVE('',#45395,#45396,#25061,.T.);
#60278=EDGE_CURVE('',#45395,#45397,#25062,.T.);
#60279=EDGE_CURVE('',#45396,#45398,#25063,.T.);
#60280=EDGE_CURVE('',#45397,#45398,#25064,.T.);
#60281=EDGE_CURVE('',#45397,#45399,#36535,.T.);
#60282=EDGE_CURVE('',#45398,#45400,#36536,.T.);
#60283=EDGE_CURVE('',#45399,#45400,#25065,.T.);
#60284=EDGE_CURVE('',#45399,#45401,#25066,.T.);
#60285=EDGE_CURVE('',#45400,#45402,#25067,.T.);
#60286=EDGE_CURVE('',#45401,#45402,#25068,.T.);
#60287=EDGE_CURVE('',#45401,#45403,#36537,.T.);
#60288=EDGE_CURVE('',#45402,#45404,#36538,.T.);
#60289=EDGE_CURVE('',#45403,#45404,#25069,.T.);
#60290=EDGE_CURVE('',#45403,#45405,#25070,.T.);
#60291=EDGE_CURVE('',#45404,#45406,#25071,.T.);
#60292=EDGE_CURVE('',#45405,#45406,#25072,.T.);
#60293=EDGE_CURVE('',#45405,#45407,#36539,.T.);
#60294=EDGE_CURVE('',#45406,#45408,#36540,.T.);
#60295=EDGE_CURVE('',#45407,#45408,#25073,.T.);
#60296=EDGE_CURVE('',#45407,#45409,#25074,.T.);
#60297=EDGE_CURVE('',#45408,#45410,#25075,.T.);
#60298=EDGE_CURVE('',#45409,#45410,#25076,.T.);
#60299=EDGE_CURVE('',#45409,#45411,#25077,.T.);
#60300=EDGE_CURVE('',#45410,#45412,#25078,.T.);
#60301=EDGE_CURVE('',#45411,#45412,#25079,.T.);
#60302=EDGE_CURVE('',#45411,#45413,#25080,.T.);
#60303=EDGE_CURVE('',#45412,#45414,#25081,.T.);
#60304=EDGE_CURVE('',#45413,#45414,#25082,.T.);
#60305=EDGE_CURVE('',#45413,#45415,#25083,.T.);
#60306=EDGE_CURVE('',#45414,#45416,#25084,.T.);
#60307=EDGE_CURVE('',#45415,#45416,#25085,.T.);
#60308=EDGE_CURVE('',#45415,#45417,#36541,.T.);
#60309=EDGE_CURVE('',#45416,#45418,#36542,.T.);
#60310=EDGE_CURVE('',#45417,#45418,#25086,.T.);
#60311=EDGE_CURVE('',#45417,#45419,#25087,.T.);
#60312=EDGE_CURVE('',#45418,#45420,#25088,.T.);
#60313=EDGE_CURVE('',#45419,#45420,#25089,.T.);
#60314=EDGE_CURVE('',#45419,#45421,#36543,.T.);
#60315=EDGE_CURVE('',#45420,#45422,#36544,.T.);
#60316=EDGE_CURVE('',#45421,#45422,#25090,.T.);
#60317=EDGE_CURVE('',#45421,#45423,#25091,.T.);
#60318=EDGE_CURVE('',#45422,#45424,#25092,.T.);
#60319=EDGE_CURVE('',#45423,#45424,#25093,.T.);
#60320=EDGE_CURVE('',#45423,#45425,#36545,.T.);
#60321=EDGE_CURVE('',#45424,#45426,#36546,.T.);
#60322=EDGE_CURVE('',#45425,#45426,#25094,.T.);
#60323=EDGE_CURVE('',#45425,#45427,#25095,.T.);
#60324=EDGE_CURVE('',#45426,#45428,#25096,.T.);
#60325=EDGE_CURVE('',#45427,#45428,#25097,.T.);
#60326=EDGE_CURVE('',#45427,#45429,#36547,.T.);
#60327=EDGE_CURVE('',#45428,#45430,#36548,.T.);
#60328=EDGE_CURVE('',#45429,#45430,#25098,.T.);
#60329=EDGE_CURVE('',#45429,#45431,#25099,.T.);
#60330=EDGE_CURVE('',#45430,#45432,#25100,.T.);
#60331=EDGE_CURVE('',#45431,#45432,#25101,.T.);
#60332=EDGE_CURVE('',#45431,#45433,#25102,.T.);
#60333=EDGE_CURVE('',#45432,#45434,#25103,.T.);
#60334=EDGE_CURVE('',#45433,#45434,#25104,.T.);
#60335=EDGE_CURVE('',#45433,#45435,#25105,.T.);
#60336=EDGE_CURVE('',#45434,#45436,#25106,.T.);
#60337=EDGE_CURVE('',#45435,#45436,#25107,.T.);
#60338=EDGE_CURVE('',#45435,#45437,#25108,.T.);
#60339=EDGE_CURVE('',#45436,#45438,#25109,.T.);
#60340=EDGE_CURVE('',#45437,#45438,#25110,.T.);
#60341=EDGE_CURVE('',#45437,#45439,#36549,.T.);
#60342=EDGE_CURVE('',#45438,#45440,#36550,.T.);
#60343=EDGE_CURVE('',#45439,#45440,#25111,.T.);
#60344=EDGE_CURVE('',#45439,#45441,#25112,.T.);
#60345=EDGE_CURVE('',#45440,#45442,#25113,.T.);
#60346=EDGE_CURVE('',#45441,#45442,#25114,.T.);
#60347=EDGE_CURVE('',#45441,#45443,#25115,.T.);
#60348=EDGE_CURVE('',#45442,#45444,#25116,.T.);
#60349=EDGE_CURVE('',#45443,#45444,#25117,.T.);
#60350=EDGE_CURVE('',#45443,#45445,#25118,.T.);
#60351=EDGE_CURVE('',#45444,#45446,#25119,.T.);
#60352=EDGE_CURVE('',#45445,#45446,#25120,.T.);
#60353=EDGE_CURVE('',#45445,#45447,#25121,.T.);
#60354=EDGE_CURVE('',#45446,#45448,#25122,.T.);
#60355=EDGE_CURVE('',#45447,#45448,#25123,.T.);
#60356=EDGE_CURVE('',#45447,#45449,#36551,.T.);
#60357=EDGE_CURVE('',#45448,#45450,#36552,.T.);
#60358=EDGE_CURVE('',#45449,#45450,#25124,.T.);
#60359=EDGE_CURVE('',#45449,#45451,#25125,.T.);
#60360=EDGE_CURVE('',#45450,#45452,#25126,.T.);
#60361=EDGE_CURVE('',#45451,#45452,#25127,.T.);
#60362=EDGE_CURVE('',#45451,#45453,#36553,.T.);
#60363=EDGE_CURVE('',#45452,#45454,#36554,.T.);
#60364=EDGE_CURVE('',#45453,#45454,#25128,.T.);
#60365=EDGE_CURVE('',#45453,#45455,#25129,.T.);
#60366=EDGE_CURVE('',#45454,#45456,#25130,.T.);
#60367=EDGE_CURVE('',#45455,#45456,#25131,.T.);
#60368=EDGE_CURVE('',#45455,#45457,#36555,.T.);
#60369=EDGE_CURVE('',#45456,#45458,#36556,.T.);
#60370=EDGE_CURVE('',#45457,#45458,#25132,.T.);
#60371=EDGE_CURVE('',#45457,#45459,#25133,.T.);
#60372=EDGE_CURVE('',#45458,#45460,#25134,.T.);
#60373=EDGE_CURVE('',#45459,#45460,#25135,.T.);
#60374=EDGE_CURVE('',#45459,#45461,#36557,.T.);
#60375=EDGE_CURVE('',#45460,#45462,#36558,.T.);
#60376=EDGE_CURVE('',#45461,#45462,#25136,.T.);
#60377=EDGE_CURVE('',#45461,#45363,#25137,.T.);
#60378=EDGE_CURVE('',#45462,#45365,#25138,.T.);
#60379=EDGE_CURVE('',#45463,#45043,#25139,.T.);
#60380=EDGE_CURVE('',#45464,#45463,#25140,.T.);
#60381=EDGE_CURVE('',#45464,#45045,#25141,.T.);
#60382=EDGE_CURVE('',#45143,#45463,#25142,.T.);
#60383=EDGE_CURVE('',#45144,#45464,#25143,.T.);
#60384=EDGE_CURVE('',#45040,#45465,#25144,.T.);
#60385=EDGE_CURVE('',#45042,#45466,#25145,.T.);
#60386=EDGE_CURVE('',#45466,#45465,#25146,.T.);
#60387=EDGE_CURVE('',#45465,#45117,#25147,.T.);
#60388=EDGE_CURVE('',#45466,#45119,#25148,.T.);
#60389=EDGE_CURVE('',#45467,#45468,#25149,.T.);
#60390=EDGE_CURVE('',#45469,#45467,#25150,.T.);
#60391=EDGE_CURVE('',#45470,#45469,#25151,.T.);
#60392=EDGE_CURVE('',#45470,#45471,#25152,.T.);
#60393=EDGE_CURVE('',#45472,#45471,#25153,.T.);
#60394=EDGE_CURVE('',#45472,#45473,#25154,.T.);
#60395=EDGE_CURVE('',#45473,#45474,#25155,.T.);
#60396=EDGE_CURVE('',#45468,#45474,#25156,.T.);
#60397=EDGE_CURVE('',#45475,#45476,#25157,.T.);
#60398=EDGE_CURVE('',#45468,#45475,#25158,.T.);
#60399=EDGE_CURVE('',#45474,#45476,#25159,.T.);
#60400=EDGE_CURVE('',#45477,#45476,#25160,.T.);
#60401=EDGE_CURVE('',#45473,#45477,#25161,.T.);
#60402=EDGE_CURVE('',#45478,#45477,#25162,.T.);
#60403=EDGE_CURVE('',#45472,#45478,#25163,.T.);
#60404=EDGE_CURVE('',#45478,#45479,#25164,.T.);
#60405=EDGE_CURVE('',#45471,#45479,#25165,.T.);
#60406=EDGE_CURVE('',#45480,#45479,#25166,.T.);
#60407=EDGE_CURVE('',#45470,#45480,#25167,.T.);
#60408=EDGE_CURVE('',#45480,#45481,#25168,.T.);
#60409=EDGE_CURVE('',#45469,#45481,#25169,.T.);
#60410=EDGE_CURVE('',#45481,#45482,#25170,.T.);
#60411=EDGE_CURVE('',#45467,#45482,#25171,.T.);
#60412=EDGE_CURVE('',#45482,#45475,#25172,.T.);
#60413=EDGE_CURVE('',#45483,#45484,#25173,.T.);
#60414=EDGE_CURVE('',#45485,#45483,#25174,.T.);
#60415=EDGE_CURVE('',#45485,#45486,#25175,.T.);
#60416=EDGE_CURVE('',#45486,#45484,#25176,.T.);
#60417=EDGE_CURVE('',#45484,#45487,#25177,.T.);
#60418=EDGE_CURVE('',#45486,#45488,#25178,.T.);
#60419=EDGE_CURVE('',#45488,#45487,#25179,.T.);
#60420=EDGE_CURVE('',#45487,#45489,#25180,.T.);
#60421=EDGE_CURVE('',#45488,#45490,#25181,.T.);
#60422=EDGE_CURVE('',#45490,#45489,#25182,.T.);
#60423=EDGE_CURVE('',#45489,#45483,#25183,.T.);
#60424=EDGE_CURVE('',#45490,#45485,#25184,.T.);
#60425=ORIENTED_EDGE('',*,*,#45491,.T.);
#60426=ORIENTED_EDGE('',*,*,#45492,.T.);
#60427=ORIENTED_EDGE('',*,*,#45493,.T.);
#60428=ORIENTED_EDGE('',*,*,#45492,.F.);
#60429=ORIENTED_EDGE('',*,*,#45494,.T.);
#60430=ORIENTED_EDGE('',*,*,#45495,.T.);
#60431=ORIENTED_EDGE('',*,*,#45496,.T.);
#60432=ORIENTED_EDGE('',*,*,#45495,.F.);
#60433=ORIENTED_EDGE('',*,*,#45497,.T.);
#60434=ORIENTED_EDGE('',*,*,#45498,.T.);
#60435=ORIENTED_EDGE('',*,*,#45499,.T.);
#60436=ORIENTED_EDGE('',*,*,#45498,.F.);
#60437=ORIENTED_EDGE('',*,*,#45500,.T.);
#60438=ORIENTED_EDGE('',*,*,#45501,.T.);
#60439=ORIENTED_EDGE('',*,*,#45502,.T.);
#60440=ORIENTED_EDGE('',*,*,#45501,.F.);
#60441=ORIENTED_EDGE('',*,*,#45503,.F.);
#60442=ORIENTED_EDGE('',*,*,#45504,.F.);
#60443=ORIENTED_EDGE('',*,*,#45505,.T.);
#60444=ORIENTED_EDGE('',*,*,#45506,.T.);
#60445=ORIENTED_EDGE('',*,*,#45507,.F.);
#60446=ORIENTED_EDGE('',*,*,#45508,.F.);
#60447=ORIENTED_EDGE('',*,*,#45509,.T.);
#60448=ORIENTED_EDGE('',*,*,#45504,.T.);
#60449=ORIENTED_EDGE('',*,*,#45510,.F.);
#60450=ORIENTED_EDGE('',*,*,#45511,.F.);
#60451=ORIENTED_EDGE('',*,*,#45512,.T.);
#60452=ORIENTED_EDGE('',*,*,#45508,.T.);
#60453=ORIENTED_EDGE('',*,*,#45513,.F.);
#60454=ORIENTED_EDGE('',*,*,#45506,.F.);
#60455=ORIENTED_EDGE('',*,*,#45514,.T.);
#60456=ORIENTED_EDGE('',*,*,#45511,.T.);
#60457=ORIENTED_EDGE('',*,*,#45503,.T.);
#60458=ORIENTED_EDGE('',*,*,#45513,.T.);
#60459=ORIENTED_EDGE('',*,*,#45510,.T.);
#60460=ORIENTED_EDGE('',*,*,#45507,.T.);
#60461=ORIENTED_EDGE('',*,*,#45515,.F.);
#60462=ORIENTED_EDGE('',*,*,#45516,.F.);
#60463=ORIENTED_EDGE('',*,*,#45517,.F.);
#60464=ORIENTED_EDGE('',*,*,#45518,.F.);
#60465=ORIENTED_EDGE('',*,*,#45519,.T.);
#60466=ORIENTED_EDGE('',*,*,#45514,.F.);
#60467=ORIENTED_EDGE('',*,*,#45520,.F.);
#60468=ORIENTED_EDGE('',*,*,#45521,.F.);
#60469=ORIENTED_EDGE('',*,*,#45520,.T.);
#60470=ORIENTED_EDGE('',*,*,#45505,.F.);
#60471=ORIENTED_EDGE('',*,*,#45522,.F.);
#60472=ORIENTED_EDGE('',*,*,#45523,.F.);
#60473=ORIENTED_EDGE('',*,*,#45524,.T.);
#60474=ORIENTED_EDGE('',*,*,#45512,.F.);
#60475=ORIENTED_EDGE('',*,*,#45519,.F.);
#60476=ORIENTED_EDGE('',*,*,#45525,.F.);
#60477=ORIENTED_EDGE('',*,*,#45522,.T.);
#60478=ORIENTED_EDGE('',*,*,#45509,.F.);
#60479=ORIENTED_EDGE('',*,*,#45524,.F.);
#60480=ORIENTED_EDGE('',*,*,#45526,.F.);
#60481=ORIENTED_EDGE('',*,*,#45515,.T.);
#60482=ORIENTED_EDGE('',*,*,#45527,.F.);
#60483=ORIENTED_EDGE('',*,*,#45528,.F.);
#60484=ORIENTED_EDGE('',*,*,#45529,.T.);
#60485=ORIENTED_EDGE('',*,*,#45516,.T.);
#60486=ORIENTED_EDGE('',*,*,#45529,.F.);
#60487=ORIENTED_EDGE('',*,*,#45530,.F.);
#60488=ORIENTED_EDGE('',*,*,#45531,.T.);
#60489=ORIENTED_EDGE('',*,*,#45517,.T.);
#60490=ORIENTED_EDGE('',*,*,#45531,.F.);
#60491=ORIENTED_EDGE('',*,*,#45532,.F.);
#60492=ORIENTED_EDGE('',*,*,#45533,.T.);
#60493=ORIENTED_EDGE('',*,*,#45518,.T.);
#60494=ORIENTED_EDGE('',*,*,#45533,.F.);
#60495=ORIENTED_EDGE('',*,*,#45534,.F.);
#60496=ORIENTED_EDGE('',*,*,#45527,.T.);
#60497=ORIENTED_EDGE('',*,*,#45535,.F.);
#60498=ORIENTED_EDGE('',*,*,#45536,.T.);
#60499=ORIENTED_EDGE('',*,*,#45537,.T.);
#60500=ORIENTED_EDGE('',*,*,#45534,.T.);
#60501=ORIENTED_EDGE('',*,*,#45537,.F.);
#60502=ORIENTED_EDGE('',*,*,#45538,.T.);
#60503=ORIENTED_EDGE('',*,*,#45539,.T.);
#60504=ORIENTED_EDGE('',*,*,#45528,.T.);
#60505=ORIENTED_EDGE('',*,*,#45540,.F.);
#60506=ORIENTED_EDGE('',*,*,#45541,.T.);
#60507=ORIENTED_EDGE('',*,*,#45535,.T.);
#60508=ORIENTED_EDGE('',*,*,#45532,.T.);
#60509=ORIENTED_EDGE('',*,*,#45539,.F.);
#60510=ORIENTED_EDGE('',*,*,#45542,.T.);
#60511=ORIENTED_EDGE('',*,*,#45540,.T.);
#60512=ORIENTED_EDGE('',*,*,#45530,.T.);
#60513=ORIENTED_EDGE('',*,*,#45543,.F.);
#60514=ORIENTED_EDGE('',*,*,#45544,.T.);
#60515=ORIENTED_EDGE('',*,*,#45545,.T.);
#60516=ORIENTED_EDGE('',*,*,#45536,.F.);
#60517=ORIENTED_EDGE('',*,*,#45545,.F.);
#60518=ORIENTED_EDGE('',*,*,#45546,.T.);
#60519=ORIENTED_EDGE('',*,*,#45547,.T.);
#60520=ORIENTED_EDGE('',*,*,#45538,.F.);
#60521=ORIENTED_EDGE('',*,*,#45547,.F.);
#60522=ORIENTED_EDGE('',*,*,#45548,.T.);
#60523=ORIENTED_EDGE('',*,*,#45549,.T.);
#60524=ORIENTED_EDGE('',*,*,#45542,.F.);
#60525=ORIENTED_EDGE('',*,*,#45549,.F.);
#60526=ORIENTED_EDGE('',*,*,#45550,.T.);
#60527=ORIENTED_EDGE('',*,*,#45543,.T.);
#60528=ORIENTED_EDGE('',*,*,#45541,.F.);
#60529=ORIENTED_EDGE('',*,*,#45551,.T.);
#60530=ORIENTED_EDGE('',*,*,#45552,.T.);
#60531=ORIENTED_EDGE('',*,*,#45553,.T.);
#60532=ORIENTED_EDGE('',*,*,#45554,.T.);
#60533=ORIENTED_EDGE('',*,*,#45555,.T.);
#60534=ORIENTED_EDGE('',*,*,#45556,.T.);
#60535=ORIENTED_EDGE('',*,*,#45557,.T.);
#60536=ORIENTED_EDGE('',*,*,#45558,.T.);
#60537=ORIENTED_EDGE('',*,*,#45491,.F.);
#60538=ORIENTED_EDGE('',*,*,#45494,.F.);
#60539=ORIENTED_EDGE('',*,*,#45497,.F.);
#60540=ORIENTED_EDGE('',*,*,#45500,.F.);
#60541=ORIENTED_EDGE('',*,*,#45526,.T.);
#60542=ORIENTED_EDGE('',*,*,#45525,.T.);
#60543=ORIENTED_EDGE('',*,*,#45521,.T.);
#60544=ORIENTED_EDGE('',*,*,#45523,.T.);
#60545=ORIENTED_EDGE('',*,*,#45559,.T.);
#60546=ORIENTED_EDGE('',*,*,#45560,.T.);
#60547=ORIENTED_EDGE('',*,*,#45561,.T.);
#60548=ORIENTED_EDGE('',*,*,#45562,.T.);
#60549=ORIENTED_EDGE('',*,*,#45563,.T.);
#60550=ORIENTED_EDGE('',*,*,#45564,.T.);
#60551=ORIENTED_EDGE('',*,*,#45565,.T.);
#60552=ORIENTED_EDGE('',*,*,#45566,.T.);
#60553=ORIENTED_EDGE('',*,*,#45548,.F.);
#60554=ORIENTED_EDGE('',*,*,#45546,.F.);
#60555=ORIENTED_EDGE('',*,*,#45544,.F.);
#60556=ORIENTED_EDGE('',*,*,#45550,.F.);
#60557=ORIENTED_EDGE('',*,*,#45493,.F.);
#60558=ORIENTED_EDGE('',*,*,#45496,.F.);
#60559=ORIENTED_EDGE('',*,*,#45499,.F.);
#60560=ORIENTED_EDGE('',*,*,#45502,.F.);
#60561=ORIENTED_EDGE('',*,*,#45567,.T.);
#60562=ORIENTED_EDGE('',*,*,#45568,.T.);
#60563=ORIENTED_EDGE('',*,*,#45569,.T.);
#60564=ORIENTED_EDGE('',*,*,#45559,.F.);
#60565=ORIENTED_EDGE('',*,*,#45570,.T.);
#60566=ORIENTED_EDGE('',*,*,#45571,.T.);
#60567=ORIENTED_EDGE('',*,*,#45572,.T.);
#60568=ORIENTED_EDGE('',*,*,#45561,.F.);
#60569=ORIENTED_EDGE('',*,*,#45573,.T.);
#60570=ORIENTED_EDGE('',*,*,#45574,.T.);
#60571=ORIENTED_EDGE('',*,*,#45575,.T.);
#60572=ORIENTED_EDGE('',*,*,#45563,.F.);
#60573=ORIENTED_EDGE('',*,*,#45576,.T.);
#60574=ORIENTED_EDGE('',*,*,#45577,.T.);
#60575=ORIENTED_EDGE('',*,*,#45578,.T.);
#60576=ORIENTED_EDGE('',*,*,#45565,.F.);
#60577=ORIENTED_EDGE('',*,*,#45569,.F.);
#60578=ORIENTED_EDGE('',*,*,#45579,.T.);
#60579=ORIENTED_EDGE('',*,*,#45570,.F.);
#60580=ORIENTED_EDGE('',*,*,#45560,.F.);
#60581=ORIENTED_EDGE('',*,*,#45578,.F.);
#60582=ORIENTED_EDGE('',*,*,#45580,.T.);
#60583=ORIENTED_EDGE('',*,*,#45567,.F.);
#60584=ORIENTED_EDGE('',*,*,#45566,.F.);
#60585=ORIENTED_EDGE('',*,*,#45575,.F.);
#60586=ORIENTED_EDGE('',*,*,#45581,.T.);
#60587=ORIENTED_EDGE('',*,*,#45576,.F.);
#60588=ORIENTED_EDGE('',*,*,#45564,.F.);
#60589=ORIENTED_EDGE('',*,*,#45572,.F.);
#60590=ORIENTED_EDGE('',*,*,#45582,.T.);
#60591=ORIENTED_EDGE('',*,*,#45573,.F.);
#60592=ORIENTED_EDGE('',*,*,#45562,.F.);
#60593=ORIENTED_EDGE('',*,*,#45583,.F.);
#60594=ORIENTED_EDGE('',*,*,#45582,.F.);
#60595=ORIENTED_EDGE('',*,*,#45584,.F.);
#60596=ORIENTED_EDGE('',*,*,#45556,.F.);
#60597=ORIENTED_EDGE('',*,*,#45584,.T.);
#60598=ORIENTED_EDGE('',*,*,#45571,.F.);
#60599=ORIENTED_EDGE('',*,*,#45585,.F.);
#60600=ORIENTED_EDGE('',*,*,#45557,.F.);
#60601=ORIENTED_EDGE('',*,*,#45583,.T.);
#60602=ORIENTED_EDGE('',*,*,#45555,.F.);
#60603=ORIENTED_EDGE('',*,*,#45586,.F.);
#60604=ORIENTED_EDGE('',*,*,#45574,.F.);
#60605=ORIENTED_EDGE('',*,*,#45585,.T.);
#60606=ORIENTED_EDGE('',*,*,#45579,.F.);
#60607=ORIENTED_EDGE('',*,*,#45587,.F.);
#60608=ORIENTED_EDGE('',*,*,#45558,.F.);
#60609=ORIENTED_EDGE('',*,*,#45586,.T.);
#60610=ORIENTED_EDGE('',*,*,#45554,.F.);
#60611=ORIENTED_EDGE('',*,*,#45588,.F.);
#60612=ORIENTED_EDGE('',*,*,#45581,.F.);
#60613=ORIENTED_EDGE('',*,*,#45587,.T.);
#60614=ORIENTED_EDGE('',*,*,#45568,.F.);
#60615=ORIENTED_EDGE('',*,*,#45589,.F.);
#60616=ORIENTED_EDGE('',*,*,#45551,.F.);
#60617=ORIENTED_EDGE('',*,*,#45588,.T.);
#60618=ORIENTED_EDGE('',*,*,#45553,.F.);
#60619=ORIENTED_EDGE('',*,*,#45590,.F.);
#60620=ORIENTED_EDGE('',*,*,#45577,.F.);
#60621=ORIENTED_EDGE('',*,*,#45589,.T.);
#60622=ORIENTED_EDGE('',*,*,#45580,.F.);
#60623=ORIENTED_EDGE('',*,*,#45590,.T.);
#60624=ORIENTED_EDGE('',*,*,#45552,.F.);
#60625=ORIENTED_EDGE('',*,*,#45591,.F.);
#60626=ORIENTED_EDGE('',*,*,#45592,.F.);
#60627=ORIENTED_EDGE('',*,*,#45593,.T.);
#60628=ORIENTED_EDGE('',*,*,#45594,.F.);
#60629=ORIENTED_EDGE('',*,*,#45593,.F.);
#60630=ORIENTED_EDGE('',*,*,#45595,.F.);
#60631=ORIENTED_EDGE('',*,*,#45596,.T.);
#60632=ORIENTED_EDGE('',*,*,#45597,.F.);
#60633=ORIENTED_EDGE('',*,*,#45598,.F.);
#60634=ORIENTED_EDGE('',*,*,#45596,.F.);
#60635=ORIENTED_EDGE('',*,*,#45599,.T.);
#60636=ORIENTED_EDGE('',*,*,#45600,.T.);
#60637=ORIENTED_EDGE('',*,*,#45601,.T.);
#60638=ORIENTED_EDGE('',*,*,#45602,.T.);
#60639=ORIENTED_EDGE('',*,*,#45600,.F.);
#60640=ORIENTED_EDGE('',*,*,#45603,.T.);
#60641=ORIENTED_EDGE('',*,*,#45604,.T.);
#60642=ORIENTED_EDGE('',*,*,#45605,.T.);
#60643=ORIENTED_EDGE('',*,*,#45606,.T.);
#60644=ORIENTED_EDGE('',*,*,#45607,.T.);
#60645=ORIENTED_EDGE('',*,*,#45605,.F.);
#60646=ORIENTED_EDGE('',*,*,#45608,.T.);
#60647=ORIENTED_EDGE('',*,*,#45609,.T.);
#60648=ORIENTED_EDGE('',*,*,#45610,.T.);
#60649=ORIENTED_EDGE('',*,*,#45611,.T.);
#60650=ORIENTED_EDGE('',*,*,#45612,.T.);
#60651=ORIENTED_EDGE('',*,*,#45610,.F.);
#60652=ORIENTED_EDGE('',*,*,#45613,.T.);
#60653=ORIENTED_EDGE('',*,*,#45614,.T.);
#60654=ORIENTED_EDGE('',*,*,#45615,.T.);
#60655=ORIENTED_EDGE('',*,*,#45616,.T.);
#60656=ORIENTED_EDGE('',*,*,#45617,.T.);
#60657=ORIENTED_EDGE('',*,*,#45615,.F.);
#60658=ORIENTED_EDGE('',*,*,#45618,.T.);
#60659=ORIENTED_EDGE('',*,*,#45619,.F.);
#60660=ORIENTED_EDGE('',*,*,#45620,.T.);
#60661=ORIENTED_EDGE('',*,*,#45616,.F.);
#60662=ORIENTED_EDGE('',*,*,#45621,.T.);
#60663=ORIENTED_EDGE('',*,*,#45597,.T.);
#60664=ORIENTED_EDGE('',*,*,#45598,.T.);
#60665=ORIENTED_EDGE('',*,*,#45621,.F.);
#60666=ORIENTED_EDGE('',*,*,#45617,.F.);
#60667=ORIENTED_EDGE('',*,*,#45620,.F.);
#60668=ORIENTED_EDGE('',*,*,#45609,.F.);
#60669=ORIENTED_EDGE('',*,*,#45613,.F.);
#60670=ORIENTED_EDGE('',*,*,#45599,.F.);
#60671=ORIENTED_EDGE('',*,*,#45603,.F.);
#60672=ORIENTED_EDGE('',*,*,#45607,.F.);
#60673=ORIENTED_EDGE('',*,*,#45606,.F.);
#60674=ORIENTED_EDGE('',*,*,#45591,.T.);
#60675=ORIENTED_EDGE('',*,*,#45592,.T.);
#60676=ORIENTED_EDGE('',*,*,#45622,.T.);
#60677=ORIENTED_EDGE('',*,*,#45614,.F.);
#60678=ORIENTED_EDGE('',*,*,#45623,.T.);
#60679=ORIENTED_EDGE('',*,*,#45624,.T.);
#60680=ORIENTED_EDGE('',*,*,#45623,.F.);
#60681=ORIENTED_EDGE('',*,*,#45618,.F.);
#60682=ORIENTED_EDGE('',*,*,#45622,.F.);
#60683=ORIENTED_EDGE('',*,*,#45612,.F.);
#60684=ORIENTED_EDGE('',*,*,#45611,.F.);
#60685=ORIENTED_EDGE('',*,*,#45604,.F.);
#60686=ORIENTED_EDGE('',*,*,#45608,.F.);
#60687=ORIENTED_EDGE('',*,*,#45602,.F.);
#60688=ORIENTED_EDGE('',*,*,#45601,.F.);
#60689=ORIENTED_EDGE('',*,*,#45595,.T.);
#60690=ORIENTED_EDGE('',*,*,#45594,.T.);
#60691=ORIENTED_EDGE('',*,*,#45619,.T.);
#60692=ORIENTED_EDGE('',*,*,#45624,.F.);
#60693=ORIENTED_EDGE('',*,*,#45625,.F.);
#60694=ORIENTED_EDGE('',*,*,#45626,.F.);
#60695=ORIENTED_EDGE('',*,*,#45627,.F.);
#60696=ORIENTED_EDGE('',*,*,#45628,.T.);
#60697=ORIENTED_EDGE('',*,*,#45629,.F.);
#60698=ORIENTED_EDGE('',*,*,#45630,.F.);
#60699=ORIENTED_EDGE('',*,*,#45625,.T.);
#60700=ORIENTED_EDGE('',*,*,#45631,.T.);
#60701=ORIENTED_EDGE('',*,*,#45632,.F.);
#60702=ORIENTED_EDGE('',*,*,#45633,.F.);
#60703=ORIENTED_EDGE('',*,*,#45629,.T.);
#60704=ORIENTED_EDGE('',*,*,#45634,.T.);
#60705=ORIENTED_EDGE('',*,*,#45635,.F.);
#60706=ORIENTED_EDGE('',*,*,#45636,.F.);
#60707=ORIENTED_EDGE('',*,*,#45632,.T.);
#60708=ORIENTED_EDGE('',*,*,#45637,.T.);
#60709=ORIENTED_EDGE('',*,*,#45638,.F.);
#60710=ORIENTED_EDGE('',*,*,#45639,.F.);
#60711=ORIENTED_EDGE('',*,*,#45635,.T.);
#60712=ORIENTED_EDGE('',*,*,#45640,.T.);
#60713=ORIENTED_EDGE('',*,*,#45641,.F.);
#60714=ORIENTED_EDGE('',*,*,#45642,.F.);
#60715=ORIENTED_EDGE('',*,*,#45638,.T.);
#60716=ORIENTED_EDGE('',*,*,#45643,.T.);
#60717=ORIENTED_EDGE('',*,*,#45644,.F.);
#60718=ORIENTED_EDGE('',*,*,#45645,.F.);
#60719=ORIENTED_EDGE('',*,*,#45641,.T.);
#60720=ORIENTED_EDGE('',*,*,#45646,.T.);
#60721=ORIENTED_EDGE('',*,*,#45647,.F.);
#60722=ORIENTED_EDGE('',*,*,#45648,.F.);
#60723=ORIENTED_EDGE('',*,*,#45644,.T.);
#60724=ORIENTED_EDGE('',*,*,#45649,.T.);
#60725=ORIENTED_EDGE('',*,*,#45650,.F.);
#60726=ORIENTED_EDGE('',*,*,#45651,.F.);
#60727=ORIENTED_EDGE('',*,*,#45652,.T.);
#60728=ORIENTED_EDGE('',*,*,#45653,.F.);
#60729=ORIENTED_EDGE('',*,*,#45654,.F.);
#60730=ORIENTED_EDGE('',*,*,#45655,.F.);
#60731=ORIENTED_EDGE('',*,*,#45656,.F.);
#60732=ORIENTED_EDGE('',*,*,#45657,.F.);
#60733=ORIENTED_EDGE('',*,*,#45658,.F.);
#60734=ORIENTED_EDGE('',*,*,#45659,.F.);
#60735=ORIENTED_EDGE('',*,*,#45660,.F.);
#60736=ORIENTED_EDGE('',*,*,#45661,.F.);
#60737=ORIENTED_EDGE('',*,*,#45650,.T.);
#60738=ORIENTED_EDGE('',*,*,#45662,.F.);
#60739=ORIENTED_EDGE('',*,*,#45654,.T.);
#60740=ORIENTED_EDGE('',*,*,#45663,.T.);
#60741=ORIENTED_EDGE('',*,*,#45664,.F.);
#60742=ORIENTED_EDGE('',*,*,#45665,.F.);
#60743=ORIENTED_EDGE('',*,*,#45666,.F.);
#60744=ORIENTED_EDGE('',*,*,#45667,.F.);
#60745=ORIENTED_EDGE('',*,*,#45660,.T.);
#60746=ORIENTED_EDGE('',*,*,#45668,.T.);
#60747=ORIENTED_EDGE('',*,*,#45669,.F.);
#60748=ORIENTED_EDGE('',*,*,#45670,.F.);
#60749=ORIENTED_EDGE('',*,*,#45666,.T.);
#60750=ORIENTED_EDGE('',*,*,#45671,.T.);
#60751=ORIENTED_EDGE('',*,*,#45672,.F.);
#60752=ORIENTED_EDGE('',*,*,#45673,.F.);
#60753=ORIENTED_EDGE('',*,*,#45669,.T.);
#60754=ORIENTED_EDGE('',*,*,#45674,.T.);
#60755=ORIENTED_EDGE('',*,*,#45675,.F.);
#60756=ORIENTED_EDGE('',*,*,#45676,.F.);
#60757=ORIENTED_EDGE('',*,*,#45672,.T.);
#60758=ORIENTED_EDGE('',*,*,#45677,.T.);
#60759=ORIENTED_EDGE('',*,*,#45678,.F.);
#60760=ORIENTED_EDGE('',*,*,#45679,.F.);
#60761=ORIENTED_EDGE('',*,*,#45675,.T.);
#60762=ORIENTED_EDGE('',*,*,#45680,.T.);
#60763=ORIENTED_EDGE('',*,*,#45681,.F.);
#60764=ORIENTED_EDGE('',*,*,#45682,.F.);
#60765=ORIENTED_EDGE('',*,*,#45678,.T.);
#60766=ORIENTED_EDGE('',*,*,#45683,.T.);
#60767=ORIENTED_EDGE('',*,*,#45684,.F.);
#60768=ORIENTED_EDGE('',*,*,#45685,.T.);
#60769=ORIENTED_EDGE('',*,*,#45686,.F.);
#60770=ORIENTED_EDGE('',*,*,#45687,.T.);
#60771=ORIENTED_EDGE('',*,*,#45688,.F.);
#60772=ORIENTED_EDGE('',*,*,#45689,.T.);
#60773=ORIENTED_EDGE('',*,*,#45684,.T.);
#60774=ORIENTED_EDGE('',*,*,#45690,.T.);
#60775=ORIENTED_EDGE('',*,*,#45691,.F.);
#60776=ORIENTED_EDGE('',*,*,#45692,.T.);
#60777=ORIENTED_EDGE('',*,*,#45688,.T.);
#60778=ORIENTED_EDGE('',*,*,#45693,.T.);
#60779=ORIENTED_EDGE('',*,*,#45694,.F.);
#60780=ORIENTED_EDGE('',*,*,#45695,.T.);
#60781=ORIENTED_EDGE('',*,*,#45691,.T.);
#60782=ORIENTED_EDGE('',*,*,#45696,.T.);
#60783=ORIENTED_EDGE('',*,*,#45697,.F.);
#60784=ORIENTED_EDGE('',*,*,#45698,.T.);
#60785=ORIENTED_EDGE('',*,*,#45694,.T.);
#60786=ORIENTED_EDGE('',*,*,#45699,.T.);
#60787=ORIENTED_EDGE('',*,*,#45700,.F.);
#60788=ORIENTED_EDGE('',*,*,#45701,.T.);
#60789=ORIENTED_EDGE('',*,*,#45697,.T.);
#60790=ORIENTED_EDGE('',*,*,#45702,.T.);
#60791=ORIENTED_EDGE('',*,*,#45703,.F.);
#60792=ORIENTED_EDGE('',*,*,#45704,.T.);
#60793=ORIENTED_EDGE('',*,*,#45700,.T.);
#60794=ORIENTED_EDGE('',*,*,#45705,.T.);
#60795=ORIENTED_EDGE('',*,*,#45706,.F.);
#60796=ORIENTED_EDGE('',*,*,#45707,.T.);
#60797=ORIENTED_EDGE('',*,*,#45703,.T.);
#60798=ORIENTED_EDGE('',*,*,#45708,.T.);
#60799=ORIENTED_EDGE('',*,*,#45658,.T.);
#60800=ORIENTED_EDGE('',*,*,#45709,.T.);
#60801=ORIENTED_EDGE('',*,*,#45710,.T.);
#60802=ORIENTED_EDGE('',*,*,#45711,.T.);
#60803=ORIENTED_EDGE('',*,*,#45709,.F.);
#60804=ORIENTED_EDGE('',*,*,#45659,.T.);
#60805=ORIENTED_EDGE('',*,*,#45712,.T.);
#60806=ORIENTED_EDGE('',*,*,#45713,.T.);
#60807=ORIENTED_EDGE('',*,*,#45657,.T.);
#60808=ORIENTED_EDGE('',*,*,#45656,.T.);
#60809=ORIENTED_EDGE('',*,*,#45713,.F.);
#60810=ORIENTED_EDGE('',*,*,#45714,.T.);
#60811=ORIENTED_EDGE('',*,*,#45664,.T.);
#60812=ORIENTED_EDGE('',*,*,#45715,.T.);
#60813=ORIENTED_EDGE('',*,*,#45716,.T.);
#60814=ORIENTED_EDGE('',*,*,#45717,.T.);
#60815=ORIENTED_EDGE('',*,*,#45715,.F.);
#60816=ORIENTED_EDGE('',*,*,#45665,.T.);
#60817=ORIENTED_EDGE('',*,*,#45718,.T.);
#60818=ORIENTED_EDGE('',*,*,#45719,.T.);
#60819=ORIENTED_EDGE('',*,*,#45662,.T.);
#60820=ORIENTED_EDGE('',*,*,#45655,.T.);
#60821=ORIENTED_EDGE('',*,*,#45719,.F.);
#60822=ORIENTED_EDGE('',*,*,#45720,.T.);
#60823=ORIENTED_EDGE('',*,*,#45706,.T.);
#60824=ORIENTED_EDGE('',*,*,#45721,.T.);
#60825=ORIENTED_EDGE('',*,*,#45722,.F.);
#60826=ORIENTED_EDGE('',*,*,#45723,.T.);
#60827=ORIENTED_EDGE('',*,*,#45681,.T.);
#60828=ORIENTED_EDGE('',*,*,#45724,.T.);
#60829=ORIENTED_EDGE('',*,*,#45725,.T.);
#60830=ORIENTED_EDGE('',*,*,#45726,.T.);
#60831=ORIENTED_EDGE('',*,*,#45727,.F.);
#60832=ORIENTED_EDGE('',*,*,#45728,.F.);
#60833=ORIENTED_EDGE('',*,*,#45729,.T.);
#60834=ORIENTED_EDGE('',*,*,#45718,.F.);
#60835=ORIENTED_EDGE('',*,*,#45730,.T.);
#60836=ORIENTED_EDGE('',*,*,#45731,.T.);
#60837=ORIENTED_EDGE('',*,*,#45730,.F.);
#60838=ORIENTED_EDGE('',*,*,#45720,.F.);
#60839=ORIENTED_EDGE('',*,*,#45729,.F.);
#60840=ORIENTED_EDGE('',*,*,#45717,.F.);
#60841=ORIENTED_EDGE('',*,*,#45716,.F.);
#60842=ORIENTED_EDGE('',*,*,#45712,.F.);
#60843=ORIENTED_EDGE('',*,*,#45714,.F.);
#60844=ORIENTED_EDGE('',*,*,#45711,.F.);
#60845=ORIENTED_EDGE('',*,*,#45710,.F.);
#60846=ORIENTED_EDGE('',*,*,#45732,.F.);
#60847=ORIENTED_EDGE('',*,*,#45733,.F.);
#60848=ORIENTED_EDGE('',*,*,#45734,.F.);
#60849=ORIENTED_EDGE('',*,*,#45721,.F.);
#60850=ORIENTED_EDGE('',*,*,#45708,.F.);
#60851=ORIENTED_EDGE('',*,*,#45705,.F.);
#60852=ORIENTED_EDGE('',*,*,#45702,.F.);
#60853=ORIENTED_EDGE('',*,*,#45699,.F.);
#60854=ORIENTED_EDGE('',*,*,#45696,.F.);
#60855=ORIENTED_EDGE('',*,*,#45693,.F.);
#60856=ORIENTED_EDGE('',*,*,#45690,.F.);
#60857=ORIENTED_EDGE('',*,*,#45687,.F.);
#60858=ORIENTED_EDGE('',*,*,#45735,.F.);
#60859=ORIENTED_EDGE('',*,*,#45685,.F.);
#60860=ORIENTED_EDGE('',*,*,#45689,.F.);
#60861=ORIENTED_EDGE('',*,*,#45692,.F.);
#60862=ORIENTED_EDGE('',*,*,#45695,.F.);
#60863=ORIENTED_EDGE('',*,*,#45698,.F.);
#60864=ORIENTED_EDGE('',*,*,#45701,.F.);
#60865=ORIENTED_EDGE('',*,*,#45704,.F.);
#60866=ORIENTED_EDGE('',*,*,#45707,.F.);
#60867=ORIENTED_EDGE('',*,*,#45723,.F.);
#60868=ORIENTED_EDGE('',*,*,#45736,.F.);
#60869=ORIENTED_EDGE('',*,*,#45626,.T.);
#60870=ORIENTED_EDGE('',*,*,#45630,.T.);
#60871=ORIENTED_EDGE('',*,*,#45633,.T.);
#60872=ORIENTED_EDGE('',*,*,#45636,.T.);
#60873=ORIENTED_EDGE('',*,*,#45639,.T.);
#60874=ORIENTED_EDGE('',*,*,#45642,.T.);
#60875=ORIENTED_EDGE('',*,*,#45645,.T.);
#60876=ORIENTED_EDGE('',*,*,#45648,.T.);
#60877=ORIENTED_EDGE('',*,*,#45737,.T.);
#60878=ORIENTED_EDGE('',*,*,#45738,.F.);
#60879=ORIENTED_EDGE('',*,*,#45739,.F.);
#60880=ORIENTED_EDGE('',*,*,#45649,.F.);
#60881=ORIENTED_EDGE('',*,*,#45646,.F.);
#60882=ORIENTED_EDGE('',*,*,#45643,.F.);
#60883=ORIENTED_EDGE('',*,*,#45640,.F.);
#60884=ORIENTED_EDGE('',*,*,#45637,.F.);
#60885=ORIENTED_EDGE('',*,*,#45634,.F.);
#60886=ORIENTED_EDGE('',*,*,#45631,.F.);
#60887=ORIENTED_EDGE('',*,*,#45628,.F.);
#60888=ORIENTED_EDGE('',*,*,#45740,.F.);
#60889=ORIENTED_EDGE('',*,*,#45651,.T.);
#60890=ORIENTED_EDGE('',*,*,#45661,.T.);
#60891=ORIENTED_EDGE('',*,*,#45667,.T.);
#60892=ORIENTED_EDGE('',*,*,#45670,.T.);
#60893=ORIENTED_EDGE('',*,*,#45673,.T.);
#60894=ORIENTED_EDGE('',*,*,#45676,.T.);
#60895=ORIENTED_EDGE('',*,*,#45679,.T.);
#60896=ORIENTED_EDGE('',*,*,#45682,.T.);
#60897=ORIENTED_EDGE('',*,*,#45727,.T.);
#60898=ORIENTED_EDGE('',*,*,#45741,.F.);
#60899=ORIENTED_EDGE('',*,*,#45725,.F.);
#60900=ORIENTED_EDGE('',*,*,#45724,.F.);
#60901=ORIENTED_EDGE('',*,*,#45683,.F.);
#60902=ORIENTED_EDGE('',*,*,#45680,.F.);
#60903=ORIENTED_EDGE('',*,*,#45677,.F.);
#60904=ORIENTED_EDGE('',*,*,#45674,.F.);
#60905=ORIENTED_EDGE('',*,*,#45671,.F.);
#60906=ORIENTED_EDGE('',*,*,#45668,.F.);
#60907=ORIENTED_EDGE('',*,*,#45663,.F.);
#60908=ORIENTED_EDGE('',*,*,#45742,.F.);
#60909=ORIENTED_EDGE('',*,*,#45743,.T.);
#60910=ORIENTED_EDGE('',*,*,#45744,.F.);
#60911=ORIENTED_EDGE('',*,*,#45743,.F.);
#60912=ORIENTED_EDGE('',*,*,#45745,.F.);
#60913=ORIENTED_EDGE('',*,*,#45733,.T.);
#60914=ORIENTED_EDGE('',*,*,#45647,.T.);
#60915=ORIENTED_EDGE('',*,*,#45739,.T.);
#60916=ORIENTED_EDGE('',*,*,#45746,.F.);
#60917=ORIENTED_EDGE('',*,*,#45737,.F.);
#60918=ORIENTED_EDGE('',*,*,#45736,.T.);
#60919=ORIENTED_EDGE('',*,*,#45722,.T.);
#60920=ORIENTED_EDGE('',*,*,#45734,.T.);
#60921=ORIENTED_EDGE('',*,*,#45745,.T.);
#60922=ORIENTED_EDGE('',*,*,#45742,.T.);
#60923=ORIENTED_EDGE('',*,*,#45653,.T.);
#60924=ORIENTED_EDGE('',*,*,#45740,.T.);
#60925=ORIENTED_EDGE('',*,*,#45627,.T.);
#60926=ORIENTED_EDGE('',*,*,#45652,.F.);
#60927=ORIENTED_EDGE('',*,*,#45728,.T.);
#60928=ORIENTED_EDGE('',*,*,#45732,.T.);
#60929=ORIENTED_EDGE('',*,*,#45686,.T.);
#60930=ORIENTED_EDGE('',*,*,#45735,.T.);
#60931=ORIENTED_EDGE('',*,*,#45746,.T.);
#60932=ORIENTED_EDGE('',*,*,#45738,.T.);
#60933=ORIENTED_EDGE('',*,*,#45726,.F.);
#60934=ORIENTED_EDGE('',*,*,#45741,.T.);
#60935=ORIENTED_EDGE('',*,*,#45744,.T.);
#60936=ORIENTED_EDGE('',*,*,#45731,.F.);
#60937=ORIENTED_EDGE('',*,*,#45747,.F.);
#60938=ORIENTED_EDGE('',*,*,#45748,.T.);
#60939=ORIENTED_EDGE('',*,*,#45749,.T.);
#60940=ORIENTED_EDGE('',*,*,#45750,.T.);
#60941=ORIENTED_EDGE('',*,*,#45748,.F.);
#60942=ORIENTED_EDGE('',*,*,#45751,.F.);
#60943=ORIENTED_EDGE('',*,*,#45752,.F.);
#60944=ORIENTED_EDGE('',*,*,#45753,.F.);
#60945=ORIENTED_EDGE('',*,*,#45754,.F.);
#60946=ORIENTED_EDGE('',*,*,#45755,.F.);
#60947=ORIENTED_EDGE('',*,*,#45756,.F.);
#60948=ORIENTED_EDGE('',*,*,#45753,.T.);
#60949=ORIENTED_EDGE('',*,*,#45757,.F.);
#60950=ORIENTED_EDGE('',*,*,#45758,.F.);
#60951=ORIENTED_EDGE('',*,*,#45759,.T.);
#60952=ORIENTED_EDGE('',*,*,#45760,.T.);
#60953=ORIENTED_EDGE('',*,*,#45759,.F.);
#60954=ORIENTED_EDGE('',*,*,#45761,.F.);
#60955=ORIENTED_EDGE('',*,*,#45762,.F.);
#60956=ORIENTED_EDGE('',*,*,#45763,.T.);
#60957=ORIENTED_EDGE('',*,*,#45764,.F.);
#60958=ORIENTED_EDGE('',*,*,#45765,.F.);
#60959=ORIENTED_EDGE('',*,*,#45766,.T.);
#60960=ORIENTED_EDGE('',*,*,#45767,.T.);
#60961=ORIENTED_EDGE('',*,*,#45768,.T.);
#60962=ORIENTED_EDGE('',*,*,#45761,.T.);
#60963=ORIENTED_EDGE('',*,*,#45769,.T.);
#60964=ORIENTED_EDGE('',*,*,#45749,.F.);
#60965=ORIENTED_EDGE('',*,*,#45750,.F.);
#60966=ORIENTED_EDGE('',*,*,#45769,.F.);
#60967=ORIENTED_EDGE('',*,*,#45765,.T.);
#60968=ORIENTED_EDGE('',*,*,#45770,.T.);
#60969=ORIENTED_EDGE('',*,*,#45771,.T.);
#60970=ORIENTED_EDGE('',*,*,#45772,.F.);
#60971=ORIENTED_EDGE('',*,*,#45747,.T.);
#60972=ORIENTED_EDGE('',*,*,#45773,.F.);
#60973=ORIENTED_EDGE('',*,*,#45774,.F.);
#60974=ORIENTED_EDGE('',*,*,#45775,.T.);
#60975=ORIENTED_EDGE('',*,*,#45772,.T.);
#60976=ORIENTED_EDGE('',*,*,#45775,.F.);
#60977=ORIENTED_EDGE('',*,*,#45773,.T.);
#60978=ORIENTED_EDGE('',*,*,#45774,.T.);
#60979=ORIENTED_EDGE('',*,*,#45776,.T.);
#60980=ORIENTED_EDGE('',*,*,#45777,.F.);
#60981=ORIENTED_EDGE('',*,*,#45778,.F.);
#60982=ORIENTED_EDGE('',*,*,#45776,.F.);
#60983=ORIENTED_EDGE('',*,*,#45779,.F.);
#60984=ORIENTED_EDGE('',*,*,#45780,.T.);
#60985=ORIENTED_EDGE('',*,*,#45777,.T.);
#60986=ORIENTED_EDGE('',*,*,#45778,.T.);
#60987=ORIENTED_EDGE('',*,*,#45780,.F.);
#60988=ORIENTED_EDGE('',*,*,#45781,.F.);
#60989=ORIENTED_EDGE('',*,*,#45782,.T.);
#60990=ORIENTED_EDGE('',*,*,#45783,.T.);
#60991=ORIENTED_EDGE('',*,*,#45782,.F.);
#60992=ORIENTED_EDGE('',*,*,#45779,.T.);
#60993=ORIENTED_EDGE('',*,*,#45783,.F.);
#60994=ORIENTED_EDGE('',*,*,#45781,.T.);
#60995=ORIENTED_EDGE('',*,*,#45784,.F.);
#60996=ORIENTED_EDGE('',*,*,#45751,.T.);
#60997=ORIENTED_EDGE('',*,*,#45785,.F.);
#60998=ORIENTED_EDGE('',*,*,#45766,.F.);
#60999=ORIENTED_EDGE('',*,*,#45786,.F.);
#61000=ORIENTED_EDGE('',*,*,#45787,.T.);
#61001=ORIENTED_EDGE('',*,*,#45788,.F.);
#61002=ORIENTED_EDGE('',*,*,#45771,.F.);
#61003=ORIENTED_EDGE('',*,*,#45789,.F.);
#61004=ORIENTED_EDGE('',*,*,#45790,.T.);
#61005=ORIENTED_EDGE('',*,*,#45791,.F.);
#61006=ORIENTED_EDGE('',*,*,#45770,.F.);
#61007=ORIENTED_EDGE('',*,*,#45792,.F.);
#61008=ORIENTED_EDGE('',*,*,#45793,.T.);
#61009=ORIENTED_EDGE('',*,*,#45794,.F.);
#61010=ORIENTED_EDGE('',*,*,#45768,.F.);
#61011=ORIENTED_EDGE('',*,*,#45795,.F.);
#61012=ORIENTED_EDGE('',*,*,#45796,.T.);
#61013=ORIENTED_EDGE('',*,*,#45797,.F.);
#61014=ORIENTED_EDGE('',*,*,#45767,.F.);
#61015=ORIENTED_EDGE('',*,*,#45760,.F.);
#61016=ORIENTED_EDGE('',*,*,#45755,.T.);
#61017=ORIENTED_EDGE('',*,*,#45798,.T.);
#61018=ORIENTED_EDGE('',*,*,#45799,.T.);
#61019=ORIENTED_EDGE('',*,*,#45800,.T.);
#61020=ORIENTED_EDGE('',*,*,#45801,.T.);
#61021=ORIENTED_EDGE('',*,*,#45802,.T.);
#61022=ORIENTED_EDGE('',*,*,#45758,.T.);
#61023=ORIENTED_EDGE('',*,*,#45803,.F.);
#61024=ORIENTED_EDGE('',*,*,#45804,.T.);
#61025=ORIENTED_EDGE('',*,*,#45805,.F.);
#61026=ORIENTED_EDGE('',*,*,#45802,.F.);
#61027=ORIENTED_EDGE('',*,*,#45806,.F.);
#61028=ORIENTED_EDGE('',*,*,#45807,.T.);
#61029=ORIENTED_EDGE('',*,*,#45808,.F.);
#61030=ORIENTED_EDGE('',*,*,#45801,.F.);
#61031=ORIENTED_EDGE('',*,*,#45809,.F.);
#61032=ORIENTED_EDGE('',*,*,#45810,.T.);
#61033=ORIENTED_EDGE('',*,*,#45811,.F.);
#61034=ORIENTED_EDGE('',*,*,#45800,.F.);
#61035=ORIENTED_EDGE('',*,*,#45812,.F.);
#61036=ORIENTED_EDGE('',*,*,#45813,.T.);
#61037=ORIENTED_EDGE('',*,*,#45814,.F.);
#61038=ORIENTED_EDGE('',*,*,#45799,.F.);
#61039=ORIENTED_EDGE('',*,*,#45815,.F.);
#61040=ORIENTED_EDGE('',*,*,#45816,.T.);
#61041=ORIENTED_EDGE('',*,*,#45817,.F.);
#61042=ORIENTED_EDGE('',*,*,#45798,.F.);
#61043=ORIENTED_EDGE('',*,*,#45788,.T.);
#61044=ORIENTED_EDGE('',*,*,#45818,.T.);
#61045=ORIENTED_EDGE('',*,*,#45815,.T.);
#61046=ORIENTED_EDGE('',*,*,#45757,.T.);
#61047=ORIENTED_EDGE('',*,*,#45752,.T.);
#61048=ORIENTED_EDGE('',*,*,#45784,.T.);
#61049=ORIENTED_EDGE('',*,*,#45817,.T.);
#61050=ORIENTED_EDGE('',*,*,#45819,.T.);
#61051=ORIENTED_EDGE('',*,*,#45786,.T.);
#61052=ORIENTED_EDGE('',*,*,#45791,.T.);
#61053=ORIENTED_EDGE('',*,*,#45820,.T.);
#61054=ORIENTED_EDGE('',*,*,#45812,.T.);
#61055=ORIENTED_EDGE('',*,*,#45814,.T.);
#61056=ORIENTED_EDGE('',*,*,#45821,.T.);
#61057=ORIENTED_EDGE('',*,*,#45789,.T.);
#61058=ORIENTED_EDGE('',*,*,#45764,.T.);
#61059=ORIENTED_EDGE('',*,*,#45822,.T.);
#61060=ORIENTED_EDGE('',*,*,#45809,.T.);
#61061=ORIENTED_EDGE('',*,*,#45794,.T.);
#61062=ORIENTED_EDGE('',*,*,#45823,.T.);
#61063=ORIENTED_EDGE('',*,*,#45806,.T.);
#61064=ORIENTED_EDGE('',*,*,#45811,.T.);
#61065=ORIENTED_EDGE('',*,*,#45824,.T.);
#61066=ORIENTED_EDGE('',*,*,#45762,.T.);
#61067=ORIENTED_EDGE('',*,*,#45797,.T.);
#61068=ORIENTED_EDGE('',*,*,#45825,.T.);
#61069=ORIENTED_EDGE('',*,*,#45803,.T.);
#61070=ORIENTED_EDGE('',*,*,#45808,.T.);
#61071=ORIENTED_EDGE('',*,*,#45826,.T.);
#61072=ORIENTED_EDGE('',*,*,#45792,.T.);
#61073=ORIENTED_EDGE('',*,*,#45785,.T.);
#61074=ORIENTED_EDGE('',*,*,#45754,.T.);
#61075=ORIENTED_EDGE('',*,*,#45756,.T.);
#61076=ORIENTED_EDGE('',*,*,#45805,.T.);
#61077=ORIENTED_EDGE('',*,*,#45827,.T.);
#61078=ORIENTED_EDGE('',*,*,#45795,.T.);
#61079=ORIENTED_EDGE('',*,*,#45787,.F.);
#61080=ORIENTED_EDGE('',*,*,#45819,.F.);
#61081=ORIENTED_EDGE('',*,*,#45816,.F.);
#61082=ORIENTED_EDGE('',*,*,#45818,.F.);
#61083=ORIENTED_EDGE('',*,*,#45796,.F.);
#61084=ORIENTED_EDGE('',*,*,#45827,.F.);
#61085=ORIENTED_EDGE('',*,*,#45804,.F.);
#61086=ORIENTED_EDGE('',*,*,#45825,.F.);
#61087=ORIENTED_EDGE('',*,*,#45793,.F.);
#61088=ORIENTED_EDGE('',*,*,#45826,.F.);
#61089=ORIENTED_EDGE('',*,*,#45807,.F.);
#61090=ORIENTED_EDGE('',*,*,#45823,.F.);
#61091=ORIENTED_EDGE('',*,*,#45790,.F.);
#61092=ORIENTED_EDGE('',*,*,#45821,.F.);
#61093=ORIENTED_EDGE('',*,*,#45813,.F.);
#61094=ORIENTED_EDGE('',*,*,#45820,.F.);
#61095=ORIENTED_EDGE('',*,*,#45763,.F.);
#61096=ORIENTED_EDGE('',*,*,#45824,.F.);
#61097=ORIENTED_EDGE('',*,*,#45810,.F.);
#61098=ORIENTED_EDGE('',*,*,#45822,.F.);
#61099=ORIENTED_EDGE('',*,*,#45828,.T.);
#61100=ORIENTED_EDGE('',*,*,#45829,.T.);
#61101=ORIENTED_EDGE('',*,*,#45830,.F.);
#61102=ORIENTED_EDGE('',*,*,#45829,.F.);
#61103=ORIENTED_EDGE('',*,*,#45831,.T.);
#61104=ORIENTED_EDGE('',*,*,#45832,.T.);
#61105=ORIENTED_EDGE('',*,*,#45833,.F.);
#61106=ORIENTED_EDGE('',*,*,#45832,.F.);
#61107=ORIENTED_EDGE('',*,*,#45831,.F.);
#61108=ORIENTED_EDGE('',*,*,#45830,.T.);
#61109=ORIENTED_EDGE('',*,*,#45833,.T.);
#61110=ORIENTED_EDGE('',*,*,#45828,.F.);
#61111=ORIENTED_EDGE('',*,*,#45834,.T.);
#61112=ORIENTED_EDGE('',*,*,#45835,.T.);
#61113=ORIENTED_EDGE('',*,*,#45836,.F.);
#61114=ORIENTED_EDGE('',*,*,#45835,.F.);
#61115=ORIENTED_EDGE('',*,*,#45837,.T.);
#61116=ORIENTED_EDGE('',*,*,#45838,.T.);
#61117=ORIENTED_EDGE('',*,*,#45839,.F.);
#61118=ORIENTED_EDGE('',*,*,#45838,.F.);
#61119=ORIENTED_EDGE('',*,*,#45837,.F.);
#61120=ORIENTED_EDGE('',*,*,#45836,.T.);
#61121=ORIENTED_EDGE('',*,*,#45839,.T.);
#61122=ORIENTED_EDGE('',*,*,#45834,.F.);
#61123=ORIENTED_EDGE('',*,*,#45840,.T.);
#61124=ORIENTED_EDGE('',*,*,#45841,.T.);
#61125=ORIENTED_EDGE('',*,*,#45842,.F.);
#61126=ORIENTED_EDGE('',*,*,#45841,.F.);
#61127=ORIENTED_EDGE('',*,*,#45843,.T.);
#61128=ORIENTED_EDGE('',*,*,#45844,.T.);
#61129=ORIENTED_EDGE('',*,*,#45845,.F.);
#61130=ORIENTED_EDGE('',*,*,#45844,.F.);
#61131=ORIENTED_EDGE('',*,*,#45843,.F.);
#61132=ORIENTED_EDGE('',*,*,#45842,.T.);
#61133=ORIENTED_EDGE('',*,*,#45845,.T.);
#61134=ORIENTED_EDGE('',*,*,#45840,.F.);
#61135=ORIENTED_EDGE('',*,*,#45846,.T.);
#61136=ORIENTED_EDGE('',*,*,#45847,.T.);
#61137=ORIENTED_EDGE('',*,*,#45848,.F.);
#61138=ORIENTED_EDGE('',*,*,#45847,.F.);
#61139=ORIENTED_EDGE('',*,*,#45849,.T.);
#61140=ORIENTED_EDGE('',*,*,#45850,.T.);
#61141=ORIENTED_EDGE('',*,*,#45851,.F.);
#61142=ORIENTED_EDGE('',*,*,#45850,.F.);
#61143=ORIENTED_EDGE('',*,*,#45849,.F.);
#61144=ORIENTED_EDGE('',*,*,#45848,.T.);
#61145=ORIENTED_EDGE('',*,*,#45851,.T.);
#61146=ORIENTED_EDGE('',*,*,#45846,.F.);
#61147=ORIENTED_EDGE('',*,*,#45852,.F.);
#61148=ORIENTED_EDGE('',*,*,#45853,.F.);
#61149=ORIENTED_EDGE('',*,*,#45854,.T.);
#61150=ORIENTED_EDGE('',*,*,#45855,.F.);
#61151=ORIENTED_EDGE('',*,*,#45854,.F.);
#61152=ORIENTED_EDGE('',*,*,#45856,.F.);
#61153=ORIENTED_EDGE('',*,*,#45857,.T.);
#61154=ORIENTED_EDGE('',*,*,#45858,.F.);
#61155=ORIENTED_EDGE('',*,*,#45859,.F.);
#61156=ORIENTED_EDGE('',*,*,#45857,.F.);
#61157=ORIENTED_EDGE('',*,*,#45860,.T.);
#61158=ORIENTED_EDGE('',*,*,#45861,.T.);
#61159=ORIENTED_EDGE('',*,*,#45858,.T.);
#61160=ORIENTED_EDGE('',*,*,#45859,.T.);
#61161=ORIENTED_EDGE('',*,*,#45861,.F.);
#61162=ORIENTED_EDGE('',*,*,#45852,.T.);
#61163=ORIENTED_EDGE('',*,*,#45853,.T.);
#61164=ORIENTED_EDGE('',*,*,#45862,.T.);
#61165=ORIENTED_EDGE('',*,*,#45863,.T.);
#61166=ORIENTED_EDGE('',*,*,#45862,.F.);
#61167=ORIENTED_EDGE('',*,*,#45860,.F.);
#61168=ORIENTED_EDGE('',*,*,#45863,.F.);
#61169=ORIENTED_EDGE('',*,*,#45856,.T.);
#61170=ORIENTED_EDGE('',*,*,#45855,.T.);
#61171=ORIENTED_EDGE('',*,*,#45864,.F.);
#61172=ORIENTED_EDGE('',*,*,#45865,.T.);
#61173=ORIENTED_EDGE('',*,*,#45866,.F.);
#61174=ORIENTED_EDGE('',*,*,#45867,.F.);
#61175=ORIENTED_EDGE('',*,*,#45865,.F.);
#61176=ORIENTED_EDGE('',*,*,#45868,.F.);
#61177=ORIENTED_EDGE('',*,*,#45869,.F.);
#61178=ORIENTED_EDGE('',*,*,#45870,.T.);
#61179=ORIENTED_EDGE('',*,*,#45871,.F.);
#61180=ORIENTED_EDGE('',*,*,#45870,.F.);
#61181=ORIENTED_EDGE('',*,*,#45872,.T.);
#61182=ORIENTED_EDGE('',*,*,#45873,.T.);
#61183=ORIENTED_EDGE('',*,*,#45866,.T.);
#61184=ORIENTED_EDGE('',*,*,#45867,.T.);
#61185=ORIENTED_EDGE('',*,*,#45873,.F.);
#61186=ORIENTED_EDGE('',*,*,#45868,.T.);
#61187=ORIENTED_EDGE('',*,*,#45869,.T.);
#61188=ORIENTED_EDGE('',*,*,#45874,.T.);
#61189=ORIENTED_EDGE('',*,*,#45875,.F.);
#61190=ORIENTED_EDGE('',*,*,#45874,.F.);
#61191=ORIENTED_EDGE('',*,*,#45872,.F.);
#61192=ORIENTED_EDGE('',*,*,#45875,.T.);
#61193=ORIENTED_EDGE('',*,*,#45864,.T.);
#61194=ORIENTED_EDGE('',*,*,#45871,.T.);
#61195=ORIENTED_EDGE('',*,*,#45876,.T.);
#61196=ORIENTED_EDGE('',*,*,#45877,.T.);
#61197=ORIENTED_EDGE('',*,*,#45878,.F.);
#61198=ORIENTED_EDGE('',*,*,#45877,.F.);
#61199=ORIENTED_EDGE('',*,*,#45879,.T.);
#61200=ORIENTED_EDGE('',*,*,#45880,.T.);
#61201=ORIENTED_EDGE('',*,*,#45881,.F.);
#61202=ORIENTED_EDGE('',*,*,#45880,.F.);
#61203=ORIENTED_EDGE('',*,*,#45879,.F.);
#61204=ORIENTED_EDGE('',*,*,#45878,.T.);
#61205=ORIENTED_EDGE('',*,*,#45881,.T.);
#61206=ORIENTED_EDGE('',*,*,#45876,.F.);
#61207=ORIENTED_EDGE('',*,*,#45882,.F.);
#61208=ORIENTED_EDGE('',*,*,#45883,.F.);
#61209=ORIENTED_EDGE('',*,*,#45884,.F.);
#61210=ORIENTED_EDGE('',*,*,#45885,.T.);
#61211=ORIENTED_EDGE('',*,*,#45886,.F.);
#61212=ORIENTED_EDGE('',*,*,#45887,.F.);
#61213=ORIENTED_EDGE('',*,*,#45888,.F.);
#61214=ORIENTED_EDGE('',*,*,#45889,.T.);
#61215=ORIENTED_EDGE('',*,*,#45890,.F.);
#61216=ORIENTED_EDGE('',*,*,#45891,.F.);
#61217=ORIENTED_EDGE('',*,*,#45892,.F.);
#61218=ORIENTED_EDGE('',*,*,#45893,.T.);
#61219=ORIENTED_EDGE('',*,*,#45894,.F.);
#61220=ORIENTED_EDGE('',*,*,#45895,.F.);
#61221=ORIENTED_EDGE('',*,*,#45896,.F.);
#61222=ORIENTED_EDGE('',*,*,#45897,.T.);
#61223=ORIENTED_EDGE('',*,*,#45898,.F.);
#61224=ORIENTED_EDGE('',*,*,#45899,.F.);
#61225=ORIENTED_EDGE('',*,*,#45900,.T.);
#61226=ORIENTED_EDGE('',*,*,#45901,.F.);
#61227=ORIENTED_EDGE('',*,*,#45902,.F.);
#61228=ORIENTED_EDGE('',*,*,#45900,.F.);
#61229=ORIENTED_EDGE('',*,*,#45903,.F.);
#61230=ORIENTED_EDGE('',*,*,#45904,.T.);
#61231=ORIENTED_EDGE('',*,*,#45905,.F.);
#61232=ORIENTED_EDGE('',*,*,#45904,.F.);
#61233=ORIENTED_EDGE('',*,*,#45906,.F.);
#61234=ORIENTED_EDGE('',*,*,#45907,.T.);
#61235=ORIENTED_EDGE('',*,*,#45908,.F.);
#61236=ORIENTED_EDGE('',*,*,#45909,.F.);
#61237=ORIENTED_EDGE('',*,*,#45907,.F.);
#61238=ORIENTED_EDGE('',*,*,#45910,.F.);
#61239=ORIENTED_EDGE('',*,*,#45911,.T.);
#61240=ORIENTED_EDGE('',*,*,#45912,.F.);
#61241=ORIENTED_EDGE('',*,*,#45911,.F.);
#61242=ORIENTED_EDGE('',*,*,#45913,.F.);
#61243=ORIENTED_EDGE('',*,*,#45914,.T.);
#61244=ORIENTED_EDGE('',*,*,#45915,.T.);
#61245=ORIENTED_EDGE('',*,*,#45914,.F.);
#61246=ORIENTED_EDGE('',*,*,#45915,.F.);
#61247=ORIENTED_EDGE('',*,*,#45916,.T.);
#61248=ORIENTED_EDGE('',*,*,#45910,.T.);
#61249=ORIENTED_EDGE('',*,*,#45916,.F.);
#61250=ORIENTED_EDGE('',*,*,#45917,.T.);
#61251=ORIENTED_EDGE('',*,*,#45918,.T.);
#61252=ORIENTED_EDGE('',*,*,#45919,.T.);
#61253=ORIENTED_EDGE('',*,*,#45920,.T.);
#61254=ORIENTED_EDGE('',*,*,#45921,.T.);
#61255=ORIENTED_EDGE('',*,*,#45922,.T.);
#61256=ORIENTED_EDGE('',*,*,#45923,.T.);
#61257=ORIENTED_EDGE('',*,*,#45924,.T.);
#61258=ORIENTED_EDGE('',*,*,#45925,.T.);
#61259=ORIENTED_EDGE('',*,*,#45926,.T.);
#61260=ORIENTED_EDGE('',*,*,#45927,.T.);
#61261=ORIENTED_EDGE('',*,*,#45928,.T.);
#61262=ORIENTED_EDGE('',*,*,#45929,.T.);
#61263=ORIENTED_EDGE('',*,*,#45930,.T.);
#61264=ORIENTED_EDGE('',*,*,#45931,.T.);
#61265=ORIENTED_EDGE('',*,*,#45932,.T.);
#61266=ORIENTED_EDGE('',*,*,#45933,.T.);
#61267=ORIENTED_EDGE('',*,*,#45934,.T.);
#61268=ORIENTED_EDGE('',*,*,#45935,.T.);
#61269=ORIENTED_EDGE('',*,*,#45936,.T.);
#61270=ORIENTED_EDGE('',*,*,#45937,.T.);
#61271=ORIENTED_EDGE('',*,*,#45938,.T.);
#61272=ORIENTED_EDGE('',*,*,#45939,.T.);
#61273=ORIENTED_EDGE('',*,*,#45940,.T.);
#61274=ORIENTED_EDGE('',*,*,#45941,.T.);
#61275=ORIENTED_EDGE('',*,*,#45942,.T.);
#61276=ORIENTED_EDGE('',*,*,#45943,.T.);
#61277=ORIENTED_EDGE('',*,*,#45944,.T.);
#61278=ORIENTED_EDGE('',*,*,#45945,.T.);
#61279=ORIENTED_EDGE('',*,*,#45946,.T.);
#61280=ORIENTED_EDGE('',*,*,#45947,.T.);
#61281=ORIENTED_EDGE('',*,*,#45948,.T.);
#61282=ORIENTED_EDGE('',*,*,#45949,.T.);
#61283=ORIENTED_EDGE('',*,*,#45950,.T.);
#61284=ORIENTED_EDGE('',*,*,#45951,.T.);
#61285=ORIENTED_EDGE('',*,*,#45952,.T.);
#61286=ORIENTED_EDGE('',*,*,#45953,.T.);
#61287=ORIENTED_EDGE('',*,*,#45954,.T.);
#61288=ORIENTED_EDGE('',*,*,#45955,.T.);
#61289=ORIENTED_EDGE('',*,*,#45956,.T.);
#61290=ORIENTED_EDGE('',*,*,#45957,.T.);
#61291=ORIENTED_EDGE('',*,*,#45958,.T.);
#61292=ORIENTED_EDGE('',*,*,#45959,.T.);
#61293=ORIENTED_EDGE('',*,*,#45960,.T.);
#61294=ORIENTED_EDGE('',*,*,#45961,.T.);
#61295=ORIENTED_EDGE('',*,*,#45962,.T.);
#61296=ORIENTED_EDGE('',*,*,#45963,.T.);
#61297=ORIENTED_EDGE('',*,*,#45964,.T.);
#61298=ORIENTED_EDGE('',*,*,#45965,.T.);
#61299=ORIENTED_EDGE('',*,*,#45966,.T.);
#61300=ORIENTED_EDGE('',*,*,#45967,.T.);
#61301=ORIENTED_EDGE('',*,*,#45968,.T.);
#61302=ORIENTED_EDGE('',*,*,#45969,.T.);
#61303=ORIENTED_EDGE('',*,*,#45970,.T.);
#61304=ORIENTED_EDGE('',*,*,#45971,.T.);
#61305=ORIENTED_EDGE('',*,*,#45972,.T.);
#61306=ORIENTED_EDGE('',*,*,#45973,.T.);
#61307=ORIENTED_EDGE('',*,*,#45974,.T.);
#61308=ORIENTED_EDGE('',*,*,#45975,.T.);
#61309=ORIENTED_EDGE('',*,*,#45976,.T.);
#61310=ORIENTED_EDGE('',*,*,#45977,.T.);
#61311=ORIENTED_EDGE('',*,*,#45978,.T.);
#61312=ORIENTED_EDGE('',*,*,#45979,.T.);
#61313=ORIENTED_EDGE('',*,*,#45980,.T.);
#61314=ORIENTED_EDGE('',*,*,#45981,.T.);
#61315=ORIENTED_EDGE('',*,*,#45982,.T.);
#61316=ORIENTED_EDGE('',*,*,#45983,.T.);
#61317=ORIENTED_EDGE('',*,*,#45984,.T.);
#61318=ORIENTED_EDGE('',*,*,#45985,.T.);
#61319=ORIENTED_EDGE('',*,*,#45986,.T.);
#61320=ORIENTED_EDGE('',*,*,#45987,.T.);
#61321=ORIENTED_EDGE('',*,*,#45988,.T.);
#61322=ORIENTED_EDGE('',*,*,#45989,.T.);
#61323=ORIENTED_EDGE('',*,*,#45990,.T.);
#61324=ORIENTED_EDGE('',*,*,#45991,.T.);
#61325=ORIENTED_EDGE('',*,*,#45992,.T.);
#61326=ORIENTED_EDGE('',*,*,#45993,.T.);
#61327=ORIENTED_EDGE('',*,*,#45994,.T.);
#61328=ORIENTED_EDGE('',*,*,#45995,.T.);
#61329=ORIENTED_EDGE('',*,*,#45996,.T.);
#61330=ORIENTED_EDGE('',*,*,#45997,.T.);
#61331=ORIENTED_EDGE('',*,*,#45998,.T.);
#61332=ORIENTED_EDGE('',*,*,#45999,.T.);
#61333=ORIENTED_EDGE('',*,*,#46000,.T.);
#61334=ORIENTED_EDGE('',*,*,#46001,.T.);
#61335=ORIENTED_EDGE('',*,*,#46002,.T.);
#61336=ORIENTED_EDGE('',*,*,#46003,.T.);
#61337=ORIENTED_EDGE('',*,*,#46004,.T.);
#61338=ORIENTED_EDGE('',*,*,#46005,.T.);
#61339=ORIENTED_EDGE('',*,*,#46006,.T.);
#61340=ORIENTED_EDGE('',*,*,#46007,.T.);
#61341=ORIENTED_EDGE('',*,*,#46008,.T.);
#61342=ORIENTED_EDGE('',*,*,#46009,.T.);
#61343=ORIENTED_EDGE('',*,*,#46010,.T.);
#61344=ORIENTED_EDGE('',*,*,#46011,.T.);
#61345=ORIENTED_EDGE('',*,*,#46012,.T.);
#61346=ORIENTED_EDGE('',*,*,#46013,.T.);
#61347=ORIENTED_EDGE('',*,*,#46014,.T.);
#61348=ORIENTED_EDGE('',*,*,#46015,.T.);
#61349=ORIENTED_EDGE('',*,*,#46016,.T.);
#61350=ORIENTED_EDGE('',*,*,#46017,.T.);
#61351=ORIENTED_EDGE('',*,*,#46018,.T.);
#61352=ORIENTED_EDGE('',*,*,#46019,.T.);
#61353=ORIENTED_EDGE('',*,*,#46020,.T.);
#61354=ORIENTED_EDGE('',*,*,#46021,.T.);
#61355=ORIENTED_EDGE('',*,*,#46022,.T.);
#61356=ORIENTED_EDGE('',*,*,#46023,.T.);
#61357=ORIENTED_EDGE('',*,*,#46024,.T.);
#61358=ORIENTED_EDGE('',*,*,#46025,.T.);
#61359=ORIENTED_EDGE('',*,*,#46026,.T.);
#61360=ORIENTED_EDGE('',*,*,#46027,.T.);
#61361=ORIENTED_EDGE('',*,*,#46028,.T.);
#61362=ORIENTED_EDGE('',*,*,#46029,.T.);
#61363=ORIENTED_EDGE('',*,*,#46030,.T.);
#61364=ORIENTED_EDGE('',*,*,#46031,.T.);
#61365=ORIENTED_EDGE('',*,*,#46032,.T.);
#61366=ORIENTED_EDGE('',*,*,#46033,.T.);
#61367=ORIENTED_EDGE('',*,*,#46034,.T.);
#61368=ORIENTED_EDGE('',*,*,#46035,.T.);
#61369=ORIENTED_EDGE('',*,*,#46036,.T.);
#61370=ORIENTED_EDGE('',*,*,#46037,.T.);
#61371=ORIENTED_EDGE('',*,*,#46038,.T.);
#61372=ORIENTED_EDGE('',*,*,#46039,.T.);
#61373=ORIENTED_EDGE('',*,*,#46040,.T.);
#61374=ORIENTED_EDGE('',*,*,#46041,.T.);
#61375=ORIENTED_EDGE('',*,*,#46042,.T.);
#61376=ORIENTED_EDGE('',*,*,#46043,.T.);
#61377=ORIENTED_EDGE('',*,*,#46044,.T.);
#61378=ORIENTED_EDGE('',*,*,#46045,.T.);
#61379=ORIENTED_EDGE('',*,*,#46046,.T.);
#61380=ORIENTED_EDGE('',*,*,#46047,.T.);
#61381=ORIENTED_EDGE('',*,*,#46048,.T.);
#61382=ORIENTED_EDGE('',*,*,#46049,.T.);
#61383=ORIENTED_EDGE('',*,*,#46050,.T.);
#61384=ORIENTED_EDGE('',*,*,#46051,.T.);
#61385=ORIENTED_EDGE('',*,*,#46052,.T.);
#61386=ORIENTED_EDGE('',*,*,#46053,.T.);
#61387=ORIENTED_EDGE('',*,*,#46054,.T.);
#61388=ORIENTED_EDGE('',*,*,#46055,.T.);
#61389=ORIENTED_EDGE('',*,*,#46056,.T.);
#61390=ORIENTED_EDGE('',*,*,#46057,.T.);
#61391=ORIENTED_EDGE('',*,*,#46058,.T.);
#61392=ORIENTED_EDGE('',*,*,#46059,.T.);
#61393=ORIENTED_EDGE('',*,*,#46060,.T.);
#61394=ORIENTED_EDGE('',*,*,#46061,.T.);
#61395=ORIENTED_EDGE('',*,*,#46062,.T.);
#61396=ORIENTED_EDGE('',*,*,#46063,.T.);
#61397=ORIENTED_EDGE('',*,*,#46064,.T.);
#61398=ORIENTED_EDGE('',*,*,#46065,.T.);
#61399=ORIENTED_EDGE('',*,*,#46066,.T.);
#61400=ORIENTED_EDGE('',*,*,#46067,.T.);
#61401=ORIENTED_EDGE('',*,*,#46068,.T.);
#61402=ORIENTED_EDGE('',*,*,#46069,.T.);
#61403=ORIENTED_EDGE('',*,*,#46070,.T.);
#61404=ORIENTED_EDGE('',*,*,#46071,.T.);
#61405=ORIENTED_EDGE('',*,*,#46072,.T.);
#61406=ORIENTED_EDGE('',*,*,#46073,.T.);
#61407=ORIENTED_EDGE('',*,*,#46074,.T.);
#61408=ORIENTED_EDGE('',*,*,#46075,.T.);
#61409=ORIENTED_EDGE('',*,*,#46076,.T.);
#61410=ORIENTED_EDGE('',*,*,#46077,.T.);
#61411=ORIENTED_EDGE('',*,*,#46078,.T.);
#61412=ORIENTED_EDGE('',*,*,#46079,.T.);
#61413=ORIENTED_EDGE('',*,*,#46080,.T.);
#61414=ORIENTED_EDGE('',*,*,#46081,.T.);
#61415=ORIENTED_EDGE('',*,*,#46082,.T.);
#61416=ORIENTED_EDGE('',*,*,#46083,.T.);
#61417=ORIENTED_EDGE('',*,*,#46084,.T.);
#61418=ORIENTED_EDGE('',*,*,#46085,.T.);
#61419=ORIENTED_EDGE('',*,*,#46086,.T.);
#61420=ORIENTED_EDGE('',*,*,#46087,.T.);
#61421=ORIENTED_EDGE('',*,*,#46088,.T.);
#61422=ORIENTED_EDGE('',*,*,#46089,.T.);
#61423=ORIENTED_EDGE('',*,*,#46090,.T.);
#61424=ORIENTED_EDGE('',*,*,#46091,.T.);
#61425=ORIENTED_EDGE('',*,*,#46092,.T.);
#61426=ORIENTED_EDGE('',*,*,#46093,.T.);
#61427=ORIENTED_EDGE('',*,*,#46094,.T.);
#61428=ORIENTED_EDGE('',*,*,#46095,.T.);
#61429=ORIENTED_EDGE('',*,*,#46096,.T.);
#61430=ORIENTED_EDGE('',*,*,#45894,.T.);
#61431=ORIENTED_EDGE('',*,*,#46097,.T.);
#61432=ORIENTED_EDGE('',*,*,#45908,.T.);
#61433=ORIENTED_EDGE('',*,*,#45909,.T.);
#61434=ORIENTED_EDGE('',*,*,#46097,.F.);
#61435=ORIENTED_EDGE('',*,*,#45898,.T.);
#61436=ORIENTED_EDGE('',*,*,#46098,.T.);
#61437=ORIENTED_EDGE('',*,*,#46099,.T.);
#61438=ORIENTED_EDGE('',*,*,#46100,.T.);
#61439=ORIENTED_EDGE('',*,*,#46101,.T.);
#61440=ORIENTED_EDGE('',*,*,#46102,.T.);
#61441=ORIENTED_EDGE('',*,*,#46103,.T.);
#61442=ORIENTED_EDGE('',*,*,#46104,.T.);
#61443=ORIENTED_EDGE('',*,*,#46105,.T.);
#61444=ORIENTED_EDGE('',*,*,#46106,.T.);
#61445=ORIENTED_EDGE('',*,*,#46107,.T.);
#61446=ORIENTED_EDGE('',*,*,#46108,.T.);
#61447=ORIENTED_EDGE('',*,*,#46109,.T.);
#61448=ORIENTED_EDGE('',*,*,#46110,.T.);
#61449=ORIENTED_EDGE('',*,*,#46111,.T.);
#61450=ORIENTED_EDGE('',*,*,#46112,.T.);
#61451=ORIENTED_EDGE('',*,*,#46113,.T.);
#61452=ORIENTED_EDGE('',*,*,#46114,.T.);
#61453=ORIENTED_EDGE('',*,*,#46115,.T.);
#61454=ORIENTED_EDGE('',*,*,#46116,.T.);
#61455=ORIENTED_EDGE('',*,*,#46117,.T.);
#61456=ORIENTED_EDGE('',*,*,#46118,.T.);
#61457=ORIENTED_EDGE('',*,*,#46119,.T.);
#61458=ORIENTED_EDGE('',*,*,#46120,.T.);
#61459=ORIENTED_EDGE('',*,*,#46121,.T.);
#61460=ORIENTED_EDGE('',*,*,#46122,.T.);
#61461=ORIENTED_EDGE('',*,*,#46123,.T.);
#61462=ORIENTED_EDGE('',*,*,#46124,.T.);
#61463=ORIENTED_EDGE('',*,*,#46125,.T.);
#61464=ORIENTED_EDGE('',*,*,#46126,.T.);
#61465=ORIENTED_EDGE('',*,*,#46127,.T.);
#61466=ORIENTED_EDGE('',*,*,#46128,.T.);
#61467=ORIENTED_EDGE('',*,*,#46129,.T.);
#61468=ORIENTED_EDGE('',*,*,#46130,.T.);
#61469=ORIENTED_EDGE('',*,*,#46131,.T.);
#61470=ORIENTED_EDGE('',*,*,#46132,.T.);
#61471=ORIENTED_EDGE('',*,*,#46133,.T.);
#61472=ORIENTED_EDGE('',*,*,#46134,.T.);
#61473=ORIENTED_EDGE('',*,*,#46135,.T.);
#61474=ORIENTED_EDGE('',*,*,#46136,.T.);
#61475=ORIENTED_EDGE('',*,*,#46137,.T.);
#61476=ORIENTED_EDGE('',*,*,#46138,.T.);
#61477=ORIENTED_EDGE('',*,*,#46139,.T.);
#61478=ORIENTED_EDGE('',*,*,#46140,.T.);
#61479=ORIENTED_EDGE('',*,*,#46141,.T.);
#61480=ORIENTED_EDGE('',*,*,#46142,.T.);
#61481=ORIENTED_EDGE('',*,*,#46143,.T.);
#61482=ORIENTED_EDGE('',*,*,#46144,.T.);
#61483=ORIENTED_EDGE('',*,*,#46145,.T.);
#61484=ORIENTED_EDGE('',*,*,#46146,.T.);
#61485=ORIENTED_EDGE('',*,*,#46147,.T.);
#61486=ORIENTED_EDGE('',*,*,#46148,.T.);
#61487=ORIENTED_EDGE('',*,*,#46149,.T.);
#61488=ORIENTED_EDGE('',*,*,#46150,.T.);
#61489=ORIENTED_EDGE('',*,*,#46151,.T.);
#61490=ORIENTED_EDGE('',*,*,#46152,.T.);
#61491=ORIENTED_EDGE('',*,*,#46153,.T.);
#61492=ORIENTED_EDGE('',*,*,#46154,.T.);
#61493=ORIENTED_EDGE('',*,*,#46155,.T.);
#61494=ORIENTED_EDGE('',*,*,#46156,.T.);
#61495=ORIENTED_EDGE('',*,*,#46157,.T.);
#61496=ORIENTED_EDGE('',*,*,#46158,.T.);
#61497=ORIENTED_EDGE('',*,*,#46159,.T.);
#61498=ORIENTED_EDGE('',*,*,#46160,.T.);
#61499=ORIENTED_EDGE('',*,*,#46161,.T.);
#61500=ORIENTED_EDGE('',*,*,#46162,.T.);
#61501=ORIENTED_EDGE('',*,*,#46163,.T.);
#61502=ORIENTED_EDGE('',*,*,#46164,.T.);
#61503=ORIENTED_EDGE('',*,*,#46165,.T.);
#61504=ORIENTED_EDGE('',*,*,#46166,.T.);
#61505=ORIENTED_EDGE('',*,*,#46167,.T.);
#61506=ORIENTED_EDGE('',*,*,#46168,.T.);
#61507=ORIENTED_EDGE('',*,*,#46169,.T.);
#61508=ORIENTED_EDGE('',*,*,#46170,.T.);
#61509=ORIENTED_EDGE('',*,*,#46171,.T.);
#61510=ORIENTED_EDGE('',*,*,#46172,.T.);
#61511=ORIENTED_EDGE('',*,*,#46173,.T.);
#61512=ORIENTED_EDGE('',*,*,#46174,.T.);
#61513=ORIENTED_EDGE('',*,*,#46175,.T.);
#61514=ORIENTED_EDGE('',*,*,#46176,.T.);
#61515=ORIENTED_EDGE('',*,*,#46177,.T.);
#61516=ORIENTED_EDGE('',*,*,#46178,.T.);
#61517=ORIENTED_EDGE('',*,*,#46179,.T.);
#61518=ORIENTED_EDGE('',*,*,#46180,.T.);
#61519=ORIENTED_EDGE('',*,*,#46181,.T.);
#61520=ORIENTED_EDGE('',*,*,#46182,.T.);
#61521=ORIENTED_EDGE('',*,*,#46183,.T.);
#61522=ORIENTED_EDGE('',*,*,#46184,.T.);
#61523=ORIENTED_EDGE('',*,*,#46185,.T.);
#61524=ORIENTED_EDGE('',*,*,#46186,.T.);
#61525=ORIENTED_EDGE('',*,*,#45886,.T.);
#61526=ORIENTED_EDGE('',*,*,#46187,.T.);
#61527=ORIENTED_EDGE('',*,*,#46188,.T.);
#61528=ORIENTED_EDGE('',*,*,#46189,.T.);
#61529=ORIENTED_EDGE('',*,*,#46190,.T.);
#61530=ORIENTED_EDGE('',*,*,#46191,.T.);
#61531=ORIENTED_EDGE('',*,*,#46192,.T.);
#61532=ORIENTED_EDGE('',*,*,#46193,.T.);
#61533=ORIENTED_EDGE('',*,*,#46194,.T.);
#61534=ORIENTED_EDGE('',*,*,#46195,.T.);
#61535=ORIENTED_EDGE('',*,*,#46196,.T.);
#61536=ORIENTED_EDGE('',*,*,#46197,.T.);
#61537=ORIENTED_EDGE('',*,*,#46198,.T.);
#61538=ORIENTED_EDGE('',*,*,#46199,.T.);
#61539=ORIENTED_EDGE('',*,*,#46200,.T.);
#61540=ORIENTED_EDGE('',*,*,#46201,.T.);
#61541=ORIENTED_EDGE('',*,*,#46202,.T.);
#61542=ORIENTED_EDGE('',*,*,#46203,.T.);
#61543=ORIENTED_EDGE('',*,*,#46204,.T.);
#61544=ORIENTED_EDGE('',*,*,#46205,.T.);
#61545=ORIENTED_EDGE('',*,*,#46206,.T.);
#61546=ORIENTED_EDGE('',*,*,#46207,.T.);
#61547=ORIENTED_EDGE('',*,*,#46208,.T.);
#61548=ORIENTED_EDGE('',*,*,#46209,.T.);
#61549=ORIENTED_EDGE('',*,*,#46210,.T.);
#61550=ORIENTED_EDGE('',*,*,#46211,.T.);
#61551=ORIENTED_EDGE('',*,*,#46212,.T.);
#61552=ORIENTED_EDGE('',*,*,#46213,.T.);
#61553=ORIENTED_EDGE('',*,*,#46214,.T.);
#61554=ORIENTED_EDGE('',*,*,#46215,.T.);
#61555=ORIENTED_EDGE('',*,*,#46216,.T.);
#61556=ORIENTED_EDGE('',*,*,#46217,.T.);
#61557=ORIENTED_EDGE('',*,*,#46218,.T.);
#61558=ORIENTED_EDGE('',*,*,#46219,.T.);
#61559=ORIENTED_EDGE('',*,*,#46220,.T.);
#61560=ORIENTED_EDGE('',*,*,#46221,.T.);
#61561=ORIENTED_EDGE('',*,*,#46222,.T.);
#61562=ORIENTED_EDGE('',*,*,#46223,.T.);
#61563=ORIENTED_EDGE('',*,*,#46224,.T.);
#61564=ORIENTED_EDGE('',*,*,#46225,.T.);
#61565=ORIENTED_EDGE('',*,*,#46226,.T.);
#61566=ORIENTED_EDGE('',*,*,#46227,.T.);
#61567=ORIENTED_EDGE('',*,*,#46228,.T.);
#61568=ORIENTED_EDGE('',*,*,#46229,.T.);
#61569=ORIENTED_EDGE('',*,*,#46230,.T.);
#61570=ORIENTED_EDGE('',*,*,#46231,.T.);
#61571=ORIENTED_EDGE('',*,*,#46232,.T.);
#61572=ORIENTED_EDGE('',*,*,#46233,.T.);
#61573=ORIENTED_EDGE('',*,*,#46234,.T.);
#61574=ORIENTED_EDGE('',*,*,#46235,.T.);
#61575=ORIENTED_EDGE('',*,*,#46236,.T.);
#61576=ORIENTED_EDGE('',*,*,#46237,.T.);
#61577=ORIENTED_EDGE('',*,*,#46238,.T.);
#61578=ORIENTED_EDGE('',*,*,#46239,.T.);
#61579=ORIENTED_EDGE('',*,*,#46240,.T.);
#61580=ORIENTED_EDGE('',*,*,#46241,.T.);
#61581=ORIENTED_EDGE('',*,*,#46242,.T.);
#61582=ORIENTED_EDGE('',*,*,#46243,.T.);
#61583=ORIENTED_EDGE('',*,*,#46244,.T.);
#61584=ORIENTED_EDGE('',*,*,#46245,.T.);
#61585=ORIENTED_EDGE('',*,*,#46246,.T.);
#61586=ORIENTED_EDGE('',*,*,#46247,.T.);
#61587=ORIENTED_EDGE('',*,*,#46248,.T.);
#61588=ORIENTED_EDGE('',*,*,#46249,.T.);
#61589=ORIENTED_EDGE('',*,*,#46250,.T.);
#61590=ORIENTED_EDGE('',*,*,#46251,.T.);
#61591=ORIENTED_EDGE('',*,*,#46252,.T.);
#61592=ORIENTED_EDGE('',*,*,#46253,.T.);
#61593=ORIENTED_EDGE('',*,*,#46254,.T.);
#61594=ORIENTED_EDGE('',*,*,#46255,.T.);
#61595=ORIENTED_EDGE('',*,*,#46256,.T.);
#61596=ORIENTED_EDGE('',*,*,#46257,.T.);
#61597=ORIENTED_EDGE('',*,*,#46258,.T.);
#61598=ORIENTED_EDGE('',*,*,#46259,.T.);
#61599=ORIENTED_EDGE('',*,*,#46260,.T.);
#61600=ORIENTED_EDGE('',*,*,#46261,.T.);
#61601=ORIENTED_EDGE('',*,*,#46262,.T.);
#61602=ORIENTED_EDGE('',*,*,#46263,.T.);
#61603=ORIENTED_EDGE('',*,*,#46264,.T.);
#61604=ORIENTED_EDGE('',*,*,#46265,.T.);
#61605=ORIENTED_EDGE('',*,*,#46266,.T.);
#61606=ORIENTED_EDGE('',*,*,#46267,.T.);
#61607=ORIENTED_EDGE('',*,*,#46268,.T.);
#61608=ORIENTED_EDGE('',*,*,#46269,.T.);
#61609=ORIENTED_EDGE('',*,*,#46270,.T.);
#61610=ORIENTED_EDGE('',*,*,#46271,.T.);
#61611=ORIENTED_EDGE('',*,*,#46272,.T.);
#61612=ORIENTED_EDGE('',*,*,#46273,.T.);
#61613=ORIENTED_EDGE('',*,*,#46274,.T.);
#61614=ORIENTED_EDGE('',*,*,#46275,.T.);
#61615=ORIENTED_EDGE('',*,*,#45892,.T.);
#61616=ORIENTED_EDGE('',*,*,#46276,.T.);
#61617=ORIENTED_EDGE('',*,*,#46277,.T.);
#61618=ORIENTED_EDGE('',*,*,#46278,.T.);
#61619=ORIENTED_EDGE('',*,*,#46279,.T.);
#61620=ORIENTED_EDGE('',*,*,#46280,.T.);
#61621=ORIENTED_EDGE('',*,*,#46281,.T.);
#61622=ORIENTED_EDGE('',*,*,#46282,.T.);
#61623=ORIENTED_EDGE('',*,*,#46283,.T.);
#61624=ORIENTED_EDGE('',*,*,#46284,.T.);
#61625=ORIENTED_EDGE('',*,*,#46285,.T.);
#61626=ORIENTED_EDGE('',*,*,#46286,.T.);
#61627=ORIENTED_EDGE('',*,*,#46287,.T.);
#61628=ORIENTED_EDGE('',*,*,#46288,.T.);
#61629=ORIENTED_EDGE('',*,*,#46289,.T.);
#61630=ORIENTED_EDGE('',*,*,#46290,.T.);
#61631=ORIENTED_EDGE('',*,*,#46291,.T.);
#61632=ORIENTED_EDGE('',*,*,#46292,.T.);
#61633=ORIENTED_EDGE('',*,*,#46293,.T.);
#61634=ORIENTED_EDGE('',*,*,#46294,.T.);
#61635=ORIENTED_EDGE('',*,*,#46295,.T.);
#61636=ORIENTED_EDGE('',*,*,#46296,.T.);
#61637=ORIENTED_EDGE('',*,*,#46297,.T.);
#61638=ORIENTED_EDGE('',*,*,#46298,.T.);
#61639=ORIENTED_EDGE('',*,*,#46299,.T.);
#61640=ORIENTED_EDGE('',*,*,#46300,.T.);
#61641=ORIENTED_EDGE('',*,*,#46301,.T.);
#61642=ORIENTED_EDGE('',*,*,#46302,.T.);
#61643=ORIENTED_EDGE('',*,*,#46303,.T.);
#61644=ORIENTED_EDGE('',*,*,#46304,.T.);
#61645=ORIENTED_EDGE('',*,*,#46305,.T.);
#61646=ORIENTED_EDGE('',*,*,#46306,.T.);
#61647=ORIENTED_EDGE('',*,*,#46307,.T.);
#61648=ORIENTED_EDGE('',*,*,#46308,.T.);
#61649=ORIENTED_EDGE('',*,*,#46309,.T.);
#61650=ORIENTED_EDGE('',*,*,#46310,.T.);
#61651=ORIENTED_EDGE('',*,*,#46311,.T.);
#61652=ORIENTED_EDGE('',*,*,#46312,.T.);
#61653=ORIENTED_EDGE('',*,*,#46313,.T.);
#61654=ORIENTED_EDGE('',*,*,#46314,.T.);
#61655=ORIENTED_EDGE('',*,*,#46315,.T.);
#61656=ORIENTED_EDGE('',*,*,#46316,.T.);
#61657=ORIENTED_EDGE('',*,*,#46317,.T.);
#61658=ORIENTED_EDGE('',*,*,#46318,.T.);
#61659=ORIENTED_EDGE('',*,*,#46319,.T.);
#61660=ORIENTED_EDGE('',*,*,#46320,.T.);
#61661=ORIENTED_EDGE('',*,*,#46321,.T.);
#61662=ORIENTED_EDGE('',*,*,#46322,.T.);
#61663=ORIENTED_EDGE('',*,*,#46323,.T.);
#61664=ORIENTED_EDGE('',*,*,#46324,.T.);
#61665=ORIENTED_EDGE('',*,*,#46325,.T.);
#61666=ORIENTED_EDGE('',*,*,#46326,.T.);
#61667=ORIENTED_EDGE('',*,*,#46327,.T.);
#61668=ORIENTED_EDGE('',*,*,#46328,.T.);
#61669=ORIENTED_EDGE('',*,*,#46329,.T.);
#61670=ORIENTED_EDGE('',*,*,#46330,.T.);
#61671=ORIENTED_EDGE('',*,*,#46331,.T.);
#61672=ORIENTED_EDGE('',*,*,#46332,.T.);
#61673=ORIENTED_EDGE('',*,*,#46333,.T.);
#61674=ORIENTED_EDGE('',*,*,#46334,.T.);
#61675=ORIENTED_EDGE('',*,*,#46335,.T.);
#61676=ORIENTED_EDGE('',*,*,#46336,.T.);
#61677=ORIENTED_EDGE('',*,*,#46337,.T.);
#61678=ORIENTED_EDGE('',*,*,#46338,.T.);
#61679=ORIENTED_EDGE('',*,*,#46339,.T.);
#61680=ORIENTED_EDGE('',*,*,#46340,.T.);
#61681=ORIENTED_EDGE('',*,*,#46341,.T.);
#61682=ORIENTED_EDGE('',*,*,#46342,.T.);
#61683=ORIENTED_EDGE('',*,*,#46343,.T.);
#61684=ORIENTED_EDGE('',*,*,#46344,.T.);
#61685=ORIENTED_EDGE('',*,*,#46345,.T.);
#61686=ORIENTED_EDGE('',*,*,#46346,.T.);
#61687=ORIENTED_EDGE('',*,*,#46347,.T.);
#61688=ORIENTED_EDGE('',*,*,#46348,.T.);
#61689=ORIENTED_EDGE('',*,*,#46349,.T.);
#61690=ORIENTED_EDGE('',*,*,#46350,.T.);
#61691=ORIENTED_EDGE('',*,*,#46351,.T.);
#61692=ORIENTED_EDGE('',*,*,#46352,.T.);
#61693=ORIENTED_EDGE('',*,*,#46353,.T.);
#61694=ORIENTED_EDGE('',*,*,#46354,.T.);
#61695=ORIENTED_EDGE('',*,*,#46355,.T.);
#61696=ORIENTED_EDGE('',*,*,#46356,.T.);
#61697=ORIENTED_EDGE('',*,*,#46357,.T.);
#61698=ORIENTED_EDGE('',*,*,#46358,.T.);
#61699=ORIENTED_EDGE('',*,*,#46359,.T.);
#61700=ORIENTED_EDGE('',*,*,#46360,.T.);
#61701=ORIENTED_EDGE('',*,*,#46361,.T.);
#61702=ORIENTED_EDGE('',*,*,#46362,.T.);
#61703=ORIENTED_EDGE('',*,*,#46363,.T.);
#61704=ORIENTED_EDGE('',*,*,#46364,.T.);
#61705=ORIENTED_EDGE('',*,*,#46365,.T.);
#61706=ORIENTED_EDGE('',*,*,#46366,.T.);
#61707=ORIENTED_EDGE('',*,*,#46367,.T.);
#61708=ORIENTED_EDGE('',*,*,#46368,.T.);
#61709=ORIENTED_EDGE('',*,*,#46369,.T.);
#61710=ORIENTED_EDGE('',*,*,#46370,.T.);
#61711=ORIENTED_EDGE('',*,*,#46371,.T.);
#61712=ORIENTED_EDGE('',*,*,#46372,.T.);
#61713=ORIENTED_EDGE('',*,*,#46373,.T.);
#61714=ORIENTED_EDGE('',*,*,#46374,.T.);
#61715=ORIENTED_EDGE('',*,*,#46375,.T.);
#61716=ORIENTED_EDGE('',*,*,#46376,.T.);
#61717=ORIENTED_EDGE('',*,*,#46377,.T.);
#61718=ORIENTED_EDGE('',*,*,#46378,.T.);
#61719=ORIENTED_EDGE('',*,*,#46379,.T.);
#61720=ORIENTED_EDGE('',*,*,#46380,.T.);
#61721=ORIENTED_EDGE('',*,*,#46381,.T.);
#61722=ORIENTED_EDGE('',*,*,#46382,.T.);
#61723=ORIENTED_EDGE('',*,*,#46383,.T.);
#61724=ORIENTED_EDGE('',*,*,#46384,.T.);
#61725=ORIENTED_EDGE('',*,*,#46385,.T.);
#61726=ORIENTED_EDGE('',*,*,#46386,.T.);
#61727=ORIENTED_EDGE('',*,*,#46387,.T.);
#61728=ORIENTED_EDGE('',*,*,#46388,.T.);
#61729=ORIENTED_EDGE('',*,*,#46389,.T.);
#61730=ORIENTED_EDGE('',*,*,#46390,.T.);
#61731=ORIENTED_EDGE('',*,*,#46391,.T.);
#61732=ORIENTED_EDGE('',*,*,#46392,.T.);
#61733=ORIENTED_EDGE('',*,*,#46393,.T.);
#61734=ORIENTED_EDGE('',*,*,#46394,.T.);
#61735=ORIENTED_EDGE('',*,*,#46395,.T.);
#61736=ORIENTED_EDGE('',*,*,#46396,.T.);
#61737=ORIENTED_EDGE('',*,*,#46397,.T.);
#61738=ORIENTED_EDGE('',*,*,#46398,.T.);
#61739=ORIENTED_EDGE('',*,*,#46399,.T.);
#61740=ORIENTED_EDGE('',*,*,#46400,.T.);
#61741=ORIENTED_EDGE('',*,*,#46401,.T.);
#61742=ORIENTED_EDGE('',*,*,#46402,.T.);
#61743=ORIENTED_EDGE('',*,*,#46403,.T.);
#61744=ORIENTED_EDGE('',*,*,#46404,.T.);
#61745=ORIENTED_EDGE('',*,*,#46405,.T.);
#61746=ORIENTED_EDGE('',*,*,#46406,.T.);
#61747=ORIENTED_EDGE('',*,*,#46407,.T.);
#61748=ORIENTED_EDGE('',*,*,#46408,.T.);
#61749=ORIENTED_EDGE('',*,*,#46409,.T.);
#61750=ORIENTED_EDGE('',*,*,#46410,.T.);
#61751=ORIENTED_EDGE('',*,*,#46411,.T.);
#61752=ORIENTED_EDGE('',*,*,#46412,.T.);
#61753=ORIENTED_EDGE('',*,*,#46413,.T.);
#61754=ORIENTED_EDGE('',*,*,#46414,.T.);
#61755=ORIENTED_EDGE('',*,*,#46415,.T.);
#61756=ORIENTED_EDGE('',*,*,#46416,.T.);
#61757=ORIENTED_EDGE('',*,*,#46417,.T.);
#61758=ORIENTED_EDGE('',*,*,#46418,.T.);
#61759=ORIENTED_EDGE('',*,*,#46419,.T.);
#61760=ORIENTED_EDGE('',*,*,#46420,.T.);
#61761=ORIENTED_EDGE('',*,*,#46421,.T.);
#61762=ORIENTED_EDGE('',*,*,#46422,.T.);
#61763=ORIENTED_EDGE('',*,*,#46423,.T.);
#61764=ORIENTED_EDGE('',*,*,#46424,.T.);
#61765=ORIENTED_EDGE('',*,*,#46425,.T.);
#61766=ORIENTED_EDGE('',*,*,#46426,.T.);
#61767=ORIENTED_EDGE('',*,*,#46427,.T.);
#61768=ORIENTED_EDGE('',*,*,#46428,.T.);
#61769=ORIENTED_EDGE('',*,*,#46429,.T.);
#61770=ORIENTED_EDGE('',*,*,#46430,.T.);
#61771=ORIENTED_EDGE('',*,*,#46431,.T.);
#61772=ORIENTED_EDGE('',*,*,#46432,.T.);
#61773=ORIENTED_EDGE('',*,*,#46433,.T.);
#61774=ORIENTED_EDGE('',*,*,#46434,.T.);
#61775=ORIENTED_EDGE('',*,*,#46435,.T.);
#61776=ORIENTED_EDGE('',*,*,#46436,.T.);
#61777=ORIENTED_EDGE('',*,*,#46437,.T.);
#61778=ORIENTED_EDGE('',*,*,#46438,.T.);
#61779=ORIENTED_EDGE('',*,*,#46439,.T.);
#61780=ORIENTED_EDGE('',*,*,#46440,.T.);
#61781=ORIENTED_EDGE('',*,*,#46441,.T.);
#61782=ORIENTED_EDGE('',*,*,#46442,.T.);
#61783=ORIENTED_EDGE('',*,*,#46443,.T.);
#61784=ORIENTED_EDGE('',*,*,#46444,.T.);
#61785=ORIENTED_EDGE('',*,*,#46445,.T.);
#61786=ORIENTED_EDGE('',*,*,#46446,.T.);
#61787=ORIENTED_EDGE('',*,*,#46447,.T.);
#61788=ORIENTED_EDGE('',*,*,#46448,.T.);
#61789=ORIENTED_EDGE('',*,*,#46449,.T.);
#61790=ORIENTED_EDGE('',*,*,#46450,.T.);
#61791=ORIENTED_EDGE('',*,*,#46451,.T.);
#61792=ORIENTED_EDGE('',*,*,#46452,.T.);
#61793=ORIENTED_EDGE('',*,*,#46453,.T.);
#61794=ORIENTED_EDGE('',*,*,#46454,.T.);
#61795=ORIENTED_EDGE('',*,*,#46455,.T.);
#61796=ORIENTED_EDGE('',*,*,#46456,.T.);
#61797=ORIENTED_EDGE('',*,*,#45903,.T.);
#61798=ORIENTED_EDGE('',*,*,#46456,.F.);
#61799=ORIENTED_EDGE('',*,*,#46457,.T.);
#61800=ORIENTED_EDGE('',*,*,#46458,.T.);
#61801=ORIENTED_EDGE('',*,*,#46459,.T.);
#61802=ORIENTED_EDGE('',*,*,#46460,.T.);
#61803=ORIENTED_EDGE('',*,*,#46461,.T.);
#61804=ORIENTED_EDGE('',*,*,#46462,.T.);
#61805=ORIENTED_EDGE('',*,*,#46463,.T.);
#61806=ORIENTED_EDGE('',*,*,#46464,.T.);
#61807=ORIENTED_EDGE('',*,*,#46465,.T.);
#61808=ORIENTED_EDGE('',*,*,#46466,.T.);
#61809=ORIENTED_EDGE('',*,*,#46467,.T.);
#61810=ORIENTED_EDGE('',*,*,#46468,.T.);
#61811=ORIENTED_EDGE('',*,*,#46469,.T.);
#61812=ORIENTED_EDGE('',*,*,#46470,.T.);
#61813=ORIENTED_EDGE('',*,*,#46471,.T.);
#61814=ORIENTED_EDGE('',*,*,#46472,.T.);
#61815=ORIENTED_EDGE('',*,*,#46473,.T.);
#61816=ORIENTED_EDGE('',*,*,#46474,.T.);
#61817=ORIENTED_EDGE('',*,*,#46475,.T.);
#61818=ORIENTED_EDGE('',*,*,#46476,.T.);
#61819=ORIENTED_EDGE('',*,*,#46477,.T.);
#61820=ORIENTED_EDGE('',*,*,#46478,.T.);
#61821=ORIENTED_EDGE('',*,*,#46479,.T.);
#61822=ORIENTED_EDGE('',*,*,#46480,.T.);
#61823=ORIENTED_EDGE('',*,*,#46481,.T.);
#61824=ORIENTED_EDGE('',*,*,#46482,.T.);
#61825=ORIENTED_EDGE('',*,*,#46483,.T.);
#61826=ORIENTED_EDGE('',*,*,#46484,.T.);
#61827=ORIENTED_EDGE('',*,*,#46485,.T.);
#61828=ORIENTED_EDGE('',*,*,#46486,.T.);
#61829=ORIENTED_EDGE('',*,*,#46487,.T.);
#61830=ORIENTED_EDGE('',*,*,#46488,.T.);
#61831=ORIENTED_EDGE('',*,*,#46489,.T.);
#61832=ORIENTED_EDGE('',*,*,#46490,.T.);
#61833=ORIENTED_EDGE('',*,*,#46491,.T.);
#61834=ORIENTED_EDGE('',*,*,#46492,.T.);
#61835=ORIENTED_EDGE('',*,*,#46493,.T.);
#61836=ORIENTED_EDGE('',*,*,#46494,.T.);
#61837=ORIENTED_EDGE('',*,*,#46495,.T.);
#61838=ORIENTED_EDGE('',*,*,#46496,.T.);
#61839=ORIENTED_EDGE('',*,*,#46497,.T.);
#61840=ORIENTED_EDGE('',*,*,#46498,.T.);
#61841=ORIENTED_EDGE('',*,*,#46499,.T.);
#61842=ORIENTED_EDGE('',*,*,#46500,.T.);
#61843=ORIENTED_EDGE('',*,*,#46501,.T.);
#61844=ORIENTED_EDGE('',*,*,#46502,.T.);
#61845=ORIENTED_EDGE('',*,*,#46503,.T.);
#61846=ORIENTED_EDGE('',*,*,#46504,.T.);
#61847=ORIENTED_EDGE('',*,*,#46505,.T.);
#61848=ORIENTED_EDGE('',*,*,#46506,.T.);
#61849=ORIENTED_EDGE('',*,*,#46507,.T.);
#61850=ORIENTED_EDGE('',*,*,#46508,.T.);
#61851=ORIENTED_EDGE('',*,*,#46509,.T.);
#61852=ORIENTED_EDGE('',*,*,#46510,.T.);
#61853=ORIENTED_EDGE('',*,*,#46511,.T.);
#61854=ORIENTED_EDGE('',*,*,#46512,.T.);
#61855=ORIENTED_EDGE('',*,*,#46513,.T.);
#61856=ORIENTED_EDGE('',*,*,#46514,.T.);
#61857=ORIENTED_EDGE('',*,*,#46515,.T.);
#61858=ORIENTED_EDGE('',*,*,#46516,.T.);
#61859=ORIENTED_EDGE('',*,*,#46517,.T.);
#61860=ORIENTED_EDGE('',*,*,#46518,.T.);
#61861=ORIENTED_EDGE('',*,*,#46519,.T.);
#61862=ORIENTED_EDGE('',*,*,#46520,.T.);
#61863=ORIENTED_EDGE('',*,*,#46521,.T.);
#61864=ORIENTED_EDGE('',*,*,#46522,.T.);
#61865=ORIENTED_EDGE('',*,*,#46523,.T.);
#61866=ORIENTED_EDGE('',*,*,#46524,.T.);
#61867=ORIENTED_EDGE('',*,*,#46525,.T.);
#61868=ORIENTED_EDGE('',*,*,#46526,.T.);
#61869=ORIENTED_EDGE('',*,*,#46527,.T.);
#61870=ORIENTED_EDGE('',*,*,#46528,.T.);
#61871=ORIENTED_EDGE('',*,*,#46529,.T.);
#61872=ORIENTED_EDGE('',*,*,#46530,.T.);
#61873=ORIENTED_EDGE('',*,*,#46531,.T.);
#61874=ORIENTED_EDGE('',*,*,#46532,.T.);
#61875=ORIENTED_EDGE('',*,*,#46533,.T.);
#61876=ORIENTED_EDGE('',*,*,#46534,.T.);
#61877=ORIENTED_EDGE('',*,*,#46535,.T.);
#61878=ORIENTED_EDGE('',*,*,#46536,.T.);
#61879=ORIENTED_EDGE('',*,*,#46537,.T.);
#61880=ORIENTED_EDGE('',*,*,#46538,.T.);
#61881=ORIENTED_EDGE('',*,*,#46539,.T.);
#61882=ORIENTED_EDGE('',*,*,#46540,.T.);
#61883=ORIENTED_EDGE('',*,*,#46541,.T.);
#61884=ORIENTED_EDGE('',*,*,#46542,.T.);
#61885=ORIENTED_EDGE('',*,*,#46543,.T.);
#61886=ORIENTED_EDGE('',*,*,#46544,.T.);
#61887=ORIENTED_EDGE('',*,*,#46545,.T.);
#61888=ORIENTED_EDGE('',*,*,#46546,.T.);
#61889=ORIENTED_EDGE('',*,*,#45884,.T.);
#61890=ORIENTED_EDGE('',*,*,#46547,.T.);
#61891=ORIENTED_EDGE('',*,*,#46548,.T.);
#61892=ORIENTED_EDGE('',*,*,#46549,.T.);
#61893=ORIENTED_EDGE('',*,*,#46550,.T.);
#61894=ORIENTED_EDGE('',*,*,#46551,.T.);
#61895=ORIENTED_EDGE('',*,*,#46552,.T.);
#61896=ORIENTED_EDGE('',*,*,#46553,.T.);
#61897=ORIENTED_EDGE('',*,*,#46554,.T.);
#61898=ORIENTED_EDGE('',*,*,#46555,.T.);
#61899=ORIENTED_EDGE('',*,*,#46556,.T.);
#61900=ORIENTED_EDGE('',*,*,#46557,.T.);
#61901=ORIENTED_EDGE('',*,*,#46558,.T.);
#61902=ORIENTED_EDGE('',*,*,#46559,.T.);
#61903=ORIENTED_EDGE('',*,*,#46560,.T.);
#61904=ORIENTED_EDGE('',*,*,#46561,.T.);
#61905=ORIENTED_EDGE('',*,*,#46562,.T.);
#61906=ORIENTED_EDGE('',*,*,#46563,.T.);
#61907=ORIENTED_EDGE('',*,*,#46564,.T.);
#61908=ORIENTED_EDGE('',*,*,#46565,.T.);
#61909=ORIENTED_EDGE('',*,*,#46566,.T.);
#61910=ORIENTED_EDGE('',*,*,#46567,.T.);
#61911=ORIENTED_EDGE('',*,*,#46568,.T.);
#61912=ORIENTED_EDGE('',*,*,#46569,.T.);
#61913=ORIENTED_EDGE('',*,*,#46570,.T.);
#61914=ORIENTED_EDGE('',*,*,#46571,.T.);
#61915=ORIENTED_EDGE('',*,*,#46572,.T.);
#61916=ORIENTED_EDGE('',*,*,#46573,.T.);
#61917=ORIENTED_EDGE('',*,*,#46574,.T.);
#61918=ORIENTED_EDGE('',*,*,#46575,.T.);
#61919=ORIENTED_EDGE('',*,*,#46576,.T.);
#61920=ORIENTED_EDGE('',*,*,#46577,.T.);
#61921=ORIENTED_EDGE('',*,*,#46578,.T.);
#61922=ORIENTED_EDGE('',*,*,#46579,.T.);
#61923=ORIENTED_EDGE('',*,*,#46580,.T.);
#61924=ORIENTED_EDGE('',*,*,#46581,.T.);
#61925=ORIENTED_EDGE('',*,*,#46582,.T.);
#61926=ORIENTED_EDGE('',*,*,#46583,.T.);
#61927=ORIENTED_EDGE('',*,*,#46584,.T.);
#61928=ORIENTED_EDGE('',*,*,#46585,.T.);
#61929=ORIENTED_EDGE('',*,*,#46586,.T.);
#61930=ORIENTED_EDGE('',*,*,#46587,.T.);
#61931=ORIENTED_EDGE('',*,*,#46588,.T.);
#61932=ORIENTED_EDGE('',*,*,#46589,.T.);
#61933=ORIENTED_EDGE('',*,*,#46590,.T.);
#61934=ORIENTED_EDGE('',*,*,#46591,.T.);
#61935=ORIENTED_EDGE('',*,*,#46592,.T.);
#61936=ORIENTED_EDGE('',*,*,#46593,.T.);
#61937=ORIENTED_EDGE('',*,*,#46594,.T.);
#61938=ORIENTED_EDGE('',*,*,#46595,.T.);
#61939=ORIENTED_EDGE('',*,*,#46596,.T.);
#61940=ORIENTED_EDGE('',*,*,#46597,.T.);
#61941=ORIENTED_EDGE('',*,*,#46598,.T.);
#61942=ORIENTED_EDGE('',*,*,#46599,.T.);
#61943=ORIENTED_EDGE('',*,*,#46600,.T.);
#61944=ORIENTED_EDGE('',*,*,#46601,.T.);
#61945=ORIENTED_EDGE('',*,*,#46602,.T.);
#61946=ORIENTED_EDGE('',*,*,#46603,.T.);
#61947=ORIENTED_EDGE('',*,*,#46604,.T.);
#61948=ORIENTED_EDGE('',*,*,#46605,.T.);
#61949=ORIENTED_EDGE('',*,*,#46606,.T.);
#61950=ORIENTED_EDGE('',*,*,#46607,.T.);
#61951=ORIENTED_EDGE('',*,*,#46608,.T.);
#61952=ORIENTED_EDGE('',*,*,#46609,.T.);
#61953=ORIENTED_EDGE('',*,*,#46610,.T.);
#61954=ORIENTED_EDGE('',*,*,#46611,.T.);
#61955=ORIENTED_EDGE('',*,*,#46612,.T.);
#61956=ORIENTED_EDGE('',*,*,#46613,.T.);
#61957=ORIENTED_EDGE('',*,*,#46614,.T.);
#61958=ORIENTED_EDGE('',*,*,#46615,.T.);
#61959=ORIENTED_EDGE('',*,*,#46616,.T.);
#61960=ORIENTED_EDGE('',*,*,#46617,.T.);
#61961=ORIENTED_EDGE('',*,*,#46618,.T.);
#61962=ORIENTED_EDGE('',*,*,#46619,.T.);
#61963=ORIENTED_EDGE('',*,*,#46620,.T.);
#61964=ORIENTED_EDGE('',*,*,#46621,.T.);
#61965=ORIENTED_EDGE('',*,*,#46622,.T.);
#61966=ORIENTED_EDGE('',*,*,#46623,.T.);
#61967=ORIENTED_EDGE('',*,*,#46624,.T.);
#61968=ORIENTED_EDGE('',*,*,#46625,.T.);
#61969=ORIENTED_EDGE('',*,*,#46626,.T.);
#61970=ORIENTED_EDGE('',*,*,#46627,.T.);
#61971=ORIENTED_EDGE('',*,*,#46628,.T.);
#61972=ORIENTED_EDGE('',*,*,#46629,.T.);
#61973=ORIENTED_EDGE('',*,*,#46630,.T.);
#61974=ORIENTED_EDGE('',*,*,#46631,.T.);
#61975=ORIENTED_EDGE('',*,*,#46632,.T.);
#61976=ORIENTED_EDGE('',*,*,#46633,.T.);
#61977=ORIENTED_EDGE('',*,*,#46634,.T.);
#61978=ORIENTED_EDGE('',*,*,#46635,.T.);
#61979=ORIENTED_EDGE('',*,*,#46636,.T.);
#61980=ORIENTED_EDGE('',*,*,#46637,.T.);
#61981=ORIENTED_EDGE('',*,*,#45901,.T.);
#61982=ORIENTED_EDGE('',*,*,#45902,.T.);
#61983=ORIENTED_EDGE('',*,*,#46637,.F.);
#61984=ORIENTED_EDGE('',*,*,#46638,.T.);
#61985=ORIENTED_EDGE('',*,*,#46636,.F.);
#61986=ORIENTED_EDGE('',*,*,#46639,.T.);
#61987=ORIENTED_EDGE('',*,*,#46640,.T.);
#61988=ORIENTED_EDGE('',*,*,#46639,.F.);
#61989=ORIENTED_EDGE('',*,*,#46638,.F.);
#61990=ORIENTED_EDGE('',*,*,#46641,.F.);
#61991=ORIENTED_EDGE('',*,*,#46642,.T.);
#61992=ORIENTED_EDGE('',*,*,#46643,.T.);
#61993=ORIENTED_EDGE('',*,*,#46644,.T.);
#61994=ORIENTED_EDGE('',*,*,#46645,.F.);
#61995=ORIENTED_EDGE('',*,*,#46646,.F.);
#61996=ORIENTED_EDGE('',*,*,#46647,.T.);
#61997=ORIENTED_EDGE('',*,*,#46648,.T.);
#61998=ORIENTED_EDGE('',*,*,#46646,.T.);
#61999=ORIENTED_EDGE('',*,*,#46649,.T.);
#62000=ORIENTED_EDGE('',*,*,#46650,.T.);
#62001=ORIENTED_EDGE('',*,*,#46651,.T.);
#62002=ORIENTED_EDGE('',*,*,#46652,.T.);
#62003=ORIENTED_EDGE('',*,*,#46653,.T.);
#62004=ORIENTED_EDGE('',*,*,#46654,.F.);
#62005=ORIENTED_EDGE('',*,*,#46655,.T.);
#62006=ORIENTED_EDGE('',*,*,#46656,.T.);
#62007=ORIENTED_EDGE('',*,*,#46657,.T.);
#62008=ORIENTED_EDGE('',*,*,#46658,.F.);
#62009=ORIENTED_EDGE('',*,*,#46659,.F.);
#62010=ORIENTED_EDGE('',*,*,#46660,.T.);
#62011=ORIENTED_EDGE('',*,*,#46661,.T.);
#62012=ORIENTED_EDGE('',*,*,#46659,.T.);
#62013=ORIENTED_EDGE('',*,*,#46662,.T.);
#62014=ORIENTED_EDGE('',*,*,#46643,.F.);
#62015=ORIENTED_EDGE('',*,*,#46663,.T.);
#62016=ORIENTED_EDGE('',*,*,#46460,.F.);
#62017=ORIENTED_EDGE('',*,*,#46664,.T.);
#62018=ORIENTED_EDGE('',*,*,#46273,.F.);
#62019=ORIENTED_EDGE('',*,*,#46665,.T.);
#62020=ORIENTED_EDGE('',*,*,#46660,.F.);
#62021=ORIENTED_EDGE('',*,*,#46666,.T.);
#62022=ORIENTED_EDGE('',*,*,#46656,.F.);
#62023=ORIENTED_EDGE('',*,*,#46667,.T.);
#62024=ORIENTED_EDGE('',*,*,#46650,.F.);
#62025=ORIENTED_EDGE('',*,*,#46668,.T.);
#62026=ORIENTED_EDGE('',*,*,#46652,.F.);
#62027=ORIENTED_EDGE('',*,*,#46669,.T.);
#62028=ORIENTED_EDGE('',*,*,#46647,.F.);
#62029=ORIENTED_EDGE('',*,*,#46670,.T.);
#62030=ORIENTED_EDGE('',*,*,#46671,.T.);
#62031=ORIENTED_EDGE('',*,*,#46672,.T.);
#62032=ORIENTED_EDGE('',*,*,#46673,.F.);
#62033=ORIENTED_EDGE('',*,*,#46674,.F.);
#62034=ORIENTED_EDGE('',*,*,#46675,.F.);
#62035=ORIENTED_EDGE('',*,*,#46676,.T.);
#62036=ORIENTED_EDGE('',*,*,#46674,.T.);
#62037=ORIENTED_EDGE('',*,*,#46677,.T.);
#62038=ORIENTED_EDGE('',*,*,#46678,.T.);
#62039=ORIENTED_EDGE('',*,*,#46679,.T.);
#62040=ORIENTED_EDGE('',*,*,#46680,.T.);
#62041=ORIENTED_EDGE('',*,*,#46681,.T.);
#62042=ORIENTED_EDGE('',*,*,#46682,.T.);
#62043=ORIENTED_EDGE('',*,*,#46683,.T.);
#62044=ORIENTED_EDGE('',*,*,#46684,.T.);
#62045=ORIENTED_EDGE('',*,*,#46685,.T.);
#62046=ORIENTED_EDGE('',*,*,#46686,.F.);
#62047=ORIENTED_EDGE('',*,*,#46687,.F.);
#62048=ORIENTED_EDGE('',*,*,#46688,.F.);
#62049=ORIENTED_EDGE('',*,*,#46689,.T.);
#62050=ORIENTED_EDGE('',*,*,#46687,.T.);
#62051=ORIENTED_EDGE('',*,*,#46690,.T.);
#62052=ORIENTED_EDGE('',*,*,#46691,.T.);
#62053=ORIENTED_EDGE('',*,*,#46692,.T.);
#62054=ORIENTED_EDGE('',*,*,#46466,.F.);
#62055=ORIENTED_EDGE('',*,*,#46693,.T.);
#62056=ORIENTED_EDGE('',*,*,#46671,.F.);
#62057=ORIENTED_EDGE('',*,*,#46694,.T.);
#62058=ORIENTED_EDGE('',*,*,#46691,.F.);
#62059=ORIENTED_EDGE('',*,*,#46695,.T.);
#62060=ORIENTED_EDGE('',*,*,#46267,.F.);
#62061=ORIENTED_EDGE('',*,*,#46696,.T.);
#62062=ORIENTED_EDGE('',*,*,#46682,.F.);
#62063=ORIENTED_EDGE('',*,*,#46697,.T.);
#62064=ORIENTED_EDGE('',*,*,#46684,.F.);
#62065=ORIENTED_EDGE('',*,*,#46698,.T.);
#62066=ORIENTED_EDGE('',*,*,#46678,.F.);
#62067=ORIENTED_EDGE('',*,*,#46699,.T.);
#62068=ORIENTED_EDGE('',*,*,#46680,.F.);
#62069=ORIENTED_EDGE('',*,*,#46700,.T.);
#62070=ORIENTED_EDGE('',*,*,#46701,.T.);
#62071=ORIENTED_EDGE('',*,*,#46702,.T.);
#62072=ORIENTED_EDGE('',*,*,#46703,.F.);
#62073=ORIENTED_EDGE('',*,*,#46704,.F.);
#62074=ORIENTED_EDGE('',*,*,#46705,.F.);
#62075=ORIENTED_EDGE('',*,*,#46706,.T.);
#62076=ORIENTED_EDGE('',*,*,#46704,.T.);
#62077=ORIENTED_EDGE('',*,*,#46707,.T.);
#62078=ORIENTED_EDGE('',*,*,#46708,.T.);
#62079=ORIENTED_EDGE('',*,*,#46709,.T.);
#62080=ORIENTED_EDGE('',*,*,#46710,.T.);
#62081=ORIENTED_EDGE('',*,*,#46711,.T.);
#62082=ORIENTED_EDGE('',*,*,#46712,.T.);
#62083=ORIENTED_EDGE('',*,*,#46713,.T.);
#62084=ORIENTED_EDGE('',*,*,#46714,.T.);
#62085=ORIENTED_EDGE('',*,*,#46715,.T.);
#62086=ORIENTED_EDGE('',*,*,#46716,.F.);
#62087=ORIENTED_EDGE('',*,*,#46717,.F.);
#62088=ORIENTED_EDGE('',*,*,#46718,.F.);
#62089=ORIENTED_EDGE('',*,*,#46719,.T.);
#62090=ORIENTED_EDGE('',*,*,#46717,.T.);
#62091=ORIENTED_EDGE('',*,*,#46720,.T.);
#62092=ORIENTED_EDGE('',*,*,#46721,.T.);
#62093=ORIENTED_EDGE('',*,*,#46722,.T.);
#62094=ORIENTED_EDGE('',*,*,#46472,.F.);
#62095=ORIENTED_EDGE('',*,*,#46723,.T.);
#62096=ORIENTED_EDGE('',*,*,#46701,.F.);
#62097=ORIENTED_EDGE('',*,*,#46724,.T.);
#62098=ORIENTED_EDGE('',*,*,#46721,.F.);
#62099=ORIENTED_EDGE('',*,*,#46725,.T.);
#62100=ORIENTED_EDGE('',*,*,#46261,.F.);
#62101=ORIENTED_EDGE('',*,*,#46726,.T.);
#62102=ORIENTED_EDGE('',*,*,#46712,.F.);
#62103=ORIENTED_EDGE('',*,*,#46727,.T.);
#62104=ORIENTED_EDGE('',*,*,#46714,.F.);
#62105=ORIENTED_EDGE('',*,*,#46728,.T.);
#62106=ORIENTED_EDGE('',*,*,#46708,.F.);
#62107=ORIENTED_EDGE('',*,*,#46729,.T.);
#62108=ORIENTED_EDGE('',*,*,#46710,.F.);
#62109=ORIENTED_EDGE('',*,*,#46730,.T.);
#62110=ORIENTED_EDGE('',*,*,#46731,.T.);
#62111=ORIENTED_EDGE('',*,*,#46732,.T.);
#62112=ORIENTED_EDGE('',*,*,#46733,.F.);
#62113=ORIENTED_EDGE('',*,*,#46734,.F.);
#62114=ORIENTED_EDGE('',*,*,#46735,.F.);
#62115=ORIENTED_EDGE('',*,*,#46736,.T.);
#62116=ORIENTED_EDGE('',*,*,#46734,.T.);
#62117=ORIENTED_EDGE('',*,*,#46737,.T.);
#62118=ORIENTED_EDGE('',*,*,#46738,.T.);
#62119=ORIENTED_EDGE('',*,*,#46739,.T.);
#62120=ORIENTED_EDGE('',*,*,#46740,.T.);
#62121=ORIENTED_EDGE('',*,*,#46741,.T.);
#62122=ORIENTED_EDGE('',*,*,#46742,.T.);
#62123=ORIENTED_EDGE('',*,*,#46743,.T.);
#62124=ORIENTED_EDGE('',*,*,#46744,.T.);
#62125=ORIENTED_EDGE('',*,*,#46745,.T.);
#62126=ORIENTED_EDGE('',*,*,#46746,.F.);
#62127=ORIENTED_EDGE('',*,*,#46747,.F.);
#62128=ORIENTED_EDGE('',*,*,#46748,.F.);
#62129=ORIENTED_EDGE('',*,*,#46749,.T.);
#62130=ORIENTED_EDGE('',*,*,#46747,.T.);
#62131=ORIENTED_EDGE('',*,*,#46750,.T.);
#62132=ORIENTED_EDGE('',*,*,#46751,.T.);
#62133=ORIENTED_EDGE('',*,*,#46752,.T.);
#62134=ORIENTED_EDGE('',*,*,#46478,.F.);
#62135=ORIENTED_EDGE('',*,*,#46753,.T.);
#62136=ORIENTED_EDGE('',*,*,#46731,.F.);
#62137=ORIENTED_EDGE('',*,*,#46754,.T.);
#62138=ORIENTED_EDGE('',*,*,#46751,.F.);
#62139=ORIENTED_EDGE('',*,*,#46755,.T.);
#62140=ORIENTED_EDGE('',*,*,#46255,.F.);
#62141=ORIENTED_EDGE('',*,*,#46756,.T.);
#62142=ORIENTED_EDGE('',*,*,#46742,.F.);
#62143=ORIENTED_EDGE('',*,*,#46757,.T.);
#62144=ORIENTED_EDGE('',*,*,#46744,.F.);
#62145=ORIENTED_EDGE('',*,*,#46758,.T.);
#62146=ORIENTED_EDGE('',*,*,#46738,.F.);
#62147=ORIENTED_EDGE('',*,*,#46759,.T.);
#62148=ORIENTED_EDGE('',*,*,#46740,.F.);
#62149=ORIENTED_EDGE('',*,*,#46760,.T.);
#62150=ORIENTED_EDGE('',*,*,#46761,.T.);
#62151=ORIENTED_EDGE('',*,*,#46762,.T.);
#62152=ORIENTED_EDGE('',*,*,#46763,.F.);
#62153=ORIENTED_EDGE('',*,*,#46764,.F.);
#62154=ORIENTED_EDGE('',*,*,#46765,.F.);
#62155=ORIENTED_EDGE('',*,*,#46766,.T.);
#62156=ORIENTED_EDGE('',*,*,#46764,.T.);
#62157=ORIENTED_EDGE('',*,*,#46767,.T.);
#62158=ORIENTED_EDGE('',*,*,#46768,.T.);
#62159=ORIENTED_EDGE('',*,*,#46769,.T.);
#62160=ORIENTED_EDGE('',*,*,#46770,.T.);
#62161=ORIENTED_EDGE('',*,*,#46771,.T.);
#62162=ORIENTED_EDGE('',*,*,#46772,.T.);
#62163=ORIENTED_EDGE('',*,*,#46773,.T.);
#62164=ORIENTED_EDGE('',*,*,#46774,.T.);
#62165=ORIENTED_EDGE('',*,*,#46775,.T.);
#62166=ORIENTED_EDGE('',*,*,#46776,.F.);
#62167=ORIENTED_EDGE('',*,*,#46777,.F.);
#62168=ORIENTED_EDGE('',*,*,#46778,.F.);
#62169=ORIENTED_EDGE('',*,*,#46779,.T.);
#62170=ORIENTED_EDGE('',*,*,#46777,.T.);
#62171=ORIENTED_EDGE('',*,*,#46780,.T.);
#62172=ORIENTED_EDGE('',*,*,#46781,.T.);
#62173=ORIENTED_EDGE('',*,*,#46782,.T.);
#62174=ORIENTED_EDGE('',*,*,#46484,.F.);
#62175=ORIENTED_EDGE('',*,*,#46783,.T.);
#62176=ORIENTED_EDGE('',*,*,#46761,.F.);
#62177=ORIENTED_EDGE('',*,*,#46784,.T.);
#62178=ORIENTED_EDGE('',*,*,#46781,.F.);
#62179=ORIENTED_EDGE('',*,*,#46785,.T.);
#62180=ORIENTED_EDGE('',*,*,#46249,.F.);
#62181=ORIENTED_EDGE('',*,*,#46786,.T.);
#62182=ORIENTED_EDGE('',*,*,#46772,.F.);
#62183=ORIENTED_EDGE('',*,*,#46787,.T.);
#62184=ORIENTED_EDGE('',*,*,#46774,.F.);
#62185=ORIENTED_EDGE('',*,*,#46788,.T.);
#62186=ORIENTED_EDGE('',*,*,#46768,.F.);
#62187=ORIENTED_EDGE('',*,*,#46789,.T.);
#62188=ORIENTED_EDGE('',*,*,#46770,.F.);
#62189=ORIENTED_EDGE('',*,*,#46790,.T.);
#62190=ORIENTED_EDGE('',*,*,#46791,.T.);
#62191=ORIENTED_EDGE('',*,*,#46792,.T.);
#62192=ORIENTED_EDGE('',*,*,#46793,.F.);
#62193=ORIENTED_EDGE('',*,*,#46794,.F.);
#62194=ORIENTED_EDGE('',*,*,#46795,.F.);
#62195=ORIENTED_EDGE('',*,*,#46796,.T.);
#62196=ORIENTED_EDGE('',*,*,#46794,.T.);
#62197=ORIENTED_EDGE('',*,*,#46797,.T.);
#62198=ORIENTED_EDGE('',*,*,#46798,.T.);
#62199=ORIENTED_EDGE('',*,*,#46799,.T.);
#62200=ORIENTED_EDGE('',*,*,#46800,.T.);
#62201=ORIENTED_EDGE('',*,*,#46801,.T.);
#62202=ORIENTED_EDGE('',*,*,#46802,.T.);
#62203=ORIENTED_EDGE('',*,*,#46803,.T.);
#62204=ORIENTED_EDGE('',*,*,#46804,.T.);
#62205=ORIENTED_EDGE('',*,*,#46805,.T.);
#62206=ORIENTED_EDGE('',*,*,#46806,.F.);
#62207=ORIENTED_EDGE('',*,*,#46807,.F.);
#62208=ORIENTED_EDGE('',*,*,#46808,.F.);
#62209=ORIENTED_EDGE('',*,*,#46809,.T.);
#62210=ORIENTED_EDGE('',*,*,#46807,.T.);
#62211=ORIENTED_EDGE('',*,*,#46810,.T.);
#62212=ORIENTED_EDGE('',*,*,#46811,.T.);
#62213=ORIENTED_EDGE('',*,*,#46812,.T.);
#62214=ORIENTED_EDGE('',*,*,#46490,.F.);
#62215=ORIENTED_EDGE('',*,*,#46813,.T.);
#62216=ORIENTED_EDGE('',*,*,#46791,.F.);
#62217=ORIENTED_EDGE('',*,*,#46814,.T.);
#62218=ORIENTED_EDGE('',*,*,#46811,.F.);
#62219=ORIENTED_EDGE('',*,*,#46815,.T.);
#62220=ORIENTED_EDGE('',*,*,#46243,.F.);
#62221=ORIENTED_EDGE('',*,*,#46816,.T.);
#62222=ORIENTED_EDGE('',*,*,#46802,.F.);
#62223=ORIENTED_EDGE('',*,*,#46817,.T.);
#62224=ORIENTED_EDGE('',*,*,#46804,.F.);
#62225=ORIENTED_EDGE('',*,*,#46818,.T.);
#62226=ORIENTED_EDGE('',*,*,#46798,.F.);
#62227=ORIENTED_EDGE('',*,*,#46819,.T.);
#62228=ORIENTED_EDGE('',*,*,#46800,.F.);
#62229=ORIENTED_EDGE('',*,*,#46820,.T.);
#62230=ORIENTED_EDGE('',*,*,#46821,.T.);
#62231=ORIENTED_EDGE('',*,*,#46822,.T.);
#62232=ORIENTED_EDGE('',*,*,#46823,.F.);
#62233=ORIENTED_EDGE('',*,*,#46824,.F.);
#62234=ORIENTED_EDGE('',*,*,#46825,.F.);
#62235=ORIENTED_EDGE('',*,*,#46826,.T.);
#62236=ORIENTED_EDGE('',*,*,#46824,.T.);
#62237=ORIENTED_EDGE('',*,*,#46827,.T.);
#62238=ORIENTED_EDGE('',*,*,#46828,.T.);
#62239=ORIENTED_EDGE('',*,*,#46829,.T.);
#62240=ORIENTED_EDGE('',*,*,#46830,.T.);
#62241=ORIENTED_EDGE('',*,*,#46831,.T.);
#62242=ORIENTED_EDGE('',*,*,#46832,.T.);
#62243=ORIENTED_EDGE('',*,*,#46833,.T.);
#62244=ORIENTED_EDGE('',*,*,#46834,.T.);
#62245=ORIENTED_EDGE('',*,*,#46835,.T.);
#62246=ORIENTED_EDGE('',*,*,#46836,.F.);
#62247=ORIENTED_EDGE('',*,*,#46837,.F.);
#62248=ORIENTED_EDGE('',*,*,#46838,.F.);
#62249=ORIENTED_EDGE('',*,*,#46839,.T.);
#62250=ORIENTED_EDGE('',*,*,#46837,.T.);
#62251=ORIENTED_EDGE('',*,*,#46840,.T.);
#62252=ORIENTED_EDGE('',*,*,#46841,.T.);
#62253=ORIENTED_EDGE('',*,*,#46842,.T.);
#62254=ORIENTED_EDGE('',*,*,#46496,.F.);
#62255=ORIENTED_EDGE('',*,*,#46843,.T.);
#62256=ORIENTED_EDGE('',*,*,#46821,.F.);
#62257=ORIENTED_EDGE('',*,*,#46844,.T.);
#62258=ORIENTED_EDGE('',*,*,#46841,.F.);
#62259=ORIENTED_EDGE('',*,*,#46845,.T.);
#62260=ORIENTED_EDGE('',*,*,#46237,.F.);
#62261=ORIENTED_EDGE('',*,*,#46846,.T.);
#62262=ORIENTED_EDGE('',*,*,#46832,.F.);
#62263=ORIENTED_EDGE('',*,*,#46847,.T.);
#62264=ORIENTED_EDGE('',*,*,#46834,.F.);
#62265=ORIENTED_EDGE('',*,*,#46848,.T.);
#62266=ORIENTED_EDGE('',*,*,#46828,.F.);
#62267=ORIENTED_EDGE('',*,*,#46849,.T.);
#62268=ORIENTED_EDGE('',*,*,#46830,.F.);
#62269=ORIENTED_EDGE('',*,*,#46850,.T.);
#62270=ORIENTED_EDGE('',*,*,#46851,.T.);
#62271=ORIENTED_EDGE('',*,*,#46852,.T.);
#62272=ORIENTED_EDGE('',*,*,#46853,.F.);
#62273=ORIENTED_EDGE('',*,*,#46854,.F.);
#62274=ORIENTED_EDGE('',*,*,#46855,.F.);
#62275=ORIENTED_EDGE('',*,*,#46856,.T.);
#62276=ORIENTED_EDGE('',*,*,#46854,.T.);
#62277=ORIENTED_EDGE('',*,*,#46857,.T.);
#62278=ORIENTED_EDGE('',*,*,#46858,.T.);
#62279=ORIENTED_EDGE('',*,*,#46859,.T.);
#62280=ORIENTED_EDGE('',*,*,#46860,.T.);
#62281=ORIENTED_EDGE('',*,*,#46861,.T.);
#62282=ORIENTED_EDGE('',*,*,#46862,.T.);
#62283=ORIENTED_EDGE('',*,*,#46863,.T.);
#62284=ORIENTED_EDGE('',*,*,#46864,.T.);
#62285=ORIENTED_EDGE('',*,*,#46865,.T.);
#62286=ORIENTED_EDGE('',*,*,#46866,.F.);
#62287=ORIENTED_EDGE('',*,*,#46867,.F.);
#62288=ORIENTED_EDGE('',*,*,#46868,.F.);
#62289=ORIENTED_EDGE('',*,*,#46869,.T.);
#62290=ORIENTED_EDGE('',*,*,#46867,.T.);
#62291=ORIENTED_EDGE('',*,*,#46870,.T.);
#62292=ORIENTED_EDGE('',*,*,#46871,.T.);
#62293=ORIENTED_EDGE('',*,*,#46872,.T.);
#62294=ORIENTED_EDGE('',*,*,#46502,.F.);
#62295=ORIENTED_EDGE('',*,*,#46873,.T.);
#62296=ORIENTED_EDGE('',*,*,#46851,.F.);
#62297=ORIENTED_EDGE('',*,*,#46874,.T.);
#62298=ORIENTED_EDGE('',*,*,#46871,.F.);
#62299=ORIENTED_EDGE('',*,*,#46875,.T.);
#62300=ORIENTED_EDGE('',*,*,#46231,.F.);
#62301=ORIENTED_EDGE('',*,*,#46876,.T.);
#62302=ORIENTED_EDGE('',*,*,#46862,.F.);
#62303=ORIENTED_EDGE('',*,*,#46877,.T.);
#62304=ORIENTED_EDGE('',*,*,#46864,.F.);
#62305=ORIENTED_EDGE('',*,*,#46878,.T.);
#62306=ORIENTED_EDGE('',*,*,#46858,.F.);
#62307=ORIENTED_EDGE('',*,*,#46879,.T.);
#62308=ORIENTED_EDGE('',*,*,#46860,.F.);
#62309=ORIENTED_EDGE('',*,*,#46880,.T.);
#62310=ORIENTED_EDGE('',*,*,#46881,.T.);
#62311=ORIENTED_EDGE('',*,*,#46882,.T.);
#62312=ORIENTED_EDGE('',*,*,#46883,.F.);
#62313=ORIENTED_EDGE('',*,*,#46884,.F.);
#62314=ORIENTED_EDGE('',*,*,#46885,.F.);
#62315=ORIENTED_EDGE('',*,*,#46886,.T.);
#62316=ORIENTED_EDGE('',*,*,#46884,.T.);
#62317=ORIENTED_EDGE('',*,*,#46887,.T.);
#62318=ORIENTED_EDGE('',*,*,#46888,.T.);
#62319=ORIENTED_EDGE('',*,*,#46889,.T.);
#62320=ORIENTED_EDGE('',*,*,#46890,.T.);
#62321=ORIENTED_EDGE('',*,*,#46891,.T.);
#62322=ORIENTED_EDGE('',*,*,#46892,.T.);
#62323=ORIENTED_EDGE('',*,*,#46893,.T.);
#62324=ORIENTED_EDGE('',*,*,#46894,.T.);
#62325=ORIENTED_EDGE('',*,*,#46895,.T.);
#62326=ORIENTED_EDGE('',*,*,#46896,.F.);
#62327=ORIENTED_EDGE('',*,*,#46897,.F.);
#62328=ORIENTED_EDGE('',*,*,#46898,.F.);
#62329=ORIENTED_EDGE('',*,*,#46899,.T.);
#62330=ORIENTED_EDGE('',*,*,#46897,.T.);
#62331=ORIENTED_EDGE('',*,*,#46900,.T.);
#62332=ORIENTED_EDGE('',*,*,#46901,.T.);
#62333=ORIENTED_EDGE('',*,*,#46902,.T.);
#62334=ORIENTED_EDGE('',*,*,#46508,.F.);
#62335=ORIENTED_EDGE('',*,*,#46903,.T.);
#62336=ORIENTED_EDGE('',*,*,#46881,.F.);
#62337=ORIENTED_EDGE('',*,*,#46904,.T.);
#62338=ORIENTED_EDGE('',*,*,#46901,.F.);
#62339=ORIENTED_EDGE('',*,*,#46905,.T.);
#62340=ORIENTED_EDGE('',*,*,#46225,.F.);
#62341=ORIENTED_EDGE('',*,*,#46906,.T.);
#62342=ORIENTED_EDGE('',*,*,#46892,.F.);
#62343=ORIENTED_EDGE('',*,*,#46907,.T.);
#62344=ORIENTED_EDGE('',*,*,#46894,.F.);
#62345=ORIENTED_EDGE('',*,*,#46908,.T.);
#62346=ORIENTED_EDGE('',*,*,#46888,.F.);
#62347=ORIENTED_EDGE('',*,*,#46909,.T.);
#62348=ORIENTED_EDGE('',*,*,#46890,.F.);
#62349=ORIENTED_EDGE('',*,*,#46910,.T.);
#62350=ORIENTED_EDGE('',*,*,#46911,.T.);
#62351=ORIENTED_EDGE('',*,*,#46912,.T.);
#62352=ORIENTED_EDGE('',*,*,#46913,.F.);
#62353=ORIENTED_EDGE('',*,*,#46914,.F.);
#62354=ORIENTED_EDGE('',*,*,#46915,.F.);
#62355=ORIENTED_EDGE('',*,*,#46916,.T.);
#62356=ORIENTED_EDGE('',*,*,#46914,.T.);
#62357=ORIENTED_EDGE('',*,*,#46917,.T.);
#62358=ORIENTED_EDGE('',*,*,#46918,.T.);
#62359=ORIENTED_EDGE('',*,*,#46919,.T.);
#62360=ORIENTED_EDGE('',*,*,#46920,.T.);
#62361=ORIENTED_EDGE('',*,*,#46921,.T.);
#62362=ORIENTED_EDGE('',*,*,#46922,.T.);
#62363=ORIENTED_EDGE('',*,*,#46923,.T.);
#62364=ORIENTED_EDGE('',*,*,#46924,.T.);
#62365=ORIENTED_EDGE('',*,*,#46925,.T.);
#62366=ORIENTED_EDGE('',*,*,#46926,.F.);
#62367=ORIENTED_EDGE('',*,*,#46927,.F.);
#62368=ORIENTED_EDGE('',*,*,#46928,.F.);
#62369=ORIENTED_EDGE('',*,*,#46929,.T.);
#62370=ORIENTED_EDGE('',*,*,#46927,.T.);
#62371=ORIENTED_EDGE('',*,*,#46930,.T.);
#62372=ORIENTED_EDGE('',*,*,#46931,.T.);
#62373=ORIENTED_EDGE('',*,*,#46932,.T.);
#62374=ORIENTED_EDGE('',*,*,#46514,.F.);
#62375=ORIENTED_EDGE('',*,*,#46933,.T.);
#62376=ORIENTED_EDGE('',*,*,#46911,.F.);
#62377=ORIENTED_EDGE('',*,*,#46934,.T.);
#62378=ORIENTED_EDGE('',*,*,#46931,.F.);
#62379=ORIENTED_EDGE('',*,*,#46935,.T.);
#62380=ORIENTED_EDGE('',*,*,#46219,.F.);
#62381=ORIENTED_EDGE('',*,*,#46936,.T.);
#62382=ORIENTED_EDGE('',*,*,#46922,.F.);
#62383=ORIENTED_EDGE('',*,*,#46937,.T.);
#62384=ORIENTED_EDGE('',*,*,#46924,.F.);
#62385=ORIENTED_EDGE('',*,*,#46938,.T.);
#62386=ORIENTED_EDGE('',*,*,#46918,.F.);
#62387=ORIENTED_EDGE('',*,*,#46939,.T.);
#62388=ORIENTED_EDGE('',*,*,#46920,.F.);
#62389=ORIENTED_EDGE('',*,*,#46940,.T.);
#62390=ORIENTED_EDGE('',*,*,#46941,.T.);
#62391=ORIENTED_EDGE('',*,*,#46942,.T.);
#62392=ORIENTED_EDGE('',*,*,#46943,.F.);
#62393=ORIENTED_EDGE('',*,*,#46944,.F.);
#62394=ORIENTED_EDGE('',*,*,#46945,.F.);
#62395=ORIENTED_EDGE('',*,*,#46946,.T.);
#62396=ORIENTED_EDGE('',*,*,#46944,.T.);
#62397=ORIENTED_EDGE('',*,*,#46947,.T.);
#62398=ORIENTED_EDGE('',*,*,#46948,.T.);
#62399=ORIENTED_EDGE('',*,*,#46949,.T.);
#62400=ORIENTED_EDGE('',*,*,#46950,.T.);
#62401=ORIENTED_EDGE('',*,*,#46951,.T.);
#62402=ORIENTED_EDGE('',*,*,#46952,.T.);
#62403=ORIENTED_EDGE('',*,*,#46953,.T.);
#62404=ORIENTED_EDGE('',*,*,#46954,.T.);
#62405=ORIENTED_EDGE('',*,*,#46955,.T.);
#62406=ORIENTED_EDGE('',*,*,#46956,.F.);
#62407=ORIENTED_EDGE('',*,*,#46957,.F.);
#62408=ORIENTED_EDGE('',*,*,#46958,.F.);
#62409=ORIENTED_EDGE('',*,*,#46959,.T.);
#62410=ORIENTED_EDGE('',*,*,#46957,.T.);
#62411=ORIENTED_EDGE('',*,*,#46960,.T.);
#62412=ORIENTED_EDGE('',*,*,#46961,.T.);
#62413=ORIENTED_EDGE('',*,*,#46962,.T.);
#62414=ORIENTED_EDGE('',*,*,#46520,.F.);
#62415=ORIENTED_EDGE('',*,*,#46963,.T.);
#62416=ORIENTED_EDGE('',*,*,#46941,.F.);
#62417=ORIENTED_EDGE('',*,*,#46964,.T.);
#62418=ORIENTED_EDGE('',*,*,#46961,.F.);
#62419=ORIENTED_EDGE('',*,*,#46965,.T.);
#62420=ORIENTED_EDGE('',*,*,#46213,.F.);
#62421=ORIENTED_EDGE('',*,*,#46966,.T.);
#62422=ORIENTED_EDGE('',*,*,#46952,.F.);
#62423=ORIENTED_EDGE('',*,*,#46967,.T.);
#62424=ORIENTED_EDGE('',*,*,#46954,.F.);
#62425=ORIENTED_EDGE('',*,*,#46968,.T.);
#62426=ORIENTED_EDGE('',*,*,#46948,.F.);
#62427=ORIENTED_EDGE('',*,*,#46969,.T.);
#62428=ORIENTED_EDGE('',*,*,#46950,.F.);
#62429=ORIENTED_EDGE('',*,*,#46970,.T.);
#62430=ORIENTED_EDGE('',*,*,#46971,.T.);
#62431=ORIENTED_EDGE('',*,*,#46972,.T.);
#62432=ORIENTED_EDGE('',*,*,#46973,.F.);
#62433=ORIENTED_EDGE('',*,*,#46974,.F.);
#62434=ORIENTED_EDGE('',*,*,#46975,.F.);
#62435=ORIENTED_EDGE('',*,*,#46976,.T.);
#62436=ORIENTED_EDGE('',*,*,#46974,.T.);
#62437=ORIENTED_EDGE('',*,*,#46977,.T.);
#62438=ORIENTED_EDGE('',*,*,#46978,.T.);
#62439=ORIENTED_EDGE('',*,*,#46979,.T.);
#62440=ORIENTED_EDGE('',*,*,#46980,.T.);
#62441=ORIENTED_EDGE('',*,*,#46981,.T.);
#62442=ORIENTED_EDGE('',*,*,#46982,.T.);
#62443=ORIENTED_EDGE('',*,*,#46983,.T.);
#62444=ORIENTED_EDGE('',*,*,#46984,.T.);
#62445=ORIENTED_EDGE('',*,*,#46985,.T.);
#62446=ORIENTED_EDGE('',*,*,#46986,.F.);
#62447=ORIENTED_EDGE('',*,*,#46987,.F.);
#62448=ORIENTED_EDGE('',*,*,#46988,.F.);
#62449=ORIENTED_EDGE('',*,*,#46989,.T.);
#62450=ORIENTED_EDGE('',*,*,#46987,.T.);
#62451=ORIENTED_EDGE('',*,*,#46990,.T.);
#62452=ORIENTED_EDGE('',*,*,#46991,.T.);
#62453=ORIENTED_EDGE('',*,*,#46992,.T.);
#62454=ORIENTED_EDGE('',*,*,#46526,.F.);
#62455=ORIENTED_EDGE('',*,*,#46993,.T.);
#62456=ORIENTED_EDGE('',*,*,#46971,.F.);
#62457=ORIENTED_EDGE('',*,*,#46994,.T.);
#62458=ORIENTED_EDGE('',*,*,#46991,.F.);
#62459=ORIENTED_EDGE('',*,*,#46995,.T.);
#62460=ORIENTED_EDGE('',*,*,#46207,.F.);
#62461=ORIENTED_EDGE('',*,*,#46996,.T.);
#62462=ORIENTED_EDGE('',*,*,#46982,.F.);
#62463=ORIENTED_EDGE('',*,*,#46997,.T.);
#62464=ORIENTED_EDGE('',*,*,#46984,.F.);
#62465=ORIENTED_EDGE('',*,*,#46998,.T.);
#62466=ORIENTED_EDGE('',*,*,#46978,.F.);
#62467=ORIENTED_EDGE('',*,*,#46999,.T.);
#62468=ORIENTED_EDGE('',*,*,#46980,.F.);
#62469=ORIENTED_EDGE('',*,*,#47000,.T.);
#62470=ORIENTED_EDGE('',*,*,#47001,.T.);
#62471=ORIENTED_EDGE('',*,*,#47002,.T.);
#62472=ORIENTED_EDGE('',*,*,#47003,.F.);
#62473=ORIENTED_EDGE('',*,*,#47004,.F.);
#62474=ORIENTED_EDGE('',*,*,#47005,.F.);
#62475=ORIENTED_EDGE('',*,*,#47006,.T.);
#62476=ORIENTED_EDGE('',*,*,#47004,.T.);
#62477=ORIENTED_EDGE('',*,*,#47007,.T.);
#62478=ORIENTED_EDGE('',*,*,#47008,.T.);
#62479=ORIENTED_EDGE('',*,*,#47009,.T.);
#62480=ORIENTED_EDGE('',*,*,#47010,.T.);
#62481=ORIENTED_EDGE('',*,*,#47011,.T.);
#62482=ORIENTED_EDGE('',*,*,#47012,.T.);
#62483=ORIENTED_EDGE('',*,*,#47013,.T.);
#62484=ORIENTED_EDGE('',*,*,#47014,.T.);
#62485=ORIENTED_EDGE('',*,*,#47015,.T.);
#62486=ORIENTED_EDGE('',*,*,#47016,.F.);
#62487=ORIENTED_EDGE('',*,*,#47017,.F.);
#62488=ORIENTED_EDGE('',*,*,#47018,.F.);
#62489=ORIENTED_EDGE('',*,*,#47019,.T.);
#62490=ORIENTED_EDGE('',*,*,#47017,.T.);
#62491=ORIENTED_EDGE('',*,*,#47020,.T.);
#62492=ORIENTED_EDGE('',*,*,#47021,.T.);
#62493=ORIENTED_EDGE('',*,*,#47022,.T.);
#62494=ORIENTED_EDGE('',*,*,#46532,.F.);
#62495=ORIENTED_EDGE('',*,*,#47023,.T.);
#62496=ORIENTED_EDGE('',*,*,#47001,.F.);
#62497=ORIENTED_EDGE('',*,*,#47024,.T.);
#62498=ORIENTED_EDGE('',*,*,#47021,.F.);
#62499=ORIENTED_EDGE('',*,*,#47025,.T.);
#62500=ORIENTED_EDGE('',*,*,#46201,.F.);
#62501=ORIENTED_EDGE('',*,*,#47026,.T.);
#62502=ORIENTED_EDGE('',*,*,#47012,.F.);
#62503=ORIENTED_EDGE('',*,*,#47027,.T.);
#62504=ORIENTED_EDGE('',*,*,#47014,.F.);
#62505=ORIENTED_EDGE('',*,*,#47028,.T.);
#62506=ORIENTED_EDGE('',*,*,#47008,.F.);
#62507=ORIENTED_EDGE('',*,*,#47029,.T.);
#62508=ORIENTED_EDGE('',*,*,#47010,.F.);
#62509=ORIENTED_EDGE('',*,*,#47030,.T.);
#62510=ORIENTED_EDGE('',*,*,#47031,.T.);
#62511=ORIENTED_EDGE('',*,*,#47032,.T.);
#62512=ORIENTED_EDGE('',*,*,#47033,.F.);
#62513=ORIENTED_EDGE('',*,*,#47034,.F.);
#62514=ORIENTED_EDGE('',*,*,#47035,.F.);
#62515=ORIENTED_EDGE('',*,*,#47036,.T.);
#62516=ORIENTED_EDGE('',*,*,#47034,.T.);
#62517=ORIENTED_EDGE('',*,*,#47037,.T.);
#62518=ORIENTED_EDGE('',*,*,#47038,.T.);
#62519=ORIENTED_EDGE('',*,*,#47039,.T.);
#62520=ORIENTED_EDGE('',*,*,#47040,.T.);
#62521=ORIENTED_EDGE('',*,*,#47041,.T.);
#62522=ORIENTED_EDGE('',*,*,#47042,.T.);
#62523=ORIENTED_EDGE('',*,*,#47043,.T.);
#62524=ORIENTED_EDGE('',*,*,#47044,.T.);
#62525=ORIENTED_EDGE('',*,*,#47045,.T.);
#62526=ORIENTED_EDGE('',*,*,#47046,.F.);
#62527=ORIENTED_EDGE('',*,*,#47047,.F.);
#62528=ORIENTED_EDGE('',*,*,#47048,.F.);
#62529=ORIENTED_EDGE('',*,*,#47049,.T.);
#62530=ORIENTED_EDGE('',*,*,#47047,.T.);
#62531=ORIENTED_EDGE('',*,*,#47050,.T.);
#62532=ORIENTED_EDGE('',*,*,#47051,.T.);
#62533=ORIENTED_EDGE('',*,*,#47052,.T.);
#62534=ORIENTED_EDGE('',*,*,#46538,.F.);
#62535=ORIENTED_EDGE('',*,*,#47053,.T.);
#62536=ORIENTED_EDGE('',*,*,#47031,.F.);
#62537=ORIENTED_EDGE('',*,*,#47054,.T.);
#62538=ORIENTED_EDGE('',*,*,#47051,.F.);
#62539=ORIENTED_EDGE('',*,*,#47055,.T.);
#62540=ORIENTED_EDGE('',*,*,#46195,.F.);
#62541=ORIENTED_EDGE('',*,*,#47056,.T.);
#62542=ORIENTED_EDGE('',*,*,#47042,.F.);
#62543=ORIENTED_EDGE('',*,*,#47057,.T.);
#62544=ORIENTED_EDGE('',*,*,#47044,.F.);
#62545=ORIENTED_EDGE('',*,*,#47058,.T.);
#62546=ORIENTED_EDGE('',*,*,#47038,.F.);
#62547=ORIENTED_EDGE('',*,*,#47059,.T.);
#62548=ORIENTED_EDGE('',*,*,#47040,.F.);
#62549=ORIENTED_EDGE('',*,*,#47060,.T.);
#62550=ORIENTED_EDGE('',*,*,#47061,.T.);
#62551=ORIENTED_EDGE('',*,*,#47062,.T.);
#62552=ORIENTED_EDGE('',*,*,#47063,.F.);
#62553=ORIENTED_EDGE('',*,*,#47064,.F.);
#62554=ORIENTED_EDGE('',*,*,#47065,.F.);
#62555=ORIENTED_EDGE('',*,*,#47066,.T.);
#62556=ORIENTED_EDGE('',*,*,#47064,.T.);
#62557=ORIENTED_EDGE('',*,*,#47067,.T.);
#62558=ORIENTED_EDGE('',*,*,#47068,.T.);
#62559=ORIENTED_EDGE('',*,*,#47069,.T.);
#62560=ORIENTED_EDGE('',*,*,#47070,.T.);
#62561=ORIENTED_EDGE('',*,*,#47071,.T.);
#62562=ORIENTED_EDGE('',*,*,#47072,.T.);
#62563=ORIENTED_EDGE('',*,*,#47073,.T.);
#62564=ORIENTED_EDGE('',*,*,#47074,.T.);
#62565=ORIENTED_EDGE('',*,*,#47075,.T.);
#62566=ORIENTED_EDGE('',*,*,#47076,.F.);
#62567=ORIENTED_EDGE('',*,*,#47077,.F.);
#62568=ORIENTED_EDGE('',*,*,#47078,.F.);
#62569=ORIENTED_EDGE('',*,*,#47079,.T.);
#62570=ORIENTED_EDGE('',*,*,#47077,.T.);
#62571=ORIENTED_EDGE('',*,*,#47080,.T.);
#62572=ORIENTED_EDGE('',*,*,#47081,.T.);
#62573=ORIENTED_EDGE('',*,*,#47082,.T.);
#62574=ORIENTED_EDGE('',*,*,#46544,.F.);
#62575=ORIENTED_EDGE('',*,*,#47083,.T.);
#62576=ORIENTED_EDGE('',*,*,#47061,.F.);
#62577=ORIENTED_EDGE('',*,*,#47084,.T.);
#62578=ORIENTED_EDGE('',*,*,#47081,.F.);
#62579=ORIENTED_EDGE('',*,*,#47085,.T.);
#62580=ORIENTED_EDGE('',*,*,#46189,.F.);
#62581=ORIENTED_EDGE('',*,*,#47086,.T.);
#62582=ORIENTED_EDGE('',*,*,#47072,.F.);
#62583=ORIENTED_EDGE('',*,*,#47087,.T.);
#62584=ORIENTED_EDGE('',*,*,#47074,.F.);
#62585=ORIENTED_EDGE('',*,*,#47088,.T.);
#62586=ORIENTED_EDGE('',*,*,#47068,.F.);
#62587=ORIENTED_EDGE('',*,*,#47089,.T.);
#62588=ORIENTED_EDGE('',*,*,#47070,.F.);
#62589=ORIENTED_EDGE('',*,*,#47090,.T.);
#62590=ORIENTED_EDGE('',*,*,#47091,.T.);
#62591=ORIENTED_EDGE('',*,*,#47092,.T.);
#62592=ORIENTED_EDGE('',*,*,#47093,.F.);
#62593=ORIENTED_EDGE('',*,*,#47094,.F.);
#62594=ORIENTED_EDGE('',*,*,#47095,.F.);
#62595=ORIENTED_EDGE('',*,*,#47096,.T.);
#62596=ORIENTED_EDGE('',*,*,#47094,.T.);
#62597=ORIENTED_EDGE('',*,*,#47097,.T.);
#62598=ORIENTED_EDGE('',*,*,#47098,.T.);
#62599=ORIENTED_EDGE('',*,*,#47099,.T.);
#62600=ORIENTED_EDGE('',*,*,#47100,.T.);
#62601=ORIENTED_EDGE('',*,*,#47101,.T.);
#62602=ORIENTED_EDGE('',*,*,#47102,.T.);
#62603=ORIENTED_EDGE('',*,*,#47103,.T.);
#62604=ORIENTED_EDGE('',*,*,#47104,.T.);
#62605=ORIENTED_EDGE('',*,*,#47105,.T.);
#62606=ORIENTED_EDGE('',*,*,#47106,.F.);
#62607=ORIENTED_EDGE('',*,*,#47107,.F.);
#62608=ORIENTED_EDGE('',*,*,#47108,.F.);
#62609=ORIENTED_EDGE('',*,*,#47109,.T.);
#62610=ORIENTED_EDGE('',*,*,#47107,.T.);
#62611=ORIENTED_EDGE('',*,*,#47110,.T.);
#62612=ORIENTED_EDGE('',*,*,#47111,.T.);
#62613=ORIENTED_EDGE('',*,*,#47112,.T.);
#62614=ORIENTED_EDGE('',*,*,#46549,.F.);
#62615=ORIENTED_EDGE('',*,*,#47113,.T.);
#62616=ORIENTED_EDGE('',*,*,#47091,.F.);
#62617=ORIENTED_EDGE('',*,*,#47114,.T.);
#62618=ORIENTED_EDGE('',*,*,#47111,.F.);
#62619=ORIENTED_EDGE('',*,*,#47115,.T.);
#62620=ORIENTED_EDGE('',*,*,#46184,.F.);
#62621=ORIENTED_EDGE('',*,*,#47116,.T.);
#62622=ORIENTED_EDGE('',*,*,#47102,.F.);
#62623=ORIENTED_EDGE('',*,*,#47117,.T.);
#62624=ORIENTED_EDGE('',*,*,#47104,.F.);
#62625=ORIENTED_EDGE('',*,*,#47118,.T.);
#62626=ORIENTED_EDGE('',*,*,#47098,.F.);
#62627=ORIENTED_EDGE('',*,*,#47119,.T.);
#62628=ORIENTED_EDGE('',*,*,#47100,.F.);
#62629=ORIENTED_EDGE('',*,*,#47120,.T.);
#62630=ORIENTED_EDGE('',*,*,#47121,.T.);
#62631=ORIENTED_EDGE('',*,*,#47122,.T.);
#62632=ORIENTED_EDGE('',*,*,#47123,.F.);
#62633=ORIENTED_EDGE('',*,*,#47124,.F.);
#62634=ORIENTED_EDGE('',*,*,#47125,.F.);
#62635=ORIENTED_EDGE('',*,*,#47126,.T.);
#62636=ORIENTED_EDGE('',*,*,#47124,.T.);
#62637=ORIENTED_EDGE('',*,*,#47127,.T.);
#62638=ORIENTED_EDGE('',*,*,#47128,.T.);
#62639=ORIENTED_EDGE('',*,*,#47129,.T.);
#62640=ORIENTED_EDGE('',*,*,#47130,.T.);
#62641=ORIENTED_EDGE('',*,*,#47131,.T.);
#62642=ORIENTED_EDGE('',*,*,#47132,.T.);
#62643=ORIENTED_EDGE('',*,*,#47133,.T.);
#62644=ORIENTED_EDGE('',*,*,#47134,.T.);
#62645=ORIENTED_EDGE('',*,*,#47135,.T.);
#62646=ORIENTED_EDGE('',*,*,#47136,.F.);
#62647=ORIENTED_EDGE('',*,*,#47137,.F.);
#62648=ORIENTED_EDGE('',*,*,#47138,.F.);
#62649=ORIENTED_EDGE('',*,*,#47139,.T.);
#62650=ORIENTED_EDGE('',*,*,#47137,.T.);
#62651=ORIENTED_EDGE('',*,*,#47140,.T.);
#62652=ORIENTED_EDGE('',*,*,#47141,.T.);
#62653=ORIENTED_EDGE('',*,*,#47142,.T.);
#62654=ORIENTED_EDGE('',*,*,#46555,.F.);
#62655=ORIENTED_EDGE('',*,*,#47143,.T.);
#62656=ORIENTED_EDGE('',*,*,#47121,.F.);
#62657=ORIENTED_EDGE('',*,*,#47144,.T.);
#62658=ORIENTED_EDGE('',*,*,#47141,.F.);
#62659=ORIENTED_EDGE('',*,*,#47145,.T.);
#62660=ORIENTED_EDGE('',*,*,#46178,.F.);
#62661=ORIENTED_EDGE('',*,*,#47146,.T.);
#62662=ORIENTED_EDGE('',*,*,#47132,.F.);
#62663=ORIENTED_EDGE('',*,*,#47147,.T.);
#62664=ORIENTED_EDGE('',*,*,#47134,.F.);
#62665=ORIENTED_EDGE('',*,*,#47148,.T.);
#62666=ORIENTED_EDGE('',*,*,#47128,.F.);
#62667=ORIENTED_EDGE('',*,*,#47149,.T.);
#62668=ORIENTED_EDGE('',*,*,#47130,.F.);
#62669=ORIENTED_EDGE('',*,*,#47150,.T.);
#62670=ORIENTED_EDGE('',*,*,#47151,.T.);
#62671=ORIENTED_EDGE('',*,*,#47152,.T.);
#62672=ORIENTED_EDGE('',*,*,#47153,.F.);
#62673=ORIENTED_EDGE('',*,*,#47154,.F.);
#62674=ORIENTED_EDGE('',*,*,#47155,.F.);
#62675=ORIENTED_EDGE('',*,*,#47156,.T.);
#62676=ORIENTED_EDGE('',*,*,#47154,.T.);
#62677=ORIENTED_EDGE('',*,*,#47157,.T.);
#62678=ORIENTED_EDGE('',*,*,#47158,.T.);
#62679=ORIENTED_EDGE('',*,*,#47159,.T.);
#62680=ORIENTED_EDGE('',*,*,#47160,.T.);
#62681=ORIENTED_EDGE('',*,*,#47161,.T.);
#62682=ORIENTED_EDGE('',*,*,#47162,.T.);
#62683=ORIENTED_EDGE('',*,*,#47163,.T.);
#62684=ORIENTED_EDGE('',*,*,#47164,.T.);
#62685=ORIENTED_EDGE('',*,*,#47165,.T.);
#62686=ORIENTED_EDGE('',*,*,#47166,.F.);
#62687=ORIENTED_EDGE('',*,*,#47167,.F.);
#62688=ORIENTED_EDGE('',*,*,#47168,.F.);
#62689=ORIENTED_EDGE('',*,*,#47169,.T.);
#62690=ORIENTED_EDGE('',*,*,#47167,.T.);
#62691=ORIENTED_EDGE('',*,*,#47170,.T.);
#62692=ORIENTED_EDGE('',*,*,#47171,.T.);
#62693=ORIENTED_EDGE('',*,*,#47172,.T.);
#62694=ORIENTED_EDGE('',*,*,#46561,.F.);
#62695=ORIENTED_EDGE('',*,*,#47173,.T.);
#62696=ORIENTED_EDGE('',*,*,#47151,.F.);
#62697=ORIENTED_EDGE('',*,*,#47174,.T.);
#62698=ORIENTED_EDGE('',*,*,#47171,.F.);
#62699=ORIENTED_EDGE('',*,*,#47175,.T.);
#62700=ORIENTED_EDGE('',*,*,#46172,.F.);
#62701=ORIENTED_EDGE('',*,*,#47176,.T.);
#62702=ORIENTED_EDGE('',*,*,#47162,.F.);
#62703=ORIENTED_EDGE('',*,*,#47177,.T.);
#62704=ORIENTED_EDGE('',*,*,#47164,.F.);
#62705=ORIENTED_EDGE('',*,*,#47178,.T.);
#62706=ORIENTED_EDGE('',*,*,#47158,.F.);
#62707=ORIENTED_EDGE('',*,*,#47179,.T.);
#62708=ORIENTED_EDGE('',*,*,#47160,.F.);
#62709=ORIENTED_EDGE('',*,*,#47180,.T.);
#62710=ORIENTED_EDGE('',*,*,#47181,.T.);
#62711=ORIENTED_EDGE('',*,*,#47182,.T.);
#62712=ORIENTED_EDGE('',*,*,#47183,.F.);
#62713=ORIENTED_EDGE('',*,*,#47184,.F.);
#62714=ORIENTED_EDGE('',*,*,#47185,.F.);
#62715=ORIENTED_EDGE('',*,*,#47186,.T.);
#62716=ORIENTED_EDGE('',*,*,#47184,.T.);
#62717=ORIENTED_EDGE('',*,*,#47187,.T.);
#62718=ORIENTED_EDGE('',*,*,#47188,.T.);
#62719=ORIENTED_EDGE('',*,*,#47189,.T.);
#62720=ORIENTED_EDGE('',*,*,#47190,.T.);
#62721=ORIENTED_EDGE('',*,*,#47191,.T.);
#62722=ORIENTED_EDGE('',*,*,#47192,.T.);
#62723=ORIENTED_EDGE('',*,*,#47193,.T.);
#62724=ORIENTED_EDGE('',*,*,#47194,.T.);
#62725=ORIENTED_EDGE('',*,*,#47195,.T.);
#62726=ORIENTED_EDGE('',*,*,#47196,.F.);
#62727=ORIENTED_EDGE('',*,*,#47197,.F.);
#62728=ORIENTED_EDGE('',*,*,#47198,.F.);
#62729=ORIENTED_EDGE('',*,*,#47199,.T.);
#62730=ORIENTED_EDGE('',*,*,#47197,.T.);
#62731=ORIENTED_EDGE('',*,*,#47200,.T.);
#62732=ORIENTED_EDGE('',*,*,#47201,.T.);
#62733=ORIENTED_EDGE('',*,*,#47202,.T.);
#62734=ORIENTED_EDGE('',*,*,#46567,.F.);
#62735=ORIENTED_EDGE('',*,*,#47203,.T.);
#62736=ORIENTED_EDGE('',*,*,#47181,.F.);
#62737=ORIENTED_EDGE('',*,*,#47204,.T.);
#62738=ORIENTED_EDGE('',*,*,#47201,.F.);
#62739=ORIENTED_EDGE('',*,*,#47205,.T.);
#62740=ORIENTED_EDGE('',*,*,#46166,.F.);
#62741=ORIENTED_EDGE('',*,*,#47206,.T.);
#62742=ORIENTED_EDGE('',*,*,#47192,.F.);
#62743=ORIENTED_EDGE('',*,*,#47207,.T.);
#62744=ORIENTED_EDGE('',*,*,#47194,.F.);
#62745=ORIENTED_EDGE('',*,*,#47208,.T.);
#62746=ORIENTED_EDGE('',*,*,#47188,.F.);
#62747=ORIENTED_EDGE('',*,*,#47209,.T.);
#62748=ORIENTED_EDGE('',*,*,#47190,.F.);
#62749=ORIENTED_EDGE('',*,*,#47210,.T.);
#62750=ORIENTED_EDGE('',*,*,#47211,.T.);
#62751=ORIENTED_EDGE('',*,*,#47212,.T.);
#62752=ORIENTED_EDGE('',*,*,#47213,.F.);
#62753=ORIENTED_EDGE('',*,*,#47214,.F.);
#62754=ORIENTED_EDGE('',*,*,#47215,.F.);
#62755=ORIENTED_EDGE('',*,*,#47216,.T.);
#62756=ORIENTED_EDGE('',*,*,#47214,.T.);
#62757=ORIENTED_EDGE('',*,*,#47217,.T.);
#62758=ORIENTED_EDGE('',*,*,#47218,.T.);
#62759=ORIENTED_EDGE('',*,*,#47219,.T.);
#62760=ORIENTED_EDGE('',*,*,#47220,.T.);
#62761=ORIENTED_EDGE('',*,*,#47221,.T.);
#62762=ORIENTED_EDGE('',*,*,#47222,.T.);
#62763=ORIENTED_EDGE('',*,*,#47223,.T.);
#62764=ORIENTED_EDGE('',*,*,#47224,.T.);
#62765=ORIENTED_EDGE('',*,*,#47225,.T.);
#62766=ORIENTED_EDGE('',*,*,#47226,.F.);
#62767=ORIENTED_EDGE('',*,*,#47227,.F.);
#62768=ORIENTED_EDGE('',*,*,#47228,.F.);
#62769=ORIENTED_EDGE('',*,*,#47229,.T.);
#62770=ORIENTED_EDGE('',*,*,#47227,.T.);
#62771=ORIENTED_EDGE('',*,*,#47230,.T.);
#62772=ORIENTED_EDGE('',*,*,#47231,.T.);
#62773=ORIENTED_EDGE('',*,*,#47232,.T.);
#62774=ORIENTED_EDGE('',*,*,#46573,.F.);
#62775=ORIENTED_EDGE('',*,*,#47233,.T.);
#62776=ORIENTED_EDGE('',*,*,#47211,.F.);
#62777=ORIENTED_EDGE('',*,*,#47234,.T.);
#62778=ORIENTED_EDGE('',*,*,#47231,.F.);
#62779=ORIENTED_EDGE('',*,*,#47235,.T.);
#62780=ORIENTED_EDGE('',*,*,#46160,.F.);
#62781=ORIENTED_EDGE('',*,*,#47236,.T.);
#62782=ORIENTED_EDGE('',*,*,#47222,.F.);
#62783=ORIENTED_EDGE('',*,*,#47237,.T.);
#62784=ORIENTED_EDGE('',*,*,#47224,.F.);
#62785=ORIENTED_EDGE('',*,*,#47238,.T.);
#62786=ORIENTED_EDGE('',*,*,#47218,.F.);
#62787=ORIENTED_EDGE('',*,*,#47239,.T.);
#62788=ORIENTED_EDGE('',*,*,#47220,.F.);
#62789=ORIENTED_EDGE('',*,*,#47240,.T.);
#62790=ORIENTED_EDGE('',*,*,#47241,.T.);
#62791=ORIENTED_EDGE('',*,*,#47242,.T.);
#62792=ORIENTED_EDGE('',*,*,#47243,.F.);
#62793=ORIENTED_EDGE('',*,*,#47244,.F.);
#62794=ORIENTED_EDGE('',*,*,#47245,.F.);
#62795=ORIENTED_EDGE('',*,*,#47246,.T.);
#62796=ORIENTED_EDGE('',*,*,#47244,.T.);
#62797=ORIENTED_EDGE('',*,*,#47247,.T.);
#62798=ORIENTED_EDGE('',*,*,#47248,.T.);
#62799=ORIENTED_EDGE('',*,*,#47249,.T.);
#62800=ORIENTED_EDGE('',*,*,#47250,.T.);
#62801=ORIENTED_EDGE('',*,*,#47251,.T.);
#62802=ORIENTED_EDGE('',*,*,#47252,.T.);
#62803=ORIENTED_EDGE('',*,*,#47253,.T.);
#62804=ORIENTED_EDGE('',*,*,#47254,.T.);
#62805=ORIENTED_EDGE('',*,*,#47255,.T.);
#62806=ORIENTED_EDGE('',*,*,#47256,.F.);
#62807=ORIENTED_EDGE('',*,*,#47257,.F.);
#62808=ORIENTED_EDGE('',*,*,#47258,.F.);
#62809=ORIENTED_EDGE('',*,*,#47259,.T.);
#62810=ORIENTED_EDGE('',*,*,#47257,.T.);
#62811=ORIENTED_EDGE('',*,*,#47260,.T.);
#62812=ORIENTED_EDGE('',*,*,#47261,.T.);
#62813=ORIENTED_EDGE('',*,*,#47262,.T.);
#62814=ORIENTED_EDGE('',*,*,#46579,.F.);
#62815=ORIENTED_EDGE('',*,*,#47263,.T.);
#62816=ORIENTED_EDGE('',*,*,#47241,.F.);
#62817=ORIENTED_EDGE('',*,*,#47264,.T.);
#62818=ORIENTED_EDGE('',*,*,#47261,.F.);
#62819=ORIENTED_EDGE('',*,*,#47265,.T.);
#62820=ORIENTED_EDGE('',*,*,#46154,.F.);
#62821=ORIENTED_EDGE('',*,*,#47266,.T.);
#62822=ORIENTED_EDGE('',*,*,#47252,.F.);
#62823=ORIENTED_EDGE('',*,*,#47267,.T.);
#62824=ORIENTED_EDGE('',*,*,#47254,.F.);
#62825=ORIENTED_EDGE('',*,*,#47268,.T.);
#62826=ORIENTED_EDGE('',*,*,#47248,.F.);
#62827=ORIENTED_EDGE('',*,*,#47269,.T.);
#62828=ORIENTED_EDGE('',*,*,#47250,.F.);
#62829=ORIENTED_EDGE('',*,*,#47270,.T.);
#62830=ORIENTED_EDGE('',*,*,#47271,.T.);
#62831=ORIENTED_EDGE('',*,*,#47272,.T.);
#62832=ORIENTED_EDGE('',*,*,#47273,.F.);
#62833=ORIENTED_EDGE('',*,*,#47274,.F.);
#62834=ORIENTED_EDGE('',*,*,#47275,.F.);
#62835=ORIENTED_EDGE('',*,*,#47276,.T.);
#62836=ORIENTED_EDGE('',*,*,#47274,.T.);
#62837=ORIENTED_EDGE('',*,*,#47277,.T.);
#62838=ORIENTED_EDGE('',*,*,#47278,.T.);
#62839=ORIENTED_EDGE('',*,*,#47279,.T.);
#62840=ORIENTED_EDGE('',*,*,#47280,.T.);
#62841=ORIENTED_EDGE('',*,*,#47281,.T.);
#62842=ORIENTED_EDGE('',*,*,#47282,.T.);
#62843=ORIENTED_EDGE('',*,*,#47283,.T.);
#62844=ORIENTED_EDGE('',*,*,#47284,.T.);
#62845=ORIENTED_EDGE('',*,*,#47285,.T.);
#62846=ORIENTED_EDGE('',*,*,#47286,.F.);
#62847=ORIENTED_EDGE('',*,*,#47287,.F.);
#62848=ORIENTED_EDGE('',*,*,#47288,.F.);
#62849=ORIENTED_EDGE('',*,*,#47289,.T.);
#62850=ORIENTED_EDGE('',*,*,#47287,.T.);
#62851=ORIENTED_EDGE('',*,*,#47290,.T.);
#62852=ORIENTED_EDGE('',*,*,#47291,.T.);
#62853=ORIENTED_EDGE('',*,*,#47292,.T.);
#62854=ORIENTED_EDGE('',*,*,#46585,.F.);
#62855=ORIENTED_EDGE('',*,*,#47293,.T.);
#62856=ORIENTED_EDGE('',*,*,#47271,.F.);
#62857=ORIENTED_EDGE('',*,*,#47294,.T.);
#62858=ORIENTED_EDGE('',*,*,#47291,.F.);
#62859=ORIENTED_EDGE('',*,*,#47295,.T.);
#62860=ORIENTED_EDGE('',*,*,#46148,.F.);
#62861=ORIENTED_EDGE('',*,*,#47296,.T.);
#62862=ORIENTED_EDGE('',*,*,#47282,.F.);
#62863=ORIENTED_EDGE('',*,*,#47297,.T.);
#62864=ORIENTED_EDGE('',*,*,#47284,.F.);
#62865=ORIENTED_EDGE('',*,*,#47298,.T.);
#62866=ORIENTED_EDGE('',*,*,#47278,.F.);
#62867=ORIENTED_EDGE('',*,*,#47299,.T.);
#62868=ORIENTED_EDGE('',*,*,#47280,.F.);
#62869=ORIENTED_EDGE('',*,*,#47300,.T.);
#62870=ORIENTED_EDGE('',*,*,#47301,.T.);
#62871=ORIENTED_EDGE('',*,*,#47302,.T.);
#62872=ORIENTED_EDGE('',*,*,#47303,.F.);
#62873=ORIENTED_EDGE('',*,*,#47304,.F.);
#62874=ORIENTED_EDGE('',*,*,#47305,.F.);
#62875=ORIENTED_EDGE('',*,*,#47306,.T.);
#62876=ORIENTED_EDGE('',*,*,#47304,.T.);
#62877=ORIENTED_EDGE('',*,*,#47307,.T.);
#62878=ORIENTED_EDGE('',*,*,#47308,.T.);
#62879=ORIENTED_EDGE('',*,*,#47309,.T.);
#62880=ORIENTED_EDGE('',*,*,#47310,.T.);
#62881=ORIENTED_EDGE('',*,*,#47311,.T.);
#62882=ORIENTED_EDGE('',*,*,#47312,.T.);
#62883=ORIENTED_EDGE('',*,*,#47313,.T.);
#62884=ORIENTED_EDGE('',*,*,#47314,.T.);
#62885=ORIENTED_EDGE('',*,*,#47315,.T.);
#62886=ORIENTED_EDGE('',*,*,#47316,.F.);
#62887=ORIENTED_EDGE('',*,*,#47317,.F.);
#62888=ORIENTED_EDGE('',*,*,#47318,.F.);
#62889=ORIENTED_EDGE('',*,*,#47319,.T.);
#62890=ORIENTED_EDGE('',*,*,#47317,.T.);
#62891=ORIENTED_EDGE('',*,*,#47320,.T.);
#62892=ORIENTED_EDGE('',*,*,#47321,.T.);
#62893=ORIENTED_EDGE('',*,*,#47322,.T.);
#62894=ORIENTED_EDGE('',*,*,#46591,.F.);
#62895=ORIENTED_EDGE('',*,*,#47323,.T.);
#62896=ORIENTED_EDGE('',*,*,#47301,.F.);
#62897=ORIENTED_EDGE('',*,*,#47324,.T.);
#62898=ORIENTED_EDGE('',*,*,#47321,.F.);
#62899=ORIENTED_EDGE('',*,*,#47325,.T.);
#62900=ORIENTED_EDGE('',*,*,#46142,.F.);
#62901=ORIENTED_EDGE('',*,*,#47326,.T.);
#62902=ORIENTED_EDGE('',*,*,#47312,.F.);
#62903=ORIENTED_EDGE('',*,*,#47327,.T.);
#62904=ORIENTED_EDGE('',*,*,#47314,.F.);
#62905=ORIENTED_EDGE('',*,*,#47328,.T.);
#62906=ORIENTED_EDGE('',*,*,#47308,.F.);
#62907=ORIENTED_EDGE('',*,*,#47329,.T.);
#62908=ORIENTED_EDGE('',*,*,#47310,.F.);
#62909=ORIENTED_EDGE('',*,*,#47330,.T.);
#62910=ORIENTED_EDGE('',*,*,#47331,.T.);
#62911=ORIENTED_EDGE('',*,*,#47332,.T.);
#62912=ORIENTED_EDGE('',*,*,#47333,.F.);
#62913=ORIENTED_EDGE('',*,*,#47334,.F.);
#62914=ORIENTED_EDGE('',*,*,#47335,.F.);
#62915=ORIENTED_EDGE('',*,*,#47336,.T.);
#62916=ORIENTED_EDGE('',*,*,#47334,.T.);
#62917=ORIENTED_EDGE('',*,*,#47337,.T.);
#62918=ORIENTED_EDGE('',*,*,#47338,.T.);
#62919=ORIENTED_EDGE('',*,*,#47339,.T.);
#62920=ORIENTED_EDGE('',*,*,#47340,.T.);
#62921=ORIENTED_EDGE('',*,*,#47341,.T.);
#62922=ORIENTED_EDGE('',*,*,#47342,.T.);
#62923=ORIENTED_EDGE('',*,*,#47343,.T.);
#62924=ORIENTED_EDGE('',*,*,#47344,.T.);
#62925=ORIENTED_EDGE('',*,*,#47345,.T.);
#62926=ORIENTED_EDGE('',*,*,#47346,.F.);
#62927=ORIENTED_EDGE('',*,*,#47347,.F.);
#62928=ORIENTED_EDGE('',*,*,#47348,.F.);
#62929=ORIENTED_EDGE('',*,*,#47349,.T.);
#62930=ORIENTED_EDGE('',*,*,#47347,.T.);
#62931=ORIENTED_EDGE('',*,*,#47350,.T.);
#62932=ORIENTED_EDGE('',*,*,#47351,.T.);
#62933=ORIENTED_EDGE('',*,*,#47352,.T.);
#62934=ORIENTED_EDGE('',*,*,#46597,.F.);
#62935=ORIENTED_EDGE('',*,*,#47353,.T.);
#62936=ORIENTED_EDGE('',*,*,#47331,.F.);
#62937=ORIENTED_EDGE('',*,*,#47354,.T.);
#62938=ORIENTED_EDGE('',*,*,#47351,.F.);
#62939=ORIENTED_EDGE('',*,*,#47355,.T.);
#62940=ORIENTED_EDGE('',*,*,#46136,.F.);
#62941=ORIENTED_EDGE('',*,*,#47356,.T.);
#62942=ORIENTED_EDGE('',*,*,#47342,.F.);
#62943=ORIENTED_EDGE('',*,*,#47357,.T.);
#62944=ORIENTED_EDGE('',*,*,#47344,.F.);
#62945=ORIENTED_EDGE('',*,*,#47358,.T.);
#62946=ORIENTED_EDGE('',*,*,#47338,.F.);
#62947=ORIENTED_EDGE('',*,*,#47359,.T.);
#62948=ORIENTED_EDGE('',*,*,#47340,.F.);
#62949=ORIENTED_EDGE('',*,*,#47360,.T.);
#62950=ORIENTED_EDGE('',*,*,#47361,.T.);
#62951=ORIENTED_EDGE('',*,*,#47362,.T.);
#62952=ORIENTED_EDGE('',*,*,#47363,.F.);
#62953=ORIENTED_EDGE('',*,*,#47364,.F.);
#62954=ORIENTED_EDGE('',*,*,#47365,.F.);
#62955=ORIENTED_EDGE('',*,*,#47366,.T.);
#62956=ORIENTED_EDGE('',*,*,#47364,.T.);
#62957=ORIENTED_EDGE('',*,*,#47367,.T.);
#62958=ORIENTED_EDGE('',*,*,#47368,.T.);
#62959=ORIENTED_EDGE('',*,*,#47369,.T.);
#62960=ORIENTED_EDGE('',*,*,#47370,.T.);
#62961=ORIENTED_EDGE('',*,*,#47371,.T.);
#62962=ORIENTED_EDGE('',*,*,#47372,.T.);
#62963=ORIENTED_EDGE('',*,*,#47373,.T.);
#62964=ORIENTED_EDGE('',*,*,#47374,.T.);
#62965=ORIENTED_EDGE('',*,*,#47375,.T.);
#62966=ORIENTED_EDGE('',*,*,#47376,.F.);
#62967=ORIENTED_EDGE('',*,*,#47377,.F.);
#62968=ORIENTED_EDGE('',*,*,#47378,.F.);
#62969=ORIENTED_EDGE('',*,*,#47379,.T.);
#62970=ORIENTED_EDGE('',*,*,#47377,.T.);
#62971=ORIENTED_EDGE('',*,*,#47380,.T.);
#62972=ORIENTED_EDGE('',*,*,#47381,.T.);
#62973=ORIENTED_EDGE('',*,*,#47382,.T.);
#62974=ORIENTED_EDGE('',*,*,#46603,.F.);
#62975=ORIENTED_EDGE('',*,*,#47383,.T.);
#62976=ORIENTED_EDGE('',*,*,#47361,.F.);
#62977=ORIENTED_EDGE('',*,*,#47384,.T.);
#62978=ORIENTED_EDGE('',*,*,#47381,.F.);
#62979=ORIENTED_EDGE('',*,*,#47385,.T.);
#62980=ORIENTED_EDGE('',*,*,#46130,.F.);
#62981=ORIENTED_EDGE('',*,*,#47386,.T.);
#62982=ORIENTED_EDGE('',*,*,#47372,.F.);
#62983=ORIENTED_EDGE('',*,*,#47387,.T.);
#62984=ORIENTED_EDGE('',*,*,#47374,.F.);
#62985=ORIENTED_EDGE('',*,*,#47388,.T.);
#62986=ORIENTED_EDGE('',*,*,#47368,.F.);
#62987=ORIENTED_EDGE('',*,*,#47389,.T.);
#62988=ORIENTED_EDGE('',*,*,#47370,.F.);
#62989=ORIENTED_EDGE('',*,*,#47390,.T.);
#62990=ORIENTED_EDGE('',*,*,#47391,.T.);
#62991=ORIENTED_EDGE('',*,*,#47392,.T.);
#62992=ORIENTED_EDGE('',*,*,#47393,.F.);
#62993=ORIENTED_EDGE('',*,*,#47394,.F.);
#62994=ORIENTED_EDGE('',*,*,#47395,.F.);
#62995=ORIENTED_EDGE('',*,*,#47396,.T.);
#62996=ORIENTED_EDGE('',*,*,#47394,.T.);
#62997=ORIENTED_EDGE('',*,*,#47397,.T.);
#62998=ORIENTED_EDGE('',*,*,#47398,.T.);
#62999=ORIENTED_EDGE('',*,*,#47399,.T.);
#63000=ORIENTED_EDGE('',*,*,#47400,.T.);
#63001=ORIENTED_EDGE('',*,*,#47401,.T.);
#63002=ORIENTED_EDGE('',*,*,#47402,.T.);
#63003=ORIENTED_EDGE('',*,*,#47403,.T.);
#63004=ORIENTED_EDGE('',*,*,#47404,.T.);
#63005=ORIENTED_EDGE('',*,*,#47405,.T.);
#63006=ORIENTED_EDGE('',*,*,#47406,.F.);
#63007=ORIENTED_EDGE('',*,*,#47407,.F.);
#63008=ORIENTED_EDGE('',*,*,#47408,.F.);
#63009=ORIENTED_EDGE('',*,*,#47409,.T.);
#63010=ORIENTED_EDGE('',*,*,#47407,.T.);
#63011=ORIENTED_EDGE('',*,*,#47410,.T.);
#63012=ORIENTED_EDGE('',*,*,#47411,.T.);
#63013=ORIENTED_EDGE('',*,*,#47412,.T.);
#63014=ORIENTED_EDGE('',*,*,#46609,.F.);
#63015=ORIENTED_EDGE('',*,*,#47413,.T.);
#63016=ORIENTED_EDGE('',*,*,#47391,.F.);
#63017=ORIENTED_EDGE('',*,*,#47414,.T.);
#63018=ORIENTED_EDGE('',*,*,#47411,.F.);
#63019=ORIENTED_EDGE('',*,*,#47415,.T.);
#63020=ORIENTED_EDGE('',*,*,#46124,.F.);
#63021=ORIENTED_EDGE('',*,*,#47416,.T.);
#63022=ORIENTED_EDGE('',*,*,#47402,.F.);
#63023=ORIENTED_EDGE('',*,*,#47417,.T.);
#63024=ORIENTED_EDGE('',*,*,#47404,.F.);
#63025=ORIENTED_EDGE('',*,*,#47418,.T.);
#63026=ORIENTED_EDGE('',*,*,#47398,.F.);
#63027=ORIENTED_EDGE('',*,*,#47419,.T.);
#63028=ORIENTED_EDGE('',*,*,#47400,.F.);
#63029=ORIENTED_EDGE('',*,*,#47420,.T.);
#63030=ORIENTED_EDGE('',*,*,#47421,.T.);
#63031=ORIENTED_EDGE('',*,*,#47422,.T.);
#63032=ORIENTED_EDGE('',*,*,#47423,.F.);
#63033=ORIENTED_EDGE('',*,*,#47424,.F.);
#63034=ORIENTED_EDGE('',*,*,#47425,.F.);
#63035=ORIENTED_EDGE('',*,*,#47426,.T.);
#63036=ORIENTED_EDGE('',*,*,#47424,.T.);
#63037=ORIENTED_EDGE('',*,*,#47427,.T.);
#63038=ORIENTED_EDGE('',*,*,#47428,.T.);
#63039=ORIENTED_EDGE('',*,*,#47429,.T.);
#63040=ORIENTED_EDGE('',*,*,#47430,.T.);
#63041=ORIENTED_EDGE('',*,*,#47431,.T.);
#63042=ORIENTED_EDGE('',*,*,#47432,.T.);
#63043=ORIENTED_EDGE('',*,*,#47433,.T.);
#63044=ORIENTED_EDGE('',*,*,#47434,.T.);
#63045=ORIENTED_EDGE('',*,*,#47435,.T.);
#63046=ORIENTED_EDGE('',*,*,#47436,.F.);
#63047=ORIENTED_EDGE('',*,*,#47437,.F.);
#63048=ORIENTED_EDGE('',*,*,#47438,.F.);
#63049=ORIENTED_EDGE('',*,*,#47439,.T.);
#63050=ORIENTED_EDGE('',*,*,#47437,.T.);
#63051=ORIENTED_EDGE('',*,*,#47440,.T.);
#63052=ORIENTED_EDGE('',*,*,#47441,.T.);
#63053=ORIENTED_EDGE('',*,*,#47442,.T.);
#63054=ORIENTED_EDGE('',*,*,#46615,.F.);
#63055=ORIENTED_EDGE('',*,*,#47443,.T.);
#63056=ORIENTED_EDGE('',*,*,#47421,.F.);
#63057=ORIENTED_EDGE('',*,*,#47444,.T.);
#63058=ORIENTED_EDGE('',*,*,#47441,.F.);
#63059=ORIENTED_EDGE('',*,*,#47445,.T.);
#63060=ORIENTED_EDGE('',*,*,#46118,.F.);
#63061=ORIENTED_EDGE('',*,*,#47446,.T.);
#63062=ORIENTED_EDGE('',*,*,#47432,.F.);
#63063=ORIENTED_EDGE('',*,*,#47447,.T.);
#63064=ORIENTED_EDGE('',*,*,#47434,.F.);
#63065=ORIENTED_EDGE('',*,*,#47448,.T.);
#63066=ORIENTED_EDGE('',*,*,#47428,.F.);
#63067=ORIENTED_EDGE('',*,*,#47449,.T.);
#63068=ORIENTED_EDGE('',*,*,#47430,.F.);
#63069=ORIENTED_EDGE('',*,*,#47450,.T.);
#63070=ORIENTED_EDGE('',*,*,#47451,.T.);
#63071=ORIENTED_EDGE('',*,*,#47452,.T.);
#63072=ORIENTED_EDGE('',*,*,#47453,.F.);
#63073=ORIENTED_EDGE('',*,*,#47454,.F.);
#63074=ORIENTED_EDGE('',*,*,#47455,.F.);
#63075=ORIENTED_EDGE('',*,*,#47456,.T.);
#63076=ORIENTED_EDGE('',*,*,#47454,.T.);
#63077=ORIENTED_EDGE('',*,*,#47457,.T.);
#63078=ORIENTED_EDGE('',*,*,#47458,.T.);
#63079=ORIENTED_EDGE('',*,*,#47459,.T.);
#63080=ORIENTED_EDGE('',*,*,#47460,.T.);
#63081=ORIENTED_EDGE('',*,*,#47461,.T.);
#63082=ORIENTED_EDGE('',*,*,#47462,.T.);
#63083=ORIENTED_EDGE('',*,*,#47463,.T.);
#63084=ORIENTED_EDGE('',*,*,#47464,.T.);
#63085=ORIENTED_EDGE('',*,*,#47465,.T.);
#63086=ORIENTED_EDGE('',*,*,#47466,.F.);
#63087=ORIENTED_EDGE('',*,*,#47467,.F.);
#63088=ORIENTED_EDGE('',*,*,#47468,.F.);
#63089=ORIENTED_EDGE('',*,*,#47469,.T.);
#63090=ORIENTED_EDGE('',*,*,#47467,.T.);
#63091=ORIENTED_EDGE('',*,*,#47470,.T.);
#63092=ORIENTED_EDGE('',*,*,#47471,.T.);
#63093=ORIENTED_EDGE('',*,*,#47472,.T.);
#63094=ORIENTED_EDGE('',*,*,#46621,.F.);
#63095=ORIENTED_EDGE('',*,*,#47473,.T.);
#63096=ORIENTED_EDGE('',*,*,#47451,.F.);
#63097=ORIENTED_EDGE('',*,*,#47474,.T.);
#63098=ORIENTED_EDGE('',*,*,#47471,.F.);
#63099=ORIENTED_EDGE('',*,*,#47475,.T.);
#63100=ORIENTED_EDGE('',*,*,#46112,.F.);
#63101=ORIENTED_EDGE('',*,*,#47476,.T.);
#63102=ORIENTED_EDGE('',*,*,#47462,.F.);
#63103=ORIENTED_EDGE('',*,*,#47477,.T.);
#63104=ORIENTED_EDGE('',*,*,#47464,.F.);
#63105=ORIENTED_EDGE('',*,*,#47478,.T.);
#63106=ORIENTED_EDGE('',*,*,#47458,.F.);
#63107=ORIENTED_EDGE('',*,*,#47479,.T.);
#63108=ORIENTED_EDGE('',*,*,#47460,.F.);
#63109=ORIENTED_EDGE('',*,*,#47480,.T.);
#63110=ORIENTED_EDGE('',*,*,#47481,.T.);
#63111=ORIENTED_EDGE('',*,*,#47482,.T.);
#63112=ORIENTED_EDGE('',*,*,#47483,.F.);
#63113=ORIENTED_EDGE('',*,*,#47484,.F.);
#63114=ORIENTED_EDGE('',*,*,#47485,.F.);
#63115=ORIENTED_EDGE('',*,*,#47486,.T.);
#63116=ORIENTED_EDGE('',*,*,#47484,.T.);
#63117=ORIENTED_EDGE('',*,*,#47487,.T.);
#63118=ORIENTED_EDGE('',*,*,#47488,.T.);
#63119=ORIENTED_EDGE('',*,*,#47489,.T.);
#63120=ORIENTED_EDGE('',*,*,#47490,.T.);
#63121=ORIENTED_EDGE('',*,*,#47491,.T.);
#63122=ORIENTED_EDGE('',*,*,#47492,.T.);
#63123=ORIENTED_EDGE('',*,*,#47493,.T.);
#63124=ORIENTED_EDGE('',*,*,#47494,.T.);
#63125=ORIENTED_EDGE('',*,*,#47495,.T.);
#63126=ORIENTED_EDGE('',*,*,#47496,.F.);
#63127=ORIENTED_EDGE('',*,*,#47497,.F.);
#63128=ORIENTED_EDGE('',*,*,#47498,.F.);
#63129=ORIENTED_EDGE('',*,*,#47499,.T.);
#63130=ORIENTED_EDGE('',*,*,#47497,.T.);
#63131=ORIENTED_EDGE('',*,*,#47500,.T.);
#63132=ORIENTED_EDGE('',*,*,#47501,.T.);
#63133=ORIENTED_EDGE('',*,*,#47502,.T.);
#63134=ORIENTED_EDGE('',*,*,#46627,.F.);
#63135=ORIENTED_EDGE('',*,*,#47503,.T.);
#63136=ORIENTED_EDGE('',*,*,#47481,.F.);
#63137=ORIENTED_EDGE('',*,*,#47504,.T.);
#63138=ORIENTED_EDGE('',*,*,#47501,.F.);
#63139=ORIENTED_EDGE('',*,*,#47505,.T.);
#63140=ORIENTED_EDGE('',*,*,#46106,.F.);
#63141=ORIENTED_EDGE('',*,*,#47506,.T.);
#63142=ORIENTED_EDGE('',*,*,#47492,.F.);
#63143=ORIENTED_EDGE('',*,*,#47507,.T.);
#63144=ORIENTED_EDGE('',*,*,#47494,.F.);
#63145=ORIENTED_EDGE('',*,*,#47508,.T.);
#63146=ORIENTED_EDGE('',*,*,#47488,.F.);
#63147=ORIENTED_EDGE('',*,*,#47509,.T.);
#63148=ORIENTED_EDGE('',*,*,#47490,.F.);
#63149=ORIENTED_EDGE('',*,*,#47510,.T.);
#63150=ORIENTED_EDGE('',*,*,#47511,.T.);
#63151=ORIENTED_EDGE('',*,*,#47512,.T.);
#63152=ORIENTED_EDGE('',*,*,#47513,.F.);
#63153=ORIENTED_EDGE('',*,*,#47514,.F.);
#63154=ORIENTED_EDGE('',*,*,#47515,.F.);
#63155=ORIENTED_EDGE('',*,*,#47516,.T.);
#63156=ORIENTED_EDGE('',*,*,#47514,.T.);
#63157=ORIENTED_EDGE('',*,*,#47517,.T.);
#63158=ORIENTED_EDGE('',*,*,#47518,.T.);
#63159=ORIENTED_EDGE('',*,*,#47519,.T.);
#63160=ORIENTED_EDGE('',*,*,#47520,.T.);
#63161=ORIENTED_EDGE('',*,*,#47521,.T.);
#63162=ORIENTED_EDGE('',*,*,#47522,.T.);
#63163=ORIENTED_EDGE('',*,*,#47523,.T.);
#63164=ORIENTED_EDGE('',*,*,#47524,.T.);
#63165=ORIENTED_EDGE('',*,*,#47525,.T.);
#63166=ORIENTED_EDGE('',*,*,#47526,.F.);
#63167=ORIENTED_EDGE('',*,*,#47527,.F.);
#63168=ORIENTED_EDGE('',*,*,#47528,.F.);
#63169=ORIENTED_EDGE('',*,*,#47529,.T.);
#63170=ORIENTED_EDGE('',*,*,#47527,.T.);
#63171=ORIENTED_EDGE('',*,*,#47530,.T.);
#63172=ORIENTED_EDGE('',*,*,#47531,.T.);
#63173=ORIENTED_EDGE('',*,*,#47532,.T.);
#63174=ORIENTED_EDGE('',*,*,#46633,.F.);
#63175=ORIENTED_EDGE('',*,*,#47533,.T.);
#63176=ORIENTED_EDGE('',*,*,#47511,.F.);
#63177=ORIENTED_EDGE('',*,*,#47534,.T.);
#63178=ORIENTED_EDGE('',*,*,#47531,.F.);
#63179=ORIENTED_EDGE('',*,*,#47535,.T.);
#63180=ORIENTED_EDGE('',*,*,#46100,.F.);
#63181=ORIENTED_EDGE('',*,*,#47536,.T.);
#63182=ORIENTED_EDGE('',*,*,#47522,.F.);
#63183=ORIENTED_EDGE('',*,*,#47537,.T.);
#63184=ORIENTED_EDGE('',*,*,#47524,.F.);
#63185=ORIENTED_EDGE('',*,*,#47538,.T.);
#63186=ORIENTED_EDGE('',*,*,#47518,.F.);
#63187=ORIENTED_EDGE('',*,*,#47539,.T.);
#63188=ORIENTED_EDGE('',*,*,#47520,.F.);
#63189=ORIENTED_EDGE('',*,*,#47540,.T.);
#63190=ORIENTED_EDGE('',*,*,#47541,.T.);
#63191=ORIENTED_EDGE('',*,*,#47542,.T.);
#63192=ORIENTED_EDGE('',*,*,#47543,.F.);
#63193=ORIENTED_EDGE('',*,*,#47544,.F.);
#63194=ORIENTED_EDGE('',*,*,#47545,.F.);
#63195=ORIENTED_EDGE('',*,*,#47546,.T.);
#63196=ORIENTED_EDGE('',*,*,#47544,.T.);
#63197=ORIENTED_EDGE('',*,*,#47547,.T.);
#63198=ORIENTED_EDGE('',*,*,#47548,.T.);
#63199=ORIENTED_EDGE('',*,*,#47549,.T.);
#63200=ORIENTED_EDGE('',*,*,#47550,.T.);
#63201=ORIENTED_EDGE('',*,*,#47551,.T.);
#63202=ORIENTED_EDGE('',*,*,#47552,.T.);
#63203=ORIENTED_EDGE('',*,*,#47553,.T.);
#63204=ORIENTED_EDGE('',*,*,#47554,.T.);
#63205=ORIENTED_EDGE('',*,*,#47555,.T.);
#63206=ORIENTED_EDGE('',*,*,#47556,.F.);
#63207=ORIENTED_EDGE('',*,*,#47557,.F.);
#63208=ORIENTED_EDGE('',*,*,#47558,.F.);
#63209=ORIENTED_EDGE('',*,*,#47559,.T.);
#63210=ORIENTED_EDGE('',*,*,#47557,.T.);
#63211=ORIENTED_EDGE('',*,*,#47560,.T.);
#63212=ORIENTED_EDGE('',*,*,#47561,.T.);
#63213=ORIENTED_EDGE('',*,*,#47562,.T.);
#63214=ORIENTED_EDGE('',*,*,#46278,.F.);
#63215=ORIENTED_EDGE('',*,*,#47563,.T.);
#63216=ORIENTED_EDGE('',*,*,#47541,.F.);
#63217=ORIENTED_EDGE('',*,*,#47564,.T.);
#63218=ORIENTED_EDGE('',*,*,#47561,.F.);
#63219=ORIENTED_EDGE('',*,*,#47565,.T.);
#63220=ORIENTED_EDGE('',*,*,#46094,.F.);
#63221=ORIENTED_EDGE('',*,*,#47566,.T.);
#63222=ORIENTED_EDGE('',*,*,#47552,.F.);
#63223=ORIENTED_EDGE('',*,*,#47567,.T.);
#63224=ORIENTED_EDGE('',*,*,#47554,.F.);
#63225=ORIENTED_EDGE('',*,*,#47568,.T.);
#63226=ORIENTED_EDGE('',*,*,#47548,.F.);
#63227=ORIENTED_EDGE('',*,*,#47569,.T.);
#63228=ORIENTED_EDGE('',*,*,#47550,.F.);
#63229=ORIENTED_EDGE('',*,*,#47570,.T.);
#63230=ORIENTED_EDGE('',*,*,#47571,.T.);
#63231=ORIENTED_EDGE('',*,*,#47572,.T.);
#63232=ORIENTED_EDGE('',*,*,#47573,.F.);
#63233=ORIENTED_EDGE('',*,*,#47574,.F.);
#63234=ORIENTED_EDGE('',*,*,#47575,.F.);
#63235=ORIENTED_EDGE('',*,*,#47576,.T.);
#63236=ORIENTED_EDGE('',*,*,#47574,.T.);
#63237=ORIENTED_EDGE('',*,*,#47577,.T.);
#63238=ORIENTED_EDGE('',*,*,#47578,.T.);
#63239=ORIENTED_EDGE('',*,*,#47579,.T.);
#63240=ORIENTED_EDGE('',*,*,#47580,.T.);
#63241=ORIENTED_EDGE('',*,*,#47581,.T.);
#63242=ORIENTED_EDGE('',*,*,#47582,.T.);
#63243=ORIENTED_EDGE('',*,*,#47583,.T.);
#63244=ORIENTED_EDGE('',*,*,#47584,.T.);
#63245=ORIENTED_EDGE('',*,*,#47585,.T.);
#63246=ORIENTED_EDGE('',*,*,#47586,.F.);
#63247=ORIENTED_EDGE('',*,*,#47587,.F.);
#63248=ORIENTED_EDGE('',*,*,#47588,.F.);
#63249=ORIENTED_EDGE('',*,*,#47589,.T.);
#63250=ORIENTED_EDGE('',*,*,#47587,.T.);
#63251=ORIENTED_EDGE('',*,*,#47590,.T.);
#63252=ORIENTED_EDGE('',*,*,#47591,.T.);
#63253=ORIENTED_EDGE('',*,*,#47592,.T.);
#63254=ORIENTED_EDGE('',*,*,#46284,.F.);
#63255=ORIENTED_EDGE('',*,*,#47593,.T.);
#63256=ORIENTED_EDGE('',*,*,#47571,.F.);
#63257=ORIENTED_EDGE('',*,*,#47594,.T.);
#63258=ORIENTED_EDGE('',*,*,#47591,.F.);
#63259=ORIENTED_EDGE('',*,*,#47595,.T.);
#63260=ORIENTED_EDGE('',*,*,#46088,.F.);
#63261=ORIENTED_EDGE('',*,*,#47596,.T.);
#63262=ORIENTED_EDGE('',*,*,#47582,.F.);
#63263=ORIENTED_EDGE('',*,*,#47597,.T.);
#63264=ORIENTED_EDGE('',*,*,#47584,.F.);
#63265=ORIENTED_EDGE('',*,*,#47598,.T.);
#63266=ORIENTED_EDGE('',*,*,#47578,.F.);
#63267=ORIENTED_EDGE('',*,*,#47599,.T.);
#63268=ORIENTED_EDGE('',*,*,#47580,.F.);
#63269=ORIENTED_EDGE('',*,*,#47600,.T.);
#63270=ORIENTED_EDGE('',*,*,#47601,.T.);
#63271=ORIENTED_EDGE('',*,*,#47602,.T.);
#63272=ORIENTED_EDGE('',*,*,#47603,.F.);
#63273=ORIENTED_EDGE('',*,*,#47604,.F.);
#63274=ORIENTED_EDGE('',*,*,#47605,.F.);
#63275=ORIENTED_EDGE('',*,*,#47606,.T.);
#63276=ORIENTED_EDGE('',*,*,#47604,.T.);
#63277=ORIENTED_EDGE('',*,*,#47607,.T.);
#63278=ORIENTED_EDGE('',*,*,#47608,.T.);
#63279=ORIENTED_EDGE('',*,*,#47609,.T.);
#63280=ORIENTED_EDGE('',*,*,#47610,.T.);
#63281=ORIENTED_EDGE('',*,*,#47611,.T.);
#63282=ORIENTED_EDGE('',*,*,#47612,.T.);
#63283=ORIENTED_EDGE('',*,*,#47613,.T.);
#63284=ORIENTED_EDGE('',*,*,#47614,.T.);
#63285=ORIENTED_EDGE('',*,*,#47615,.T.);
#63286=ORIENTED_EDGE('',*,*,#47616,.F.);
#63287=ORIENTED_EDGE('',*,*,#47617,.F.);
#63288=ORIENTED_EDGE('',*,*,#47618,.F.);
#63289=ORIENTED_EDGE('',*,*,#47619,.T.);
#63290=ORIENTED_EDGE('',*,*,#47617,.T.);
#63291=ORIENTED_EDGE('',*,*,#47620,.T.);
#63292=ORIENTED_EDGE('',*,*,#47621,.T.);
#63293=ORIENTED_EDGE('',*,*,#47622,.T.);
#63294=ORIENTED_EDGE('',*,*,#46290,.F.);
#63295=ORIENTED_EDGE('',*,*,#47623,.T.);
#63296=ORIENTED_EDGE('',*,*,#47601,.F.);
#63297=ORIENTED_EDGE('',*,*,#47624,.T.);
#63298=ORIENTED_EDGE('',*,*,#47621,.F.);
#63299=ORIENTED_EDGE('',*,*,#47625,.T.);
#63300=ORIENTED_EDGE('',*,*,#46082,.F.);
#63301=ORIENTED_EDGE('',*,*,#47626,.T.);
#63302=ORIENTED_EDGE('',*,*,#47612,.F.);
#63303=ORIENTED_EDGE('',*,*,#47627,.T.);
#63304=ORIENTED_EDGE('',*,*,#47614,.F.);
#63305=ORIENTED_EDGE('',*,*,#47628,.T.);
#63306=ORIENTED_EDGE('',*,*,#47608,.F.);
#63307=ORIENTED_EDGE('',*,*,#47629,.T.);
#63308=ORIENTED_EDGE('',*,*,#47610,.F.);
#63309=ORIENTED_EDGE('',*,*,#47630,.T.);
#63310=ORIENTED_EDGE('',*,*,#47631,.T.);
#63311=ORIENTED_EDGE('',*,*,#47632,.T.);
#63312=ORIENTED_EDGE('',*,*,#47633,.F.);
#63313=ORIENTED_EDGE('',*,*,#47634,.F.);
#63314=ORIENTED_EDGE('',*,*,#47635,.F.);
#63315=ORIENTED_EDGE('',*,*,#47636,.T.);
#63316=ORIENTED_EDGE('',*,*,#47634,.T.);
#63317=ORIENTED_EDGE('',*,*,#47637,.T.);
#63318=ORIENTED_EDGE('',*,*,#47638,.T.);
#63319=ORIENTED_EDGE('',*,*,#47639,.T.);
#63320=ORIENTED_EDGE('',*,*,#47640,.T.);
#63321=ORIENTED_EDGE('',*,*,#47641,.T.);
#63322=ORIENTED_EDGE('',*,*,#47642,.T.);
#63323=ORIENTED_EDGE('',*,*,#47643,.T.);
#63324=ORIENTED_EDGE('',*,*,#47644,.T.);
#63325=ORIENTED_EDGE('',*,*,#47645,.T.);
#63326=ORIENTED_EDGE('',*,*,#47646,.F.);
#63327=ORIENTED_EDGE('',*,*,#47647,.F.);
#63328=ORIENTED_EDGE('',*,*,#47648,.F.);
#63329=ORIENTED_EDGE('',*,*,#47649,.T.);
#63330=ORIENTED_EDGE('',*,*,#47647,.T.);
#63331=ORIENTED_EDGE('',*,*,#47650,.T.);
#63332=ORIENTED_EDGE('',*,*,#47651,.T.);
#63333=ORIENTED_EDGE('',*,*,#47652,.T.);
#63334=ORIENTED_EDGE('',*,*,#46296,.F.);
#63335=ORIENTED_EDGE('',*,*,#47653,.T.);
#63336=ORIENTED_EDGE('',*,*,#47631,.F.);
#63337=ORIENTED_EDGE('',*,*,#47654,.T.);
#63338=ORIENTED_EDGE('',*,*,#47651,.F.);
#63339=ORIENTED_EDGE('',*,*,#47655,.T.);
#63340=ORIENTED_EDGE('',*,*,#46076,.F.);
#63341=ORIENTED_EDGE('',*,*,#47656,.T.);
#63342=ORIENTED_EDGE('',*,*,#47642,.F.);
#63343=ORIENTED_EDGE('',*,*,#47657,.T.);
#63344=ORIENTED_EDGE('',*,*,#47644,.F.);
#63345=ORIENTED_EDGE('',*,*,#47658,.T.);
#63346=ORIENTED_EDGE('',*,*,#47638,.F.);
#63347=ORIENTED_EDGE('',*,*,#47659,.T.);
#63348=ORIENTED_EDGE('',*,*,#47640,.F.);
#63349=ORIENTED_EDGE('',*,*,#47660,.T.);
#63350=ORIENTED_EDGE('',*,*,#47661,.T.);
#63351=ORIENTED_EDGE('',*,*,#47662,.T.);
#63352=ORIENTED_EDGE('',*,*,#47663,.F.);
#63353=ORIENTED_EDGE('',*,*,#47664,.F.);
#63354=ORIENTED_EDGE('',*,*,#47665,.F.);
#63355=ORIENTED_EDGE('',*,*,#47666,.T.);
#63356=ORIENTED_EDGE('',*,*,#47664,.T.);
#63357=ORIENTED_EDGE('',*,*,#47667,.T.);
#63358=ORIENTED_EDGE('',*,*,#47668,.T.);
#63359=ORIENTED_EDGE('',*,*,#47669,.T.);
#63360=ORIENTED_EDGE('',*,*,#47670,.T.);
#63361=ORIENTED_EDGE('',*,*,#47671,.T.);
#63362=ORIENTED_EDGE('',*,*,#47672,.T.);
#63363=ORIENTED_EDGE('',*,*,#47673,.T.);
#63364=ORIENTED_EDGE('',*,*,#47674,.T.);
#63365=ORIENTED_EDGE('',*,*,#47675,.T.);
#63366=ORIENTED_EDGE('',*,*,#47676,.F.);
#63367=ORIENTED_EDGE('',*,*,#47677,.F.);
#63368=ORIENTED_EDGE('',*,*,#47678,.F.);
#63369=ORIENTED_EDGE('',*,*,#47679,.T.);
#63370=ORIENTED_EDGE('',*,*,#47677,.T.);
#63371=ORIENTED_EDGE('',*,*,#47680,.T.);
#63372=ORIENTED_EDGE('',*,*,#47681,.T.);
#63373=ORIENTED_EDGE('',*,*,#47682,.T.);
#63374=ORIENTED_EDGE('',*,*,#46302,.F.);
#63375=ORIENTED_EDGE('',*,*,#47683,.T.);
#63376=ORIENTED_EDGE('',*,*,#47661,.F.);
#63377=ORIENTED_EDGE('',*,*,#47684,.T.);
#63378=ORIENTED_EDGE('',*,*,#47681,.F.);
#63379=ORIENTED_EDGE('',*,*,#47685,.T.);
#63380=ORIENTED_EDGE('',*,*,#46070,.F.);
#63381=ORIENTED_EDGE('',*,*,#47686,.T.);
#63382=ORIENTED_EDGE('',*,*,#47672,.F.);
#63383=ORIENTED_EDGE('',*,*,#47687,.T.);
#63384=ORIENTED_EDGE('',*,*,#47674,.F.);
#63385=ORIENTED_EDGE('',*,*,#47688,.T.);
#63386=ORIENTED_EDGE('',*,*,#47668,.F.);
#63387=ORIENTED_EDGE('',*,*,#47689,.T.);
#63388=ORIENTED_EDGE('',*,*,#47670,.F.);
#63389=ORIENTED_EDGE('',*,*,#47690,.T.);
#63390=ORIENTED_EDGE('',*,*,#47691,.T.);
#63391=ORIENTED_EDGE('',*,*,#47692,.T.);
#63392=ORIENTED_EDGE('',*,*,#47693,.F.);
#63393=ORIENTED_EDGE('',*,*,#47694,.F.);
#63394=ORIENTED_EDGE('',*,*,#47695,.F.);
#63395=ORIENTED_EDGE('',*,*,#47696,.T.);
#63396=ORIENTED_EDGE('',*,*,#47694,.T.);
#63397=ORIENTED_EDGE('',*,*,#47697,.T.);
#63398=ORIENTED_EDGE('',*,*,#47698,.T.);
#63399=ORIENTED_EDGE('',*,*,#47699,.T.);
#63400=ORIENTED_EDGE('',*,*,#47700,.T.);
#63401=ORIENTED_EDGE('',*,*,#47701,.T.);
#63402=ORIENTED_EDGE('',*,*,#47702,.T.);
#63403=ORIENTED_EDGE('',*,*,#47703,.T.);
#63404=ORIENTED_EDGE('',*,*,#47704,.T.);
#63405=ORIENTED_EDGE('',*,*,#47705,.T.);
#63406=ORIENTED_EDGE('',*,*,#47706,.F.);
#63407=ORIENTED_EDGE('',*,*,#47707,.F.);
#63408=ORIENTED_EDGE('',*,*,#47708,.F.);
#63409=ORIENTED_EDGE('',*,*,#47709,.T.);
#63410=ORIENTED_EDGE('',*,*,#47707,.T.);
#63411=ORIENTED_EDGE('',*,*,#47710,.T.);
#63412=ORIENTED_EDGE('',*,*,#47711,.T.);
#63413=ORIENTED_EDGE('',*,*,#47712,.T.);
#63414=ORIENTED_EDGE('',*,*,#46308,.F.);
#63415=ORIENTED_EDGE('',*,*,#47713,.T.);
#63416=ORIENTED_EDGE('',*,*,#47691,.F.);
#63417=ORIENTED_EDGE('',*,*,#47714,.T.);
#63418=ORIENTED_EDGE('',*,*,#47711,.F.);
#63419=ORIENTED_EDGE('',*,*,#47715,.T.);
#63420=ORIENTED_EDGE('',*,*,#46064,.F.);
#63421=ORIENTED_EDGE('',*,*,#47716,.T.);
#63422=ORIENTED_EDGE('',*,*,#47702,.F.);
#63423=ORIENTED_EDGE('',*,*,#47717,.T.);
#63424=ORIENTED_EDGE('',*,*,#47704,.F.);
#63425=ORIENTED_EDGE('',*,*,#47718,.T.);
#63426=ORIENTED_EDGE('',*,*,#47698,.F.);
#63427=ORIENTED_EDGE('',*,*,#47719,.T.);
#63428=ORIENTED_EDGE('',*,*,#47700,.F.);
#63429=ORIENTED_EDGE('',*,*,#47720,.T.);
#63430=ORIENTED_EDGE('',*,*,#47721,.T.);
#63431=ORIENTED_EDGE('',*,*,#47722,.T.);
#63432=ORIENTED_EDGE('',*,*,#47723,.F.);
#63433=ORIENTED_EDGE('',*,*,#47724,.F.);
#63434=ORIENTED_EDGE('',*,*,#47725,.F.);
#63435=ORIENTED_EDGE('',*,*,#47726,.T.);
#63436=ORIENTED_EDGE('',*,*,#47724,.T.);
#63437=ORIENTED_EDGE('',*,*,#47727,.T.);
#63438=ORIENTED_EDGE('',*,*,#47728,.T.);
#63439=ORIENTED_EDGE('',*,*,#47729,.T.);
#63440=ORIENTED_EDGE('',*,*,#47730,.T.);
#63441=ORIENTED_EDGE('',*,*,#47731,.T.);
#63442=ORIENTED_EDGE('',*,*,#47732,.T.);
#63443=ORIENTED_EDGE('',*,*,#47733,.T.);
#63444=ORIENTED_EDGE('',*,*,#47734,.T.);
#63445=ORIENTED_EDGE('',*,*,#47735,.T.);
#63446=ORIENTED_EDGE('',*,*,#47736,.F.);
#63447=ORIENTED_EDGE('',*,*,#47737,.F.);
#63448=ORIENTED_EDGE('',*,*,#47738,.F.);
#63449=ORIENTED_EDGE('',*,*,#47739,.T.);
#63450=ORIENTED_EDGE('',*,*,#47737,.T.);
#63451=ORIENTED_EDGE('',*,*,#47740,.T.);
#63452=ORIENTED_EDGE('',*,*,#47741,.T.);
#63453=ORIENTED_EDGE('',*,*,#47742,.T.);
#63454=ORIENTED_EDGE('',*,*,#46314,.F.);
#63455=ORIENTED_EDGE('',*,*,#47743,.T.);
#63456=ORIENTED_EDGE('',*,*,#47721,.F.);
#63457=ORIENTED_EDGE('',*,*,#47744,.T.);
#63458=ORIENTED_EDGE('',*,*,#47741,.F.);
#63459=ORIENTED_EDGE('',*,*,#47745,.T.);
#63460=ORIENTED_EDGE('',*,*,#46058,.F.);
#63461=ORIENTED_EDGE('',*,*,#47746,.T.);
#63462=ORIENTED_EDGE('',*,*,#47732,.F.);
#63463=ORIENTED_EDGE('',*,*,#47747,.T.);
#63464=ORIENTED_EDGE('',*,*,#47734,.F.);
#63465=ORIENTED_EDGE('',*,*,#47748,.T.);
#63466=ORIENTED_EDGE('',*,*,#47728,.F.);
#63467=ORIENTED_EDGE('',*,*,#47749,.T.);
#63468=ORIENTED_EDGE('',*,*,#47730,.F.);
#63469=ORIENTED_EDGE('',*,*,#47750,.T.);
#63470=ORIENTED_EDGE('',*,*,#47751,.T.);
#63471=ORIENTED_EDGE('',*,*,#47752,.T.);
#63472=ORIENTED_EDGE('',*,*,#47753,.F.);
#63473=ORIENTED_EDGE('',*,*,#47754,.F.);
#63474=ORIENTED_EDGE('',*,*,#47755,.F.);
#63475=ORIENTED_EDGE('',*,*,#47756,.T.);
#63476=ORIENTED_EDGE('',*,*,#47754,.T.);
#63477=ORIENTED_EDGE('',*,*,#47757,.T.);
#63478=ORIENTED_EDGE('',*,*,#47758,.T.);
#63479=ORIENTED_EDGE('',*,*,#47759,.T.);
#63480=ORIENTED_EDGE('',*,*,#47760,.T.);
#63481=ORIENTED_EDGE('',*,*,#47761,.T.);
#63482=ORIENTED_EDGE('',*,*,#47762,.T.);
#63483=ORIENTED_EDGE('',*,*,#47763,.T.);
#63484=ORIENTED_EDGE('',*,*,#47764,.T.);
#63485=ORIENTED_EDGE('',*,*,#47765,.T.);
#63486=ORIENTED_EDGE('',*,*,#47766,.F.);
#63487=ORIENTED_EDGE('',*,*,#47767,.F.);
#63488=ORIENTED_EDGE('',*,*,#47768,.F.);
#63489=ORIENTED_EDGE('',*,*,#47769,.T.);
#63490=ORIENTED_EDGE('',*,*,#47767,.T.);
#63491=ORIENTED_EDGE('',*,*,#47770,.T.);
#63492=ORIENTED_EDGE('',*,*,#47771,.T.);
#63493=ORIENTED_EDGE('',*,*,#47772,.T.);
#63494=ORIENTED_EDGE('',*,*,#46320,.F.);
#63495=ORIENTED_EDGE('',*,*,#47773,.T.);
#63496=ORIENTED_EDGE('',*,*,#47751,.F.);
#63497=ORIENTED_EDGE('',*,*,#47774,.T.);
#63498=ORIENTED_EDGE('',*,*,#47771,.F.);
#63499=ORIENTED_EDGE('',*,*,#47775,.T.);
#63500=ORIENTED_EDGE('',*,*,#46052,.F.);
#63501=ORIENTED_EDGE('',*,*,#47776,.T.);
#63502=ORIENTED_EDGE('',*,*,#47762,.F.);
#63503=ORIENTED_EDGE('',*,*,#47777,.T.);
#63504=ORIENTED_EDGE('',*,*,#47764,.F.);
#63505=ORIENTED_EDGE('',*,*,#47778,.T.);
#63506=ORIENTED_EDGE('',*,*,#47758,.F.);
#63507=ORIENTED_EDGE('',*,*,#47779,.T.);
#63508=ORIENTED_EDGE('',*,*,#47760,.F.);
#63509=ORIENTED_EDGE('',*,*,#47780,.T.);
#63510=ORIENTED_EDGE('',*,*,#47781,.T.);
#63511=ORIENTED_EDGE('',*,*,#47782,.T.);
#63512=ORIENTED_EDGE('',*,*,#47783,.F.);
#63513=ORIENTED_EDGE('',*,*,#47784,.F.);
#63514=ORIENTED_EDGE('',*,*,#47785,.F.);
#63515=ORIENTED_EDGE('',*,*,#47786,.T.);
#63516=ORIENTED_EDGE('',*,*,#47784,.T.);
#63517=ORIENTED_EDGE('',*,*,#47787,.T.);
#63518=ORIENTED_EDGE('',*,*,#47788,.T.);
#63519=ORIENTED_EDGE('',*,*,#47789,.T.);
#63520=ORIENTED_EDGE('',*,*,#47790,.T.);
#63521=ORIENTED_EDGE('',*,*,#47791,.T.);
#63522=ORIENTED_EDGE('',*,*,#47792,.T.);
#63523=ORIENTED_EDGE('',*,*,#47793,.T.);
#63524=ORIENTED_EDGE('',*,*,#47794,.T.);
#63525=ORIENTED_EDGE('',*,*,#47795,.T.);
#63526=ORIENTED_EDGE('',*,*,#47796,.F.);
#63527=ORIENTED_EDGE('',*,*,#47797,.F.);
#63528=ORIENTED_EDGE('',*,*,#47798,.F.);
#63529=ORIENTED_EDGE('',*,*,#47799,.T.);
#63530=ORIENTED_EDGE('',*,*,#47797,.T.);
#63531=ORIENTED_EDGE('',*,*,#47800,.T.);
#63532=ORIENTED_EDGE('',*,*,#47801,.T.);
#63533=ORIENTED_EDGE('',*,*,#47802,.T.);
#63534=ORIENTED_EDGE('',*,*,#46326,.F.);
#63535=ORIENTED_EDGE('',*,*,#47803,.T.);
#63536=ORIENTED_EDGE('',*,*,#47781,.F.);
#63537=ORIENTED_EDGE('',*,*,#47804,.T.);
#63538=ORIENTED_EDGE('',*,*,#47801,.F.);
#63539=ORIENTED_EDGE('',*,*,#47805,.T.);
#63540=ORIENTED_EDGE('',*,*,#46046,.F.);
#63541=ORIENTED_EDGE('',*,*,#47806,.T.);
#63542=ORIENTED_EDGE('',*,*,#47792,.F.);
#63543=ORIENTED_EDGE('',*,*,#47807,.T.);
#63544=ORIENTED_EDGE('',*,*,#47794,.F.);
#63545=ORIENTED_EDGE('',*,*,#47808,.T.);
#63546=ORIENTED_EDGE('',*,*,#47788,.F.);
#63547=ORIENTED_EDGE('',*,*,#47809,.T.);
#63548=ORIENTED_EDGE('',*,*,#47790,.F.);
#63549=ORIENTED_EDGE('',*,*,#47810,.T.);
#63550=ORIENTED_EDGE('',*,*,#47811,.T.);
#63551=ORIENTED_EDGE('',*,*,#47812,.T.);
#63552=ORIENTED_EDGE('',*,*,#47813,.F.);
#63553=ORIENTED_EDGE('',*,*,#47814,.F.);
#63554=ORIENTED_EDGE('',*,*,#47815,.F.);
#63555=ORIENTED_EDGE('',*,*,#47816,.T.);
#63556=ORIENTED_EDGE('',*,*,#47814,.T.);
#63557=ORIENTED_EDGE('',*,*,#47817,.T.);
#63558=ORIENTED_EDGE('',*,*,#47818,.T.);
#63559=ORIENTED_EDGE('',*,*,#47819,.T.);
#63560=ORIENTED_EDGE('',*,*,#47820,.T.);
#63561=ORIENTED_EDGE('',*,*,#47821,.T.);
#63562=ORIENTED_EDGE('',*,*,#47822,.T.);
#63563=ORIENTED_EDGE('',*,*,#47823,.T.);
#63564=ORIENTED_EDGE('',*,*,#47824,.T.);
#63565=ORIENTED_EDGE('',*,*,#47825,.T.);
#63566=ORIENTED_EDGE('',*,*,#47826,.F.);
#63567=ORIENTED_EDGE('',*,*,#47827,.F.);
#63568=ORIENTED_EDGE('',*,*,#47828,.F.);
#63569=ORIENTED_EDGE('',*,*,#47829,.T.);
#63570=ORIENTED_EDGE('',*,*,#47827,.T.);
#63571=ORIENTED_EDGE('',*,*,#47830,.T.);
#63572=ORIENTED_EDGE('',*,*,#47831,.T.);
#63573=ORIENTED_EDGE('',*,*,#47832,.T.);
#63574=ORIENTED_EDGE('',*,*,#46332,.F.);
#63575=ORIENTED_EDGE('',*,*,#47833,.T.);
#63576=ORIENTED_EDGE('',*,*,#47811,.F.);
#63577=ORIENTED_EDGE('',*,*,#47834,.T.);
#63578=ORIENTED_EDGE('',*,*,#47831,.F.);
#63579=ORIENTED_EDGE('',*,*,#47835,.T.);
#63580=ORIENTED_EDGE('',*,*,#46040,.F.);
#63581=ORIENTED_EDGE('',*,*,#47836,.T.);
#63582=ORIENTED_EDGE('',*,*,#47822,.F.);
#63583=ORIENTED_EDGE('',*,*,#47837,.T.);
#63584=ORIENTED_EDGE('',*,*,#47824,.F.);
#63585=ORIENTED_EDGE('',*,*,#47838,.T.);
#63586=ORIENTED_EDGE('',*,*,#47818,.F.);
#63587=ORIENTED_EDGE('',*,*,#47839,.T.);
#63588=ORIENTED_EDGE('',*,*,#47820,.F.);
#63589=ORIENTED_EDGE('',*,*,#47840,.T.);
#63590=ORIENTED_EDGE('',*,*,#47841,.T.);
#63591=ORIENTED_EDGE('',*,*,#47842,.T.);
#63592=ORIENTED_EDGE('',*,*,#47843,.F.);
#63593=ORIENTED_EDGE('',*,*,#47844,.F.);
#63594=ORIENTED_EDGE('',*,*,#47845,.F.);
#63595=ORIENTED_EDGE('',*,*,#47846,.T.);
#63596=ORIENTED_EDGE('',*,*,#47844,.T.);
#63597=ORIENTED_EDGE('',*,*,#47847,.T.);
#63598=ORIENTED_EDGE('',*,*,#47848,.T.);
#63599=ORIENTED_EDGE('',*,*,#47849,.T.);
#63600=ORIENTED_EDGE('',*,*,#47850,.T.);
#63601=ORIENTED_EDGE('',*,*,#47851,.T.);
#63602=ORIENTED_EDGE('',*,*,#47852,.T.);
#63603=ORIENTED_EDGE('',*,*,#47853,.T.);
#63604=ORIENTED_EDGE('',*,*,#47854,.T.);
#63605=ORIENTED_EDGE('',*,*,#47855,.T.);
#63606=ORIENTED_EDGE('',*,*,#47856,.F.);
#63607=ORIENTED_EDGE('',*,*,#47857,.F.);
#63608=ORIENTED_EDGE('',*,*,#47858,.F.);
#63609=ORIENTED_EDGE('',*,*,#47859,.T.);
#63610=ORIENTED_EDGE('',*,*,#47857,.T.);
#63611=ORIENTED_EDGE('',*,*,#47860,.T.);
#63612=ORIENTED_EDGE('',*,*,#47861,.T.);
#63613=ORIENTED_EDGE('',*,*,#47862,.T.);
#63614=ORIENTED_EDGE('',*,*,#46338,.F.);
#63615=ORIENTED_EDGE('',*,*,#47863,.T.);
#63616=ORIENTED_EDGE('',*,*,#47841,.F.);
#63617=ORIENTED_EDGE('',*,*,#47864,.T.);
#63618=ORIENTED_EDGE('',*,*,#47861,.F.);
#63619=ORIENTED_EDGE('',*,*,#47865,.T.);
#63620=ORIENTED_EDGE('',*,*,#46034,.F.);
#63621=ORIENTED_EDGE('',*,*,#47866,.T.);
#63622=ORIENTED_EDGE('',*,*,#47852,.F.);
#63623=ORIENTED_EDGE('',*,*,#47867,.T.);
#63624=ORIENTED_EDGE('',*,*,#47854,.F.);
#63625=ORIENTED_EDGE('',*,*,#47868,.T.);
#63626=ORIENTED_EDGE('',*,*,#47848,.F.);
#63627=ORIENTED_EDGE('',*,*,#47869,.T.);
#63628=ORIENTED_EDGE('',*,*,#47850,.F.);
#63629=ORIENTED_EDGE('',*,*,#47870,.T.);
#63630=ORIENTED_EDGE('',*,*,#47871,.T.);
#63631=ORIENTED_EDGE('',*,*,#47872,.T.);
#63632=ORIENTED_EDGE('',*,*,#47873,.F.);
#63633=ORIENTED_EDGE('',*,*,#47874,.F.);
#63634=ORIENTED_EDGE('',*,*,#47875,.F.);
#63635=ORIENTED_EDGE('',*,*,#47876,.T.);
#63636=ORIENTED_EDGE('',*,*,#47874,.T.);
#63637=ORIENTED_EDGE('',*,*,#47877,.T.);
#63638=ORIENTED_EDGE('',*,*,#47878,.T.);
#63639=ORIENTED_EDGE('',*,*,#47879,.T.);
#63640=ORIENTED_EDGE('',*,*,#47880,.T.);
#63641=ORIENTED_EDGE('',*,*,#47881,.T.);
#63642=ORIENTED_EDGE('',*,*,#47882,.T.);
#63643=ORIENTED_EDGE('',*,*,#47883,.T.);
#63644=ORIENTED_EDGE('',*,*,#47884,.T.);
#63645=ORIENTED_EDGE('',*,*,#47885,.T.);
#63646=ORIENTED_EDGE('',*,*,#47886,.F.);
#63647=ORIENTED_EDGE('',*,*,#47887,.F.);
#63648=ORIENTED_EDGE('',*,*,#47888,.F.);
#63649=ORIENTED_EDGE('',*,*,#47889,.T.);
#63650=ORIENTED_EDGE('',*,*,#47887,.T.);
#63651=ORIENTED_EDGE('',*,*,#47890,.T.);
#63652=ORIENTED_EDGE('',*,*,#47891,.T.);
#63653=ORIENTED_EDGE('',*,*,#47892,.T.);
#63654=ORIENTED_EDGE('',*,*,#46344,.F.);
#63655=ORIENTED_EDGE('',*,*,#47893,.T.);
#63656=ORIENTED_EDGE('',*,*,#47871,.F.);
#63657=ORIENTED_EDGE('',*,*,#47894,.T.);
#63658=ORIENTED_EDGE('',*,*,#47891,.F.);
#63659=ORIENTED_EDGE('',*,*,#47895,.T.);
#63660=ORIENTED_EDGE('',*,*,#46028,.F.);
#63661=ORIENTED_EDGE('',*,*,#47896,.T.);
#63662=ORIENTED_EDGE('',*,*,#47882,.F.);
#63663=ORIENTED_EDGE('',*,*,#47897,.T.);
#63664=ORIENTED_EDGE('',*,*,#47884,.F.);
#63665=ORIENTED_EDGE('',*,*,#47898,.T.);
#63666=ORIENTED_EDGE('',*,*,#47878,.F.);
#63667=ORIENTED_EDGE('',*,*,#47899,.T.);
#63668=ORIENTED_EDGE('',*,*,#47880,.F.);
#63669=ORIENTED_EDGE('',*,*,#47900,.T.);
#63670=ORIENTED_EDGE('',*,*,#47901,.T.);
#63671=ORIENTED_EDGE('',*,*,#47902,.T.);
#63672=ORIENTED_EDGE('',*,*,#47903,.F.);
#63673=ORIENTED_EDGE('',*,*,#47904,.F.);
#63674=ORIENTED_EDGE('',*,*,#47905,.F.);
#63675=ORIENTED_EDGE('',*,*,#47906,.T.);
#63676=ORIENTED_EDGE('',*,*,#47904,.T.);
#63677=ORIENTED_EDGE('',*,*,#47907,.T.);
#63678=ORIENTED_EDGE('',*,*,#47908,.T.);
#63679=ORIENTED_EDGE('',*,*,#47909,.T.);
#63680=ORIENTED_EDGE('',*,*,#47910,.T.);
#63681=ORIENTED_EDGE('',*,*,#47911,.T.);
#63682=ORIENTED_EDGE('',*,*,#47912,.T.);
#63683=ORIENTED_EDGE('',*,*,#47913,.T.);
#63684=ORIENTED_EDGE('',*,*,#47914,.T.);
#63685=ORIENTED_EDGE('',*,*,#47915,.T.);
#63686=ORIENTED_EDGE('',*,*,#47916,.F.);
#63687=ORIENTED_EDGE('',*,*,#47917,.F.);
#63688=ORIENTED_EDGE('',*,*,#47918,.F.);
#63689=ORIENTED_EDGE('',*,*,#47919,.T.);
#63690=ORIENTED_EDGE('',*,*,#47917,.T.);
#63691=ORIENTED_EDGE('',*,*,#47920,.T.);
#63692=ORIENTED_EDGE('',*,*,#47921,.T.);
#63693=ORIENTED_EDGE('',*,*,#47922,.T.);
#63694=ORIENTED_EDGE('',*,*,#46350,.F.);
#63695=ORIENTED_EDGE('',*,*,#47923,.T.);
#63696=ORIENTED_EDGE('',*,*,#47901,.F.);
#63697=ORIENTED_EDGE('',*,*,#47924,.T.);
#63698=ORIENTED_EDGE('',*,*,#47921,.F.);
#63699=ORIENTED_EDGE('',*,*,#47925,.T.);
#63700=ORIENTED_EDGE('',*,*,#46022,.F.);
#63701=ORIENTED_EDGE('',*,*,#47926,.T.);
#63702=ORIENTED_EDGE('',*,*,#47912,.F.);
#63703=ORIENTED_EDGE('',*,*,#47927,.T.);
#63704=ORIENTED_EDGE('',*,*,#47914,.F.);
#63705=ORIENTED_EDGE('',*,*,#47928,.T.);
#63706=ORIENTED_EDGE('',*,*,#47908,.F.);
#63707=ORIENTED_EDGE('',*,*,#47929,.T.);
#63708=ORIENTED_EDGE('',*,*,#47910,.F.);
#63709=ORIENTED_EDGE('',*,*,#47930,.T.);
#63710=ORIENTED_EDGE('',*,*,#47931,.T.);
#63711=ORIENTED_EDGE('',*,*,#47932,.T.);
#63712=ORIENTED_EDGE('',*,*,#47933,.F.);
#63713=ORIENTED_EDGE('',*,*,#47934,.F.);
#63714=ORIENTED_EDGE('',*,*,#47935,.F.);
#63715=ORIENTED_EDGE('',*,*,#47936,.T.);
#63716=ORIENTED_EDGE('',*,*,#47934,.T.);
#63717=ORIENTED_EDGE('',*,*,#47937,.T.);
#63718=ORIENTED_EDGE('',*,*,#47938,.T.);
#63719=ORIENTED_EDGE('',*,*,#47939,.T.);
#63720=ORIENTED_EDGE('',*,*,#47940,.T.);
#63721=ORIENTED_EDGE('',*,*,#47941,.T.);
#63722=ORIENTED_EDGE('',*,*,#47942,.T.);
#63723=ORIENTED_EDGE('',*,*,#47943,.T.);
#63724=ORIENTED_EDGE('',*,*,#47944,.T.);
#63725=ORIENTED_EDGE('',*,*,#47945,.T.);
#63726=ORIENTED_EDGE('',*,*,#47946,.F.);
#63727=ORIENTED_EDGE('',*,*,#47947,.F.);
#63728=ORIENTED_EDGE('',*,*,#47948,.F.);
#63729=ORIENTED_EDGE('',*,*,#47949,.T.);
#63730=ORIENTED_EDGE('',*,*,#47947,.T.);
#63731=ORIENTED_EDGE('',*,*,#47950,.T.);
#63732=ORIENTED_EDGE('',*,*,#47951,.T.);
#63733=ORIENTED_EDGE('',*,*,#47952,.T.);
#63734=ORIENTED_EDGE('',*,*,#46356,.F.);
#63735=ORIENTED_EDGE('',*,*,#47953,.T.);
#63736=ORIENTED_EDGE('',*,*,#47931,.F.);
#63737=ORIENTED_EDGE('',*,*,#47954,.T.);
#63738=ORIENTED_EDGE('',*,*,#47951,.F.);
#63739=ORIENTED_EDGE('',*,*,#47955,.T.);
#63740=ORIENTED_EDGE('',*,*,#46016,.F.);
#63741=ORIENTED_EDGE('',*,*,#47956,.T.);
#63742=ORIENTED_EDGE('',*,*,#47942,.F.);
#63743=ORIENTED_EDGE('',*,*,#47957,.T.);
#63744=ORIENTED_EDGE('',*,*,#47944,.F.);
#63745=ORIENTED_EDGE('',*,*,#47958,.T.);
#63746=ORIENTED_EDGE('',*,*,#47938,.F.);
#63747=ORIENTED_EDGE('',*,*,#47959,.T.);
#63748=ORIENTED_EDGE('',*,*,#47940,.F.);
#63749=ORIENTED_EDGE('',*,*,#47960,.T.);
#63750=ORIENTED_EDGE('',*,*,#47961,.T.);
#63751=ORIENTED_EDGE('',*,*,#47962,.T.);
#63752=ORIENTED_EDGE('',*,*,#47963,.F.);
#63753=ORIENTED_EDGE('',*,*,#47964,.F.);
#63754=ORIENTED_EDGE('',*,*,#47965,.F.);
#63755=ORIENTED_EDGE('',*,*,#47966,.T.);
#63756=ORIENTED_EDGE('',*,*,#47964,.T.);
#63757=ORIENTED_EDGE('',*,*,#47967,.T.);
#63758=ORIENTED_EDGE('',*,*,#47968,.T.);
#63759=ORIENTED_EDGE('',*,*,#47969,.T.);
#63760=ORIENTED_EDGE('',*,*,#47970,.T.);
#63761=ORIENTED_EDGE('',*,*,#47971,.T.);
#63762=ORIENTED_EDGE('',*,*,#47972,.T.);
#63763=ORIENTED_EDGE('',*,*,#47973,.T.);
#63764=ORIENTED_EDGE('',*,*,#47974,.T.);
#63765=ORIENTED_EDGE('',*,*,#47975,.T.);
#63766=ORIENTED_EDGE('',*,*,#47976,.F.);
#63767=ORIENTED_EDGE('',*,*,#47977,.F.);
#63768=ORIENTED_EDGE('',*,*,#47978,.F.);
#63769=ORIENTED_EDGE('',*,*,#47979,.T.);
#63770=ORIENTED_EDGE('',*,*,#47977,.T.);
#63771=ORIENTED_EDGE('',*,*,#47980,.T.);
#63772=ORIENTED_EDGE('',*,*,#47981,.T.);
#63773=ORIENTED_EDGE('',*,*,#47982,.T.);
#63774=ORIENTED_EDGE('',*,*,#46362,.F.);
#63775=ORIENTED_EDGE('',*,*,#47983,.T.);
#63776=ORIENTED_EDGE('',*,*,#47961,.F.);
#63777=ORIENTED_EDGE('',*,*,#47984,.T.);
#63778=ORIENTED_EDGE('',*,*,#47981,.F.);
#63779=ORIENTED_EDGE('',*,*,#47985,.T.);
#63780=ORIENTED_EDGE('',*,*,#46010,.F.);
#63781=ORIENTED_EDGE('',*,*,#47986,.T.);
#63782=ORIENTED_EDGE('',*,*,#47972,.F.);
#63783=ORIENTED_EDGE('',*,*,#47987,.T.);
#63784=ORIENTED_EDGE('',*,*,#47974,.F.);
#63785=ORIENTED_EDGE('',*,*,#47988,.T.);
#63786=ORIENTED_EDGE('',*,*,#47968,.F.);
#63787=ORIENTED_EDGE('',*,*,#47989,.T.);
#63788=ORIENTED_EDGE('',*,*,#47970,.F.);
#63789=ORIENTED_EDGE('',*,*,#47990,.T.);
#63790=ORIENTED_EDGE('',*,*,#47991,.T.);
#63791=ORIENTED_EDGE('',*,*,#47992,.T.);
#63792=ORIENTED_EDGE('',*,*,#47993,.F.);
#63793=ORIENTED_EDGE('',*,*,#47994,.F.);
#63794=ORIENTED_EDGE('',*,*,#47995,.F.);
#63795=ORIENTED_EDGE('',*,*,#47996,.T.);
#63796=ORIENTED_EDGE('',*,*,#47994,.T.);
#63797=ORIENTED_EDGE('',*,*,#47997,.T.);
#63798=ORIENTED_EDGE('',*,*,#47998,.T.);
#63799=ORIENTED_EDGE('',*,*,#47999,.T.);
#63800=ORIENTED_EDGE('',*,*,#48000,.T.);
#63801=ORIENTED_EDGE('',*,*,#48001,.T.);
#63802=ORIENTED_EDGE('',*,*,#48002,.T.);
#63803=ORIENTED_EDGE('',*,*,#48003,.T.);
#63804=ORIENTED_EDGE('',*,*,#48004,.T.);
#63805=ORIENTED_EDGE('',*,*,#48005,.T.);
#63806=ORIENTED_EDGE('',*,*,#48006,.F.);
#63807=ORIENTED_EDGE('',*,*,#48007,.F.);
#63808=ORIENTED_EDGE('',*,*,#48008,.F.);
#63809=ORIENTED_EDGE('',*,*,#48009,.T.);
#63810=ORIENTED_EDGE('',*,*,#48007,.T.);
#63811=ORIENTED_EDGE('',*,*,#48010,.T.);
#63812=ORIENTED_EDGE('',*,*,#48011,.T.);
#63813=ORIENTED_EDGE('',*,*,#48012,.T.);
#63814=ORIENTED_EDGE('',*,*,#46368,.F.);
#63815=ORIENTED_EDGE('',*,*,#48013,.T.);
#63816=ORIENTED_EDGE('',*,*,#47991,.F.);
#63817=ORIENTED_EDGE('',*,*,#48014,.T.);
#63818=ORIENTED_EDGE('',*,*,#48011,.F.);
#63819=ORIENTED_EDGE('',*,*,#48015,.T.);
#63820=ORIENTED_EDGE('',*,*,#46004,.F.);
#63821=ORIENTED_EDGE('',*,*,#48016,.T.);
#63822=ORIENTED_EDGE('',*,*,#48002,.F.);
#63823=ORIENTED_EDGE('',*,*,#48017,.T.);
#63824=ORIENTED_EDGE('',*,*,#48004,.F.);
#63825=ORIENTED_EDGE('',*,*,#48018,.T.);
#63826=ORIENTED_EDGE('',*,*,#47998,.F.);
#63827=ORIENTED_EDGE('',*,*,#48019,.T.);
#63828=ORIENTED_EDGE('',*,*,#48000,.F.);
#63829=ORIENTED_EDGE('',*,*,#48020,.T.);
#63830=ORIENTED_EDGE('',*,*,#48021,.T.);
#63831=ORIENTED_EDGE('',*,*,#48022,.T.);
#63832=ORIENTED_EDGE('',*,*,#48023,.F.);
#63833=ORIENTED_EDGE('',*,*,#48024,.F.);
#63834=ORIENTED_EDGE('',*,*,#48025,.F.);
#63835=ORIENTED_EDGE('',*,*,#48026,.T.);
#63836=ORIENTED_EDGE('',*,*,#48024,.T.);
#63837=ORIENTED_EDGE('',*,*,#48027,.T.);
#63838=ORIENTED_EDGE('',*,*,#48028,.T.);
#63839=ORIENTED_EDGE('',*,*,#48029,.T.);
#63840=ORIENTED_EDGE('',*,*,#48030,.T.);
#63841=ORIENTED_EDGE('',*,*,#48031,.T.);
#63842=ORIENTED_EDGE('',*,*,#48032,.T.);
#63843=ORIENTED_EDGE('',*,*,#48033,.T.);
#63844=ORIENTED_EDGE('',*,*,#48034,.T.);
#63845=ORIENTED_EDGE('',*,*,#48035,.T.);
#63846=ORIENTED_EDGE('',*,*,#48036,.F.);
#63847=ORIENTED_EDGE('',*,*,#48037,.F.);
#63848=ORIENTED_EDGE('',*,*,#48038,.F.);
#63849=ORIENTED_EDGE('',*,*,#48039,.T.);
#63850=ORIENTED_EDGE('',*,*,#48037,.T.);
#63851=ORIENTED_EDGE('',*,*,#48040,.T.);
#63852=ORIENTED_EDGE('',*,*,#48041,.T.);
#63853=ORIENTED_EDGE('',*,*,#48042,.T.);
#63854=ORIENTED_EDGE('',*,*,#46374,.F.);
#63855=ORIENTED_EDGE('',*,*,#48043,.T.);
#63856=ORIENTED_EDGE('',*,*,#48021,.F.);
#63857=ORIENTED_EDGE('',*,*,#48044,.T.);
#63858=ORIENTED_EDGE('',*,*,#48041,.F.);
#63859=ORIENTED_EDGE('',*,*,#48045,.T.);
#63860=ORIENTED_EDGE('',*,*,#45998,.F.);
#63861=ORIENTED_EDGE('',*,*,#48046,.T.);
#63862=ORIENTED_EDGE('',*,*,#48032,.F.);
#63863=ORIENTED_EDGE('',*,*,#48047,.T.);
#63864=ORIENTED_EDGE('',*,*,#48034,.F.);
#63865=ORIENTED_EDGE('',*,*,#48048,.T.);
#63866=ORIENTED_EDGE('',*,*,#48028,.F.);
#63867=ORIENTED_EDGE('',*,*,#48049,.T.);
#63868=ORIENTED_EDGE('',*,*,#48030,.F.);
#63869=ORIENTED_EDGE('',*,*,#48050,.T.);
#63870=ORIENTED_EDGE('',*,*,#48051,.T.);
#63871=ORIENTED_EDGE('',*,*,#48052,.T.);
#63872=ORIENTED_EDGE('',*,*,#48053,.F.);
#63873=ORIENTED_EDGE('',*,*,#48054,.F.);
#63874=ORIENTED_EDGE('',*,*,#48055,.F.);
#63875=ORIENTED_EDGE('',*,*,#48056,.T.);
#63876=ORIENTED_EDGE('',*,*,#48054,.T.);
#63877=ORIENTED_EDGE('',*,*,#48057,.T.);
#63878=ORIENTED_EDGE('',*,*,#48058,.T.);
#63879=ORIENTED_EDGE('',*,*,#48059,.T.);
#63880=ORIENTED_EDGE('',*,*,#48060,.T.);
#63881=ORIENTED_EDGE('',*,*,#48061,.T.);
#63882=ORIENTED_EDGE('',*,*,#48062,.T.);
#63883=ORIENTED_EDGE('',*,*,#48063,.T.);
#63884=ORIENTED_EDGE('',*,*,#48064,.T.);
#63885=ORIENTED_EDGE('',*,*,#48065,.T.);
#63886=ORIENTED_EDGE('',*,*,#48066,.F.);
#63887=ORIENTED_EDGE('',*,*,#48067,.F.);
#63888=ORIENTED_EDGE('',*,*,#48068,.F.);
#63889=ORIENTED_EDGE('',*,*,#48069,.T.);
#63890=ORIENTED_EDGE('',*,*,#48067,.T.);
#63891=ORIENTED_EDGE('',*,*,#48070,.T.);
#63892=ORIENTED_EDGE('',*,*,#48071,.T.);
#63893=ORIENTED_EDGE('',*,*,#48072,.T.);
#63894=ORIENTED_EDGE('',*,*,#46380,.F.);
#63895=ORIENTED_EDGE('',*,*,#48073,.T.);
#63896=ORIENTED_EDGE('',*,*,#48051,.F.);
#63897=ORIENTED_EDGE('',*,*,#48074,.T.);
#63898=ORIENTED_EDGE('',*,*,#48071,.F.);
#63899=ORIENTED_EDGE('',*,*,#48075,.T.);
#63900=ORIENTED_EDGE('',*,*,#45992,.F.);
#63901=ORIENTED_EDGE('',*,*,#48076,.T.);
#63902=ORIENTED_EDGE('',*,*,#48062,.F.);
#63903=ORIENTED_EDGE('',*,*,#48077,.T.);
#63904=ORIENTED_EDGE('',*,*,#48064,.F.);
#63905=ORIENTED_EDGE('',*,*,#48078,.T.);
#63906=ORIENTED_EDGE('',*,*,#48058,.F.);
#63907=ORIENTED_EDGE('',*,*,#48079,.T.);
#63908=ORIENTED_EDGE('',*,*,#48060,.F.);
#63909=ORIENTED_EDGE('',*,*,#48080,.T.);
#63910=ORIENTED_EDGE('',*,*,#48081,.T.);
#63911=ORIENTED_EDGE('',*,*,#48082,.T.);
#63912=ORIENTED_EDGE('',*,*,#48083,.F.);
#63913=ORIENTED_EDGE('',*,*,#48084,.F.);
#63914=ORIENTED_EDGE('',*,*,#48085,.F.);
#63915=ORIENTED_EDGE('',*,*,#48086,.T.);
#63916=ORIENTED_EDGE('',*,*,#48084,.T.);
#63917=ORIENTED_EDGE('',*,*,#48087,.T.);
#63918=ORIENTED_EDGE('',*,*,#48088,.T.);
#63919=ORIENTED_EDGE('',*,*,#48089,.T.);
#63920=ORIENTED_EDGE('',*,*,#48090,.T.);
#63921=ORIENTED_EDGE('',*,*,#48091,.T.);
#63922=ORIENTED_EDGE('',*,*,#48092,.T.);
#63923=ORIENTED_EDGE('',*,*,#48093,.T.);
#63924=ORIENTED_EDGE('',*,*,#48094,.T.);
#63925=ORIENTED_EDGE('',*,*,#48095,.T.);
#63926=ORIENTED_EDGE('',*,*,#48096,.F.);
#63927=ORIENTED_EDGE('',*,*,#48097,.F.);
#63928=ORIENTED_EDGE('',*,*,#48098,.F.);
#63929=ORIENTED_EDGE('',*,*,#48099,.T.);
#63930=ORIENTED_EDGE('',*,*,#48097,.T.);
#63931=ORIENTED_EDGE('',*,*,#48100,.T.);
#63932=ORIENTED_EDGE('',*,*,#48101,.T.);
#63933=ORIENTED_EDGE('',*,*,#48102,.T.);
#63934=ORIENTED_EDGE('',*,*,#46386,.F.);
#63935=ORIENTED_EDGE('',*,*,#48103,.T.);
#63936=ORIENTED_EDGE('',*,*,#48081,.F.);
#63937=ORIENTED_EDGE('',*,*,#48104,.T.);
#63938=ORIENTED_EDGE('',*,*,#48101,.F.);
#63939=ORIENTED_EDGE('',*,*,#48105,.T.);
#63940=ORIENTED_EDGE('',*,*,#45986,.F.);
#63941=ORIENTED_EDGE('',*,*,#48106,.T.);
#63942=ORIENTED_EDGE('',*,*,#48092,.F.);
#63943=ORIENTED_EDGE('',*,*,#48107,.T.);
#63944=ORIENTED_EDGE('',*,*,#48094,.F.);
#63945=ORIENTED_EDGE('',*,*,#48108,.T.);
#63946=ORIENTED_EDGE('',*,*,#48088,.F.);
#63947=ORIENTED_EDGE('',*,*,#48109,.T.);
#63948=ORIENTED_EDGE('',*,*,#48090,.F.);
#63949=ORIENTED_EDGE('',*,*,#48110,.T.);
#63950=ORIENTED_EDGE('',*,*,#48111,.T.);
#63951=ORIENTED_EDGE('',*,*,#48112,.T.);
#63952=ORIENTED_EDGE('',*,*,#48113,.F.);
#63953=ORIENTED_EDGE('',*,*,#48114,.F.);
#63954=ORIENTED_EDGE('',*,*,#48115,.F.);
#63955=ORIENTED_EDGE('',*,*,#48116,.T.);
#63956=ORIENTED_EDGE('',*,*,#48114,.T.);
#63957=ORIENTED_EDGE('',*,*,#48117,.T.);
#63958=ORIENTED_EDGE('',*,*,#48118,.T.);
#63959=ORIENTED_EDGE('',*,*,#48119,.T.);
#63960=ORIENTED_EDGE('',*,*,#48120,.T.);
#63961=ORIENTED_EDGE('',*,*,#48121,.T.);
#63962=ORIENTED_EDGE('',*,*,#48122,.T.);
#63963=ORIENTED_EDGE('',*,*,#48123,.T.);
#63964=ORIENTED_EDGE('',*,*,#48124,.T.);
#63965=ORIENTED_EDGE('',*,*,#48125,.T.);
#63966=ORIENTED_EDGE('',*,*,#48126,.F.);
#63967=ORIENTED_EDGE('',*,*,#48127,.F.);
#63968=ORIENTED_EDGE('',*,*,#48128,.F.);
#63969=ORIENTED_EDGE('',*,*,#48129,.T.);
#63970=ORIENTED_EDGE('',*,*,#48127,.T.);
#63971=ORIENTED_EDGE('',*,*,#48130,.T.);
#63972=ORIENTED_EDGE('',*,*,#48131,.T.);
#63973=ORIENTED_EDGE('',*,*,#48132,.T.);
#63974=ORIENTED_EDGE('',*,*,#46392,.F.);
#63975=ORIENTED_EDGE('',*,*,#48133,.T.);
#63976=ORIENTED_EDGE('',*,*,#48111,.F.);
#63977=ORIENTED_EDGE('',*,*,#48134,.T.);
#63978=ORIENTED_EDGE('',*,*,#48131,.F.);
#63979=ORIENTED_EDGE('',*,*,#48135,.T.);
#63980=ORIENTED_EDGE('',*,*,#45980,.F.);
#63981=ORIENTED_EDGE('',*,*,#48136,.T.);
#63982=ORIENTED_EDGE('',*,*,#48122,.F.);
#63983=ORIENTED_EDGE('',*,*,#48137,.T.);
#63984=ORIENTED_EDGE('',*,*,#48124,.F.);
#63985=ORIENTED_EDGE('',*,*,#48138,.T.);
#63986=ORIENTED_EDGE('',*,*,#48118,.F.);
#63987=ORIENTED_EDGE('',*,*,#48139,.T.);
#63988=ORIENTED_EDGE('',*,*,#48120,.F.);
#63989=ORIENTED_EDGE('',*,*,#48140,.T.);
#63990=ORIENTED_EDGE('',*,*,#48141,.T.);
#63991=ORIENTED_EDGE('',*,*,#48142,.T.);
#63992=ORIENTED_EDGE('',*,*,#48143,.F.);
#63993=ORIENTED_EDGE('',*,*,#48144,.F.);
#63994=ORIENTED_EDGE('',*,*,#48145,.F.);
#63995=ORIENTED_EDGE('',*,*,#48146,.T.);
#63996=ORIENTED_EDGE('',*,*,#48144,.T.);
#63997=ORIENTED_EDGE('',*,*,#48147,.T.);
#63998=ORIENTED_EDGE('',*,*,#48148,.T.);
#63999=ORIENTED_EDGE('',*,*,#48149,.T.);
#64000=ORIENTED_EDGE('',*,*,#48150,.T.);
#64001=ORIENTED_EDGE('',*,*,#48151,.T.);
#64002=ORIENTED_EDGE('',*,*,#48152,.T.);
#64003=ORIENTED_EDGE('',*,*,#48153,.T.);
#64004=ORIENTED_EDGE('',*,*,#48154,.T.);
#64005=ORIENTED_EDGE('',*,*,#48155,.T.);
#64006=ORIENTED_EDGE('',*,*,#48156,.F.);
#64007=ORIENTED_EDGE('',*,*,#48157,.F.);
#64008=ORIENTED_EDGE('',*,*,#48158,.F.);
#64009=ORIENTED_EDGE('',*,*,#48159,.T.);
#64010=ORIENTED_EDGE('',*,*,#48157,.T.);
#64011=ORIENTED_EDGE('',*,*,#48160,.T.);
#64012=ORIENTED_EDGE('',*,*,#48161,.T.);
#64013=ORIENTED_EDGE('',*,*,#48162,.T.);
#64014=ORIENTED_EDGE('',*,*,#46398,.F.);
#64015=ORIENTED_EDGE('',*,*,#48163,.T.);
#64016=ORIENTED_EDGE('',*,*,#48141,.F.);
#64017=ORIENTED_EDGE('',*,*,#48164,.T.);
#64018=ORIENTED_EDGE('',*,*,#48161,.F.);
#64019=ORIENTED_EDGE('',*,*,#48165,.T.);
#64020=ORIENTED_EDGE('',*,*,#45974,.F.);
#64021=ORIENTED_EDGE('',*,*,#48166,.T.);
#64022=ORIENTED_EDGE('',*,*,#48152,.F.);
#64023=ORIENTED_EDGE('',*,*,#48167,.T.);
#64024=ORIENTED_EDGE('',*,*,#48154,.F.);
#64025=ORIENTED_EDGE('',*,*,#48168,.T.);
#64026=ORIENTED_EDGE('',*,*,#48148,.F.);
#64027=ORIENTED_EDGE('',*,*,#48169,.T.);
#64028=ORIENTED_EDGE('',*,*,#48150,.F.);
#64029=ORIENTED_EDGE('',*,*,#48170,.T.);
#64030=ORIENTED_EDGE('',*,*,#48171,.T.);
#64031=ORIENTED_EDGE('',*,*,#48172,.T.);
#64032=ORIENTED_EDGE('',*,*,#48173,.F.);
#64033=ORIENTED_EDGE('',*,*,#48174,.F.);
#64034=ORIENTED_EDGE('',*,*,#48175,.F.);
#64035=ORIENTED_EDGE('',*,*,#48176,.T.);
#64036=ORIENTED_EDGE('',*,*,#48174,.T.);
#64037=ORIENTED_EDGE('',*,*,#48177,.T.);
#64038=ORIENTED_EDGE('',*,*,#48178,.T.);
#64039=ORIENTED_EDGE('',*,*,#48179,.T.);
#64040=ORIENTED_EDGE('',*,*,#48180,.T.);
#64041=ORIENTED_EDGE('',*,*,#48181,.T.);
#64042=ORIENTED_EDGE('',*,*,#48182,.T.);
#64043=ORIENTED_EDGE('',*,*,#48183,.T.);
#64044=ORIENTED_EDGE('',*,*,#48184,.T.);
#64045=ORIENTED_EDGE('',*,*,#48185,.T.);
#64046=ORIENTED_EDGE('',*,*,#48186,.F.);
#64047=ORIENTED_EDGE('',*,*,#48187,.F.);
#64048=ORIENTED_EDGE('',*,*,#48188,.F.);
#64049=ORIENTED_EDGE('',*,*,#48189,.T.);
#64050=ORIENTED_EDGE('',*,*,#48187,.T.);
#64051=ORIENTED_EDGE('',*,*,#48190,.T.);
#64052=ORIENTED_EDGE('',*,*,#48191,.T.);
#64053=ORIENTED_EDGE('',*,*,#48192,.T.);
#64054=ORIENTED_EDGE('',*,*,#46404,.F.);
#64055=ORIENTED_EDGE('',*,*,#48193,.T.);
#64056=ORIENTED_EDGE('',*,*,#48171,.F.);
#64057=ORIENTED_EDGE('',*,*,#48194,.T.);
#64058=ORIENTED_EDGE('',*,*,#48191,.F.);
#64059=ORIENTED_EDGE('',*,*,#48195,.T.);
#64060=ORIENTED_EDGE('',*,*,#45968,.F.);
#64061=ORIENTED_EDGE('',*,*,#48196,.T.);
#64062=ORIENTED_EDGE('',*,*,#48182,.F.);
#64063=ORIENTED_EDGE('',*,*,#48197,.T.);
#64064=ORIENTED_EDGE('',*,*,#48184,.F.);
#64065=ORIENTED_EDGE('',*,*,#48198,.T.);
#64066=ORIENTED_EDGE('',*,*,#48178,.F.);
#64067=ORIENTED_EDGE('',*,*,#48199,.T.);
#64068=ORIENTED_EDGE('',*,*,#48180,.F.);
#64069=ORIENTED_EDGE('',*,*,#48200,.T.);
#64070=ORIENTED_EDGE('',*,*,#48201,.T.);
#64071=ORIENTED_EDGE('',*,*,#48202,.T.);
#64072=ORIENTED_EDGE('',*,*,#48203,.F.);
#64073=ORIENTED_EDGE('',*,*,#48204,.F.);
#64074=ORIENTED_EDGE('',*,*,#48205,.F.);
#64075=ORIENTED_EDGE('',*,*,#48206,.T.);
#64076=ORIENTED_EDGE('',*,*,#48204,.T.);
#64077=ORIENTED_EDGE('',*,*,#48207,.T.);
#64078=ORIENTED_EDGE('',*,*,#48208,.T.);
#64079=ORIENTED_EDGE('',*,*,#48209,.T.);
#64080=ORIENTED_EDGE('',*,*,#48210,.T.);
#64081=ORIENTED_EDGE('',*,*,#48211,.T.);
#64082=ORIENTED_EDGE('',*,*,#48212,.T.);
#64083=ORIENTED_EDGE('',*,*,#48213,.T.);
#64084=ORIENTED_EDGE('',*,*,#48214,.T.);
#64085=ORIENTED_EDGE('',*,*,#48215,.T.);
#64086=ORIENTED_EDGE('',*,*,#48216,.F.);
#64087=ORIENTED_EDGE('',*,*,#48217,.F.);
#64088=ORIENTED_EDGE('',*,*,#48218,.F.);
#64089=ORIENTED_EDGE('',*,*,#48219,.T.);
#64090=ORIENTED_EDGE('',*,*,#48217,.T.);
#64091=ORIENTED_EDGE('',*,*,#48220,.T.);
#64092=ORIENTED_EDGE('',*,*,#48221,.T.);
#64093=ORIENTED_EDGE('',*,*,#48222,.T.);
#64094=ORIENTED_EDGE('',*,*,#46410,.F.);
#64095=ORIENTED_EDGE('',*,*,#48223,.T.);
#64096=ORIENTED_EDGE('',*,*,#48201,.F.);
#64097=ORIENTED_EDGE('',*,*,#48224,.T.);
#64098=ORIENTED_EDGE('',*,*,#48221,.F.);
#64099=ORIENTED_EDGE('',*,*,#48225,.T.);
#64100=ORIENTED_EDGE('',*,*,#45962,.F.);
#64101=ORIENTED_EDGE('',*,*,#48226,.T.);
#64102=ORIENTED_EDGE('',*,*,#48212,.F.);
#64103=ORIENTED_EDGE('',*,*,#48227,.T.);
#64104=ORIENTED_EDGE('',*,*,#48214,.F.);
#64105=ORIENTED_EDGE('',*,*,#48228,.T.);
#64106=ORIENTED_EDGE('',*,*,#48208,.F.);
#64107=ORIENTED_EDGE('',*,*,#48229,.T.);
#64108=ORIENTED_EDGE('',*,*,#48210,.F.);
#64109=ORIENTED_EDGE('',*,*,#48230,.T.);
#64110=ORIENTED_EDGE('',*,*,#48231,.T.);
#64111=ORIENTED_EDGE('',*,*,#48232,.T.);
#64112=ORIENTED_EDGE('',*,*,#48233,.F.);
#64113=ORIENTED_EDGE('',*,*,#48234,.F.);
#64114=ORIENTED_EDGE('',*,*,#48235,.F.);
#64115=ORIENTED_EDGE('',*,*,#48236,.T.);
#64116=ORIENTED_EDGE('',*,*,#48234,.T.);
#64117=ORIENTED_EDGE('',*,*,#48237,.T.);
#64118=ORIENTED_EDGE('',*,*,#48238,.T.);
#64119=ORIENTED_EDGE('',*,*,#48239,.T.);
#64120=ORIENTED_EDGE('',*,*,#48240,.T.);
#64121=ORIENTED_EDGE('',*,*,#48241,.T.);
#64122=ORIENTED_EDGE('',*,*,#48242,.T.);
#64123=ORIENTED_EDGE('',*,*,#48243,.T.);
#64124=ORIENTED_EDGE('',*,*,#48244,.T.);
#64125=ORIENTED_EDGE('',*,*,#48245,.T.);
#64126=ORIENTED_EDGE('',*,*,#48246,.F.);
#64127=ORIENTED_EDGE('',*,*,#48247,.F.);
#64128=ORIENTED_EDGE('',*,*,#48248,.F.);
#64129=ORIENTED_EDGE('',*,*,#48249,.T.);
#64130=ORIENTED_EDGE('',*,*,#48247,.T.);
#64131=ORIENTED_EDGE('',*,*,#48250,.T.);
#64132=ORIENTED_EDGE('',*,*,#48251,.T.);
#64133=ORIENTED_EDGE('',*,*,#48252,.T.);
#64134=ORIENTED_EDGE('',*,*,#46416,.F.);
#64135=ORIENTED_EDGE('',*,*,#48253,.T.);
#64136=ORIENTED_EDGE('',*,*,#48231,.F.);
#64137=ORIENTED_EDGE('',*,*,#48254,.T.);
#64138=ORIENTED_EDGE('',*,*,#48251,.F.);
#64139=ORIENTED_EDGE('',*,*,#48255,.T.);
#64140=ORIENTED_EDGE('',*,*,#45956,.F.);
#64141=ORIENTED_EDGE('',*,*,#48256,.T.);
#64142=ORIENTED_EDGE('',*,*,#48242,.F.);
#64143=ORIENTED_EDGE('',*,*,#48257,.T.);
#64144=ORIENTED_EDGE('',*,*,#48244,.F.);
#64145=ORIENTED_EDGE('',*,*,#48258,.T.);
#64146=ORIENTED_EDGE('',*,*,#48238,.F.);
#64147=ORIENTED_EDGE('',*,*,#48259,.T.);
#64148=ORIENTED_EDGE('',*,*,#48240,.F.);
#64149=ORIENTED_EDGE('',*,*,#48260,.T.);
#64150=ORIENTED_EDGE('',*,*,#48261,.T.);
#64151=ORIENTED_EDGE('',*,*,#48262,.T.);
#64152=ORIENTED_EDGE('',*,*,#48263,.F.);
#64153=ORIENTED_EDGE('',*,*,#48264,.F.);
#64154=ORIENTED_EDGE('',*,*,#48265,.F.);
#64155=ORIENTED_EDGE('',*,*,#48266,.T.);
#64156=ORIENTED_EDGE('',*,*,#48264,.T.);
#64157=ORIENTED_EDGE('',*,*,#48267,.T.);
#64158=ORIENTED_EDGE('',*,*,#48268,.T.);
#64159=ORIENTED_EDGE('',*,*,#48269,.T.);
#64160=ORIENTED_EDGE('',*,*,#48270,.T.);
#64161=ORIENTED_EDGE('',*,*,#48271,.T.);
#64162=ORIENTED_EDGE('',*,*,#48272,.T.);
#64163=ORIENTED_EDGE('',*,*,#48273,.T.);
#64164=ORIENTED_EDGE('',*,*,#48274,.T.);
#64165=ORIENTED_EDGE('',*,*,#48275,.T.);
#64166=ORIENTED_EDGE('',*,*,#48276,.F.);
#64167=ORIENTED_EDGE('',*,*,#48277,.F.);
#64168=ORIENTED_EDGE('',*,*,#48278,.F.);
#64169=ORIENTED_EDGE('',*,*,#48279,.T.);
#64170=ORIENTED_EDGE('',*,*,#48277,.T.);
#64171=ORIENTED_EDGE('',*,*,#48280,.T.);
#64172=ORIENTED_EDGE('',*,*,#48281,.T.);
#64173=ORIENTED_EDGE('',*,*,#48282,.T.);
#64174=ORIENTED_EDGE('',*,*,#46422,.F.);
#64175=ORIENTED_EDGE('',*,*,#48283,.T.);
#64176=ORIENTED_EDGE('',*,*,#48261,.F.);
#64177=ORIENTED_EDGE('',*,*,#48284,.T.);
#64178=ORIENTED_EDGE('',*,*,#48281,.F.);
#64179=ORIENTED_EDGE('',*,*,#48285,.T.);
#64180=ORIENTED_EDGE('',*,*,#45950,.F.);
#64181=ORIENTED_EDGE('',*,*,#48286,.T.);
#64182=ORIENTED_EDGE('',*,*,#48272,.F.);
#64183=ORIENTED_EDGE('',*,*,#48287,.T.);
#64184=ORIENTED_EDGE('',*,*,#48274,.F.);
#64185=ORIENTED_EDGE('',*,*,#48288,.T.);
#64186=ORIENTED_EDGE('',*,*,#48268,.F.);
#64187=ORIENTED_EDGE('',*,*,#48289,.T.);
#64188=ORIENTED_EDGE('',*,*,#48270,.F.);
#64189=ORIENTED_EDGE('',*,*,#48290,.T.);
#64190=ORIENTED_EDGE('',*,*,#48291,.T.);
#64191=ORIENTED_EDGE('',*,*,#48292,.T.);
#64192=ORIENTED_EDGE('',*,*,#48293,.F.);
#64193=ORIENTED_EDGE('',*,*,#48294,.F.);
#64194=ORIENTED_EDGE('',*,*,#48295,.F.);
#64195=ORIENTED_EDGE('',*,*,#48296,.T.);
#64196=ORIENTED_EDGE('',*,*,#48294,.T.);
#64197=ORIENTED_EDGE('',*,*,#48297,.T.);
#64198=ORIENTED_EDGE('',*,*,#48298,.T.);
#64199=ORIENTED_EDGE('',*,*,#48299,.T.);
#64200=ORIENTED_EDGE('',*,*,#48300,.T.);
#64201=ORIENTED_EDGE('',*,*,#48301,.T.);
#64202=ORIENTED_EDGE('',*,*,#48302,.T.);
#64203=ORIENTED_EDGE('',*,*,#48303,.T.);
#64204=ORIENTED_EDGE('',*,*,#48304,.T.);
#64205=ORIENTED_EDGE('',*,*,#48305,.T.);
#64206=ORIENTED_EDGE('',*,*,#48306,.F.);
#64207=ORIENTED_EDGE('',*,*,#48307,.F.);
#64208=ORIENTED_EDGE('',*,*,#48308,.F.);
#64209=ORIENTED_EDGE('',*,*,#48309,.T.);
#64210=ORIENTED_EDGE('',*,*,#48307,.T.);
#64211=ORIENTED_EDGE('',*,*,#48310,.T.);
#64212=ORIENTED_EDGE('',*,*,#48311,.T.);
#64213=ORIENTED_EDGE('',*,*,#48312,.T.);
#64214=ORIENTED_EDGE('',*,*,#46428,.F.);
#64215=ORIENTED_EDGE('',*,*,#48313,.T.);
#64216=ORIENTED_EDGE('',*,*,#48291,.F.);
#64217=ORIENTED_EDGE('',*,*,#48314,.T.);
#64218=ORIENTED_EDGE('',*,*,#48311,.F.);
#64219=ORIENTED_EDGE('',*,*,#48315,.T.);
#64220=ORIENTED_EDGE('',*,*,#45944,.F.);
#64221=ORIENTED_EDGE('',*,*,#48316,.T.);
#64222=ORIENTED_EDGE('',*,*,#48302,.F.);
#64223=ORIENTED_EDGE('',*,*,#48317,.T.);
#64224=ORIENTED_EDGE('',*,*,#48304,.F.);
#64225=ORIENTED_EDGE('',*,*,#48318,.T.);
#64226=ORIENTED_EDGE('',*,*,#48298,.F.);
#64227=ORIENTED_EDGE('',*,*,#48319,.T.);
#64228=ORIENTED_EDGE('',*,*,#48300,.F.);
#64229=ORIENTED_EDGE('',*,*,#48320,.T.);
#64230=ORIENTED_EDGE('',*,*,#48321,.T.);
#64231=ORIENTED_EDGE('',*,*,#48322,.T.);
#64232=ORIENTED_EDGE('',*,*,#48323,.F.);
#64233=ORIENTED_EDGE('',*,*,#48324,.F.);
#64234=ORIENTED_EDGE('',*,*,#48325,.F.);
#64235=ORIENTED_EDGE('',*,*,#48326,.T.);
#64236=ORIENTED_EDGE('',*,*,#48324,.T.);
#64237=ORIENTED_EDGE('',*,*,#48327,.T.);
#64238=ORIENTED_EDGE('',*,*,#48328,.T.);
#64239=ORIENTED_EDGE('',*,*,#48329,.T.);
#64240=ORIENTED_EDGE('',*,*,#48330,.T.);
#64241=ORIENTED_EDGE('',*,*,#48331,.T.);
#64242=ORIENTED_EDGE('',*,*,#48332,.T.);
#64243=ORIENTED_EDGE('',*,*,#48333,.T.);
#64244=ORIENTED_EDGE('',*,*,#48334,.T.);
#64245=ORIENTED_EDGE('',*,*,#48335,.T.);
#64246=ORIENTED_EDGE('',*,*,#48336,.F.);
#64247=ORIENTED_EDGE('',*,*,#48337,.F.);
#64248=ORIENTED_EDGE('',*,*,#48338,.F.);
#64249=ORIENTED_EDGE('',*,*,#48339,.T.);
#64250=ORIENTED_EDGE('',*,*,#48337,.T.);
#64251=ORIENTED_EDGE('',*,*,#48340,.T.);
#64252=ORIENTED_EDGE('',*,*,#48341,.T.);
#64253=ORIENTED_EDGE('',*,*,#48342,.T.);
#64254=ORIENTED_EDGE('',*,*,#46434,.F.);
#64255=ORIENTED_EDGE('',*,*,#48343,.T.);
#64256=ORIENTED_EDGE('',*,*,#48321,.F.);
#64257=ORIENTED_EDGE('',*,*,#48344,.T.);
#64258=ORIENTED_EDGE('',*,*,#48341,.F.);
#64259=ORIENTED_EDGE('',*,*,#48345,.T.);
#64260=ORIENTED_EDGE('',*,*,#45938,.F.);
#64261=ORIENTED_EDGE('',*,*,#48346,.T.);
#64262=ORIENTED_EDGE('',*,*,#48332,.F.);
#64263=ORIENTED_EDGE('',*,*,#48347,.T.);
#64264=ORIENTED_EDGE('',*,*,#48334,.F.);
#64265=ORIENTED_EDGE('',*,*,#48348,.T.);
#64266=ORIENTED_EDGE('',*,*,#48328,.F.);
#64267=ORIENTED_EDGE('',*,*,#48349,.T.);
#64268=ORIENTED_EDGE('',*,*,#48330,.F.);
#64269=ORIENTED_EDGE('',*,*,#48350,.T.);
#64270=ORIENTED_EDGE('',*,*,#48351,.T.);
#64271=ORIENTED_EDGE('',*,*,#48352,.T.);
#64272=ORIENTED_EDGE('',*,*,#48353,.F.);
#64273=ORIENTED_EDGE('',*,*,#48354,.F.);
#64274=ORIENTED_EDGE('',*,*,#48355,.F.);
#64275=ORIENTED_EDGE('',*,*,#48356,.T.);
#64276=ORIENTED_EDGE('',*,*,#48354,.T.);
#64277=ORIENTED_EDGE('',*,*,#48357,.T.);
#64278=ORIENTED_EDGE('',*,*,#48358,.T.);
#64279=ORIENTED_EDGE('',*,*,#48359,.T.);
#64280=ORIENTED_EDGE('',*,*,#48360,.T.);
#64281=ORIENTED_EDGE('',*,*,#48361,.T.);
#64282=ORIENTED_EDGE('',*,*,#48362,.T.);
#64283=ORIENTED_EDGE('',*,*,#48363,.T.);
#64284=ORIENTED_EDGE('',*,*,#48364,.T.);
#64285=ORIENTED_EDGE('',*,*,#48365,.T.);
#64286=ORIENTED_EDGE('',*,*,#48366,.F.);
#64287=ORIENTED_EDGE('',*,*,#48367,.F.);
#64288=ORIENTED_EDGE('',*,*,#48368,.F.);
#64289=ORIENTED_EDGE('',*,*,#48369,.T.);
#64290=ORIENTED_EDGE('',*,*,#48367,.T.);
#64291=ORIENTED_EDGE('',*,*,#48370,.T.);
#64292=ORIENTED_EDGE('',*,*,#48371,.T.);
#64293=ORIENTED_EDGE('',*,*,#48372,.T.);
#64294=ORIENTED_EDGE('',*,*,#46440,.F.);
#64295=ORIENTED_EDGE('',*,*,#48373,.T.);
#64296=ORIENTED_EDGE('',*,*,#48351,.F.);
#64297=ORIENTED_EDGE('',*,*,#48374,.T.);
#64298=ORIENTED_EDGE('',*,*,#48371,.F.);
#64299=ORIENTED_EDGE('',*,*,#48375,.T.);
#64300=ORIENTED_EDGE('',*,*,#45932,.F.);
#64301=ORIENTED_EDGE('',*,*,#48376,.T.);
#64302=ORIENTED_EDGE('',*,*,#48362,.F.);
#64303=ORIENTED_EDGE('',*,*,#48377,.T.);
#64304=ORIENTED_EDGE('',*,*,#48364,.F.);
#64305=ORIENTED_EDGE('',*,*,#48378,.T.);
#64306=ORIENTED_EDGE('',*,*,#48358,.F.);
#64307=ORIENTED_EDGE('',*,*,#48379,.T.);
#64308=ORIENTED_EDGE('',*,*,#48360,.F.);
#64309=ORIENTED_EDGE('',*,*,#48380,.T.);
#64310=ORIENTED_EDGE('',*,*,#48381,.T.);
#64311=ORIENTED_EDGE('',*,*,#48382,.T.);
#64312=ORIENTED_EDGE('',*,*,#48383,.F.);
#64313=ORIENTED_EDGE('',*,*,#48384,.F.);
#64314=ORIENTED_EDGE('',*,*,#48385,.F.);
#64315=ORIENTED_EDGE('',*,*,#48386,.T.);
#64316=ORIENTED_EDGE('',*,*,#48384,.T.);
#64317=ORIENTED_EDGE('',*,*,#48387,.T.);
#64318=ORIENTED_EDGE('',*,*,#48388,.T.);
#64319=ORIENTED_EDGE('',*,*,#48389,.T.);
#64320=ORIENTED_EDGE('',*,*,#48390,.T.);
#64321=ORIENTED_EDGE('',*,*,#48391,.T.);
#64322=ORIENTED_EDGE('',*,*,#48392,.T.);
#64323=ORIENTED_EDGE('',*,*,#48393,.T.);
#64324=ORIENTED_EDGE('',*,*,#48394,.T.);
#64325=ORIENTED_EDGE('',*,*,#48395,.T.);
#64326=ORIENTED_EDGE('',*,*,#48396,.F.);
#64327=ORIENTED_EDGE('',*,*,#48397,.F.);
#64328=ORIENTED_EDGE('',*,*,#48398,.F.);
#64329=ORIENTED_EDGE('',*,*,#48399,.T.);
#64330=ORIENTED_EDGE('',*,*,#48397,.T.);
#64331=ORIENTED_EDGE('',*,*,#48400,.T.);
#64332=ORIENTED_EDGE('',*,*,#48401,.T.);
#64333=ORIENTED_EDGE('',*,*,#48402,.T.);
#64334=ORIENTED_EDGE('',*,*,#46446,.F.);
#64335=ORIENTED_EDGE('',*,*,#48403,.T.);
#64336=ORIENTED_EDGE('',*,*,#48381,.F.);
#64337=ORIENTED_EDGE('',*,*,#48404,.T.);
#64338=ORIENTED_EDGE('',*,*,#48401,.F.);
#64339=ORIENTED_EDGE('',*,*,#48405,.T.);
#64340=ORIENTED_EDGE('',*,*,#45926,.F.);
#64341=ORIENTED_EDGE('',*,*,#48406,.T.);
#64342=ORIENTED_EDGE('',*,*,#48392,.F.);
#64343=ORIENTED_EDGE('',*,*,#48407,.T.);
#64344=ORIENTED_EDGE('',*,*,#48394,.F.);
#64345=ORIENTED_EDGE('',*,*,#48408,.T.);
#64346=ORIENTED_EDGE('',*,*,#48388,.F.);
#64347=ORIENTED_EDGE('',*,*,#48409,.T.);
#64348=ORIENTED_EDGE('',*,*,#48390,.F.);
#64349=ORIENTED_EDGE('',*,*,#48410,.T.);
#64350=ORIENTED_EDGE('',*,*,#45905,.T.);
#64351=ORIENTED_EDGE('',*,*,#45899,.T.);
#64352=ORIENTED_EDGE('',*,*,#48411,.T.);
#64353=ORIENTED_EDGE('',*,*,#48412,.T.);
#64354=ORIENTED_EDGE('',*,*,#48413,.F.);
#64355=ORIENTED_EDGE('',*,*,#48414,.F.);
#64356=ORIENTED_EDGE('',*,*,#48415,.F.);
#64357=ORIENTED_EDGE('',*,*,#48416,.T.);
#64358=ORIENTED_EDGE('',*,*,#48414,.T.);
#64359=ORIENTED_EDGE('',*,*,#48417,.T.);
#64360=ORIENTED_EDGE('',*,*,#48418,.T.);
#64361=ORIENTED_EDGE('',*,*,#48419,.T.);
#64362=ORIENTED_EDGE('',*,*,#48420,.T.);
#64363=ORIENTED_EDGE('',*,*,#48421,.T.);
#64364=ORIENTED_EDGE('',*,*,#48422,.T.);
#64365=ORIENTED_EDGE('',*,*,#48423,.T.);
#64366=ORIENTED_EDGE('',*,*,#48424,.T.);
#64367=ORIENTED_EDGE('',*,*,#48425,.T.);
#64368=ORIENTED_EDGE('',*,*,#48426,.F.);
#64369=ORIENTED_EDGE('',*,*,#48427,.F.);
#64370=ORIENTED_EDGE('',*,*,#48428,.F.);
#64371=ORIENTED_EDGE('',*,*,#48429,.T.);
#64372=ORIENTED_EDGE('',*,*,#48427,.T.);
#64373=ORIENTED_EDGE('',*,*,#48430,.T.);
#64374=ORIENTED_EDGE('',*,*,#48431,.T.);
#64375=ORIENTED_EDGE('',*,*,#48432,.T.);
#64376=ORIENTED_EDGE('',*,*,#45912,.T.);
#64377=ORIENTED_EDGE('',*,*,#45906,.T.);
#64378=ORIENTED_EDGE('',*,*,#45913,.T.);
#64379=ORIENTED_EDGE('',*,*,#46640,.F.);
#64380=ORIENTED_EDGE('',*,*,#46452,.F.);
#64381=ORIENTED_EDGE('',*,*,#48433,.T.);
#64382=ORIENTED_EDGE('',*,*,#48411,.F.);
#64383=ORIENTED_EDGE('',*,*,#48434,.T.);
#64384=ORIENTED_EDGE('',*,*,#48431,.F.);
#64385=ORIENTED_EDGE('',*,*,#48435,.T.);
#64386=ORIENTED_EDGE('',*,*,#45920,.F.);
#64387=ORIENTED_EDGE('',*,*,#48436,.T.);
#64388=ORIENTED_EDGE('',*,*,#48422,.F.);
#64389=ORIENTED_EDGE('',*,*,#48437,.T.);
#64390=ORIENTED_EDGE('',*,*,#48424,.F.);
#64391=ORIENTED_EDGE('',*,*,#48438,.T.);
#64392=ORIENTED_EDGE('',*,*,#48418,.F.);
#64393=ORIENTED_EDGE('',*,*,#48439,.T.);
#64394=ORIENTED_EDGE('',*,*,#48420,.F.);
#64395=ORIENTED_EDGE('',*,*,#48440,.T.);
#64396=ORIENTED_EDGE('',*,*,#48441,.T.);
#64397=ORIENTED_EDGE('',*,*,#48442,.T.);
#64398=ORIENTED_EDGE('',*,*,#48443,.T.);
#64399=ORIENTED_EDGE('',*,*,#48444,.T.);
#64400=ORIENTED_EDGE('',*,*,#48445,.T.);
#64401=ORIENTED_EDGE('',*,*,#48446,.T.);
#64402=ORIENTED_EDGE('',*,*,#48447,.T.);
#64403=ORIENTED_EDGE('',*,*,#48448,.T.);
#64404=ORIENTED_EDGE('',*,*,#48449,.T.);
#64405=ORIENTED_EDGE('',*,*,#48450,.T.);
#64406=ORIENTED_EDGE('',*,*,#48451,.T.);
#64407=ORIENTED_EDGE('',*,*,#48452,.T.);
#64408=ORIENTED_EDGE('',*,*,#48453,.T.);
#64409=ORIENTED_EDGE('',*,*,#48454,.T.);
#64410=ORIENTED_EDGE('',*,*,#48455,.T.);
#64411=ORIENTED_EDGE('',*,*,#48456,.T.);
#64412=ORIENTED_EDGE('',*,*,#48457,.T.);
#64413=ORIENTED_EDGE('',*,*,#48458,.T.);
#64414=ORIENTED_EDGE('',*,*,#48459,.T.);
#64415=ORIENTED_EDGE('',*,*,#48460,.T.);
#64416=ORIENTED_EDGE('',*,*,#48461,.T.);
#64417=ORIENTED_EDGE('',*,*,#48462,.T.);
#64418=ORIENTED_EDGE('',*,*,#48463,.T.);
#64419=ORIENTED_EDGE('',*,*,#48464,.T.);
#64420=ORIENTED_EDGE('',*,*,#48465,.T.);
#64421=ORIENTED_EDGE('',*,*,#48466,.T.);
#64422=ORIENTED_EDGE('',*,*,#48467,.T.);
#64423=ORIENTED_EDGE('',*,*,#48468,.T.);
#64424=ORIENTED_EDGE('',*,*,#48459,.F.);
#64425=ORIENTED_EDGE('',*,*,#48469,.T.);
#64426=ORIENTED_EDGE('',*,*,#48441,.F.);
#64427=ORIENTED_EDGE('',*,*,#48470,.T.);
#64428=ORIENTED_EDGE('',*,*,#48443,.F.);
#64429=ORIENTED_EDGE('',*,*,#48471,.T.);
#64430=ORIENTED_EDGE('',*,*,#48447,.F.);
#64431=ORIENTED_EDGE('',*,*,#48472,.T.);
#64432=ORIENTED_EDGE('',*,*,#48473,.F.);
#64433=ORIENTED_EDGE('',*,*,#48467,.F.);
#64434=ORIENTED_EDGE('',*,*,#48474,.F.);
#64435=ORIENTED_EDGE('',*,*,#48429,.F.);
#64436=ORIENTED_EDGE('',*,*,#48474,.T.);
#64437=ORIENTED_EDGE('',*,*,#48466,.F.);
#64438=ORIENTED_EDGE('',*,*,#48475,.F.);
#64439=ORIENTED_EDGE('',*,*,#48438,.F.);
#64440=ORIENTED_EDGE('',*,*,#48428,.T.);
#64441=ORIENTED_EDGE('',*,*,#48432,.F.);
#64442=ORIENTED_EDGE('',*,*,#48476,.F.);
#64443=ORIENTED_EDGE('',*,*,#48468,.F.);
#64444=ORIENTED_EDGE('',*,*,#48473,.T.);
#64445=ORIENTED_EDGE('',*,*,#48475,.T.);
#64446=ORIENTED_EDGE('',*,*,#48465,.F.);
#64447=ORIENTED_EDGE('',*,*,#48477,.F.);
#64448=ORIENTED_EDGE('',*,*,#48423,.F.);
#64449=ORIENTED_EDGE('',*,*,#48476,.T.);
#64450=ORIENTED_EDGE('',*,*,#48436,.F.);
#64451=ORIENTED_EDGE('',*,*,#48478,.F.);
#64452=ORIENTED_EDGE('',*,*,#48457,.F.);
#64453=ORIENTED_EDGE('',*,*,#48477,.T.);
#64454=ORIENTED_EDGE('',*,*,#48464,.F.);
#64455=ORIENTED_EDGE('',*,*,#48479,.F.);
#64456=ORIENTED_EDGE('',*,*,#48440,.F.);
#64457=ORIENTED_EDGE('',*,*,#48478,.T.);
#64458=ORIENTED_EDGE('',*,*,#45919,.F.);
#64459=ORIENTED_EDGE('',*,*,#48480,.F.);
#64460=ORIENTED_EDGE('',*,*,#48458,.F.);
#64461=ORIENTED_EDGE('',*,*,#48479,.T.);
#64462=ORIENTED_EDGE('',*,*,#48463,.F.);
#64463=ORIENTED_EDGE('',*,*,#48481,.F.);
#64464=ORIENTED_EDGE('',*,*,#48415,.T.);
#64465=ORIENTED_EDGE('',*,*,#48419,.F.);
#64466=ORIENTED_EDGE('',*,*,#48480,.T.);
#64467=ORIENTED_EDGE('',*,*,#45918,.F.);
#64468=ORIENTED_EDGE('',*,*,#48482,.F.);
#64469=ORIENTED_EDGE('',*,*,#48469,.F.);
#64470=ORIENTED_EDGE('',*,*,#48481,.T.);
#64471=ORIENTED_EDGE('',*,*,#48462,.F.);
#64472=ORIENTED_EDGE('',*,*,#48483,.F.);
#64473=ORIENTED_EDGE('',*,*,#48416,.F.);
#64474=ORIENTED_EDGE('',*,*,#48482,.T.);
#64475=ORIENTED_EDGE('',*,*,#45917,.F.);
#64476=ORIENTED_EDGE('',*,*,#48484,.F.);
#64477=ORIENTED_EDGE('',*,*,#48442,.F.);
#64478=ORIENTED_EDGE('',*,*,#48483,.T.);
#64479=ORIENTED_EDGE('',*,*,#48461,.F.);
#64480=ORIENTED_EDGE('',*,*,#48485,.F.);
#64481=ORIENTED_EDGE('',*,*,#48434,.F.);
#64482=ORIENTED_EDGE('',*,*,#48484,.T.);
#64483=ORIENTED_EDGE('',*,*,#46275,.F.);
#64484=ORIENTED_EDGE('',*,*,#48486,.F.);
#64485=ORIENTED_EDGE('',*,*,#48471,.F.);
#64486=ORIENTED_EDGE('',*,*,#48485,.T.);
#64487=ORIENTED_EDGE('',*,*,#48460,.F.);
#64488=ORIENTED_EDGE('',*,*,#48487,.F.);
#64489=ORIENTED_EDGE('',*,*,#46453,.F.);
#64490=ORIENTED_EDGE('',*,*,#48486,.T.);
#64491=ORIENTED_EDGE('',*,*,#46274,.F.);
#64492=ORIENTED_EDGE('',*,*,#48488,.F.);
#64493=ORIENTED_EDGE('',*,*,#48448,.F.);
#64494=ORIENTED_EDGE('',*,*,#48487,.T.);
#64495=ORIENTED_EDGE('',*,*,#48470,.F.);
#64496=ORIENTED_EDGE('',*,*,#48489,.F.);
#64497=ORIENTED_EDGE('',*,*,#46454,.F.);
#64498=ORIENTED_EDGE('',*,*,#48488,.T.);
#64499=ORIENTED_EDGE('',*,*,#46666,.F.);
#64500=ORIENTED_EDGE('',*,*,#48490,.F.);
#64501=ORIENTED_EDGE('',*,*,#48449,.F.);
#64502=ORIENTED_EDGE('',*,*,#48489,.T.);
#64503=ORIENTED_EDGE('',*,*,#48444,.F.);
#64504=ORIENTED_EDGE('',*,*,#48491,.F.);
#64505=ORIENTED_EDGE('',*,*,#46457,.F.);
#64506=ORIENTED_EDGE('',*,*,#46455,.F.);
#64507=ORIENTED_EDGE('',*,*,#46662,.F.);
#64508=ORIENTED_EDGE('',*,*,#46658,.T.);
#64509=ORIENTED_EDGE('',*,*,#48492,.F.);
#64510=ORIENTED_EDGE('',*,*,#48450,.F.);
#64511=ORIENTED_EDGE('',*,*,#48490,.T.);
#64512=ORIENTED_EDGE('',*,*,#48491,.T.);
#64513=ORIENTED_EDGE('',*,*,#48472,.F.);
#64514=ORIENTED_EDGE('',*,*,#48493,.F.);
#64515=ORIENTED_EDGE('',*,*,#46458,.F.);
#64516=ORIENTED_EDGE('',*,*,#48492,.T.);
#64517=ORIENTED_EDGE('',*,*,#46657,.F.);
#64518=ORIENTED_EDGE('',*,*,#48494,.F.);
#64519=ORIENTED_EDGE('',*,*,#48451,.F.);
#64520=ORIENTED_EDGE('',*,*,#48493,.T.);
#64521=ORIENTED_EDGE('',*,*,#48446,.F.);
#64522=ORIENTED_EDGE('',*,*,#48495,.F.);
#64523=ORIENTED_EDGE('',*,*,#46459,.F.);
#64524=ORIENTED_EDGE('',*,*,#48494,.T.);
#64525=ORIENTED_EDGE('',*,*,#46668,.F.);
#64526=ORIENTED_EDGE('',*,*,#48496,.F.);
#64527=ORIENTED_EDGE('',*,*,#48452,.F.);
#64528=ORIENTED_EDGE('',*,*,#48495,.T.);
#64529=ORIENTED_EDGE('',*,*,#48445,.F.);
#64530=ORIENTED_EDGE('',*,*,#48497,.F.);
#64531=ORIENTED_EDGE('',*,*,#46664,.F.);
#64532=ORIENTED_EDGE('',*,*,#48496,.T.);
#64533=ORIENTED_EDGE('',*,*,#46653,.F.);
#64534=ORIENTED_EDGE('',*,*,#48498,.F.);
#64535=ORIENTED_EDGE('',*,*,#48453,.F.);
#64536=ORIENTED_EDGE('',*,*,#48497,.T.);
#64537=ORIENTED_EDGE('',*,*,#48456,.F.);
#64538=ORIENTED_EDGE('',*,*,#48499,.F.);
#64539=ORIENTED_EDGE('',*,*,#46644,.F.);
#64540=ORIENTED_EDGE('',*,*,#48498,.T.);
#64541=ORIENTED_EDGE('',*,*,#46670,.F.);
#64542=ORIENTED_EDGE('',*,*,#48500,.F.);
#64543=ORIENTED_EDGE('',*,*,#48454,.F.);
#64544=ORIENTED_EDGE('',*,*,#48499,.T.);
#64545=ORIENTED_EDGE('',*,*,#48455,.F.);
#64546=ORIENTED_EDGE('',*,*,#48500,.T.);
#64547=ORIENTED_EDGE('',*,*,#46649,.F.);
#64548=ORIENTED_EDGE('',*,*,#46645,.T.);
#64549=ORIENTED_EDGE('',*,*,#48501,.T.);
#64550=ORIENTED_EDGE('',*,*,#48502,.T.);
#64551=ORIENTED_EDGE('',*,*,#48503,.T.);
#64552=ORIENTED_EDGE('',*,*,#48504,.T.);
#64553=ORIENTED_EDGE('',*,*,#48505,.T.);
#64554=ORIENTED_EDGE('',*,*,#48506,.T.);
#64555=ORIENTED_EDGE('',*,*,#48507,.T.);
#64556=ORIENTED_EDGE('',*,*,#48508,.T.);
#64557=ORIENTED_EDGE('',*,*,#48509,.T.);
#64558=ORIENTED_EDGE('',*,*,#48510,.T.);
#64559=ORIENTED_EDGE('',*,*,#48511,.T.);
#64560=ORIENTED_EDGE('',*,*,#48512,.T.);
#64561=ORIENTED_EDGE('',*,*,#48513,.T.);
#64562=ORIENTED_EDGE('',*,*,#48514,.T.);
#64563=ORIENTED_EDGE('',*,*,#48515,.T.);
#64564=ORIENTED_EDGE('',*,*,#48516,.T.);
#64565=ORIENTED_EDGE('',*,*,#48517,.T.);
#64566=ORIENTED_EDGE('',*,*,#48518,.T.);
#64567=ORIENTED_EDGE('',*,*,#48519,.T.);
#64568=ORIENTED_EDGE('',*,*,#48520,.T.);
#64569=ORIENTED_EDGE('',*,*,#48521,.T.);
#64570=ORIENTED_EDGE('',*,*,#48522,.T.);
#64571=ORIENTED_EDGE('',*,*,#48523,.T.);
#64572=ORIENTED_EDGE('',*,*,#48524,.T.);
#64573=ORIENTED_EDGE('',*,*,#48525,.T.);
#64574=ORIENTED_EDGE('',*,*,#48526,.T.);
#64575=ORIENTED_EDGE('',*,*,#48527,.T.);
#64576=ORIENTED_EDGE('',*,*,#48528,.T.);
#64577=ORIENTED_EDGE('',*,*,#48529,.T.);
#64578=ORIENTED_EDGE('',*,*,#48530,.T.);
#64579=ORIENTED_EDGE('',*,*,#48531,.T.);
#64580=ORIENTED_EDGE('',*,*,#48532,.T.);
#64581=ORIENTED_EDGE('',*,*,#48533,.T.);
#64582=ORIENTED_EDGE('',*,*,#48534,.T.);
#64583=ORIENTED_EDGE('',*,*,#48535,.T.);
#64584=ORIENTED_EDGE('',*,*,#48536,.T.);
#64585=ORIENTED_EDGE('',*,*,#48537,.T.);
#64586=ORIENTED_EDGE('',*,*,#48538,.T.);
#64587=ORIENTED_EDGE('',*,*,#48539,.T.);
#64588=ORIENTED_EDGE('',*,*,#48540,.T.);
#64589=ORIENTED_EDGE('',*,*,#48541,.T.);
#64590=ORIENTED_EDGE('',*,*,#48542,.T.);
#64591=ORIENTED_EDGE('',*,*,#48543,.T.);
#64592=ORIENTED_EDGE('',*,*,#48544,.T.);
#64593=ORIENTED_EDGE('',*,*,#48545,.T.);
#64594=ORIENTED_EDGE('',*,*,#48546,.T.);
#64595=ORIENTED_EDGE('',*,*,#48547,.T.);
#64596=ORIENTED_EDGE('',*,*,#48548,.T.);
#64597=ORIENTED_EDGE('',*,*,#48549,.T.);
#64598=ORIENTED_EDGE('',*,*,#48550,.T.);
#64599=ORIENTED_EDGE('',*,*,#48551,.T.);
#64600=ORIENTED_EDGE('',*,*,#48552,.T.);
#64601=ORIENTED_EDGE('',*,*,#48553,.T.);
#64602=ORIENTED_EDGE('',*,*,#48554,.T.);
#64603=ORIENTED_EDGE('',*,*,#48555,.T.);
#64604=ORIENTED_EDGE('',*,*,#48556,.T.);
#64605=ORIENTED_EDGE('',*,*,#48557,.T.);
#64606=ORIENTED_EDGE('',*,*,#48558,.T.);
#64607=ORIENTED_EDGE('',*,*,#48559,.T.);
#64608=ORIENTED_EDGE('',*,*,#48560,.T.);
#64609=ORIENTED_EDGE('',*,*,#48561,.T.);
#64610=ORIENTED_EDGE('',*,*,#48562,.T.);
#64611=ORIENTED_EDGE('',*,*,#48563,.T.);
#64612=ORIENTED_EDGE('',*,*,#48564,.T.);
#64613=ORIENTED_EDGE('',*,*,#48565,.T.);
#64614=ORIENTED_EDGE('',*,*,#48566,.T.);
#64615=ORIENTED_EDGE('',*,*,#48567,.T.);
#64616=ORIENTED_EDGE('',*,*,#48568,.T.);
#64617=ORIENTED_EDGE('',*,*,#48569,.T.);
#64618=ORIENTED_EDGE('',*,*,#48570,.T.);
#64619=ORIENTED_EDGE('',*,*,#48571,.T.);
#64620=ORIENTED_EDGE('',*,*,#48572,.T.);
#64621=ORIENTED_EDGE('',*,*,#48573,.T.);
#64622=ORIENTED_EDGE('',*,*,#48574,.T.);
#64623=ORIENTED_EDGE('',*,*,#48575,.T.);
#64624=ORIENTED_EDGE('',*,*,#48576,.T.);
#64625=ORIENTED_EDGE('',*,*,#48577,.T.);
#64626=ORIENTED_EDGE('',*,*,#48578,.T.);
#64627=ORIENTED_EDGE('',*,*,#48579,.T.);
#64628=ORIENTED_EDGE('',*,*,#48580,.T.);
#64629=ORIENTED_EDGE('',*,*,#48581,.T.);
#64630=ORIENTED_EDGE('',*,*,#48582,.T.);
#64631=ORIENTED_EDGE('',*,*,#48583,.T.);
#64632=ORIENTED_EDGE('',*,*,#48584,.T.);
#64633=ORIENTED_EDGE('',*,*,#48585,.T.);
#64634=ORIENTED_EDGE('',*,*,#48586,.T.);
#64635=ORIENTED_EDGE('',*,*,#48587,.T.);
#64636=ORIENTED_EDGE('',*,*,#48588,.T.);
#64637=ORIENTED_EDGE('',*,*,#48589,.T.);
#64638=ORIENTED_EDGE('',*,*,#48590,.T.);
#64639=ORIENTED_EDGE('',*,*,#48591,.T.);
#64640=ORIENTED_EDGE('',*,*,#48592,.T.);
#64641=ORIENTED_EDGE('',*,*,#48593,.T.);
#64642=ORIENTED_EDGE('',*,*,#48594,.T.);
#64643=ORIENTED_EDGE('',*,*,#48595,.T.);
#64644=ORIENTED_EDGE('',*,*,#48596,.T.);
#64645=ORIENTED_EDGE('',*,*,#48597,.T.);
#64646=ORIENTED_EDGE('',*,*,#48598,.T.);
#64647=ORIENTED_EDGE('',*,*,#48599,.T.);
#64648=ORIENTED_EDGE('',*,*,#48600,.T.);
#64649=ORIENTED_EDGE('',*,*,#48601,.T.);
#64650=ORIENTED_EDGE('',*,*,#48602,.T.);
#64651=ORIENTED_EDGE('',*,*,#48603,.T.);
#64652=ORIENTED_EDGE('',*,*,#48604,.T.);
#64653=ORIENTED_EDGE('',*,*,#48605,.T.);
#64654=ORIENTED_EDGE('',*,*,#48606,.T.);
#64655=ORIENTED_EDGE('',*,*,#48607,.T.);
#64656=ORIENTED_EDGE('',*,*,#48608,.T.);
#64657=ORIENTED_EDGE('',*,*,#48609,.T.);
#64658=ORIENTED_EDGE('',*,*,#48610,.T.);
#64659=ORIENTED_EDGE('',*,*,#48611,.T.);
#64660=ORIENTED_EDGE('',*,*,#48612,.T.);
#64661=ORIENTED_EDGE('',*,*,#48613,.T.);
#64662=ORIENTED_EDGE('',*,*,#48614,.T.);
#64663=ORIENTED_EDGE('',*,*,#48615,.T.);
#64664=ORIENTED_EDGE('',*,*,#48616,.T.);
#64665=ORIENTED_EDGE('',*,*,#48617,.T.);
#64666=ORIENTED_EDGE('',*,*,#48618,.T.);
#64667=ORIENTED_EDGE('',*,*,#48619,.T.);
#64668=ORIENTED_EDGE('',*,*,#48620,.T.);
#64669=ORIENTED_EDGE('',*,*,#48621,.T.);
#64670=ORIENTED_EDGE('',*,*,#48622,.T.);
#64671=ORIENTED_EDGE('',*,*,#48623,.T.);
#64672=ORIENTED_EDGE('',*,*,#48624,.T.);
#64673=ORIENTED_EDGE('',*,*,#48625,.T.);
#64674=ORIENTED_EDGE('',*,*,#48626,.T.);
#64675=ORIENTED_EDGE('',*,*,#48627,.T.);
#64676=ORIENTED_EDGE('',*,*,#48628,.T.);
#64677=ORIENTED_EDGE('',*,*,#48629,.T.);
#64678=ORIENTED_EDGE('',*,*,#48630,.T.);
#64679=ORIENTED_EDGE('',*,*,#48631,.T.);
#64680=ORIENTED_EDGE('',*,*,#48632,.T.);
#64681=ORIENTED_EDGE('',*,*,#48633,.T.);
#64682=ORIENTED_EDGE('',*,*,#48634,.T.);
#64683=ORIENTED_EDGE('',*,*,#48635,.T.);
#64684=ORIENTED_EDGE('',*,*,#48636,.T.);
#64685=ORIENTED_EDGE('',*,*,#48637,.T.);
#64686=ORIENTED_EDGE('',*,*,#48638,.T.);
#64687=ORIENTED_EDGE('',*,*,#48639,.T.);
#64688=ORIENTED_EDGE('',*,*,#48640,.T.);
#64689=ORIENTED_EDGE('',*,*,#48641,.T.);
#64690=ORIENTED_EDGE('',*,*,#48642,.T.);
#64691=ORIENTED_EDGE('',*,*,#48643,.T.);
#64692=ORIENTED_EDGE('',*,*,#48644,.T.);
#64693=ORIENTED_EDGE('',*,*,#48645,.T.);
#64694=ORIENTED_EDGE('',*,*,#48646,.T.);
#64695=ORIENTED_EDGE('',*,*,#48647,.T.);
#64696=ORIENTED_EDGE('',*,*,#48648,.T.);
#64697=ORIENTED_EDGE('',*,*,#48649,.T.);
#64698=ORIENTED_EDGE('',*,*,#48650,.T.);
#64699=ORIENTED_EDGE('',*,*,#48651,.T.);
#64700=ORIENTED_EDGE('',*,*,#48652,.T.);
#64701=ORIENTED_EDGE('',*,*,#48653,.T.);
#64702=ORIENTED_EDGE('',*,*,#48654,.T.);
#64703=ORIENTED_EDGE('',*,*,#48655,.T.);
#64704=ORIENTED_EDGE('',*,*,#48656,.T.);
#64705=ORIENTED_EDGE('',*,*,#48657,.T.);
#64706=ORIENTED_EDGE('',*,*,#48658,.T.);
#64707=ORIENTED_EDGE('',*,*,#48659,.T.);
#64708=ORIENTED_EDGE('',*,*,#48660,.T.);
#64709=ORIENTED_EDGE('',*,*,#48661,.T.);
#64710=ORIENTED_EDGE('',*,*,#48662,.T.);
#64711=ORIENTED_EDGE('',*,*,#48663,.T.);
#64712=ORIENTED_EDGE('',*,*,#48664,.T.);
#64713=ORIENTED_EDGE('',*,*,#48665,.T.);
#64714=ORIENTED_EDGE('',*,*,#48666,.T.);
#64715=ORIENTED_EDGE('',*,*,#48667,.T.);
#64716=ORIENTED_EDGE('',*,*,#48668,.T.);
#64717=ORIENTED_EDGE('',*,*,#48669,.T.);
#64718=ORIENTED_EDGE('',*,*,#48670,.T.);
#64719=ORIENTED_EDGE('',*,*,#48671,.T.);
#64720=ORIENTED_EDGE('',*,*,#48672,.T.);
#64721=ORIENTED_EDGE('',*,*,#48673,.T.);
#64722=ORIENTED_EDGE('',*,*,#48674,.T.);
#64723=ORIENTED_EDGE('',*,*,#48675,.T.);
#64724=ORIENTED_EDGE('',*,*,#48676,.T.);
#64725=ORIENTED_EDGE('',*,*,#48677,.T.);
#64726=ORIENTED_EDGE('',*,*,#48678,.T.);
#64727=ORIENTED_EDGE('',*,*,#48679,.T.);
#64728=ORIENTED_EDGE('',*,*,#48680,.T.);
#64729=ORIENTED_EDGE('',*,*,#48681,.T.);
#64730=ORIENTED_EDGE('',*,*,#48682,.T.);
#64731=ORIENTED_EDGE('',*,*,#48683,.T.);
#64732=ORIENTED_EDGE('',*,*,#48684,.T.);
#64733=ORIENTED_EDGE('',*,*,#48685,.T.);
#64734=ORIENTED_EDGE('',*,*,#48686,.T.);
#64735=ORIENTED_EDGE('',*,*,#48687,.T.);
#64736=ORIENTED_EDGE('',*,*,#48688,.T.);
#64737=ORIENTED_EDGE('',*,*,#48689,.T.);
#64738=ORIENTED_EDGE('',*,*,#48690,.T.);
#64739=ORIENTED_EDGE('',*,*,#48691,.T.);
#64740=ORIENTED_EDGE('',*,*,#48692,.T.);
#64741=ORIENTED_EDGE('',*,*,#48693,.T.);
#64742=ORIENTED_EDGE('',*,*,#48694,.T.);
#64743=ORIENTED_EDGE('',*,*,#48695,.T.);
#64744=ORIENTED_EDGE('',*,*,#48696,.T.);
#64745=ORIENTED_EDGE('',*,*,#48697,.T.);
#64746=ORIENTED_EDGE('',*,*,#48698,.T.);
#64747=ORIENTED_EDGE('',*,*,#48699,.T.);
#64748=ORIENTED_EDGE('',*,*,#48700,.T.);
#64749=ORIENTED_EDGE('',*,*,#48701,.T.);
#64750=ORIENTED_EDGE('',*,*,#48702,.T.);
#64751=ORIENTED_EDGE('',*,*,#48703,.T.);
#64752=ORIENTED_EDGE('',*,*,#48704,.T.);
#64753=ORIENTED_EDGE('',*,*,#48705,.T.);
#64754=ORIENTED_EDGE('',*,*,#48706,.T.);
#64755=ORIENTED_EDGE('',*,*,#48707,.T.);
#64756=ORIENTED_EDGE('',*,*,#48708,.T.);
#64757=ORIENTED_EDGE('',*,*,#48709,.T.);
#64758=ORIENTED_EDGE('',*,*,#48710,.T.);
#64759=ORIENTED_EDGE('',*,*,#48711,.T.);
#64760=ORIENTED_EDGE('',*,*,#48712,.T.);
#64761=ORIENTED_EDGE('',*,*,#48713,.T.);
#64762=ORIENTED_EDGE('',*,*,#48714,.T.);
#64763=ORIENTED_EDGE('',*,*,#48715,.T.);
#64764=ORIENTED_EDGE('',*,*,#48716,.T.);
#64765=ORIENTED_EDGE('',*,*,#48717,.T.);
#64766=ORIENTED_EDGE('',*,*,#48718,.T.);
#64767=ORIENTED_EDGE('',*,*,#48719,.T.);
#64768=ORIENTED_EDGE('',*,*,#48720,.T.);
#64769=ORIENTED_EDGE('',*,*,#48721,.T.);
#64770=ORIENTED_EDGE('',*,*,#48722,.T.);
#64771=ORIENTED_EDGE('',*,*,#48723,.T.);
#64772=ORIENTED_EDGE('',*,*,#48724,.T.);
#64773=ORIENTED_EDGE('',*,*,#48725,.T.);
#64774=ORIENTED_EDGE('',*,*,#48726,.T.);
#64775=ORIENTED_EDGE('',*,*,#48727,.T.);
#64776=ORIENTED_EDGE('',*,*,#48728,.T.);
#64777=ORIENTED_EDGE('',*,*,#48729,.T.);
#64778=ORIENTED_EDGE('',*,*,#48730,.T.);
#64779=ORIENTED_EDGE('',*,*,#48731,.T.);
#64780=ORIENTED_EDGE('',*,*,#48732,.T.);
#64781=ORIENTED_EDGE('',*,*,#48733,.T.);
#64782=ORIENTED_EDGE('',*,*,#48734,.T.);
#64783=ORIENTED_EDGE('',*,*,#48735,.T.);
#64784=ORIENTED_EDGE('',*,*,#48736,.T.);
#64785=ORIENTED_EDGE('',*,*,#48737,.T.);
#64786=ORIENTED_EDGE('',*,*,#48738,.T.);
#64787=ORIENTED_EDGE('',*,*,#48739,.T.);
#64788=ORIENTED_EDGE('',*,*,#48740,.T.);
#64789=ORIENTED_EDGE('',*,*,#48741,.T.);
#64790=ORIENTED_EDGE('',*,*,#48742,.T.);
#64791=ORIENTED_EDGE('',*,*,#48743,.T.);
#64792=ORIENTED_EDGE('',*,*,#48744,.T.);
#64793=ORIENTED_EDGE('',*,*,#48745,.T.);
#64794=ORIENTED_EDGE('',*,*,#48746,.T.);
#64795=ORIENTED_EDGE('',*,*,#48747,.T.);
#64796=ORIENTED_EDGE('',*,*,#48748,.T.);
#64797=ORIENTED_EDGE('',*,*,#48749,.T.);
#64798=ORIENTED_EDGE('',*,*,#48750,.T.);
#64799=ORIENTED_EDGE('',*,*,#48751,.T.);
#64800=ORIENTED_EDGE('',*,*,#48752,.T.);
#64801=ORIENTED_EDGE('',*,*,#48753,.T.);
#64802=ORIENTED_EDGE('',*,*,#48754,.T.);
#64803=ORIENTED_EDGE('',*,*,#48755,.T.);
#64804=ORIENTED_EDGE('',*,*,#48756,.T.);
#64805=ORIENTED_EDGE('',*,*,#48757,.T.);
#64806=ORIENTED_EDGE('',*,*,#48758,.T.);
#64807=ORIENTED_EDGE('',*,*,#48759,.T.);
#64808=ORIENTED_EDGE('',*,*,#48760,.T.);
#64809=ORIENTED_EDGE('',*,*,#48761,.T.);
#64810=ORIENTED_EDGE('',*,*,#48762,.T.);
#64811=ORIENTED_EDGE('',*,*,#48763,.T.);
#64812=ORIENTED_EDGE('',*,*,#48764,.T.);
#64813=ORIENTED_EDGE('',*,*,#48765,.T.);
#64814=ORIENTED_EDGE('',*,*,#48766,.T.);
#64815=ORIENTED_EDGE('',*,*,#48767,.T.);
#64816=ORIENTED_EDGE('',*,*,#48768,.T.);
#64817=ORIENTED_EDGE('',*,*,#48769,.T.);
#64818=ORIENTED_EDGE('',*,*,#48770,.T.);
#64819=ORIENTED_EDGE('',*,*,#48771,.T.);
#64820=ORIENTED_EDGE('',*,*,#48772,.T.);
#64821=ORIENTED_EDGE('',*,*,#48773,.T.);
#64822=ORIENTED_EDGE('',*,*,#48774,.T.);
#64823=ORIENTED_EDGE('',*,*,#48775,.T.);
#64824=ORIENTED_EDGE('',*,*,#48776,.T.);
#64825=ORIENTED_EDGE('',*,*,#48777,.T.);
#64826=ORIENTED_EDGE('',*,*,#48778,.T.);
#64827=ORIENTED_EDGE('',*,*,#48779,.T.);
#64828=ORIENTED_EDGE('',*,*,#48780,.T.);
#64829=ORIENTED_EDGE('',*,*,#48781,.T.);
#64830=ORIENTED_EDGE('',*,*,#48782,.T.);
#64831=ORIENTED_EDGE('',*,*,#48783,.T.);
#64832=ORIENTED_EDGE('',*,*,#48784,.T.);
#64833=ORIENTED_EDGE('',*,*,#48785,.T.);
#64834=ORIENTED_EDGE('',*,*,#48786,.T.);
#64835=ORIENTED_EDGE('',*,*,#48787,.T.);
#64836=ORIENTED_EDGE('',*,*,#48788,.T.);
#64837=ORIENTED_EDGE('',*,*,#48789,.T.);
#64838=ORIENTED_EDGE('',*,*,#48790,.T.);
#64839=ORIENTED_EDGE('',*,*,#48791,.T.);
#64840=ORIENTED_EDGE('',*,*,#48792,.T.);
#64841=ORIENTED_EDGE('',*,*,#48793,.T.);
#64842=ORIENTED_EDGE('',*,*,#48794,.T.);
#64843=ORIENTED_EDGE('',*,*,#48795,.T.);
#64844=ORIENTED_EDGE('',*,*,#48796,.T.);
#64845=ORIENTED_EDGE('',*,*,#48797,.T.);
#64846=ORIENTED_EDGE('',*,*,#48798,.T.);
#64847=ORIENTED_EDGE('',*,*,#48799,.T.);
#64848=ORIENTED_EDGE('',*,*,#48800,.T.);
#64849=ORIENTED_EDGE('',*,*,#48801,.T.);
#64850=ORIENTED_EDGE('',*,*,#48802,.T.);
#64851=ORIENTED_EDGE('',*,*,#48803,.T.);
#64852=ORIENTED_EDGE('',*,*,#48804,.T.);
#64853=ORIENTED_EDGE('',*,*,#48805,.T.);
#64854=ORIENTED_EDGE('',*,*,#48806,.T.);
#64855=ORIENTED_EDGE('',*,*,#48807,.T.);
#64856=ORIENTED_EDGE('',*,*,#48808,.T.);
#64857=ORIENTED_EDGE('',*,*,#48809,.T.);
#64858=ORIENTED_EDGE('',*,*,#48810,.T.);
#64859=ORIENTED_EDGE('',*,*,#48811,.T.);
#64860=ORIENTED_EDGE('',*,*,#48812,.T.);
#64861=ORIENTED_EDGE('',*,*,#48813,.T.);
#64862=ORIENTED_EDGE('',*,*,#48814,.T.);
#64863=ORIENTED_EDGE('',*,*,#48815,.T.);
#64864=ORIENTED_EDGE('',*,*,#48816,.T.);
#64865=ORIENTED_EDGE('',*,*,#48817,.T.);
#64866=ORIENTED_EDGE('',*,*,#48818,.T.);
#64867=ORIENTED_EDGE('',*,*,#48819,.T.);
#64868=ORIENTED_EDGE('',*,*,#48820,.T.);
#64869=ORIENTED_EDGE('',*,*,#48821,.T.);
#64870=ORIENTED_EDGE('',*,*,#48822,.T.);
#64871=ORIENTED_EDGE('',*,*,#48823,.T.);
#64872=ORIENTED_EDGE('',*,*,#48824,.T.);
#64873=ORIENTED_EDGE('',*,*,#48825,.T.);
#64874=ORIENTED_EDGE('',*,*,#48826,.T.);
#64875=ORIENTED_EDGE('',*,*,#48827,.T.);
#64876=ORIENTED_EDGE('',*,*,#48828,.T.);
#64877=ORIENTED_EDGE('',*,*,#48829,.T.);
#64878=ORIENTED_EDGE('',*,*,#48830,.T.);
#64879=ORIENTED_EDGE('',*,*,#48831,.T.);
#64880=ORIENTED_EDGE('',*,*,#48832,.T.);
#64881=ORIENTED_EDGE('',*,*,#48833,.T.);
#64882=ORIENTED_EDGE('',*,*,#48834,.T.);
#64883=ORIENTED_EDGE('',*,*,#48835,.T.);
#64884=ORIENTED_EDGE('',*,*,#48836,.T.);
#64885=ORIENTED_EDGE('',*,*,#48837,.T.);
#64886=ORIENTED_EDGE('',*,*,#48838,.T.);
#64887=ORIENTED_EDGE('',*,*,#48839,.T.);
#64888=ORIENTED_EDGE('',*,*,#48840,.T.);
#64889=ORIENTED_EDGE('',*,*,#48841,.T.);
#64890=ORIENTED_EDGE('',*,*,#48842,.T.);
#64891=ORIENTED_EDGE('',*,*,#48843,.T.);
#64892=ORIENTED_EDGE('',*,*,#48844,.T.);
#64893=ORIENTED_EDGE('',*,*,#48845,.T.);
#64894=ORIENTED_EDGE('',*,*,#48846,.T.);
#64895=ORIENTED_EDGE('',*,*,#48847,.T.);
#64896=ORIENTED_EDGE('',*,*,#48848,.T.);
#64897=ORIENTED_EDGE('',*,*,#48849,.T.);
#64898=ORIENTED_EDGE('',*,*,#48850,.T.);
#64899=ORIENTED_EDGE('',*,*,#48851,.T.);
#64900=ORIENTED_EDGE('',*,*,#48852,.T.);
#64901=ORIENTED_EDGE('',*,*,#48853,.T.);
#64902=ORIENTED_EDGE('',*,*,#48854,.T.);
#64903=ORIENTED_EDGE('',*,*,#48855,.T.);
#64904=ORIENTED_EDGE('',*,*,#48856,.T.);
#64905=ORIENTED_EDGE('',*,*,#48857,.T.);
#64906=ORIENTED_EDGE('',*,*,#48858,.T.);
#64907=ORIENTED_EDGE('',*,*,#48859,.T.);
#64908=ORIENTED_EDGE('',*,*,#48860,.T.);
#64909=ORIENTED_EDGE('',*,*,#48861,.T.);
#64910=ORIENTED_EDGE('',*,*,#48862,.T.);
#64911=ORIENTED_EDGE('',*,*,#48863,.T.);
#64912=ORIENTED_EDGE('',*,*,#48864,.T.);
#64913=ORIENTED_EDGE('',*,*,#48865,.T.);
#64914=ORIENTED_EDGE('',*,*,#48866,.T.);
#64915=ORIENTED_EDGE('',*,*,#48867,.T.);
#64916=ORIENTED_EDGE('',*,*,#48868,.T.);
#64917=ORIENTED_EDGE('',*,*,#48869,.T.);
#64918=ORIENTED_EDGE('',*,*,#48870,.T.);
#64919=ORIENTED_EDGE('',*,*,#48871,.T.);
#64920=ORIENTED_EDGE('',*,*,#48872,.T.);
#64921=ORIENTED_EDGE('',*,*,#48873,.T.);
#64922=ORIENTED_EDGE('',*,*,#48874,.T.);
#64923=ORIENTED_EDGE('',*,*,#48875,.T.);
#64924=ORIENTED_EDGE('',*,*,#48876,.T.);
#64925=ORIENTED_EDGE('',*,*,#48877,.T.);
#64926=ORIENTED_EDGE('',*,*,#48878,.T.);
#64927=ORIENTED_EDGE('',*,*,#48879,.T.);
#64928=ORIENTED_EDGE('',*,*,#48880,.T.);
#64929=ORIENTED_EDGE('',*,*,#48881,.T.);
#64930=ORIENTED_EDGE('',*,*,#48882,.T.);
#64931=ORIENTED_EDGE('',*,*,#48883,.T.);
#64932=ORIENTED_EDGE('',*,*,#48884,.T.);
#64933=ORIENTED_EDGE('',*,*,#48885,.T.);
#64934=ORIENTED_EDGE('',*,*,#48886,.T.);
#64935=ORIENTED_EDGE('',*,*,#48887,.T.);
#64936=ORIENTED_EDGE('',*,*,#48888,.T.);
#64937=ORIENTED_EDGE('',*,*,#48889,.T.);
#64938=ORIENTED_EDGE('',*,*,#48890,.T.);
#64939=ORIENTED_EDGE('',*,*,#48891,.T.);
#64940=ORIENTED_EDGE('',*,*,#48892,.T.);
#64941=ORIENTED_EDGE('',*,*,#48893,.T.);
#64942=ORIENTED_EDGE('',*,*,#48894,.T.);
#64943=ORIENTED_EDGE('',*,*,#48895,.T.);
#64944=ORIENTED_EDGE('',*,*,#48896,.T.);
#64945=ORIENTED_EDGE('',*,*,#48897,.T.);
#64946=ORIENTED_EDGE('',*,*,#48898,.T.);
#64947=ORIENTED_EDGE('',*,*,#48899,.T.);
#64948=ORIENTED_EDGE('',*,*,#48900,.T.);
#64949=ORIENTED_EDGE('',*,*,#48901,.T.);
#64950=ORIENTED_EDGE('',*,*,#48902,.T.);
#64951=ORIENTED_EDGE('',*,*,#48903,.T.);
#64952=ORIENTED_EDGE('',*,*,#48904,.T.);
#64953=ORIENTED_EDGE('',*,*,#48905,.T.);
#64954=ORIENTED_EDGE('',*,*,#48906,.T.);
#64955=ORIENTED_EDGE('',*,*,#48907,.T.);
#64956=ORIENTED_EDGE('',*,*,#48908,.T.);
#64957=ORIENTED_EDGE('',*,*,#48909,.T.);
#64958=ORIENTED_EDGE('',*,*,#48910,.T.);
#64959=ORIENTED_EDGE('',*,*,#48911,.T.);
#64960=ORIENTED_EDGE('',*,*,#48912,.T.);
#64961=ORIENTED_EDGE('',*,*,#48913,.T.);
#64962=ORIENTED_EDGE('',*,*,#48914,.T.);
#64963=ORIENTED_EDGE('',*,*,#48915,.T.);
#64964=ORIENTED_EDGE('',*,*,#48916,.T.);
#64965=ORIENTED_EDGE('',*,*,#48917,.T.);
#64966=ORIENTED_EDGE('',*,*,#48918,.T.);
#64967=ORIENTED_EDGE('',*,*,#48919,.T.);
#64968=ORIENTED_EDGE('',*,*,#48920,.T.);
#64969=ORIENTED_EDGE('',*,*,#48921,.T.);
#64970=ORIENTED_EDGE('',*,*,#48922,.T.);
#64971=ORIENTED_EDGE('',*,*,#48923,.T.);
#64972=ORIENTED_EDGE('',*,*,#48924,.T.);
#64973=ORIENTED_EDGE('',*,*,#48925,.T.);
#64974=ORIENTED_EDGE('',*,*,#48926,.T.);
#64975=ORIENTED_EDGE('',*,*,#48927,.T.);
#64976=ORIENTED_EDGE('',*,*,#48928,.T.);
#64977=ORIENTED_EDGE('',*,*,#48929,.T.);
#64978=ORIENTED_EDGE('',*,*,#48930,.T.);
#64979=ORIENTED_EDGE('',*,*,#48931,.T.);
#64980=ORIENTED_EDGE('',*,*,#48932,.T.);
#64981=ORIENTED_EDGE('',*,*,#48933,.T.);
#64982=ORIENTED_EDGE('',*,*,#48934,.T.);
#64983=ORIENTED_EDGE('',*,*,#48935,.T.);
#64984=ORIENTED_EDGE('',*,*,#48936,.T.);
#64985=ORIENTED_EDGE('',*,*,#48937,.T.);
#64986=ORIENTED_EDGE('',*,*,#48938,.T.);
#64987=ORIENTED_EDGE('',*,*,#48939,.T.);
#64988=ORIENTED_EDGE('',*,*,#48940,.T.);
#64989=ORIENTED_EDGE('',*,*,#48941,.T.);
#64990=ORIENTED_EDGE('',*,*,#48942,.T.);
#64991=ORIENTED_EDGE('',*,*,#48943,.T.);
#64992=ORIENTED_EDGE('',*,*,#48944,.T.);
#64993=ORIENTED_EDGE('',*,*,#48945,.T.);
#64994=ORIENTED_EDGE('',*,*,#48946,.T.);
#64995=ORIENTED_EDGE('',*,*,#48947,.T.);
#64996=ORIENTED_EDGE('',*,*,#48948,.T.);
#64997=ORIENTED_EDGE('',*,*,#48949,.T.);
#64998=ORIENTED_EDGE('',*,*,#48950,.T.);
#64999=ORIENTED_EDGE('',*,*,#48951,.T.);
#65000=ORIENTED_EDGE('',*,*,#48952,.T.);
#65001=ORIENTED_EDGE('',*,*,#48953,.T.);
#65002=ORIENTED_EDGE('',*,*,#48954,.T.);
#65003=ORIENTED_EDGE('',*,*,#48955,.T.);
#65004=ORIENTED_EDGE('',*,*,#48956,.T.);
#65005=ORIENTED_EDGE('',*,*,#48957,.T.);
#65006=ORIENTED_EDGE('',*,*,#48958,.T.);
#65007=ORIENTED_EDGE('',*,*,#48959,.T.);
#65008=ORIENTED_EDGE('',*,*,#48960,.T.);
#65009=ORIENTED_EDGE('',*,*,#48961,.T.);
#65010=ORIENTED_EDGE('',*,*,#48962,.T.);
#65011=ORIENTED_EDGE('',*,*,#48963,.T.);
#65012=ORIENTED_EDGE('',*,*,#48964,.T.);
#65013=ORIENTED_EDGE('',*,*,#48965,.T.);
#65014=ORIENTED_EDGE('',*,*,#48966,.T.);
#65015=ORIENTED_EDGE('',*,*,#48967,.T.);
#65016=ORIENTED_EDGE('',*,*,#48968,.T.);
#65017=ORIENTED_EDGE('',*,*,#48969,.T.);
#65018=ORIENTED_EDGE('',*,*,#48970,.T.);
#65019=ORIENTED_EDGE('',*,*,#48971,.T.);
#65020=ORIENTED_EDGE('',*,*,#48972,.T.);
#65021=ORIENTED_EDGE('',*,*,#48973,.T.);
#65022=ORIENTED_EDGE('',*,*,#48974,.T.);
#65023=ORIENTED_EDGE('',*,*,#48975,.T.);
#65024=ORIENTED_EDGE('',*,*,#48976,.T.);
#65025=ORIENTED_EDGE('',*,*,#48977,.T.);
#65026=ORIENTED_EDGE('',*,*,#48978,.T.);
#65027=ORIENTED_EDGE('',*,*,#48979,.T.);
#65028=ORIENTED_EDGE('',*,*,#48980,.T.);
#65029=ORIENTED_EDGE('',*,*,#48981,.T.);
#65030=ORIENTED_EDGE('',*,*,#48982,.T.);
#65031=ORIENTED_EDGE('',*,*,#48983,.T.);
#65032=ORIENTED_EDGE('',*,*,#48984,.T.);
#65033=ORIENTED_EDGE('',*,*,#48985,.T.);
#65034=ORIENTED_EDGE('',*,*,#48986,.T.);
#65035=ORIENTED_EDGE('',*,*,#48987,.T.);
#65036=ORIENTED_EDGE('',*,*,#48988,.T.);
#65037=ORIENTED_EDGE('',*,*,#48989,.T.);
#65038=ORIENTED_EDGE('',*,*,#48990,.T.);
#65039=ORIENTED_EDGE('',*,*,#48991,.T.);
#65040=ORIENTED_EDGE('',*,*,#48992,.T.);
#65041=ORIENTED_EDGE('',*,*,#48993,.T.);
#65042=ORIENTED_EDGE('',*,*,#48994,.T.);
#65043=ORIENTED_EDGE('',*,*,#48995,.T.);
#65044=ORIENTED_EDGE('',*,*,#48996,.T.);
#65045=ORIENTED_EDGE('',*,*,#48997,.T.);
#65046=ORIENTED_EDGE('',*,*,#48998,.T.);
#65047=ORIENTED_EDGE('',*,*,#48999,.T.);
#65048=ORIENTED_EDGE('',*,*,#49000,.T.);
#65049=ORIENTED_EDGE('',*,*,#49001,.T.);
#65050=ORIENTED_EDGE('',*,*,#49002,.T.);
#65051=ORIENTED_EDGE('',*,*,#49003,.T.);
#65052=ORIENTED_EDGE('',*,*,#49004,.T.);
#65053=ORIENTED_EDGE('',*,*,#49005,.T.);
#65054=ORIENTED_EDGE('',*,*,#49006,.T.);
#65055=ORIENTED_EDGE('',*,*,#49007,.T.);
#65056=ORIENTED_EDGE('',*,*,#49008,.T.);
#65057=ORIENTED_EDGE('',*,*,#49009,.T.);
#65058=ORIENTED_EDGE('',*,*,#49010,.T.);
#65059=ORIENTED_EDGE('',*,*,#49011,.T.);
#65060=ORIENTED_EDGE('',*,*,#49012,.T.);
#65061=ORIENTED_EDGE('',*,*,#49013,.T.);
#65062=ORIENTED_EDGE('',*,*,#49014,.T.);
#65063=ORIENTED_EDGE('',*,*,#49015,.T.);
#65064=ORIENTED_EDGE('',*,*,#49016,.T.);
#65065=ORIENTED_EDGE('',*,*,#49017,.T.);
#65066=ORIENTED_EDGE('',*,*,#49018,.T.);
#65067=ORIENTED_EDGE('',*,*,#49019,.T.);
#65068=ORIENTED_EDGE('',*,*,#49020,.T.);
#65069=ORIENTED_EDGE('',*,*,#49021,.T.);
#65070=ORIENTED_EDGE('',*,*,#49022,.T.);
#65071=ORIENTED_EDGE('',*,*,#49023,.T.);
#65072=ORIENTED_EDGE('',*,*,#49024,.T.);
#65073=ORIENTED_EDGE('',*,*,#49025,.T.);
#65074=ORIENTED_EDGE('',*,*,#49026,.T.);
#65075=ORIENTED_EDGE('',*,*,#49027,.T.);
#65076=ORIENTED_EDGE('',*,*,#49028,.T.);
#65077=ORIENTED_EDGE('',*,*,#49029,.T.);
#65078=ORIENTED_EDGE('',*,*,#49030,.T.);
#65079=ORIENTED_EDGE('',*,*,#49031,.T.);
#65080=ORIENTED_EDGE('',*,*,#49032,.T.);
#65081=ORIENTED_EDGE('',*,*,#49033,.T.);
#65082=ORIENTED_EDGE('',*,*,#49034,.T.);
#65083=ORIENTED_EDGE('',*,*,#49035,.T.);
#65084=ORIENTED_EDGE('',*,*,#49036,.T.);
#65085=ORIENTED_EDGE('',*,*,#49037,.T.);
#65086=ORIENTED_EDGE('',*,*,#49038,.T.);
#65087=ORIENTED_EDGE('',*,*,#49039,.T.);
#65088=ORIENTED_EDGE('',*,*,#49040,.T.);
#65089=ORIENTED_EDGE('',*,*,#49041,.T.);
#65090=ORIENTED_EDGE('',*,*,#49042,.T.);
#65091=ORIENTED_EDGE('',*,*,#49043,.T.);
#65092=ORIENTED_EDGE('',*,*,#49044,.T.);
#65093=ORIENTED_EDGE('',*,*,#49045,.T.);
#65094=ORIENTED_EDGE('',*,*,#49046,.T.);
#65095=ORIENTED_EDGE('',*,*,#49047,.T.);
#65096=ORIENTED_EDGE('',*,*,#49048,.T.);
#65097=ORIENTED_EDGE('',*,*,#49049,.T.);
#65098=ORIENTED_EDGE('',*,*,#49050,.T.);
#65099=ORIENTED_EDGE('',*,*,#49051,.T.);
#65100=ORIENTED_EDGE('',*,*,#49052,.T.);
#65101=ORIENTED_EDGE('',*,*,#49053,.T.);
#65102=ORIENTED_EDGE('',*,*,#49054,.T.);
#65103=ORIENTED_EDGE('',*,*,#49055,.T.);
#65104=ORIENTED_EDGE('',*,*,#49056,.T.);
#65105=ORIENTED_EDGE('',*,*,#49057,.T.);
#65106=ORIENTED_EDGE('',*,*,#49058,.T.);
#65107=ORIENTED_EDGE('',*,*,#49059,.T.);
#65108=ORIENTED_EDGE('',*,*,#49060,.T.);
#65109=ORIENTED_EDGE('',*,*,#49061,.T.);
#65110=ORIENTED_EDGE('',*,*,#49062,.T.);
#65111=ORIENTED_EDGE('',*,*,#49063,.T.);
#65112=ORIENTED_EDGE('',*,*,#49064,.T.);
#65113=ORIENTED_EDGE('',*,*,#49065,.T.);
#65114=ORIENTED_EDGE('',*,*,#49066,.T.);
#65115=ORIENTED_EDGE('',*,*,#49067,.T.);
#65116=ORIENTED_EDGE('',*,*,#49068,.T.);
#65117=ORIENTED_EDGE('',*,*,#49069,.T.);
#65118=ORIENTED_EDGE('',*,*,#49070,.T.);
#65119=ORIENTED_EDGE('',*,*,#49071,.T.);
#65120=ORIENTED_EDGE('',*,*,#49072,.T.);
#65121=ORIENTED_EDGE('',*,*,#49073,.T.);
#65122=ORIENTED_EDGE('',*,*,#49074,.T.);
#65123=ORIENTED_EDGE('',*,*,#49075,.T.);
#65124=ORIENTED_EDGE('',*,*,#49076,.T.);
#65125=ORIENTED_EDGE('',*,*,#49077,.T.);
#65126=ORIENTED_EDGE('',*,*,#49078,.T.);
#65127=ORIENTED_EDGE('',*,*,#49079,.T.);
#65128=ORIENTED_EDGE('',*,*,#49080,.T.);
#65129=ORIENTED_EDGE('',*,*,#49081,.T.);
#65130=ORIENTED_EDGE('',*,*,#49082,.T.);
#65131=ORIENTED_EDGE('',*,*,#49083,.T.);
#65132=ORIENTED_EDGE('',*,*,#49084,.T.);
#65133=ORIENTED_EDGE('',*,*,#49085,.T.);
#65134=ORIENTED_EDGE('',*,*,#49086,.T.);
#65135=ORIENTED_EDGE('',*,*,#49087,.T.);
#65136=ORIENTED_EDGE('',*,*,#49088,.T.);
#65137=ORIENTED_EDGE('',*,*,#49089,.T.);
#65138=ORIENTED_EDGE('',*,*,#49090,.T.);
#65139=ORIENTED_EDGE('',*,*,#49091,.T.);
#65140=ORIENTED_EDGE('',*,*,#49092,.T.);
#65141=ORIENTED_EDGE('',*,*,#49093,.T.);
#65142=ORIENTED_EDGE('',*,*,#49094,.T.);
#65143=ORIENTED_EDGE('',*,*,#49095,.T.);
#65144=ORIENTED_EDGE('',*,*,#49096,.T.);
#65145=ORIENTED_EDGE('',*,*,#49097,.T.);
#65146=ORIENTED_EDGE('',*,*,#49098,.T.);
#65147=ORIENTED_EDGE('',*,*,#49099,.T.);
#65148=ORIENTED_EDGE('',*,*,#49100,.T.);
#65149=ORIENTED_EDGE('',*,*,#49101,.T.);
#65150=ORIENTED_EDGE('',*,*,#49102,.T.);
#65151=ORIENTED_EDGE('',*,*,#49103,.T.);
#65152=ORIENTED_EDGE('',*,*,#49104,.T.);
#65153=ORIENTED_EDGE('',*,*,#49105,.T.);
#65154=ORIENTED_EDGE('',*,*,#49106,.T.);
#65155=ORIENTED_EDGE('',*,*,#49107,.T.);
#65156=ORIENTED_EDGE('',*,*,#49108,.T.);
#65157=ORIENTED_EDGE('',*,*,#49109,.T.);
#65158=ORIENTED_EDGE('',*,*,#49110,.T.);
#65159=ORIENTED_EDGE('',*,*,#49111,.T.);
#65160=ORIENTED_EDGE('',*,*,#49112,.T.);
#65161=ORIENTED_EDGE('',*,*,#49113,.T.);
#65162=ORIENTED_EDGE('',*,*,#49114,.T.);
#65163=ORIENTED_EDGE('',*,*,#49115,.T.);
#65164=ORIENTED_EDGE('',*,*,#49116,.T.);
#65165=ORIENTED_EDGE('',*,*,#49117,.T.);
#65166=ORIENTED_EDGE('',*,*,#49118,.T.);
#65167=ORIENTED_EDGE('',*,*,#49119,.T.);
#65168=ORIENTED_EDGE('',*,*,#49120,.T.);
#65169=ORIENTED_EDGE('',*,*,#49121,.T.);
#65170=ORIENTED_EDGE('',*,*,#49122,.T.);
#65171=ORIENTED_EDGE('',*,*,#49123,.T.);
#65172=ORIENTED_EDGE('',*,*,#49124,.T.);
#65173=ORIENTED_EDGE('',*,*,#49125,.T.);
#65174=ORIENTED_EDGE('',*,*,#49126,.T.);
#65175=ORIENTED_EDGE('',*,*,#49127,.T.);
#65176=ORIENTED_EDGE('',*,*,#49128,.T.);
#65177=ORIENTED_EDGE('',*,*,#49129,.T.);
#65178=ORIENTED_EDGE('',*,*,#49130,.T.);
#65179=ORIENTED_EDGE('',*,*,#49131,.T.);
#65180=ORIENTED_EDGE('',*,*,#49132,.T.);
#65181=ORIENTED_EDGE('',*,*,#49133,.T.);
#65182=ORIENTED_EDGE('',*,*,#49134,.T.);
#65183=ORIENTED_EDGE('',*,*,#49135,.T.);
#65184=ORIENTED_EDGE('',*,*,#49136,.T.);
#65185=ORIENTED_EDGE('',*,*,#49137,.T.);
#65186=ORIENTED_EDGE('',*,*,#49138,.T.);
#65187=ORIENTED_EDGE('',*,*,#49139,.T.);
#65188=ORIENTED_EDGE('',*,*,#49140,.T.);
#65189=ORIENTED_EDGE('',*,*,#49141,.T.);
#65190=ORIENTED_EDGE('',*,*,#49142,.T.);
#65191=ORIENTED_EDGE('',*,*,#49143,.T.);
#65192=ORIENTED_EDGE('',*,*,#49144,.T.);
#65193=ORIENTED_EDGE('',*,*,#49145,.T.);
#65194=ORIENTED_EDGE('',*,*,#49146,.T.);
#65195=ORIENTED_EDGE('',*,*,#49147,.T.);
#65196=ORIENTED_EDGE('',*,*,#49148,.T.);
#65197=ORIENTED_EDGE('',*,*,#49149,.T.);
#65198=ORIENTED_EDGE('',*,*,#49150,.T.);
#65199=ORIENTED_EDGE('',*,*,#49151,.T.);
#65200=ORIENTED_EDGE('',*,*,#49152,.T.);
#65201=ORIENTED_EDGE('',*,*,#49153,.T.);
#65202=ORIENTED_EDGE('',*,*,#49154,.T.);
#65203=ORIENTED_EDGE('',*,*,#49155,.T.);
#65204=ORIENTED_EDGE('',*,*,#49156,.T.);
#65205=ORIENTED_EDGE('',*,*,#49157,.T.);
#65206=ORIENTED_EDGE('',*,*,#49158,.T.);
#65207=ORIENTED_EDGE('',*,*,#49159,.T.);
#65208=ORIENTED_EDGE('',*,*,#49160,.T.);
#65209=ORIENTED_EDGE('',*,*,#49161,.T.);
#65210=ORIENTED_EDGE('',*,*,#49162,.T.);
#65211=ORIENTED_EDGE('',*,*,#49163,.T.);
#65212=ORIENTED_EDGE('',*,*,#49164,.T.);
#65213=ORIENTED_EDGE('',*,*,#49165,.T.);
#65214=ORIENTED_EDGE('',*,*,#49166,.T.);
#65215=ORIENTED_EDGE('',*,*,#49167,.T.);
#65216=ORIENTED_EDGE('',*,*,#49168,.T.);
#65217=ORIENTED_EDGE('',*,*,#49169,.T.);
#65218=ORIENTED_EDGE('',*,*,#49170,.T.);
#65219=ORIENTED_EDGE('',*,*,#49171,.T.);
#65220=ORIENTED_EDGE('',*,*,#49172,.T.);
#65221=ORIENTED_EDGE('',*,*,#49173,.T.);
#65222=ORIENTED_EDGE('',*,*,#49174,.T.);
#65223=ORIENTED_EDGE('',*,*,#49175,.T.);
#65224=ORIENTED_EDGE('',*,*,#49176,.T.);
#65225=ORIENTED_EDGE('',*,*,#49177,.T.);
#65226=ORIENTED_EDGE('',*,*,#49178,.T.);
#65227=ORIENTED_EDGE('',*,*,#49179,.T.);
#65228=ORIENTED_EDGE('',*,*,#49180,.T.);
#65229=ORIENTED_EDGE('',*,*,#49181,.T.);
#65230=ORIENTED_EDGE('',*,*,#49182,.T.);
#65231=ORIENTED_EDGE('',*,*,#49183,.T.);
#65232=ORIENTED_EDGE('',*,*,#49184,.T.);
#65233=ORIENTED_EDGE('',*,*,#49185,.T.);
#65234=ORIENTED_EDGE('',*,*,#49186,.T.);
#65235=ORIENTED_EDGE('',*,*,#49187,.T.);
#65236=ORIENTED_EDGE('',*,*,#49188,.T.);
#65237=ORIENTED_EDGE('',*,*,#49189,.T.);
#65238=ORIENTED_EDGE('',*,*,#49190,.T.);
#65239=ORIENTED_EDGE('',*,*,#49191,.T.);
#65240=ORIENTED_EDGE('',*,*,#49192,.T.);
#65241=ORIENTED_EDGE('',*,*,#49193,.T.);
#65242=ORIENTED_EDGE('',*,*,#49194,.T.);
#65243=ORIENTED_EDGE('',*,*,#49195,.T.);
#65244=ORIENTED_EDGE('',*,*,#49196,.T.);
#65245=ORIENTED_EDGE('',*,*,#49197,.T.);
#65246=ORIENTED_EDGE('',*,*,#49198,.T.);
#65247=ORIENTED_EDGE('',*,*,#49199,.T.);
#65248=ORIENTED_EDGE('',*,*,#49200,.T.);
#65249=ORIENTED_EDGE('',*,*,#49201,.T.);
#65250=ORIENTED_EDGE('',*,*,#49202,.T.);
#65251=ORIENTED_EDGE('',*,*,#49203,.T.);
#65252=ORIENTED_EDGE('',*,*,#49204,.T.);
#65253=ORIENTED_EDGE('',*,*,#49205,.T.);
#65254=ORIENTED_EDGE('',*,*,#49206,.T.);
#65255=ORIENTED_EDGE('',*,*,#49207,.T.);
#65256=ORIENTED_EDGE('',*,*,#49208,.T.);
#65257=ORIENTED_EDGE('',*,*,#49209,.T.);
#65258=ORIENTED_EDGE('',*,*,#49210,.T.);
#65259=ORIENTED_EDGE('',*,*,#49211,.T.);
#65260=ORIENTED_EDGE('',*,*,#49212,.T.);
#65261=ORIENTED_EDGE('',*,*,#49213,.T.);
#65262=ORIENTED_EDGE('',*,*,#49214,.T.);
#65263=ORIENTED_EDGE('',*,*,#49215,.T.);
#65264=ORIENTED_EDGE('',*,*,#49216,.T.);
#65265=ORIENTED_EDGE('',*,*,#49217,.T.);
#65266=ORIENTED_EDGE('',*,*,#49218,.T.);
#65267=ORIENTED_EDGE('',*,*,#49219,.T.);
#65268=ORIENTED_EDGE('',*,*,#49220,.T.);
#65269=ORIENTED_EDGE('',*,*,#49221,.T.);
#65270=ORIENTED_EDGE('',*,*,#49222,.T.);
#65271=ORIENTED_EDGE('',*,*,#49223,.T.);
#65272=ORIENTED_EDGE('',*,*,#49224,.T.);
#65273=ORIENTED_EDGE('',*,*,#49225,.T.);
#65274=ORIENTED_EDGE('',*,*,#49226,.T.);
#65275=ORIENTED_EDGE('',*,*,#49227,.T.);
#65276=ORIENTED_EDGE('',*,*,#49228,.T.);
#65277=ORIENTED_EDGE('',*,*,#49229,.T.);
#65278=ORIENTED_EDGE('',*,*,#49230,.T.);
#65279=ORIENTED_EDGE('',*,*,#49231,.T.);
#65280=ORIENTED_EDGE('',*,*,#49232,.T.);
#65281=ORIENTED_EDGE('',*,*,#49233,.T.);
#65282=ORIENTED_EDGE('',*,*,#49234,.T.);
#65283=ORIENTED_EDGE('',*,*,#49235,.T.);
#65284=ORIENTED_EDGE('',*,*,#49236,.T.);
#65285=ORIENTED_EDGE('',*,*,#49237,.T.);
#65286=ORIENTED_EDGE('',*,*,#49238,.T.);
#65287=ORIENTED_EDGE('',*,*,#49239,.T.);
#65288=ORIENTED_EDGE('',*,*,#49240,.T.);
#65289=ORIENTED_EDGE('',*,*,#49241,.T.);
#65290=ORIENTED_EDGE('',*,*,#49242,.T.);
#65291=ORIENTED_EDGE('',*,*,#49243,.T.);
#65292=ORIENTED_EDGE('',*,*,#49244,.T.);
#65293=ORIENTED_EDGE('',*,*,#49245,.T.);
#65294=ORIENTED_EDGE('',*,*,#49246,.T.);
#65295=ORIENTED_EDGE('',*,*,#49247,.T.);
#65296=ORIENTED_EDGE('',*,*,#49248,.T.);
#65297=ORIENTED_EDGE('',*,*,#49249,.T.);
#65298=ORIENTED_EDGE('',*,*,#49250,.T.);
#65299=ORIENTED_EDGE('',*,*,#49251,.T.);
#65300=ORIENTED_EDGE('',*,*,#49252,.T.);
#65301=ORIENTED_EDGE('',*,*,#49253,.T.);
#65302=ORIENTED_EDGE('',*,*,#49254,.T.);
#65303=ORIENTED_EDGE('',*,*,#49255,.T.);
#65304=ORIENTED_EDGE('',*,*,#49256,.T.);
#65305=ORIENTED_EDGE('',*,*,#49257,.T.);
#65306=ORIENTED_EDGE('',*,*,#49258,.T.);
#65307=ORIENTED_EDGE('',*,*,#49259,.T.);
#65308=ORIENTED_EDGE('',*,*,#49260,.T.);
#65309=ORIENTED_EDGE('',*,*,#49261,.T.);
#65310=ORIENTED_EDGE('',*,*,#49262,.T.);
#65311=ORIENTED_EDGE('',*,*,#49263,.T.);
#65312=ORIENTED_EDGE('',*,*,#49264,.T.);
#65313=ORIENTED_EDGE('',*,*,#49265,.T.);
#65314=ORIENTED_EDGE('',*,*,#49266,.T.);
#65315=ORIENTED_EDGE('',*,*,#49267,.T.);
#65316=ORIENTED_EDGE('',*,*,#49268,.T.);
#65317=ORIENTED_EDGE('',*,*,#49269,.T.);
#65318=ORIENTED_EDGE('',*,*,#49270,.T.);
#65319=ORIENTED_EDGE('',*,*,#49271,.T.);
#65320=ORIENTED_EDGE('',*,*,#49272,.T.);
#65321=ORIENTED_EDGE('',*,*,#49273,.T.);
#65322=ORIENTED_EDGE('',*,*,#49274,.T.);
#65323=ORIENTED_EDGE('',*,*,#49275,.T.);
#65324=ORIENTED_EDGE('',*,*,#49276,.T.);
#65325=ORIENTED_EDGE('',*,*,#49277,.T.);
#65326=ORIENTED_EDGE('',*,*,#49278,.T.);
#65327=ORIENTED_EDGE('',*,*,#49279,.T.);
#65328=ORIENTED_EDGE('',*,*,#49280,.T.);
#65329=ORIENTED_EDGE('',*,*,#49281,.T.);
#65330=ORIENTED_EDGE('',*,*,#49282,.T.);
#65331=ORIENTED_EDGE('',*,*,#49283,.T.);
#65332=ORIENTED_EDGE('',*,*,#49284,.T.);
#65333=ORIENTED_EDGE('',*,*,#49285,.T.);
#65334=ORIENTED_EDGE('',*,*,#49286,.T.);
#65335=ORIENTED_EDGE('',*,*,#49287,.T.);
#65336=ORIENTED_EDGE('',*,*,#49288,.T.);
#65337=ORIENTED_EDGE('',*,*,#49289,.T.);
#65338=ORIENTED_EDGE('',*,*,#49290,.T.);
#65339=ORIENTED_EDGE('',*,*,#49291,.T.);
#65340=ORIENTED_EDGE('',*,*,#49292,.T.);
#65341=ORIENTED_EDGE('',*,*,#49293,.T.);
#65342=ORIENTED_EDGE('',*,*,#49294,.T.);
#65343=ORIENTED_EDGE('',*,*,#49295,.T.);
#65344=ORIENTED_EDGE('',*,*,#49296,.T.);
#65345=ORIENTED_EDGE('',*,*,#49297,.T.);
#65346=ORIENTED_EDGE('',*,*,#49298,.T.);
#65347=ORIENTED_EDGE('',*,*,#49299,.T.);
#65348=ORIENTED_EDGE('',*,*,#49300,.T.);
#65349=ORIENTED_EDGE('',*,*,#49301,.T.);
#65350=ORIENTED_EDGE('',*,*,#49302,.T.);
#65351=ORIENTED_EDGE('',*,*,#49303,.T.);
#65352=ORIENTED_EDGE('',*,*,#49304,.T.);
#65353=ORIENTED_EDGE('',*,*,#49305,.T.);
#65354=ORIENTED_EDGE('',*,*,#49306,.T.);
#65355=ORIENTED_EDGE('',*,*,#49307,.T.);
#65356=ORIENTED_EDGE('',*,*,#49308,.T.);
#65357=ORIENTED_EDGE('',*,*,#49309,.T.);
#65358=ORIENTED_EDGE('',*,*,#49310,.T.);
#65359=ORIENTED_EDGE('',*,*,#49311,.T.);
#65360=ORIENTED_EDGE('',*,*,#49312,.T.);
#65361=ORIENTED_EDGE('',*,*,#49313,.T.);
#65362=ORIENTED_EDGE('',*,*,#45896,.T.);
#65363=ORIENTED_EDGE('',*,*,#49314,.T.);
#65364=ORIENTED_EDGE('',*,*,#45890,.T.);
#65365=ORIENTED_EDGE('',*,*,#49315,.T.);
#65366=ORIENTED_EDGE('',*,*,#49316,.T.);
#65367=ORIENTED_EDGE('',*,*,#49317,.T.);
#65368=ORIENTED_EDGE('',*,*,#49318,.T.);
#65369=ORIENTED_EDGE('',*,*,#49319,.T.);
#65370=ORIENTED_EDGE('',*,*,#49320,.T.);
#65371=ORIENTED_EDGE('',*,*,#49321,.T.);
#65372=ORIENTED_EDGE('',*,*,#49322,.T.);
#65373=ORIENTED_EDGE('',*,*,#49323,.T.);
#65374=ORIENTED_EDGE('',*,*,#49324,.T.);
#65375=ORIENTED_EDGE('',*,*,#49325,.T.);
#65376=ORIENTED_EDGE('',*,*,#49326,.T.);
#65377=ORIENTED_EDGE('',*,*,#49327,.T.);
#65378=ORIENTED_EDGE('',*,*,#49328,.T.);
#65379=ORIENTED_EDGE('',*,*,#49329,.T.);
#65380=ORIENTED_EDGE('',*,*,#49330,.T.);
#65381=ORIENTED_EDGE('',*,*,#49331,.T.);
#65382=ORIENTED_EDGE('',*,*,#49332,.T.);
#65383=ORIENTED_EDGE('',*,*,#49333,.T.);
#65384=ORIENTED_EDGE('',*,*,#49334,.T.);
#65385=ORIENTED_EDGE('',*,*,#49335,.T.);
#65386=ORIENTED_EDGE('',*,*,#49336,.T.);
#65387=ORIENTED_EDGE('',*,*,#49337,.T.);
#65388=ORIENTED_EDGE('',*,*,#49338,.T.);
#65389=ORIENTED_EDGE('',*,*,#49339,.T.);
#65390=ORIENTED_EDGE('',*,*,#49340,.T.);
#65391=ORIENTED_EDGE('',*,*,#49341,.T.);
#65392=ORIENTED_EDGE('',*,*,#49342,.T.);
#65393=ORIENTED_EDGE('',*,*,#49343,.T.);
#65394=ORIENTED_EDGE('',*,*,#49344,.T.);
#65395=ORIENTED_EDGE('',*,*,#49345,.T.);
#65396=ORIENTED_EDGE('',*,*,#49346,.T.);
#65397=ORIENTED_EDGE('',*,*,#49347,.T.);
#65398=ORIENTED_EDGE('',*,*,#49348,.T.);
#65399=ORIENTED_EDGE('',*,*,#49349,.T.);
#65400=ORIENTED_EDGE('',*,*,#49350,.T.);
#65401=ORIENTED_EDGE('',*,*,#49351,.T.);
#65402=ORIENTED_EDGE('',*,*,#49352,.T.);
#65403=ORIENTED_EDGE('',*,*,#49353,.T.);
#65404=ORIENTED_EDGE('',*,*,#49354,.T.);
#65405=ORIENTED_EDGE('',*,*,#49355,.T.);
#65406=ORIENTED_EDGE('',*,*,#49356,.T.);
#65407=ORIENTED_EDGE('',*,*,#49357,.T.);
#65408=ORIENTED_EDGE('',*,*,#49358,.T.);
#65409=ORIENTED_EDGE('',*,*,#49359,.T.);
#65410=ORIENTED_EDGE('',*,*,#49360,.T.);
#65411=ORIENTED_EDGE('',*,*,#49361,.T.);
#65412=ORIENTED_EDGE('',*,*,#49362,.T.);
#65413=ORIENTED_EDGE('',*,*,#49363,.T.);
#65414=ORIENTED_EDGE('',*,*,#49364,.T.);
#65415=ORIENTED_EDGE('',*,*,#49365,.T.);
#65416=ORIENTED_EDGE('',*,*,#49366,.T.);
#65417=ORIENTED_EDGE('',*,*,#49367,.T.);
#65418=ORIENTED_EDGE('',*,*,#49368,.T.);
#65419=ORIENTED_EDGE('',*,*,#49369,.T.);
#65420=ORIENTED_EDGE('',*,*,#49370,.T.);
#65421=ORIENTED_EDGE('',*,*,#49371,.T.);
#65422=ORIENTED_EDGE('',*,*,#49372,.T.);
#65423=ORIENTED_EDGE('',*,*,#49373,.T.);
#65424=ORIENTED_EDGE('',*,*,#49374,.T.);
#65425=ORIENTED_EDGE('',*,*,#49375,.T.);
#65426=ORIENTED_EDGE('',*,*,#49376,.T.);
#65427=ORIENTED_EDGE('',*,*,#49377,.T.);
#65428=ORIENTED_EDGE('',*,*,#49378,.T.);
#65429=ORIENTED_EDGE('',*,*,#49379,.T.);
#65430=ORIENTED_EDGE('',*,*,#49380,.T.);
#65431=ORIENTED_EDGE('',*,*,#49381,.T.);
#65432=ORIENTED_EDGE('',*,*,#49382,.T.);
#65433=ORIENTED_EDGE('',*,*,#49383,.T.);
#65434=ORIENTED_EDGE('',*,*,#49384,.T.);
#65435=ORIENTED_EDGE('',*,*,#49385,.T.);
#65436=ORIENTED_EDGE('',*,*,#49386,.T.);
#65437=ORIENTED_EDGE('',*,*,#49387,.T.);
#65438=ORIENTED_EDGE('',*,*,#49388,.T.);
#65439=ORIENTED_EDGE('',*,*,#49389,.T.);
#65440=ORIENTED_EDGE('',*,*,#49390,.T.);
#65441=ORIENTED_EDGE('',*,*,#49391,.T.);
#65442=ORIENTED_EDGE('',*,*,#49392,.T.);
#65443=ORIENTED_EDGE('',*,*,#49393,.T.);
#65444=ORIENTED_EDGE('',*,*,#49394,.T.);
#65445=ORIENTED_EDGE('',*,*,#49395,.T.);
#65446=ORIENTED_EDGE('',*,*,#49396,.T.);
#65447=ORIENTED_EDGE('',*,*,#49397,.T.);
#65448=ORIENTED_EDGE('',*,*,#49398,.T.);
#65449=ORIENTED_EDGE('',*,*,#49399,.T.);
#65450=ORIENTED_EDGE('',*,*,#49400,.T.);
#65451=ORIENTED_EDGE('',*,*,#49401,.T.);
#65452=ORIENTED_EDGE('',*,*,#49402,.T.);
#65453=ORIENTED_EDGE('',*,*,#49403,.T.);
#65454=ORIENTED_EDGE('',*,*,#49404,.T.);
#65455=ORIENTED_EDGE('',*,*,#49405,.T.);
#65456=ORIENTED_EDGE('',*,*,#49406,.T.);
#65457=ORIENTED_EDGE('',*,*,#49407,.T.);
#65458=ORIENTED_EDGE('',*,*,#49408,.T.);
#65459=ORIENTED_EDGE('',*,*,#49409,.T.);
#65460=ORIENTED_EDGE('',*,*,#49410,.T.);
#65461=ORIENTED_EDGE('',*,*,#49411,.T.);
#65462=ORIENTED_EDGE('',*,*,#49412,.T.);
#65463=ORIENTED_EDGE('',*,*,#49413,.T.);
#65464=ORIENTED_EDGE('',*,*,#49414,.T.);
#65465=ORIENTED_EDGE('',*,*,#49415,.T.);
#65466=ORIENTED_EDGE('',*,*,#49416,.T.);
#65467=ORIENTED_EDGE('',*,*,#49417,.T.);
#65468=ORIENTED_EDGE('',*,*,#49418,.T.);
#65469=ORIENTED_EDGE('',*,*,#49419,.T.);
#65470=ORIENTED_EDGE('',*,*,#49420,.T.);
#65471=ORIENTED_EDGE('',*,*,#49421,.T.);
#65472=ORIENTED_EDGE('',*,*,#49422,.T.);
#65473=ORIENTED_EDGE('',*,*,#49423,.T.);
#65474=ORIENTED_EDGE('',*,*,#49424,.T.);
#65475=ORIENTED_EDGE('',*,*,#49425,.T.);
#65476=ORIENTED_EDGE('',*,*,#49426,.T.);
#65477=ORIENTED_EDGE('',*,*,#49427,.T.);
#65478=ORIENTED_EDGE('',*,*,#49428,.T.);
#65479=ORIENTED_EDGE('',*,*,#49429,.T.);
#65480=ORIENTED_EDGE('',*,*,#49430,.T.);
#65481=ORIENTED_EDGE('',*,*,#49431,.T.);
#65482=ORIENTED_EDGE('',*,*,#49432,.T.);
#65483=ORIENTED_EDGE('',*,*,#49433,.T.);
#65484=ORIENTED_EDGE('',*,*,#49434,.T.);
#65485=ORIENTED_EDGE('',*,*,#49435,.T.);
#65486=ORIENTED_EDGE('',*,*,#49436,.T.);
#65487=ORIENTED_EDGE('',*,*,#49437,.T.);
#65488=ORIENTED_EDGE('',*,*,#49438,.T.);
#65489=ORIENTED_EDGE('',*,*,#49439,.T.);
#65490=ORIENTED_EDGE('',*,*,#49440,.T.);
#65491=ORIENTED_EDGE('',*,*,#49441,.T.);
#65492=ORIENTED_EDGE('',*,*,#49442,.T.);
#65493=ORIENTED_EDGE('',*,*,#49443,.T.);
#65494=ORIENTED_EDGE('',*,*,#49444,.T.);
#65495=ORIENTED_EDGE('',*,*,#49445,.T.);
#65496=ORIENTED_EDGE('',*,*,#49446,.T.);
#65497=ORIENTED_EDGE('',*,*,#49447,.T.);
#65498=ORIENTED_EDGE('',*,*,#49448,.T.);
#65499=ORIENTED_EDGE('',*,*,#49449,.T.);
#65500=ORIENTED_EDGE('',*,*,#49450,.T.);
#65501=ORIENTED_EDGE('',*,*,#49451,.T.);
#65502=ORIENTED_EDGE('',*,*,#49452,.T.);
#65503=ORIENTED_EDGE('',*,*,#49453,.T.);
#65504=ORIENTED_EDGE('',*,*,#49454,.T.);
#65505=ORIENTED_EDGE('',*,*,#49455,.T.);
#65506=ORIENTED_EDGE('',*,*,#49456,.T.);
#65507=ORIENTED_EDGE('',*,*,#49457,.T.);
#65508=ORIENTED_EDGE('',*,*,#49458,.T.);
#65509=ORIENTED_EDGE('',*,*,#49459,.T.);
#65510=ORIENTED_EDGE('',*,*,#49460,.T.);
#65511=ORIENTED_EDGE('',*,*,#49461,.T.);
#65512=ORIENTED_EDGE('',*,*,#49462,.T.);
#65513=ORIENTED_EDGE('',*,*,#49463,.T.);
#65514=ORIENTED_EDGE('',*,*,#49464,.T.);
#65515=ORIENTED_EDGE('',*,*,#49465,.T.);
#65516=ORIENTED_EDGE('',*,*,#49466,.T.);
#65517=ORIENTED_EDGE('',*,*,#49467,.T.);
#65518=ORIENTED_EDGE('',*,*,#49468,.T.);
#65519=ORIENTED_EDGE('',*,*,#49469,.T.);
#65520=ORIENTED_EDGE('',*,*,#49470,.T.);
#65521=ORIENTED_EDGE('',*,*,#49471,.T.);
#65522=ORIENTED_EDGE('',*,*,#49472,.T.);
#65523=ORIENTED_EDGE('',*,*,#49473,.T.);
#65524=ORIENTED_EDGE('',*,*,#49474,.T.);
#65525=ORIENTED_EDGE('',*,*,#49475,.T.);
#65526=ORIENTED_EDGE('',*,*,#49476,.T.);
#65527=ORIENTED_EDGE('',*,*,#49477,.T.);
#65528=ORIENTED_EDGE('',*,*,#49478,.T.);
#65529=ORIENTED_EDGE('',*,*,#49479,.T.);
#65530=ORIENTED_EDGE('',*,*,#49480,.T.);
#65531=ORIENTED_EDGE('',*,*,#49481,.T.);
#65532=ORIENTED_EDGE('',*,*,#49482,.T.);
#65533=ORIENTED_EDGE('',*,*,#49483,.T.);
#65534=ORIENTED_EDGE('',*,*,#49484,.T.);
#65535=ORIENTED_EDGE('',*,*,#49485,.T.);
#65536=ORIENTED_EDGE('',*,*,#49486,.T.);
#65537=ORIENTED_EDGE('',*,*,#49487,.T.);
#65538=ORIENTED_EDGE('',*,*,#49488,.T.);
#65539=ORIENTED_EDGE('',*,*,#49489,.T.);
#65540=ORIENTED_EDGE('',*,*,#49490,.T.);
#65541=ORIENTED_EDGE('',*,*,#49491,.T.);
#65542=ORIENTED_EDGE('',*,*,#49492,.T.);
#65543=ORIENTED_EDGE('',*,*,#49493,.T.);
#65544=ORIENTED_EDGE('',*,*,#49494,.T.);
#65545=ORIENTED_EDGE('',*,*,#49495,.T.);
#65546=ORIENTED_EDGE('',*,*,#49496,.T.);
#65547=ORIENTED_EDGE('',*,*,#49497,.T.);
#65548=ORIENTED_EDGE('',*,*,#49498,.T.);
#65549=ORIENTED_EDGE('',*,*,#49499,.T.);
#65550=ORIENTED_EDGE('',*,*,#49500,.T.);
#65551=ORIENTED_EDGE('',*,*,#49501,.T.);
#65552=ORIENTED_EDGE('',*,*,#49502,.T.);
#65553=ORIENTED_EDGE('',*,*,#49503,.T.);
#65554=ORIENTED_EDGE('',*,*,#49504,.T.);
#65555=ORIENTED_EDGE('',*,*,#49505,.T.);
#65556=ORIENTED_EDGE('',*,*,#49506,.T.);
#65557=ORIENTED_EDGE('',*,*,#49507,.T.);
#65558=ORIENTED_EDGE('',*,*,#49508,.T.);
#65559=ORIENTED_EDGE('',*,*,#49509,.T.);
#65560=ORIENTED_EDGE('',*,*,#49510,.T.);
#65561=ORIENTED_EDGE('',*,*,#49511,.T.);
#65562=ORIENTED_EDGE('',*,*,#49512,.T.);
#65563=ORIENTED_EDGE('',*,*,#49513,.T.);
#65564=ORIENTED_EDGE('',*,*,#49514,.T.);
#65565=ORIENTED_EDGE('',*,*,#49515,.T.);
#65566=ORIENTED_EDGE('',*,*,#49516,.T.);
#65567=ORIENTED_EDGE('',*,*,#49517,.T.);
#65568=ORIENTED_EDGE('',*,*,#49518,.T.);
#65569=ORIENTED_EDGE('',*,*,#49519,.T.);
#65570=ORIENTED_EDGE('',*,*,#49520,.T.);
#65571=ORIENTED_EDGE('',*,*,#49521,.T.);
#65572=ORIENTED_EDGE('',*,*,#49522,.T.);
#65573=ORIENTED_EDGE('',*,*,#49523,.T.);
#65574=ORIENTED_EDGE('',*,*,#49524,.T.);
#65575=ORIENTED_EDGE('',*,*,#49525,.T.);
#65576=ORIENTED_EDGE('',*,*,#49526,.T.);
#65577=ORIENTED_EDGE('',*,*,#49527,.T.);
#65578=ORIENTED_EDGE('',*,*,#49528,.T.);
#65579=ORIENTED_EDGE('',*,*,#49529,.T.);
#65580=ORIENTED_EDGE('',*,*,#49530,.T.);
#65581=ORIENTED_EDGE('',*,*,#49531,.T.);
#65582=ORIENTED_EDGE('',*,*,#49532,.T.);
#65583=ORIENTED_EDGE('',*,*,#49533,.T.);
#65584=ORIENTED_EDGE('',*,*,#49534,.T.);
#65585=ORIENTED_EDGE('',*,*,#49535,.T.);
#65586=ORIENTED_EDGE('',*,*,#49536,.T.);
#65587=ORIENTED_EDGE('',*,*,#49537,.T.);
#65588=ORIENTED_EDGE('',*,*,#49538,.T.);
#65589=ORIENTED_EDGE('',*,*,#49539,.T.);
#65590=ORIENTED_EDGE('',*,*,#49540,.T.);
#65591=ORIENTED_EDGE('',*,*,#49541,.T.);
#65592=ORIENTED_EDGE('',*,*,#49542,.T.);
#65593=ORIENTED_EDGE('',*,*,#49543,.T.);
#65594=ORIENTED_EDGE('',*,*,#49544,.T.);
#65595=ORIENTED_EDGE('',*,*,#49545,.T.);
#65596=ORIENTED_EDGE('',*,*,#49546,.T.);
#65597=ORIENTED_EDGE('',*,*,#49547,.T.);
#65598=ORIENTED_EDGE('',*,*,#49548,.T.);
#65599=ORIENTED_EDGE('',*,*,#49549,.T.);
#65600=ORIENTED_EDGE('',*,*,#49550,.T.);
#65601=ORIENTED_EDGE('',*,*,#49551,.T.);
#65602=ORIENTED_EDGE('',*,*,#49552,.T.);
#65603=ORIENTED_EDGE('',*,*,#49553,.T.);
#65604=ORIENTED_EDGE('',*,*,#49554,.T.);
#65605=ORIENTED_EDGE('',*,*,#49555,.T.);
#65606=ORIENTED_EDGE('',*,*,#49556,.T.);
#65607=ORIENTED_EDGE('',*,*,#49557,.T.);
#65608=ORIENTED_EDGE('',*,*,#49558,.T.);
#65609=ORIENTED_EDGE('',*,*,#49559,.T.);
#65610=ORIENTED_EDGE('',*,*,#49560,.T.);
#65611=ORIENTED_EDGE('',*,*,#49561,.T.);
#65612=ORIENTED_EDGE('',*,*,#49562,.T.);
#65613=ORIENTED_EDGE('',*,*,#49563,.T.);
#65614=ORIENTED_EDGE('',*,*,#49564,.T.);
#65615=ORIENTED_EDGE('',*,*,#49565,.T.);
#65616=ORIENTED_EDGE('',*,*,#49566,.T.);
#65617=ORIENTED_EDGE('',*,*,#49567,.T.);
#65618=ORIENTED_EDGE('',*,*,#49568,.T.);
#65619=ORIENTED_EDGE('',*,*,#49569,.T.);
#65620=ORIENTED_EDGE('',*,*,#49570,.T.);
#65621=ORIENTED_EDGE('',*,*,#49571,.T.);
#65622=ORIENTED_EDGE('',*,*,#49572,.T.);
#65623=ORIENTED_EDGE('',*,*,#49573,.T.);
#65624=ORIENTED_EDGE('',*,*,#49574,.T.);
#65625=ORIENTED_EDGE('',*,*,#49575,.T.);
#65626=ORIENTED_EDGE('',*,*,#49576,.T.);
#65627=ORIENTED_EDGE('',*,*,#49577,.T.);
#65628=ORIENTED_EDGE('',*,*,#49578,.T.);
#65629=ORIENTED_EDGE('',*,*,#49579,.T.);
#65630=ORIENTED_EDGE('',*,*,#49580,.T.);
#65631=ORIENTED_EDGE('',*,*,#49581,.T.);
#65632=ORIENTED_EDGE('',*,*,#49582,.T.);
#65633=ORIENTED_EDGE('',*,*,#49583,.T.);
#65634=ORIENTED_EDGE('',*,*,#49584,.T.);
#65635=ORIENTED_EDGE('',*,*,#49585,.T.);
#65636=ORIENTED_EDGE('',*,*,#49586,.T.);
#65637=ORIENTED_EDGE('',*,*,#49587,.T.);
#65638=ORIENTED_EDGE('',*,*,#49588,.T.);
#65639=ORIENTED_EDGE('',*,*,#49589,.T.);
#65640=ORIENTED_EDGE('',*,*,#49590,.T.);
#65641=ORIENTED_EDGE('',*,*,#49591,.T.);
#65642=ORIENTED_EDGE('',*,*,#49592,.T.);
#65643=ORIENTED_EDGE('',*,*,#49593,.T.);
#65644=ORIENTED_EDGE('',*,*,#49594,.T.);
#65645=ORIENTED_EDGE('',*,*,#49595,.T.);
#65646=ORIENTED_EDGE('',*,*,#49596,.T.);
#65647=ORIENTED_EDGE('',*,*,#49597,.T.);
#65648=ORIENTED_EDGE('',*,*,#49598,.T.);
#65649=ORIENTED_EDGE('',*,*,#49599,.T.);
#65650=ORIENTED_EDGE('',*,*,#49600,.T.);
#65651=ORIENTED_EDGE('',*,*,#49601,.T.);
#65652=ORIENTED_EDGE('',*,*,#49602,.T.);
#65653=ORIENTED_EDGE('',*,*,#49603,.T.);
#65654=ORIENTED_EDGE('',*,*,#49604,.T.);
#65655=ORIENTED_EDGE('',*,*,#49605,.T.);
#65656=ORIENTED_EDGE('',*,*,#49606,.T.);
#65657=ORIENTED_EDGE('',*,*,#49607,.T.);
#65658=ORIENTED_EDGE('',*,*,#49608,.T.);
#65659=ORIENTED_EDGE('',*,*,#49609,.T.);
#65660=ORIENTED_EDGE('',*,*,#49610,.T.);
#65661=ORIENTED_EDGE('',*,*,#49611,.T.);
#65662=ORIENTED_EDGE('',*,*,#49612,.T.);
#65663=ORIENTED_EDGE('',*,*,#49613,.T.);
#65664=ORIENTED_EDGE('',*,*,#49614,.T.);
#65665=ORIENTED_EDGE('',*,*,#49615,.T.);
#65666=ORIENTED_EDGE('',*,*,#49616,.T.);
#65667=ORIENTED_EDGE('',*,*,#49617,.T.);
#65668=ORIENTED_EDGE('',*,*,#49618,.T.);
#65669=ORIENTED_EDGE('',*,*,#49619,.T.);
#65670=ORIENTED_EDGE('',*,*,#49620,.T.);
#65671=ORIENTED_EDGE('',*,*,#49621,.T.);
#65672=ORIENTED_EDGE('',*,*,#49622,.T.);
#65673=ORIENTED_EDGE('',*,*,#49623,.T.);
#65674=ORIENTED_EDGE('',*,*,#49624,.T.);
#65675=ORIENTED_EDGE('',*,*,#49625,.T.);
#65676=ORIENTED_EDGE('',*,*,#49626,.T.);
#65677=ORIENTED_EDGE('',*,*,#49627,.T.);
#65678=ORIENTED_EDGE('',*,*,#49628,.T.);
#65679=ORIENTED_EDGE('',*,*,#49629,.T.);
#65680=ORIENTED_EDGE('',*,*,#49630,.T.);
#65681=ORIENTED_EDGE('',*,*,#49631,.T.);
#65682=ORIENTED_EDGE('',*,*,#49632,.T.);
#65683=ORIENTED_EDGE('',*,*,#49633,.T.);
#65684=ORIENTED_EDGE('',*,*,#49634,.T.);
#65685=ORIENTED_EDGE('',*,*,#49635,.T.);
#65686=ORIENTED_EDGE('',*,*,#49636,.T.);
#65687=ORIENTED_EDGE('',*,*,#49637,.T.);
#65688=ORIENTED_EDGE('',*,*,#49638,.T.);
#65689=ORIENTED_EDGE('',*,*,#49639,.T.);
#65690=ORIENTED_EDGE('',*,*,#49640,.T.);
#65691=ORIENTED_EDGE('',*,*,#49641,.T.);
#65692=ORIENTED_EDGE('',*,*,#49642,.T.);
#65693=ORIENTED_EDGE('',*,*,#49643,.T.);
#65694=ORIENTED_EDGE('',*,*,#49644,.T.);
#65695=ORIENTED_EDGE('',*,*,#49645,.T.);
#65696=ORIENTED_EDGE('',*,*,#49646,.T.);
#65697=ORIENTED_EDGE('',*,*,#49647,.T.);
#65698=ORIENTED_EDGE('',*,*,#49648,.T.);
#65699=ORIENTED_EDGE('',*,*,#49649,.T.);
#65700=ORIENTED_EDGE('',*,*,#49650,.T.);
#65701=ORIENTED_EDGE('',*,*,#49651,.T.);
#65702=ORIENTED_EDGE('',*,*,#49652,.T.);
#65703=ORIENTED_EDGE('',*,*,#49653,.T.);
#65704=ORIENTED_EDGE('',*,*,#49654,.T.);
#65705=ORIENTED_EDGE('',*,*,#49655,.T.);
#65706=ORIENTED_EDGE('',*,*,#49656,.T.);
#65707=ORIENTED_EDGE('',*,*,#49657,.T.);
#65708=ORIENTED_EDGE('',*,*,#49658,.T.);
#65709=ORIENTED_EDGE('',*,*,#49659,.T.);
#65710=ORIENTED_EDGE('',*,*,#49660,.T.);
#65711=ORIENTED_EDGE('',*,*,#49661,.T.);
#65712=ORIENTED_EDGE('',*,*,#49662,.T.);
#65713=ORIENTED_EDGE('',*,*,#49663,.T.);
#65714=ORIENTED_EDGE('',*,*,#49664,.T.);
#65715=ORIENTED_EDGE('',*,*,#49665,.T.);
#65716=ORIENTED_EDGE('',*,*,#49666,.T.);
#65717=ORIENTED_EDGE('',*,*,#49667,.T.);
#65718=ORIENTED_EDGE('',*,*,#49668,.T.);
#65719=ORIENTED_EDGE('',*,*,#49669,.T.);
#65720=ORIENTED_EDGE('',*,*,#49670,.T.);
#65721=ORIENTED_EDGE('',*,*,#49671,.T.);
#65722=ORIENTED_EDGE('',*,*,#49672,.T.);
#65723=ORIENTED_EDGE('',*,*,#49673,.T.);
#65724=ORIENTED_EDGE('',*,*,#49674,.T.);
#65725=ORIENTED_EDGE('',*,*,#49675,.T.);
#65726=ORIENTED_EDGE('',*,*,#49676,.T.);
#65727=ORIENTED_EDGE('',*,*,#49677,.T.);
#65728=ORIENTED_EDGE('',*,*,#49678,.T.);
#65729=ORIENTED_EDGE('',*,*,#49679,.T.);
#65730=ORIENTED_EDGE('',*,*,#49680,.T.);
#65731=ORIENTED_EDGE('',*,*,#49681,.T.);
#65732=ORIENTED_EDGE('',*,*,#49682,.T.);
#65733=ORIENTED_EDGE('',*,*,#49683,.T.);
#65734=ORIENTED_EDGE('',*,*,#49684,.T.);
#65735=ORIENTED_EDGE('',*,*,#49685,.T.);
#65736=ORIENTED_EDGE('',*,*,#49686,.T.);
#65737=ORIENTED_EDGE('',*,*,#49687,.T.);
#65738=ORIENTED_EDGE('',*,*,#49688,.T.);
#65739=ORIENTED_EDGE('',*,*,#49689,.T.);
#65740=ORIENTED_EDGE('',*,*,#49690,.T.);
#65741=ORIENTED_EDGE('',*,*,#49691,.T.);
#65742=ORIENTED_EDGE('',*,*,#49692,.T.);
#65743=ORIENTED_EDGE('',*,*,#49693,.T.);
#65744=ORIENTED_EDGE('',*,*,#49694,.T.);
#65745=ORIENTED_EDGE('',*,*,#49695,.T.);
#65746=ORIENTED_EDGE('',*,*,#49696,.T.);
#65747=ORIENTED_EDGE('',*,*,#49697,.T.);
#65748=ORIENTED_EDGE('',*,*,#49698,.T.);
#65749=ORIENTED_EDGE('',*,*,#49699,.T.);
#65750=ORIENTED_EDGE('',*,*,#49700,.T.);
#65751=ORIENTED_EDGE('',*,*,#49701,.T.);
#65752=ORIENTED_EDGE('',*,*,#49702,.T.);
#65753=ORIENTED_EDGE('',*,*,#49703,.T.);
#65754=ORIENTED_EDGE('',*,*,#49704,.T.);
#65755=ORIENTED_EDGE('',*,*,#49705,.T.);
#65756=ORIENTED_EDGE('',*,*,#49706,.T.);
#65757=ORIENTED_EDGE('',*,*,#49707,.T.);
#65758=ORIENTED_EDGE('',*,*,#49708,.T.);
#65759=ORIENTED_EDGE('',*,*,#49709,.T.);
#65760=ORIENTED_EDGE('',*,*,#49710,.T.);
#65761=ORIENTED_EDGE('',*,*,#49711,.T.);
#65762=ORIENTED_EDGE('',*,*,#49712,.T.);
#65763=ORIENTED_EDGE('',*,*,#49713,.T.);
#65764=ORIENTED_EDGE('',*,*,#49714,.T.);
#65765=ORIENTED_EDGE('',*,*,#49715,.T.);
#65766=ORIENTED_EDGE('',*,*,#49716,.T.);
#65767=ORIENTED_EDGE('',*,*,#49717,.T.);
#65768=ORIENTED_EDGE('',*,*,#49718,.T.);
#65769=ORIENTED_EDGE('',*,*,#49719,.T.);
#65770=ORIENTED_EDGE('',*,*,#49720,.T.);
#65771=ORIENTED_EDGE('',*,*,#49721,.T.);
#65772=ORIENTED_EDGE('',*,*,#49722,.T.);
#65773=ORIENTED_EDGE('',*,*,#49723,.T.);
#65774=ORIENTED_EDGE('',*,*,#49724,.T.);
#65775=ORIENTED_EDGE('',*,*,#49725,.T.);
#65776=ORIENTED_EDGE('',*,*,#49726,.T.);
#65777=ORIENTED_EDGE('',*,*,#49727,.T.);
#65778=ORIENTED_EDGE('',*,*,#49728,.T.);
#65779=ORIENTED_EDGE('',*,*,#49729,.T.);
#65780=ORIENTED_EDGE('',*,*,#49730,.T.);
#65781=ORIENTED_EDGE('',*,*,#49731,.T.);
#65782=ORIENTED_EDGE('',*,*,#45888,.T.);
#65783=ORIENTED_EDGE('',*,*,#49732,.T.);
#65784=ORIENTED_EDGE('',*,*,#45882,.T.);
#65785=ORIENTED_EDGE('',*,*,#49733,.T.);
#65786=ORIENTED_EDGE('',*,*,#49734,.T.);
#65787=ORIENTED_EDGE('',*,*,#49735,.T.);
#65788=ORIENTED_EDGE('',*,*,#49736,.T.);
#65789=ORIENTED_EDGE('',*,*,#49737,.T.);
#65790=ORIENTED_EDGE('',*,*,#49738,.T.);
#65791=ORIENTED_EDGE('',*,*,#49739,.T.);
#65792=ORIENTED_EDGE('',*,*,#49740,.T.);
#65793=ORIENTED_EDGE('',*,*,#49741,.T.);
#65794=ORIENTED_EDGE('',*,*,#49742,.T.);
#65795=ORIENTED_EDGE('',*,*,#49743,.T.);
#65796=ORIENTED_EDGE('',*,*,#49744,.T.);
#65797=ORIENTED_EDGE('',*,*,#49745,.T.);
#65798=ORIENTED_EDGE('',*,*,#49746,.T.);
#65799=ORIENTED_EDGE('',*,*,#49747,.T.);
#65800=ORIENTED_EDGE('',*,*,#49748,.T.);
#65801=ORIENTED_EDGE('',*,*,#49749,.T.);
#65802=ORIENTED_EDGE('',*,*,#49750,.T.);
#65803=ORIENTED_EDGE('',*,*,#49751,.T.);
#65804=ORIENTED_EDGE('',*,*,#49752,.T.);
#65805=ORIENTED_EDGE('',*,*,#49753,.T.);
#65806=ORIENTED_EDGE('',*,*,#49754,.T.);
#65807=ORIENTED_EDGE('',*,*,#49755,.T.);
#65808=ORIENTED_EDGE('',*,*,#49756,.T.);
#65809=ORIENTED_EDGE('',*,*,#49757,.T.);
#65810=ORIENTED_EDGE('',*,*,#49758,.T.);
#65811=ORIENTED_EDGE('',*,*,#49759,.T.);
#65812=ORIENTED_EDGE('',*,*,#49760,.T.);
#65813=ORIENTED_EDGE('',*,*,#49761,.T.);
#65814=ORIENTED_EDGE('',*,*,#49762,.T.);
#65815=ORIENTED_EDGE('',*,*,#49763,.T.);
#65816=ORIENTED_EDGE('',*,*,#49764,.T.);
#65817=ORIENTED_EDGE('',*,*,#49765,.T.);
#65818=ORIENTED_EDGE('',*,*,#49766,.T.);
#65819=ORIENTED_EDGE('',*,*,#49767,.T.);
#65820=ORIENTED_EDGE('',*,*,#49768,.T.);
#65821=ORIENTED_EDGE('',*,*,#49769,.T.);
#65822=ORIENTED_EDGE('',*,*,#49770,.T.);
#65823=ORIENTED_EDGE('',*,*,#49771,.T.);
#65824=ORIENTED_EDGE('',*,*,#49772,.T.);
#65825=ORIENTED_EDGE('',*,*,#49773,.T.);
#65826=ORIENTED_EDGE('',*,*,#49774,.T.);
#65827=ORIENTED_EDGE('',*,*,#49775,.T.);
#65828=ORIENTED_EDGE('',*,*,#49776,.T.);
#65829=ORIENTED_EDGE('',*,*,#49777,.T.);
#65830=ORIENTED_EDGE('',*,*,#49778,.T.);
#65831=ORIENTED_EDGE('',*,*,#49779,.T.);
#65832=ORIENTED_EDGE('',*,*,#49780,.T.);
#65833=ORIENTED_EDGE('',*,*,#49781,.T.);
#65834=ORIENTED_EDGE('',*,*,#49782,.T.);
#65835=ORIENTED_EDGE('',*,*,#49783,.T.);
#65836=ORIENTED_EDGE('',*,*,#49784,.T.);
#65837=ORIENTED_EDGE('',*,*,#49785,.T.);
#65838=ORIENTED_EDGE('',*,*,#49786,.T.);
#65839=ORIENTED_EDGE('',*,*,#49787,.T.);
#65840=ORIENTED_EDGE('',*,*,#49788,.T.);
#65841=ORIENTED_EDGE('',*,*,#49789,.T.);
#65842=ORIENTED_EDGE('',*,*,#49790,.T.);
#65843=ORIENTED_EDGE('',*,*,#49791,.T.);
#65844=ORIENTED_EDGE('',*,*,#49792,.T.);
#65845=ORIENTED_EDGE('',*,*,#49793,.T.);
#65846=ORIENTED_EDGE('',*,*,#49794,.T.);
#65847=ORIENTED_EDGE('',*,*,#49795,.T.);
#65848=ORIENTED_EDGE('',*,*,#49796,.T.);
#65849=ORIENTED_EDGE('',*,*,#49797,.T.);
#65850=ORIENTED_EDGE('',*,*,#49798,.T.);
#65851=ORIENTED_EDGE('',*,*,#49799,.T.);
#65852=ORIENTED_EDGE('',*,*,#49800,.T.);
#65853=ORIENTED_EDGE('',*,*,#49801,.T.);
#65854=ORIENTED_EDGE('',*,*,#49802,.T.);
#65855=ORIENTED_EDGE('',*,*,#49803,.T.);
#65856=ORIENTED_EDGE('',*,*,#49804,.T.);
#65857=ORIENTED_EDGE('',*,*,#49805,.T.);
#65858=ORIENTED_EDGE('',*,*,#49806,.T.);
#65859=ORIENTED_EDGE('',*,*,#49807,.T.);
#65860=ORIENTED_EDGE('',*,*,#49808,.T.);
#65861=ORIENTED_EDGE('',*,*,#49809,.T.);
#65862=ORIENTED_EDGE('',*,*,#49810,.T.);
#65863=ORIENTED_EDGE('',*,*,#49811,.T.);
#65864=ORIENTED_EDGE('',*,*,#49812,.T.);
#65865=ORIENTED_EDGE('',*,*,#49813,.T.);
#65866=ORIENTED_EDGE('',*,*,#49814,.T.);
#65867=ORIENTED_EDGE('',*,*,#49815,.T.);
#65868=ORIENTED_EDGE('',*,*,#49816,.T.);
#65869=ORIENTED_EDGE('',*,*,#49817,.T.);
#65870=ORIENTED_EDGE('',*,*,#49818,.T.);
#65871=ORIENTED_EDGE('',*,*,#49819,.T.);
#65872=ORIENTED_EDGE('',*,*,#49820,.T.);
#65873=ORIENTED_EDGE('',*,*,#49821,.T.);
#65874=ORIENTED_EDGE('',*,*,#49822,.T.);
#65875=ORIENTED_EDGE('',*,*,#49823,.T.);
#65876=ORIENTED_EDGE('',*,*,#49824,.T.);
#65877=ORIENTED_EDGE('',*,*,#49825,.T.);
#65878=ORIENTED_EDGE('',*,*,#49826,.T.);
#65879=ORIENTED_EDGE('',*,*,#49827,.T.);
#65880=ORIENTED_EDGE('',*,*,#49828,.T.);
#65881=ORIENTED_EDGE('',*,*,#49829,.T.);
#65882=ORIENTED_EDGE('',*,*,#49830,.T.);
#65883=ORIENTED_EDGE('',*,*,#49831,.T.);
#65884=ORIENTED_EDGE('',*,*,#49832,.T.);
#65885=ORIENTED_EDGE('',*,*,#49833,.T.);
#65886=ORIENTED_EDGE('',*,*,#49834,.T.);
#65887=ORIENTED_EDGE('',*,*,#49835,.T.);
#65888=ORIENTED_EDGE('',*,*,#49836,.T.);
#65889=ORIENTED_EDGE('',*,*,#49837,.T.);
#65890=ORIENTED_EDGE('',*,*,#49838,.T.);
#65891=ORIENTED_EDGE('',*,*,#49839,.T.);
#65892=ORIENTED_EDGE('',*,*,#49840,.T.);
#65893=ORIENTED_EDGE('',*,*,#49841,.T.);
#65894=ORIENTED_EDGE('',*,*,#49842,.T.);
#65895=ORIENTED_EDGE('',*,*,#49843,.T.);
#65896=ORIENTED_EDGE('',*,*,#49844,.T.);
#65897=ORIENTED_EDGE('',*,*,#49845,.T.);
#65898=ORIENTED_EDGE('',*,*,#49846,.T.);
#65899=ORIENTED_EDGE('',*,*,#49847,.T.);
#65900=ORIENTED_EDGE('',*,*,#49848,.T.);
#65901=ORIENTED_EDGE('',*,*,#49849,.T.);
#65902=ORIENTED_EDGE('',*,*,#49850,.T.);
#65903=ORIENTED_EDGE('',*,*,#49851,.T.);
#65904=ORIENTED_EDGE('',*,*,#49852,.T.);
#65905=ORIENTED_EDGE('',*,*,#49853,.T.);
#65906=ORIENTED_EDGE('',*,*,#49854,.T.);
#65907=ORIENTED_EDGE('',*,*,#49855,.T.);
#65908=ORIENTED_EDGE('',*,*,#49856,.T.);
#65909=ORIENTED_EDGE('',*,*,#49857,.T.);
#65910=ORIENTED_EDGE('',*,*,#49858,.T.);
#65911=ORIENTED_EDGE('',*,*,#49859,.T.);
#65912=ORIENTED_EDGE('',*,*,#49860,.T.);
#65913=ORIENTED_EDGE('',*,*,#49861,.T.);
#65914=ORIENTED_EDGE('',*,*,#49862,.T.);
#65915=ORIENTED_EDGE('',*,*,#49863,.T.);
#65916=ORIENTED_EDGE('',*,*,#49864,.T.);
#65917=ORIENTED_EDGE('',*,*,#49865,.T.);
#65918=ORIENTED_EDGE('',*,*,#49866,.T.);
#65919=ORIENTED_EDGE('',*,*,#49867,.T.);
#65920=ORIENTED_EDGE('',*,*,#49868,.T.);
#65921=ORIENTED_EDGE('',*,*,#49869,.T.);
#65922=ORIENTED_EDGE('',*,*,#49870,.T.);
#65923=ORIENTED_EDGE('',*,*,#49871,.T.);
#65924=ORIENTED_EDGE('',*,*,#49872,.T.);
#65925=ORIENTED_EDGE('',*,*,#49873,.T.);
#65926=ORIENTED_EDGE('',*,*,#49874,.T.);
#65927=ORIENTED_EDGE('',*,*,#49875,.T.);
#65928=ORIENTED_EDGE('',*,*,#49876,.T.);
#65929=ORIENTED_EDGE('',*,*,#49877,.T.);
#65930=ORIENTED_EDGE('',*,*,#49878,.T.);
#65931=ORIENTED_EDGE('',*,*,#49879,.T.);
#65932=ORIENTED_EDGE('',*,*,#49880,.T.);
#65933=ORIENTED_EDGE('',*,*,#49881,.T.);
#65934=ORIENTED_EDGE('',*,*,#49882,.T.);
#65935=ORIENTED_EDGE('',*,*,#49883,.T.);
#65936=ORIENTED_EDGE('',*,*,#49884,.T.);
#65937=ORIENTED_EDGE('',*,*,#49885,.T.);
#65938=ORIENTED_EDGE('',*,*,#49886,.T.);
#65939=ORIENTED_EDGE('',*,*,#49887,.T.);
#65940=ORIENTED_EDGE('',*,*,#49888,.T.);
#65941=ORIENTED_EDGE('',*,*,#49889,.T.);
#65942=ORIENTED_EDGE('',*,*,#49890,.T.);
#65943=ORIENTED_EDGE('',*,*,#49891,.T.);
#65944=ORIENTED_EDGE('',*,*,#49892,.T.);
#65945=ORIENTED_EDGE('',*,*,#49893,.T.);
#65946=ORIENTED_EDGE('',*,*,#49894,.T.);
#65947=ORIENTED_EDGE('',*,*,#49895,.T.);
#65948=ORIENTED_EDGE('',*,*,#49896,.T.);
#65949=ORIENTED_EDGE('',*,*,#49897,.T.);
#65950=ORIENTED_EDGE('',*,*,#49898,.T.);
#65951=ORIENTED_EDGE('',*,*,#49899,.T.);
#65952=ORIENTED_EDGE('',*,*,#49900,.T.);
#65953=ORIENTED_EDGE('',*,*,#49901,.T.);
#65954=ORIENTED_EDGE('',*,*,#49902,.T.);
#65955=ORIENTED_EDGE('',*,*,#49903,.T.);
#65956=ORIENTED_EDGE('',*,*,#49904,.T.);
#65957=ORIENTED_EDGE('',*,*,#49905,.T.);
#65958=ORIENTED_EDGE('',*,*,#49906,.T.);
#65959=ORIENTED_EDGE('',*,*,#49907,.T.);
#65960=ORIENTED_EDGE('',*,*,#49908,.T.);
#65961=ORIENTED_EDGE('',*,*,#49909,.T.);
#65962=ORIENTED_EDGE('',*,*,#49910,.T.);
#65963=ORIENTED_EDGE('',*,*,#49911,.T.);
#65964=ORIENTED_EDGE('',*,*,#49912,.T.);
#65965=ORIENTED_EDGE('',*,*,#49913,.T.);
#65966=ORIENTED_EDGE('',*,*,#49914,.T.);
#65967=ORIENTED_EDGE('',*,*,#49915,.T.);
#65968=ORIENTED_EDGE('',*,*,#49916,.T.);
#65969=ORIENTED_EDGE('',*,*,#49917,.T.);
#65970=ORIENTED_EDGE('',*,*,#49918,.T.);
#65971=ORIENTED_EDGE('',*,*,#49919,.T.);
#65972=ORIENTED_EDGE('',*,*,#49920,.T.);
#65973=ORIENTED_EDGE('',*,*,#49921,.T.);
#65974=ORIENTED_EDGE('',*,*,#49922,.T.);
#65975=ORIENTED_EDGE('',*,*,#49923,.T.);
#65976=ORIENTED_EDGE('',*,*,#49924,.T.);
#65977=ORIENTED_EDGE('',*,*,#49925,.T.);
#65978=ORIENTED_EDGE('',*,*,#49926,.T.);
#65979=ORIENTED_EDGE('',*,*,#49927,.T.);
#65980=ORIENTED_EDGE('',*,*,#49928,.T.);
#65981=ORIENTED_EDGE('',*,*,#49929,.T.);
#65982=ORIENTED_EDGE('',*,*,#49930,.T.);
#65983=ORIENTED_EDGE('',*,*,#49931,.T.);
#65984=ORIENTED_EDGE('',*,*,#49932,.T.);
#65985=ORIENTED_EDGE('',*,*,#49933,.T.);
#65986=ORIENTED_EDGE('',*,*,#49934,.T.);
#65987=ORIENTED_EDGE('',*,*,#49935,.T.);
#65988=ORIENTED_EDGE('',*,*,#49936,.T.);
#65989=ORIENTED_EDGE('',*,*,#49937,.T.);
#65990=ORIENTED_EDGE('',*,*,#49938,.T.);
#65991=ORIENTED_EDGE('',*,*,#49939,.T.);
#65992=ORIENTED_EDGE('',*,*,#49940,.T.);
#65993=ORIENTED_EDGE('',*,*,#49941,.T.);
#65994=ORIENTED_EDGE('',*,*,#49942,.T.);
#65995=ORIENTED_EDGE('',*,*,#49943,.T.);
#65996=ORIENTED_EDGE('',*,*,#49944,.T.);
#65997=ORIENTED_EDGE('',*,*,#49945,.T.);
#65998=ORIENTED_EDGE('',*,*,#49946,.T.);
#65999=ORIENTED_EDGE('',*,*,#49947,.T.);
#66000=ORIENTED_EDGE('',*,*,#49948,.T.);
#66001=ORIENTED_EDGE('',*,*,#49949,.T.);
#66002=ORIENTED_EDGE('',*,*,#49950,.T.);
#66003=ORIENTED_EDGE('',*,*,#49951,.T.);
#66004=ORIENTED_EDGE('',*,*,#49952,.T.);
#66005=ORIENTED_EDGE('',*,*,#49953,.T.);
#66006=ORIENTED_EDGE('',*,*,#49954,.T.);
#66007=ORIENTED_EDGE('',*,*,#49955,.T.);
#66008=ORIENTED_EDGE('',*,*,#49956,.T.);
#66009=ORIENTED_EDGE('',*,*,#49957,.T.);
#66010=ORIENTED_EDGE('',*,*,#49958,.T.);
#66011=ORIENTED_EDGE('',*,*,#49959,.T.);
#66012=ORIENTED_EDGE('',*,*,#49960,.T.);
#66013=ORIENTED_EDGE('',*,*,#49961,.T.);
#66014=ORIENTED_EDGE('',*,*,#49962,.T.);
#66015=ORIENTED_EDGE('',*,*,#49963,.T.);
#66016=ORIENTED_EDGE('',*,*,#49964,.T.);
#66017=ORIENTED_EDGE('',*,*,#49965,.T.);
#66018=ORIENTED_EDGE('',*,*,#49966,.T.);
#66019=ORIENTED_EDGE('',*,*,#49967,.T.);
#66020=ORIENTED_EDGE('',*,*,#49968,.T.);
#66021=ORIENTED_EDGE('',*,*,#49969,.T.);
#66022=ORIENTED_EDGE('',*,*,#49970,.T.);
#66023=ORIENTED_EDGE('',*,*,#49971,.T.);
#66024=ORIENTED_EDGE('',*,*,#49972,.T.);
#66025=ORIENTED_EDGE('',*,*,#49973,.T.);
#66026=ORIENTED_EDGE('',*,*,#49974,.T.);
#66027=ORIENTED_EDGE('',*,*,#49975,.T.);
#66028=ORIENTED_EDGE('',*,*,#49976,.T.);
#66029=ORIENTED_EDGE('',*,*,#49977,.T.);
#66030=ORIENTED_EDGE('',*,*,#49978,.T.);
#66031=ORIENTED_EDGE('',*,*,#49979,.T.);
#66032=ORIENTED_EDGE('',*,*,#49980,.T.);
#66033=ORIENTED_EDGE('',*,*,#49981,.T.);
#66034=ORIENTED_EDGE('',*,*,#49982,.T.);
#66035=ORIENTED_EDGE('',*,*,#49983,.T.);
#66036=ORIENTED_EDGE('',*,*,#49984,.T.);
#66037=ORIENTED_EDGE('',*,*,#49985,.T.);
#66038=ORIENTED_EDGE('',*,*,#49986,.T.);
#66039=ORIENTED_EDGE('',*,*,#49987,.T.);
#66040=ORIENTED_EDGE('',*,*,#49988,.T.);
#66041=ORIENTED_EDGE('',*,*,#49989,.T.);
#66042=ORIENTED_EDGE('',*,*,#49990,.T.);
#66043=ORIENTED_EDGE('',*,*,#49991,.T.);
#66044=ORIENTED_EDGE('',*,*,#49992,.T.);
#66045=ORIENTED_EDGE('',*,*,#49993,.T.);
#66046=ORIENTED_EDGE('',*,*,#49994,.T.);
#66047=ORIENTED_EDGE('',*,*,#49995,.T.);
#66048=ORIENTED_EDGE('',*,*,#49996,.T.);
#66049=ORIENTED_EDGE('',*,*,#49997,.T.);
#66050=ORIENTED_EDGE('',*,*,#49998,.T.);
#66051=ORIENTED_EDGE('',*,*,#49999,.T.);
#66052=ORIENTED_EDGE('',*,*,#50000,.T.);
#66053=ORIENTED_EDGE('',*,*,#50001,.T.);
#66054=ORIENTED_EDGE('',*,*,#50002,.T.);
#66055=ORIENTED_EDGE('',*,*,#50003,.T.);
#66056=ORIENTED_EDGE('',*,*,#50004,.T.);
#66057=ORIENTED_EDGE('',*,*,#50005,.T.);
#66058=ORIENTED_EDGE('',*,*,#50006,.T.);
#66059=ORIENTED_EDGE('',*,*,#50007,.T.);
#66060=ORIENTED_EDGE('',*,*,#50008,.T.);
#66061=ORIENTED_EDGE('',*,*,#50009,.T.);
#66062=ORIENTED_EDGE('',*,*,#50010,.T.);
#66063=ORIENTED_EDGE('',*,*,#50011,.T.);
#66064=ORIENTED_EDGE('',*,*,#50012,.T.);
#66065=ORIENTED_EDGE('',*,*,#50013,.T.);
#66066=ORIENTED_EDGE('',*,*,#50014,.T.);
#66067=ORIENTED_EDGE('',*,*,#50015,.T.);
#66068=ORIENTED_EDGE('',*,*,#50016,.T.);
#66069=ORIENTED_EDGE('',*,*,#50017,.T.);
#66070=ORIENTED_EDGE('',*,*,#50018,.T.);
#66071=ORIENTED_EDGE('',*,*,#50019,.T.);
#66072=ORIENTED_EDGE('',*,*,#50020,.T.);
#66073=ORIENTED_EDGE('',*,*,#50021,.T.);
#66074=ORIENTED_EDGE('',*,*,#50022,.T.);
#66075=ORIENTED_EDGE('',*,*,#50023,.T.);
#66076=ORIENTED_EDGE('',*,*,#50024,.T.);
#66077=ORIENTED_EDGE('',*,*,#50025,.T.);
#66078=ORIENTED_EDGE('',*,*,#50026,.T.);
#66079=ORIENTED_EDGE('',*,*,#50027,.T.);
#66080=ORIENTED_EDGE('',*,*,#50028,.T.);
#66081=ORIENTED_EDGE('',*,*,#50029,.T.);
#66082=ORIENTED_EDGE('',*,*,#50030,.T.);
#66083=ORIENTED_EDGE('',*,*,#50031,.T.);
#66084=ORIENTED_EDGE('',*,*,#50032,.T.);
#66085=ORIENTED_EDGE('',*,*,#50033,.T.);
#66086=ORIENTED_EDGE('',*,*,#50034,.T.);
#66087=ORIENTED_EDGE('',*,*,#50035,.T.);
#66088=ORIENTED_EDGE('',*,*,#50036,.T.);
#66089=ORIENTED_EDGE('',*,*,#50037,.T.);
#66090=ORIENTED_EDGE('',*,*,#50038,.T.);
#66091=ORIENTED_EDGE('',*,*,#50039,.T.);
#66092=ORIENTED_EDGE('',*,*,#50040,.T.);
#66093=ORIENTED_EDGE('',*,*,#50041,.T.);
#66094=ORIENTED_EDGE('',*,*,#50042,.T.);
#66095=ORIENTED_EDGE('',*,*,#50043,.T.);
#66096=ORIENTED_EDGE('',*,*,#50044,.T.);
#66097=ORIENTED_EDGE('',*,*,#50045,.T.);
#66098=ORIENTED_EDGE('',*,*,#50046,.T.);
#66099=ORIENTED_EDGE('',*,*,#50047,.T.);
#66100=ORIENTED_EDGE('',*,*,#50048,.T.);
#66101=ORIENTED_EDGE('',*,*,#50049,.T.);
#66102=ORIENTED_EDGE('',*,*,#50050,.T.);
#66103=ORIENTED_EDGE('',*,*,#50051,.T.);
#66104=ORIENTED_EDGE('',*,*,#50052,.T.);
#66105=ORIENTED_EDGE('',*,*,#50053,.T.);
#66106=ORIENTED_EDGE('',*,*,#50054,.T.);
#66107=ORIENTED_EDGE('',*,*,#50055,.T.);
#66108=ORIENTED_EDGE('',*,*,#50056,.T.);
#66109=ORIENTED_EDGE('',*,*,#50057,.T.);
#66110=ORIENTED_EDGE('',*,*,#50058,.T.);
#66111=ORIENTED_EDGE('',*,*,#50059,.T.);
#66112=ORIENTED_EDGE('',*,*,#50060,.T.);
#66113=ORIENTED_EDGE('',*,*,#50061,.T.);
#66114=ORIENTED_EDGE('',*,*,#50062,.T.);
#66115=ORIENTED_EDGE('',*,*,#50063,.T.);
#66116=ORIENTED_EDGE('',*,*,#50064,.T.);
#66117=ORIENTED_EDGE('',*,*,#50065,.T.);
#66118=ORIENTED_EDGE('',*,*,#50066,.T.);
#66119=ORIENTED_EDGE('',*,*,#50067,.T.);
#66120=ORIENTED_EDGE('',*,*,#50068,.T.);
#66121=ORIENTED_EDGE('',*,*,#50069,.T.);
#66122=ORIENTED_EDGE('',*,*,#50070,.T.);
#66123=ORIENTED_EDGE('',*,*,#50071,.T.);
#66124=ORIENTED_EDGE('',*,*,#50072,.T.);
#66125=ORIENTED_EDGE('',*,*,#50073,.T.);
#66126=ORIENTED_EDGE('',*,*,#50074,.T.);
#66127=ORIENTED_EDGE('',*,*,#50075,.T.);
#66128=ORIENTED_EDGE('',*,*,#50076,.T.);
#66129=ORIENTED_EDGE('',*,*,#50077,.T.);
#66130=ORIENTED_EDGE('',*,*,#50078,.T.);
#66131=ORIENTED_EDGE('',*,*,#50079,.T.);
#66132=ORIENTED_EDGE('',*,*,#50080,.T.);
#66133=ORIENTED_EDGE('',*,*,#50081,.T.);
#66134=ORIENTED_EDGE('',*,*,#50082,.T.);
#66135=ORIENTED_EDGE('',*,*,#50083,.T.);
#66136=ORIENTED_EDGE('',*,*,#50084,.T.);
#66137=ORIENTED_EDGE('',*,*,#50085,.T.);
#66138=ORIENTED_EDGE('',*,*,#50086,.T.);
#66139=ORIENTED_EDGE('',*,*,#50087,.T.);
#66140=ORIENTED_EDGE('',*,*,#50088,.T.);
#66141=ORIENTED_EDGE('',*,*,#50089,.T.);
#66142=ORIENTED_EDGE('',*,*,#50090,.T.);
#66143=ORIENTED_EDGE('',*,*,#50091,.T.);
#66144=ORIENTED_EDGE('',*,*,#50092,.T.);
#66145=ORIENTED_EDGE('',*,*,#50093,.T.);
#66146=ORIENTED_EDGE('',*,*,#50094,.T.);
#66147=ORIENTED_EDGE('',*,*,#50095,.T.);
#66148=ORIENTED_EDGE('',*,*,#50096,.T.);
#66149=ORIENTED_EDGE('',*,*,#50097,.T.);
#66150=ORIENTED_EDGE('',*,*,#50098,.T.);
#66151=ORIENTED_EDGE('',*,*,#50099,.T.);
#66152=ORIENTED_EDGE('',*,*,#50100,.T.);
#66153=ORIENTED_EDGE('',*,*,#50101,.T.);
#66154=ORIENTED_EDGE('',*,*,#50102,.T.);
#66155=ORIENTED_EDGE('',*,*,#50103,.T.);
#66156=ORIENTED_EDGE('',*,*,#50104,.T.);
#66157=ORIENTED_EDGE('',*,*,#50105,.T.);
#66158=ORIENTED_EDGE('',*,*,#50106,.T.);
#66159=ORIENTED_EDGE('',*,*,#50107,.T.);
#66160=ORIENTED_EDGE('',*,*,#50108,.T.);
#66161=ORIENTED_EDGE('',*,*,#50109,.T.);
#66162=ORIENTED_EDGE('',*,*,#50110,.T.);
#66163=ORIENTED_EDGE('',*,*,#50111,.T.);
#66164=ORIENTED_EDGE('',*,*,#50112,.T.);
#66165=ORIENTED_EDGE('',*,*,#50113,.T.);
#66166=ORIENTED_EDGE('',*,*,#50114,.T.);
#66167=ORIENTED_EDGE('',*,*,#50115,.T.);
#66168=ORIENTED_EDGE('',*,*,#50116,.T.);
#66169=ORIENTED_EDGE('',*,*,#50117,.T.);
#66170=ORIENTED_EDGE('',*,*,#50118,.T.);
#66171=ORIENTED_EDGE('',*,*,#50119,.T.);
#66172=ORIENTED_EDGE('',*,*,#50120,.T.);
#66173=ORIENTED_EDGE('',*,*,#50121,.T.);
#66174=ORIENTED_EDGE('',*,*,#50122,.T.);
#66175=ORIENTED_EDGE('',*,*,#50123,.T.);
#66176=ORIENTED_EDGE('',*,*,#50124,.T.);
#66177=ORIENTED_EDGE('',*,*,#50125,.T.);
#66178=ORIENTED_EDGE('',*,*,#50126,.T.);
#66179=ORIENTED_EDGE('',*,*,#50127,.T.);
#66180=ORIENTED_EDGE('',*,*,#50128,.T.);
#66181=ORIENTED_EDGE('',*,*,#50129,.T.);
#66182=ORIENTED_EDGE('',*,*,#50130,.T.);
#66183=ORIENTED_EDGE('',*,*,#50131,.T.);
#66184=ORIENTED_EDGE('',*,*,#50132,.T.);
#66185=ORIENTED_EDGE('',*,*,#50133,.T.);
#66186=ORIENTED_EDGE('',*,*,#50134,.T.);
#66187=ORIENTED_EDGE('',*,*,#50135,.T.);
#66188=ORIENTED_EDGE('',*,*,#50136,.T.);
#66189=ORIENTED_EDGE('',*,*,#50137,.T.);
#66190=ORIENTED_EDGE('',*,*,#50138,.T.);
#66191=ORIENTED_EDGE('',*,*,#50139,.T.);
#66192=ORIENTED_EDGE('',*,*,#50140,.T.);
#66193=ORIENTED_EDGE('',*,*,#50141,.T.);
#66194=ORIENTED_EDGE('',*,*,#50142,.T.);
#66195=ORIENTED_EDGE('',*,*,#50143,.T.);
#66196=ORIENTED_EDGE('',*,*,#50144,.T.);
#66197=ORIENTED_EDGE('',*,*,#50145,.T.);
#66198=ORIENTED_EDGE('',*,*,#50146,.T.);
#66199=ORIENTED_EDGE('',*,*,#50147,.T.);
#66200=ORIENTED_EDGE('',*,*,#50148,.T.);
#66201=ORIENTED_EDGE('',*,*,#48519,.F.);
#66202=ORIENTED_EDGE('',*,*,#50149,.T.);
#66203=ORIENTED_EDGE('',*,*,#48501,.F.);
#66204=ORIENTED_EDGE('',*,*,#50150,.T.);
#66205=ORIENTED_EDGE('',*,*,#48503,.F.);
#66206=ORIENTED_EDGE('',*,*,#50151,.T.);
#66207=ORIENTED_EDGE('',*,*,#48507,.F.);
#66208=ORIENTED_EDGE('',*,*,#50152,.T.);
#66209=ORIENTED_EDGE('',*,*,#48547,.F.);
#66210=ORIENTED_EDGE('',*,*,#50153,.T.);
#66211=ORIENTED_EDGE('',*,*,#48529,.F.);
#66212=ORIENTED_EDGE('',*,*,#50154,.T.);
#66213=ORIENTED_EDGE('',*,*,#48531,.F.);
#66214=ORIENTED_EDGE('',*,*,#50155,.T.);
#66215=ORIENTED_EDGE('',*,*,#48535,.F.);
#66216=ORIENTED_EDGE('',*,*,#50156,.T.);
#66217=ORIENTED_EDGE('',*,*,#48575,.F.);
#66218=ORIENTED_EDGE('',*,*,#50157,.T.);
#66219=ORIENTED_EDGE('',*,*,#48557,.F.);
#66220=ORIENTED_EDGE('',*,*,#50158,.T.);
#66221=ORIENTED_EDGE('',*,*,#48559,.F.);
#66222=ORIENTED_EDGE('',*,*,#50159,.T.);
#66223=ORIENTED_EDGE('',*,*,#48563,.F.);
#66224=ORIENTED_EDGE('',*,*,#50160,.T.);
#66225=ORIENTED_EDGE('',*,*,#48603,.F.);
#66226=ORIENTED_EDGE('',*,*,#50161,.T.);
#66227=ORIENTED_EDGE('',*,*,#48585,.F.);
#66228=ORIENTED_EDGE('',*,*,#50162,.T.);
#66229=ORIENTED_EDGE('',*,*,#48587,.F.);
#66230=ORIENTED_EDGE('',*,*,#50163,.T.);
#66231=ORIENTED_EDGE('',*,*,#48591,.F.);
#66232=ORIENTED_EDGE('',*,*,#50164,.T.);
#66233=ORIENTED_EDGE('',*,*,#48631,.F.);
#66234=ORIENTED_EDGE('',*,*,#50165,.T.);
#66235=ORIENTED_EDGE('',*,*,#48613,.F.);
#66236=ORIENTED_EDGE('',*,*,#50166,.T.);
#66237=ORIENTED_EDGE('',*,*,#48615,.F.);
#66238=ORIENTED_EDGE('',*,*,#50167,.T.);
#66239=ORIENTED_EDGE('',*,*,#48619,.F.);
#66240=ORIENTED_EDGE('',*,*,#50168,.T.);
#66241=ORIENTED_EDGE('',*,*,#48659,.F.);
#66242=ORIENTED_EDGE('',*,*,#50169,.T.);
#66243=ORIENTED_EDGE('',*,*,#48641,.F.);
#66244=ORIENTED_EDGE('',*,*,#50170,.T.);
#66245=ORIENTED_EDGE('',*,*,#48643,.F.);
#66246=ORIENTED_EDGE('',*,*,#50171,.T.);
#66247=ORIENTED_EDGE('',*,*,#48647,.F.);
#66248=ORIENTED_EDGE('',*,*,#50172,.T.);
#66249=ORIENTED_EDGE('',*,*,#48687,.F.);
#66250=ORIENTED_EDGE('',*,*,#50173,.T.);
#66251=ORIENTED_EDGE('',*,*,#48669,.F.);
#66252=ORIENTED_EDGE('',*,*,#50174,.T.);
#66253=ORIENTED_EDGE('',*,*,#48671,.F.);
#66254=ORIENTED_EDGE('',*,*,#50175,.T.);
#66255=ORIENTED_EDGE('',*,*,#48675,.F.);
#66256=ORIENTED_EDGE('',*,*,#50176,.T.);
#66257=ORIENTED_EDGE('',*,*,#48715,.F.);
#66258=ORIENTED_EDGE('',*,*,#50177,.T.);
#66259=ORIENTED_EDGE('',*,*,#48697,.F.);
#66260=ORIENTED_EDGE('',*,*,#50178,.T.);
#66261=ORIENTED_EDGE('',*,*,#48699,.F.);
#66262=ORIENTED_EDGE('',*,*,#50179,.T.);
#66263=ORIENTED_EDGE('',*,*,#48703,.F.);
#66264=ORIENTED_EDGE('',*,*,#50180,.T.);
#66265=ORIENTED_EDGE('',*,*,#48743,.F.);
#66266=ORIENTED_EDGE('',*,*,#50181,.T.);
#66267=ORIENTED_EDGE('',*,*,#48725,.F.);
#66268=ORIENTED_EDGE('',*,*,#50182,.T.);
#66269=ORIENTED_EDGE('',*,*,#48727,.F.);
#66270=ORIENTED_EDGE('',*,*,#50183,.T.);
#66271=ORIENTED_EDGE('',*,*,#48731,.F.);
#66272=ORIENTED_EDGE('',*,*,#50184,.T.);
#66273=ORIENTED_EDGE('',*,*,#48771,.F.);
#66274=ORIENTED_EDGE('',*,*,#50185,.T.);
#66275=ORIENTED_EDGE('',*,*,#48753,.F.);
#66276=ORIENTED_EDGE('',*,*,#50186,.T.);
#66277=ORIENTED_EDGE('',*,*,#48755,.F.);
#66278=ORIENTED_EDGE('',*,*,#50187,.T.);
#66279=ORIENTED_EDGE('',*,*,#48759,.F.);
#66280=ORIENTED_EDGE('',*,*,#50188,.T.);
#66281=ORIENTED_EDGE('',*,*,#48799,.F.);
#66282=ORIENTED_EDGE('',*,*,#50189,.T.);
#66283=ORIENTED_EDGE('',*,*,#48781,.F.);
#66284=ORIENTED_EDGE('',*,*,#50190,.T.);
#66285=ORIENTED_EDGE('',*,*,#48783,.F.);
#66286=ORIENTED_EDGE('',*,*,#50191,.T.);
#66287=ORIENTED_EDGE('',*,*,#48787,.F.);
#66288=ORIENTED_EDGE('',*,*,#50192,.T.);
#66289=ORIENTED_EDGE('',*,*,#48827,.F.);
#66290=ORIENTED_EDGE('',*,*,#50193,.T.);
#66291=ORIENTED_EDGE('',*,*,#48809,.F.);
#66292=ORIENTED_EDGE('',*,*,#50194,.T.);
#66293=ORIENTED_EDGE('',*,*,#48811,.F.);
#66294=ORIENTED_EDGE('',*,*,#50195,.T.);
#66295=ORIENTED_EDGE('',*,*,#48815,.F.);
#66296=ORIENTED_EDGE('',*,*,#50196,.T.);
#66297=ORIENTED_EDGE('',*,*,#48855,.F.);
#66298=ORIENTED_EDGE('',*,*,#50197,.T.);
#66299=ORIENTED_EDGE('',*,*,#48837,.F.);
#66300=ORIENTED_EDGE('',*,*,#50198,.T.);
#66301=ORIENTED_EDGE('',*,*,#48839,.F.);
#66302=ORIENTED_EDGE('',*,*,#50199,.T.);
#66303=ORIENTED_EDGE('',*,*,#48843,.F.);
#66304=ORIENTED_EDGE('',*,*,#50200,.T.);
#66305=ORIENTED_EDGE('',*,*,#48883,.F.);
#66306=ORIENTED_EDGE('',*,*,#50201,.T.);
#66307=ORIENTED_EDGE('',*,*,#48865,.F.);
#66308=ORIENTED_EDGE('',*,*,#50202,.T.);
#66309=ORIENTED_EDGE('',*,*,#48867,.F.);
#66310=ORIENTED_EDGE('',*,*,#50203,.T.);
#66311=ORIENTED_EDGE('',*,*,#48871,.F.);
#66312=ORIENTED_EDGE('',*,*,#50204,.T.);
#66313=ORIENTED_EDGE('',*,*,#48911,.F.);
#66314=ORIENTED_EDGE('',*,*,#50205,.T.);
#66315=ORIENTED_EDGE('',*,*,#48893,.F.);
#66316=ORIENTED_EDGE('',*,*,#50206,.T.);
#66317=ORIENTED_EDGE('',*,*,#48895,.F.);
#66318=ORIENTED_EDGE('',*,*,#50207,.T.);
#66319=ORIENTED_EDGE('',*,*,#48899,.F.);
#66320=ORIENTED_EDGE('',*,*,#50208,.T.);
#66321=ORIENTED_EDGE('',*,*,#48939,.F.);
#66322=ORIENTED_EDGE('',*,*,#50209,.T.);
#66323=ORIENTED_EDGE('',*,*,#48921,.F.);
#66324=ORIENTED_EDGE('',*,*,#50210,.T.);
#66325=ORIENTED_EDGE('',*,*,#48923,.F.);
#66326=ORIENTED_EDGE('',*,*,#50211,.T.);
#66327=ORIENTED_EDGE('',*,*,#48927,.F.);
#66328=ORIENTED_EDGE('',*,*,#50212,.T.);
#66329=ORIENTED_EDGE('',*,*,#48967,.F.);
#66330=ORIENTED_EDGE('',*,*,#50213,.T.);
#66331=ORIENTED_EDGE('',*,*,#48949,.F.);
#66332=ORIENTED_EDGE('',*,*,#50214,.T.);
#66333=ORIENTED_EDGE('',*,*,#48951,.F.);
#66334=ORIENTED_EDGE('',*,*,#50215,.T.);
#66335=ORIENTED_EDGE('',*,*,#48955,.F.);
#66336=ORIENTED_EDGE('',*,*,#50216,.T.);
#66337=ORIENTED_EDGE('',*,*,#48995,.F.);
#66338=ORIENTED_EDGE('',*,*,#50217,.T.);
#66339=ORIENTED_EDGE('',*,*,#48977,.F.);
#66340=ORIENTED_EDGE('',*,*,#50218,.T.);
#66341=ORIENTED_EDGE('',*,*,#48979,.F.);
#66342=ORIENTED_EDGE('',*,*,#50219,.T.);
#66343=ORIENTED_EDGE('',*,*,#48983,.F.);
#66344=ORIENTED_EDGE('',*,*,#50220,.T.);
#66345=ORIENTED_EDGE('',*,*,#49023,.F.);
#66346=ORIENTED_EDGE('',*,*,#50221,.T.);
#66347=ORIENTED_EDGE('',*,*,#49005,.F.);
#66348=ORIENTED_EDGE('',*,*,#50222,.T.);
#66349=ORIENTED_EDGE('',*,*,#49007,.F.);
#66350=ORIENTED_EDGE('',*,*,#50223,.T.);
#66351=ORIENTED_EDGE('',*,*,#49011,.F.);
#66352=ORIENTED_EDGE('',*,*,#50224,.T.);
#66353=ORIENTED_EDGE('',*,*,#49051,.F.);
#66354=ORIENTED_EDGE('',*,*,#50225,.T.);
#66355=ORIENTED_EDGE('',*,*,#49033,.F.);
#66356=ORIENTED_EDGE('',*,*,#50226,.T.);
#66357=ORIENTED_EDGE('',*,*,#49035,.F.);
#66358=ORIENTED_EDGE('',*,*,#50227,.T.);
#66359=ORIENTED_EDGE('',*,*,#49039,.F.);
#66360=ORIENTED_EDGE('',*,*,#50228,.T.);
#66361=ORIENTED_EDGE('',*,*,#49079,.F.);
#66362=ORIENTED_EDGE('',*,*,#50229,.T.);
#66363=ORIENTED_EDGE('',*,*,#49061,.F.);
#66364=ORIENTED_EDGE('',*,*,#50230,.T.);
#66365=ORIENTED_EDGE('',*,*,#49063,.F.);
#66366=ORIENTED_EDGE('',*,*,#50231,.T.);
#66367=ORIENTED_EDGE('',*,*,#49067,.F.);
#66368=ORIENTED_EDGE('',*,*,#50232,.T.);
#66369=ORIENTED_EDGE('',*,*,#49107,.F.);
#66370=ORIENTED_EDGE('',*,*,#50233,.T.);
#66371=ORIENTED_EDGE('',*,*,#49089,.F.);
#66372=ORIENTED_EDGE('',*,*,#50234,.T.);
#66373=ORIENTED_EDGE('',*,*,#49091,.F.);
#66374=ORIENTED_EDGE('',*,*,#50235,.T.);
#66375=ORIENTED_EDGE('',*,*,#49095,.F.);
#66376=ORIENTED_EDGE('',*,*,#50236,.T.);
#66377=ORIENTED_EDGE('',*,*,#49135,.F.);
#66378=ORIENTED_EDGE('',*,*,#50237,.T.);
#66379=ORIENTED_EDGE('',*,*,#49117,.F.);
#66380=ORIENTED_EDGE('',*,*,#50238,.T.);
#66381=ORIENTED_EDGE('',*,*,#49119,.F.);
#66382=ORIENTED_EDGE('',*,*,#50239,.T.);
#66383=ORIENTED_EDGE('',*,*,#49123,.F.);
#66384=ORIENTED_EDGE('',*,*,#50240,.T.);
#66385=ORIENTED_EDGE('',*,*,#49163,.F.);
#66386=ORIENTED_EDGE('',*,*,#50241,.T.);
#66387=ORIENTED_EDGE('',*,*,#49145,.F.);
#66388=ORIENTED_EDGE('',*,*,#50242,.T.);
#66389=ORIENTED_EDGE('',*,*,#49147,.F.);
#66390=ORIENTED_EDGE('',*,*,#50243,.T.);
#66391=ORIENTED_EDGE('',*,*,#49151,.F.);
#66392=ORIENTED_EDGE('',*,*,#50244,.T.);
#66393=ORIENTED_EDGE('',*,*,#49191,.F.);
#66394=ORIENTED_EDGE('',*,*,#50245,.T.);
#66395=ORIENTED_EDGE('',*,*,#49173,.F.);
#66396=ORIENTED_EDGE('',*,*,#50246,.T.);
#66397=ORIENTED_EDGE('',*,*,#49175,.F.);
#66398=ORIENTED_EDGE('',*,*,#50247,.T.);
#66399=ORIENTED_EDGE('',*,*,#49179,.F.);
#66400=ORIENTED_EDGE('',*,*,#50248,.T.);
#66401=ORIENTED_EDGE('',*,*,#49219,.F.);
#66402=ORIENTED_EDGE('',*,*,#50249,.T.);
#66403=ORIENTED_EDGE('',*,*,#49201,.F.);
#66404=ORIENTED_EDGE('',*,*,#50250,.T.);
#66405=ORIENTED_EDGE('',*,*,#49203,.F.);
#66406=ORIENTED_EDGE('',*,*,#50251,.T.);
#66407=ORIENTED_EDGE('',*,*,#49207,.F.);
#66408=ORIENTED_EDGE('',*,*,#50252,.T.);
#66409=ORIENTED_EDGE('',*,*,#49247,.F.);
#66410=ORIENTED_EDGE('',*,*,#50253,.T.);
#66411=ORIENTED_EDGE('',*,*,#49229,.F.);
#66412=ORIENTED_EDGE('',*,*,#50254,.T.);
#66413=ORIENTED_EDGE('',*,*,#49231,.F.);
#66414=ORIENTED_EDGE('',*,*,#50255,.T.);
#66415=ORIENTED_EDGE('',*,*,#49235,.F.);
#66416=ORIENTED_EDGE('',*,*,#50256,.T.);
#66417=ORIENTED_EDGE('',*,*,#49275,.F.);
#66418=ORIENTED_EDGE('',*,*,#50257,.T.);
#66419=ORIENTED_EDGE('',*,*,#49257,.F.);
#66420=ORIENTED_EDGE('',*,*,#50258,.T.);
#66421=ORIENTED_EDGE('',*,*,#49259,.F.);
#66422=ORIENTED_EDGE('',*,*,#50259,.T.);
#66423=ORIENTED_EDGE('',*,*,#49263,.F.);
#66424=ORIENTED_EDGE('',*,*,#50260,.T.);
#66425=ORIENTED_EDGE('',*,*,#49303,.F.);
#66426=ORIENTED_EDGE('',*,*,#50261,.T.);
#66427=ORIENTED_EDGE('',*,*,#49285,.F.);
#66428=ORIENTED_EDGE('',*,*,#50262,.T.);
#66429=ORIENTED_EDGE('',*,*,#49287,.F.);
#66430=ORIENTED_EDGE('',*,*,#50263,.T.);
#66431=ORIENTED_EDGE('',*,*,#49291,.F.);
#66432=ORIENTED_EDGE('',*,*,#50264,.T.);
#66433=ORIENTED_EDGE('',*,*,#49329,.F.);
#66434=ORIENTED_EDGE('',*,*,#50265,.T.);
#66435=ORIENTED_EDGE('',*,*,#49313,.F.);
#66436=ORIENTED_EDGE('',*,*,#50266,.T.);
#66437=ORIENTED_EDGE('',*,*,#49314,.F.);
#66438=ORIENTED_EDGE('',*,*,#50267,.T.);
#66439=ORIENTED_EDGE('',*,*,#49317,.F.);
#66440=ORIENTED_EDGE('',*,*,#50268,.T.);
#66441=ORIENTED_EDGE('',*,*,#49357,.F.);
#66442=ORIENTED_EDGE('',*,*,#50269,.T.);
#66443=ORIENTED_EDGE('',*,*,#49339,.F.);
#66444=ORIENTED_EDGE('',*,*,#50270,.T.);
#66445=ORIENTED_EDGE('',*,*,#49341,.F.);
#66446=ORIENTED_EDGE('',*,*,#50271,.T.);
#66447=ORIENTED_EDGE('',*,*,#49345,.F.);
#66448=ORIENTED_EDGE('',*,*,#50272,.T.);
#66449=ORIENTED_EDGE('',*,*,#49385,.F.);
#66450=ORIENTED_EDGE('',*,*,#50273,.T.);
#66451=ORIENTED_EDGE('',*,*,#49367,.F.);
#66452=ORIENTED_EDGE('',*,*,#50274,.T.);
#66453=ORIENTED_EDGE('',*,*,#49369,.F.);
#66454=ORIENTED_EDGE('',*,*,#50275,.T.);
#66455=ORIENTED_EDGE('',*,*,#49373,.F.);
#66456=ORIENTED_EDGE('',*,*,#50276,.T.);
#66457=ORIENTED_EDGE('',*,*,#49413,.F.);
#66458=ORIENTED_EDGE('',*,*,#50277,.T.);
#66459=ORIENTED_EDGE('',*,*,#49395,.F.);
#66460=ORIENTED_EDGE('',*,*,#50278,.T.);
#66461=ORIENTED_EDGE('',*,*,#49397,.F.);
#66462=ORIENTED_EDGE('',*,*,#50279,.T.);
#66463=ORIENTED_EDGE('',*,*,#49401,.F.);
#66464=ORIENTED_EDGE('',*,*,#50280,.T.);
#66465=ORIENTED_EDGE('',*,*,#49441,.F.);
#66466=ORIENTED_EDGE('',*,*,#50281,.T.);
#66467=ORIENTED_EDGE('',*,*,#49423,.F.);
#66468=ORIENTED_EDGE('',*,*,#50282,.T.);
#66469=ORIENTED_EDGE('',*,*,#49425,.F.);
#66470=ORIENTED_EDGE('',*,*,#50283,.T.);
#66471=ORIENTED_EDGE('',*,*,#49429,.F.);
#66472=ORIENTED_EDGE('',*,*,#50284,.T.);
#66473=ORIENTED_EDGE('',*,*,#49469,.F.);
#66474=ORIENTED_EDGE('',*,*,#50285,.T.);
#66475=ORIENTED_EDGE('',*,*,#49451,.F.);
#66476=ORIENTED_EDGE('',*,*,#50286,.T.);
#66477=ORIENTED_EDGE('',*,*,#49453,.F.);
#66478=ORIENTED_EDGE('',*,*,#50287,.T.);
#66479=ORIENTED_EDGE('',*,*,#49457,.F.);
#66480=ORIENTED_EDGE('',*,*,#50288,.T.);
#66481=ORIENTED_EDGE('',*,*,#49497,.F.);
#66482=ORIENTED_EDGE('',*,*,#50289,.T.);
#66483=ORIENTED_EDGE('',*,*,#49479,.F.);
#66484=ORIENTED_EDGE('',*,*,#50290,.T.);
#66485=ORIENTED_EDGE('',*,*,#49481,.F.);
#66486=ORIENTED_EDGE('',*,*,#50291,.T.);
#66487=ORIENTED_EDGE('',*,*,#49485,.F.);
#66488=ORIENTED_EDGE('',*,*,#50292,.T.);
#66489=ORIENTED_EDGE('',*,*,#49525,.F.);
#66490=ORIENTED_EDGE('',*,*,#50293,.T.);
#66491=ORIENTED_EDGE('',*,*,#49507,.F.);
#66492=ORIENTED_EDGE('',*,*,#50294,.T.);
#66493=ORIENTED_EDGE('',*,*,#49509,.F.);
#66494=ORIENTED_EDGE('',*,*,#50295,.T.);
#66495=ORIENTED_EDGE('',*,*,#49513,.F.);
#66496=ORIENTED_EDGE('',*,*,#50296,.T.);
#66497=ORIENTED_EDGE('',*,*,#49553,.F.);
#66498=ORIENTED_EDGE('',*,*,#50297,.T.);
#66499=ORIENTED_EDGE('',*,*,#49535,.F.);
#66500=ORIENTED_EDGE('',*,*,#50298,.T.);
#66501=ORIENTED_EDGE('',*,*,#49537,.F.);
#66502=ORIENTED_EDGE('',*,*,#50299,.T.);
#66503=ORIENTED_EDGE('',*,*,#49541,.F.);
#66504=ORIENTED_EDGE('',*,*,#50300,.T.);
#66505=ORIENTED_EDGE('',*,*,#49581,.F.);
#66506=ORIENTED_EDGE('',*,*,#50301,.T.);
#66507=ORIENTED_EDGE('',*,*,#49563,.F.);
#66508=ORIENTED_EDGE('',*,*,#50302,.T.);
#66509=ORIENTED_EDGE('',*,*,#49565,.F.);
#66510=ORIENTED_EDGE('',*,*,#50303,.T.);
#66511=ORIENTED_EDGE('',*,*,#49569,.F.);
#66512=ORIENTED_EDGE('',*,*,#50304,.T.);
#66513=ORIENTED_EDGE('',*,*,#49609,.F.);
#66514=ORIENTED_EDGE('',*,*,#50305,.T.);
#66515=ORIENTED_EDGE('',*,*,#49591,.F.);
#66516=ORIENTED_EDGE('',*,*,#50306,.T.);
#66517=ORIENTED_EDGE('',*,*,#49593,.F.);
#66518=ORIENTED_EDGE('',*,*,#50307,.T.);
#66519=ORIENTED_EDGE('',*,*,#49597,.F.);
#66520=ORIENTED_EDGE('',*,*,#50308,.T.);
#66521=ORIENTED_EDGE('',*,*,#49637,.F.);
#66522=ORIENTED_EDGE('',*,*,#50309,.T.);
#66523=ORIENTED_EDGE('',*,*,#49619,.F.);
#66524=ORIENTED_EDGE('',*,*,#50310,.T.);
#66525=ORIENTED_EDGE('',*,*,#49621,.F.);
#66526=ORIENTED_EDGE('',*,*,#50311,.T.);
#66527=ORIENTED_EDGE('',*,*,#49625,.F.);
#66528=ORIENTED_EDGE('',*,*,#50312,.T.);
#66529=ORIENTED_EDGE('',*,*,#49665,.F.);
#66530=ORIENTED_EDGE('',*,*,#50313,.T.);
#66531=ORIENTED_EDGE('',*,*,#49647,.F.);
#66532=ORIENTED_EDGE('',*,*,#50314,.T.);
#66533=ORIENTED_EDGE('',*,*,#49649,.F.);
#66534=ORIENTED_EDGE('',*,*,#50315,.T.);
#66535=ORIENTED_EDGE('',*,*,#49653,.F.);
#66536=ORIENTED_EDGE('',*,*,#50316,.T.);
#66537=ORIENTED_EDGE('',*,*,#49693,.F.);
#66538=ORIENTED_EDGE('',*,*,#50317,.T.);
#66539=ORIENTED_EDGE('',*,*,#49675,.F.);
#66540=ORIENTED_EDGE('',*,*,#50318,.T.);
#66541=ORIENTED_EDGE('',*,*,#49677,.F.);
#66542=ORIENTED_EDGE('',*,*,#50319,.T.);
#66543=ORIENTED_EDGE('',*,*,#49681,.F.);
#66544=ORIENTED_EDGE('',*,*,#50320,.T.);
#66545=ORIENTED_EDGE('',*,*,#49721,.F.);
#66546=ORIENTED_EDGE('',*,*,#50321,.T.);
#66547=ORIENTED_EDGE('',*,*,#49703,.F.);
#66548=ORIENTED_EDGE('',*,*,#50322,.T.);
#66549=ORIENTED_EDGE('',*,*,#49705,.F.);
#66550=ORIENTED_EDGE('',*,*,#50323,.T.);
#66551=ORIENTED_EDGE('',*,*,#49709,.F.);
#66552=ORIENTED_EDGE('',*,*,#50324,.T.);
#66553=ORIENTED_EDGE('',*,*,#49747,.F.);
#66554=ORIENTED_EDGE('',*,*,#50325,.T.);
#66555=ORIENTED_EDGE('',*,*,#49731,.F.);
#66556=ORIENTED_EDGE('',*,*,#50326,.T.);
#66557=ORIENTED_EDGE('',*,*,#49732,.F.);
#66558=ORIENTED_EDGE('',*,*,#50327,.T.);
#66559=ORIENTED_EDGE('',*,*,#49735,.F.);
#66560=ORIENTED_EDGE('',*,*,#50328,.T.);
#66561=ORIENTED_EDGE('',*,*,#49775,.F.);
#66562=ORIENTED_EDGE('',*,*,#50329,.T.);
#66563=ORIENTED_EDGE('',*,*,#49757,.F.);
#66564=ORIENTED_EDGE('',*,*,#50330,.T.);
#66565=ORIENTED_EDGE('',*,*,#49759,.F.);
#66566=ORIENTED_EDGE('',*,*,#50331,.T.);
#66567=ORIENTED_EDGE('',*,*,#49763,.F.);
#66568=ORIENTED_EDGE('',*,*,#50332,.T.);
#66569=ORIENTED_EDGE('',*,*,#49803,.F.);
#66570=ORIENTED_EDGE('',*,*,#50333,.T.);
#66571=ORIENTED_EDGE('',*,*,#49785,.F.);
#66572=ORIENTED_EDGE('',*,*,#50334,.T.);
#66573=ORIENTED_EDGE('',*,*,#49787,.F.);
#66574=ORIENTED_EDGE('',*,*,#50335,.T.);
#66575=ORIENTED_EDGE('',*,*,#49791,.F.);
#66576=ORIENTED_EDGE('',*,*,#50336,.T.);
#66577=ORIENTED_EDGE('',*,*,#49831,.F.);
#66578=ORIENTED_EDGE('',*,*,#50337,.T.);
#66579=ORIENTED_EDGE('',*,*,#49813,.F.);
#66580=ORIENTED_EDGE('',*,*,#50338,.T.);
#66581=ORIENTED_EDGE('',*,*,#49815,.F.);
#66582=ORIENTED_EDGE('',*,*,#50339,.T.);
#66583=ORIENTED_EDGE('',*,*,#49819,.F.);
#66584=ORIENTED_EDGE('',*,*,#50340,.T.);
#66585=ORIENTED_EDGE('',*,*,#49859,.F.);
#66586=ORIENTED_EDGE('',*,*,#50341,.T.);
#66587=ORIENTED_EDGE('',*,*,#49841,.F.);
#66588=ORIENTED_EDGE('',*,*,#50342,.T.);
#66589=ORIENTED_EDGE('',*,*,#49843,.F.);
#66590=ORIENTED_EDGE('',*,*,#50343,.T.);
#66591=ORIENTED_EDGE('',*,*,#49847,.F.);
#66592=ORIENTED_EDGE('',*,*,#50344,.T.);
#66593=ORIENTED_EDGE('',*,*,#49887,.F.);
#66594=ORIENTED_EDGE('',*,*,#50345,.T.);
#66595=ORIENTED_EDGE('',*,*,#49869,.F.);
#66596=ORIENTED_EDGE('',*,*,#50346,.T.);
#66597=ORIENTED_EDGE('',*,*,#49871,.F.);
#66598=ORIENTED_EDGE('',*,*,#50347,.T.);
#66599=ORIENTED_EDGE('',*,*,#49875,.F.);
#66600=ORIENTED_EDGE('',*,*,#50348,.T.);
#66601=ORIENTED_EDGE('',*,*,#49915,.F.);
#66602=ORIENTED_EDGE('',*,*,#50349,.T.);
#66603=ORIENTED_EDGE('',*,*,#49897,.F.);
#66604=ORIENTED_EDGE('',*,*,#50350,.T.);
#66605=ORIENTED_EDGE('',*,*,#49899,.F.);
#66606=ORIENTED_EDGE('',*,*,#50351,.T.);
#66607=ORIENTED_EDGE('',*,*,#49903,.F.);
#66608=ORIENTED_EDGE('',*,*,#50352,.T.);
#66609=ORIENTED_EDGE('',*,*,#49943,.F.);
#66610=ORIENTED_EDGE('',*,*,#50353,.T.);
#66611=ORIENTED_EDGE('',*,*,#49925,.F.);
#66612=ORIENTED_EDGE('',*,*,#50354,.T.);
#66613=ORIENTED_EDGE('',*,*,#49927,.F.);
#66614=ORIENTED_EDGE('',*,*,#50355,.T.);
#66615=ORIENTED_EDGE('',*,*,#49931,.F.);
#66616=ORIENTED_EDGE('',*,*,#50356,.T.);
#66617=ORIENTED_EDGE('',*,*,#49971,.F.);
#66618=ORIENTED_EDGE('',*,*,#50357,.T.);
#66619=ORIENTED_EDGE('',*,*,#49953,.F.);
#66620=ORIENTED_EDGE('',*,*,#50358,.T.);
#66621=ORIENTED_EDGE('',*,*,#49955,.F.);
#66622=ORIENTED_EDGE('',*,*,#50359,.T.);
#66623=ORIENTED_EDGE('',*,*,#49959,.F.);
#66624=ORIENTED_EDGE('',*,*,#50360,.T.);
#66625=ORIENTED_EDGE('',*,*,#49999,.F.);
#66626=ORIENTED_EDGE('',*,*,#50361,.T.);
#66627=ORIENTED_EDGE('',*,*,#49981,.F.);
#66628=ORIENTED_EDGE('',*,*,#50362,.T.);
#66629=ORIENTED_EDGE('',*,*,#49983,.F.);
#66630=ORIENTED_EDGE('',*,*,#50363,.T.);
#66631=ORIENTED_EDGE('',*,*,#49987,.F.);
#66632=ORIENTED_EDGE('',*,*,#50364,.T.);
#66633=ORIENTED_EDGE('',*,*,#50027,.F.);
#66634=ORIENTED_EDGE('',*,*,#50365,.T.);
#66635=ORIENTED_EDGE('',*,*,#50009,.F.);
#66636=ORIENTED_EDGE('',*,*,#50366,.T.);
#66637=ORIENTED_EDGE('',*,*,#50011,.F.);
#66638=ORIENTED_EDGE('',*,*,#50367,.T.);
#66639=ORIENTED_EDGE('',*,*,#50015,.F.);
#66640=ORIENTED_EDGE('',*,*,#50368,.T.);
#66641=ORIENTED_EDGE('',*,*,#50055,.F.);
#66642=ORIENTED_EDGE('',*,*,#50369,.T.);
#66643=ORIENTED_EDGE('',*,*,#50037,.F.);
#66644=ORIENTED_EDGE('',*,*,#50370,.T.);
#66645=ORIENTED_EDGE('',*,*,#50039,.F.);
#66646=ORIENTED_EDGE('',*,*,#50371,.T.);
#66647=ORIENTED_EDGE('',*,*,#50043,.F.);
#66648=ORIENTED_EDGE('',*,*,#50372,.T.);
#66649=ORIENTED_EDGE('',*,*,#50083,.F.);
#66650=ORIENTED_EDGE('',*,*,#50373,.T.);
#66651=ORIENTED_EDGE('',*,*,#50065,.F.);
#66652=ORIENTED_EDGE('',*,*,#50374,.T.);
#66653=ORIENTED_EDGE('',*,*,#50067,.F.);
#66654=ORIENTED_EDGE('',*,*,#50375,.T.);
#66655=ORIENTED_EDGE('',*,*,#50071,.F.);
#66656=ORIENTED_EDGE('',*,*,#50376,.T.);
#66657=ORIENTED_EDGE('',*,*,#50111,.F.);
#66658=ORIENTED_EDGE('',*,*,#50377,.T.);
#66659=ORIENTED_EDGE('',*,*,#50093,.F.);
#66660=ORIENTED_EDGE('',*,*,#50378,.T.);
#66661=ORIENTED_EDGE('',*,*,#50095,.F.);
#66662=ORIENTED_EDGE('',*,*,#50379,.T.);
#66663=ORIENTED_EDGE('',*,*,#50099,.F.);
#66664=ORIENTED_EDGE('',*,*,#50380,.T.);
#66665=ORIENTED_EDGE('',*,*,#50139,.F.);
#66666=ORIENTED_EDGE('',*,*,#50381,.T.);
#66667=ORIENTED_EDGE('',*,*,#50121,.F.);
#66668=ORIENTED_EDGE('',*,*,#50382,.T.);
#66669=ORIENTED_EDGE('',*,*,#50123,.F.);
#66670=ORIENTED_EDGE('',*,*,#50383,.T.);
#66671=ORIENTED_EDGE('',*,*,#50127,.F.);
#66672=ORIENTED_EDGE('',*,*,#50384,.T.);
#66673=ORIENTED_EDGE('',*,*,#50385,.F.);
#66674=ORIENTED_EDGE('',*,*,#48527,.F.);
#66675=ORIENTED_EDGE('',*,*,#50386,.F.);
#66676=ORIENTED_EDGE('',*,*,#48399,.F.);
#66677=ORIENTED_EDGE('',*,*,#50386,.T.);
#66678=ORIENTED_EDGE('',*,*,#48526,.F.);
#66679=ORIENTED_EDGE('',*,*,#50387,.F.);
#66680=ORIENTED_EDGE('',*,*,#48408,.F.);
#66681=ORIENTED_EDGE('',*,*,#48398,.T.);
#66682=ORIENTED_EDGE('',*,*,#48402,.F.);
#66683=ORIENTED_EDGE('',*,*,#50388,.F.);
#66684=ORIENTED_EDGE('',*,*,#48528,.F.);
#66685=ORIENTED_EDGE('',*,*,#50385,.T.);
#66686=ORIENTED_EDGE('',*,*,#50387,.T.);
#66687=ORIENTED_EDGE('',*,*,#48525,.F.);
#66688=ORIENTED_EDGE('',*,*,#50389,.F.);
#66689=ORIENTED_EDGE('',*,*,#48393,.F.);
#66690=ORIENTED_EDGE('',*,*,#50388,.T.);
#66691=ORIENTED_EDGE('',*,*,#48406,.F.);
#66692=ORIENTED_EDGE('',*,*,#50390,.F.);
#66693=ORIENTED_EDGE('',*,*,#48517,.F.);
#66694=ORIENTED_EDGE('',*,*,#50389,.T.);
#66695=ORIENTED_EDGE('',*,*,#48524,.F.);
#66696=ORIENTED_EDGE('',*,*,#50391,.F.);
#66697=ORIENTED_EDGE('',*,*,#48410,.F.);
#66698=ORIENTED_EDGE('',*,*,#50390,.T.);
#66699=ORIENTED_EDGE('',*,*,#45925,.F.);
#66700=ORIENTED_EDGE('',*,*,#50392,.F.);
#66701=ORIENTED_EDGE('',*,*,#48518,.F.);
#66702=ORIENTED_EDGE('',*,*,#50391,.T.);
#66703=ORIENTED_EDGE('',*,*,#48523,.F.);
#66704=ORIENTED_EDGE('',*,*,#50393,.F.);
#66705=ORIENTED_EDGE('',*,*,#48385,.T.);
#66706=ORIENTED_EDGE('',*,*,#48389,.F.);
#66707=ORIENTED_EDGE('',*,*,#50392,.T.);
#66708=ORIENTED_EDGE('',*,*,#45924,.F.);
#66709=ORIENTED_EDGE('',*,*,#50394,.F.);
#66710=ORIENTED_EDGE('',*,*,#50149,.F.);
#66711=ORIENTED_EDGE('',*,*,#50393,.T.);
#66712=ORIENTED_EDGE('',*,*,#48522,.F.);
#66713=ORIENTED_EDGE('',*,*,#50395,.F.);
#66714=ORIENTED_EDGE('',*,*,#48386,.F.);
#66715=ORIENTED_EDGE('',*,*,#50394,.T.);
#66716=ORIENTED_EDGE('',*,*,#45923,.F.);
#66717=ORIENTED_EDGE('',*,*,#50396,.F.);
#66718=ORIENTED_EDGE('',*,*,#48502,.F.);
#66719=ORIENTED_EDGE('',*,*,#50395,.T.);
#66720=ORIENTED_EDGE('',*,*,#48521,.F.);
#66721=ORIENTED_EDGE('',*,*,#50397,.F.);
#66722=ORIENTED_EDGE('',*,*,#48404,.F.);
#66723=ORIENTED_EDGE('',*,*,#50396,.T.);
#66724=ORIENTED_EDGE('',*,*,#45922,.F.);
#66725=ORIENTED_EDGE('',*,*,#50398,.F.);
#66726=ORIENTED_EDGE('',*,*,#50151,.F.);
#66727=ORIENTED_EDGE('',*,*,#50397,.T.);
#66728=ORIENTED_EDGE('',*,*,#48520,.F.);
#66729=ORIENTED_EDGE('',*,*,#50399,.F.);
#66730=ORIENTED_EDGE('',*,*,#46447,.F.);
#66731=ORIENTED_EDGE('',*,*,#50398,.T.);
#66732=ORIENTED_EDGE('',*,*,#45921,.F.);
#66733=ORIENTED_EDGE('',*,*,#50400,.F.);
#66734=ORIENTED_EDGE('',*,*,#48508,.F.);
#66735=ORIENTED_EDGE('',*,*,#50399,.T.);
#66736=ORIENTED_EDGE('',*,*,#50150,.F.);
#66737=ORIENTED_EDGE('',*,*,#50401,.F.);
#66738=ORIENTED_EDGE('',*,*,#46448,.F.);
#66739=ORIENTED_EDGE('',*,*,#50400,.T.);
#66740=ORIENTED_EDGE('',*,*,#48435,.F.);
#66741=ORIENTED_EDGE('',*,*,#50402,.F.);
#66742=ORIENTED_EDGE('',*,*,#48509,.F.);
#66743=ORIENTED_EDGE('',*,*,#50401,.T.);
#66744=ORIENTED_EDGE('',*,*,#48504,.F.);
#66745=ORIENTED_EDGE('',*,*,#50403,.F.);
#66746=ORIENTED_EDGE('',*,*,#46449,.F.);
#66747=ORIENTED_EDGE('',*,*,#48430,.F.);
#66748=ORIENTED_EDGE('',*,*,#48426,.T.);
#66749=ORIENTED_EDGE('',*,*,#50404,.F.);
#66750=ORIENTED_EDGE('',*,*,#48510,.F.);
#66751=ORIENTED_EDGE('',*,*,#50402,.T.);
#66752=ORIENTED_EDGE('',*,*,#50403,.T.);
#66753=ORIENTED_EDGE('',*,*,#50152,.F.);
#66754=ORIENTED_EDGE('',*,*,#50405,.F.);
#66755=ORIENTED_EDGE('',*,*,#46450,.F.);
#66756=ORIENTED_EDGE('',*,*,#50404,.T.);
#66757=ORIENTED_EDGE('',*,*,#48425,.F.);
#66758=ORIENTED_EDGE('',*,*,#50406,.F.);
#66759=ORIENTED_EDGE('',*,*,#48511,.F.);
#66760=ORIENTED_EDGE('',*,*,#50405,.T.);
#66761=ORIENTED_EDGE('',*,*,#48506,.F.);
#66762=ORIENTED_EDGE('',*,*,#50407,.F.);
#66763=ORIENTED_EDGE('',*,*,#46451,.F.);
#66764=ORIENTED_EDGE('',*,*,#50406,.T.);
#66765=ORIENTED_EDGE('',*,*,#48437,.F.);
#66766=ORIENTED_EDGE('',*,*,#50408,.F.);
#66767=ORIENTED_EDGE('',*,*,#48512,.F.);
#66768=ORIENTED_EDGE('',*,*,#50407,.T.);
#66769=ORIENTED_EDGE('',*,*,#48505,.F.);
#66770=ORIENTED_EDGE('',*,*,#50409,.F.);
#66771=ORIENTED_EDGE('',*,*,#48433,.F.);
#66772=ORIENTED_EDGE('',*,*,#50408,.T.);
#66773=ORIENTED_EDGE('',*,*,#48421,.F.);
#66774=ORIENTED_EDGE('',*,*,#50410,.F.);
#66775=ORIENTED_EDGE('',*,*,#48513,.F.);
#66776=ORIENTED_EDGE('',*,*,#50409,.T.);
#66777=ORIENTED_EDGE('',*,*,#48516,.F.);
#66778=ORIENTED_EDGE('',*,*,#50411,.F.);
#66779=ORIENTED_EDGE('',*,*,#48412,.F.);
#66780=ORIENTED_EDGE('',*,*,#50410,.T.);
#66781=ORIENTED_EDGE('',*,*,#48439,.F.);
#66782=ORIENTED_EDGE('',*,*,#50412,.F.);
#66783=ORIENTED_EDGE('',*,*,#48514,.F.);
#66784=ORIENTED_EDGE('',*,*,#50411,.T.);
#66785=ORIENTED_EDGE('',*,*,#48515,.F.);
#66786=ORIENTED_EDGE('',*,*,#50412,.T.);
#66787=ORIENTED_EDGE('',*,*,#48417,.F.);
#66788=ORIENTED_EDGE('',*,*,#48413,.T.);
#66789=ORIENTED_EDGE('',*,*,#50413,.F.);
#66790=ORIENTED_EDGE('',*,*,#48555,.F.);
#66791=ORIENTED_EDGE('',*,*,#50414,.F.);
#66792=ORIENTED_EDGE('',*,*,#48369,.F.);
#66793=ORIENTED_EDGE('',*,*,#50414,.T.);
#66794=ORIENTED_EDGE('',*,*,#48554,.F.);
#66795=ORIENTED_EDGE('',*,*,#50415,.F.);
#66796=ORIENTED_EDGE('',*,*,#48378,.F.);
#66797=ORIENTED_EDGE('',*,*,#48368,.T.);
#66798=ORIENTED_EDGE('',*,*,#48372,.F.);
#66799=ORIENTED_EDGE('',*,*,#50416,.F.);
#66800=ORIENTED_EDGE('',*,*,#48556,.F.);
#66801=ORIENTED_EDGE('',*,*,#50413,.T.);
#66802=ORIENTED_EDGE('',*,*,#50415,.T.);
#66803=ORIENTED_EDGE('',*,*,#48553,.F.);
#66804=ORIENTED_EDGE('',*,*,#50417,.F.);
#66805=ORIENTED_EDGE('',*,*,#48363,.F.);
#66806=ORIENTED_EDGE('',*,*,#50416,.T.);
#66807=ORIENTED_EDGE('',*,*,#48376,.F.);
#66808=ORIENTED_EDGE('',*,*,#50418,.F.);
#66809=ORIENTED_EDGE('',*,*,#48545,.F.);
#66810=ORIENTED_EDGE('',*,*,#50417,.T.);
#66811=ORIENTED_EDGE('',*,*,#48552,.F.);
#66812=ORIENTED_EDGE('',*,*,#50419,.F.);
#66813=ORIENTED_EDGE('',*,*,#48380,.F.);
#66814=ORIENTED_EDGE('',*,*,#50418,.T.);
#66815=ORIENTED_EDGE('',*,*,#45931,.F.);
#66816=ORIENTED_EDGE('',*,*,#50420,.F.);
#66817=ORIENTED_EDGE('',*,*,#48546,.F.);
#66818=ORIENTED_EDGE('',*,*,#50419,.T.);
#66819=ORIENTED_EDGE('',*,*,#48551,.F.);
#66820=ORIENTED_EDGE('',*,*,#50421,.F.);
#66821=ORIENTED_EDGE('',*,*,#48355,.T.);
#66822=ORIENTED_EDGE('',*,*,#48359,.F.);
#66823=ORIENTED_EDGE('',*,*,#50420,.T.);
#66824=ORIENTED_EDGE('',*,*,#45930,.F.);
#66825=ORIENTED_EDGE('',*,*,#50422,.F.);
#66826=ORIENTED_EDGE('',*,*,#50153,.F.);
#66827=ORIENTED_EDGE('',*,*,#50421,.T.);
#66828=ORIENTED_EDGE('',*,*,#48550,.F.);
#66829=ORIENTED_EDGE('',*,*,#50423,.F.);
#66830=ORIENTED_EDGE('',*,*,#48356,.F.);
#66831=ORIENTED_EDGE('',*,*,#50422,.T.);
#66832=ORIENTED_EDGE('',*,*,#45929,.F.);
#66833=ORIENTED_EDGE('',*,*,#50424,.F.);
#66834=ORIENTED_EDGE('',*,*,#48530,.F.);
#66835=ORIENTED_EDGE('',*,*,#50423,.T.);
#66836=ORIENTED_EDGE('',*,*,#48549,.F.);
#66837=ORIENTED_EDGE('',*,*,#50425,.F.);
#66838=ORIENTED_EDGE('',*,*,#48374,.F.);
#66839=ORIENTED_EDGE('',*,*,#50424,.T.);
#66840=ORIENTED_EDGE('',*,*,#45928,.F.);
#66841=ORIENTED_EDGE('',*,*,#50426,.F.);
#66842=ORIENTED_EDGE('',*,*,#50155,.F.);
#66843=ORIENTED_EDGE('',*,*,#50425,.T.);
#66844=ORIENTED_EDGE('',*,*,#48548,.F.);
#66845=ORIENTED_EDGE('',*,*,#50427,.F.);
#66846=ORIENTED_EDGE('',*,*,#46441,.F.);
#66847=ORIENTED_EDGE('',*,*,#50426,.T.);
#66848=ORIENTED_EDGE('',*,*,#45927,.F.);
#66849=ORIENTED_EDGE('',*,*,#50428,.F.);
#66850=ORIENTED_EDGE('',*,*,#48536,.F.);
#66851=ORIENTED_EDGE('',*,*,#50427,.T.);
#66852=ORIENTED_EDGE('',*,*,#50154,.F.);
#66853=ORIENTED_EDGE('',*,*,#50429,.F.);
#66854=ORIENTED_EDGE('',*,*,#46442,.F.);
#66855=ORIENTED_EDGE('',*,*,#50428,.T.);
#66856=ORIENTED_EDGE('',*,*,#48405,.F.);
#66857=ORIENTED_EDGE('',*,*,#50430,.F.);
#66858=ORIENTED_EDGE('',*,*,#48537,.F.);
#66859=ORIENTED_EDGE('',*,*,#50429,.T.);
#66860=ORIENTED_EDGE('',*,*,#48532,.F.);
#66861=ORIENTED_EDGE('',*,*,#50431,.F.);
#66862=ORIENTED_EDGE('',*,*,#46443,.F.);
#66863=ORIENTED_EDGE('',*,*,#48400,.F.);
#66864=ORIENTED_EDGE('',*,*,#48396,.T.);
#66865=ORIENTED_EDGE('',*,*,#50432,.F.);
#66866=ORIENTED_EDGE('',*,*,#48538,.F.);
#66867=ORIENTED_EDGE('',*,*,#50430,.T.);
#66868=ORIENTED_EDGE('',*,*,#50431,.T.);
#66869=ORIENTED_EDGE('',*,*,#50156,.F.);
#66870=ORIENTED_EDGE('',*,*,#50433,.F.);
#66871=ORIENTED_EDGE('',*,*,#46444,.F.);
#66872=ORIENTED_EDGE('',*,*,#50432,.T.);
#66873=ORIENTED_EDGE('',*,*,#48395,.F.);
#66874=ORIENTED_EDGE('',*,*,#50434,.F.);
#66875=ORIENTED_EDGE('',*,*,#48539,.F.);
#66876=ORIENTED_EDGE('',*,*,#50433,.T.);
#66877=ORIENTED_EDGE('',*,*,#48534,.F.);
#66878=ORIENTED_EDGE('',*,*,#50435,.F.);
#66879=ORIENTED_EDGE('',*,*,#46445,.F.);
#66880=ORIENTED_EDGE('',*,*,#50434,.T.);
#66881=ORIENTED_EDGE('',*,*,#48407,.F.);
#66882=ORIENTED_EDGE('',*,*,#50436,.F.);
#66883=ORIENTED_EDGE('',*,*,#48540,.F.);
#66884=ORIENTED_EDGE('',*,*,#50435,.T.);
#66885=ORIENTED_EDGE('',*,*,#48533,.F.);
#66886=ORIENTED_EDGE('',*,*,#50437,.F.);
#66887=ORIENTED_EDGE('',*,*,#48403,.F.);
#66888=ORIENTED_EDGE('',*,*,#50436,.T.);
#66889=ORIENTED_EDGE('',*,*,#48391,.F.);
#66890=ORIENTED_EDGE('',*,*,#50438,.F.);
#66891=ORIENTED_EDGE('',*,*,#48541,.F.);
#66892=ORIENTED_EDGE('',*,*,#50437,.T.);
#66893=ORIENTED_EDGE('',*,*,#48544,.F.);
#66894=ORIENTED_EDGE('',*,*,#50439,.F.);
#66895=ORIENTED_EDGE('',*,*,#48382,.F.);
#66896=ORIENTED_EDGE('',*,*,#50438,.T.);
#66897=ORIENTED_EDGE('',*,*,#48409,.F.);
#66898=ORIENTED_EDGE('',*,*,#50440,.F.);
#66899=ORIENTED_EDGE('',*,*,#48542,.F.);
#66900=ORIENTED_EDGE('',*,*,#50439,.T.);
#66901=ORIENTED_EDGE('',*,*,#48543,.F.);
#66902=ORIENTED_EDGE('',*,*,#50440,.T.);
#66903=ORIENTED_EDGE('',*,*,#48387,.F.);
#66904=ORIENTED_EDGE('',*,*,#48383,.T.);
#66905=ORIENTED_EDGE('',*,*,#50441,.F.);
#66906=ORIENTED_EDGE('',*,*,#48583,.F.);
#66907=ORIENTED_EDGE('',*,*,#50442,.F.);
#66908=ORIENTED_EDGE('',*,*,#48339,.F.);
#66909=ORIENTED_EDGE('',*,*,#50442,.T.);
#66910=ORIENTED_EDGE('',*,*,#48582,.F.);
#66911=ORIENTED_EDGE('',*,*,#50443,.F.);
#66912=ORIENTED_EDGE('',*,*,#48348,.F.);
#66913=ORIENTED_EDGE('',*,*,#48338,.T.);
#66914=ORIENTED_EDGE('',*,*,#48342,.F.);
#66915=ORIENTED_EDGE('',*,*,#50444,.F.);
#66916=ORIENTED_EDGE('',*,*,#48584,.F.);
#66917=ORIENTED_EDGE('',*,*,#50441,.T.);
#66918=ORIENTED_EDGE('',*,*,#50443,.T.);
#66919=ORIENTED_EDGE('',*,*,#48581,.F.);
#66920=ORIENTED_EDGE('',*,*,#50445,.F.);
#66921=ORIENTED_EDGE('',*,*,#48333,.F.);
#66922=ORIENTED_EDGE('',*,*,#50444,.T.);
#66923=ORIENTED_EDGE('',*,*,#48346,.F.);
#66924=ORIENTED_EDGE('',*,*,#50446,.F.);
#66925=ORIENTED_EDGE('',*,*,#48573,.F.);
#66926=ORIENTED_EDGE('',*,*,#50445,.T.);
#66927=ORIENTED_EDGE('',*,*,#48580,.F.);
#66928=ORIENTED_EDGE('',*,*,#50447,.F.);
#66929=ORIENTED_EDGE('',*,*,#48350,.F.);
#66930=ORIENTED_EDGE('',*,*,#50446,.T.);
#66931=ORIENTED_EDGE('',*,*,#45937,.F.);
#66932=ORIENTED_EDGE('',*,*,#50448,.F.);
#66933=ORIENTED_EDGE('',*,*,#48574,.F.);
#66934=ORIENTED_EDGE('',*,*,#50447,.T.);
#66935=ORIENTED_EDGE('',*,*,#48579,.F.);
#66936=ORIENTED_EDGE('',*,*,#50449,.F.);
#66937=ORIENTED_EDGE('',*,*,#48325,.T.);
#66938=ORIENTED_EDGE('',*,*,#48329,.F.);
#66939=ORIENTED_EDGE('',*,*,#50448,.T.);
#66940=ORIENTED_EDGE('',*,*,#45936,.F.);
#66941=ORIENTED_EDGE('',*,*,#50450,.F.);
#66942=ORIENTED_EDGE('',*,*,#50157,.F.);
#66943=ORIENTED_EDGE('',*,*,#50449,.T.);
#66944=ORIENTED_EDGE('',*,*,#48578,.F.);
#66945=ORIENTED_EDGE('',*,*,#50451,.F.);
#66946=ORIENTED_EDGE('',*,*,#48326,.F.);
#66947=ORIENTED_EDGE('',*,*,#50450,.T.);
#66948=ORIENTED_EDGE('',*,*,#45935,.F.);
#66949=ORIENTED_EDGE('',*,*,#50452,.F.);
#66950=ORIENTED_EDGE('',*,*,#48558,.F.);
#66951=ORIENTED_EDGE('',*,*,#50451,.T.);
#66952=ORIENTED_EDGE('',*,*,#48577,.F.);
#66953=ORIENTED_EDGE('',*,*,#50453,.F.);
#66954=ORIENTED_EDGE('',*,*,#48344,.F.);
#66955=ORIENTED_EDGE('',*,*,#50452,.T.);
#66956=ORIENTED_EDGE('',*,*,#45934,.F.);
#66957=ORIENTED_EDGE('',*,*,#50454,.F.);
#66958=ORIENTED_EDGE('',*,*,#50159,.F.);
#66959=ORIENTED_EDGE('',*,*,#50453,.T.);
#66960=ORIENTED_EDGE('',*,*,#48576,.F.);
#66961=ORIENTED_EDGE('',*,*,#50455,.F.);
#66962=ORIENTED_EDGE('',*,*,#46435,.F.);
#66963=ORIENTED_EDGE('',*,*,#50454,.T.);
#66964=ORIENTED_EDGE('',*,*,#45933,.F.);
#66965=ORIENTED_EDGE('',*,*,#50456,.F.);
#66966=ORIENTED_EDGE('',*,*,#48564,.F.);
#66967=ORIENTED_EDGE('',*,*,#50455,.T.);
#66968=ORIENTED_EDGE('',*,*,#50158,.F.);
#66969=ORIENTED_EDGE('',*,*,#50457,.F.);
#66970=ORIENTED_EDGE('',*,*,#46436,.F.);
#66971=ORIENTED_EDGE('',*,*,#50456,.T.);
#66972=ORIENTED_EDGE('',*,*,#48375,.F.);
#66973=ORIENTED_EDGE('',*,*,#50458,.F.);
#66974=ORIENTED_EDGE('',*,*,#48565,.F.);
#66975=ORIENTED_EDGE('',*,*,#50457,.T.);
#66976=ORIENTED_EDGE('',*,*,#48560,.F.);
#66977=ORIENTED_EDGE('',*,*,#50459,.F.);
#66978=ORIENTED_EDGE('',*,*,#46437,.F.);
#66979=ORIENTED_EDGE('',*,*,#48370,.F.);
#66980=ORIENTED_EDGE('',*,*,#48366,.T.);
#66981=ORIENTED_EDGE('',*,*,#50460,.F.);
#66982=ORIENTED_EDGE('',*,*,#48566,.F.);
#66983=ORIENTED_EDGE('',*,*,#50458,.T.);
#66984=ORIENTED_EDGE('',*,*,#50459,.T.);
#66985=ORIENTED_EDGE('',*,*,#50160,.F.);
#66986=ORIENTED_EDGE('',*,*,#50461,.F.);
#66987=ORIENTED_EDGE('',*,*,#46438,.F.);
#66988=ORIENTED_EDGE('',*,*,#50460,.T.);
#66989=ORIENTED_EDGE('',*,*,#48365,.F.);
#66990=ORIENTED_EDGE('',*,*,#50462,.F.);
#66991=ORIENTED_EDGE('',*,*,#48567,.F.);
#66992=ORIENTED_EDGE('',*,*,#50461,.T.);
#66993=ORIENTED_EDGE('',*,*,#48562,.F.);
#66994=ORIENTED_EDGE('',*,*,#50463,.F.);
#66995=ORIENTED_EDGE('',*,*,#46439,.F.);
#66996=ORIENTED_EDGE('',*,*,#50462,.T.);
#66997=ORIENTED_EDGE('',*,*,#48377,.F.);
#66998=ORIENTED_EDGE('',*,*,#50464,.F.);
#66999=ORIENTED_EDGE('',*,*,#48568,.F.);
#67000=ORIENTED_EDGE('',*,*,#50463,.T.);
#67001=ORIENTED_EDGE('',*,*,#48561,.F.);
#67002=ORIENTED_EDGE('',*,*,#50465,.F.);
#67003=ORIENTED_EDGE('',*,*,#48373,.F.);
#67004=ORIENTED_EDGE('',*,*,#50464,.T.);
#67005=ORIENTED_EDGE('',*,*,#48361,.F.);
#67006=ORIENTED_EDGE('',*,*,#50466,.F.);
#67007=ORIENTED_EDGE('',*,*,#48569,.F.);
#67008=ORIENTED_EDGE('',*,*,#50465,.T.);
#67009=ORIENTED_EDGE('',*,*,#48572,.F.);
#67010=ORIENTED_EDGE('',*,*,#50467,.F.);
#67011=ORIENTED_EDGE('',*,*,#48352,.F.);
#67012=ORIENTED_EDGE('',*,*,#50466,.T.);
#67013=ORIENTED_EDGE('',*,*,#48379,.F.);
#67014=ORIENTED_EDGE('',*,*,#50468,.F.);
#67015=ORIENTED_EDGE('',*,*,#48570,.F.);
#67016=ORIENTED_EDGE('',*,*,#50467,.T.);
#67017=ORIENTED_EDGE('',*,*,#48571,.F.);
#67018=ORIENTED_EDGE('',*,*,#50468,.T.);
#67019=ORIENTED_EDGE('',*,*,#48357,.F.);
#67020=ORIENTED_EDGE('',*,*,#48353,.T.);
#67021=ORIENTED_EDGE('',*,*,#50469,.F.);
#67022=ORIENTED_EDGE('',*,*,#48611,.F.);
#67023=ORIENTED_EDGE('',*,*,#50470,.F.);
#67024=ORIENTED_EDGE('',*,*,#48309,.F.);
#67025=ORIENTED_EDGE('',*,*,#50470,.T.);
#67026=ORIENTED_EDGE('',*,*,#48610,.F.);
#67027=ORIENTED_EDGE('',*,*,#50471,.F.);
#67028=ORIENTED_EDGE('',*,*,#48318,.F.);
#67029=ORIENTED_EDGE('',*,*,#48308,.T.);
#67030=ORIENTED_EDGE('',*,*,#48312,.F.);
#67031=ORIENTED_EDGE('',*,*,#50472,.F.);
#67032=ORIENTED_EDGE('',*,*,#48612,.F.);
#67033=ORIENTED_EDGE('',*,*,#50469,.T.);
#67034=ORIENTED_EDGE('',*,*,#50471,.T.);
#67035=ORIENTED_EDGE('',*,*,#48609,.F.);
#67036=ORIENTED_EDGE('',*,*,#50473,.F.);
#67037=ORIENTED_EDGE('',*,*,#48303,.F.);
#67038=ORIENTED_EDGE('',*,*,#50472,.T.);
#67039=ORIENTED_EDGE('',*,*,#48316,.F.);
#67040=ORIENTED_EDGE('',*,*,#50474,.F.);
#67041=ORIENTED_EDGE('',*,*,#48601,.F.);
#67042=ORIENTED_EDGE('',*,*,#50473,.T.);
#67043=ORIENTED_EDGE('',*,*,#48608,.F.);
#67044=ORIENTED_EDGE('',*,*,#50475,.F.);
#67045=ORIENTED_EDGE('',*,*,#48320,.F.);
#67046=ORIENTED_EDGE('',*,*,#50474,.T.);
#67047=ORIENTED_EDGE('',*,*,#45943,.F.);
#67048=ORIENTED_EDGE('',*,*,#50476,.F.);
#67049=ORIENTED_EDGE('',*,*,#48602,.F.);
#67050=ORIENTED_EDGE('',*,*,#50475,.T.);
#67051=ORIENTED_EDGE('',*,*,#48607,.F.);
#67052=ORIENTED_EDGE('',*,*,#50477,.F.);
#67053=ORIENTED_EDGE('',*,*,#48295,.T.);
#67054=ORIENTED_EDGE('',*,*,#48299,.F.);
#67055=ORIENTED_EDGE('',*,*,#50476,.T.);
#67056=ORIENTED_EDGE('',*,*,#45942,.F.);
#67057=ORIENTED_EDGE('',*,*,#50478,.F.);
#67058=ORIENTED_EDGE('',*,*,#50161,.F.);
#67059=ORIENTED_EDGE('',*,*,#50477,.T.);
#67060=ORIENTED_EDGE('',*,*,#48606,.F.);
#67061=ORIENTED_EDGE('',*,*,#50479,.F.);
#67062=ORIENTED_EDGE('',*,*,#48296,.F.);
#67063=ORIENTED_EDGE('',*,*,#50478,.T.);
#67064=ORIENTED_EDGE('',*,*,#45941,.F.);
#67065=ORIENTED_EDGE('',*,*,#50480,.F.);
#67066=ORIENTED_EDGE('',*,*,#48586,.F.);
#67067=ORIENTED_EDGE('',*,*,#50479,.T.);
#67068=ORIENTED_EDGE('',*,*,#48605,.F.);
#67069=ORIENTED_EDGE('',*,*,#50481,.F.);
#67070=ORIENTED_EDGE('',*,*,#48314,.F.);
#67071=ORIENTED_EDGE('',*,*,#50480,.T.);
#67072=ORIENTED_EDGE('',*,*,#45940,.F.);
#67073=ORIENTED_EDGE('',*,*,#50482,.F.);
#67074=ORIENTED_EDGE('',*,*,#50163,.F.);
#67075=ORIENTED_EDGE('',*,*,#50481,.T.);
#67076=ORIENTED_EDGE('',*,*,#48604,.F.);
#67077=ORIENTED_EDGE('',*,*,#50483,.F.);
#67078=ORIENTED_EDGE('',*,*,#46429,.F.);
#67079=ORIENTED_EDGE('',*,*,#50482,.T.);
#67080=ORIENTED_EDGE('',*,*,#45939,.F.);
#67081=ORIENTED_EDGE('',*,*,#50484,.F.);
#67082=ORIENTED_EDGE('',*,*,#48592,.F.);
#67083=ORIENTED_EDGE('',*,*,#50483,.T.);
#67084=ORIENTED_EDGE('',*,*,#50162,.F.);
#67085=ORIENTED_EDGE('',*,*,#50485,.F.);
#67086=ORIENTED_EDGE('',*,*,#46430,.F.);
#67087=ORIENTED_EDGE('',*,*,#50484,.T.);
#67088=ORIENTED_EDGE('',*,*,#48345,.F.);
#67089=ORIENTED_EDGE('',*,*,#50486,.F.);
#67090=ORIENTED_EDGE('',*,*,#48593,.F.);
#67091=ORIENTED_EDGE('',*,*,#50485,.T.);
#67092=ORIENTED_EDGE('',*,*,#48588,.F.);
#67093=ORIENTED_EDGE('',*,*,#50487,.F.);
#67094=ORIENTED_EDGE('',*,*,#46431,.F.);
#67095=ORIENTED_EDGE('',*,*,#48340,.F.);
#67096=ORIENTED_EDGE('',*,*,#48336,.T.);
#67097=ORIENTED_EDGE('',*,*,#50488,.F.);
#67098=ORIENTED_EDGE('',*,*,#48594,.F.);
#67099=ORIENTED_EDGE('',*,*,#50486,.T.);
#67100=ORIENTED_EDGE('',*,*,#50487,.T.);
#67101=ORIENTED_EDGE('',*,*,#50164,.F.);
#67102=ORIENTED_EDGE('',*,*,#50489,.F.);
#67103=ORIENTED_EDGE('',*,*,#46432,.F.);
#67104=ORIENTED_EDGE('',*,*,#50488,.T.);
#67105=ORIENTED_EDGE('',*,*,#48335,.F.);
#67106=ORIENTED_EDGE('',*,*,#50490,.F.);
#67107=ORIENTED_EDGE('',*,*,#48595,.F.);
#67108=ORIENTED_EDGE('',*,*,#50489,.T.);
#67109=ORIENTED_EDGE('',*,*,#48590,.F.);
#67110=ORIENTED_EDGE('',*,*,#50491,.F.);
#67111=ORIENTED_EDGE('',*,*,#46433,.F.);
#67112=ORIENTED_EDGE('',*,*,#50490,.T.);
#67113=ORIENTED_EDGE('',*,*,#48347,.F.);
#67114=ORIENTED_EDGE('',*,*,#50492,.F.);
#67115=ORIENTED_EDGE('',*,*,#48596,.F.);
#67116=ORIENTED_EDGE('',*,*,#50491,.T.);
#67117=ORIENTED_EDGE('',*,*,#48589,.F.);
#67118=ORIENTED_EDGE('',*,*,#50493,.F.);
#67119=ORIENTED_EDGE('',*,*,#48343,.F.);
#67120=ORIENTED_EDGE('',*,*,#50492,.T.);
#67121=ORIENTED_EDGE('',*,*,#48331,.F.);
#67122=ORIENTED_EDGE('',*,*,#50494,.F.);
#67123=ORIENTED_EDGE('',*,*,#48597,.F.);
#67124=ORIENTED_EDGE('',*,*,#50493,.T.);
#67125=ORIENTED_EDGE('',*,*,#48600,.F.);
#67126=ORIENTED_EDGE('',*,*,#50495,.F.);
#67127=ORIENTED_EDGE('',*,*,#48322,.F.);
#67128=ORIENTED_EDGE('',*,*,#50494,.T.);
#67129=ORIENTED_EDGE('',*,*,#48349,.F.);
#67130=ORIENTED_EDGE('',*,*,#50496,.F.);
#67131=ORIENTED_EDGE('',*,*,#48598,.F.);
#67132=ORIENTED_EDGE('',*,*,#50495,.T.);
#67133=ORIENTED_EDGE('',*,*,#48599,.F.);
#67134=ORIENTED_EDGE('',*,*,#50496,.T.);
#67135=ORIENTED_EDGE('',*,*,#48327,.F.);
#67136=ORIENTED_EDGE('',*,*,#48323,.T.);
#67137=ORIENTED_EDGE('',*,*,#50497,.F.);
#67138=ORIENTED_EDGE('',*,*,#48639,.F.);
#67139=ORIENTED_EDGE('',*,*,#50498,.F.);
#67140=ORIENTED_EDGE('',*,*,#48279,.F.);
#67141=ORIENTED_EDGE('',*,*,#50498,.T.);
#67142=ORIENTED_EDGE('',*,*,#48638,.F.);
#67143=ORIENTED_EDGE('',*,*,#50499,.F.);
#67144=ORIENTED_EDGE('',*,*,#48288,.F.);
#67145=ORIENTED_EDGE('',*,*,#48278,.T.);
#67146=ORIENTED_EDGE('',*,*,#48282,.F.);
#67147=ORIENTED_EDGE('',*,*,#50500,.F.);
#67148=ORIENTED_EDGE('',*,*,#48640,.F.);
#67149=ORIENTED_EDGE('',*,*,#50497,.T.);
#67150=ORIENTED_EDGE('',*,*,#50499,.T.);
#67151=ORIENTED_EDGE('',*,*,#48637,.F.);
#67152=ORIENTED_EDGE('',*,*,#50501,.F.);
#67153=ORIENTED_EDGE('',*,*,#48273,.F.);
#67154=ORIENTED_EDGE('',*,*,#50500,.T.);
#67155=ORIENTED_EDGE('',*,*,#48286,.F.);
#67156=ORIENTED_EDGE('',*,*,#50502,.F.);
#67157=ORIENTED_EDGE('',*,*,#48629,.F.);
#67158=ORIENTED_EDGE('',*,*,#50501,.T.);
#67159=ORIENTED_EDGE('',*,*,#48636,.F.);
#67160=ORIENTED_EDGE('',*,*,#50503,.F.);
#67161=ORIENTED_EDGE('',*,*,#48290,.F.);
#67162=ORIENTED_EDGE('',*,*,#50502,.T.);
#67163=ORIENTED_EDGE('',*,*,#45949,.F.);
#67164=ORIENTED_EDGE('',*,*,#50504,.F.);
#67165=ORIENTED_EDGE('',*,*,#48630,.F.);
#67166=ORIENTED_EDGE('',*,*,#50503,.T.);
#67167=ORIENTED_EDGE('',*,*,#48635,.F.);
#67168=ORIENTED_EDGE('',*,*,#50505,.F.);
#67169=ORIENTED_EDGE('',*,*,#48265,.T.);
#67170=ORIENTED_EDGE('',*,*,#48269,.F.);
#67171=ORIENTED_EDGE('',*,*,#50504,.T.);
#67172=ORIENTED_EDGE('',*,*,#45948,.F.);
#67173=ORIENTED_EDGE('',*,*,#50506,.F.);
#67174=ORIENTED_EDGE('',*,*,#50165,.F.);
#67175=ORIENTED_EDGE('',*,*,#50505,.T.);
#67176=ORIENTED_EDGE('',*,*,#48634,.F.);
#67177=ORIENTED_EDGE('',*,*,#50507,.F.);
#67178=ORIENTED_EDGE('',*,*,#48266,.F.);
#67179=ORIENTED_EDGE('',*,*,#50506,.T.);
#67180=ORIENTED_EDGE('',*,*,#45947,.F.);
#67181=ORIENTED_EDGE('',*,*,#50508,.F.);
#67182=ORIENTED_EDGE('',*,*,#48614,.F.);
#67183=ORIENTED_EDGE('',*,*,#50507,.T.);
#67184=ORIENTED_EDGE('',*,*,#48633,.F.);
#67185=ORIENTED_EDGE('',*,*,#50509,.F.);
#67186=ORIENTED_EDGE('',*,*,#48284,.F.);
#67187=ORIENTED_EDGE('',*,*,#50508,.T.);
#67188=ORIENTED_EDGE('',*,*,#45946,.F.);
#67189=ORIENTED_EDGE('',*,*,#50510,.F.);
#67190=ORIENTED_EDGE('',*,*,#50167,.F.);
#67191=ORIENTED_EDGE('',*,*,#50509,.T.);
#67192=ORIENTED_EDGE('',*,*,#48632,.F.);
#67193=ORIENTED_EDGE('',*,*,#50511,.F.);
#67194=ORIENTED_EDGE('',*,*,#46423,.F.);
#67195=ORIENTED_EDGE('',*,*,#50510,.T.);
#67196=ORIENTED_EDGE('',*,*,#45945,.F.);
#67197=ORIENTED_EDGE('',*,*,#50512,.F.);
#67198=ORIENTED_EDGE('',*,*,#48620,.F.);
#67199=ORIENTED_EDGE('',*,*,#50511,.T.);
#67200=ORIENTED_EDGE('',*,*,#50166,.F.);
#67201=ORIENTED_EDGE('',*,*,#50513,.F.);
#67202=ORIENTED_EDGE('',*,*,#46424,.F.);
#67203=ORIENTED_EDGE('',*,*,#50512,.T.);
#67204=ORIENTED_EDGE('',*,*,#48315,.F.);
#67205=ORIENTED_EDGE('',*,*,#50514,.F.);
#67206=ORIENTED_EDGE('',*,*,#48621,.F.);
#67207=ORIENTED_EDGE('',*,*,#50513,.T.);
#67208=ORIENTED_EDGE('',*,*,#48616,.F.);
#67209=ORIENTED_EDGE('',*,*,#50515,.F.);
#67210=ORIENTED_EDGE('',*,*,#46425,.F.);
#67211=ORIENTED_EDGE('',*,*,#48310,.F.);
#67212=ORIENTED_EDGE('',*,*,#48306,.T.);
#67213=ORIENTED_EDGE('',*,*,#50516,.F.);
#67214=ORIENTED_EDGE('',*,*,#48622,.F.);
#67215=ORIENTED_EDGE('',*,*,#50514,.T.);
#67216=ORIENTED_EDGE('',*,*,#50515,.T.);
#67217=ORIENTED_EDGE('',*,*,#50168,.F.);
#67218=ORIENTED_EDGE('',*,*,#50517,.F.);
#67219=ORIENTED_EDGE('',*,*,#46426,.F.);
#67220=ORIENTED_EDGE('',*,*,#50516,.T.);
#67221=ORIENTED_EDGE('',*,*,#48305,.F.);
#67222=ORIENTED_EDGE('',*,*,#50518,.F.);
#67223=ORIENTED_EDGE('',*,*,#48623,.F.);
#67224=ORIENTED_EDGE('',*,*,#50517,.T.);
#67225=ORIENTED_EDGE('',*,*,#48618,.F.);
#67226=ORIENTED_EDGE('',*,*,#50519,.F.);
#67227=ORIENTED_EDGE('',*,*,#46427,.F.);
#67228=ORIENTED_EDGE('',*,*,#50518,.T.);
#67229=ORIENTED_EDGE('',*,*,#48317,.F.);
#67230=ORIENTED_EDGE('',*,*,#50520,.F.);
#67231=ORIENTED_EDGE('',*,*,#48624,.F.);
#67232=ORIENTED_EDGE('',*,*,#50519,.T.);
#67233=ORIENTED_EDGE('',*,*,#48617,.F.);
#67234=ORIENTED_EDGE('',*,*,#50521,.F.);
#67235=ORIENTED_EDGE('',*,*,#48313,.F.);
#67236=ORIENTED_EDGE('',*,*,#50520,.T.);
#67237=ORIENTED_EDGE('',*,*,#48301,.F.);
#67238=ORIENTED_EDGE('',*,*,#50522,.F.);
#67239=ORIENTED_EDGE('',*,*,#48625,.F.);
#67240=ORIENTED_EDGE('',*,*,#50521,.T.);
#67241=ORIENTED_EDGE('',*,*,#48628,.F.);
#67242=ORIENTED_EDGE('',*,*,#50523,.F.);
#67243=ORIENTED_EDGE('',*,*,#48292,.F.);
#67244=ORIENTED_EDGE('',*,*,#50522,.T.);
#67245=ORIENTED_EDGE('',*,*,#48319,.F.);
#67246=ORIENTED_EDGE('',*,*,#50524,.F.);
#67247=ORIENTED_EDGE('',*,*,#48626,.F.);
#67248=ORIENTED_EDGE('',*,*,#50523,.T.);
#67249=ORIENTED_EDGE('',*,*,#48627,.F.);
#67250=ORIENTED_EDGE('',*,*,#50524,.T.);
#67251=ORIENTED_EDGE('',*,*,#48297,.F.);
#67252=ORIENTED_EDGE('',*,*,#48293,.T.);
#67253=ORIENTED_EDGE('',*,*,#50525,.F.);
#67254=ORIENTED_EDGE('',*,*,#48667,.F.);
#67255=ORIENTED_EDGE('',*,*,#50526,.F.);
#67256=ORIENTED_EDGE('',*,*,#48249,.F.);
#67257=ORIENTED_EDGE('',*,*,#50526,.T.);
#67258=ORIENTED_EDGE('',*,*,#48666,.F.);
#67259=ORIENTED_EDGE('',*,*,#50527,.F.);
#67260=ORIENTED_EDGE('',*,*,#48258,.F.);
#67261=ORIENTED_EDGE('',*,*,#48248,.T.);
#67262=ORIENTED_EDGE('',*,*,#48252,.F.);
#67263=ORIENTED_EDGE('',*,*,#50528,.F.);
#67264=ORIENTED_EDGE('',*,*,#48668,.F.);
#67265=ORIENTED_EDGE('',*,*,#50525,.T.);
#67266=ORIENTED_EDGE('',*,*,#50527,.T.);
#67267=ORIENTED_EDGE('',*,*,#48665,.F.);
#67268=ORIENTED_EDGE('',*,*,#50529,.F.);
#67269=ORIENTED_EDGE('',*,*,#48243,.F.);
#67270=ORIENTED_EDGE('',*,*,#50528,.T.);
#67271=ORIENTED_EDGE('',*,*,#48256,.F.);
#67272=ORIENTED_EDGE('',*,*,#50530,.F.);
#67273=ORIENTED_EDGE('',*,*,#48657,.F.);
#67274=ORIENTED_EDGE('',*,*,#50529,.T.);
#67275=ORIENTED_EDGE('',*,*,#48664,.F.);
#67276=ORIENTED_EDGE('',*,*,#50531,.F.);
#67277=ORIENTED_EDGE('',*,*,#48260,.F.);
#67278=ORIENTED_EDGE('',*,*,#50530,.T.);
#67279=ORIENTED_EDGE('',*,*,#45955,.F.);
#67280=ORIENTED_EDGE('',*,*,#50532,.F.);
#67281=ORIENTED_EDGE('',*,*,#48658,.F.);
#67282=ORIENTED_EDGE('',*,*,#50531,.T.);
#67283=ORIENTED_EDGE('',*,*,#48663,.F.);
#67284=ORIENTED_EDGE('',*,*,#50533,.F.);
#67285=ORIENTED_EDGE('',*,*,#48235,.T.);
#67286=ORIENTED_EDGE('',*,*,#48239,.F.);
#67287=ORIENTED_EDGE('',*,*,#50532,.T.);
#67288=ORIENTED_EDGE('',*,*,#45954,.F.);
#67289=ORIENTED_EDGE('',*,*,#50534,.F.);
#67290=ORIENTED_EDGE('',*,*,#50169,.F.);
#67291=ORIENTED_EDGE('',*,*,#50533,.T.);
#67292=ORIENTED_EDGE('',*,*,#48662,.F.);
#67293=ORIENTED_EDGE('',*,*,#50535,.F.);
#67294=ORIENTED_EDGE('',*,*,#48236,.F.);
#67295=ORIENTED_EDGE('',*,*,#50534,.T.);
#67296=ORIENTED_EDGE('',*,*,#45953,.F.);
#67297=ORIENTED_EDGE('',*,*,#50536,.F.);
#67298=ORIENTED_EDGE('',*,*,#48642,.F.);
#67299=ORIENTED_EDGE('',*,*,#50535,.T.);
#67300=ORIENTED_EDGE('',*,*,#48661,.F.);
#67301=ORIENTED_EDGE('',*,*,#50537,.F.);
#67302=ORIENTED_EDGE('',*,*,#48254,.F.);
#67303=ORIENTED_EDGE('',*,*,#50536,.T.);
#67304=ORIENTED_EDGE('',*,*,#45952,.F.);
#67305=ORIENTED_EDGE('',*,*,#50538,.F.);
#67306=ORIENTED_EDGE('',*,*,#50171,.F.);
#67307=ORIENTED_EDGE('',*,*,#50537,.T.);
#67308=ORIENTED_EDGE('',*,*,#48660,.F.);
#67309=ORIENTED_EDGE('',*,*,#50539,.F.);
#67310=ORIENTED_EDGE('',*,*,#46417,.F.);
#67311=ORIENTED_EDGE('',*,*,#50538,.T.);
#67312=ORIENTED_EDGE('',*,*,#45951,.F.);
#67313=ORIENTED_EDGE('',*,*,#50540,.F.);
#67314=ORIENTED_EDGE('',*,*,#48648,.F.);
#67315=ORIENTED_EDGE('',*,*,#50539,.T.);
#67316=ORIENTED_EDGE('',*,*,#50170,.F.);
#67317=ORIENTED_EDGE('',*,*,#50541,.F.);
#67318=ORIENTED_EDGE('',*,*,#46418,.F.);
#67319=ORIENTED_EDGE('',*,*,#50540,.T.);
#67320=ORIENTED_EDGE('',*,*,#48285,.F.);
#67321=ORIENTED_EDGE('',*,*,#50542,.F.);
#67322=ORIENTED_EDGE('',*,*,#48649,.F.);
#67323=ORIENTED_EDGE('',*,*,#50541,.T.);
#67324=ORIENTED_EDGE('',*,*,#48644,.F.);
#67325=ORIENTED_EDGE('',*,*,#50543,.F.);
#67326=ORIENTED_EDGE('',*,*,#46419,.F.);
#67327=ORIENTED_EDGE('',*,*,#48280,.F.);
#67328=ORIENTED_EDGE('',*,*,#48276,.T.);
#67329=ORIENTED_EDGE('',*,*,#50544,.F.);
#67330=ORIENTED_EDGE('',*,*,#48650,.F.);
#67331=ORIENTED_EDGE('',*,*,#50542,.T.);
#67332=ORIENTED_EDGE('',*,*,#50543,.T.);
#67333=ORIENTED_EDGE('',*,*,#50172,.F.);
#67334=ORIENTED_EDGE('',*,*,#50545,.F.);
#67335=ORIENTED_EDGE('',*,*,#46420,.F.);
#67336=ORIENTED_EDGE('',*,*,#50544,.T.);
#67337=ORIENTED_EDGE('',*,*,#48275,.F.);
#67338=ORIENTED_EDGE('',*,*,#50546,.F.);
#67339=ORIENTED_EDGE('',*,*,#48651,.F.);
#67340=ORIENTED_EDGE('',*,*,#50545,.T.);
#67341=ORIENTED_EDGE('',*,*,#48646,.F.);
#67342=ORIENTED_EDGE('',*,*,#50547,.F.);
#67343=ORIENTED_EDGE('',*,*,#46421,.F.);
#67344=ORIENTED_EDGE('',*,*,#50546,.T.);
#67345=ORIENTED_EDGE('',*,*,#48287,.F.);
#67346=ORIENTED_EDGE('',*,*,#50548,.F.);
#67347=ORIENTED_EDGE('',*,*,#48652,.F.);
#67348=ORIENTED_EDGE('',*,*,#50547,.T.);
#67349=ORIENTED_EDGE('',*,*,#48645,.F.);
#67350=ORIENTED_EDGE('',*,*,#50549,.F.);
#67351=ORIENTED_EDGE('',*,*,#48283,.F.);
#67352=ORIENTED_EDGE('',*,*,#50548,.T.);
#67353=ORIENTED_EDGE('',*,*,#48271,.F.);
#67354=ORIENTED_EDGE('',*,*,#50550,.F.);
#67355=ORIENTED_EDGE('',*,*,#48653,.F.);
#67356=ORIENTED_EDGE('',*,*,#50549,.T.);
#67357=ORIENTED_EDGE('',*,*,#48656,.F.);
#67358=ORIENTED_EDGE('',*,*,#50551,.F.);
#67359=ORIENTED_EDGE('',*,*,#48262,.F.);
#67360=ORIENTED_EDGE('',*,*,#50550,.T.);
#67361=ORIENTED_EDGE('',*,*,#48289,.F.);
#67362=ORIENTED_EDGE('',*,*,#50552,.F.);
#67363=ORIENTED_EDGE('',*,*,#48654,.F.);
#67364=ORIENTED_EDGE('',*,*,#50551,.T.);
#67365=ORIENTED_EDGE('',*,*,#48655,.F.);
#67366=ORIENTED_EDGE('',*,*,#50552,.T.);
#67367=ORIENTED_EDGE('',*,*,#48267,.F.);
#67368=ORIENTED_EDGE('',*,*,#48263,.T.);
#67369=ORIENTED_EDGE('',*,*,#50553,.F.);
#67370=ORIENTED_EDGE('',*,*,#48695,.F.);
#67371=ORIENTED_EDGE('',*,*,#50554,.F.);
#67372=ORIENTED_EDGE('',*,*,#48219,.F.);
#67373=ORIENTED_EDGE('',*,*,#50554,.T.);
#67374=ORIENTED_EDGE('',*,*,#48694,.F.);
#67375=ORIENTED_EDGE('',*,*,#50555,.F.);
#67376=ORIENTED_EDGE('',*,*,#48228,.F.);
#67377=ORIENTED_EDGE('',*,*,#48218,.T.);
#67378=ORIENTED_EDGE('',*,*,#48222,.F.);
#67379=ORIENTED_EDGE('',*,*,#50556,.F.);
#67380=ORIENTED_EDGE('',*,*,#48696,.F.);
#67381=ORIENTED_EDGE('',*,*,#50553,.T.);
#67382=ORIENTED_EDGE('',*,*,#50555,.T.);
#67383=ORIENTED_EDGE('',*,*,#48693,.F.);
#67384=ORIENTED_EDGE('',*,*,#50557,.F.);
#67385=ORIENTED_EDGE('',*,*,#48213,.F.);
#67386=ORIENTED_EDGE('',*,*,#50556,.T.);
#67387=ORIENTED_EDGE('',*,*,#48226,.F.);
#67388=ORIENTED_EDGE('',*,*,#50558,.F.);
#67389=ORIENTED_EDGE('',*,*,#48685,.F.);
#67390=ORIENTED_EDGE('',*,*,#50557,.T.);
#67391=ORIENTED_EDGE('',*,*,#48692,.F.);
#67392=ORIENTED_EDGE('',*,*,#50559,.F.);
#67393=ORIENTED_EDGE('',*,*,#48230,.F.);
#67394=ORIENTED_EDGE('',*,*,#50558,.T.);
#67395=ORIENTED_EDGE('',*,*,#45961,.F.);
#67396=ORIENTED_EDGE('',*,*,#50560,.F.);
#67397=ORIENTED_EDGE('',*,*,#48686,.F.);
#67398=ORIENTED_EDGE('',*,*,#50559,.T.);
#67399=ORIENTED_EDGE('',*,*,#48691,.F.);
#67400=ORIENTED_EDGE('',*,*,#50561,.F.);
#67401=ORIENTED_EDGE('',*,*,#48205,.T.);
#67402=ORIENTED_EDGE('',*,*,#48209,.F.);
#67403=ORIENTED_EDGE('',*,*,#50560,.T.);
#67404=ORIENTED_EDGE('',*,*,#45960,.F.);
#67405=ORIENTED_EDGE('',*,*,#50562,.F.);
#67406=ORIENTED_EDGE('',*,*,#50173,.F.);
#67407=ORIENTED_EDGE('',*,*,#50561,.T.);
#67408=ORIENTED_EDGE('',*,*,#48690,.F.);
#67409=ORIENTED_EDGE('',*,*,#50563,.F.);
#67410=ORIENTED_EDGE('',*,*,#48206,.F.);
#67411=ORIENTED_EDGE('',*,*,#50562,.T.);
#67412=ORIENTED_EDGE('',*,*,#45959,.F.);
#67413=ORIENTED_EDGE('',*,*,#50564,.F.);
#67414=ORIENTED_EDGE('',*,*,#48670,.F.);
#67415=ORIENTED_EDGE('',*,*,#50563,.T.);
#67416=ORIENTED_EDGE('',*,*,#48689,.F.);
#67417=ORIENTED_EDGE('',*,*,#50565,.F.);
#67418=ORIENTED_EDGE('',*,*,#48224,.F.);
#67419=ORIENTED_EDGE('',*,*,#50564,.T.);
#67420=ORIENTED_EDGE('',*,*,#45958,.F.);
#67421=ORIENTED_EDGE('',*,*,#50566,.F.);
#67422=ORIENTED_EDGE('',*,*,#50175,.F.);
#67423=ORIENTED_EDGE('',*,*,#50565,.T.);
#67424=ORIENTED_EDGE('',*,*,#48688,.F.);
#67425=ORIENTED_EDGE('',*,*,#50567,.F.);
#67426=ORIENTED_EDGE('',*,*,#46411,.F.);
#67427=ORIENTED_EDGE('',*,*,#50566,.T.);
#67428=ORIENTED_EDGE('',*,*,#45957,.F.);
#67429=ORIENTED_EDGE('',*,*,#50568,.F.);
#67430=ORIENTED_EDGE('',*,*,#48676,.F.);
#67431=ORIENTED_EDGE('',*,*,#50567,.T.);
#67432=ORIENTED_EDGE('',*,*,#50174,.F.);
#67433=ORIENTED_EDGE('',*,*,#50569,.F.);
#67434=ORIENTED_EDGE('',*,*,#46412,.F.);
#67435=ORIENTED_EDGE('',*,*,#50568,.T.);
#67436=ORIENTED_EDGE('',*,*,#48255,.F.);
#67437=ORIENTED_EDGE('',*,*,#50570,.F.);
#67438=ORIENTED_EDGE('',*,*,#48677,.F.);
#67439=ORIENTED_EDGE('',*,*,#50569,.T.);
#67440=ORIENTED_EDGE('',*,*,#48672,.F.);
#67441=ORIENTED_EDGE('',*,*,#50571,.F.);
#67442=ORIENTED_EDGE('',*,*,#46413,.F.);
#67443=ORIENTED_EDGE('',*,*,#48250,.F.);
#67444=ORIENTED_EDGE('',*,*,#48246,.T.);
#67445=ORIENTED_EDGE('',*,*,#50572,.F.);
#67446=ORIENTED_EDGE('',*,*,#48678,.F.);
#67447=ORIENTED_EDGE('',*,*,#50570,.T.);
#67448=ORIENTED_EDGE('',*,*,#50571,.T.);
#67449=ORIENTED_EDGE('',*,*,#50176,.F.);
#67450=ORIENTED_EDGE('',*,*,#50573,.F.);
#67451=ORIENTED_EDGE('',*,*,#46414,.F.);
#67452=ORIENTED_EDGE('',*,*,#50572,.T.);
#67453=ORIENTED_EDGE('',*,*,#48245,.F.);
#67454=ORIENTED_EDGE('',*,*,#50574,.F.);
#67455=ORIENTED_EDGE('',*,*,#48679,.F.);
#67456=ORIENTED_EDGE('',*,*,#50573,.T.);
#67457=ORIENTED_EDGE('',*,*,#48674,.F.);
#67458=ORIENTED_EDGE('',*,*,#50575,.F.);
#67459=ORIENTED_EDGE('',*,*,#46415,.F.);
#67460=ORIENTED_EDGE('',*,*,#50574,.T.);
#67461=ORIENTED_EDGE('',*,*,#48257,.F.);
#67462=ORIENTED_EDGE('',*,*,#50576,.F.);
#67463=ORIENTED_EDGE('',*,*,#48680,.F.);
#67464=ORIENTED_EDGE('',*,*,#50575,.T.);
#67465=ORIENTED_EDGE('',*,*,#48673,.F.);
#67466=ORIENTED_EDGE('',*,*,#50577,.F.);
#67467=ORIENTED_EDGE('',*,*,#48253,.F.);
#67468=ORIENTED_EDGE('',*,*,#50576,.T.);
#67469=ORIENTED_EDGE('',*,*,#48241,.F.);
#67470=ORIENTED_EDGE('',*,*,#50578,.F.);
#67471=ORIENTED_EDGE('',*,*,#48681,.F.);
#67472=ORIENTED_EDGE('',*,*,#50577,.T.);
#67473=ORIENTED_EDGE('',*,*,#48684,.F.);
#67474=ORIENTED_EDGE('',*,*,#50579,.F.);
#67475=ORIENTED_EDGE('',*,*,#48232,.F.);
#67476=ORIENTED_EDGE('',*,*,#50578,.T.);
#67477=ORIENTED_EDGE('',*,*,#48259,.F.);
#67478=ORIENTED_EDGE('',*,*,#50580,.F.);
#67479=ORIENTED_EDGE('',*,*,#48682,.F.);
#67480=ORIENTED_EDGE('',*,*,#50579,.T.);
#67481=ORIENTED_EDGE('',*,*,#48683,.F.);
#67482=ORIENTED_EDGE('',*,*,#50580,.T.);
#67483=ORIENTED_EDGE('',*,*,#48237,.F.);
#67484=ORIENTED_EDGE('',*,*,#48233,.T.);
#67485=ORIENTED_EDGE('',*,*,#50581,.F.);
#67486=ORIENTED_EDGE('',*,*,#48723,.F.);
#67487=ORIENTED_EDGE('',*,*,#50582,.F.);
#67488=ORIENTED_EDGE('',*,*,#48189,.F.);
#67489=ORIENTED_EDGE('',*,*,#50582,.T.);
#67490=ORIENTED_EDGE('',*,*,#48722,.F.);
#67491=ORIENTED_EDGE('',*,*,#50583,.F.);
#67492=ORIENTED_EDGE('',*,*,#48198,.F.);
#67493=ORIENTED_EDGE('',*,*,#48188,.T.);
#67494=ORIENTED_EDGE('',*,*,#48192,.F.);
#67495=ORIENTED_EDGE('',*,*,#50584,.F.);
#67496=ORIENTED_EDGE('',*,*,#48724,.F.);
#67497=ORIENTED_EDGE('',*,*,#50581,.T.);
#67498=ORIENTED_EDGE('',*,*,#50583,.T.);
#67499=ORIENTED_EDGE('',*,*,#48721,.F.);
#67500=ORIENTED_EDGE('',*,*,#50585,.F.);
#67501=ORIENTED_EDGE('',*,*,#48183,.F.);
#67502=ORIENTED_EDGE('',*,*,#50584,.T.);
#67503=ORIENTED_EDGE('',*,*,#48196,.F.);
#67504=ORIENTED_EDGE('',*,*,#50586,.F.);
#67505=ORIENTED_EDGE('',*,*,#48713,.F.);
#67506=ORIENTED_EDGE('',*,*,#50585,.T.);
#67507=ORIENTED_EDGE('',*,*,#48720,.F.);
#67508=ORIENTED_EDGE('',*,*,#50587,.F.);
#67509=ORIENTED_EDGE('',*,*,#48200,.F.);
#67510=ORIENTED_EDGE('',*,*,#50586,.T.);
#67511=ORIENTED_EDGE('',*,*,#45967,.F.);
#67512=ORIENTED_EDGE('',*,*,#50588,.F.);
#67513=ORIENTED_EDGE('',*,*,#48714,.F.);
#67514=ORIENTED_EDGE('',*,*,#50587,.T.);
#67515=ORIENTED_EDGE('',*,*,#48719,.F.);
#67516=ORIENTED_EDGE('',*,*,#50589,.F.);
#67517=ORIENTED_EDGE('',*,*,#48175,.T.);
#67518=ORIENTED_EDGE('',*,*,#48179,.F.);
#67519=ORIENTED_EDGE('',*,*,#50588,.T.);
#67520=ORIENTED_EDGE('',*,*,#45966,.F.);
#67521=ORIENTED_EDGE('',*,*,#50590,.F.);
#67522=ORIENTED_EDGE('',*,*,#50177,.F.);
#67523=ORIENTED_EDGE('',*,*,#50589,.T.);
#67524=ORIENTED_EDGE('',*,*,#48718,.F.);
#67525=ORIENTED_EDGE('',*,*,#50591,.F.);
#67526=ORIENTED_EDGE('',*,*,#48176,.F.);
#67527=ORIENTED_EDGE('',*,*,#50590,.T.);
#67528=ORIENTED_EDGE('',*,*,#45965,.F.);
#67529=ORIENTED_EDGE('',*,*,#50592,.F.);
#67530=ORIENTED_EDGE('',*,*,#48698,.F.);
#67531=ORIENTED_EDGE('',*,*,#50591,.T.);
#67532=ORIENTED_EDGE('',*,*,#48717,.F.);
#67533=ORIENTED_EDGE('',*,*,#50593,.F.);
#67534=ORIENTED_EDGE('',*,*,#48194,.F.);
#67535=ORIENTED_EDGE('',*,*,#50592,.T.);
#67536=ORIENTED_EDGE('',*,*,#45964,.F.);
#67537=ORIENTED_EDGE('',*,*,#50594,.F.);
#67538=ORIENTED_EDGE('',*,*,#50179,.F.);
#67539=ORIENTED_EDGE('',*,*,#50593,.T.);
#67540=ORIENTED_EDGE('',*,*,#48716,.F.);
#67541=ORIENTED_EDGE('',*,*,#50595,.F.);
#67542=ORIENTED_EDGE('',*,*,#46405,.F.);
#67543=ORIENTED_EDGE('',*,*,#50594,.T.);
#67544=ORIENTED_EDGE('',*,*,#45963,.F.);
#67545=ORIENTED_EDGE('',*,*,#50596,.F.);
#67546=ORIENTED_EDGE('',*,*,#48704,.F.);
#67547=ORIENTED_EDGE('',*,*,#50595,.T.);
#67548=ORIENTED_EDGE('',*,*,#50178,.F.);
#67549=ORIENTED_EDGE('',*,*,#50597,.F.);
#67550=ORIENTED_EDGE('',*,*,#46406,.F.);
#67551=ORIENTED_EDGE('',*,*,#50596,.T.);
#67552=ORIENTED_EDGE('',*,*,#48225,.F.);
#67553=ORIENTED_EDGE('',*,*,#50598,.F.);
#67554=ORIENTED_EDGE('',*,*,#48705,.F.);
#67555=ORIENTED_EDGE('',*,*,#50597,.T.);
#67556=ORIENTED_EDGE('',*,*,#48700,.F.);
#67557=ORIENTED_EDGE('',*,*,#50599,.F.);
#67558=ORIENTED_EDGE('',*,*,#46407,.F.);
#67559=ORIENTED_EDGE('',*,*,#48220,.F.);
#67560=ORIENTED_EDGE('',*,*,#48216,.T.);
#67561=ORIENTED_EDGE('',*,*,#50600,.F.);
#67562=ORIENTED_EDGE('',*,*,#48706,.F.);
#67563=ORIENTED_EDGE('',*,*,#50598,.T.);
#67564=ORIENTED_EDGE('',*,*,#50599,.T.);
#67565=ORIENTED_EDGE('',*,*,#50180,.F.);
#67566=ORIENTED_EDGE('',*,*,#50601,.F.);
#67567=ORIENTED_EDGE('',*,*,#46408,.F.);
#67568=ORIENTED_EDGE('',*,*,#50600,.T.);
#67569=ORIENTED_EDGE('',*,*,#48215,.F.);
#67570=ORIENTED_EDGE('',*,*,#50602,.F.);
#67571=ORIENTED_EDGE('',*,*,#48707,.F.);
#67572=ORIENTED_EDGE('',*,*,#50601,.T.);
#67573=ORIENTED_EDGE('',*,*,#48702,.F.);
#67574=ORIENTED_EDGE('',*,*,#50603,.F.);
#67575=ORIENTED_EDGE('',*,*,#46409,.F.);
#67576=ORIENTED_EDGE('',*,*,#50602,.T.);
#67577=ORIENTED_EDGE('',*,*,#48227,.F.);
#67578=ORIENTED_EDGE('',*,*,#50604,.F.);
#67579=ORIENTED_EDGE('',*,*,#48708,.F.);
#67580=ORIENTED_EDGE('',*,*,#50603,.T.);
#67581=ORIENTED_EDGE('',*,*,#48701,.F.);
#67582=ORIENTED_EDGE('',*,*,#50605,.F.);
#67583=ORIENTED_EDGE('',*,*,#48223,.F.);
#67584=ORIENTED_EDGE('',*,*,#50604,.T.);
#67585=ORIENTED_EDGE('',*,*,#48211,.F.);
#67586=ORIENTED_EDGE('',*,*,#50606,.F.);
#67587=ORIENTED_EDGE('',*,*,#48709,.F.);
#67588=ORIENTED_EDGE('',*,*,#50605,.T.);
#67589=ORIENTED_EDGE('',*,*,#48712,.F.);
#67590=ORIENTED_EDGE('',*,*,#50607,.F.);
#67591=ORIENTED_EDGE('',*,*,#48202,.F.);
#67592=ORIENTED_EDGE('',*,*,#50606,.T.);
#67593=ORIENTED_EDGE('',*,*,#48229,.F.);
#67594=ORIENTED_EDGE('',*,*,#50608,.F.);
#67595=ORIENTED_EDGE('',*,*,#48710,.F.);
#67596=ORIENTED_EDGE('',*,*,#50607,.T.);
#67597=ORIENTED_EDGE('',*,*,#48711,.F.);
#67598=ORIENTED_EDGE('',*,*,#50608,.T.);
#67599=ORIENTED_EDGE('',*,*,#48207,.F.);
#67600=ORIENTED_EDGE('',*,*,#48203,.T.);
#67601=ORIENTED_EDGE('',*,*,#50609,.F.);
#67602=ORIENTED_EDGE('',*,*,#48751,.F.);
#67603=ORIENTED_EDGE('',*,*,#50610,.F.);
#67604=ORIENTED_EDGE('',*,*,#48159,.F.);
#67605=ORIENTED_EDGE('',*,*,#50610,.T.);
#67606=ORIENTED_EDGE('',*,*,#48750,.F.);
#67607=ORIENTED_EDGE('',*,*,#50611,.F.);
#67608=ORIENTED_EDGE('',*,*,#48168,.F.);
#67609=ORIENTED_EDGE('',*,*,#48158,.T.);
#67610=ORIENTED_EDGE('',*,*,#48162,.F.);
#67611=ORIENTED_EDGE('',*,*,#50612,.F.);
#67612=ORIENTED_EDGE('',*,*,#48752,.F.);
#67613=ORIENTED_EDGE('',*,*,#50609,.T.);
#67614=ORIENTED_EDGE('',*,*,#50611,.T.);
#67615=ORIENTED_EDGE('',*,*,#48749,.F.);
#67616=ORIENTED_EDGE('',*,*,#50613,.F.);
#67617=ORIENTED_EDGE('',*,*,#48153,.F.);
#67618=ORIENTED_EDGE('',*,*,#50612,.T.);
#67619=ORIENTED_EDGE('',*,*,#48166,.F.);
#67620=ORIENTED_EDGE('',*,*,#50614,.F.);
#67621=ORIENTED_EDGE('',*,*,#48741,.F.);
#67622=ORIENTED_EDGE('',*,*,#50613,.T.);
#67623=ORIENTED_EDGE('',*,*,#48748,.F.);
#67624=ORIENTED_EDGE('',*,*,#50615,.F.);
#67625=ORIENTED_EDGE('',*,*,#48170,.F.);
#67626=ORIENTED_EDGE('',*,*,#50614,.T.);
#67627=ORIENTED_EDGE('',*,*,#45973,.F.);
#67628=ORIENTED_EDGE('',*,*,#50616,.F.);
#67629=ORIENTED_EDGE('',*,*,#48742,.F.);
#67630=ORIENTED_EDGE('',*,*,#50615,.T.);
#67631=ORIENTED_EDGE('',*,*,#48747,.F.);
#67632=ORIENTED_EDGE('',*,*,#50617,.F.);
#67633=ORIENTED_EDGE('',*,*,#48145,.T.);
#67634=ORIENTED_EDGE('',*,*,#48149,.F.);
#67635=ORIENTED_EDGE('',*,*,#50616,.T.);
#67636=ORIENTED_EDGE('',*,*,#45972,.F.);
#67637=ORIENTED_EDGE('',*,*,#50618,.F.);
#67638=ORIENTED_EDGE('',*,*,#50181,.F.);
#67639=ORIENTED_EDGE('',*,*,#50617,.T.);
#67640=ORIENTED_EDGE('',*,*,#48746,.F.);
#67641=ORIENTED_EDGE('',*,*,#50619,.F.);
#67642=ORIENTED_EDGE('',*,*,#48146,.F.);
#67643=ORIENTED_EDGE('',*,*,#50618,.T.);
#67644=ORIENTED_EDGE('',*,*,#45971,.F.);
#67645=ORIENTED_EDGE('',*,*,#50620,.F.);
#67646=ORIENTED_EDGE('',*,*,#48726,.F.);
#67647=ORIENTED_EDGE('',*,*,#50619,.T.);
#67648=ORIENTED_EDGE('',*,*,#48745,.F.);
#67649=ORIENTED_EDGE('',*,*,#50621,.F.);
#67650=ORIENTED_EDGE('',*,*,#48164,.F.);
#67651=ORIENTED_EDGE('',*,*,#50620,.T.);
#67652=ORIENTED_EDGE('',*,*,#45970,.F.);
#67653=ORIENTED_EDGE('',*,*,#50622,.F.);
#67654=ORIENTED_EDGE('',*,*,#50183,.F.);
#67655=ORIENTED_EDGE('',*,*,#50621,.T.);
#67656=ORIENTED_EDGE('',*,*,#48744,.F.);
#67657=ORIENTED_EDGE('',*,*,#50623,.F.);
#67658=ORIENTED_EDGE('',*,*,#46399,.F.);
#67659=ORIENTED_EDGE('',*,*,#50622,.T.);
#67660=ORIENTED_EDGE('',*,*,#45969,.F.);
#67661=ORIENTED_EDGE('',*,*,#50624,.F.);
#67662=ORIENTED_EDGE('',*,*,#48732,.F.);
#67663=ORIENTED_EDGE('',*,*,#50623,.T.);
#67664=ORIENTED_EDGE('',*,*,#50182,.F.);
#67665=ORIENTED_EDGE('',*,*,#50625,.F.);
#67666=ORIENTED_EDGE('',*,*,#46400,.F.);
#67667=ORIENTED_EDGE('',*,*,#50624,.T.);
#67668=ORIENTED_EDGE('',*,*,#48195,.F.);
#67669=ORIENTED_EDGE('',*,*,#50626,.F.);
#67670=ORIENTED_EDGE('',*,*,#48733,.F.);
#67671=ORIENTED_EDGE('',*,*,#50625,.T.);
#67672=ORIENTED_EDGE('',*,*,#48728,.F.);
#67673=ORIENTED_EDGE('',*,*,#50627,.F.);
#67674=ORIENTED_EDGE('',*,*,#46401,.F.);
#67675=ORIENTED_EDGE('',*,*,#48190,.F.);
#67676=ORIENTED_EDGE('',*,*,#48186,.T.);
#67677=ORIENTED_EDGE('',*,*,#50628,.F.);
#67678=ORIENTED_EDGE('',*,*,#48734,.F.);
#67679=ORIENTED_EDGE('',*,*,#50626,.T.);
#67680=ORIENTED_EDGE('',*,*,#50627,.T.);
#67681=ORIENTED_EDGE('',*,*,#50184,.F.);
#67682=ORIENTED_EDGE('',*,*,#50629,.F.);
#67683=ORIENTED_EDGE('',*,*,#46402,.F.);
#67684=ORIENTED_EDGE('',*,*,#50628,.T.);
#67685=ORIENTED_EDGE('',*,*,#48185,.F.);
#67686=ORIENTED_EDGE('',*,*,#50630,.F.);
#67687=ORIENTED_EDGE('',*,*,#48735,.F.);
#67688=ORIENTED_EDGE('',*,*,#50629,.T.);
#67689=ORIENTED_EDGE('',*,*,#48730,.F.);
#67690=ORIENTED_EDGE('',*,*,#50631,.F.);
#67691=ORIENTED_EDGE('',*,*,#46403,.F.);
#67692=ORIENTED_EDGE('',*,*,#50630,.T.);
#67693=ORIENTED_EDGE('',*,*,#48197,.F.);
#67694=ORIENTED_EDGE('',*,*,#50632,.F.);
#67695=ORIENTED_EDGE('',*,*,#48736,.F.);
#67696=ORIENTED_EDGE('',*,*,#50631,.T.);
#67697=ORIENTED_EDGE('',*,*,#48729,.F.);
#67698=ORIENTED_EDGE('',*,*,#50633,.F.);
#67699=ORIENTED_EDGE('',*,*,#48193,.F.);
#67700=ORIENTED_EDGE('',*,*,#50632,.T.);
#67701=ORIENTED_EDGE('',*,*,#48181,.F.);
#67702=ORIENTED_EDGE('',*,*,#50634,.F.);
#67703=ORIENTED_EDGE('',*,*,#48737,.F.);
#67704=ORIENTED_EDGE('',*,*,#50633,.T.);
#67705=ORIENTED_EDGE('',*,*,#48740,.F.);
#67706=ORIENTED_EDGE('',*,*,#50635,.F.);
#67707=ORIENTED_EDGE('',*,*,#48172,.F.);
#67708=ORIENTED_EDGE('',*,*,#50634,.T.);
#67709=ORIENTED_EDGE('',*,*,#48199,.F.);
#67710=ORIENTED_EDGE('',*,*,#50636,.F.);
#67711=ORIENTED_EDGE('',*,*,#48738,.F.);
#67712=ORIENTED_EDGE('',*,*,#50635,.T.);
#67713=ORIENTED_EDGE('',*,*,#48739,.F.);
#67714=ORIENTED_EDGE('',*,*,#50636,.T.);
#67715=ORIENTED_EDGE('',*,*,#48177,.F.);
#67716=ORIENTED_EDGE('',*,*,#48173,.T.);
#67717=ORIENTED_EDGE('',*,*,#50637,.F.);
#67718=ORIENTED_EDGE('',*,*,#48779,.F.);
#67719=ORIENTED_EDGE('',*,*,#50638,.F.);
#67720=ORIENTED_EDGE('',*,*,#48129,.F.);
#67721=ORIENTED_EDGE('',*,*,#50638,.T.);
#67722=ORIENTED_EDGE('',*,*,#48778,.F.);
#67723=ORIENTED_EDGE('',*,*,#50639,.F.);
#67724=ORIENTED_EDGE('',*,*,#48138,.F.);
#67725=ORIENTED_EDGE('',*,*,#48128,.T.);
#67726=ORIENTED_EDGE('',*,*,#48132,.F.);
#67727=ORIENTED_EDGE('',*,*,#50640,.F.);
#67728=ORIENTED_EDGE('',*,*,#48780,.F.);
#67729=ORIENTED_EDGE('',*,*,#50637,.T.);
#67730=ORIENTED_EDGE('',*,*,#50639,.T.);
#67731=ORIENTED_EDGE('',*,*,#48777,.F.);
#67732=ORIENTED_EDGE('',*,*,#50641,.F.);
#67733=ORIENTED_EDGE('',*,*,#48123,.F.);
#67734=ORIENTED_EDGE('',*,*,#50640,.T.);
#67735=ORIENTED_EDGE('',*,*,#48136,.F.);
#67736=ORIENTED_EDGE('',*,*,#50642,.F.);
#67737=ORIENTED_EDGE('',*,*,#48769,.F.);
#67738=ORIENTED_EDGE('',*,*,#50641,.T.);
#67739=ORIENTED_EDGE('',*,*,#48776,.F.);
#67740=ORIENTED_EDGE('',*,*,#50643,.F.);
#67741=ORIENTED_EDGE('',*,*,#48140,.F.);
#67742=ORIENTED_EDGE('',*,*,#50642,.T.);
#67743=ORIENTED_EDGE('',*,*,#45979,.F.);
#67744=ORIENTED_EDGE('',*,*,#50644,.F.);
#67745=ORIENTED_EDGE('',*,*,#48770,.F.);
#67746=ORIENTED_EDGE('',*,*,#50643,.T.);
#67747=ORIENTED_EDGE('',*,*,#48775,.F.);
#67748=ORIENTED_EDGE('',*,*,#50645,.F.);
#67749=ORIENTED_EDGE('',*,*,#48115,.T.);
#67750=ORIENTED_EDGE('',*,*,#48119,.F.);
#67751=ORIENTED_EDGE('',*,*,#50644,.T.);
#67752=ORIENTED_EDGE('',*,*,#45978,.F.);
#67753=ORIENTED_EDGE('',*,*,#50646,.F.);
#67754=ORIENTED_EDGE('',*,*,#50185,.F.);
#67755=ORIENTED_EDGE('',*,*,#50645,.T.);
#67756=ORIENTED_EDGE('',*,*,#48774,.F.);
#67757=ORIENTED_EDGE('',*,*,#50647,.F.);
#67758=ORIENTED_EDGE('',*,*,#48116,.F.);
#67759=ORIENTED_EDGE('',*,*,#50646,.T.);
#67760=ORIENTED_EDGE('',*,*,#45977,.F.);
#67761=ORIENTED_EDGE('',*,*,#50648,.F.);
#67762=ORIENTED_EDGE('',*,*,#48754,.F.);
#67763=ORIENTED_EDGE('',*,*,#50647,.T.);
#67764=ORIENTED_EDGE('',*,*,#48773,.F.);
#67765=ORIENTED_EDGE('',*,*,#50649,.F.);
#67766=ORIENTED_EDGE('',*,*,#48134,.F.);
#67767=ORIENTED_EDGE('',*,*,#50648,.T.);
#67768=ORIENTED_EDGE('',*,*,#45976,.F.);
#67769=ORIENTED_EDGE('',*,*,#50650,.F.);
#67770=ORIENTED_EDGE('',*,*,#50187,.F.);
#67771=ORIENTED_EDGE('',*,*,#50649,.T.);
#67772=ORIENTED_EDGE('',*,*,#48772,.F.);
#67773=ORIENTED_EDGE('',*,*,#50651,.F.);
#67774=ORIENTED_EDGE('',*,*,#46393,.F.);
#67775=ORIENTED_EDGE('',*,*,#50650,.T.);
#67776=ORIENTED_EDGE('',*,*,#45975,.F.);
#67777=ORIENTED_EDGE('',*,*,#50652,.F.);
#67778=ORIENTED_EDGE('',*,*,#48760,.F.);
#67779=ORIENTED_EDGE('',*,*,#50651,.T.);
#67780=ORIENTED_EDGE('',*,*,#50186,.F.);
#67781=ORIENTED_EDGE('',*,*,#50653,.F.);
#67782=ORIENTED_EDGE('',*,*,#46394,.F.);
#67783=ORIENTED_EDGE('',*,*,#50652,.T.);
#67784=ORIENTED_EDGE('',*,*,#48165,.F.);
#67785=ORIENTED_EDGE('',*,*,#50654,.F.);
#67786=ORIENTED_EDGE('',*,*,#48761,.F.);
#67787=ORIENTED_EDGE('',*,*,#50653,.T.);
#67788=ORIENTED_EDGE('',*,*,#48756,.F.);
#67789=ORIENTED_EDGE('',*,*,#50655,.F.);
#67790=ORIENTED_EDGE('',*,*,#46395,.F.);
#67791=ORIENTED_EDGE('',*,*,#48160,.F.);
#67792=ORIENTED_EDGE('',*,*,#48156,.T.);
#67793=ORIENTED_EDGE('',*,*,#50656,.F.);
#67794=ORIENTED_EDGE('',*,*,#48762,.F.);
#67795=ORIENTED_EDGE('',*,*,#50654,.T.);
#67796=ORIENTED_EDGE('',*,*,#50655,.T.);
#67797=ORIENTED_EDGE('',*,*,#50188,.F.);
#67798=ORIENTED_EDGE('',*,*,#50657,.F.);
#67799=ORIENTED_EDGE('',*,*,#46396,.F.);
#67800=ORIENTED_EDGE('',*,*,#50656,.T.);
#67801=ORIENTED_EDGE('',*,*,#48155,.F.);
#67802=ORIENTED_EDGE('',*,*,#50658,.F.);
#67803=ORIENTED_EDGE('',*,*,#48763,.F.);
#67804=ORIENTED_EDGE('',*,*,#50657,.T.);
#67805=ORIENTED_EDGE('',*,*,#48758,.F.);
#67806=ORIENTED_EDGE('',*,*,#50659,.F.);
#67807=ORIENTED_EDGE('',*,*,#46397,.F.);
#67808=ORIENTED_EDGE('',*,*,#50658,.T.);
#67809=ORIENTED_EDGE('',*,*,#48167,.F.);
#67810=ORIENTED_EDGE('',*,*,#50660,.F.);
#67811=ORIENTED_EDGE('',*,*,#48764,.F.);
#67812=ORIENTED_EDGE('',*,*,#50659,.T.);
#67813=ORIENTED_EDGE('',*,*,#48757,.F.);
#67814=ORIENTED_EDGE('',*,*,#50661,.F.);
#67815=ORIENTED_EDGE('',*,*,#48163,.F.);
#67816=ORIENTED_EDGE('',*,*,#50660,.T.);
#67817=ORIENTED_EDGE('',*,*,#48151,.F.);
#67818=ORIENTED_EDGE('',*,*,#50662,.F.);
#67819=ORIENTED_EDGE('',*,*,#48765,.F.);
#67820=ORIENTED_EDGE('',*,*,#50661,.T.);
#67821=ORIENTED_EDGE('',*,*,#48768,.F.);
#67822=ORIENTED_EDGE('',*,*,#50663,.F.);
#67823=ORIENTED_EDGE('',*,*,#48142,.F.);
#67824=ORIENTED_EDGE('',*,*,#50662,.T.);
#67825=ORIENTED_EDGE('',*,*,#48169,.F.);
#67826=ORIENTED_EDGE('',*,*,#50664,.F.);
#67827=ORIENTED_EDGE('',*,*,#48766,.F.);
#67828=ORIENTED_EDGE('',*,*,#50663,.T.);
#67829=ORIENTED_EDGE('',*,*,#48767,.F.);
#67830=ORIENTED_EDGE('',*,*,#50664,.T.);
#67831=ORIENTED_EDGE('',*,*,#48147,.F.);
#67832=ORIENTED_EDGE('',*,*,#48143,.T.);
#67833=ORIENTED_EDGE('',*,*,#50665,.F.);
#67834=ORIENTED_EDGE('',*,*,#48807,.F.);
#67835=ORIENTED_EDGE('',*,*,#50666,.F.);
#67836=ORIENTED_EDGE('',*,*,#48099,.F.);
#67837=ORIENTED_EDGE('',*,*,#50666,.T.);
#67838=ORIENTED_EDGE('',*,*,#48806,.F.);
#67839=ORIENTED_EDGE('',*,*,#50667,.F.);
#67840=ORIENTED_EDGE('',*,*,#48108,.F.);
#67841=ORIENTED_EDGE('',*,*,#48098,.T.);
#67842=ORIENTED_EDGE('',*,*,#48102,.F.);
#67843=ORIENTED_EDGE('',*,*,#50668,.F.);
#67844=ORIENTED_EDGE('',*,*,#48808,.F.);
#67845=ORIENTED_EDGE('',*,*,#50665,.T.);
#67846=ORIENTED_EDGE('',*,*,#50667,.T.);
#67847=ORIENTED_EDGE('',*,*,#48805,.F.);
#67848=ORIENTED_EDGE('',*,*,#50669,.F.);
#67849=ORIENTED_EDGE('',*,*,#48093,.F.);
#67850=ORIENTED_EDGE('',*,*,#50668,.T.);
#67851=ORIENTED_EDGE('',*,*,#48106,.F.);
#67852=ORIENTED_EDGE('',*,*,#50670,.F.);
#67853=ORIENTED_EDGE('',*,*,#48797,.F.);
#67854=ORIENTED_EDGE('',*,*,#50669,.T.);
#67855=ORIENTED_EDGE('',*,*,#48804,.F.);
#67856=ORIENTED_EDGE('',*,*,#50671,.F.);
#67857=ORIENTED_EDGE('',*,*,#48110,.F.);
#67858=ORIENTED_EDGE('',*,*,#50670,.T.);
#67859=ORIENTED_EDGE('',*,*,#45985,.F.);
#67860=ORIENTED_EDGE('',*,*,#50672,.F.);
#67861=ORIENTED_EDGE('',*,*,#48798,.F.);
#67862=ORIENTED_EDGE('',*,*,#50671,.T.);
#67863=ORIENTED_EDGE('',*,*,#48803,.F.);
#67864=ORIENTED_EDGE('',*,*,#50673,.F.);
#67865=ORIENTED_EDGE('',*,*,#48085,.T.);
#67866=ORIENTED_EDGE('',*,*,#48089,.F.);
#67867=ORIENTED_EDGE('',*,*,#50672,.T.);
#67868=ORIENTED_EDGE('',*,*,#45984,.F.);
#67869=ORIENTED_EDGE('',*,*,#50674,.F.);
#67870=ORIENTED_EDGE('',*,*,#50189,.F.);
#67871=ORIENTED_EDGE('',*,*,#50673,.T.);
#67872=ORIENTED_EDGE('',*,*,#48802,.F.);
#67873=ORIENTED_EDGE('',*,*,#50675,.F.);
#67874=ORIENTED_EDGE('',*,*,#48086,.F.);
#67875=ORIENTED_EDGE('',*,*,#50674,.T.);
#67876=ORIENTED_EDGE('',*,*,#45983,.F.);
#67877=ORIENTED_EDGE('',*,*,#50676,.F.);
#67878=ORIENTED_EDGE('',*,*,#48782,.F.);
#67879=ORIENTED_EDGE('',*,*,#50675,.T.);
#67880=ORIENTED_EDGE('',*,*,#48801,.F.);
#67881=ORIENTED_EDGE('',*,*,#50677,.F.);
#67882=ORIENTED_EDGE('',*,*,#48104,.F.);
#67883=ORIENTED_EDGE('',*,*,#50676,.T.);
#67884=ORIENTED_EDGE('',*,*,#45982,.F.);
#67885=ORIENTED_EDGE('',*,*,#50678,.F.);
#67886=ORIENTED_EDGE('',*,*,#50191,.F.);
#67887=ORIENTED_EDGE('',*,*,#50677,.T.);
#67888=ORIENTED_EDGE('',*,*,#48800,.F.);
#67889=ORIENTED_EDGE('',*,*,#50679,.F.);
#67890=ORIENTED_EDGE('',*,*,#46387,.F.);
#67891=ORIENTED_EDGE('',*,*,#50678,.T.);
#67892=ORIENTED_EDGE('',*,*,#45981,.F.);
#67893=ORIENTED_EDGE('',*,*,#50680,.F.);
#67894=ORIENTED_EDGE('',*,*,#48788,.F.);
#67895=ORIENTED_EDGE('',*,*,#50679,.T.);
#67896=ORIENTED_EDGE('',*,*,#50190,.F.);
#67897=ORIENTED_EDGE('',*,*,#50681,.F.);
#67898=ORIENTED_EDGE('',*,*,#46388,.F.);
#67899=ORIENTED_EDGE('',*,*,#50680,.T.);
#67900=ORIENTED_EDGE('',*,*,#48135,.F.);
#67901=ORIENTED_EDGE('',*,*,#50682,.F.);
#67902=ORIENTED_EDGE('',*,*,#48789,.F.);
#67903=ORIENTED_EDGE('',*,*,#50681,.T.);
#67904=ORIENTED_EDGE('',*,*,#48784,.F.);
#67905=ORIENTED_EDGE('',*,*,#50683,.F.);
#67906=ORIENTED_EDGE('',*,*,#46389,.F.);
#67907=ORIENTED_EDGE('',*,*,#48130,.F.);
#67908=ORIENTED_EDGE('',*,*,#48126,.T.);
#67909=ORIENTED_EDGE('',*,*,#50684,.F.);
#67910=ORIENTED_EDGE('',*,*,#48790,.F.);
#67911=ORIENTED_EDGE('',*,*,#50682,.T.);
#67912=ORIENTED_EDGE('',*,*,#50683,.T.);
#67913=ORIENTED_EDGE('',*,*,#50192,.F.);
#67914=ORIENTED_EDGE('',*,*,#50685,.F.);
#67915=ORIENTED_EDGE('',*,*,#46390,.F.);
#67916=ORIENTED_EDGE('',*,*,#50684,.T.);
#67917=ORIENTED_EDGE('',*,*,#48125,.F.);
#67918=ORIENTED_EDGE('',*,*,#50686,.F.);
#67919=ORIENTED_EDGE('',*,*,#48791,.F.);
#67920=ORIENTED_EDGE('',*,*,#50685,.T.);
#67921=ORIENTED_EDGE('',*,*,#48786,.F.);
#67922=ORIENTED_EDGE('',*,*,#50687,.F.);
#67923=ORIENTED_EDGE('',*,*,#46391,.F.);
#67924=ORIENTED_EDGE('',*,*,#50686,.T.);
#67925=ORIENTED_EDGE('',*,*,#48137,.F.);
#67926=ORIENTED_EDGE('',*,*,#50688,.F.);
#67927=ORIENTED_EDGE('',*,*,#48792,.F.);
#67928=ORIENTED_EDGE('',*,*,#50687,.T.);
#67929=ORIENTED_EDGE('',*,*,#48785,.F.);
#67930=ORIENTED_EDGE('',*,*,#50689,.F.);
#67931=ORIENTED_EDGE('',*,*,#48133,.F.);
#67932=ORIENTED_EDGE('',*,*,#50688,.T.);
#67933=ORIENTED_EDGE('',*,*,#48121,.F.);
#67934=ORIENTED_EDGE('',*,*,#50690,.F.);
#67935=ORIENTED_EDGE('',*,*,#48793,.F.);
#67936=ORIENTED_EDGE('',*,*,#50689,.T.);
#67937=ORIENTED_EDGE('',*,*,#48796,.F.);
#67938=ORIENTED_EDGE('',*,*,#50691,.F.);
#67939=ORIENTED_EDGE('',*,*,#48112,.F.);
#67940=ORIENTED_EDGE('',*,*,#50690,.T.);
#67941=ORIENTED_EDGE('',*,*,#48139,.F.);
#67942=ORIENTED_EDGE('',*,*,#50692,.F.);
#67943=ORIENTED_EDGE('',*,*,#48794,.F.);
#67944=ORIENTED_EDGE('',*,*,#50691,.T.);
#67945=ORIENTED_EDGE('',*,*,#48795,.F.);
#67946=ORIENTED_EDGE('',*,*,#50692,.T.);
#67947=ORIENTED_EDGE('',*,*,#48117,.F.);
#67948=ORIENTED_EDGE('',*,*,#48113,.T.);
#67949=ORIENTED_EDGE('',*,*,#50693,.F.);
#67950=ORIENTED_EDGE('',*,*,#48835,.F.);
#67951=ORIENTED_EDGE('',*,*,#50694,.F.);
#67952=ORIENTED_EDGE('',*,*,#48069,.F.);
#67953=ORIENTED_EDGE('',*,*,#50694,.T.);
#67954=ORIENTED_EDGE('',*,*,#48834,.F.);
#67955=ORIENTED_EDGE('',*,*,#50695,.F.);
#67956=ORIENTED_EDGE('',*,*,#48078,.F.);
#67957=ORIENTED_EDGE('',*,*,#48068,.T.);
#67958=ORIENTED_EDGE('',*,*,#48072,.F.);
#67959=ORIENTED_EDGE('',*,*,#50696,.F.);
#67960=ORIENTED_EDGE('',*,*,#48836,.F.);
#67961=ORIENTED_EDGE('',*,*,#50693,.T.);
#67962=ORIENTED_EDGE('',*,*,#50695,.T.);
#67963=ORIENTED_EDGE('',*,*,#48833,.F.);
#67964=ORIENTED_EDGE('',*,*,#50697,.F.);
#67965=ORIENTED_EDGE('',*,*,#48063,.F.);
#67966=ORIENTED_EDGE('',*,*,#50696,.T.);
#67967=ORIENTED_EDGE('',*,*,#48076,.F.);
#67968=ORIENTED_EDGE('',*,*,#50698,.F.);
#67969=ORIENTED_EDGE('',*,*,#48825,.F.);
#67970=ORIENTED_EDGE('',*,*,#50697,.T.);
#67971=ORIENTED_EDGE('',*,*,#48832,.F.);
#67972=ORIENTED_EDGE('',*,*,#50699,.F.);
#67973=ORIENTED_EDGE('',*,*,#48080,.F.);
#67974=ORIENTED_EDGE('',*,*,#50698,.T.);
#67975=ORIENTED_EDGE('',*,*,#45991,.F.);
#67976=ORIENTED_EDGE('',*,*,#50700,.F.);
#67977=ORIENTED_EDGE('',*,*,#48826,.F.);
#67978=ORIENTED_EDGE('',*,*,#50699,.T.);
#67979=ORIENTED_EDGE('',*,*,#48831,.F.);
#67980=ORIENTED_EDGE('',*,*,#50701,.F.);
#67981=ORIENTED_EDGE('',*,*,#48055,.T.);
#67982=ORIENTED_EDGE('',*,*,#48059,.F.);
#67983=ORIENTED_EDGE('',*,*,#50700,.T.);
#67984=ORIENTED_EDGE('',*,*,#45990,.F.);
#67985=ORIENTED_EDGE('',*,*,#50702,.F.);
#67986=ORIENTED_EDGE('',*,*,#50193,.F.);
#67987=ORIENTED_EDGE('',*,*,#50701,.T.);
#67988=ORIENTED_EDGE('',*,*,#48830,.F.);
#67989=ORIENTED_EDGE('',*,*,#50703,.F.);
#67990=ORIENTED_EDGE('',*,*,#48056,.F.);
#67991=ORIENTED_EDGE('',*,*,#50702,.T.);
#67992=ORIENTED_EDGE('',*,*,#45989,.F.);
#67993=ORIENTED_EDGE('',*,*,#50704,.F.);
#67994=ORIENTED_EDGE('',*,*,#48810,.F.);
#67995=ORIENTED_EDGE('',*,*,#50703,.T.);
#67996=ORIENTED_EDGE('',*,*,#48829,.F.);
#67997=ORIENTED_EDGE('',*,*,#50705,.F.);
#67998=ORIENTED_EDGE('',*,*,#48074,.F.);
#67999=ORIENTED_EDGE('',*,*,#50704,.T.);
#68000=ORIENTED_EDGE('',*,*,#45988,.F.);
#68001=ORIENTED_EDGE('',*,*,#50706,.F.);
#68002=ORIENTED_EDGE('',*,*,#50195,.F.);
#68003=ORIENTED_EDGE('',*,*,#50705,.T.);
#68004=ORIENTED_EDGE('',*,*,#48828,.F.);
#68005=ORIENTED_EDGE('',*,*,#50707,.F.);
#68006=ORIENTED_EDGE('',*,*,#46381,.F.);
#68007=ORIENTED_EDGE('',*,*,#50706,.T.);
#68008=ORIENTED_EDGE('',*,*,#45987,.F.);
#68009=ORIENTED_EDGE('',*,*,#50708,.F.);
#68010=ORIENTED_EDGE('',*,*,#48816,.F.);
#68011=ORIENTED_EDGE('',*,*,#50707,.T.);
#68012=ORIENTED_EDGE('',*,*,#50194,.F.);
#68013=ORIENTED_EDGE('',*,*,#50709,.F.);
#68014=ORIENTED_EDGE('',*,*,#46382,.F.);
#68015=ORIENTED_EDGE('',*,*,#50708,.T.);
#68016=ORIENTED_EDGE('',*,*,#48105,.F.);
#68017=ORIENTED_EDGE('',*,*,#50710,.F.);
#68018=ORIENTED_EDGE('',*,*,#48817,.F.);
#68019=ORIENTED_EDGE('',*,*,#50709,.T.);
#68020=ORIENTED_EDGE('',*,*,#48812,.F.);
#68021=ORIENTED_EDGE('',*,*,#50711,.F.);
#68022=ORIENTED_EDGE('',*,*,#46383,.F.);
#68023=ORIENTED_EDGE('',*,*,#48100,.F.);
#68024=ORIENTED_EDGE('',*,*,#48096,.T.);
#68025=ORIENTED_EDGE('',*,*,#50712,.F.);
#68026=ORIENTED_EDGE('',*,*,#48818,.F.);
#68027=ORIENTED_EDGE('',*,*,#50710,.T.);
#68028=ORIENTED_EDGE('',*,*,#50711,.T.);
#68029=ORIENTED_EDGE('',*,*,#50196,.F.);
#68030=ORIENTED_EDGE('',*,*,#50713,.F.);
#68031=ORIENTED_EDGE('',*,*,#46384,.F.);
#68032=ORIENTED_EDGE('',*,*,#50712,.T.);
#68033=ORIENTED_EDGE('',*,*,#48095,.F.);
#68034=ORIENTED_EDGE('',*,*,#50714,.F.);
#68035=ORIENTED_EDGE('',*,*,#48819,.F.);
#68036=ORIENTED_EDGE('',*,*,#50713,.T.);
#68037=ORIENTED_EDGE('',*,*,#48814,.F.);
#68038=ORIENTED_EDGE('',*,*,#50715,.F.);
#68039=ORIENTED_EDGE('',*,*,#46385,.F.);
#68040=ORIENTED_EDGE('',*,*,#50714,.T.);
#68041=ORIENTED_EDGE('',*,*,#48107,.F.);
#68042=ORIENTED_EDGE('',*,*,#50716,.F.);
#68043=ORIENTED_EDGE('',*,*,#48820,.F.);
#68044=ORIENTED_EDGE('',*,*,#50715,.T.);
#68045=ORIENTED_EDGE('',*,*,#48813,.F.);
#68046=ORIENTED_EDGE('',*,*,#50717,.F.);
#68047=ORIENTED_EDGE('',*,*,#48103,.F.);
#68048=ORIENTED_EDGE('',*,*,#50716,.T.);
#68049=ORIENTED_EDGE('',*,*,#48091,.F.);
#68050=ORIENTED_EDGE('',*,*,#50718,.F.);
#68051=ORIENTED_EDGE('',*,*,#48821,.F.);
#68052=ORIENTED_EDGE('',*,*,#50717,.T.);
#68053=ORIENTED_EDGE('',*,*,#48824,.F.);
#68054=ORIENTED_EDGE('',*,*,#50719,.F.);
#68055=ORIENTED_EDGE('',*,*,#48082,.F.);
#68056=ORIENTED_EDGE('',*,*,#50718,.T.);
#68057=ORIENTED_EDGE('',*,*,#48109,.F.);
#68058=ORIENTED_EDGE('',*,*,#50720,.F.);
#68059=ORIENTED_EDGE('',*,*,#48822,.F.);
#68060=ORIENTED_EDGE('',*,*,#50719,.T.);
#68061=ORIENTED_EDGE('',*,*,#48823,.F.);
#68062=ORIENTED_EDGE('',*,*,#50720,.T.);
#68063=ORIENTED_EDGE('',*,*,#48087,.F.);
#68064=ORIENTED_EDGE('',*,*,#48083,.T.);
#68065=ORIENTED_EDGE('',*,*,#50721,.F.);
#68066=ORIENTED_EDGE('',*,*,#48863,.F.);
#68067=ORIENTED_EDGE('',*,*,#50722,.F.);
#68068=ORIENTED_EDGE('',*,*,#48039,.F.);
#68069=ORIENTED_EDGE('',*,*,#50722,.T.);
#68070=ORIENTED_EDGE('',*,*,#48862,.F.);
#68071=ORIENTED_EDGE('',*,*,#50723,.F.);
#68072=ORIENTED_EDGE('',*,*,#48048,.F.);
#68073=ORIENTED_EDGE('',*,*,#48038,.T.);
#68074=ORIENTED_EDGE('',*,*,#48042,.F.);
#68075=ORIENTED_EDGE('',*,*,#50724,.F.);
#68076=ORIENTED_EDGE('',*,*,#48864,.F.);
#68077=ORIENTED_EDGE('',*,*,#50721,.T.);
#68078=ORIENTED_EDGE('',*,*,#50723,.T.);
#68079=ORIENTED_EDGE('',*,*,#48861,.F.);
#68080=ORIENTED_EDGE('',*,*,#50725,.F.);
#68081=ORIENTED_EDGE('',*,*,#48033,.F.);
#68082=ORIENTED_EDGE('',*,*,#50724,.T.);
#68083=ORIENTED_EDGE('',*,*,#48046,.F.);
#68084=ORIENTED_EDGE('',*,*,#50726,.F.);
#68085=ORIENTED_EDGE('',*,*,#48853,.F.);
#68086=ORIENTED_EDGE('',*,*,#50725,.T.);
#68087=ORIENTED_EDGE('',*,*,#48860,.F.);
#68088=ORIENTED_EDGE('',*,*,#50727,.F.);
#68089=ORIENTED_EDGE('',*,*,#48050,.F.);
#68090=ORIENTED_EDGE('',*,*,#50726,.T.);
#68091=ORIENTED_EDGE('',*,*,#45997,.F.);
#68092=ORIENTED_EDGE('',*,*,#50728,.F.);
#68093=ORIENTED_EDGE('',*,*,#48854,.F.);
#68094=ORIENTED_EDGE('',*,*,#50727,.T.);
#68095=ORIENTED_EDGE('',*,*,#48859,.F.);
#68096=ORIENTED_EDGE('',*,*,#50729,.F.);
#68097=ORIENTED_EDGE('',*,*,#48025,.T.);
#68098=ORIENTED_EDGE('',*,*,#48029,.F.);
#68099=ORIENTED_EDGE('',*,*,#50728,.T.);
#68100=ORIENTED_EDGE('',*,*,#45996,.F.);
#68101=ORIENTED_EDGE('',*,*,#50730,.F.);
#68102=ORIENTED_EDGE('',*,*,#50197,.F.);
#68103=ORIENTED_EDGE('',*,*,#50729,.T.);
#68104=ORIENTED_EDGE('',*,*,#48858,.F.);
#68105=ORIENTED_EDGE('',*,*,#50731,.F.);
#68106=ORIENTED_EDGE('',*,*,#48026,.F.);
#68107=ORIENTED_EDGE('',*,*,#50730,.T.);
#68108=ORIENTED_EDGE('',*,*,#45995,.F.);
#68109=ORIENTED_EDGE('',*,*,#50732,.F.);
#68110=ORIENTED_EDGE('',*,*,#48838,.F.);
#68111=ORIENTED_EDGE('',*,*,#50731,.T.);
#68112=ORIENTED_EDGE('',*,*,#48857,.F.);
#68113=ORIENTED_EDGE('',*,*,#50733,.F.);
#68114=ORIENTED_EDGE('',*,*,#48044,.F.);
#68115=ORIENTED_EDGE('',*,*,#50732,.T.);
#68116=ORIENTED_EDGE('',*,*,#45994,.F.);
#68117=ORIENTED_EDGE('',*,*,#50734,.F.);
#68118=ORIENTED_EDGE('',*,*,#50199,.F.);
#68119=ORIENTED_EDGE('',*,*,#50733,.T.);
#68120=ORIENTED_EDGE('',*,*,#48856,.F.);
#68121=ORIENTED_EDGE('',*,*,#50735,.F.);
#68122=ORIENTED_EDGE('',*,*,#46375,.F.);
#68123=ORIENTED_EDGE('',*,*,#50734,.T.);
#68124=ORIENTED_EDGE('',*,*,#45993,.F.);
#68125=ORIENTED_EDGE('',*,*,#50736,.F.);
#68126=ORIENTED_EDGE('',*,*,#48844,.F.);
#68127=ORIENTED_EDGE('',*,*,#50735,.T.);
#68128=ORIENTED_EDGE('',*,*,#50198,.F.);
#68129=ORIENTED_EDGE('',*,*,#50737,.F.);
#68130=ORIENTED_EDGE('',*,*,#46376,.F.);
#68131=ORIENTED_EDGE('',*,*,#50736,.T.);
#68132=ORIENTED_EDGE('',*,*,#48075,.F.);
#68133=ORIENTED_EDGE('',*,*,#50738,.F.);
#68134=ORIENTED_EDGE('',*,*,#48845,.F.);
#68135=ORIENTED_EDGE('',*,*,#50737,.T.);
#68136=ORIENTED_EDGE('',*,*,#48840,.F.);
#68137=ORIENTED_EDGE('',*,*,#50739,.F.);
#68138=ORIENTED_EDGE('',*,*,#46377,.F.);
#68139=ORIENTED_EDGE('',*,*,#48070,.F.);
#68140=ORIENTED_EDGE('',*,*,#48066,.T.);
#68141=ORIENTED_EDGE('',*,*,#50740,.F.);
#68142=ORIENTED_EDGE('',*,*,#48846,.F.);
#68143=ORIENTED_EDGE('',*,*,#50738,.T.);
#68144=ORIENTED_EDGE('',*,*,#50739,.T.);
#68145=ORIENTED_EDGE('',*,*,#50200,.F.);
#68146=ORIENTED_EDGE('',*,*,#50741,.F.);
#68147=ORIENTED_EDGE('',*,*,#46378,.F.);
#68148=ORIENTED_EDGE('',*,*,#50740,.T.);
#68149=ORIENTED_EDGE('',*,*,#48065,.F.);
#68150=ORIENTED_EDGE('',*,*,#50742,.F.);
#68151=ORIENTED_EDGE('',*,*,#48847,.F.);
#68152=ORIENTED_EDGE('',*,*,#50741,.T.);
#68153=ORIENTED_EDGE('',*,*,#48842,.F.);
#68154=ORIENTED_EDGE('',*,*,#50743,.F.);
#68155=ORIENTED_EDGE('',*,*,#46379,.F.);
#68156=ORIENTED_EDGE('',*,*,#50742,.T.);
#68157=ORIENTED_EDGE('',*,*,#48077,.F.);
#68158=ORIENTED_EDGE('',*,*,#50744,.F.);
#68159=ORIENTED_EDGE('',*,*,#48848,.F.);
#68160=ORIENTED_EDGE('',*,*,#50743,.T.);
#68161=ORIENTED_EDGE('',*,*,#48841,.F.);
#68162=ORIENTED_EDGE('',*,*,#50745,.F.);
#68163=ORIENTED_EDGE('',*,*,#48073,.F.);
#68164=ORIENTED_EDGE('',*,*,#50744,.T.);
#68165=ORIENTED_EDGE('',*,*,#48061,.F.);
#68166=ORIENTED_EDGE('',*,*,#50746,.F.);
#68167=ORIENTED_EDGE('',*,*,#48849,.F.);
#68168=ORIENTED_EDGE('',*,*,#50745,.T.);
#68169=ORIENTED_EDGE('',*,*,#48852,.F.);
#68170=ORIENTED_EDGE('',*,*,#50747,.F.);
#68171=ORIENTED_EDGE('',*,*,#48052,.F.);
#68172=ORIENTED_EDGE('',*,*,#50746,.T.);
#68173=ORIENTED_EDGE('',*,*,#48079,.F.);
#68174=ORIENTED_EDGE('',*,*,#50748,.F.);
#68175=ORIENTED_EDGE('',*,*,#48850,.F.);
#68176=ORIENTED_EDGE('',*,*,#50747,.T.);
#68177=ORIENTED_EDGE('',*,*,#48851,.F.);
#68178=ORIENTED_EDGE('',*,*,#50748,.T.);
#68179=ORIENTED_EDGE('',*,*,#48057,.F.);
#68180=ORIENTED_EDGE('',*,*,#48053,.T.);
#68181=ORIENTED_EDGE('',*,*,#50749,.F.);
#68182=ORIENTED_EDGE('',*,*,#48891,.F.);
#68183=ORIENTED_EDGE('',*,*,#50750,.F.);
#68184=ORIENTED_EDGE('',*,*,#48009,.F.);
#68185=ORIENTED_EDGE('',*,*,#50750,.T.);
#68186=ORIENTED_EDGE('',*,*,#48890,.F.);
#68187=ORIENTED_EDGE('',*,*,#50751,.F.);
#68188=ORIENTED_EDGE('',*,*,#48018,.F.);
#68189=ORIENTED_EDGE('',*,*,#48008,.T.);
#68190=ORIENTED_EDGE('',*,*,#48012,.F.);
#68191=ORIENTED_EDGE('',*,*,#50752,.F.);
#68192=ORIENTED_EDGE('',*,*,#48892,.F.);
#68193=ORIENTED_EDGE('',*,*,#50749,.T.);
#68194=ORIENTED_EDGE('',*,*,#50751,.T.);
#68195=ORIENTED_EDGE('',*,*,#48889,.F.);
#68196=ORIENTED_EDGE('',*,*,#50753,.F.);
#68197=ORIENTED_EDGE('',*,*,#48003,.F.);
#68198=ORIENTED_EDGE('',*,*,#50752,.T.);
#68199=ORIENTED_EDGE('',*,*,#48016,.F.);
#68200=ORIENTED_EDGE('',*,*,#50754,.F.);
#68201=ORIENTED_EDGE('',*,*,#48881,.F.);
#68202=ORIENTED_EDGE('',*,*,#50753,.T.);
#68203=ORIENTED_EDGE('',*,*,#48888,.F.);
#68204=ORIENTED_EDGE('',*,*,#50755,.F.);
#68205=ORIENTED_EDGE('',*,*,#48020,.F.);
#68206=ORIENTED_EDGE('',*,*,#50754,.T.);
#68207=ORIENTED_EDGE('',*,*,#46003,.F.);
#68208=ORIENTED_EDGE('',*,*,#50756,.F.);
#68209=ORIENTED_EDGE('',*,*,#48882,.F.);
#68210=ORIENTED_EDGE('',*,*,#50755,.T.);
#68211=ORIENTED_EDGE('',*,*,#48887,.F.);
#68212=ORIENTED_EDGE('',*,*,#50757,.F.);
#68213=ORIENTED_EDGE('',*,*,#47995,.T.);
#68214=ORIENTED_EDGE('',*,*,#47999,.F.);
#68215=ORIENTED_EDGE('',*,*,#50756,.T.);
#68216=ORIENTED_EDGE('',*,*,#46002,.F.);
#68217=ORIENTED_EDGE('',*,*,#50758,.F.);
#68218=ORIENTED_EDGE('',*,*,#50201,.F.);
#68219=ORIENTED_EDGE('',*,*,#50757,.T.);
#68220=ORIENTED_EDGE('',*,*,#48886,.F.);
#68221=ORIENTED_EDGE('',*,*,#50759,.F.);
#68222=ORIENTED_EDGE('',*,*,#47996,.F.);
#68223=ORIENTED_EDGE('',*,*,#50758,.T.);
#68224=ORIENTED_EDGE('',*,*,#46001,.F.);
#68225=ORIENTED_EDGE('',*,*,#50760,.F.);
#68226=ORIENTED_EDGE('',*,*,#48866,.F.);
#68227=ORIENTED_EDGE('',*,*,#50759,.T.);
#68228=ORIENTED_EDGE('',*,*,#48885,.F.);
#68229=ORIENTED_EDGE('',*,*,#50761,.F.);
#68230=ORIENTED_EDGE('',*,*,#48014,.F.);
#68231=ORIENTED_EDGE('',*,*,#50760,.T.);
#68232=ORIENTED_EDGE('',*,*,#46000,.F.);
#68233=ORIENTED_EDGE('',*,*,#50762,.F.);
#68234=ORIENTED_EDGE('',*,*,#50203,.F.);
#68235=ORIENTED_EDGE('',*,*,#50761,.T.);
#68236=ORIENTED_EDGE('',*,*,#48884,.F.);
#68237=ORIENTED_EDGE('',*,*,#50763,.F.);
#68238=ORIENTED_EDGE('',*,*,#46369,.F.);
#68239=ORIENTED_EDGE('',*,*,#50762,.T.);
#68240=ORIENTED_EDGE('',*,*,#45999,.F.);
#68241=ORIENTED_EDGE('',*,*,#50764,.F.);
#68242=ORIENTED_EDGE('',*,*,#48872,.F.);
#68243=ORIENTED_EDGE('',*,*,#50763,.T.);
#68244=ORIENTED_EDGE('',*,*,#50202,.F.);
#68245=ORIENTED_EDGE('',*,*,#50765,.F.);
#68246=ORIENTED_EDGE('',*,*,#46370,.F.);
#68247=ORIENTED_EDGE('',*,*,#50764,.T.);
#68248=ORIENTED_EDGE('',*,*,#48045,.F.);
#68249=ORIENTED_EDGE('',*,*,#50766,.F.);
#68250=ORIENTED_EDGE('',*,*,#48873,.F.);
#68251=ORIENTED_EDGE('',*,*,#50765,.T.);
#68252=ORIENTED_EDGE('',*,*,#48868,.F.);
#68253=ORIENTED_EDGE('',*,*,#50767,.F.);
#68254=ORIENTED_EDGE('',*,*,#46371,.F.);
#68255=ORIENTED_EDGE('',*,*,#48040,.F.);
#68256=ORIENTED_EDGE('',*,*,#48036,.T.);
#68257=ORIENTED_EDGE('',*,*,#50768,.F.);
#68258=ORIENTED_EDGE('',*,*,#48874,.F.);
#68259=ORIENTED_EDGE('',*,*,#50766,.T.);
#68260=ORIENTED_EDGE('',*,*,#50767,.T.);
#68261=ORIENTED_EDGE('',*,*,#50204,.F.);
#68262=ORIENTED_EDGE('',*,*,#50769,.F.);
#68263=ORIENTED_EDGE('',*,*,#46372,.F.);
#68264=ORIENTED_EDGE('',*,*,#50768,.T.);
#68265=ORIENTED_EDGE('',*,*,#48035,.F.);
#68266=ORIENTED_EDGE('',*,*,#50770,.F.);
#68267=ORIENTED_EDGE('',*,*,#48875,.F.);
#68268=ORIENTED_EDGE('',*,*,#50769,.T.);
#68269=ORIENTED_EDGE('',*,*,#48870,.F.);
#68270=ORIENTED_EDGE('',*,*,#50771,.F.);
#68271=ORIENTED_EDGE('',*,*,#46373,.F.);
#68272=ORIENTED_EDGE('',*,*,#50770,.T.);
#68273=ORIENTED_EDGE('',*,*,#48047,.F.);
#68274=ORIENTED_EDGE('',*,*,#50772,.F.);
#68275=ORIENTED_EDGE('',*,*,#48876,.F.);
#68276=ORIENTED_EDGE('',*,*,#50771,.T.);
#68277=ORIENTED_EDGE('',*,*,#48869,.F.);
#68278=ORIENTED_EDGE('',*,*,#50773,.F.);
#68279=ORIENTED_EDGE('',*,*,#48043,.F.);
#68280=ORIENTED_EDGE('',*,*,#50772,.T.);
#68281=ORIENTED_EDGE('',*,*,#48031,.F.);
#68282=ORIENTED_EDGE('',*,*,#50774,.F.);
#68283=ORIENTED_EDGE('',*,*,#48877,.F.);
#68284=ORIENTED_EDGE('',*,*,#50773,.T.);
#68285=ORIENTED_EDGE('',*,*,#48880,.F.);
#68286=ORIENTED_EDGE('',*,*,#50775,.F.);
#68287=ORIENTED_EDGE('',*,*,#48022,.F.);
#68288=ORIENTED_EDGE('',*,*,#50774,.T.);
#68289=ORIENTED_EDGE('',*,*,#48049,.F.);
#68290=ORIENTED_EDGE('',*,*,#50776,.F.);
#68291=ORIENTED_EDGE('',*,*,#48878,.F.);
#68292=ORIENTED_EDGE('',*,*,#50775,.T.);
#68293=ORIENTED_EDGE('',*,*,#48879,.F.);
#68294=ORIENTED_EDGE('',*,*,#50776,.T.);
#68295=ORIENTED_EDGE('',*,*,#48027,.F.);
#68296=ORIENTED_EDGE('',*,*,#48023,.T.);
#68297=ORIENTED_EDGE('',*,*,#50777,.F.);
#68298=ORIENTED_EDGE('',*,*,#48919,.F.);
#68299=ORIENTED_EDGE('',*,*,#50778,.F.);
#68300=ORIENTED_EDGE('',*,*,#47979,.F.);
#68301=ORIENTED_EDGE('',*,*,#50778,.T.);
#68302=ORIENTED_EDGE('',*,*,#48918,.F.);
#68303=ORIENTED_EDGE('',*,*,#50779,.F.);
#68304=ORIENTED_EDGE('',*,*,#47988,.F.);
#68305=ORIENTED_EDGE('',*,*,#47978,.T.);
#68306=ORIENTED_EDGE('',*,*,#47982,.F.);
#68307=ORIENTED_EDGE('',*,*,#50780,.F.);
#68308=ORIENTED_EDGE('',*,*,#48920,.F.);
#68309=ORIENTED_EDGE('',*,*,#50777,.T.);
#68310=ORIENTED_EDGE('',*,*,#50779,.T.);
#68311=ORIENTED_EDGE('',*,*,#48917,.F.);
#68312=ORIENTED_EDGE('',*,*,#50781,.F.);
#68313=ORIENTED_EDGE('',*,*,#47973,.F.);
#68314=ORIENTED_EDGE('',*,*,#50780,.T.);
#68315=ORIENTED_EDGE('',*,*,#47986,.F.);
#68316=ORIENTED_EDGE('',*,*,#50782,.F.);
#68317=ORIENTED_EDGE('',*,*,#48909,.F.);
#68318=ORIENTED_EDGE('',*,*,#50781,.T.);
#68319=ORIENTED_EDGE('',*,*,#48916,.F.);
#68320=ORIENTED_EDGE('',*,*,#50783,.F.);
#68321=ORIENTED_EDGE('',*,*,#47990,.F.);
#68322=ORIENTED_EDGE('',*,*,#50782,.T.);
#68323=ORIENTED_EDGE('',*,*,#46009,.F.);
#68324=ORIENTED_EDGE('',*,*,#50784,.F.);
#68325=ORIENTED_EDGE('',*,*,#48910,.F.);
#68326=ORIENTED_EDGE('',*,*,#50783,.T.);
#68327=ORIENTED_EDGE('',*,*,#48915,.F.);
#68328=ORIENTED_EDGE('',*,*,#50785,.F.);
#68329=ORIENTED_EDGE('',*,*,#47965,.T.);
#68330=ORIENTED_EDGE('',*,*,#47969,.F.);
#68331=ORIENTED_EDGE('',*,*,#50784,.T.);
#68332=ORIENTED_EDGE('',*,*,#46008,.F.);
#68333=ORIENTED_EDGE('',*,*,#50786,.F.);
#68334=ORIENTED_EDGE('',*,*,#50205,.F.);
#68335=ORIENTED_EDGE('',*,*,#50785,.T.);
#68336=ORIENTED_EDGE('',*,*,#48914,.F.);
#68337=ORIENTED_EDGE('',*,*,#50787,.F.);
#68338=ORIENTED_EDGE('',*,*,#47966,.F.);
#68339=ORIENTED_EDGE('',*,*,#50786,.T.);
#68340=ORIENTED_EDGE('',*,*,#46007,.F.);
#68341=ORIENTED_EDGE('',*,*,#50788,.F.);
#68342=ORIENTED_EDGE('',*,*,#48894,.F.);
#68343=ORIENTED_EDGE('',*,*,#50787,.T.);
#68344=ORIENTED_EDGE('',*,*,#48913,.F.);
#68345=ORIENTED_EDGE('',*,*,#50789,.F.);
#68346=ORIENTED_EDGE('',*,*,#47984,.F.);
#68347=ORIENTED_EDGE('',*,*,#50788,.T.);
#68348=ORIENTED_EDGE('',*,*,#46006,.F.);
#68349=ORIENTED_EDGE('',*,*,#50790,.F.);
#68350=ORIENTED_EDGE('',*,*,#50207,.F.);
#68351=ORIENTED_EDGE('',*,*,#50789,.T.);
#68352=ORIENTED_EDGE('',*,*,#48912,.F.);
#68353=ORIENTED_EDGE('',*,*,#50791,.F.);
#68354=ORIENTED_EDGE('',*,*,#46363,.F.);
#68355=ORIENTED_EDGE('',*,*,#50790,.T.);
#68356=ORIENTED_EDGE('',*,*,#46005,.F.);
#68357=ORIENTED_EDGE('',*,*,#50792,.F.);
#68358=ORIENTED_EDGE('',*,*,#48900,.F.);
#68359=ORIENTED_EDGE('',*,*,#50791,.T.);
#68360=ORIENTED_EDGE('',*,*,#50206,.F.);
#68361=ORIENTED_EDGE('',*,*,#50793,.F.);
#68362=ORIENTED_EDGE('',*,*,#46364,.F.);
#68363=ORIENTED_EDGE('',*,*,#50792,.T.);
#68364=ORIENTED_EDGE('',*,*,#48015,.F.);
#68365=ORIENTED_EDGE('',*,*,#50794,.F.);
#68366=ORIENTED_EDGE('',*,*,#48901,.F.);
#68367=ORIENTED_EDGE('',*,*,#50793,.T.);
#68368=ORIENTED_EDGE('',*,*,#48896,.F.);
#68369=ORIENTED_EDGE('',*,*,#50795,.F.);
#68370=ORIENTED_EDGE('',*,*,#46365,.F.);
#68371=ORIENTED_EDGE('',*,*,#48010,.F.);
#68372=ORIENTED_EDGE('',*,*,#48006,.T.);
#68373=ORIENTED_EDGE('',*,*,#50796,.F.);
#68374=ORIENTED_EDGE('',*,*,#48902,.F.);
#68375=ORIENTED_EDGE('',*,*,#50794,.T.);
#68376=ORIENTED_EDGE('',*,*,#50795,.T.);
#68377=ORIENTED_EDGE('',*,*,#50208,.F.);
#68378=ORIENTED_EDGE('',*,*,#50797,.F.);
#68379=ORIENTED_EDGE('',*,*,#46366,.F.);
#68380=ORIENTED_EDGE('',*,*,#50796,.T.);
#68381=ORIENTED_EDGE('',*,*,#48005,.F.);
#68382=ORIENTED_EDGE('',*,*,#50798,.F.);
#68383=ORIENTED_EDGE('',*,*,#48903,.F.);
#68384=ORIENTED_EDGE('',*,*,#50797,.T.);
#68385=ORIENTED_EDGE('',*,*,#48898,.F.);
#68386=ORIENTED_EDGE('',*,*,#50799,.F.);
#68387=ORIENTED_EDGE('',*,*,#46367,.F.);
#68388=ORIENTED_EDGE('',*,*,#50798,.T.);
#68389=ORIENTED_EDGE('',*,*,#48017,.F.);
#68390=ORIENTED_EDGE('',*,*,#50800,.F.);
#68391=ORIENTED_EDGE('',*,*,#48904,.F.);
#68392=ORIENTED_EDGE('',*,*,#50799,.T.);
#68393=ORIENTED_EDGE('',*,*,#48897,.F.);
#68394=ORIENTED_EDGE('',*,*,#50801,.F.);
#68395=ORIENTED_EDGE('',*,*,#48013,.F.);
#68396=ORIENTED_EDGE('',*,*,#50800,.T.);
#68397=ORIENTED_EDGE('',*,*,#48001,.F.);
#68398=ORIENTED_EDGE('',*,*,#50802,.F.);
#68399=ORIENTED_EDGE('',*,*,#48905,.F.);
#68400=ORIENTED_EDGE('',*,*,#50801,.T.);
#68401=ORIENTED_EDGE('',*,*,#48908,.F.);
#68402=ORIENTED_EDGE('',*,*,#50803,.F.);
#68403=ORIENTED_EDGE('',*,*,#47992,.F.);
#68404=ORIENTED_EDGE('',*,*,#50802,.T.);
#68405=ORIENTED_EDGE('',*,*,#48019,.F.);
#68406=ORIENTED_EDGE('',*,*,#50804,.F.);
#68407=ORIENTED_EDGE('',*,*,#48906,.F.);
#68408=ORIENTED_EDGE('',*,*,#50803,.T.);
#68409=ORIENTED_EDGE('',*,*,#48907,.F.);
#68410=ORIENTED_EDGE('',*,*,#50804,.T.);
#68411=ORIENTED_EDGE('',*,*,#47997,.F.);
#68412=ORIENTED_EDGE('',*,*,#47993,.T.);
#68413=ORIENTED_EDGE('',*,*,#50805,.F.);
#68414=ORIENTED_EDGE('',*,*,#48947,.F.);
#68415=ORIENTED_EDGE('',*,*,#50806,.F.);
#68416=ORIENTED_EDGE('',*,*,#47949,.F.);
#68417=ORIENTED_EDGE('',*,*,#50806,.T.);
#68418=ORIENTED_EDGE('',*,*,#48946,.F.);
#68419=ORIENTED_EDGE('',*,*,#50807,.F.);
#68420=ORIENTED_EDGE('',*,*,#47958,.F.);
#68421=ORIENTED_EDGE('',*,*,#47948,.T.);
#68422=ORIENTED_EDGE('',*,*,#47952,.F.);
#68423=ORIENTED_EDGE('',*,*,#50808,.F.);
#68424=ORIENTED_EDGE('',*,*,#48948,.F.);
#68425=ORIENTED_EDGE('',*,*,#50805,.T.);
#68426=ORIENTED_EDGE('',*,*,#50807,.T.);
#68427=ORIENTED_EDGE('',*,*,#48945,.F.);
#68428=ORIENTED_EDGE('',*,*,#50809,.F.);
#68429=ORIENTED_EDGE('',*,*,#47943,.F.);
#68430=ORIENTED_EDGE('',*,*,#50808,.T.);
#68431=ORIENTED_EDGE('',*,*,#47956,.F.);
#68432=ORIENTED_EDGE('',*,*,#50810,.F.);
#68433=ORIENTED_EDGE('',*,*,#48937,.F.);
#68434=ORIENTED_EDGE('',*,*,#50809,.T.);
#68435=ORIENTED_EDGE('',*,*,#48944,.F.);
#68436=ORIENTED_EDGE('',*,*,#50811,.F.);
#68437=ORIENTED_EDGE('',*,*,#47960,.F.);
#68438=ORIENTED_EDGE('',*,*,#50810,.T.);
#68439=ORIENTED_EDGE('',*,*,#46015,.F.);
#68440=ORIENTED_EDGE('',*,*,#50812,.F.);
#68441=ORIENTED_EDGE('',*,*,#48938,.F.);
#68442=ORIENTED_EDGE('',*,*,#50811,.T.);
#68443=ORIENTED_EDGE('',*,*,#48943,.F.);
#68444=ORIENTED_EDGE('',*,*,#50813,.F.);
#68445=ORIENTED_EDGE('',*,*,#47935,.T.);
#68446=ORIENTED_EDGE('',*,*,#47939,.F.);
#68447=ORIENTED_EDGE('',*,*,#50812,.T.);
#68448=ORIENTED_EDGE('',*,*,#46014,.F.);
#68449=ORIENTED_EDGE('',*,*,#50814,.F.);
#68450=ORIENTED_EDGE('',*,*,#50209,.F.);
#68451=ORIENTED_EDGE('',*,*,#50813,.T.);
#68452=ORIENTED_EDGE('',*,*,#48942,.F.);
#68453=ORIENTED_EDGE('',*,*,#50815,.F.);
#68454=ORIENTED_EDGE('',*,*,#47936,.F.);
#68455=ORIENTED_EDGE('',*,*,#50814,.T.);
#68456=ORIENTED_EDGE('',*,*,#46013,.F.);
#68457=ORIENTED_EDGE('',*,*,#50816,.F.);
#68458=ORIENTED_EDGE('',*,*,#48922,.F.);
#68459=ORIENTED_EDGE('',*,*,#50815,.T.);
#68460=ORIENTED_EDGE('',*,*,#48941,.F.);
#68461=ORIENTED_EDGE('',*,*,#50817,.F.);
#68462=ORIENTED_EDGE('',*,*,#47954,.F.);
#68463=ORIENTED_EDGE('',*,*,#50816,.T.);
#68464=ORIENTED_EDGE('',*,*,#46012,.F.);
#68465=ORIENTED_EDGE('',*,*,#50818,.F.);
#68466=ORIENTED_EDGE('',*,*,#50211,.F.);
#68467=ORIENTED_EDGE('',*,*,#50817,.T.);
#68468=ORIENTED_EDGE('',*,*,#48940,.F.);
#68469=ORIENTED_EDGE('',*,*,#50819,.F.);
#68470=ORIENTED_EDGE('',*,*,#46357,.F.);
#68471=ORIENTED_EDGE('',*,*,#50818,.T.);
#68472=ORIENTED_EDGE('',*,*,#46011,.F.);
#68473=ORIENTED_EDGE('',*,*,#50820,.F.);
#68474=ORIENTED_EDGE('',*,*,#48928,.F.);
#68475=ORIENTED_EDGE('',*,*,#50819,.T.);
#68476=ORIENTED_EDGE('',*,*,#50210,.F.);
#68477=ORIENTED_EDGE('',*,*,#50821,.F.);
#68478=ORIENTED_EDGE('',*,*,#46358,.F.);
#68479=ORIENTED_EDGE('',*,*,#50820,.T.);
#68480=ORIENTED_EDGE('',*,*,#47985,.F.);
#68481=ORIENTED_EDGE('',*,*,#50822,.F.);
#68482=ORIENTED_EDGE('',*,*,#48929,.F.);
#68483=ORIENTED_EDGE('',*,*,#50821,.T.);
#68484=ORIENTED_EDGE('',*,*,#48924,.F.);
#68485=ORIENTED_EDGE('',*,*,#50823,.F.);
#68486=ORIENTED_EDGE('',*,*,#46359,.F.);
#68487=ORIENTED_EDGE('',*,*,#47980,.F.);
#68488=ORIENTED_EDGE('',*,*,#47976,.T.);
#68489=ORIENTED_EDGE('',*,*,#50824,.F.);
#68490=ORIENTED_EDGE('',*,*,#48930,.F.);
#68491=ORIENTED_EDGE('',*,*,#50822,.T.);
#68492=ORIENTED_EDGE('',*,*,#50823,.T.);
#68493=ORIENTED_EDGE('',*,*,#50212,.F.);
#68494=ORIENTED_EDGE('',*,*,#50825,.F.);
#68495=ORIENTED_EDGE('',*,*,#46360,.F.);
#68496=ORIENTED_EDGE('',*,*,#50824,.T.);
#68497=ORIENTED_EDGE('',*,*,#47975,.F.);
#68498=ORIENTED_EDGE('',*,*,#50826,.F.);
#68499=ORIENTED_EDGE('',*,*,#48931,.F.);
#68500=ORIENTED_EDGE('',*,*,#50825,.T.);
#68501=ORIENTED_EDGE('',*,*,#48926,.F.);
#68502=ORIENTED_EDGE('',*,*,#50827,.F.);
#68503=ORIENTED_EDGE('',*,*,#46361,.F.);
#68504=ORIENTED_EDGE('',*,*,#50826,.T.);
#68505=ORIENTED_EDGE('',*,*,#47987,.F.);
#68506=ORIENTED_EDGE('',*,*,#50828,.F.);
#68507=ORIENTED_EDGE('',*,*,#48932,.F.);
#68508=ORIENTED_EDGE('',*,*,#50827,.T.);
#68509=ORIENTED_EDGE('',*,*,#48925,.F.);
#68510=ORIENTED_EDGE('',*,*,#50829,.F.);
#68511=ORIENTED_EDGE('',*,*,#47983,.F.);
#68512=ORIENTED_EDGE('',*,*,#50828,.T.);
#68513=ORIENTED_EDGE('',*,*,#47971,.F.);
#68514=ORIENTED_EDGE('',*,*,#50830,.F.);
#68515=ORIENTED_EDGE('',*,*,#48933,.F.);
#68516=ORIENTED_EDGE('',*,*,#50829,.T.);
#68517=ORIENTED_EDGE('',*,*,#48936,.F.);
#68518=ORIENTED_EDGE('',*,*,#50831,.F.);
#68519=ORIENTED_EDGE('',*,*,#47962,.F.);
#68520=ORIENTED_EDGE('',*,*,#50830,.T.);
#68521=ORIENTED_EDGE('',*,*,#47989,.F.);
#68522=ORIENTED_EDGE('',*,*,#50832,.F.);
#68523=ORIENTED_EDGE('',*,*,#48934,.F.);
#68524=ORIENTED_EDGE('',*,*,#50831,.T.);
#68525=ORIENTED_EDGE('',*,*,#48935,.F.);
#68526=ORIENTED_EDGE('',*,*,#50832,.T.);
#68527=ORIENTED_EDGE('',*,*,#47967,.F.);
#68528=ORIENTED_EDGE('',*,*,#47963,.T.);
#68529=ORIENTED_EDGE('',*,*,#50833,.F.);
#68530=ORIENTED_EDGE('',*,*,#48975,.F.);
#68531=ORIENTED_EDGE('',*,*,#50834,.F.);
#68532=ORIENTED_EDGE('',*,*,#47919,.F.);
#68533=ORIENTED_EDGE('',*,*,#50834,.T.);
#68534=ORIENTED_EDGE('',*,*,#48974,.F.);
#68535=ORIENTED_EDGE('',*,*,#50835,.F.);
#68536=ORIENTED_EDGE('',*,*,#47928,.F.);
#68537=ORIENTED_EDGE('',*,*,#47918,.T.);
#68538=ORIENTED_EDGE('',*,*,#47922,.F.);
#68539=ORIENTED_EDGE('',*,*,#50836,.F.);
#68540=ORIENTED_EDGE('',*,*,#48976,.F.);
#68541=ORIENTED_EDGE('',*,*,#50833,.T.);
#68542=ORIENTED_EDGE('',*,*,#50835,.T.);
#68543=ORIENTED_EDGE('',*,*,#48973,.F.);
#68544=ORIENTED_EDGE('',*,*,#50837,.F.);
#68545=ORIENTED_EDGE('',*,*,#47913,.F.);
#68546=ORIENTED_EDGE('',*,*,#50836,.T.);
#68547=ORIENTED_EDGE('',*,*,#47926,.F.);
#68548=ORIENTED_EDGE('',*,*,#50838,.F.);
#68549=ORIENTED_EDGE('',*,*,#48965,.F.);
#68550=ORIENTED_EDGE('',*,*,#50837,.T.);
#68551=ORIENTED_EDGE('',*,*,#48972,.F.);
#68552=ORIENTED_EDGE('',*,*,#50839,.F.);
#68553=ORIENTED_EDGE('',*,*,#47930,.F.);
#68554=ORIENTED_EDGE('',*,*,#50838,.T.);
#68555=ORIENTED_EDGE('',*,*,#46021,.F.);
#68556=ORIENTED_EDGE('',*,*,#50840,.F.);
#68557=ORIENTED_EDGE('',*,*,#48966,.F.);
#68558=ORIENTED_EDGE('',*,*,#50839,.T.);
#68559=ORIENTED_EDGE('',*,*,#48971,.F.);
#68560=ORIENTED_EDGE('',*,*,#50841,.F.);
#68561=ORIENTED_EDGE('',*,*,#47905,.T.);
#68562=ORIENTED_EDGE('',*,*,#47909,.F.);
#68563=ORIENTED_EDGE('',*,*,#50840,.T.);
#68564=ORIENTED_EDGE('',*,*,#46020,.F.);
#68565=ORIENTED_EDGE('',*,*,#50842,.F.);
#68566=ORIENTED_EDGE('',*,*,#50213,.F.);
#68567=ORIENTED_EDGE('',*,*,#50841,.T.);
#68568=ORIENTED_EDGE('',*,*,#48970,.F.);
#68569=ORIENTED_EDGE('',*,*,#50843,.F.);
#68570=ORIENTED_EDGE('',*,*,#47906,.F.);
#68571=ORIENTED_EDGE('',*,*,#50842,.T.);
#68572=ORIENTED_EDGE('',*,*,#46019,.F.);
#68573=ORIENTED_EDGE('',*,*,#50844,.F.);
#68574=ORIENTED_EDGE('',*,*,#48950,.F.);
#68575=ORIENTED_EDGE('',*,*,#50843,.T.);
#68576=ORIENTED_EDGE('',*,*,#48969,.F.);
#68577=ORIENTED_EDGE('',*,*,#50845,.F.);
#68578=ORIENTED_EDGE('',*,*,#47924,.F.);
#68579=ORIENTED_EDGE('',*,*,#50844,.T.);
#68580=ORIENTED_EDGE('',*,*,#46018,.F.);
#68581=ORIENTED_EDGE('',*,*,#50846,.F.);
#68582=ORIENTED_EDGE('',*,*,#50215,.F.);
#68583=ORIENTED_EDGE('',*,*,#50845,.T.);
#68584=ORIENTED_EDGE('',*,*,#48968,.F.);
#68585=ORIENTED_EDGE('',*,*,#50847,.F.);
#68586=ORIENTED_EDGE('',*,*,#46351,.F.);
#68587=ORIENTED_EDGE('',*,*,#50846,.T.);
#68588=ORIENTED_EDGE('',*,*,#46017,.F.);
#68589=ORIENTED_EDGE('',*,*,#50848,.F.);
#68590=ORIENTED_EDGE('',*,*,#48956,.F.);
#68591=ORIENTED_EDGE('',*,*,#50847,.T.);
#68592=ORIENTED_EDGE('',*,*,#50214,.F.);
#68593=ORIENTED_EDGE('',*,*,#50849,.F.);
#68594=ORIENTED_EDGE('',*,*,#46352,.F.);
#68595=ORIENTED_EDGE('',*,*,#50848,.T.);
#68596=ORIENTED_EDGE('',*,*,#47955,.F.);
#68597=ORIENTED_EDGE('',*,*,#50850,.F.);
#68598=ORIENTED_EDGE('',*,*,#48957,.F.);
#68599=ORIENTED_EDGE('',*,*,#50849,.T.);
#68600=ORIENTED_EDGE('',*,*,#48952,.F.);
#68601=ORIENTED_EDGE('',*,*,#50851,.F.);
#68602=ORIENTED_EDGE('',*,*,#46353,.F.);
#68603=ORIENTED_EDGE('',*,*,#47950,.F.);
#68604=ORIENTED_EDGE('',*,*,#47946,.T.);
#68605=ORIENTED_EDGE('',*,*,#50852,.F.);
#68606=ORIENTED_EDGE('',*,*,#48958,.F.);
#68607=ORIENTED_EDGE('',*,*,#50850,.T.);
#68608=ORIENTED_EDGE('',*,*,#50851,.T.);
#68609=ORIENTED_EDGE('',*,*,#50216,.F.);
#68610=ORIENTED_EDGE('',*,*,#50853,.F.);
#68611=ORIENTED_EDGE('',*,*,#46354,.F.);
#68612=ORIENTED_EDGE('',*,*,#50852,.T.);
#68613=ORIENTED_EDGE('',*,*,#47945,.F.);
#68614=ORIENTED_EDGE('',*,*,#50854,.F.);
#68615=ORIENTED_EDGE('',*,*,#48959,.F.);
#68616=ORIENTED_EDGE('',*,*,#50853,.T.);
#68617=ORIENTED_EDGE('',*,*,#48954,.F.);
#68618=ORIENTED_EDGE('',*,*,#50855,.F.);
#68619=ORIENTED_EDGE('',*,*,#46355,.F.);
#68620=ORIENTED_EDGE('',*,*,#50854,.T.);
#68621=ORIENTED_EDGE('',*,*,#47957,.F.);
#68622=ORIENTED_EDGE('',*,*,#50856,.F.);
#68623=ORIENTED_EDGE('',*,*,#48960,.F.);
#68624=ORIENTED_EDGE('',*,*,#50855,.T.);
#68625=ORIENTED_EDGE('',*,*,#48953,.F.);
#68626=ORIENTED_EDGE('',*,*,#50857,.F.);
#68627=ORIENTED_EDGE('',*,*,#47953,.F.);
#68628=ORIENTED_EDGE('',*,*,#50856,.T.);
#68629=ORIENTED_EDGE('',*,*,#47941,.F.);
#68630=ORIENTED_EDGE('',*,*,#50858,.F.);
#68631=ORIENTED_EDGE('',*,*,#48961,.F.);
#68632=ORIENTED_EDGE('',*,*,#50857,.T.);
#68633=ORIENTED_EDGE('',*,*,#48964,.F.);
#68634=ORIENTED_EDGE('',*,*,#50859,.F.);
#68635=ORIENTED_EDGE('',*,*,#47932,.F.);
#68636=ORIENTED_EDGE('',*,*,#50858,.T.);
#68637=ORIENTED_EDGE('',*,*,#47959,.F.);
#68638=ORIENTED_EDGE('',*,*,#50860,.F.);
#68639=ORIENTED_EDGE('',*,*,#48962,.F.);
#68640=ORIENTED_EDGE('',*,*,#50859,.T.);
#68641=ORIENTED_EDGE('',*,*,#48963,.F.);
#68642=ORIENTED_EDGE('',*,*,#50860,.T.);
#68643=ORIENTED_EDGE('',*,*,#47937,.F.);
#68644=ORIENTED_EDGE('',*,*,#47933,.T.);
#68645=ORIENTED_EDGE('',*,*,#50861,.F.);
#68646=ORIENTED_EDGE('',*,*,#49003,.F.);
#68647=ORIENTED_EDGE('',*,*,#50862,.F.);
#68648=ORIENTED_EDGE('',*,*,#47889,.F.);
#68649=ORIENTED_EDGE('',*,*,#50862,.T.);
#68650=ORIENTED_EDGE('',*,*,#49002,.F.);
#68651=ORIENTED_EDGE('',*,*,#50863,.F.);
#68652=ORIENTED_EDGE('',*,*,#47898,.F.);
#68653=ORIENTED_EDGE('',*,*,#47888,.T.);
#68654=ORIENTED_EDGE('',*,*,#47892,.F.);
#68655=ORIENTED_EDGE('',*,*,#50864,.F.);
#68656=ORIENTED_EDGE('',*,*,#49004,.F.);
#68657=ORIENTED_EDGE('',*,*,#50861,.T.);
#68658=ORIENTED_EDGE('',*,*,#50863,.T.);
#68659=ORIENTED_EDGE('',*,*,#49001,.F.);
#68660=ORIENTED_EDGE('',*,*,#50865,.F.);
#68661=ORIENTED_EDGE('',*,*,#47883,.F.);
#68662=ORIENTED_EDGE('',*,*,#50864,.T.);
#68663=ORIENTED_EDGE('',*,*,#47896,.F.);
#68664=ORIENTED_EDGE('',*,*,#50866,.F.);
#68665=ORIENTED_EDGE('',*,*,#48993,.F.);
#68666=ORIENTED_EDGE('',*,*,#50865,.T.);
#68667=ORIENTED_EDGE('',*,*,#49000,.F.);
#68668=ORIENTED_EDGE('',*,*,#50867,.F.);
#68669=ORIENTED_EDGE('',*,*,#47900,.F.);
#68670=ORIENTED_EDGE('',*,*,#50866,.T.);
#68671=ORIENTED_EDGE('',*,*,#46027,.F.);
#68672=ORIENTED_EDGE('',*,*,#50868,.F.);
#68673=ORIENTED_EDGE('',*,*,#48994,.F.);
#68674=ORIENTED_EDGE('',*,*,#50867,.T.);
#68675=ORIENTED_EDGE('',*,*,#48999,.F.);
#68676=ORIENTED_EDGE('',*,*,#50869,.F.);
#68677=ORIENTED_EDGE('',*,*,#47875,.T.);
#68678=ORIENTED_EDGE('',*,*,#47879,.F.);
#68679=ORIENTED_EDGE('',*,*,#50868,.T.);
#68680=ORIENTED_EDGE('',*,*,#46026,.F.);
#68681=ORIENTED_EDGE('',*,*,#50870,.F.);
#68682=ORIENTED_EDGE('',*,*,#50217,.F.);
#68683=ORIENTED_EDGE('',*,*,#50869,.T.);
#68684=ORIENTED_EDGE('',*,*,#48998,.F.);
#68685=ORIENTED_EDGE('',*,*,#50871,.F.);
#68686=ORIENTED_EDGE('',*,*,#47876,.F.);
#68687=ORIENTED_EDGE('',*,*,#50870,.T.);
#68688=ORIENTED_EDGE('',*,*,#46025,.F.);
#68689=ORIENTED_EDGE('',*,*,#50872,.F.);
#68690=ORIENTED_EDGE('',*,*,#48978,.F.);
#68691=ORIENTED_EDGE('',*,*,#50871,.T.);
#68692=ORIENTED_EDGE('',*,*,#48997,.F.);
#68693=ORIENTED_EDGE('',*,*,#50873,.F.);
#68694=ORIENTED_EDGE('',*,*,#47894,.F.);
#68695=ORIENTED_EDGE('',*,*,#50872,.T.);
#68696=ORIENTED_EDGE('',*,*,#46024,.F.);
#68697=ORIENTED_EDGE('',*,*,#50874,.F.);
#68698=ORIENTED_EDGE('',*,*,#50219,.F.);
#68699=ORIENTED_EDGE('',*,*,#50873,.T.);
#68700=ORIENTED_EDGE('',*,*,#48996,.F.);
#68701=ORIENTED_EDGE('',*,*,#50875,.F.);
#68702=ORIENTED_EDGE('',*,*,#46345,.F.);
#68703=ORIENTED_EDGE('',*,*,#50874,.T.);
#68704=ORIENTED_EDGE('',*,*,#46023,.F.);
#68705=ORIENTED_EDGE('',*,*,#50876,.F.);
#68706=ORIENTED_EDGE('',*,*,#48984,.F.);
#68707=ORIENTED_EDGE('',*,*,#50875,.T.);
#68708=ORIENTED_EDGE('',*,*,#50218,.F.);
#68709=ORIENTED_EDGE('',*,*,#50877,.F.);
#68710=ORIENTED_EDGE('',*,*,#46346,.F.);
#68711=ORIENTED_EDGE('',*,*,#50876,.T.);
#68712=ORIENTED_EDGE('',*,*,#47925,.F.);
#68713=ORIENTED_EDGE('',*,*,#50878,.F.);
#68714=ORIENTED_EDGE('',*,*,#48985,.F.);
#68715=ORIENTED_EDGE('',*,*,#50877,.T.);
#68716=ORIENTED_EDGE('',*,*,#48980,.F.);
#68717=ORIENTED_EDGE('',*,*,#50879,.F.);
#68718=ORIENTED_EDGE('',*,*,#46347,.F.);
#68719=ORIENTED_EDGE('',*,*,#47920,.F.);
#68720=ORIENTED_EDGE('',*,*,#47916,.T.);
#68721=ORIENTED_EDGE('',*,*,#50880,.F.);
#68722=ORIENTED_EDGE('',*,*,#48986,.F.);
#68723=ORIENTED_EDGE('',*,*,#50878,.T.);
#68724=ORIENTED_EDGE('',*,*,#50879,.T.);
#68725=ORIENTED_EDGE('',*,*,#50220,.F.);
#68726=ORIENTED_EDGE('',*,*,#50881,.F.);
#68727=ORIENTED_EDGE('',*,*,#46348,.F.);
#68728=ORIENTED_EDGE('',*,*,#50880,.T.);
#68729=ORIENTED_EDGE('',*,*,#47915,.F.);
#68730=ORIENTED_EDGE('',*,*,#50882,.F.);
#68731=ORIENTED_EDGE('',*,*,#48987,.F.);
#68732=ORIENTED_EDGE('',*,*,#50881,.T.);
#68733=ORIENTED_EDGE('',*,*,#48982,.F.);
#68734=ORIENTED_EDGE('',*,*,#50883,.F.);
#68735=ORIENTED_EDGE('',*,*,#46349,.F.);
#68736=ORIENTED_EDGE('',*,*,#50882,.T.);
#68737=ORIENTED_EDGE('',*,*,#47927,.F.);
#68738=ORIENTED_EDGE('',*,*,#50884,.F.);
#68739=ORIENTED_EDGE('',*,*,#48988,.F.);
#68740=ORIENTED_EDGE('',*,*,#50883,.T.);
#68741=ORIENTED_EDGE('',*,*,#48981,.F.);
#68742=ORIENTED_EDGE('',*,*,#50885,.F.);
#68743=ORIENTED_EDGE('',*,*,#47923,.F.);
#68744=ORIENTED_EDGE('',*,*,#50884,.T.);
#68745=ORIENTED_EDGE('',*,*,#47911,.F.);
#68746=ORIENTED_EDGE('',*,*,#50886,.F.);
#68747=ORIENTED_EDGE('',*,*,#48989,.F.);
#68748=ORIENTED_EDGE('',*,*,#50885,.T.);
#68749=ORIENTED_EDGE('',*,*,#48992,.F.);
#68750=ORIENTED_EDGE('',*,*,#50887,.F.);
#68751=ORIENTED_EDGE('',*,*,#47902,.F.);
#68752=ORIENTED_EDGE('',*,*,#50886,.T.);
#68753=ORIENTED_EDGE('',*,*,#47929,.F.);
#68754=ORIENTED_EDGE('',*,*,#50888,.F.);
#68755=ORIENTED_EDGE('',*,*,#48990,.F.);
#68756=ORIENTED_EDGE('',*,*,#50887,.T.);
#68757=ORIENTED_EDGE('',*,*,#48991,.F.);
#68758=ORIENTED_EDGE('',*,*,#50888,.T.);
#68759=ORIENTED_EDGE('',*,*,#47907,.F.);
#68760=ORIENTED_EDGE('',*,*,#47903,.T.);
#68761=ORIENTED_EDGE('',*,*,#50889,.F.);
#68762=ORIENTED_EDGE('',*,*,#49031,.F.);
#68763=ORIENTED_EDGE('',*,*,#50890,.F.);
#68764=ORIENTED_EDGE('',*,*,#47859,.F.);
#68765=ORIENTED_EDGE('',*,*,#50890,.T.);
#68766=ORIENTED_EDGE('',*,*,#49030,.F.);
#68767=ORIENTED_EDGE('',*,*,#50891,.F.);
#68768=ORIENTED_EDGE('',*,*,#47868,.F.);
#68769=ORIENTED_EDGE('',*,*,#47858,.T.);
#68770=ORIENTED_EDGE('',*,*,#47862,.F.);
#68771=ORIENTED_EDGE('',*,*,#50892,.F.);
#68772=ORIENTED_EDGE('',*,*,#49032,.F.);
#68773=ORIENTED_EDGE('',*,*,#50889,.T.);
#68774=ORIENTED_EDGE('',*,*,#50891,.T.);
#68775=ORIENTED_EDGE('',*,*,#49029,.F.);
#68776=ORIENTED_EDGE('',*,*,#50893,.F.);
#68777=ORIENTED_EDGE('',*,*,#47853,.F.);
#68778=ORIENTED_EDGE('',*,*,#50892,.T.);
#68779=ORIENTED_EDGE('',*,*,#47866,.F.);
#68780=ORIENTED_EDGE('',*,*,#50894,.F.);
#68781=ORIENTED_EDGE('',*,*,#49021,.F.);
#68782=ORIENTED_EDGE('',*,*,#50893,.T.);
#68783=ORIENTED_EDGE('',*,*,#49028,.F.);
#68784=ORIENTED_EDGE('',*,*,#50895,.F.);
#68785=ORIENTED_EDGE('',*,*,#47870,.F.);
#68786=ORIENTED_EDGE('',*,*,#50894,.T.);
#68787=ORIENTED_EDGE('',*,*,#46033,.F.);
#68788=ORIENTED_EDGE('',*,*,#50896,.F.);
#68789=ORIENTED_EDGE('',*,*,#49022,.F.);
#68790=ORIENTED_EDGE('',*,*,#50895,.T.);
#68791=ORIENTED_EDGE('',*,*,#49027,.F.);
#68792=ORIENTED_EDGE('',*,*,#50897,.F.);
#68793=ORIENTED_EDGE('',*,*,#47845,.T.);
#68794=ORIENTED_EDGE('',*,*,#47849,.F.);
#68795=ORIENTED_EDGE('',*,*,#50896,.T.);
#68796=ORIENTED_EDGE('',*,*,#46032,.F.);
#68797=ORIENTED_EDGE('',*,*,#50898,.F.);
#68798=ORIENTED_EDGE('',*,*,#50221,.F.);
#68799=ORIENTED_EDGE('',*,*,#50897,.T.);
#68800=ORIENTED_EDGE('',*,*,#49026,.F.);
#68801=ORIENTED_EDGE('',*,*,#50899,.F.);
#68802=ORIENTED_EDGE('',*,*,#47846,.F.);
#68803=ORIENTED_EDGE('',*,*,#50898,.T.);
#68804=ORIENTED_EDGE('',*,*,#46031,.F.);
#68805=ORIENTED_EDGE('',*,*,#50900,.F.);
#68806=ORIENTED_EDGE('',*,*,#49006,.F.);
#68807=ORIENTED_EDGE('',*,*,#50899,.T.);
#68808=ORIENTED_EDGE('',*,*,#49025,.F.);
#68809=ORIENTED_EDGE('',*,*,#50901,.F.);
#68810=ORIENTED_EDGE('',*,*,#47864,.F.);
#68811=ORIENTED_EDGE('',*,*,#50900,.T.);
#68812=ORIENTED_EDGE('',*,*,#46030,.F.);
#68813=ORIENTED_EDGE('',*,*,#50902,.F.);
#68814=ORIENTED_EDGE('',*,*,#50223,.F.);
#68815=ORIENTED_EDGE('',*,*,#50901,.T.);
#68816=ORIENTED_EDGE('',*,*,#49024,.F.);
#68817=ORIENTED_EDGE('',*,*,#50903,.F.);
#68818=ORIENTED_EDGE('',*,*,#46339,.F.);
#68819=ORIENTED_EDGE('',*,*,#50902,.T.);
#68820=ORIENTED_EDGE('',*,*,#46029,.F.);
#68821=ORIENTED_EDGE('',*,*,#50904,.F.);
#68822=ORIENTED_EDGE('',*,*,#49012,.F.);
#68823=ORIENTED_EDGE('',*,*,#50903,.T.);
#68824=ORIENTED_EDGE('',*,*,#50222,.F.);
#68825=ORIENTED_EDGE('',*,*,#50905,.F.);
#68826=ORIENTED_EDGE('',*,*,#46340,.F.);
#68827=ORIENTED_EDGE('',*,*,#50904,.T.);
#68828=ORIENTED_EDGE('',*,*,#47895,.F.);
#68829=ORIENTED_EDGE('',*,*,#50906,.F.);
#68830=ORIENTED_EDGE('',*,*,#49013,.F.);
#68831=ORIENTED_EDGE('',*,*,#50905,.T.);
#68832=ORIENTED_EDGE('',*,*,#49008,.F.);
#68833=ORIENTED_EDGE('',*,*,#50907,.F.);
#68834=ORIENTED_EDGE('',*,*,#46341,.F.);
#68835=ORIENTED_EDGE('',*,*,#47890,.F.);
#68836=ORIENTED_EDGE('',*,*,#47886,.T.);
#68837=ORIENTED_EDGE('',*,*,#50908,.F.);
#68838=ORIENTED_EDGE('',*,*,#49014,.F.);
#68839=ORIENTED_EDGE('',*,*,#50906,.T.);
#68840=ORIENTED_EDGE('',*,*,#50907,.T.);
#68841=ORIENTED_EDGE('',*,*,#50224,.F.);
#68842=ORIENTED_EDGE('',*,*,#50909,.F.);
#68843=ORIENTED_EDGE('',*,*,#46342,.F.);
#68844=ORIENTED_EDGE('',*,*,#50908,.T.);
#68845=ORIENTED_EDGE('',*,*,#47885,.F.);
#68846=ORIENTED_EDGE('',*,*,#50910,.F.);
#68847=ORIENTED_EDGE('',*,*,#49015,.F.);
#68848=ORIENTED_EDGE('',*,*,#50909,.T.);
#68849=ORIENTED_EDGE('',*,*,#49010,.F.);
#68850=ORIENTED_EDGE('',*,*,#50911,.F.);
#68851=ORIENTED_EDGE('',*,*,#46343,.F.);
#68852=ORIENTED_EDGE('',*,*,#50910,.T.);
#68853=ORIENTED_EDGE('',*,*,#47897,.F.);
#68854=ORIENTED_EDGE('',*,*,#50912,.F.);
#68855=ORIENTED_EDGE('',*,*,#49016,.F.);
#68856=ORIENTED_EDGE('',*,*,#50911,.T.);
#68857=ORIENTED_EDGE('',*,*,#49009,.F.);
#68858=ORIENTED_EDGE('',*,*,#50913,.F.);
#68859=ORIENTED_EDGE('',*,*,#47893,.F.);
#68860=ORIENTED_EDGE('',*,*,#50912,.T.);
#68861=ORIENTED_EDGE('',*,*,#47881,.F.);
#68862=ORIENTED_EDGE('',*,*,#50914,.F.);
#68863=ORIENTED_EDGE('',*,*,#49017,.F.);
#68864=ORIENTED_EDGE('',*,*,#50913,.T.);
#68865=ORIENTED_EDGE('',*,*,#49020,.F.);
#68866=ORIENTED_EDGE('',*,*,#50915,.F.);
#68867=ORIENTED_EDGE('',*,*,#47872,.F.);
#68868=ORIENTED_EDGE('',*,*,#50914,.T.);
#68869=ORIENTED_EDGE('',*,*,#47899,.F.);
#68870=ORIENTED_EDGE('',*,*,#50916,.F.);
#68871=ORIENTED_EDGE('',*,*,#49018,.F.);
#68872=ORIENTED_EDGE('',*,*,#50915,.T.);
#68873=ORIENTED_EDGE('',*,*,#49019,.F.);
#68874=ORIENTED_EDGE('',*,*,#50916,.T.);
#68875=ORIENTED_EDGE('',*,*,#47877,.F.);
#68876=ORIENTED_EDGE('',*,*,#47873,.T.);
#68877=ORIENTED_EDGE('',*,*,#50917,.F.);
#68878=ORIENTED_EDGE('',*,*,#49059,.F.);
#68879=ORIENTED_EDGE('',*,*,#50918,.F.);
#68880=ORIENTED_EDGE('',*,*,#47829,.F.);
#68881=ORIENTED_EDGE('',*,*,#50918,.T.);
#68882=ORIENTED_EDGE('',*,*,#49058,.F.);
#68883=ORIENTED_EDGE('',*,*,#50919,.F.);
#68884=ORIENTED_EDGE('',*,*,#47838,.F.);
#68885=ORIENTED_EDGE('',*,*,#47828,.T.);
#68886=ORIENTED_EDGE('',*,*,#47832,.F.);
#68887=ORIENTED_EDGE('',*,*,#50920,.F.);
#68888=ORIENTED_EDGE('',*,*,#49060,.F.);
#68889=ORIENTED_EDGE('',*,*,#50917,.T.);
#68890=ORIENTED_EDGE('',*,*,#50919,.T.);
#68891=ORIENTED_EDGE('',*,*,#49057,.F.);
#68892=ORIENTED_EDGE('',*,*,#50921,.F.);
#68893=ORIENTED_EDGE('',*,*,#47823,.F.);
#68894=ORIENTED_EDGE('',*,*,#50920,.T.);
#68895=ORIENTED_EDGE('',*,*,#47836,.F.);
#68896=ORIENTED_EDGE('',*,*,#50922,.F.);
#68897=ORIENTED_EDGE('',*,*,#49049,.F.);
#68898=ORIENTED_EDGE('',*,*,#50921,.T.);
#68899=ORIENTED_EDGE('',*,*,#49056,.F.);
#68900=ORIENTED_EDGE('',*,*,#50923,.F.);
#68901=ORIENTED_EDGE('',*,*,#47840,.F.);
#68902=ORIENTED_EDGE('',*,*,#50922,.T.);
#68903=ORIENTED_EDGE('',*,*,#46039,.F.);
#68904=ORIENTED_EDGE('',*,*,#50924,.F.);
#68905=ORIENTED_EDGE('',*,*,#49050,.F.);
#68906=ORIENTED_EDGE('',*,*,#50923,.T.);
#68907=ORIENTED_EDGE('',*,*,#49055,.F.);
#68908=ORIENTED_EDGE('',*,*,#50925,.F.);
#68909=ORIENTED_EDGE('',*,*,#47815,.T.);
#68910=ORIENTED_EDGE('',*,*,#47819,.F.);
#68911=ORIENTED_EDGE('',*,*,#50924,.T.);
#68912=ORIENTED_EDGE('',*,*,#46038,.F.);
#68913=ORIENTED_EDGE('',*,*,#50926,.F.);
#68914=ORIENTED_EDGE('',*,*,#50225,.F.);
#68915=ORIENTED_EDGE('',*,*,#50925,.T.);
#68916=ORIENTED_EDGE('',*,*,#49054,.F.);
#68917=ORIENTED_EDGE('',*,*,#50927,.F.);
#68918=ORIENTED_EDGE('',*,*,#47816,.F.);
#68919=ORIENTED_EDGE('',*,*,#50926,.T.);
#68920=ORIENTED_EDGE('',*,*,#46037,.F.);
#68921=ORIENTED_EDGE('',*,*,#50928,.F.);
#68922=ORIENTED_EDGE('',*,*,#49034,.F.);
#68923=ORIENTED_EDGE('',*,*,#50927,.T.);
#68924=ORIENTED_EDGE('',*,*,#49053,.F.);
#68925=ORIENTED_EDGE('',*,*,#50929,.F.);
#68926=ORIENTED_EDGE('',*,*,#47834,.F.);
#68927=ORIENTED_EDGE('',*,*,#50928,.T.);
#68928=ORIENTED_EDGE('',*,*,#46036,.F.);
#68929=ORIENTED_EDGE('',*,*,#50930,.F.);
#68930=ORIENTED_EDGE('',*,*,#50227,.F.);
#68931=ORIENTED_EDGE('',*,*,#50929,.T.);
#68932=ORIENTED_EDGE('',*,*,#49052,.F.);
#68933=ORIENTED_EDGE('',*,*,#50931,.F.);
#68934=ORIENTED_EDGE('',*,*,#46333,.F.);
#68935=ORIENTED_EDGE('',*,*,#50930,.T.);
#68936=ORIENTED_EDGE('',*,*,#46035,.F.);
#68937=ORIENTED_EDGE('',*,*,#50932,.F.);
#68938=ORIENTED_EDGE('',*,*,#49040,.F.);
#68939=ORIENTED_EDGE('',*,*,#50931,.T.);
#68940=ORIENTED_EDGE('',*,*,#50226,.F.);
#68941=ORIENTED_EDGE('',*,*,#50933,.F.);
#68942=ORIENTED_EDGE('',*,*,#46334,.F.);
#68943=ORIENTED_EDGE('',*,*,#50932,.T.);
#68944=ORIENTED_EDGE('',*,*,#47865,.F.);
#68945=ORIENTED_EDGE('',*,*,#50934,.F.);
#68946=ORIENTED_EDGE('',*,*,#49041,.F.);
#68947=ORIENTED_EDGE('',*,*,#50933,.T.);
#68948=ORIENTED_EDGE('',*,*,#49036,.F.);
#68949=ORIENTED_EDGE('',*,*,#50935,.F.);
#68950=ORIENTED_EDGE('',*,*,#46335,.F.);
#68951=ORIENTED_EDGE('',*,*,#47860,.F.);
#68952=ORIENTED_EDGE('',*,*,#47856,.T.);
#68953=ORIENTED_EDGE('',*,*,#50936,.F.);
#68954=ORIENTED_EDGE('',*,*,#49042,.F.);
#68955=ORIENTED_EDGE('',*,*,#50934,.T.);
#68956=ORIENTED_EDGE('',*,*,#50935,.T.);
#68957=ORIENTED_EDGE('',*,*,#50228,.F.);
#68958=ORIENTED_EDGE('',*,*,#50937,.F.);
#68959=ORIENTED_EDGE('',*,*,#46336,.F.);
#68960=ORIENTED_EDGE('',*,*,#50936,.T.);
#68961=ORIENTED_EDGE('',*,*,#47855,.F.);
#68962=ORIENTED_EDGE('',*,*,#50938,.F.);
#68963=ORIENTED_EDGE('',*,*,#49043,.F.);
#68964=ORIENTED_EDGE('',*,*,#50937,.T.);
#68965=ORIENTED_EDGE('',*,*,#49038,.F.);
#68966=ORIENTED_EDGE('',*,*,#50939,.F.);
#68967=ORIENTED_EDGE('',*,*,#46337,.F.);
#68968=ORIENTED_EDGE('',*,*,#50938,.T.);
#68969=ORIENTED_EDGE('',*,*,#47867,.F.);
#68970=ORIENTED_EDGE('',*,*,#50940,.F.);
#68971=ORIENTED_EDGE('',*,*,#49044,.F.);
#68972=ORIENTED_EDGE('',*,*,#50939,.T.);
#68973=ORIENTED_EDGE('',*,*,#49037,.F.);
#68974=ORIENTED_EDGE('',*,*,#50941,.F.);
#68975=ORIENTED_EDGE('',*,*,#47863,.F.);
#68976=ORIENTED_EDGE('',*,*,#50940,.T.);
#68977=ORIENTED_EDGE('',*,*,#47851,.F.);
#68978=ORIENTED_EDGE('',*,*,#50942,.F.);
#68979=ORIENTED_EDGE('',*,*,#49045,.F.);
#68980=ORIENTED_EDGE('',*,*,#50941,.T.);
#68981=ORIENTED_EDGE('',*,*,#49048,.F.);
#68982=ORIENTED_EDGE('',*,*,#50943,.F.);
#68983=ORIENTED_EDGE('',*,*,#47842,.F.);
#68984=ORIENTED_EDGE('',*,*,#50942,.T.);
#68985=ORIENTED_EDGE('',*,*,#47869,.F.);
#68986=ORIENTED_EDGE('',*,*,#50944,.F.);
#68987=ORIENTED_EDGE('',*,*,#49046,.F.);
#68988=ORIENTED_EDGE('',*,*,#50943,.T.);
#68989=ORIENTED_EDGE('',*,*,#49047,.F.);
#68990=ORIENTED_EDGE('',*,*,#50944,.T.);
#68991=ORIENTED_EDGE('',*,*,#47847,.F.);
#68992=ORIENTED_EDGE('',*,*,#47843,.T.);
#68993=ORIENTED_EDGE('',*,*,#50945,.F.);
#68994=ORIENTED_EDGE('',*,*,#49087,.F.);
#68995=ORIENTED_EDGE('',*,*,#50946,.F.);
#68996=ORIENTED_EDGE('',*,*,#47799,.F.);
#68997=ORIENTED_EDGE('',*,*,#50946,.T.);
#68998=ORIENTED_EDGE('',*,*,#49086,.F.);
#68999=ORIENTED_EDGE('',*,*,#50947,.F.);
#69000=ORIENTED_EDGE('',*,*,#47808,.F.);
#69001=ORIENTED_EDGE('',*,*,#47798,.T.);
#69002=ORIENTED_EDGE('',*,*,#47802,.F.);
#69003=ORIENTED_EDGE('',*,*,#50948,.F.);
#69004=ORIENTED_EDGE('',*,*,#49088,.F.);
#69005=ORIENTED_EDGE('',*,*,#50945,.T.);
#69006=ORIENTED_EDGE('',*,*,#50947,.T.);
#69007=ORIENTED_EDGE('',*,*,#49085,.F.);
#69008=ORIENTED_EDGE('',*,*,#50949,.F.);
#69009=ORIENTED_EDGE('',*,*,#47793,.F.);
#69010=ORIENTED_EDGE('',*,*,#50948,.T.);
#69011=ORIENTED_EDGE('',*,*,#47806,.F.);
#69012=ORIENTED_EDGE('',*,*,#50950,.F.);
#69013=ORIENTED_EDGE('',*,*,#49077,.F.);
#69014=ORIENTED_EDGE('',*,*,#50949,.T.);
#69015=ORIENTED_EDGE('',*,*,#49084,.F.);
#69016=ORIENTED_EDGE('',*,*,#50951,.F.);
#69017=ORIENTED_EDGE('',*,*,#47810,.F.);
#69018=ORIENTED_EDGE('',*,*,#50950,.T.);
#69019=ORIENTED_EDGE('',*,*,#46045,.F.);
#69020=ORIENTED_EDGE('',*,*,#50952,.F.);
#69021=ORIENTED_EDGE('',*,*,#49078,.F.);
#69022=ORIENTED_EDGE('',*,*,#50951,.T.);
#69023=ORIENTED_EDGE('',*,*,#49083,.F.);
#69024=ORIENTED_EDGE('',*,*,#50953,.F.);
#69025=ORIENTED_EDGE('',*,*,#47785,.T.);
#69026=ORIENTED_EDGE('',*,*,#47789,.F.);
#69027=ORIENTED_EDGE('',*,*,#50952,.T.);
#69028=ORIENTED_EDGE('',*,*,#46044,.F.);
#69029=ORIENTED_EDGE('',*,*,#50954,.F.);
#69030=ORIENTED_EDGE('',*,*,#50229,.F.);
#69031=ORIENTED_EDGE('',*,*,#50953,.T.);
#69032=ORIENTED_EDGE('',*,*,#49082,.F.);
#69033=ORIENTED_EDGE('',*,*,#50955,.F.);
#69034=ORIENTED_EDGE('',*,*,#47786,.F.);
#69035=ORIENTED_EDGE('',*,*,#50954,.T.);
#69036=ORIENTED_EDGE('',*,*,#46043,.F.);
#69037=ORIENTED_EDGE('',*,*,#50956,.F.);
#69038=ORIENTED_EDGE('',*,*,#49062,.F.);
#69039=ORIENTED_EDGE('',*,*,#50955,.T.);
#69040=ORIENTED_EDGE('',*,*,#49081,.F.);
#69041=ORIENTED_EDGE('',*,*,#50957,.F.);
#69042=ORIENTED_EDGE('',*,*,#47804,.F.);
#69043=ORIENTED_EDGE('',*,*,#50956,.T.);
#69044=ORIENTED_EDGE('',*,*,#46042,.F.);
#69045=ORIENTED_EDGE('',*,*,#50958,.F.);
#69046=ORIENTED_EDGE('',*,*,#50231,.F.);
#69047=ORIENTED_EDGE('',*,*,#50957,.T.);
#69048=ORIENTED_EDGE('',*,*,#49080,.F.);
#69049=ORIENTED_EDGE('',*,*,#50959,.F.);
#69050=ORIENTED_EDGE('',*,*,#46327,.F.);
#69051=ORIENTED_EDGE('',*,*,#50958,.T.);
#69052=ORIENTED_EDGE('',*,*,#46041,.F.);
#69053=ORIENTED_EDGE('',*,*,#50960,.F.);
#69054=ORIENTED_EDGE('',*,*,#49068,.F.);
#69055=ORIENTED_EDGE('',*,*,#50959,.T.);
#69056=ORIENTED_EDGE('',*,*,#50230,.F.);
#69057=ORIENTED_EDGE('',*,*,#50961,.F.);
#69058=ORIENTED_EDGE('',*,*,#46328,.F.);
#69059=ORIENTED_EDGE('',*,*,#50960,.T.);
#69060=ORIENTED_EDGE('',*,*,#47835,.F.);
#69061=ORIENTED_EDGE('',*,*,#50962,.F.);
#69062=ORIENTED_EDGE('',*,*,#49069,.F.);
#69063=ORIENTED_EDGE('',*,*,#50961,.T.);
#69064=ORIENTED_EDGE('',*,*,#49064,.F.);
#69065=ORIENTED_EDGE('',*,*,#50963,.F.);
#69066=ORIENTED_EDGE('',*,*,#46329,.F.);
#69067=ORIENTED_EDGE('',*,*,#47830,.F.);
#69068=ORIENTED_EDGE('',*,*,#47826,.T.);
#69069=ORIENTED_EDGE('',*,*,#50964,.F.);
#69070=ORIENTED_EDGE('',*,*,#49070,.F.);
#69071=ORIENTED_EDGE('',*,*,#50962,.T.);
#69072=ORIENTED_EDGE('',*,*,#50963,.T.);
#69073=ORIENTED_EDGE('',*,*,#50232,.F.);
#69074=ORIENTED_EDGE('',*,*,#50965,.F.);
#69075=ORIENTED_EDGE('',*,*,#46330,.F.);
#69076=ORIENTED_EDGE('',*,*,#50964,.T.);
#69077=ORIENTED_EDGE('',*,*,#47825,.F.);
#69078=ORIENTED_EDGE('',*,*,#50966,.F.);
#69079=ORIENTED_EDGE('',*,*,#49071,.F.);
#69080=ORIENTED_EDGE('',*,*,#50965,.T.);
#69081=ORIENTED_EDGE('',*,*,#49066,.F.);
#69082=ORIENTED_EDGE('',*,*,#50967,.F.);
#69083=ORIENTED_EDGE('',*,*,#46331,.F.);
#69084=ORIENTED_EDGE('',*,*,#50966,.T.);
#69085=ORIENTED_EDGE('',*,*,#47837,.F.);
#69086=ORIENTED_EDGE('',*,*,#50968,.F.);
#69087=ORIENTED_EDGE('',*,*,#49072,.F.);
#69088=ORIENTED_EDGE('',*,*,#50967,.T.);
#69089=ORIENTED_EDGE('',*,*,#49065,.F.);
#69090=ORIENTED_EDGE('',*,*,#50969,.F.);
#69091=ORIENTED_EDGE('',*,*,#47833,.F.);
#69092=ORIENTED_EDGE('',*,*,#50968,.T.);
#69093=ORIENTED_EDGE('',*,*,#47821,.F.);
#69094=ORIENTED_EDGE('',*,*,#50970,.F.);
#69095=ORIENTED_EDGE('',*,*,#49073,.F.);
#69096=ORIENTED_EDGE('',*,*,#50969,.T.);
#69097=ORIENTED_EDGE('',*,*,#49076,.F.);
#69098=ORIENTED_EDGE('',*,*,#50971,.F.);
#69099=ORIENTED_EDGE('',*,*,#47812,.F.);
#69100=ORIENTED_EDGE('',*,*,#50970,.T.);
#69101=ORIENTED_EDGE('',*,*,#47839,.F.);
#69102=ORIENTED_EDGE('',*,*,#50972,.F.);
#69103=ORIENTED_EDGE('',*,*,#49074,.F.);
#69104=ORIENTED_EDGE('',*,*,#50971,.T.);
#69105=ORIENTED_EDGE('',*,*,#49075,.F.);
#69106=ORIENTED_EDGE('',*,*,#50972,.T.);
#69107=ORIENTED_EDGE('',*,*,#47817,.F.);
#69108=ORIENTED_EDGE('',*,*,#47813,.T.);
#69109=ORIENTED_EDGE('',*,*,#50973,.F.);
#69110=ORIENTED_EDGE('',*,*,#49115,.F.);
#69111=ORIENTED_EDGE('',*,*,#50974,.F.);
#69112=ORIENTED_EDGE('',*,*,#47769,.F.);
#69113=ORIENTED_EDGE('',*,*,#50974,.T.);
#69114=ORIENTED_EDGE('',*,*,#49114,.F.);
#69115=ORIENTED_EDGE('',*,*,#50975,.F.);
#69116=ORIENTED_EDGE('',*,*,#47778,.F.);
#69117=ORIENTED_EDGE('',*,*,#47768,.T.);
#69118=ORIENTED_EDGE('',*,*,#47772,.F.);
#69119=ORIENTED_EDGE('',*,*,#50976,.F.);
#69120=ORIENTED_EDGE('',*,*,#49116,.F.);
#69121=ORIENTED_EDGE('',*,*,#50973,.T.);
#69122=ORIENTED_EDGE('',*,*,#50975,.T.);
#69123=ORIENTED_EDGE('',*,*,#49113,.F.);
#69124=ORIENTED_EDGE('',*,*,#50977,.F.);
#69125=ORIENTED_EDGE('',*,*,#47763,.F.);
#69126=ORIENTED_EDGE('',*,*,#50976,.T.);
#69127=ORIENTED_EDGE('',*,*,#47776,.F.);
#69128=ORIENTED_EDGE('',*,*,#50978,.F.);
#69129=ORIENTED_EDGE('',*,*,#49105,.F.);
#69130=ORIENTED_EDGE('',*,*,#50977,.T.);
#69131=ORIENTED_EDGE('',*,*,#49112,.F.);
#69132=ORIENTED_EDGE('',*,*,#50979,.F.);
#69133=ORIENTED_EDGE('',*,*,#47780,.F.);
#69134=ORIENTED_EDGE('',*,*,#50978,.T.);
#69135=ORIENTED_EDGE('',*,*,#46051,.F.);
#69136=ORIENTED_EDGE('',*,*,#50980,.F.);
#69137=ORIENTED_EDGE('',*,*,#49106,.F.);
#69138=ORIENTED_EDGE('',*,*,#50979,.T.);
#69139=ORIENTED_EDGE('',*,*,#49111,.F.);
#69140=ORIENTED_EDGE('',*,*,#50981,.F.);
#69141=ORIENTED_EDGE('',*,*,#47755,.T.);
#69142=ORIENTED_EDGE('',*,*,#47759,.F.);
#69143=ORIENTED_EDGE('',*,*,#50980,.T.);
#69144=ORIENTED_EDGE('',*,*,#46050,.F.);
#69145=ORIENTED_EDGE('',*,*,#50982,.F.);
#69146=ORIENTED_EDGE('',*,*,#50233,.F.);
#69147=ORIENTED_EDGE('',*,*,#50981,.T.);
#69148=ORIENTED_EDGE('',*,*,#49110,.F.);
#69149=ORIENTED_EDGE('',*,*,#50983,.F.);
#69150=ORIENTED_EDGE('',*,*,#47756,.F.);
#69151=ORIENTED_EDGE('',*,*,#50982,.T.);
#69152=ORIENTED_EDGE('',*,*,#46049,.F.);
#69153=ORIENTED_EDGE('',*,*,#50984,.F.);
#69154=ORIENTED_EDGE('',*,*,#49090,.F.);
#69155=ORIENTED_EDGE('',*,*,#50983,.T.);
#69156=ORIENTED_EDGE('',*,*,#49109,.F.);
#69157=ORIENTED_EDGE('',*,*,#50985,.F.);
#69158=ORIENTED_EDGE('',*,*,#47774,.F.);
#69159=ORIENTED_EDGE('',*,*,#50984,.T.);
#69160=ORIENTED_EDGE('',*,*,#46048,.F.);
#69161=ORIENTED_EDGE('',*,*,#50986,.F.);
#69162=ORIENTED_EDGE('',*,*,#50235,.F.);
#69163=ORIENTED_EDGE('',*,*,#50985,.T.);
#69164=ORIENTED_EDGE('',*,*,#49108,.F.);
#69165=ORIENTED_EDGE('',*,*,#50987,.F.);
#69166=ORIENTED_EDGE('',*,*,#46321,.F.);
#69167=ORIENTED_EDGE('',*,*,#50986,.T.);
#69168=ORIENTED_EDGE('',*,*,#46047,.F.);
#69169=ORIENTED_EDGE('',*,*,#50988,.F.);
#69170=ORIENTED_EDGE('',*,*,#49096,.F.);
#69171=ORIENTED_EDGE('',*,*,#50987,.T.);
#69172=ORIENTED_EDGE('',*,*,#50234,.F.);
#69173=ORIENTED_EDGE('',*,*,#50989,.F.);
#69174=ORIENTED_EDGE('',*,*,#46322,.F.);
#69175=ORIENTED_EDGE('',*,*,#50988,.T.);
#69176=ORIENTED_EDGE('',*,*,#47805,.F.);
#69177=ORIENTED_EDGE('',*,*,#50990,.F.);
#69178=ORIENTED_EDGE('',*,*,#49097,.F.);
#69179=ORIENTED_EDGE('',*,*,#50989,.T.);
#69180=ORIENTED_EDGE('',*,*,#49092,.F.);
#69181=ORIENTED_EDGE('',*,*,#50991,.F.);
#69182=ORIENTED_EDGE('',*,*,#46323,.F.);
#69183=ORIENTED_EDGE('',*,*,#47800,.F.);
#69184=ORIENTED_EDGE('',*,*,#47796,.T.);
#69185=ORIENTED_EDGE('',*,*,#50992,.F.);
#69186=ORIENTED_EDGE('',*,*,#49098,.F.);
#69187=ORIENTED_EDGE('',*,*,#50990,.T.);
#69188=ORIENTED_EDGE('',*,*,#50991,.T.);
#69189=ORIENTED_EDGE('',*,*,#50236,.F.);
#69190=ORIENTED_EDGE('',*,*,#50993,.F.);
#69191=ORIENTED_EDGE('',*,*,#46324,.F.);
#69192=ORIENTED_EDGE('',*,*,#50992,.T.);
#69193=ORIENTED_EDGE('',*,*,#47795,.F.);
#69194=ORIENTED_EDGE('',*,*,#50994,.F.);
#69195=ORIENTED_EDGE('',*,*,#49099,.F.);
#69196=ORIENTED_EDGE('',*,*,#50993,.T.);
#69197=ORIENTED_EDGE('',*,*,#49094,.F.);
#69198=ORIENTED_EDGE('',*,*,#50995,.F.);
#69199=ORIENTED_EDGE('',*,*,#46325,.F.);
#69200=ORIENTED_EDGE('',*,*,#50994,.T.);
#69201=ORIENTED_EDGE('',*,*,#47807,.F.);
#69202=ORIENTED_EDGE('',*,*,#50996,.F.);
#69203=ORIENTED_EDGE('',*,*,#49100,.F.);
#69204=ORIENTED_EDGE('',*,*,#50995,.T.);
#69205=ORIENTED_EDGE('',*,*,#49093,.F.);
#69206=ORIENTED_EDGE('',*,*,#50997,.F.);
#69207=ORIENTED_EDGE('',*,*,#47803,.F.);
#69208=ORIENTED_EDGE('',*,*,#50996,.T.);
#69209=ORIENTED_EDGE('',*,*,#47791,.F.);
#69210=ORIENTED_EDGE('',*,*,#50998,.F.);
#69211=ORIENTED_EDGE('',*,*,#49101,.F.);
#69212=ORIENTED_EDGE('',*,*,#50997,.T.);
#69213=ORIENTED_EDGE('',*,*,#49104,.F.);
#69214=ORIENTED_EDGE('',*,*,#50999,.F.);
#69215=ORIENTED_EDGE('',*,*,#47782,.F.);
#69216=ORIENTED_EDGE('',*,*,#50998,.T.);
#69217=ORIENTED_EDGE('',*,*,#47809,.F.);
#69218=ORIENTED_EDGE('',*,*,#51000,.F.);
#69219=ORIENTED_EDGE('',*,*,#49102,.F.);
#69220=ORIENTED_EDGE('',*,*,#50999,.T.);
#69221=ORIENTED_EDGE('',*,*,#49103,.F.);
#69222=ORIENTED_EDGE('',*,*,#51000,.T.);
#69223=ORIENTED_EDGE('',*,*,#47787,.F.);
#69224=ORIENTED_EDGE('',*,*,#47783,.T.);
#69225=ORIENTED_EDGE('',*,*,#51001,.F.);
#69226=ORIENTED_EDGE('',*,*,#49143,.F.);
#69227=ORIENTED_EDGE('',*,*,#51002,.F.);
#69228=ORIENTED_EDGE('',*,*,#47739,.F.);
#69229=ORIENTED_EDGE('',*,*,#51002,.T.);
#69230=ORIENTED_EDGE('',*,*,#49142,.F.);
#69231=ORIENTED_EDGE('',*,*,#51003,.F.);
#69232=ORIENTED_EDGE('',*,*,#47748,.F.);
#69233=ORIENTED_EDGE('',*,*,#47738,.T.);
#69234=ORIENTED_EDGE('',*,*,#47742,.F.);
#69235=ORIENTED_EDGE('',*,*,#51004,.F.);
#69236=ORIENTED_EDGE('',*,*,#49144,.F.);
#69237=ORIENTED_EDGE('',*,*,#51001,.T.);
#69238=ORIENTED_EDGE('',*,*,#51003,.T.);
#69239=ORIENTED_EDGE('',*,*,#49141,.F.);
#69240=ORIENTED_EDGE('',*,*,#51005,.F.);
#69241=ORIENTED_EDGE('',*,*,#47733,.F.);
#69242=ORIENTED_EDGE('',*,*,#51004,.T.);
#69243=ORIENTED_EDGE('',*,*,#47746,.F.);
#69244=ORIENTED_EDGE('',*,*,#51006,.F.);
#69245=ORIENTED_EDGE('',*,*,#49133,.F.);
#69246=ORIENTED_EDGE('',*,*,#51005,.T.);
#69247=ORIENTED_EDGE('',*,*,#49140,.F.);
#69248=ORIENTED_EDGE('',*,*,#51007,.F.);
#69249=ORIENTED_EDGE('',*,*,#47750,.F.);
#69250=ORIENTED_EDGE('',*,*,#51006,.T.);
#69251=ORIENTED_EDGE('',*,*,#46057,.F.);
#69252=ORIENTED_EDGE('',*,*,#51008,.F.);
#69253=ORIENTED_EDGE('',*,*,#49134,.F.);
#69254=ORIENTED_EDGE('',*,*,#51007,.T.);
#69255=ORIENTED_EDGE('',*,*,#49139,.F.);
#69256=ORIENTED_EDGE('',*,*,#51009,.F.);
#69257=ORIENTED_EDGE('',*,*,#47725,.T.);
#69258=ORIENTED_EDGE('',*,*,#47729,.F.);
#69259=ORIENTED_EDGE('',*,*,#51008,.T.);
#69260=ORIENTED_EDGE('',*,*,#46056,.F.);
#69261=ORIENTED_EDGE('',*,*,#51010,.F.);
#69262=ORIENTED_EDGE('',*,*,#50237,.F.);
#69263=ORIENTED_EDGE('',*,*,#51009,.T.);
#69264=ORIENTED_EDGE('',*,*,#49138,.F.);
#69265=ORIENTED_EDGE('',*,*,#51011,.F.);
#69266=ORIENTED_EDGE('',*,*,#47726,.F.);
#69267=ORIENTED_EDGE('',*,*,#51010,.T.);
#69268=ORIENTED_EDGE('',*,*,#46055,.F.);
#69269=ORIENTED_EDGE('',*,*,#51012,.F.);
#69270=ORIENTED_EDGE('',*,*,#49118,.F.);
#69271=ORIENTED_EDGE('',*,*,#51011,.T.);
#69272=ORIENTED_EDGE('',*,*,#49137,.F.);
#69273=ORIENTED_EDGE('',*,*,#51013,.F.);
#69274=ORIENTED_EDGE('',*,*,#47744,.F.);
#69275=ORIENTED_EDGE('',*,*,#51012,.T.);
#69276=ORIENTED_EDGE('',*,*,#46054,.F.);
#69277=ORIENTED_EDGE('',*,*,#51014,.F.);
#69278=ORIENTED_EDGE('',*,*,#50239,.F.);
#69279=ORIENTED_EDGE('',*,*,#51013,.T.);
#69280=ORIENTED_EDGE('',*,*,#49136,.F.);
#69281=ORIENTED_EDGE('',*,*,#51015,.F.);
#69282=ORIENTED_EDGE('',*,*,#46315,.F.);
#69283=ORIENTED_EDGE('',*,*,#51014,.T.);
#69284=ORIENTED_EDGE('',*,*,#46053,.F.);
#69285=ORIENTED_EDGE('',*,*,#51016,.F.);
#69286=ORIENTED_EDGE('',*,*,#49124,.F.);
#69287=ORIENTED_EDGE('',*,*,#51015,.T.);
#69288=ORIENTED_EDGE('',*,*,#50238,.F.);
#69289=ORIENTED_EDGE('',*,*,#51017,.F.);
#69290=ORIENTED_EDGE('',*,*,#46316,.F.);
#69291=ORIENTED_EDGE('',*,*,#51016,.T.);
#69292=ORIENTED_EDGE('',*,*,#47775,.F.);
#69293=ORIENTED_EDGE('',*,*,#51018,.F.);
#69294=ORIENTED_EDGE('',*,*,#49125,.F.);
#69295=ORIENTED_EDGE('',*,*,#51017,.T.);
#69296=ORIENTED_EDGE('',*,*,#49120,.F.);
#69297=ORIENTED_EDGE('',*,*,#51019,.F.);
#69298=ORIENTED_EDGE('',*,*,#46317,.F.);
#69299=ORIENTED_EDGE('',*,*,#47770,.F.);
#69300=ORIENTED_EDGE('',*,*,#47766,.T.);
#69301=ORIENTED_EDGE('',*,*,#51020,.F.);
#69302=ORIENTED_EDGE('',*,*,#49126,.F.);
#69303=ORIENTED_EDGE('',*,*,#51018,.T.);
#69304=ORIENTED_EDGE('',*,*,#51019,.T.);
#69305=ORIENTED_EDGE('',*,*,#50240,.F.);
#69306=ORIENTED_EDGE('',*,*,#51021,.F.);
#69307=ORIENTED_EDGE('',*,*,#46318,.F.);
#69308=ORIENTED_EDGE('',*,*,#51020,.T.);
#69309=ORIENTED_EDGE('',*,*,#47765,.F.);
#69310=ORIENTED_EDGE('',*,*,#51022,.F.);
#69311=ORIENTED_EDGE('',*,*,#49127,.F.);
#69312=ORIENTED_EDGE('',*,*,#51021,.T.);
#69313=ORIENTED_EDGE('',*,*,#49122,.F.);
#69314=ORIENTED_EDGE('',*,*,#51023,.F.);
#69315=ORIENTED_EDGE('',*,*,#46319,.F.);
#69316=ORIENTED_EDGE('',*,*,#51022,.T.);
#69317=ORIENTED_EDGE('',*,*,#47777,.F.);
#69318=ORIENTED_EDGE('',*,*,#51024,.F.);
#69319=ORIENTED_EDGE('',*,*,#49128,.F.);
#69320=ORIENTED_EDGE('',*,*,#51023,.T.);
#69321=ORIENTED_EDGE('',*,*,#49121,.F.);
#69322=ORIENTED_EDGE('',*,*,#51025,.F.);
#69323=ORIENTED_EDGE('',*,*,#47773,.F.);
#69324=ORIENTED_EDGE('',*,*,#51024,.T.);
#69325=ORIENTED_EDGE('',*,*,#47761,.F.);
#69326=ORIENTED_EDGE('',*,*,#51026,.F.);
#69327=ORIENTED_EDGE('',*,*,#49129,.F.);
#69328=ORIENTED_EDGE('',*,*,#51025,.T.);
#69329=ORIENTED_EDGE('',*,*,#49132,.F.);
#69330=ORIENTED_EDGE('',*,*,#51027,.F.);
#69331=ORIENTED_EDGE('',*,*,#47752,.F.);
#69332=ORIENTED_EDGE('',*,*,#51026,.T.);
#69333=ORIENTED_EDGE('',*,*,#47779,.F.);
#69334=ORIENTED_EDGE('',*,*,#51028,.F.);
#69335=ORIENTED_EDGE('',*,*,#49130,.F.);
#69336=ORIENTED_EDGE('',*,*,#51027,.T.);
#69337=ORIENTED_EDGE('',*,*,#49131,.F.);
#69338=ORIENTED_EDGE('',*,*,#51028,.T.);
#69339=ORIENTED_EDGE('',*,*,#47757,.F.);
#69340=ORIENTED_EDGE('',*,*,#47753,.T.);
#69341=ORIENTED_EDGE('',*,*,#51029,.F.);
#69342=ORIENTED_EDGE('',*,*,#49171,.F.);
#69343=ORIENTED_EDGE('',*,*,#51030,.F.);
#69344=ORIENTED_EDGE('',*,*,#47709,.F.);
#69345=ORIENTED_EDGE('',*,*,#51030,.T.);
#69346=ORIENTED_EDGE('',*,*,#49170,.F.);
#69347=ORIENTED_EDGE('',*,*,#51031,.F.);
#69348=ORIENTED_EDGE('',*,*,#47718,.F.);
#69349=ORIENTED_EDGE('',*,*,#47708,.T.);
#69350=ORIENTED_EDGE('',*,*,#47712,.F.);
#69351=ORIENTED_EDGE('',*,*,#51032,.F.);
#69352=ORIENTED_EDGE('',*,*,#49172,.F.);
#69353=ORIENTED_EDGE('',*,*,#51029,.T.);
#69354=ORIENTED_EDGE('',*,*,#51031,.T.);
#69355=ORIENTED_EDGE('',*,*,#49169,.F.);
#69356=ORIENTED_EDGE('',*,*,#51033,.F.);
#69357=ORIENTED_EDGE('',*,*,#47703,.F.);
#69358=ORIENTED_EDGE('',*,*,#51032,.T.);
#69359=ORIENTED_EDGE('',*,*,#47716,.F.);
#69360=ORIENTED_EDGE('',*,*,#51034,.F.);
#69361=ORIENTED_EDGE('',*,*,#49161,.F.);
#69362=ORIENTED_EDGE('',*,*,#51033,.T.);
#69363=ORIENTED_EDGE('',*,*,#49168,.F.);
#69364=ORIENTED_EDGE('',*,*,#51035,.F.);
#69365=ORIENTED_EDGE('',*,*,#47720,.F.);
#69366=ORIENTED_EDGE('',*,*,#51034,.T.);
#69367=ORIENTED_EDGE('',*,*,#46063,.F.);
#69368=ORIENTED_EDGE('',*,*,#51036,.F.);
#69369=ORIENTED_EDGE('',*,*,#49162,.F.);
#69370=ORIENTED_EDGE('',*,*,#51035,.T.);
#69371=ORIENTED_EDGE('',*,*,#49167,.F.);
#69372=ORIENTED_EDGE('',*,*,#51037,.F.);
#69373=ORIENTED_EDGE('',*,*,#47695,.T.);
#69374=ORIENTED_EDGE('',*,*,#47699,.F.);
#69375=ORIENTED_EDGE('',*,*,#51036,.T.);
#69376=ORIENTED_EDGE('',*,*,#46062,.F.);
#69377=ORIENTED_EDGE('',*,*,#51038,.F.);
#69378=ORIENTED_EDGE('',*,*,#50241,.F.);
#69379=ORIENTED_EDGE('',*,*,#51037,.T.);
#69380=ORIENTED_EDGE('',*,*,#49166,.F.);
#69381=ORIENTED_EDGE('',*,*,#51039,.F.);
#69382=ORIENTED_EDGE('',*,*,#47696,.F.);
#69383=ORIENTED_EDGE('',*,*,#51038,.T.);
#69384=ORIENTED_EDGE('',*,*,#46061,.F.);
#69385=ORIENTED_EDGE('',*,*,#51040,.F.);
#69386=ORIENTED_EDGE('',*,*,#49146,.F.);
#69387=ORIENTED_EDGE('',*,*,#51039,.T.);
#69388=ORIENTED_EDGE('',*,*,#49165,.F.);
#69389=ORIENTED_EDGE('',*,*,#51041,.F.);
#69390=ORIENTED_EDGE('',*,*,#47714,.F.);
#69391=ORIENTED_EDGE('',*,*,#51040,.T.);
#69392=ORIENTED_EDGE('',*,*,#46060,.F.);
#69393=ORIENTED_EDGE('',*,*,#51042,.F.);
#69394=ORIENTED_EDGE('',*,*,#50243,.F.);
#69395=ORIENTED_EDGE('',*,*,#51041,.T.);
#69396=ORIENTED_EDGE('',*,*,#49164,.F.);
#69397=ORIENTED_EDGE('',*,*,#51043,.F.);
#69398=ORIENTED_EDGE('',*,*,#46309,.F.);
#69399=ORIENTED_EDGE('',*,*,#51042,.T.);
#69400=ORIENTED_EDGE('',*,*,#46059,.F.);
#69401=ORIENTED_EDGE('',*,*,#51044,.F.);
#69402=ORIENTED_EDGE('',*,*,#49152,.F.);
#69403=ORIENTED_EDGE('',*,*,#51043,.T.);
#69404=ORIENTED_EDGE('',*,*,#50242,.F.);
#69405=ORIENTED_EDGE('',*,*,#51045,.F.);
#69406=ORIENTED_EDGE('',*,*,#46310,.F.);
#69407=ORIENTED_EDGE('',*,*,#51044,.T.);
#69408=ORIENTED_EDGE('',*,*,#47745,.F.);
#69409=ORIENTED_EDGE('',*,*,#51046,.F.);
#69410=ORIENTED_EDGE('',*,*,#49153,.F.);
#69411=ORIENTED_EDGE('',*,*,#51045,.T.);
#69412=ORIENTED_EDGE('',*,*,#49148,.F.);
#69413=ORIENTED_EDGE('',*,*,#51047,.F.);
#69414=ORIENTED_EDGE('',*,*,#46311,.F.);
#69415=ORIENTED_EDGE('',*,*,#47740,.F.);
#69416=ORIENTED_EDGE('',*,*,#47736,.T.);
#69417=ORIENTED_EDGE('',*,*,#51048,.F.);
#69418=ORIENTED_EDGE('',*,*,#49154,.F.);
#69419=ORIENTED_EDGE('',*,*,#51046,.T.);
#69420=ORIENTED_EDGE('',*,*,#51047,.T.);
#69421=ORIENTED_EDGE('',*,*,#50244,.F.);
#69422=ORIENTED_EDGE('',*,*,#51049,.F.);
#69423=ORIENTED_EDGE('',*,*,#46312,.F.);
#69424=ORIENTED_EDGE('',*,*,#51048,.T.);
#69425=ORIENTED_EDGE('',*,*,#47735,.F.);
#69426=ORIENTED_EDGE('',*,*,#51050,.F.);
#69427=ORIENTED_EDGE('',*,*,#49155,.F.);
#69428=ORIENTED_EDGE('',*,*,#51049,.T.);
#69429=ORIENTED_EDGE('',*,*,#49150,.F.);
#69430=ORIENTED_EDGE('',*,*,#51051,.F.);
#69431=ORIENTED_EDGE('',*,*,#46313,.F.);
#69432=ORIENTED_EDGE('',*,*,#51050,.T.);
#69433=ORIENTED_EDGE('',*,*,#47747,.F.);
#69434=ORIENTED_EDGE('',*,*,#51052,.F.);
#69435=ORIENTED_EDGE('',*,*,#49156,.F.);
#69436=ORIENTED_EDGE('',*,*,#51051,.T.);
#69437=ORIENTED_EDGE('',*,*,#49149,.F.);
#69438=ORIENTED_EDGE('',*,*,#51053,.F.);
#69439=ORIENTED_EDGE('',*,*,#47743,.F.);
#69440=ORIENTED_EDGE('',*,*,#51052,.T.);
#69441=ORIENTED_EDGE('',*,*,#47731,.F.);
#69442=ORIENTED_EDGE('',*,*,#51054,.F.);
#69443=ORIENTED_EDGE('',*,*,#49157,.F.);
#69444=ORIENTED_EDGE('',*,*,#51053,.T.);
#69445=ORIENTED_EDGE('',*,*,#49160,.F.);
#69446=ORIENTED_EDGE('',*,*,#51055,.F.);
#69447=ORIENTED_EDGE('',*,*,#47722,.F.);
#69448=ORIENTED_EDGE('',*,*,#51054,.T.);
#69449=ORIENTED_EDGE('',*,*,#47749,.F.);
#69450=ORIENTED_EDGE('',*,*,#51056,.F.);
#69451=ORIENTED_EDGE('',*,*,#49158,.F.);
#69452=ORIENTED_EDGE('',*,*,#51055,.T.);
#69453=ORIENTED_EDGE('',*,*,#49159,.F.);
#69454=ORIENTED_EDGE('',*,*,#51056,.T.);
#69455=ORIENTED_EDGE('',*,*,#47727,.F.);
#69456=ORIENTED_EDGE('',*,*,#47723,.T.);
#69457=ORIENTED_EDGE('',*,*,#51057,.F.);
#69458=ORIENTED_EDGE('',*,*,#49199,.F.);
#69459=ORIENTED_EDGE('',*,*,#51058,.F.);
#69460=ORIENTED_EDGE('',*,*,#47679,.F.);
#69461=ORIENTED_EDGE('',*,*,#51058,.T.);
#69462=ORIENTED_EDGE('',*,*,#49198,.F.);
#69463=ORIENTED_EDGE('',*,*,#51059,.F.);
#69464=ORIENTED_EDGE('',*,*,#47688,.F.);
#69465=ORIENTED_EDGE('',*,*,#47678,.T.);
#69466=ORIENTED_EDGE('',*,*,#47682,.F.);
#69467=ORIENTED_EDGE('',*,*,#51060,.F.);
#69468=ORIENTED_EDGE('',*,*,#49200,.F.);
#69469=ORIENTED_EDGE('',*,*,#51057,.T.);
#69470=ORIENTED_EDGE('',*,*,#51059,.T.);
#69471=ORIENTED_EDGE('',*,*,#49197,.F.);
#69472=ORIENTED_EDGE('',*,*,#51061,.F.);
#69473=ORIENTED_EDGE('',*,*,#47673,.F.);
#69474=ORIENTED_EDGE('',*,*,#51060,.T.);
#69475=ORIENTED_EDGE('',*,*,#47686,.F.);
#69476=ORIENTED_EDGE('',*,*,#51062,.F.);
#69477=ORIENTED_EDGE('',*,*,#49189,.F.);
#69478=ORIENTED_EDGE('',*,*,#51061,.T.);
#69479=ORIENTED_EDGE('',*,*,#49196,.F.);
#69480=ORIENTED_EDGE('',*,*,#51063,.F.);
#69481=ORIENTED_EDGE('',*,*,#47690,.F.);
#69482=ORIENTED_EDGE('',*,*,#51062,.T.);
#69483=ORIENTED_EDGE('',*,*,#46069,.F.);
#69484=ORIENTED_EDGE('',*,*,#51064,.F.);
#69485=ORIENTED_EDGE('',*,*,#49190,.F.);
#69486=ORIENTED_EDGE('',*,*,#51063,.T.);
#69487=ORIENTED_EDGE('',*,*,#49195,.F.);
#69488=ORIENTED_EDGE('',*,*,#51065,.F.);
#69489=ORIENTED_EDGE('',*,*,#47665,.T.);
#69490=ORIENTED_EDGE('',*,*,#47669,.F.);
#69491=ORIENTED_EDGE('',*,*,#51064,.T.);
#69492=ORIENTED_EDGE('',*,*,#46068,.F.);
#69493=ORIENTED_EDGE('',*,*,#51066,.F.);
#69494=ORIENTED_EDGE('',*,*,#50245,.F.);
#69495=ORIENTED_EDGE('',*,*,#51065,.T.);
#69496=ORIENTED_EDGE('',*,*,#49194,.F.);
#69497=ORIENTED_EDGE('',*,*,#51067,.F.);
#69498=ORIENTED_EDGE('',*,*,#47666,.F.);
#69499=ORIENTED_EDGE('',*,*,#51066,.T.);
#69500=ORIENTED_EDGE('',*,*,#46067,.F.);
#69501=ORIENTED_EDGE('',*,*,#51068,.F.);
#69502=ORIENTED_EDGE('',*,*,#49174,.F.);
#69503=ORIENTED_EDGE('',*,*,#51067,.T.);
#69504=ORIENTED_EDGE('',*,*,#49193,.F.);
#69505=ORIENTED_EDGE('',*,*,#51069,.F.);
#69506=ORIENTED_EDGE('',*,*,#47684,.F.);
#69507=ORIENTED_EDGE('',*,*,#51068,.T.);
#69508=ORIENTED_EDGE('',*,*,#46066,.F.);
#69509=ORIENTED_EDGE('',*,*,#51070,.F.);
#69510=ORIENTED_EDGE('',*,*,#50247,.F.);
#69511=ORIENTED_EDGE('',*,*,#51069,.T.);
#69512=ORIENTED_EDGE('',*,*,#49192,.F.);
#69513=ORIENTED_EDGE('',*,*,#51071,.F.);
#69514=ORIENTED_EDGE('',*,*,#46303,.F.);
#69515=ORIENTED_EDGE('',*,*,#51070,.T.);
#69516=ORIENTED_EDGE('',*,*,#46065,.F.);
#69517=ORIENTED_EDGE('',*,*,#51072,.F.);
#69518=ORIENTED_EDGE('',*,*,#49180,.F.);
#69519=ORIENTED_EDGE('',*,*,#51071,.T.);
#69520=ORIENTED_EDGE('',*,*,#50246,.F.);
#69521=ORIENTED_EDGE('',*,*,#51073,.F.);
#69522=ORIENTED_EDGE('',*,*,#46304,.F.);
#69523=ORIENTED_EDGE('',*,*,#51072,.T.);
#69524=ORIENTED_EDGE('',*,*,#47715,.F.);
#69525=ORIENTED_EDGE('',*,*,#51074,.F.);
#69526=ORIENTED_EDGE('',*,*,#49181,.F.);
#69527=ORIENTED_EDGE('',*,*,#51073,.T.);
#69528=ORIENTED_EDGE('',*,*,#49176,.F.);
#69529=ORIENTED_EDGE('',*,*,#51075,.F.);
#69530=ORIENTED_EDGE('',*,*,#46305,.F.);
#69531=ORIENTED_EDGE('',*,*,#47710,.F.);
#69532=ORIENTED_EDGE('',*,*,#47706,.T.);
#69533=ORIENTED_EDGE('',*,*,#51076,.F.);
#69534=ORIENTED_EDGE('',*,*,#49182,.F.);
#69535=ORIENTED_EDGE('',*,*,#51074,.T.);
#69536=ORIENTED_EDGE('',*,*,#51075,.T.);
#69537=ORIENTED_EDGE('',*,*,#50248,.F.);
#69538=ORIENTED_EDGE('',*,*,#51077,.F.);
#69539=ORIENTED_EDGE('',*,*,#46306,.F.);
#69540=ORIENTED_EDGE('',*,*,#51076,.T.);
#69541=ORIENTED_EDGE('',*,*,#47705,.F.);
#69542=ORIENTED_EDGE('',*,*,#51078,.F.);
#69543=ORIENTED_EDGE('',*,*,#49183,.F.);
#69544=ORIENTED_EDGE('',*,*,#51077,.T.);
#69545=ORIENTED_EDGE('',*,*,#49178,.F.);
#69546=ORIENTED_EDGE('',*,*,#51079,.F.);
#69547=ORIENTED_EDGE('',*,*,#46307,.F.);
#69548=ORIENTED_EDGE('',*,*,#51078,.T.);
#69549=ORIENTED_EDGE('',*,*,#47717,.F.);
#69550=ORIENTED_EDGE('',*,*,#51080,.F.);
#69551=ORIENTED_EDGE('',*,*,#49184,.F.);
#69552=ORIENTED_EDGE('',*,*,#51079,.T.);
#69553=ORIENTED_EDGE('',*,*,#49177,.F.);
#69554=ORIENTED_EDGE('',*,*,#51081,.F.);
#69555=ORIENTED_EDGE('',*,*,#47713,.F.);
#69556=ORIENTED_EDGE('',*,*,#51080,.T.);
#69557=ORIENTED_EDGE('',*,*,#47701,.F.);
#69558=ORIENTED_EDGE('',*,*,#51082,.F.);
#69559=ORIENTED_EDGE('',*,*,#49185,.F.);
#69560=ORIENTED_EDGE('',*,*,#51081,.T.);
#69561=ORIENTED_EDGE('',*,*,#49188,.F.);
#69562=ORIENTED_EDGE('',*,*,#51083,.F.);
#69563=ORIENTED_EDGE('',*,*,#47692,.F.);
#69564=ORIENTED_EDGE('',*,*,#51082,.T.);
#69565=ORIENTED_EDGE('',*,*,#47719,.F.);
#69566=ORIENTED_EDGE('',*,*,#51084,.F.);
#69567=ORIENTED_EDGE('',*,*,#49186,.F.);
#69568=ORIENTED_EDGE('',*,*,#51083,.T.);
#69569=ORIENTED_EDGE('',*,*,#49187,.F.);
#69570=ORIENTED_EDGE('',*,*,#51084,.T.);
#69571=ORIENTED_EDGE('',*,*,#47697,.F.);
#69572=ORIENTED_EDGE('',*,*,#47693,.T.);
#69573=ORIENTED_EDGE('',*,*,#51085,.F.);
#69574=ORIENTED_EDGE('',*,*,#49227,.F.);
#69575=ORIENTED_EDGE('',*,*,#51086,.F.);
#69576=ORIENTED_EDGE('',*,*,#47649,.F.);
#69577=ORIENTED_EDGE('',*,*,#51086,.T.);
#69578=ORIENTED_EDGE('',*,*,#49226,.F.);
#69579=ORIENTED_EDGE('',*,*,#51087,.F.);
#69580=ORIENTED_EDGE('',*,*,#47658,.F.);
#69581=ORIENTED_EDGE('',*,*,#47648,.T.);
#69582=ORIENTED_EDGE('',*,*,#47652,.F.);
#69583=ORIENTED_EDGE('',*,*,#51088,.F.);
#69584=ORIENTED_EDGE('',*,*,#49228,.F.);
#69585=ORIENTED_EDGE('',*,*,#51085,.T.);
#69586=ORIENTED_EDGE('',*,*,#51087,.T.);
#69587=ORIENTED_EDGE('',*,*,#49225,.F.);
#69588=ORIENTED_EDGE('',*,*,#51089,.F.);
#69589=ORIENTED_EDGE('',*,*,#47643,.F.);
#69590=ORIENTED_EDGE('',*,*,#51088,.T.);
#69591=ORIENTED_EDGE('',*,*,#47656,.F.);
#69592=ORIENTED_EDGE('',*,*,#51090,.F.);
#69593=ORIENTED_EDGE('',*,*,#49217,.F.);
#69594=ORIENTED_EDGE('',*,*,#51089,.T.);
#69595=ORIENTED_EDGE('',*,*,#49224,.F.);
#69596=ORIENTED_EDGE('',*,*,#51091,.F.);
#69597=ORIENTED_EDGE('',*,*,#47660,.F.);
#69598=ORIENTED_EDGE('',*,*,#51090,.T.);
#69599=ORIENTED_EDGE('',*,*,#46075,.F.);
#69600=ORIENTED_EDGE('',*,*,#51092,.F.);
#69601=ORIENTED_EDGE('',*,*,#49218,.F.);
#69602=ORIENTED_EDGE('',*,*,#51091,.T.);
#69603=ORIENTED_EDGE('',*,*,#49223,.F.);
#69604=ORIENTED_EDGE('',*,*,#51093,.F.);
#69605=ORIENTED_EDGE('',*,*,#47635,.T.);
#69606=ORIENTED_EDGE('',*,*,#47639,.F.);
#69607=ORIENTED_EDGE('',*,*,#51092,.T.);
#69608=ORIENTED_EDGE('',*,*,#46074,.F.);
#69609=ORIENTED_EDGE('',*,*,#51094,.F.);
#69610=ORIENTED_EDGE('',*,*,#50249,.F.);
#69611=ORIENTED_EDGE('',*,*,#51093,.T.);
#69612=ORIENTED_EDGE('',*,*,#49222,.F.);
#69613=ORIENTED_EDGE('',*,*,#51095,.F.);
#69614=ORIENTED_EDGE('',*,*,#47636,.F.);
#69615=ORIENTED_EDGE('',*,*,#51094,.T.);
#69616=ORIENTED_EDGE('',*,*,#46073,.F.);
#69617=ORIENTED_EDGE('',*,*,#51096,.F.);
#69618=ORIENTED_EDGE('',*,*,#49202,.F.);
#69619=ORIENTED_EDGE('',*,*,#51095,.T.);
#69620=ORIENTED_EDGE('',*,*,#49221,.F.);
#69621=ORIENTED_EDGE('',*,*,#51097,.F.);
#69622=ORIENTED_EDGE('',*,*,#47654,.F.);
#69623=ORIENTED_EDGE('',*,*,#51096,.T.);
#69624=ORIENTED_EDGE('',*,*,#46072,.F.);
#69625=ORIENTED_EDGE('',*,*,#51098,.F.);
#69626=ORIENTED_EDGE('',*,*,#50251,.F.);
#69627=ORIENTED_EDGE('',*,*,#51097,.T.);
#69628=ORIENTED_EDGE('',*,*,#49220,.F.);
#69629=ORIENTED_EDGE('',*,*,#51099,.F.);
#69630=ORIENTED_EDGE('',*,*,#46297,.F.);
#69631=ORIENTED_EDGE('',*,*,#51098,.T.);
#69632=ORIENTED_EDGE('',*,*,#46071,.F.);
#69633=ORIENTED_EDGE('',*,*,#51100,.F.);
#69634=ORIENTED_EDGE('',*,*,#49208,.F.);
#69635=ORIENTED_EDGE('',*,*,#51099,.T.);
#69636=ORIENTED_EDGE('',*,*,#50250,.F.);
#69637=ORIENTED_EDGE('',*,*,#51101,.F.);
#69638=ORIENTED_EDGE('',*,*,#46298,.F.);
#69639=ORIENTED_EDGE('',*,*,#51100,.T.);
#69640=ORIENTED_EDGE('',*,*,#47685,.F.);
#69641=ORIENTED_EDGE('',*,*,#51102,.F.);
#69642=ORIENTED_EDGE('',*,*,#49209,.F.);
#69643=ORIENTED_EDGE('',*,*,#51101,.T.);
#69644=ORIENTED_EDGE('',*,*,#49204,.F.);
#69645=ORIENTED_EDGE('',*,*,#51103,.F.);
#69646=ORIENTED_EDGE('',*,*,#46299,.F.);
#69647=ORIENTED_EDGE('',*,*,#47680,.F.);
#69648=ORIENTED_EDGE('',*,*,#47676,.T.);
#69649=ORIENTED_EDGE('',*,*,#51104,.F.);
#69650=ORIENTED_EDGE('',*,*,#49210,.F.);
#69651=ORIENTED_EDGE('',*,*,#51102,.T.);
#69652=ORIENTED_EDGE('',*,*,#51103,.T.);
#69653=ORIENTED_EDGE('',*,*,#50252,.F.);
#69654=ORIENTED_EDGE('',*,*,#51105,.F.);
#69655=ORIENTED_EDGE('',*,*,#46300,.F.);
#69656=ORIENTED_EDGE('',*,*,#51104,.T.);
#69657=ORIENTED_EDGE('',*,*,#47675,.F.);
#69658=ORIENTED_EDGE('',*,*,#51106,.F.);
#69659=ORIENTED_EDGE('',*,*,#49211,.F.);
#69660=ORIENTED_EDGE('',*,*,#51105,.T.);
#69661=ORIENTED_EDGE('',*,*,#49206,.F.);
#69662=ORIENTED_EDGE('',*,*,#51107,.F.);
#69663=ORIENTED_EDGE('',*,*,#46301,.F.);
#69664=ORIENTED_EDGE('',*,*,#51106,.T.);
#69665=ORIENTED_EDGE('',*,*,#47687,.F.);
#69666=ORIENTED_EDGE('',*,*,#51108,.F.);
#69667=ORIENTED_EDGE('',*,*,#49212,.F.);
#69668=ORIENTED_EDGE('',*,*,#51107,.T.);
#69669=ORIENTED_EDGE('',*,*,#49205,.F.);
#69670=ORIENTED_EDGE('',*,*,#51109,.F.);
#69671=ORIENTED_EDGE('',*,*,#47683,.F.);
#69672=ORIENTED_EDGE('',*,*,#51108,.T.);
#69673=ORIENTED_EDGE('',*,*,#47671,.F.);
#69674=ORIENTED_EDGE('',*,*,#51110,.F.);
#69675=ORIENTED_EDGE('',*,*,#49213,.F.);
#69676=ORIENTED_EDGE('',*,*,#51109,.T.);
#69677=ORIENTED_EDGE('',*,*,#49216,.F.);
#69678=ORIENTED_EDGE('',*,*,#51111,.F.);
#69679=ORIENTED_EDGE('',*,*,#47662,.F.);
#69680=ORIENTED_EDGE('',*,*,#51110,.T.);
#69681=ORIENTED_EDGE('',*,*,#47689,.F.);
#69682=ORIENTED_EDGE('',*,*,#51112,.F.);
#69683=ORIENTED_EDGE('',*,*,#49214,.F.);
#69684=ORIENTED_EDGE('',*,*,#51111,.T.);
#69685=ORIENTED_EDGE('',*,*,#49215,.F.);
#69686=ORIENTED_EDGE('',*,*,#51112,.T.);
#69687=ORIENTED_EDGE('',*,*,#47667,.F.);
#69688=ORIENTED_EDGE('',*,*,#47663,.T.);
#69689=ORIENTED_EDGE('',*,*,#51113,.F.);
#69690=ORIENTED_EDGE('',*,*,#49255,.F.);
#69691=ORIENTED_EDGE('',*,*,#51114,.F.);
#69692=ORIENTED_EDGE('',*,*,#47619,.F.);
#69693=ORIENTED_EDGE('',*,*,#51114,.T.);
#69694=ORIENTED_EDGE('',*,*,#49254,.F.);
#69695=ORIENTED_EDGE('',*,*,#51115,.F.);
#69696=ORIENTED_EDGE('',*,*,#47628,.F.);
#69697=ORIENTED_EDGE('',*,*,#47618,.T.);
#69698=ORIENTED_EDGE('',*,*,#47622,.F.);
#69699=ORIENTED_EDGE('',*,*,#51116,.F.);
#69700=ORIENTED_EDGE('',*,*,#49256,.F.);
#69701=ORIENTED_EDGE('',*,*,#51113,.T.);
#69702=ORIENTED_EDGE('',*,*,#51115,.T.);
#69703=ORIENTED_EDGE('',*,*,#49253,.F.);
#69704=ORIENTED_EDGE('',*,*,#51117,.F.);
#69705=ORIENTED_EDGE('',*,*,#47613,.F.);
#69706=ORIENTED_EDGE('',*,*,#51116,.T.);
#69707=ORIENTED_EDGE('',*,*,#47626,.F.);
#69708=ORIENTED_EDGE('',*,*,#51118,.F.);
#69709=ORIENTED_EDGE('',*,*,#49245,.F.);
#69710=ORIENTED_EDGE('',*,*,#51117,.T.);
#69711=ORIENTED_EDGE('',*,*,#49252,.F.);
#69712=ORIENTED_EDGE('',*,*,#51119,.F.);
#69713=ORIENTED_EDGE('',*,*,#47630,.F.);
#69714=ORIENTED_EDGE('',*,*,#51118,.T.);
#69715=ORIENTED_EDGE('',*,*,#46081,.F.);
#69716=ORIENTED_EDGE('',*,*,#51120,.F.);
#69717=ORIENTED_EDGE('',*,*,#49246,.F.);
#69718=ORIENTED_EDGE('',*,*,#51119,.T.);
#69719=ORIENTED_EDGE('',*,*,#49251,.F.);
#69720=ORIENTED_EDGE('',*,*,#51121,.F.);
#69721=ORIENTED_EDGE('',*,*,#47605,.T.);
#69722=ORIENTED_EDGE('',*,*,#47609,.F.);
#69723=ORIENTED_EDGE('',*,*,#51120,.T.);
#69724=ORIENTED_EDGE('',*,*,#46080,.F.);
#69725=ORIENTED_EDGE('',*,*,#51122,.F.);
#69726=ORIENTED_EDGE('',*,*,#50253,.F.);
#69727=ORIENTED_EDGE('',*,*,#51121,.T.);
#69728=ORIENTED_EDGE('',*,*,#49250,.F.);
#69729=ORIENTED_EDGE('',*,*,#51123,.F.);
#69730=ORIENTED_EDGE('',*,*,#47606,.F.);
#69731=ORIENTED_EDGE('',*,*,#51122,.T.);
#69732=ORIENTED_EDGE('',*,*,#46079,.F.);
#69733=ORIENTED_EDGE('',*,*,#51124,.F.);
#69734=ORIENTED_EDGE('',*,*,#49230,.F.);
#69735=ORIENTED_EDGE('',*,*,#51123,.T.);
#69736=ORIENTED_EDGE('',*,*,#49249,.F.);
#69737=ORIENTED_EDGE('',*,*,#51125,.F.);
#69738=ORIENTED_EDGE('',*,*,#47624,.F.);
#69739=ORIENTED_EDGE('',*,*,#51124,.T.);
#69740=ORIENTED_EDGE('',*,*,#46078,.F.);
#69741=ORIENTED_EDGE('',*,*,#51126,.F.);
#69742=ORIENTED_EDGE('',*,*,#50255,.F.);
#69743=ORIENTED_EDGE('',*,*,#51125,.T.);
#69744=ORIENTED_EDGE('',*,*,#49248,.F.);
#69745=ORIENTED_EDGE('',*,*,#51127,.F.);
#69746=ORIENTED_EDGE('',*,*,#46291,.F.);
#69747=ORIENTED_EDGE('',*,*,#51126,.T.);
#69748=ORIENTED_EDGE('',*,*,#46077,.F.);
#69749=ORIENTED_EDGE('',*,*,#51128,.F.);
#69750=ORIENTED_EDGE('',*,*,#49236,.F.);
#69751=ORIENTED_EDGE('',*,*,#51127,.T.);
#69752=ORIENTED_EDGE('',*,*,#50254,.F.);
#69753=ORIENTED_EDGE('',*,*,#51129,.F.);
#69754=ORIENTED_EDGE('',*,*,#46292,.F.);
#69755=ORIENTED_EDGE('',*,*,#51128,.T.);
#69756=ORIENTED_EDGE('',*,*,#47655,.F.);
#69757=ORIENTED_EDGE('',*,*,#51130,.F.);
#69758=ORIENTED_EDGE('',*,*,#49237,.F.);
#69759=ORIENTED_EDGE('',*,*,#51129,.T.);
#69760=ORIENTED_EDGE('',*,*,#49232,.F.);
#69761=ORIENTED_EDGE('',*,*,#51131,.F.);
#69762=ORIENTED_EDGE('',*,*,#46293,.F.);
#69763=ORIENTED_EDGE('',*,*,#47650,.F.);
#69764=ORIENTED_EDGE('',*,*,#47646,.T.);
#69765=ORIENTED_EDGE('',*,*,#51132,.F.);
#69766=ORIENTED_EDGE('',*,*,#49238,.F.);
#69767=ORIENTED_EDGE('',*,*,#51130,.T.);
#69768=ORIENTED_EDGE('',*,*,#51131,.T.);
#69769=ORIENTED_EDGE('',*,*,#50256,.F.);
#69770=ORIENTED_EDGE('',*,*,#51133,.F.);
#69771=ORIENTED_EDGE('',*,*,#46294,.F.);
#69772=ORIENTED_EDGE('',*,*,#51132,.T.);
#69773=ORIENTED_EDGE('',*,*,#47645,.F.);
#69774=ORIENTED_EDGE('',*,*,#51134,.F.);
#69775=ORIENTED_EDGE('',*,*,#49239,.F.);
#69776=ORIENTED_EDGE('',*,*,#51133,.T.);
#69777=ORIENTED_EDGE('',*,*,#49234,.F.);
#69778=ORIENTED_EDGE('',*,*,#51135,.F.);
#69779=ORIENTED_EDGE('',*,*,#46295,.F.);
#69780=ORIENTED_EDGE('',*,*,#51134,.T.);
#69781=ORIENTED_EDGE('',*,*,#47657,.F.);
#69782=ORIENTED_EDGE('',*,*,#51136,.F.);
#69783=ORIENTED_EDGE('',*,*,#49240,.F.);
#69784=ORIENTED_EDGE('',*,*,#51135,.T.);
#69785=ORIENTED_EDGE('',*,*,#49233,.F.);
#69786=ORIENTED_EDGE('',*,*,#51137,.F.);
#69787=ORIENTED_EDGE('',*,*,#47653,.F.);
#69788=ORIENTED_EDGE('',*,*,#51136,.T.);
#69789=ORIENTED_EDGE('',*,*,#47641,.F.);
#69790=ORIENTED_EDGE('',*,*,#51138,.F.);
#69791=ORIENTED_EDGE('',*,*,#49241,.F.);
#69792=ORIENTED_EDGE('',*,*,#51137,.T.);
#69793=ORIENTED_EDGE('',*,*,#49244,.F.);
#69794=ORIENTED_EDGE('',*,*,#51139,.F.);
#69795=ORIENTED_EDGE('',*,*,#47632,.F.);
#69796=ORIENTED_EDGE('',*,*,#51138,.T.);
#69797=ORIENTED_EDGE('',*,*,#47659,.F.);
#69798=ORIENTED_EDGE('',*,*,#51140,.F.);
#69799=ORIENTED_EDGE('',*,*,#49242,.F.);
#69800=ORIENTED_EDGE('',*,*,#51139,.T.);
#69801=ORIENTED_EDGE('',*,*,#49243,.F.);
#69802=ORIENTED_EDGE('',*,*,#51140,.T.);
#69803=ORIENTED_EDGE('',*,*,#47637,.F.);
#69804=ORIENTED_EDGE('',*,*,#47633,.T.);
#69805=ORIENTED_EDGE('',*,*,#51141,.F.);
#69806=ORIENTED_EDGE('',*,*,#49283,.F.);
#69807=ORIENTED_EDGE('',*,*,#51142,.F.);
#69808=ORIENTED_EDGE('',*,*,#47589,.F.);
#69809=ORIENTED_EDGE('',*,*,#51142,.T.);
#69810=ORIENTED_EDGE('',*,*,#49282,.F.);
#69811=ORIENTED_EDGE('',*,*,#51143,.F.);
#69812=ORIENTED_EDGE('',*,*,#47598,.F.);
#69813=ORIENTED_EDGE('',*,*,#47588,.T.);
#69814=ORIENTED_EDGE('',*,*,#47592,.F.);
#69815=ORIENTED_EDGE('',*,*,#51144,.F.);
#69816=ORIENTED_EDGE('',*,*,#49284,.F.);
#69817=ORIENTED_EDGE('',*,*,#51141,.T.);
#69818=ORIENTED_EDGE('',*,*,#51143,.T.);
#69819=ORIENTED_EDGE('',*,*,#49281,.F.);
#69820=ORIENTED_EDGE('',*,*,#51145,.F.);
#69821=ORIENTED_EDGE('',*,*,#47583,.F.);
#69822=ORIENTED_EDGE('',*,*,#51144,.T.);
#69823=ORIENTED_EDGE('',*,*,#47596,.F.);
#69824=ORIENTED_EDGE('',*,*,#51146,.F.);
#69825=ORIENTED_EDGE('',*,*,#49273,.F.);
#69826=ORIENTED_EDGE('',*,*,#51145,.T.);
#69827=ORIENTED_EDGE('',*,*,#49280,.F.);
#69828=ORIENTED_EDGE('',*,*,#51147,.F.);
#69829=ORIENTED_EDGE('',*,*,#47600,.F.);
#69830=ORIENTED_EDGE('',*,*,#51146,.T.);
#69831=ORIENTED_EDGE('',*,*,#46087,.F.);
#69832=ORIENTED_EDGE('',*,*,#51148,.F.);
#69833=ORIENTED_EDGE('',*,*,#49274,.F.);
#69834=ORIENTED_EDGE('',*,*,#51147,.T.);
#69835=ORIENTED_EDGE('',*,*,#49279,.F.);
#69836=ORIENTED_EDGE('',*,*,#51149,.F.);
#69837=ORIENTED_EDGE('',*,*,#47575,.T.);
#69838=ORIENTED_EDGE('',*,*,#47579,.F.);
#69839=ORIENTED_EDGE('',*,*,#51148,.T.);
#69840=ORIENTED_EDGE('',*,*,#46086,.F.);
#69841=ORIENTED_EDGE('',*,*,#51150,.F.);
#69842=ORIENTED_EDGE('',*,*,#50257,.F.);
#69843=ORIENTED_EDGE('',*,*,#51149,.T.);
#69844=ORIENTED_EDGE('',*,*,#49278,.F.);
#69845=ORIENTED_EDGE('',*,*,#51151,.F.);
#69846=ORIENTED_EDGE('',*,*,#47576,.F.);
#69847=ORIENTED_EDGE('',*,*,#51150,.T.);
#69848=ORIENTED_EDGE('',*,*,#46085,.F.);
#69849=ORIENTED_EDGE('',*,*,#51152,.F.);
#69850=ORIENTED_EDGE('',*,*,#49258,.F.);
#69851=ORIENTED_EDGE('',*,*,#51151,.T.);
#69852=ORIENTED_EDGE('',*,*,#49277,.F.);
#69853=ORIENTED_EDGE('',*,*,#51153,.F.);
#69854=ORIENTED_EDGE('',*,*,#47594,.F.);
#69855=ORIENTED_EDGE('',*,*,#51152,.T.);
#69856=ORIENTED_EDGE('',*,*,#46084,.F.);
#69857=ORIENTED_EDGE('',*,*,#51154,.F.);
#69858=ORIENTED_EDGE('',*,*,#50259,.F.);
#69859=ORIENTED_EDGE('',*,*,#51153,.T.);
#69860=ORIENTED_EDGE('',*,*,#49276,.F.);
#69861=ORIENTED_EDGE('',*,*,#51155,.F.);
#69862=ORIENTED_EDGE('',*,*,#46285,.F.);
#69863=ORIENTED_EDGE('',*,*,#51154,.T.);
#69864=ORIENTED_EDGE('',*,*,#46083,.F.);
#69865=ORIENTED_EDGE('',*,*,#51156,.F.);
#69866=ORIENTED_EDGE('',*,*,#49264,.F.);
#69867=ORIENTED_EDGE('',*,*,#51155,.T.);
#69868=ORIENTED_EDGE('',*,*,#50258,.F.);
#69869=ORIENTED_EDGE('',*,*,#51157,.F.);
#69870=ORIENTED_EDGE('',*,*,#46286,.F.);
#69871=ORIENTED_EDGE('',*,*,#51156,.T.);
#69872=ORIENTED_EDGE('',*,*,#47625,.F.);
#69873=ORIENTED_EDGE('',*,*,#51158,.F.);
#69874=ORIENTED_EDGE('',*,*,#49265,.F.);
#69875=ORIENTED_EDGE('',*,*,#51157,.T.);
#69876=ORIENTED_EDGE('',*,*,#49260,.F.);
#69877=ORIENTED_EDGE('',*,*,#51159,.F.);
#69878=ORIENTED_EDGE('',*,*,#46287,.F.);
#69879=ORIENTED_EDGE('',*,*,#47620,.F.);
#69880=ORIENTED_EDGE('',*,*,#47616,.T.);
#69881=ORIENTED_EDGE('',*,*,#51160,.F.);
#69882=ORIENTED_EDGE('',*,*,#49266,.F.);
#69883=ORIENTED_EDGE('',*,*,#51158,.T.);
#69884=ORIENTED_EDGE('',*,*,#51159,.T.);
#69885=ORIENTED_EDGE('',*,*,#50260,.F.);
#69886=ORIENTED_EDGE('',*,*,#51161,.F.);
#69887=ORIENTED_EDGE('',*,*,#46288,.F.);
#69888=ORIENTED_EDGE('',*,*,#51160,.T.);
#69889=ORIENTED_EDGE('',*,*,#47615,.F.);
#69890=ORIENTED_EDGE('',*,*,#51162,.F.);
#69891=ORIENTED_EDGE('',*,*,#49267,.F.);
#69892=ORIENTED_EDGE('',*,*,#51161,.T.);
#69893=ORIENTED_EDGE('',*,*,#49262,.F.);
#69894=ORIENTED_EDGE('',*,*,#51163,.F.);
#69895=ORIENTED_EDGE('',*,*,#46289,.F.);
#69896=ORIENTED_EDGE('',*,*,#51162,.T.);
#69897=ORIENTED_EDGE('',*,*,#47627,.F.);
#69898=ORIENTED_EDGE('',*,*,#51164,.F.);
#69899=ORIENTED_EDGE('',*,*,#49268,.F.);
#69900=ORIENTED_EDGE('',*,*,#51163,.T.);
#69901=ORIENTED_EDGE('',*,*,#49261,.F.);
#69902=ORIENTED_EDGE('',*,*,#51165,.F.);
#69903=ORIENTED_EDGE('',*,*,#47623,.F.);
#69904=ORIENTED_EDGE('',*,*,#51164,.T.);
#69905=ORIENTED_EDGE('',*,*,#47611,.F.);
#69906=ORIENTED_EDGE('',*,*,#51166,.F.);
#69907=ORIENTED_EDGE('',*,*,#49269,.F.);
#69908=ORIENTED_EDGE('',*,*,#51165,.T.);
#69909=ORIENTED_EDGE('',*,*,#49272,.F.);
#69910=ORIENTED_EDGE('',*,*,#51167,.F.);
#69911=ORIENTED_EDGE('',*,*,#47602,.F.);
#69912=ORIENTED_EDGE('',*,*,#51166,.T.);
#69913=ORIENTED_EDGE('',*,*,#47629,.F.);
#69914=ORIENTED_EDGE('',*,*,#51168,.F.);
#69915=ORIENTED_EDGE('',*,*,#49270,.F.);
#69916=ORIENTED_EDGE('',*,*,#51167,.T.);
#69917=ORIENTED_EDGE('',*,*,#49271,.F.);
#69918=ORIENTED_EDGE('',*,*,#51168,.T.);
#69919=ORIENTED_EDGE('',*,*,#47607,.F.);
#69920=ORIENTED_EDGE('',*,*,#47603,.T.);
#69921=ORIENTED_EDGE('',*,*,#51169,.F.);
#69922=ORIENTED_EDGE('',*,*,#49311,.F.);
#69923=ORIENTED_EDGE('',*,*,#51170,.F.);
#69924=ORIENTED_EDGE('',*,*,#47559,.F.);
#69925=ORIENTED_EDGE('',*,*,#51170,.T.);
#69926=ORIENTED_EDGE('',*,*,#49310,.F.);
#69927=ORIENTED_EDGE('',*,*,#51171,.F.);
#69928=ORIENTED_EDGE('',*,*,#47568,.F.);
#69929=ORIENTED_EDGE('',*,*,#47558,.T.);
#69930=ORIENTED_EDGE('',*,*,#47562,.F.);
#69931=ORIENTED_EDGE('',*,*,#51172,.F.);
#69932=ORIENTED_EDGE('',*,*,#49312,.F.);
#69933=ORIENTED_EDGE('',*,*,#51169,.T.);
#69934=ORIENTED_EDGE('',*,*,#51171,.T.);
#69935=ORIENTED_EDGE('',*,*,#49309,.F.);
#69936=ORIENTED_EDGE('',*,*,#51173,.F.);
#69937=ORIENTED_EDGE('',*,*,#47553,.F.);
#69938=ORIENTED_EDGE('',*,*,#51172,.T.);
#69939=ORIENTED_EDGE('',*,*,#47566,.F.);
#69940=ORIENTED_EDGE('',*,*,#51174,.F.);
#69941=ORIENTED_EDGE('',*,*,#49301,.F.);
#69942=ORIENTED_EDGE('',*,*,#51173,.T.);
#69943=ORIENTED_EDGE('',*,*,#49308,.F.);
#69944=ORIENTED_EDGE('',*,*,#51175,.F.);
#69945=ORIENTED_EDGE('',*,*,#47570,.F.);
#69946=ORIENTED_EDGE('',*,*,#51174,.T.);
#69947=ORIENTED_EDGE('',*,*,#46093,.F.);
#69948=ORIENTED_EDGE('',*,*,#51176,.F.);
#69949=ORIENTED_EDGE('',*,*,#49302,.F.);
#69950=ORIENTED_EDGE('',*,*,#51175,.T.);
#69951=ORIENTED_EDGE('',*,*,#49307,.F.);
#69952=ORIENTED_EDGE('',*,*,#51177,.F.);
#69953=ORIENTED_EDGE('',*,*,#47545,.T.);
#69954=ORIENTED_EDGE('',*,*,#47549,.F.);
#69955=ORIENTED_EDGE('',*,*,#51176,.T.);
#69956=ORIENTED_EDGE('',*,*,#46092,.F.);
#69957=ORIENTED_EDGE('',*,*,#51178,.F.);
#69958=ORIENTED_EDGE('',*,*,#50261,.F.);
#69959=ORIENTED_EDGE('',*,*,#51177,.T.);
#69960=ORIENTED_EDGE('',*,*,#49306,.F.);
#69961=ORIENTED_EDGE('',*,*,#51179,.F.);
#69962=ORIENTED_EDGE('',*,*,#47546,.F.);
#69963=ORIENTED_EDGE('',*,*,#51178,.T.);
#69964=ORIENTED_EDGE('',*,*,#46091,.F.);
#69965=ORIENTED_EDGE('',*,*,#51180,.F.);
#69966=ORIENTED_EDGE('',*,*,#49286,.F.);
#69967=ORIENTED_EDGE('',*,*,#51179,.T.);
#69968=ORIENTED_EDGE('',*,*,#49305,.F.);
#69969=ORIENTED_EDGE('',*,*,#51181,.F.);
#69970=ORIENTED_EDGE('',*,*,#47564,.F.);
#69971=ORIENTED_EDGE('',*,*,#51180,.T.);
#69972=ORIENTED_EDGE('',*,*,#46090,.F.);
#69973=ORIENTED_EDGE('',*,*,#51182,.F.);
#69974=ORIENTED_EDGE('',*,*,#50263,.F.);
#69975=ORIENTED_EDGE('',*,*,#51181,.T.);
#69976=ORIENTED_EDGE('',*,*,#49304,.F.);
#69977=ORIENTED_EDGE('',*,*,#51183,.F.);
#69978=ORIENTED_EDGE('',*,*,#46279,.F.);
#69979=ORIENTED_EDGE('',*,*,#51182,.T.);
#69980=ORIENTED_EDGE('',*,*,#46089,.F.);
#69981=ORIENTED_EDGE('',*,*,#51184,.F.);
#69982=ORIENTED_EDGE('',*,*,#49292,.F.);
#69983=ORIENTED_EDGE('',*,*,#51183,.T.);
#69984=ORIENTED_EDGE('',*,*,#50262,.F.);
#69985=ORIENTED_EDGE('',*,*,#51185,.F.);
#69986=ORIENTED_EDGE('',*,*,#46280,.F.);
#69987=ORIENTED_EDGE('',*,*,#51184,.T.);
#69988=ORIENTED_EDGE('',*,*,#47595,.F.);
#69989=ORIENTED_EDGE('',*,*,#51186,.F.);
#69990=ORIENTED_EDGE('',*,*,#49293,.F.);
#69991=ORIENTED_EDGE('',*,*,#51185,.T.);
#69992=ORIENTED_EDGE('',*,*,#49288,.F.);
#69993=ORIENTED_EDGE('',*,*,#51187,.F.);
#69994=ORIENTED_EDGE('',*,*,#46281,.F.);
#69995=ORIENTED_EDGE('',*,*,#47590,.F.);
#69996=ORIENTED_EDGE('',*,*,#47586,.T.);
#69997=ORIENTED_EDGE('',*,*,#51188,.F.);
#69998=ORIENTED_EDGE('',*,*,#49294,.F.);
#69999=ORIENTED_EDGE('',*,*,#51186,.T.);
#70000=ORIENTED_EDGE('',*,*,#51187,.T.);
#70001=ORIENTED_EDGE('',*,*,#50264,.F.);
#70002=ORIENTED_EDGE('',*,*,#51189,.F.);
#70003=ORIENTED_EDGE('',*,*,#46282,.F.);
#70004=ORIENTED_EDGE('',*,*,#51188,.T.);
#70005=ORIENTED_EDGE('',*,*,#47585,.F.);
#70006=ORIENTED_EDGE('',*,*,#51190,.F.);
#70007=ORIENTED_EDGE('',*,*,#49295,.F.);
#70008=ORIENTED_EDGE('',*,*,#51189,.T.);
#70009=ORIENTED_EDGE('',*,*,#49290,.F.);
#70010=ORIENTED_EDGE('',*,*,#51191,.F.);
#70011=ORIENTED_EDGE('',*,*,#46283,.F.);
#70012=ORIENTED_EDGE('',*,*,#51190,.T.);
#70013=ORIENTED_EDGE('',*,*,#47597,.F.);
#70014=ORIENTED_EDGE('',*,*,#51192,.F.);
#70015=ORIENTED_EDGE('',*,*,#49296,.F.);
#70016=ORIENTED_EDGE('',*,*,#51191,.T.);
#70017=ORIENTED_EDGE('',*,*,#49289,.F.);
#70018=ORIENTED_EDGE('',*,*,#51193,.F.);
#70019=ORIENTED_EDGE('',*,*,#47593,.F.);
#70020=ORIENTED_EDGE('',*,*,#51192,.T.);
#70021=ORIENTED_EDGE('',*,*,#47581,.F.);
#70022=ORIENTED_EDGE('',*,*,#51194,.F.);
#70023=ORIENTED_EDGE('',*,*,#49297,.F.);
#70024=ORIENTED_EDGE('',*,*,#51193,.T.);
#70025=ORIENTED_EDGE('',*,*,#49300,.F.);
#70026=ORIENTED_EDGE('',*,*,#51195,.F.);
#70027=ORIENTED_EDGE('',*,*,#47572,.F.);
#70028=ORIENTED_EDGE('',*,*,#51194,.T.);
#70029=ORIENTED_EDGE('',*,*,#47599,.F.);
#70030=ORIENTED_EDGE('',*,*,#51196,.F.);
#70031=ORIENTED_EDGE('',*,*,#49298,.F.);
#70032=ORIENTED_EDGE('',*,*,#51195,.T.);
#70033=ORIENTED_EDGE('',*,*,#49299,.F.);
#70034=ORIENTED_EDGE('',*,*,#51196,.T.);
#70035=ORIENTED_EDGE('',*,*,#47577,.F.);
#70036=ORIENTED_EDGE('',*,*,#47573,.T.);
#70037=ORIENTED_EDGE('',*,*,#51197,.F.);
#70038=ORIENTED_EDGE('',*,*,#49337,.F.);
#70039=ORIENTED_EDGE('',*,*,#51198,.F.);
#70040=ORIENTED_EDGE('',*,*,#47529,.F.);
#70041=ORIENTED_EDGE('',*,*,#51198,.T.);
#70042=ORIENTED_EDGE('',*,*,#49336,.F.);
#70043=ORIENTED_EDGE('',*,*,#51199,.F.);
#70044=ORIENTED_EDGE('',*,*,#47538,.F.);
#70045=ORIENTED_EDGE('',*,*,#47528,.T.);
#70046=ORIENTED_EDGE('',*,*,#47532,.F.);
#70047=ORIENTED_EDGE('',*,*,#51200,.F.);
#70048=ORIENTED_EDGE('',*,*,#49338,.F.);
#70049=ORIENTED_EDGE('',*,*,#51197,.T.);
#70050=ORIENTED_EDGE('',*,*,#51199,.T.);
#70051=ORIENTED_EDGE('',*,*,#49335,.F.);
#70052=ORIENTED_EDGE('',*,*,#51201,.F.);
#70053=ORIENTED_EDGE('',*,*,#47523,.F.);
#70054=ORIENTED_EDGE('',*,*,#51200,.T.);
#70055=ORIENTED_EDGE('',*,*,#47536,.F.);
#70056=ORIENTED_EDGE('',*,*,#51202,.F.);
#70057=ORIENTED_EDGE('',*,*,#49327,.F.);
#70058=ORIENTED_EDGE('',*,*,#51201,.T.);
#70059=ORIENTED_EDGE('',*,*,#49334,.F.);
#70060=ORIENTED_EDGE('',*,*,#51203,.F.);
#70061=ORIENTED_EDGE('',*,*,#47540,.F.);
#70062=ORIENTED_EDGE('',*,*,#51202,.T.);
#70063=ORIENTED_EDGE('',*,*,#46099,.F.);
#70064=ORIENTED_EDGE('',*,*,#51204,.F.);
#70065=ORIENTED_EDGE('',*,*,#49328,.F.);
#70066=ORIENTED_EDGE('',*,*,#51203,.T.);
#70067=ORIENTED_EDGE('',*,*,#49333,.F.);
#70068=ORIENTED_EDGE('',*,*,#51205,.F.);
#70069=ORIENTED_EDGE('',*,*,#47515,.T.);
#70070=ORIENTED_EDGE('',*,*,#47519,.F.);
#70071=ORIENTED_EDGE('',*,*,#51204,.T.);
#70072=ORIENTED_EDGE('',*,*,#46098,.F.);
#70073=ORIENTED_EDGE('',*,*,#45897,.F.);
#70074=ORIENTED_EDGE('',*,*,#50265,.F.);
#70075=ORIENTED_EDGE('',*,*,#51205,.T.);
#70076=ORIENTED_EDGE('',*,*,#49332,.F.);
#70077=ORIENTED_EDGE('',*,*,#51206,.F.);
#70078=ORIENTED_EDGE('',*,*,#47516,.F.);
#70079=ORIENTED_EDGE('',*,*,#51206,.T.);
#70080=ORIENTED_EDGE('',*,*,#49331,.F.);
#70081=ORIENTED_EDGE('',*,*,#51207,.F.);
#70082=ORIENTED_EDGE('',*,*,#47534,.F.);
#70083=ORIENTED_EDGE('',*,*,#45895,.T.);
#70084=ORIENTED_EDGE('',*,*,#46096,.F.);
#70085=ORIENTED_EDGE('',*,*,#51208,.F.);
#70086=ORIENTED_EDGE('',*,*,#50267,.F.);
#70087=ORIENTED_EDGE('',*,*,#51207,.T.);
#70088=ORIENTED_EDGE('',*,*,#49330,.F.);
#70089=ORIENTED_EDGE('',*,*,#51209,.F.);
#70090=ORIENTED_EDGE('',*,*,#46634,.F.);
#70091=ORIENTED_EDGE('',*,*,#51208,.T.);
#70092=ORIENTED_EDGE('',*,*,#46095,.F.);
#70093=ORIENTED_EDGE('',*,*,#51210,.F.);
#70094=ORIENTED_EDGE('',*,*,#49318,.F.);
#70095=ORIENTED_EDGE('',*,*,#51209,.T.);
#70096=ORIENTED_EDGE('',*,*,#50266,.F.);
#70097=ORIENTED_EDGE('',*,*,#45893,.F.);
#70098=ORIENTED_EDGE('',*,*,#46635,.F.);
#70099=ORIENTED_EDGE('',*,*,#51210,.T.);
#70100=ORIENTED_EDGE('',*,*,#47565,.F.);
#70101=ORIENTED_EDGE('',*,*,#51211,.F.);
#70102=ORIENTED_EDGE('',*,*,#49319,.F.);
#70103=ORIENTED_EDGE('',*,*,#47560,.F.);
#70104=ORIENTED_EDGE('',*,*,#47556,.T.);
#70105=ORIENTED_EDGE('',*,*,#51212,.F.);
#70106=ORIENTED_EDGE('',*,*,#49320,.F.);
#70107=ORIENTED_EDGE('',*,*,#51211,.T.);
#70108=ORIENTED_EDGE('',*,*,#45891,.T.);
#70109=ORIENTED_EDGE('',*,*,#50268,.F.);
#70110=ORIENTED_EDGE('',*,*,#51213,.F.);
#70111=ORIENTED_EDGE('',*,*,#46276,.F.);
#70112=ORIENTED_EDGE('',*,*,#51212,.T.);
#70113=ORIENTED_EDGE('',*,*,#47555,.F.);
#70114=ORIENTED_EDGE('',*,*,#51214,.F.);
#70115=ORIENTED_EDGE('',*,*,#49321,.F.);
#70116=ORIENTED_EDGE('',*,*,#51213,.T.);
#70117=ORIENTED_EDGE('',*,*,#49316,.F.);
#70118=ORIENTED_EDGE('',*,*,#51215,.F.);
#70119=ORIENTED_EDGE('',*,*,#46277,.F.);
#70120=ORIENTED_EDGE('',*,*,#51214,.T.);
#70121=ORIENTED_EDGE('',*,*,#47567,.F.);
#70122=ORIENTED_EDGE('',*,*,#51216,.F.);
#70123=ORIENTED_EDGE('',*,*,#49322,.F.);
#70124=ORIENTED_EDGE('',*,*,#51215,.T.);
#70125=ORIENTED_EDGE('',*,*,#49315,.F.);
#70126=ORIENTED_EDGE('',*,*,#51217,.F.);
#70127=ORIENTED_EDGE('',*,*,#47563,.F.);
#70128=ORIENTED_EDGE('',*,*,#51216,.T.);
#70129=ORIENTED_EDGE('',*,*,#47551,.F.);
#70130=ORIENTED_EDGE('',*,*,#51218,.F.);
#70131=ORIENTED_EDGE('',*,*,#49323,.F.);
#70132=ORIENTED_EDGE('',*,*,#51217,.T.);
#70133=ORIENTED_EDGE('',*,*,#49326,.F.);
#70134=ORIENTED_EDGE('',*,*,#51219,.F.);
#70135=ORIENTED_EDGE('',*,*,#47542,.F.);
#70136=ORIENTED_EDGE('',*,*,#51218,.T.);
#70137=ORIENTED_EDGE('',*,*,#47569,.F.);
#70138=ORIENTED_EDGE('',*,*,#51220,.F.);
#70139=ORIENTED_EDGE('',*,*,#49324,.F.);
#70140=ORIENTED_EDGE('',*,*,#51219,.T.);
#70141=ORIENTED_EDGE('',*,*,#49325,.F.);
#70142=ORIENTED_EDGE('',*,*,#51220,.T.);
#70143=ORIENTED_EDGE('',*,*,#47547,.F.);
#70144=ORIENTED_EDGE('',*,*,#47543,.T.);
#70145=ORIENTED_EDGE('',*,*,#51221,.F.);
#70146=ORIENTED_EDGE('',*,*,#49365,.F.);
#70147=ORIENTED_EDGE('',*,*,#51222,.F.);
#70148=ORIENTED_EDGE('',*,*,#47499,.F.);
#70149=ORIENTED_EDGE('',*,*,#51222,.T.);
#70150=ORIENTED_EDGE('',*,*,#49364,.F.);
#70151=ORIENTED_EDGE('',*,*,#51223,.F.);
#70152=ORIENTED_EDGE('',*,*,#47508,.F.);
#70153=ORIENTED_EDGE('',*,*,#47498,.T.);
#70154=ORIENTED_EDGE('',*,*,#47502,.F.);
#70155=ORIENTED_EDGE('',*,*,#51224,.F.);
#70156=ORIENTED_EDGE('',*,*,#49366,.F.);
#70157=ORIENTED_EDGE('',*,*,#51221,.T.);
#70158=ORIENTED_EDGE('',*,*,#51223,.T.);
#70159=ORIENTED_EDGE('',*,*,#49363,.F.);
#70160=ORIENTED_EDGE('',*,*,#51225,.F.);
#70161=ORIENTED_EDGE('',*,*,#47493,.F.);
#70162=ORIENTED_EDGE('',*,*,#51224,.T.);
#70163=ORIENTED_EDGE('',*,*,#47506,.F.);
#70164=ORIENTED_EDGE('',*,*,#51226,.F.);
#70165=ORIENTED_EDGE('',*,*,#49355,.F.);
#70166=ORIENTED_EDGE('',*,*,#51225,.T.);
#70167=ORIENTED_EDGE('',*,*,#49362,.F.);
#70168=ORIENTED_EDGE('',*,*,#51227,.F.);
#70169=ORIENTED_EDGE('',*,*,#47510,.F.);
#70170=ORIENTED_EDGE('',*,*,#51226,.T.);
#70171=ORIENTED_EDGE('',*,*,#46105,.F.);
#70172=ORIENTED_EDGE('',*,*,#51228,.F.);
#70173=ORIENTED_EDGE('',*,*,#49356,.F.);
#70174=ORIENTED_EDGE('',*,*,#51227,.T.);
#70175=ORIENTED_EDGE('',*,*,#49361,.F.);
#70176=ORIENTED_EDGE('',*,*,#51229,.F.);
#70177=ORIENTED_EDGE('',*,*,#47485,.T.);
#70178=ORIENTED_EDGE('',*,*,#47489,.F.);
#70179=ORIENTED_EDGE('',*,*,#51228,.T.);
#70180=ORIENTED_EDGE('',*,*,#46104,.F.);
#70181=ORIENTED_EDGE('',*,*,#51230,.F.);
#70182=ORIENTED_EDGE('',*,*,#50269,.F.);
#70183=ORIENTED_EDGE('',*,*,#51229,.T.);
#70184=ORIENTED_EDGE('',*,*,#49360,.F.);
#70185=ORIENTED_EDGE('',*,*,#51231,.F.);
#70186=ORIENTED_EDGE('',*,*,#47486,.F.);
#70187=ORIENTED_EDGE('',*,*,#51230,.T.);
#70188=ORIENTED_EDGE('',*,*,#46103,.F.);
#70189=ORIENTED_EDGE('',*,*,#51232,.F.);
#70190=ORIENTED_EDGE('',*,*,#49340,.F.);
#70191=ORIENTED_EDGE('',*,*,#51231,.T.);
#70192=ORIENTED_EDGE('',*,*,#49359,.F.);
#70193=ORIENTED_EDGE('',*,*,#51233,.F.);
#70194=ORIENTED_EDGE('',*,*,#47504,.F.);
#70195=ORIENTED_EDGE('',*,*,#51232,.T.);
#70196=ORIENTED_EDGE('',*,*,#46102,.F.);
#70197=ORIENTED_EDGE('',*,*,#51234,.F.);
#70198=ORIENTED_EDGE('',*,*,#50271,.F.);
#70199=ORIENTED_EDGE('',*,*,#51233,.T.);
#70200=ORIENTED_EDGE('',*,*,#49358,.F.);
#70201=ORIENTED_EDGE('',*,*,#51235,.F.);
#70202=ORIENTED_EDGE('',*,*,#46628,.F.);
#70203=ORIENTED_EDGE('',*,*,#51234,.T.);
#70204=ORIENTED_EDGE('',*,*,#46101,.F.);
#70205=ORIENTED_EDGE('',*,*,#51236,.F.);
#70206=ORIENTED_EDGE('',*,*,#49346,.F.);
#70207=ORIENTED_EDGE('',*,*,#51235,.T.);
#70208=ORIENTED_EDGE('',*,*,#50270,.F.);
#70209=ORIENTED_EDGE('',*,*,#51237,.F.);
#70210=ORIENTED_EDGE('',*,*,#46629,.F.);
#70211=ORIENTED_EDGE('',*,*,#51236,.T.);
#70212=ORIENTED_EDGE('',*,*,#47535,.F.);
#70213=ORIENTED_EDGE('',*,*,#51238,.F.);
#70214=ORIENTED_EDGE('',*,*,#49347,.F.);
#70215=ORIENTED_EDGE('',*,*,#51237,.T.);
#70216=ORIENTED_EDGE('',*,*,#49342,.F.);
#70217=ORIENTED_EDGE('',*,*,#51239,.F.);
#70218=ORIENTED_EDGE('',*,*,#46630,.F.);
#70219=ORIENTED_EDGE('',*,*,#47530,.F.);
#70220=ORIENTED_EDGE('',*,*,#47526,.T.);
#70221=ORIENTED_EDGE('',*,*,#51240,.F.);
#70222=ORIENTED_EDGE('',*,*,#49348,.F.);
#70223=ORIENTED_EDGE('',*,*,#51238,.T.);
#70224=ORIENTED_EDGE('',*,*,#51239,.T.);
#70225=ORIENTED_EDGE('',*,*,#50272,.F.);
#70226=ORIENTED_EDGE('',*,*,#51241,.F.);
#70227=ORIENTED_EDGE('',*,*,#46631,.F.);
#70228=ORIENTED_EDGE('',*,*,#51240,.T.);
#70229=ORIENTED_EDGE('',*,*,#47525,.F.);
#70230=ORIENTED_EDGE('',*,*,#51242,.F.);
#70231=ORIENTED_EDGE('',*,*,#49349,.F.);
#70232=ORIENTED_EDGE('',*,*,#51241,.T.);
#70233=ORIENTED_EDGE('',*,*,#49344,.F.);
#70234=ORIENTED_EDGE('',*,*,#51243,.F.);
#70235=ORIENTED_EDGE('',*,*,#46632,.F.);
#70236=ORIENTED_EDGE('',*,*,#51242,.T.);
#70237=ORIENTED_EDGE('',*,*,#47537,.F.);
#70238=ORIENTED_EDGE('',*,*,#51244,.F.);
#70239=ORIENTED_EDGE('',*,*,#49350,.F.);
#70240=ORIENTED_EDGE('',*,*,#51243,.T.);
#70241=ORIENTED_EDGE('',*,*,#49343,.F.);
#70242=ORIENTED_EDGE('',*,*,#51245,.F.);
#70243=ORIENTED_EDGE('',*,*,#47533,.F.);
#70244=ORIENTED_EDGE('',*,*,#51244,.T.);
#70245=ORIENTED_EDGE('',*,*,#47521,.F.);
#70246=ORIENTED_EDGE('',*,*,#51246,.F.);
#70247=ORIENTED_EDGE('',*,*,#49351,.F.);
#70248=ORIENTED_EDGE('',*,*,#51245,.T.);
#70249=ORIENTED_EDGE('',*,*,#49354,.F.);
#70250=ORIENTED_EDGE('',*,*,#51247,.F.);
#70251=ORIENTED_EDGE('',*,*,#47512,.F.);
#70252=ORIENTED_EDGE('',*,*,#51246,.T.);
#70253=ORIENTED_EDGE('',*,*,#47539,.F.);
#70254=ORIENTED_EDGE('',*,*,#51248,.F.);
#70255=ORIENTED_EDGE('',*,*,#49352,.F.);
#70256=ORIENTED_EDGE('',*,*,#51247,.T.);
#70257=ORIENTED_EDGE('',*,*,#49353,.F.);
#70258=ORIENTED_EDGE('',*,*,#51248,.T.);
#70259=ORIENTED_EDGE('',*,*,#47517,.F.);
#70260=ORIENTED_EDGE('',*,*,#47513,.T.);
#70261=ORIENTED_EDGE('',*,*,#51249,.F.);
#70262=ORIENTED_EDGE('',*,*,#49393,.F.);
#70263=ORIENTED_EDGE('',*,*,#51250,.F.);
#70264=ORIENTED_EDGE('',*,*,#47469,.F.);
#70265=ORIENTED_EDGE('',*,*,#51250,.T.);
#70266=ORIENTED_EDGE('',*,*,#49392,.F.);
#70267=ORIENTED_EDGE('',*,*,#51251,.F.);
#70268=ORIENTED_EDGE('',*,*,#47478,.F.);
#70269=ORIENTED_EDGE('',*,*,#47468,.T.);
#70270=ORIENTED_EDGE('',*,*,#47472,.F.);
#70271=ORIENTED_EDGE('',*,*,#51252,.F.);
#70272=ORIENTED_EDGE('',*,*,#49394,.F.);
#70273=ORIENTED_EDGE('',*,*,#51249,.T.);
#70274=ORIENTED_EDGE('',*,*,#51251,.T.);
#70275=ORIENTED_EDGE('',*,*,#49391,.F.);
#70276=ORIENTED_EDGE('',*,*,#51253,.F.);
#70277=ORIENTED_EDGE('',*,*,#47463,.F.);
#70278=ORIENTED_EDGE('',*,*,#51252,.T.);
#70279=ORIENTED_EDGE('',*,*,#47476,.F.);
#70280=ORIENTED_EDGE('',*,*,#51254,.F.);
#70281=ORIENTED_EDGE('',*,*,#49383,.F.);
#70282=ORIENTED_EDGE('',*,*,#51253,.T.);
#70283=ORIENTED_EDGE('',*,*,#49390,.F.);
#70284=ORIENTED_EDGE('',*,*,#51255,.F.);
#70285=ORIENTED_EDGE('',*,*,#47480,.F.);
#70286=ORIENTED_EDGE('',*,*,#51254,.T.);
#70287=ORIENTED_EDGE('',*,*,#46111,.F.);
#70288=ORIENTED_EDGE('',*,*,#51256,.F.);
#70289=ORIENTED_EDGE('',*,*,#49384,.F.);
#70290=ORIENTED_EDGE('',*,*,#51255,.T.);
#70291=ORIENTED_EDGE('',*,*,#49389,.F.);
#70292=ORIENTED_EDGE('',*,*,#51257,.F.);
#70293=ORIENTED_EDGE('',*,*,#47455,.T.);
#70294=ORIENTED_EDGE('',*,*,#47459,.F.);
#70295=ORIENTED_EDGE('',*,*,#51256,.T.);
#70296=ORIENTED_EDGE('',*,*,#46110,.F.);
#70297=ORIENTED_EDGE('',*,*,#51258,.F.);
#70298=ORIENTED_EDGE('',*,*,#50273,.F.);
#70299=ORIENTED_EDGE('',*,*,#51257,.T.);
#70300=ORIENTED_EDGE('',*,*,#49388,.F.);
#70301=ORIENTED_EDGE('',*,*,#51259,.F.);
#70302=ORIENTED_EDGE('',*,*,#47456,.F.);
#70303=ORIENTED_EDGE('',*,*,#51258,.T.);
#70304=ORIENTED_EDGE('',*,*,#46109,.F.);
#70305=ORIENTED_EDGE('',*,*,#51260,.F.);
#70306=ORIENTED_EDGE('',*,*,#49368,.F.);
#70307=ORIENTED_EDGE('',*,*,#51259,.T.);
#70308=ORIENTED_EDGE('',*,*,#49387,.F.);
#70309=ORIENTED_EDGE('',*,*,#51261,.F.);
#70310=ORIENTED_EDGE('',*,*,#47474,.F.);
#70311=ORIENTED_EDGE('',*,*,#51260,.T.);
#70312=ORIENTED_EDGE('',*,*,#46108,.F.);
#70313=ORIENTED_EDGE('',*,*,#51262,.F.);
#70314=ORIENTED_EDGE('',*,*,#50275,.F.);
#70315=ORIENTED_EDGE('',*,*,#51261,.T.);
#70316=ORIENTED_EDGE('',*,*,#49386,.F.);
#70317=ORIENTED_EDGE('',*,*,#51263,.F.);
#70318=ORIENTED_EDGE('',*,*,#46622,.F.);
#70319=ORIENTED_EDGE('',*,*,#51262,.T.);
#70320=ORIENTED_EDGE('',*,*,#46107,.F.);
#70321=ORIENTED_EDGE('',*,*,#51264,.F.);
#70322=ORIENTED_EDGE('',*,*,#49374,.F.);
#70323=ORIENTED_EDGE('',*,*,#51263,.T.);
#70324=ORIENTED_EDGE('',*,*,#50274,.F.);
#70325=ORIENTED_EDGE('',*,*,#51265,.F.);
#70326=ORIENTED_EDGE('',*,*,#46623,.F.);
#70327=ORIENTED_EDGE('',*,*,#51264,.T.);
#70328=ORIENTED_EDGE('',*,*,#47505,.F.);
#70329=ORIENTED_EDGE('',*,*,#51266,.F.);
#70330=ORIENTED_EDGE('',*,*,#49375,.F.);
#70331=ORIENTED_EDGE('',*,*,#51265,.T.);
#70332=ORIENTED_EDGE('',*,*,#49370,.F.);
#70333=ORIENTED_EDGE('',*,*,#51267,.F.);
#70334=ORIENTED_EDGE('',*,*,#46624,.F.);
#70335=ORIENTED_EDGE('',*,*,#47500,.F.);
#70336=ORIENTED_EDGE('',*,*,#47496,.T.);
#70337=ORIENTED_EDGE('',*,*,#51268,.F.);
#70338=ORIENTED_EDGE('',*,*,#49376,.F.);
#70339=ORIENTED_EDGE('',*,*,#51266,.T.);
#70340=ORIENTED_EDGE('',*,*,#51267,.T.);
#70341=ORIENTED_EDGE('',*,*,#50276,.F.);
#70342=ORIENTED_EDGE('',*,*,#51269,.F.);
#70343=ORIENTED_EDGE('',*,*,#46625,.F.);
#70344=ORIENTED_EDGE('',*,*,#51268,.T.);
#70345=ORIENTED_EDGE('',*,*,#47495,.F.);
#70346=ORIENTED_EDGE('',*,*,#51270,.F.);
#70347=ORIENTED_EDGE('',*,*,#49377,.F.);
#70348=ORIENTED_EDGE('',*,*,#51269,.T.);
#70349=ORIENTED_EDGE('',*,*,#49372,.F.);
#70350=ORIENTED_EDGE('',*,*,#51271,.F.);
#70351=ORIENTED_EDGE('',*,*,#46626,.F.);
#70352=ORIENTED_EDGE('',*,*,#51270,.T.);
#70353=ORIENTED_EDGE('',*,*,#47507,.F.);
#70354=ORIENTED_EDGE('',*,*,#51272,.F.);
#70355=ORIENTED_EDGE('',*,*,#49378,.F.);
#70356=ORIENTED_EDGE('',*,*,#51271,.T.);
#70357=ORIENTED_EDGE('',*,*,#49371,.F.);
#70358=ORIENTED_EDGE('',*,*,#51273,.F.);
#70359=ORIENTED_EDGE('',*,*,#47503,.F.);
#70360=ORIENTED_EDGE('',*,*,#51272,.T.);
#70361=ORIENTED_EDGE('',*,*,#47491,.F.);
#70362=ORIENTED_EDGE('',*,*,#51274,.F.);
#70363=ORIENTED_EDGE('',*,*,#49379,.F.);
#70364=ORIENTED_EDGE('',*,*,#51273,.T.);
#70365=ORIENTED_EDGE('',*,*,#49382,.F.);
#70366=ORIENTED_EDGE('',*,*,#51275,.F.);
#70367=ORIENTED_EDGE('',*,*,#47482,.F.);
#70368=ORIENTED_EDGE('',*,*,#51274,.T.);
#70369=ORIENTED_EDGE('',*,*,#47509,.F.);
#70370=ORIENTED_EDGE('',*,*,#51276,.F.);
#70371=ORIENTED_EDGE('',*,*,#49380,.F.);
#70372=ORIENTED_EDGE('',*,*,#51275,.T.);
#70373=ORIENTED_EDGE('',*,*,#49381,.F.);
#70374=ORIENTED_EDGE('',*,*,#51276,.T.);
#70375=ORIENTED_EDGE('',*,*,#47487,.F.);
#70376=ORIENTED_EDGE('',*,*,#47483,.T.);
#70377=ORIENTED_EDGE('',*,*,#51277,.F.);
#70378=ORIENTED_EDGE('',*,*,#49421,.F.);
#70379=ORIENTED_EDGE('',*,*,#51278,.F.);
#70380=ORIENTED_EDGE('',*,*,#47439,.F.);
#70381=ORIENTED_EDGE('',*,*,#51278,.T.);
#70382=ORIENTED_EDGE('',*,*,#49420,.F.);
#70383=ORIENTED_EDGE('',*,*,#51279,.F.);
#70384=ORIENTED_EDGE('',*,*,#47448,.F.);
#70385=ORIENTED_EDGE('',*,*,#47438,.T.);
#70386=ORIENTED_EDGE('',*,*,#47442,.F.);
#70387=ORIENTED_EDGE('',*,*,#51280,.F.);
#70388=ORIENTED_EDGE('',*,*,#49422,.F.);
#70389=ORIENTED_EDGE('',*,*,#51277,.T.);
#70390=ORIENTED_EDGE('',*,*,#51279,.T.);
#70391=ORIENTED_EDGE('',*,*,#49419,.F.);
#70392=ORIENTED_EDGE('',*,*,#51281,.F.);
#70393=ORIENTED_EDGE('',*,*,#47433,.F.);
#70394=ORIENTED_EDGE('',*,*,#51280,.T.);
#70395=ORIENTED_EDGE('',*,*,#47446,.F.);
#70396=ORIENTED_EDGE('',*,*,#51282,.F.);
#70397=ORIENTED_EDGE('',*,*,#49411,.F.);
#70398=ORIENTED_EDGE('',*,*,#51281,.T.);
#70399=ORIENTED_EDGE('',*,*,#49418,.F.);
#70400=ORIENTED_EDGE('',*,*,#51283,.F.);
#70401=ORIENTED_EDGE('',*,*,#47450,.F.);
#70402=ORIENTED_EDGE('',*,*,#51282,.T.);
#70403=ORIENTED_EDGE('',*,*,#46117,.F.);
#70404=ORIENTED_EDGE('',*,*,#51284,.F.);
#70405=ORIENTED_EDGE('',*,*,#49412,.F.);
#70406=ORIENTED_EDGE('',*,*,#51283,.T.);
#70407=ORIENTED_EDGE('',*,*,#49417,.F.);
#70408=ORIENTED_EDGE('',*,*,#51285,.F.);
#70409=ORIENTED_EDGE('',*,*,#47425,.T.);
#70410=ORIENTED_EDGE('',*,*,#47429,.F.);
#70411=ORIENTED_EDGE('',*,*,#51284,.T.);
#70412=ORIENTED_EDGE('',*,*,#46116,.F.);
#70413=ORIENTED_EDGE('',*,*,#51286,.F.);
#70414=ORIENTED_EDGE('',*,*,#50277,.F.);
#70415=ORIENTED_EDGE('',*,*,#51285,.T.);
#70416=ORIENTED_EDGE('',*,*,#49416,.F.);
#70417=ORIENTED_EDGE('',*,*,#51287,.F.);
#70418=ORIENTED_EDGE('',*,*,#47426,.F.);
#70419=ORIENTED_EDGE('',*,*,#51286,.T.);
#70420=ORIENTED_EDGE('',*,*,#46115,.F.);
#70421=ORIENTED_EDGE('',*,*,#51288,.F.);
#70422=ORIENTED_EDGE('',*,*,#49396,.F.);
#70423=ORIENTED_EDGE('',*,*,#51287,.T.);
#70424=ORIENTED_EDGE('',*,*,#49415,.F.);
#70425=ORIENTED_EDGE('',*,*,#51289,.F.);
#70426=ORIENTED_EDGE('',*,*,#47444,.F.);
#70427=ORIENTED_EDGE('',*,*,#51288,.T.);
#70428=ORIENTED_EDGE('',*,*,#46114,.F.);
#70429=ORIENTED_EDGE('',*,*,#51290,.F.);
#70430=ORIENTED_EDGE('',*,*,#50279,.F.);
#70431=ORIENTED_EDGE('',*,*,#51289,.T.);
#70432=ORIENTED_EDGE('',*,*,#49414,.F.);
#70433=ORIENTED_EDGE('',*,*,#51291,.F.);
#70434=ORIENTED_EDGE('',*,*,#46616,.F.);
#70435=ORIENTED_EDGE('',*,*,#51290,.T.);
#70436=ORIENTED_EDGE('',*,*,#46113,.F.);
#70437=ORIENTED_EDGE('',*,*,#51292,.F.);
#70438=ORIENTED_EDGE('',*,*,#49402,.F.);
#70439=ORIENTED_EDGE('',*,*,#51291,.T.);
#70440=ORIENTED_EDGE('',*,*,#50278,.F.);
#70441=ORIENTED_EDGE('',*,*,#51293,.F.);
#70442=ORIENTED_EDGE('',*,*,#46617,.F.);
#70443=ORIENTED_EDGE('',*,*,#51292,.T.);
#70444=ORIENTED_EDGE('',*,*,#47475,.F.);
#70445=ORIENTED_EDGE('',*,*,#51294,.F.);
#70446=ORIENTED_EDGE('',*,*,#49403,.F.);
#70447=ORIENTED_EDGE('',*,*,#51293,.T.);
#70448=ORIENTED_EDGE('',*,*,#49398,.F.);
#70449=ORIENTED_EDGE('',*,*,#51295,.F.);
#70450=ORIENTED_EDGE('',*,*,#46618,.F.);
#70451=ORIENTED_EDGE('',*,*,#47470,.F.);
#70452=ORIENTED_EDGE('',*,*,#47466,.T.);
#70453=ORIENTED_EDGE('',*,*,#51296,.F.);
#70454=ORIENTED_EDGE('',*,*,#49404,.F.);
#70455=ORIENTED_EDGE('',*,*,#51294,.T.);
#70456=ORIENTED_EDGE('',*,*,#51295,.T.);
#70457=ORIENTED_EDGE('',*,*,#50280,.F.);
#70458=ORIENTED_EDGE('',*,*,#51297,.F.);
#70459=ORIENTED_EDGE('',*,*,#46619,.F.);
#70460=ORIENTED_EDGE('',*,*,#51296,.T.);
#70461=ORIENTED_EDGE('',*,*,#47465,.F.);
#70462=ORIENTED_EDGE('',*,*,#51298,.F.);
#70463=ORIENTED_EDGE('',*,*,#49405,.F.);
#70464=ORIENTED_EDGE('',*,*,#51297,.T.);
#70465=ORIENTED_EDGE('',*,*,#49400,.F.);
#70466=ORIENTED_EDGE('',*,*,#51299,.F.);
#70467=ORIENTED_EDGE('',*,*,#46620,.F.);
#70468=ORIENTED_EDGE('',*,*,#51298,.T.);
#70469=ORIENTED_EDGE('',*,*,#47477,.F.);
#70470=ORIENTED_EDGE('',*,*,#51300,.F.);
#70471=ORIENTED_EDGE('',*,*,#49406,.F.);
#70472=ORIENTED_EDGE('',*,*,#51299,.T.);
#70473=ORIENTED_EDGE('',*,*,#49399,.F.);
#70474=ORIENTED_EDGE('',*,*,#51301,.F.);
#70475=ORIENTED_EDGE('',*,*,#47473,.F.);
#70476=ORIENTED_EDGE('',*,*,#51300,.T.);
#70477=ORIENTED_EDGE('',*,*,#47461,.F.);
#70478=ORIENTED_EDGE('',*,*,#51302,.F.);
#70479=ORIENTED_EDGE('',*,*,#49407,.F.);
#70480=ORIENTED_EDGE('',*,*,#51301,.T.);
#70481=ORIENTED_EDGE('',*,*,#49410,.F.);
#70482=ORIENTED_EDGE('',*,*,#51303,.F.);
#70483=ORIENTED_EDGE('',*,*,#47452,.F.);
#70484=ORIENTED_EDGE('',*,*,#51302,.T.);
#70485=ORIENTED_EDGE('',*,*,#47479,.F.);
#70486=ORIENTED_EDGE('',*,*,#51304,.F.);
#70487=ORIENTED_EDGE('',*,*,#49408,.F.);
#70488=ORIENTED_EDGE('',*,*,#51303,.T.);
#70489=ORIENTED_EDGE('',*,*,#49409,.F.);
#70490=ORIENTED_EDGE('',*,*,#51304,.T.);
#70491=ORIENTED_EDGE('',*,*,#47457,.F.);
#70492=ORIENTED_EDGE('',*,*,#47453,.T.);
#70493=ORIENTED_EDGE('',*,*,#51305,.F.);
#70494=ORIENTED_EDGE('',*,*,#49449,.F.);
#70495=ORIENTED_EDGE('',*,*,#51306,.F.);
#70496=ORIENTED_EDGE('',*,*,#47409,.F.);
#70497=ORIENTED_EDGE('',*,*,#51306,.T.);
#70498=ORIENTED_EDGE('',*,*,#49448,.F.);
#70499=ORIENTED_EDGE('',*,*,#51307,.F.);
#70500=ORIENTED_EDGE('',*,*,#47418,.F.);
#70501=ORIENTED_EDGE('',*,*,#47408,.T.);
#70502=ORIENTED_EDGE('',*,*,#47412,.F.);
#70503=ORIENTED_EDGE('',*,*,#51308,.F.);
#70504=ORIENTED_EDGE('',*,*,#49450,.F.);
#70505=ORIENTED_EDGE('',*,*,#51305,.T.);
#70506=ORIENTED_EDGE('',*,*,#51307,.T.);
#70507=ORIENTED_EDGE('',*,*,#49447,.F.);
#70508=ORIENTED_EDGE('',*,*,#51309,.F.);
#70509=ORIENTED_EDGE('',*,*,#47403,.F.);
#70510=ORIENTED_EDGE('',*,*,#51308,.T.);
#70511=ORIENTED_EDGE('',*,*,#47416,.F.);
#70512=ORIENTED_EDGE('',*,*,#51310,.F.);
#70513=ORIENTED_EDGE('',*,*,#49439,.F.);
#70514=ORIENTED_EDGE('',*,*,#51309,.T.);
#70515=ORIENTED_EDGE('',*,*,#49446,.F.);
#70516=ORIENTED_EDGE('',*,*,#51311,.F.);
#70517=ORIENTED_EDGE('',*,*,#47420,.F.);
#70518=ORIENTED_EDGE('',*,*,#51310,.T.);
#70519=ORIENTED_EDGE('',*,*,#46123,.F.);
#70520=ORIENTED_EDGE('',*,*,#51312,.F.);
#70521=ORIENTED_EDGE('',*,*,#49440,.F.);
#70522=ORIENTED_EDGE('',*,*,#51311,.T.);
#70523=ORIENTED_EDGE('',*,*,#49445,.F.);
#70524=ORIENTED_EDGE('',*,*,#51313,.F.);
#70525=ORIENTED_EDGE('',*,*,#47395,.T.);
#70526=ORIENTED_EDGE('',*,*,#47399,.F.);
#70527=ORIENTED_EDGE('',*,*,#51312,.T.);
#70528=ORIENTED_EDGE('',*,*,#46122,.F.);
#70529=ORIENTED_EDGE('',*,*,#51314,.F.);
#70530=ORIENTED_EDGE('',*,*,#50281,.F.);
#70531=ORIENTED_EDGE('',*,*,#51313,.T.);
#70532=ORIENTED_EDGE('',*,*,#49444,.F.);
#70533=ORIENTED_EDGE('',*,*,#51315,.F.);
#70534=ORIENTED_EDGE('',*,*,#47396,.F.);
#70535=ORIENTED_EDGE('',*,*,#51314,.T.);
#70536=ORIENTED_EDGE('',*,*,#46121,.F.);
#70537=ORIENTED_EDGE('',*,*,#51316,.F.);
#70538=ORIENTED_EDGE('',*,*,#49424,.F.);
#70539=ORIENTED_EDGE('',*,*,#51315,.T.);
#70540=ORIENTED_EDGE('',*,*,#49443,.F.);
#70541=ORIENTED_EDGE('',*,*,#51317,.F.);
#70542=ORIENTED_EDGE('',*,*,#47414,.F.);
#70543=ORIENTED_EDGE('',*,*,#51316,.T.);
#70544=ORIENTED_EDGE('',*,*,#46120,.F.);
#70545=ORIENTED_EDGE('',*,*,#51318,.F.);
#70546=ORIENTED_EDGE('',*,*,#50283,.F.);
#70547=ORIENTED_EDGE('',*,*,#51317,.T.);
#70548=ORIENTED_EDGE('',*,*,#49442,.F.);
#70549=ORIENTED_EDGE('',*,*,#51319,.F.);
#70550=ORIENTED_EDGE('',*,*,#46610,.F.);
#70551=ORIENTED_EDGE('',*,*,#51318,.T.);
#70552=ORIENTED_EDGE('',*,*,#46119,.F.);
#70553=ORIENTED_EDGE('',*,*,#51320,.F.);
#70554=ORIENTED_EDGE('',*,*,#49430,.F.);
#70555=ORIENTED_EDGE('',*,*,#51319,.T.);
#70556=ORIENTED_EDGE('',*,*,#50282,.F.);
#70557=ORIENTED_EDGE('',*,*,#51321,.F.);
#70558=ORIENTED_EDGE('',*,*,#46611,.F.);
#70559=ORIENTED_EDGE('',*,*,#51320,.T.);
#70560=ORIENTED_EDGE('',*,*,#47445,.F.);
#70561=ORIENTED_EDGE('',*,*,#51322,.F.);
#70562=ORIENTED_EDGE('',*,*,#49431,.F.);
#70563=ORIENTED_EDGE('',*,*,#51321,.T.);
#70564=ORIENTED_EDGE('',*,*,#49426,.F.);
#70565=ORIENTED_EDGE('',*,*,#51323,.F.);
#70566=ORIENTED_EDGE('',*,*,#46612,.F.);
#70567=ORIENTED_EDGE('',*,*,#47440,.F.);
#70568=ORIENTED_EDGE('',*,*,#47436,.T.);
#70569=ORIENTED_EDGE('',*,*,#51324,.F.);
#70570=ORIENTED_EDGE('',*,*,#49432,.F.);
#70571=ORIENTED_EDGE('',*,*,#51322,.T.);
#70572=ORIENTED_EDGE('',*,*,#51323,.T.);
#70573=ORIENTED_EDGE('',*,*,#50284,.F.);
#70574=ORIENTED_EDGE('',*,*,#51325,.F.);
#70575=ORIENTED_EDGE('',*,*,#46613,.F.);
#70576=ORIENTED_EDGE('',*,*,#51324,.T.);
#70577=ORIENTED_EDGE('',*,*,#47435,.F.);
#70578=ORIENTED_EDGE('',*,*,#51326,.F.);
#70579=ORIENTED_EDGE('',*,*,#49433,.F.);
#70580=ORIENTED_EDGE('',*,*,#51325,.T.);
#70581=ORIENTED_EDGE('',*,*,#49428,.F.);
#70582=ORIENTED_EDGE('',*,*,#51327,.F.);
#70583=ORIENTED_EDGE('',*,*,#46614,.F.);
#70584=ORIENTED_EDGE('',*,*,#51326,.T.);
#70585=ORIENTED_EDGE('',*,*,#47447,.F.);
#70586=ORIENTED_EDGE('',*,*,#51328,.F.);
#70587=ORIENTED_EDGE('',*,*,#49434,.F.);
#70588=ORIENTED_EDGE('',*,*,#51327,.T.);
#70589=ORIENTED_EDGE('',*,*,#49427,.F.);
#70590=ORIENTED_EDGE('',*,*,#51329,.F.);
#70591=ORIENTED_EDGE('',*,*,#47443,.F.);
#70592=ORIENTED_EDGE('',*,*,#51328,.T.);
#70593=ORIENTED_EDGE('',*,*,#47431,.F.);
#70594=ORIENTED_EDGE('',*,*,#51330,.F.);
#70595=ORIENTED_EDGE('',*,*,#49435,.F.);
#70596=ORIENTED_EDGE('',*,*,#51329,.T.);
#70597=ORIENTED_EDGE('',*,*,#49438,.F.);
#70598=ORIENTED_EDGE('',*,*,#51331,.F.);
#70599=ORIENTED_EDGE('',*,*,#47422,.F.);
#70600=ORIENTED_EDGE('',*,*,#51330,.T.);
#70601=ORIENTED_EDGE('',*,*,#47449,.F.);
#70602=ORIENTED_EDGE('',*,*,#51332,.F.);
#70603=ORIENTED_EDGE('',*,*,#49436,.F.);
#70604=ORIENTED_EDGE('',*,*,#51331,.T.);
#70605=ORIENTED_EDGE('',*,*,#49437,.F.);
#70606=ORIENTED_EDGE('',*,*,#51332,.T.);
#70607=ORIENTED_EDGE('',*,*,#47427,.F.);
#70608=ORIENTED_EDGE('',*,*,#47423,.T.);
#70609=ORIENTED_EDGE('',*,*,#51333,.F.);
#70610=ORIENTED_EDGE('',*,*,#49477,.F.);
#70611=ORIENTED_EDGE('',*,*,#51334,.F.);
#70612=ORIENTED_EDGE('',*,*,#47379,.F.);
#70613=ORIENTED_EDGE('',*,*,#51334,.T.);
#70614=ORIENTED_EDGE('',*,*,#49476,.F.);
#70615=ORIENTED_EDGE('',*,*,#51335,.F.);
#70616=ORIENTED_EDGE('',*,*,#47388,.F.);
#70617=ORIENTED_EDGE('',*,*,#47378,.T.);
#70618=ORIENTED_EDGE('',*,*,#47382,.F.);
#70619=ORIENTED_EDGE('',*,*,#51336,.F.);
#70620=ORIENTED_EDGE('',*,*,#49478,.F.);
#70621=ORIENTED_EDGE('',*,*,#51333,.T.);
#70622=ORIENTED_EDGE('',*,*,#51335,.T.);
#70623=ORIENTED_EDGE('',*,*,#49475,.F.);
#70624=ORIENTED_EDGE('',*,*,#51337,.F.);
#70625=ORIENTED_EDGE('',*,*,#47373,.F.);
#70626=ORIENTED_EDGE('',*,*,#51336,.T.);
#70627=ORIENTED_EDGE('',*,*,#47386,.F.);
#70628=ORIENTED_EDGE('',*,*,#51338,.F.);
#70629=ORIENTED_EDGE('',*,*,#49467,.F.);
#70630=ORIENTED_EDGE('',*,*,#51337,.T.);
#70631=ORIENTED_EDGE('',*,*,#49474,.F.);
#70632=ORIENTED_EDGE('',*,*,#51339,.F.);
#70633=ORIENTED_EDGE('',*,*,#47390,.F.);
#70634=ORIENTED_EDGE('',*,*,#51338,.T.);
#70635=ORIENTED_EDGE('',*,*,#46129,.F.);
#70636=ORIENTED_EDGE('',*,*,#51340,.F.);
#70637=ORIENTED_EDGE('',*,*,#49468,.F.);
#70638=ORIENTED_EDGE('',*,*,#51339,.T.);
#70639=ORIENTED_EDGE('',*,*,#49473,.F.);
#70640=ORIENTED_EDGE('',*,*,#51341,.F.);
#70641=ORIENTED_EDGE('',*,*,#47365,.T.);
#70642=ORIENTED_EDGE('',*,*,#47369,.F.);
#70643=ORIENTED_EDGE('',*,*,#51340,.T.);
#70644=ORIENTED_EDGE('',*,*,#46128,.F.);
#70645=ORIENTED_EDGE('',*,*,#51342,.F.);
#70646=ORIENTED_EDGE('',*,*,#50285,.F.);
#70647=ORIENTED_EDGE('',*,*,#51341,.T.);
#70648=ORIENTED_EDGE('',*,*,#49472,.F.);
#70649=ORIENTED_EDGE('',*,*,#51343,.F.);
#70650=ORIENTED_EDGE('',*,*,#47366,.F.);
#70651=ORIENTED_EDGE('',*,*,#51342,.T.);
#70652=ORIENTED_EDGE('',*,*,#46127,.F.);
#70653=ORIENTED_EDGE('',*,*,#51344,.F.);
#70654=ORIENTED_EDGE('',*,*,#49452,.F.);
#70655=ORIENTED_EDGE('',*,*,#51343,.T.);
#70656=ORIENTED_EDGE('',*,*,#49471,.F.);
#70657=ORIENTED_EDGE('',*,*,#51345,.F.);
#70658=ORIENTED_EDGE('',*,*,#47384,.F.);
#70659=ORIENTED_EDGE('',*,*,#51344,.T.);
#70660=ORIENTED_EDGE('',*,*,#46126,.F.);
#70661=ORIENTED_EDGE('',*,*,#51346,.F.);
#70662=ORIENTED_EDGE('',*,*,#50287,.F.);
#70663=ORIENTED_EDGE('',*,*,#51345,.T.);
#70664=ORIENTED_EDGE('',*,*,#49470,.F.);
#70665=ORIENTED_EDGE('',*,*,#51347,.F.);
#70666=ORIENTED_EDGE('',*,*,#46604,.F.);
#70667=ORIENTED_EDGE('',*,*,#51346,.T.);
#70668=ORIENTED_EDGE('',*,*,#46125,.F.);
#70669=ORIENTED_EDGE('',*,*,#51348,.F.);
#70670=ORIENTED_EDGE('',*,*,#49458,.F.);
#70671=ORIENTED_EDGE('',*,*,#51347,.T.);
#70672=ORIENTED_EDGE('',*,*,#50286,.F.);
#70673=ORIENTED_EDGE('',*,*,#51349,.F.);
#70674=ORIENTED_EDGE('',*,*,#46605,.F.);
#70675=ORIENTED_EDGE('',*,*,#51348,.T.);
#70676=ORIENTED_EDGE('',*,*,#47415,.F.);
#70677=ORIENTED_EDGE('',*,*,#51350,.F.);
#70678=ORIENTED_EDGE('',*,*,#49459,.F.);
#70679=ORIENTED_EDGE('',*,*,#51349,.T.);
#70680=ORIENTED_EDGE('',*,*,#49454,.F.);
#70681=ORIENTED_EDGE('',*,*,#51351,.F.);
#70682=ORIENTED_EDGE('',*,*,#46606,.F.);
#70683=ORIENTED_EDGE('',*,*,#47410,.F.);
#70684=ORIENTED_EDGE('',*,*,#47406,.T.);
#70685=ORIENTED_EDGE('',*,*,#51352,.F.);
#70686=ORIENTED_EDGE('',*,*,#49460,.F.);
#70687=ORIENTED_EDGE('',*,*,#51350,.T.);
#70688=ORIENTED_EDGE('',*,*,#51351,.T.);
#70689=ORIENTED_EDGE('',*,*,#50288,.F.);
#70690=ORIENTED_EDGE('',*,*,#51353,.F.);
#70691=ORIENTED_EDGE('',*,*,#46607,.F.);
#70692=ORIENTED_EDGE('',*,*,#51352,.T.);
#70693=ORIENTED_EDGE('',*,*,#47405,.F.);
#70694=ORIENTED_EDGE('',*,*,#51354,.F.);
#70695=ORIENTED_EDGE('',*,*,#49461,.F.);
#70696=ORIENTED_EDGE('',*,*,#51353,.T.);
#70697=ORIENTED_EDGE('',*,*,#49456,.F.);
#70698=ORIENTED_EDGE('',*,*,#51355,.F.);
#70699=ORIENTED_EDGE('',*,*,#46608,.F.);
#70700=ORIENTED_EDGE('',*,*,#51354,.T.);
#70701=ORIENTED_EDGE('',*,*,#47417,.F.);
#70702=ORIENTED_EDGE('',*,*,#51356,.F.);
#70703=ORIENTED_EDGE('',*,*,#49462,.F.);
#70704=ORIENTED_EDGE('',*,*,#51355,.T.);
#70705=ORIENTED_EDGE('',*,*,#49455,.F.);
#70706=ORIENTED_EDGE('',*,*,#51357,.F.);
#70707=ORIENTED_EDGE('',*,*,#47413,.F.);
#70708=ORIENTED_EDGE('',*,*,#51356,.T.);
#70709=ORIENTED_EDGE('',*,*,#47401,.F.);
#70710=ORIENTED_EDGE('',*,*,#51358,.F.);
#70711=ORIENTED_EDGE('',*,*,#49463,.F.);
#70712=ORIENTED_EDGE('',*,*,#51357,.T.);
#70713=ORIENTED_EDGE('',*,*,#49466,.F.);
#70714=ORIENTED_EDGE('',*,*,#51359,.F.);
#70715=ORIENTED_EDGE('',*,*,#47392,.F.);
#70716=ORIENTED_EDGE('',*,*,#51358,.T.);
#70717=ORIENTED_EDGE('',*,*,#47419,.F.);
#70718=ORIENTED_EDGE('',*,*,#51360,.F.);
#70719=ORIENTED_EDGE('',*,*,#49464,.F.);
#70720=ORIENTED_EDGE('',*,*,#51359,.T.);
#70721=ORIENTED_EDGE('',*,*,#49465,.F.);
#70722=ORIENTED_EDGE('',*,*,#51360,.T.);
#70723=ORIENTED_EDGE('',*,*,#47397,.F.);
#70724=ORIENTED_EDGE('',*,*,#47393,.T.);
#70725=ORIENTED_EDGE('',*,*,#51361,.F.);
#70726=ORIENTED_EDGE('',*,*,#49505,.F.);
#70727=ORIENTED_EDGE('',*,*,#51362,.F.);
#70728=ORIENTED_EDGE('',*,*,#47349,.F.);
#70729=ORIENTED_EDGE('',*,*,#51362,.T.);
#70730=ORIENTED_EDGE('',*,*,#49504,.F.);
#70731=ORIENTED_EDGE('',*,*,#51363,.F.);
#70732=ORIENTED_EDGE('',*,*,#47358,.F.);
#70733=ORIENTED_EDGE('',*,*,#47348,.T.);
#70734=ORIENTED_EDGE('',*,*,#47352,.F.);
#70735=ORIENTED_EDGE('',*,*,#51364,.F.);
#70736=ORIENTED_EDGE('',*,*,#49506,.F.);
#70737=ORIENTED_EDGE('',*,*,#51361,.T.);
#70738=ORIENTED_EDGE('',*,*,#51363,.T.);
#70739=ORIENTED_EDGE('',*,*,#49503,.F.);
#70740=ORIENTED_EDGE('',*,*,#51365,.F.);
#70741=ORIENTED_EDGE('',*,*,#47343,.F.);
#70742=ORIENTED_EDGE('',*,*,#51364,.T.);
#70743=ORIENTED_EDGE('',*,*,#47356,.F.);
#70744=ORIENTED_EDGE('',*,*,#51366,.F.);
#70745=ORIENTED_EDGE('',*,*,#49495,.F.);
#70746=ORIENTED_EDGE('',*,*,#51365,.T.);
#70747=ORIENTED_EDGE('',*,*,#49502,.F.);
#70748=ORIENTED_EDGE('',*,*,#51367,.F.);
#70749=ORIENTED_EDGE('',*,*,#47360,.F.);
#70750=ORIENTED_EDGE('',*,*,#51366,.T.);
#70751=ORIENTED_EDGE('',*,*,#46135,.F.);
#70752=ORIENTED_EDGE('',*,*,#51368,.F.);
#70753=ORIENTED_EDGE('',*,*,#49496,.F.);
#70754=ORIENTED_EDGE('',*,*,#51367,.T.);
#70755=ORIENTED_EDGE('',*,*,#49501,.F.);
#70756=ORIENTED_EDGE('',*,*,#51369,.F.);
#70757=ORIENTED_EDGE('',*,*,#47335,.T.);
#70758=ORIENTED_EDGE('',*,*,#47339,.F.);
#70759=ORIENTED_EDGE('',*,*,#51368,.T.);
#70760=ORIENTED_EDGE('',*,*,#46134,.F.);
#70761=ORIENTED_EDGE('',*,*,#51370,.F.);
#70762=ORIENTED_EDGE('',*,*,#50289,.F.);
#70763=ORIENTED_EDGE('',*,*,#51369,.T.);
#70764=ORIENTED_EDGE('',*,*,#49500,.F.);
#70765=ORIENTED_EDGE('',*,*,#51371,.F.);
#70766=ORIENTED_EDGE('',*,*,#47336,.F.);
#70767=ORIENTED_EDGE('',*,*,#51370,.T.);
#70768=ORIENTED_EDGE('',*,*,#46133,.F.);
#70769=ORIENTED_EDGE('',*,*,#51372,.F.);
#70770=ORIENTED_EDGE('',*,*,#49480,.F.);
#70771=ORIENTED_EDGE('',*,*,#51371,.T.);
#70772=ORIENTED_EDGE('',*,*,#49499,.F.);
#70773=ORIENTED_EDGE('',*,*,#51373,.F.);
#70774=ORIENTED_EDGE('',*,*,#47354,.F.);
#70775=ORIENTED_EDGE('',*,*,#51372,.T.);
#70776=ORIENTED_EDGE('',*,*,#46132,.F.);
#70777=ORIENTED_EDGE('',*,*,#51374,.F.);
#70778=ORIENTED_EDGE('',*,*,#50291,.F.);
#70779=ORIENTED_EDGE('',*,*,#51373,.T.);
#70780=ORIENTED_EDGE('',*,*,#49498,.F.);
#70781=ORIENTED_EDGE('',*,*,#51375,.F.);
#70782=ORIENTED_EDGE('',*,*,#46598,.F.);
#70783=ORIENTED_EDGE('',*,*,#51374,.T.);
#70784=ORIENTED_EDGE('',*,*,#46131,.F.);
#70785=ORIENTED_EDGE('',*,*,#51376,.F.);
#70786=ORIENTED_EDGE('',*,*,#49486,.F.);
#70787=ORIENTED_EDGE('',*,*,#51375,.T.);
#70788=ORIENTED_EDGE('',*,*,#50290,.F.);
#70789=ORIENTED_EDGE('',*,*,#51377,.F.);
#70790=ORIENTED_EDGE('',*,*,#46599,.F.);
#70791=ORIENTED_EDGE('',*,*,#51376,.T.);
#70792=ORIENTED_EDGE('',*,*,#47385,.F.);
#70793=ORIENTED_EDGE('',*,*,#51378,.F.);
#70794=ORIENTED_EDGE('',*,*,#49487,.F.);
#70795=ORIENTED_EDGE('',*,*,#51377,.T.);
#70796=ORIENTED_EDGE('',*,*,#49482,.F.);
#70797=ORIENTED_EDGE('',*,*,#51379,.F.);
#70798=ORIENTED_EDGE('',*,*,#46600,.F.);
#70799=ORIENTED_EDGE('',*,*,#47380,.F.);
#70800=ORIENTED_EDGE('',*,*,#47376,.T.);
#70801=ORIENTED_EDGE('',*,*,#51380,.F.);
#70802=ORIENTED_EDGE('',*,*,#49488,.F.);
#70803=ORIENTED_EDGE('',*,*,#51378,.T.);
#70804=ORIENTED_EDGE('',*,*,#51379,.T.);
#70805=ORIENTED_EDGE('',*,*,#50292,.F.);
#70806=ORIENTED_EDGE('',*,*,#51381,.F.);
#70807=ORIENTED_EDGE('',*,*,#46601,.F.);
#70808=ORIENTED_EDGE('',*,*,#51380,.T.);
#70809=ORIENTED_EDGE('',*,*,#47375,.F.);
#70810=ORIENTED_EDGE('',*,*,#51382,.F.);
#70811=ORIENTED_EDGE('',*,*,#49489,.F.);
#70812=ORIENTED_EDGE('',*,*,#51381,.T.);
#70813=ORIENTED_EDGE('',*,*,#49484,.F.);
#70814=ORIENTED_EDGE('',*,*,#51383,.F.);
#70815=ORIENTED_EDGE('',*,*,#46602,.F.);
#70816=ORIENTED_EDGE('',*,*,#51382,.T.);
#70817=ORIENTED_EDGE('',*,*,#47387,.F.);
#70818=ORIENTED_EDGE('',*,*,#51384,.F.);
#70819=ORIENTED_EDGE('',*,*,#49490,.F.);
#70820=ORIENTED_EDGE('',*,*,#51383,.T.);
#70821=ORIENTED_EDGE('',*,*,#49483,.F.);
#70822=ORIENTED_EDGE('',*,*,#51385,.F.);
#70823=ORIENTED_EDGE('',*,*,#47383,.F.);
#70824=ORIENTED_EDGE('',*,*,#51384,.T.);
#70825=ORIENTED_EDGE('',*,*,#47371,.F.);
#70826=ORIENTED_EDGE('',*,*,#51386,.F.);
#70827=ORIENTED_EDGE('',*,*,#49491,.F.);
#70828=ORIENTED_EDGE('',*,*,#51385,.T.);
#70829=ORIENTED_EDGE('',*,*,#49494,.F.);
#70830=ORIENTED_EDGE('',*,*,#51387,.F.);
#70831=ORIENTED_EDGE('',*,*,#47362,.F.);
#70832=ORIENTED_EDGE('',*,*,#51386,.T.);
#70833=ORIENTED_EDGE('',*,*,#47389,.F.);
#70834=ORIENTED_EDGE('',*,*,#51388,.F.);
#70835=ORIENTED_EDGE('',*,*,#49492,.F.);
#70836=ORIENTED_EDGE('',*,*,#51387,.T.);
#70837=ORIENTED_EDGE('',*,*,#49493,.F.);
#70838=ORIENTED_EDGE('',*,*,#51388,.T.);
#70839=ORIENTED_EDGE('',*,*,#47367,.F.);
#70840=ORIENTED_EDGE('',*,*,#47363,.T.);
#70841=ORIENTED_EDGE('',*,*,#51389,.F.);
#70842=ORIENTED_EDGE('',*,*,#49533,.F.);
#70843=ORIENTED_EDGE('',*,*,#51390,.F.);
#70844=ORIENTED_EDGE('',*,*,#47319,.F.);
#70845=ORIENTED_EDGE('',*,*,#51390,.T.);
#70846=ORIENTED_EDGE('',*,*,#49532,.F.);
#70847=ORIENTED_EDGE('',*,*,#51391,.F.);
#70848=ORIENTED_EDGE('',*,*,#47328,.F.);
#70849=ORIENTED_EDGE('',*,*,#47318,.T.);
#70850=ORIENTED_EDGE('',*,*,#47322,.F.);
#70851=ORIENTED_EDGE('',*,*,#51392,.F.);
#70852=ORIENTED_EDGE('',*,*,#49534,.F.);
#70853=ORIENTED_EDGE('',*,*,#51389,.T.);
#70854=ORIENTED_EDGE('',*,*,#51391,.T.);
#70855=ORIENTED_EDGE('',*,*,#49531,.F.);
#70856=ORIENTED_EDGE('',*,*,#51393,.F.);
#70857=ORIENTED_EDGE('',*,*,#47313,.F.);
#70858=ORIENTED_EDGE('',*,*,#51392,.T.);
#70859=ORIENTED_EDGE('',*,*,#47326,.F.);
#70860=ORIENTED_EDGE('',*,*,#51394,.F.);
#70861=ORIENTED_EDGE('',*,*,#49523,.F.);
#70862=ORIENTED_EDGE('',*,*,#51393,.T.);
#70863=ORIENTED_EDGE('',*,*,#49530,.F.);
#70864=ORIENTED_EDGE('',*,*,#51395,.F.);
#70865=ORIENTED_EDGE('',*,*,#47330,.F.);
#70866=ORIENTED_EDGE('',*,*,#51394,.T.);
#70867=ORIENTED_EDGE('',*,*,#46141,.F.);
#70868=ORIENTED_EDGE('',*,*,#51396,.F.);
#70869=ORIENTED_EDGE('',*,*,#49524,.F.);
#70870=ORIENTED_EDGE('',*,*,#51395,.T.);
#70871=ORIENTED_EDGE('',*,*,#49529,.F.);
#70872=ORIENTED_EDGE('',*,*,#51397,.F.);
#70873=ORIENTED_EDGE('',*,*,#47305,.T.);
#70874=ORIENTED_EDGE('',*,*,#47309,.F.);
#70875=ORIENTED_EDGE('',*,*,#51396,.T.);
#70876=ORIENTED_EDGE('',*,*,#46140,.F.);
#70877=ORIENTED_EDGE('',*,*,#51398,.F.);
#70878=ORIENTED_EDGE('',*,*,#50293,.F.);
#70879=ORIENTED_EDGE('',*,*,#51397,.T.);
#70880=ORIENTED_EDGE('',*,*,#49528,.F.);
#70881=ORIENTED_EDGE('',*,*,#51399,.F.);
#70882=ORIENTED_EDGE('',*,*,#47306,.F.);
#70883=ORIENTED_EDGE('',*,*,#51398,.T.);
#70884=ORIENTED_EDGE('',*,*,#46139,.F.);
#70885=ORIENTED_EDGE('',*,*,#51400,.F.);
#70886=ORIENTED_EDGE('',*,*,#49508,.F.);
#70887=ORIENTED_EDGE('',*,*,#51399,.T.);
#70888=ORIENTED_EDGE('',*,*,#49527,.F.);
#70889=ORIENTED_EDGE('',*,*,#51401,.F.);
#70890=ORIENTED_EDGE('',*,*,#47324,.F.);
#70891=ORIENTED_EDGE('',*,*,#51400,.T.);
#70892=ORIENTED_EDGE('',*,*,#46138,.F.);
#70893=ORIENTED_EDGE('',*,*,#51402,.F.);
#70894=ORIENTED_EDGE('',*,*,#50295,.F.);
#70895=ORIENTED_EDGE('',*,*,#51401,.T.);
#70896=ORIENTED_EDGE('',*,*,#49526,.F.);
#70897=ORIENTED_EDGE('',*,*,#51403,.F.);
#70898=ORIENTED_EDGE('',*,*,#46592,.F.);
#70899=ORIENTED_EDGE('',*,*,#51402,.T.);
#70900=ORIENTED_EDGE('',*,*,#46137,.F.);
#70901=ORIENTED_EDGE('',*,*,#51404,.F.);
#70902=ORIENTED_EDGE('',*,*,#49514,.F.);
#70903=ORIENTED_EDGE('',*,*,#51403,.T.);
#70904=ORIENTED_EDGE('',*,*,#50294,.F.);
#70905=ORIENTED_EDGE('',*,*,#51405,.F.);
#70906=ORIENTED_EDGE('',*,*,#46593,.F.);
#70907=ORIENTED_EDGE('',*,*,#51404,.T.);
#70908=ORIENTED_EDGE('',*,*,#47355,.F.);
#70909=ORIENTED_EDGE('',*,*,#51406,.F.);
#70910=ORIENTED_EDGE('',*,*,#49515,.F.);
#70911=ORIENTED_EDGE('',*,*,#51405,.T.);
#70912=ORIENTED_EDGE('',*,*,#49510,.F.);
#70913=ORIENTED_EDGE('',*,*,#51407,.F.);
#70914=ORIENTED_EDGE('',*,*,#46594,.F.);
#70915=ORIENTED_EDGE('',*,*,#47350,.F.);
#70916=ORIENTED_EDGE('',*,*,#47346,.T.);
#70917=ORIENTED_EDGE('',*,*,#51408,.F.);
#70918=ORIENTED_EDGE('',*,*,#49516,.F.);
#70919=ORIENTED_EDGE('',*,*,#51406,.T.);
#70920=ORIENTED_EDGE('',*,*,#51407,.T.);
#70921=ORIENTED_EDGE('',*,*,#50296,.F.);
#70922=ORIENTED_EDGE('',*,*,#51409,.F.);
#70923=ORIENTED_EDGE('',*,*,#46595,.F.);
#70924=ORIENTED_EDGE('',*,*,#51408,.T.);
#70925=ORIENTED_EDGE('',*,*,#47345,.F.);
#70926=ORIENTED_EDGE('',*,*,#51410,.F.);
#70927=ORIENTED_EDGE('',*,*,#49517,.F.);
#70928=ORIENTED_EDGE('',*,*,#51409,.T.);
#70929=ORIENTED_EDGE('',*,*,#49512,.F.);
#70930=ORIENTED_EDGE('',*,*,#51411,.F.);
#70931=ORIENTED_EDGE('',*,*,#46596,.F.);
#70932=ORIENTED_EDGE('',*,*,#51410,.T.);
#70933=ORIENTED_EDGE('',*,*,#47357,.F.);
#70934=ORIENTED_EDGE('',*,*,#51412,.F.);
#70935=ORIENTED_EDGE('',*,*,#49518,.F.);
#70936=ORIENTED_EDGE('',*,*,#51411,.T.);
#70937=ORIENTED_EDGE('',*,*,#49511,.F.);
#70938=ORIENTED_EDGE('',*,*,#51413,.F.);
#70939=ORIENTED_EDGE('',*,*,#47353,.F.);
#70940=ORIENTED_EDGE('',*,*,#51412,.T.);
#70941=ORIENTED_EDGE('',*,*,#47341,.F.);
#70942=ORIENTED_EDGE('',*,*,#51414,.F.);
#70943=ORIENTED_EDGE('',*,*,#49519,.F.);
#70944=ORIENTED_EDGE('',*,*,#51413,.T.);
#70945=ORIENTED_EDGE('',*,*,#49522,.F.);
#70946=ORIENTED_EDGE('',*,*,#51415,.F.);
#70947=ORIENTED_EDGE('',*,*,#47332,.F.);
#70948=ORIENTED_EDGE('',*,*,#51414,.T.);
#70949=ORIENTED_EDGE('',*,*,#47359,.F.);
#70950=ORIENTED_EDGE('',*,*,#51416,.F.);
#70951=ORIENTED_EDGE('',*,*,#49520,.F.);
#70952=ORIENTED_EDGE('',*,*,#51415,.T.);
#70953=ORIENTED_EDGE('',*,*,#49521,.F.);
#70954=ORIENTED_EDGE('',*,*,#51416,.T.);
#70955=ORIENTED_EDGE('',*,*,#47337,.F.);
#70956=ORIENTED_EDGE('',*,*,#47333,.T.);
#70957=ORIENTED_EDGE('',*,*,#51417,.F.);
#70958=ORIENTED_EDGE('',*,*,#49561,.F.);
#70959=ORIENTED_EDGE('',*,*,#51418,.F.);
#70960=ORIENTED_EDGE('',*,*,#47289,.F.);
#70961=ORIENTED_EDGE('',*,*,#51418,.T.);
#70962=ORIENTED_EDGE('',*,*,#49560,.F.);
#70963=ORIENTED_EDGE('',*,*,#51419,.F.);
#70964=ORIENTED_EDGE('',*,*,#47298,.F.);
#70965=ORIENTED_EDGE('',*,*,#47288,.T.);
#70966=ORIENTED_EDGE('',*,*,#47292,.F.);
#70967=ORIENTED_EDGE('',*,*,#51420,.F.);
#70968=ORIENTED_EDGE('',*,*,#49562,.F.);
#70969=ORIENTED_EDGE('',*,*,#51417,.T.);
#70970=ORIENTED_EDGE('',*,*,#51419,.T.);
#70971=ORIENTED_EDGE('',*,*,#49559,.F.);
#70972=ORIENTED_EDGE('',*,*,#51421,.F.);
#70973=ORIENTED_EDGE('',*,*,#47283,.F.);
#70974=ORIENTED_EDGE('',*,*,#51420,.T.);
#70975=ORIENTED_EDGE('',*,*,#47296,.F.);
#70976=ORIENTED_EDGE('',*,*,#51422,.F.);
#70977=ORIENTED_EDGE('',*,*,#49551,.F.);
#70978=ORIENTED_EDGE('',*,*,#51421,.T.);
#70979=ORIENTED_EDGE('',*,*,#49558,.F.);
#70980=ORIENTED_EDGE('',*,*,#51423,.F.);
#70981=ORIENTED_EDGE('',*,*,#47300,.F.);
#70982=ORIENTED_EDGE('',*,*,#51422,.T.);
#70983=ORIENTED_EDGE('',*,*,#46147,.F.);
#70984=ORIENTED_EDGE('',*,*,#51424,.F.);
#70985=ORIENTED_EDGE('',*,*,#49552,.F.);
#70986=ORIENTED_EDGE('',*,*,#51423,.T.);
#70987=ORIENTED_EDGE('',*,*,#49557,.F.);
#70988=ORIENTED_EDGE('',*,*,#51425,.F.);
#70989=ORIENTED_EDGE('',*,*,#47275,.T.);
#70990=ORIENTED_EDGE('',*,*,#47279,.F.);
#70991=ORIENTED_EDGE('',*,*,#51424,.T.);
#70992=ORIENTED_EDGE('',*,*,#46146,.F.);
#70993=ORIENTED_EDGE('',*,*,#51426,.F.);
#70994=ORIENTED_EDGE('',*,*,#50297,.F.);
#70995=ORIENTED_EDGE('',*,*,#51425,.T.);
#70996=ORIENTED_EDGE('',*,*,#49556,.F.);
#70997=ORIENTED_EDGE('',*,*,#51427,.F.);
#70998=ORIENTED_EDGE('',*,*,#47276,.F.);
#70999=ORIENTED_EDGE('',*,*,#51426,.T.);
#71000=ORIENTED_EDGE('',*,*,#46145,.F.);
#71001=ORIENTED_EDGE('',*,*,#51428,.F.);
#71002=ORIENTED_EDGE('',*,*,#49536,.F.);
#71003=ORIENTED_EDGE('',*,*,#51427,.T.);
#71004=ORIENTED_EDGE('',*,*,#49555,.F.);
#71005=ORIENTED_EDGE('',*,*,#51429,.F.);
#71006=ORIENTED_EDGE('',*,*,#47294,.F.);
#71007=ORIENTED_EDGE('',*,*,#51428,.T.);
#71008=ORIENTED_EDGE('',*,*,#46144,.F.);
#71009=ORIENTED_EDGE('',*,*,#51430,.F.);
#71010=ORIENTED_EDGE('',*,*,#50299,.F.);
#71011=ORIENTED_EDGE('',*,*,#51429,.T.);
#71012=ORIENTED_EDGE('',*,*,#49554,.F.);
#71013=ORIENTED_EDGE('',*,*,#51431,.F.);
#71014=ORIENTED_EDGE('',*,*,#46586,.F.);
#71015=ORIENTED_EDGE('',*,*,#51430,.T.);
#71016=ORIENTED_EDGE('',*,*,#46143,.F.);
#71017=ORIENTED_EDGE('',*,*,#51432,.F.);
#71018=ORIENTED_EDGE('',*,*,#49542,.F.);
#71019=ORIENTED_EDGE('',*,*,#51431,.T.);
#71020=ORIENTED_EDGE('',*,*,#50298,.F.);
#71021=ORIENTED_EDGE('',*,*,#51433,.F.);
#71022=ORIENTED_EDGE('',*,*,#46587,.F.);
#71023=ORIENTED_EDGE('',*,*,#51432,.T.);
#71024=ORIENTED_EDGE('',*,*,#47325,.F.);
#71025=ORIENTED_EDGE('',*,*,#51434,.F.);
#71026=ORIENTED_EDGE('',*,*,#49543,.F.);
#71027=ORIENTED_EDGE('',*,*,#51433,.T.);
#71028=ORIENTED_EDGE('',*,*,#49538,.F.);
#71029=ORIENTED_EDGE('',*,*,#51435,.F.);
#71030=ORIENTED_EDGE('',*,*,#46588,.F.);
#71031=ORIENTED_EDGE('',*,*,#47320,.F.);
#71032=ORIENTED_EDGE('',*,*,#47316,.T.);
#71033=ORIENTED_EDGE('',*,*,#51436,.F.);
#71034=ORIENTED_EDGE('',*,*,#49544,.F.);
#71035=ORIENTED_EDGE('',*,*,#51434,.T.);
#71036=ORIENTED_EDGE('',*,*,#51435,.T.);
#71037=ORIENTED_EDGE('',*,*,#50300,.F.);
#71038=ORIENTED_EDGE('',*,*,#51437,.F.);
#71039=ORIENTED_EDGE('',*,*,#46589,.F.);
#71040=ORIENTED_EDGE('',*,*,#51436,.T.);
#71041=ORIENTED_EDGE('',*,*,#47315,.F.);
#71042=ORIENTED_EDGE('',*,*,#51438,.F.);
#71043=ORIENTED_EDGE('',*,*,#49545,.F.);
#71044=ORIENTED_EDGE('',*,*,#51437,.T.);
#71045=ORIENTED_EDGE('',*,*,#49540,.F.);
#71046=ORIENTED_EDGE('',*,*,#51439,.F.);
#71047=ORIENTED_EDGE('',*,*,#46590,.F.);
#71048=ORIENTED_EDGE('',*,*,#51438,.T.);
#71049=ORIENTED_EDGE('',*,*,#47327,.F.);
#71050=ORIENTED_EDGE('',*,*,#51440,.F.);
#71051=ORIENTED_EDGE('',*,*,#49546,.F.);
#71052=ORIENTED_EDGE('',*,*,#51439,.T.);
#71053=ORIENTED_EDGE('',*,*,#49539,.F.);
#71054=ORIENTED_EDGE('',*,*,#51441,.F.);
#71055=ORIENTED_EDGE('',*,*,#47323,.F.);
#71056=ORIENTED_EDGE('',*,*,#51440,.T.);
#71057=ORIENTED_EDGE('',*,*,#47311,.F.);
#71058=ORIENTED_EDGE('',*,*,#51442,.F.);
#71059=ORIENTED_EDGE('',*,*,#49547,.F.);
#71060=ORIENTED_EDGE('',*,*,#51441,.T.);
#71061=ORIENTED_EDGE('',*,*,#49550,.F.);
#71062=ORIENTED_EDGE('',*,*,#51443,.F.);
#71063=ORIENTED_EDGE('',*,*,#47302,.F.);
#71064=ORIENTED_EDGE('',*,*,#51442,.T.);
#71065=ORIENTED_EDGE('',*,*,#47329,.F.);
#71066=ORIENTED_EDGE('',*,*,#51444,.F.);
#71067=ORIENTED_EDGE('',*,*,#49548,.F.);
#71068=ORIENTED_EDGE('',*,*,#51443,.T.);
#71069=ORIENTED_EDGE('',*,*,#49549,.F.);
#71070=ORIENTED_EDGE('',*,*,#51444,.T.);
#71071=ORIENTED_EDGE('',*,*,#47307,.F.);
#71072=ORIENTED_EDGE('',*,*,#47303,.T.);
#71073=ORIENTED_EDGE('',*,*,#51445,.F.);
#71074=ORIENTED_EDGE('',*,*,#49589,.F.);
#71075=ORIENTED_EDGE('',*,*,#51446,.F.);
#71076=ORIENTED_EDGE('',*,*,#47259,.F.);
#71077=ORIENTED_EDGE('',*,*,#51446,.T.);
#71078=ORIENTED_EDGE('',*,*,#49588,.F.);
#71079=ORIENTED_EDGE('',*,*,#51447,.F.);
#71080=ORIENTED_EDGE('',*,*,#47268,.F.);
#71081=ORIENTED_EDGE('',*,*,#47258,.T.);
#71082=ORIENTED_EDGE('',*,*,#47262,.F.);
#71083=ORIENTED_EDGE('',*,*,#51448,.F.);
#71084=ORIENTED_EDGE('',*,*,#49590,.F.);
#71085=ORIENTED_EDGE('',*,*,#51445,.T.);
#71086=ORIENTED_EDGE('',*,*,#51447,.T.);
#71087=ORIENTED_EDGE('',*,*,#49587,.F.);
#71088=ORIENTED_EDGE('',*,*,#51449,.F.);
#71089=ORIENTED_EDGE('',*,*,#47253,.F.);
#71090=ORIENTED_EDGE('',*,*,#51448,.T.);
#71091=ORIENTED_EDGE('',*,*,#47266,.F.);
#71092=ORIENTED_EDGE('',*,*,#51450,.F.);
#71093=ORIENTED_EDGE('',*,*,#49579,.F.);
#71094=ORIENTED_EDGE('',*,*,#51449,.T.);
#71095=ORIENTED_EDGE('',*,*,#49586,.F.);
#71096=ORIENTED_EDGE('',*,*,#51451,.F.);
#71097=ORIENTED_EDGE('',*,*,#47270,.F.);
#71098=ORIENTED_EDGE('',*,*,#51450,.T.);
#71099=ORIENTED_EDGE('',*,*,#46153,.F.);
#71100=ORIENTED_EDGE('',*,*,#51452,.F.);
#71101=ORIENTED_EDGE('',*,*,#49580,.F.);
#71102=ORIENTED_EDGE('',*,*,#51451,.T.);
#71103=ORIENTED_EDGE('',*,*,#49585,.F.);
#71104=ORIENTED_EDGE('',*,*,#51453,.F.);
#71105=ORIENTED_EDGE('',*,*,#47245,.T.);
#71106=ORIENTED_EDGE('',*,*,#47249,.F.);
#71107=ORIENTED_EDGE('',*,*,#51452,.T.);
#71108=ORIENTED_EDGE('',*,*,#46152,.F.);
#71109=ORIENTED_EDGE('',*,*,#51454,.F.);
#71110=ORIENTED_EDGE('',*,*,#50301,.F.);
#71111=ORIENTED_EDGE('',*,*,#51453,.T.);
#71112=ORIENTED_EDGE('',*,*,#49584,.F.);
#71113=ORIENTED_EDGE('',*,*,#51455,.F.);
#71114=ORIENTED_EDGE('',*,*,#47246,.F.);
#71115=ORIENTED_EDGE('',*,*,#51454,.T.);
#71116=ORIENTED_EDGE('',*,*,#46151,.F.);
#71117=ORIENTED_EDGE('',*,*,#51456,.F.);
#71118=ORIENTED_EDGE('',*,*,#49564,.F.);
#71119=ORIENTED_EDGE('',*,*,#51455,.T.);
#71120=ORIENTED_EDGE('',*,*,#49583,.F.);
#71121=ORIENTED_EDGE('',*,*,#51457,.F.);
#71122=ORIENTED_EDGE('',*,*,#47264,.F.);
#71123=ORIENTED_EDGE('',*,*,#51456,.T.);
#71124=ORIENTED_EDGE('',*,*,#46150,.F.);
#71125=ORIENTED_EDGE('',*,*,#51458,.F.);
#71126=ORIENTED_EDGE('',*,*,#50303,.F.);
#71127=ORIENTED_EDGE('',*,*,#51457,.T.);
#71128=ORIENTED_EDGE('',*,*,#49582,.F.);
#71129=ORIENTED_EDGE('',*,*,#51459,.F.);
#71130=ORIENTED_EDGE('',*,*,#46580,.F.);
#71131=ORIENTED_EDGE('',*,*,#51458,.T.);
#71132=ORIENTED_EDGE('',*,*,#46149,.F.);
#71133=ORIENTED_EDGE('',*,*,#51460,.F.);
#71134=ORIENTED_EDGE('',*,*,#49570,.F.);
#71135=ORIENTED_EDGE('',*,*,#51459,.T.);
#71136=ORIENTED_EDGE('',*,*,#50302,.F.);
#71137=ORIENTED_EDGE('',*,*,#51461,.F.);
#71138=ORIENTED_EDGE('',*,*,#46581,.F.);
#71139=ORIENTED_EDGE('',*,*,#51460,.T.);
#71140=ORIENTED_EDGE('',*,*,#47295,.F.);
#71141=ORIENTED_EDGE('',*,*,#51462,.F.);
#71142=ORIENTED_EDGE('',*,*,#49571,.F.);
#71143=ORIENTED_EDGE('',*,*,#51461,.T.);
#71144=ORIENTED_EDGE('',*,*,#49566,.F.);
#71145=ORIENTED_EDGE('',*,*,#51463,.F.);
#71146=ORIENTED_EDGE('',*,*,#46582,.F.);
#71147=ORIENTED_EDGE('',*,*,#47290,.F.);
#71148=ORIENTED_EDGE('',*,*,#47286,.T.);
#71149=ORIENTED_EDGE('',*,*,#51464,.F.);
#71150=ORIENTED_EDGE('',*,*,#49572,.F.);
#71151=ORIENTED_EDGE('',*,*,#51462,.T.);
#71152=ORIENTED_EDGE('',*,*,#51463,.T.);
#71153=ORIENTED_EDGE('',*,*,#50304,.F.);
#71154=ORIENTED_EDGE('',*,*,#51465,.F.);
#71155=ORIENTED_EDGE('',*,*,#46583,.F.);
#71156=ORIENTED_EDGE('',*,*,#51464,.T.);
#71157=ORIENTED_EDGE('',*,*,#47285,.F.);
#71158=ORIENTED_EDGE('',*,*,#51466,.F.);
#71159=ORIENTED_EDGE('',*,*,#49573,.F.);
#71160=ORIENTED_EDGE('',*,*,#51465,.T.);
#71161=ORIENTED_EDGE('',*,*,#49568,.F.);
#71162=ORIENTED_EDGE('',*,*,#51467,.F.);
#71163=ORIENTED_EDGE('',*,*,#46584,.F.);
#71164=ORIENTED_EDGE('',*,*,#51466,.T.);
#71165=ORIENTED_EDGE('',*,*,#47297,.F.);
#71166=ORIENTED_EDGE('',*,*,#51468,.F.);
#71167=ORIENTED_EDGE('',*,*,#49574,.F.);
#71168=ORIENTED_EDGE('',*,*,#51467,.T.);
#71169=ORIENTED_EDGE('',*,*,#49567,.F.);
#71170=ORIENTED_EDGE('',*,*,#51469,.F.);
#71171=ORIENTED_EDGE('',*,*,#47293,.F.);
#71172=ORIENTED_EDGE('',*,*,#51468,.T.);
#71173=ORIENTED_EDGE('',*,*,#47281,.F.);
#71174=ORIENTED_EDGE('',*,*,#51470,.F.);
#71175=ORIENTED_EDGE('',*,*,#49575,.F.);
#71176=ORIENTED_EDGE('',*,*,#51469,.T.);
#71177=ORIENTED_EDGE('',*,*,#49578,.F.);
#71178=ORIENTED_EDGE('',*,*,#51471,.F.);
#71179=ORIENTED_EDGE('',*,*,#47272,.F.);
#71180=ORIENTED_EDGE('',*,*,#51470,.T.);
#71181=ORIENTED_EDGE('',*,*,#47299,.F.);
#71182=ORIENTED_EDGE('',*,*,#51472,.F.);
#71183=ORIENTED_EDGE('',*,*,#49576,.F.);
#71184=ORIENTED_EDGE('',*,*,#51471,.T.);
#71185=ORIENTED_EDGE('',*,*,#49577,.F.);
#71186=ORIENTED_EDGE('',*,*,#51472,.T.);
#71187=ORIENTED_EDGE('',*,*,#47277,.F.);
#71188=ORIENTED_EDGE('',*,*,#47273,.T.);
#71189=ORIENTED_EDGE('',*,*,#51473,.F.);
#71190=ORIENTED_EDGE('',*,*,#49617,.F.);
#71191=ORIENTED_EDGE('',*,*,#51474,.F.);
#71192=ORIENTED_EDGE('',*,*,#47229,.F.);
#71193=ORIENTED_EDGE('',*,*,#51474,.T.);
#71194=ORIENTED_EDGE('',*,*,#49616,.F.);
#71195=ORIENTED_EDGE('',*,*,#51475,.F.);
#71196=ORIENTED_EDGE('',*,*,#47238,.F.);
#71197=ORIENTED_EDGE('',*,*,#47228,.T.);
#71198=ORIENTED_EDGE('',*,*,#47232,.F.);
#71199=ORIENTED_EDGE('',*,*,#51476,.F.);
#71200=ORIENTED_EDGE('',*,*,#49618,.F.);
#71201=ORIENTED_EDGE('',*,*,#51473,.T.);
#71202=ORIENTED_EDGE('',*,*,#51475,.T.);
#71203=ORIENTED_EDGE('',*,*,#49615,.F.);
#71204=ORIENTED_EDGE('',*,*,#51477,.F.);
#71205=ORIENTED_EDGE('',*,*,#47223,.F.);
#71206=ORIENTED_EDGE('',*,*,#51476,.T.);
#71207=ORIENTED_EDGE('',*,*,#47236,.F.);
#71208=ORIENTED_EDGE('',*,*,#51478,.F.);
#71209=ORIENTED_EDGE('',*,*,#49607,.F.);
#71210=ORIENTED_EDGE('',*,*,#51477,.T.);
#71211=ORIENTED_EDGE('',*,*,#49614,.F.);
#71212=ORIENTED_EDGE('',*,*,#51479,.F.);
#71213=ORIENTED_EDGE('',*,*,#47240,.F.);
#71214=ORIENTED_EDGE('',*,*,#51478,.T.);
#71215=ORIENTED_EDGE('',*,*,#46159,.F.);
#71216=ORIENTED_EDGE('',*,*,#51480,.F.);
#71217=ORIENTED_EDGE('',*,*,#49608,.F.);
#71218=ORIENTED_EDGE('',*,*,#51479,.T.);
#71219=ORIENTED_EDGE('',*,*,#49613,.F.);
#71220=ORIENTED_EDGE('',*,*,#51481,.F.);
#71221=ORIENTED_EDGE('',*,*,#47215,.T.);
#71222=ORIENTED_EDGE('',*,*,#47219,.F.);
#71223=ORIENTED_EDGE('',*,*,#51480,.T.);
#71224=ORIENTED_EDGE('',*,*,#46158,.F.);
#71225=ORIENTED_EDGE('',*,*,#51482,.F.);
#71226=ORIENTED_EDGE('',*,*,#50305,.F.);
#71227=ORIENTED_EDGE('',*,*,#51481,.T.);
#71228=ORIENTED_EDGE('',*,*,#49612,.F.);
#71229=ORIENTED_EDGE('',*,*,#51483,.F.);
#71230=ORIENTED_EDGE('',*,*,#47216,.F.);
#71231=ORIENTED_EDGE('',*,*,#51482,.T.);
#71232=ORIENTED_EDGE('',*,*,#46157,.F.);
#71233=ORIENTED_EDGE('',*,*,#51484,.F.);
#71234=ORIENTED_EDGE('',*,*,#49592,.F.);
#71235=ORIENTED_EDGE('',*,*,#51483,.T.);
#71236=ORIENTED_EDGE('',*,*,#49611,.F.);
#71237=ORIENTED_EDGE('',*,*,#51485,.F.);
#71238=ORIENTED_EDGE('',*,*,#47234,.F.);
#71239=ORIENTED_EDGE('',*,*,#51484,.T.);
#71240=ORIENTED_EDGE('',*,*,#46156,.F.);
#71241=ORIENTED_EDGE('',*,*,#51486,.F.);
#71242=ORIENTED_EDGE('',*,*,#50307,.F.);
#71243=ORIENTED_EDGE('',*,*,#51485,.T.);
#71244=ORIENTED_EDGE('',*,*,#49610,.F.);
#71245=ORIENTED_EDGE('',*,*,#51487,.F.);
#71246=ORIENTED_EDGE('',*,*,#46574,.F.);
#71247=ORIENTED_EDGE('',*,*,#51486,.T.);
#71248=ORIENTED_EDGE('',*,*,#46155,.F.);
#71249=ORIENTED_EDGE('',*,*,#51488,.F.);
#71250=ORIENTED_EDGE('',*,*,#49598,.F.);
#71251=ORIENTED_EDGE('',*,*,#51487,.T.);
#71252=ORIENTED_EDGE('',*,*,#50306,.F.);
#71253=ORIENTED_EDGE('',*,*,#51489,.F.);
#71254=ORIENTED_EDGE('',*,*,#46575,.F.);
#71255=ORIENTED_EDGE('',*,*,#51488,.T.);
#71256=ORIENTED_EDGE('',*,*,#47265,.F.);
#71257=ORIENTED_EDGE('',*,*,#51490,.F.);
#71258=ORIENTED_EDGE('',*,*,#49599,.F.);
#71259=ORIENTED_EDGE('',*,*,#51489,.T.);
#71260=ORIENTED_EDGE('',*,*,#49594,.F.);
#71261=ORIENTED_EDGE('',*,*,#51491,.F.);
#71262=ORIENTED_EDGE('',*,*,#46576,.F.);
#71263=ORIENTED_EDGE('',*,*,#47260,.F.);
#71264=ORIENTED_EDGE('',*,*,#47256,.T.);
#71265=ORIENTED_EDGE('',*,*,#51492,.F.);
#71266=ORIENTED_EDGE('',*,*,#49600,.F.);
#71267=ORIENTED_EDGE('',*,*,#51490,.T.);
#71268=ORIENTED_EDGE('',*,*,#51491,.T.);
#71269=ORIENTED_EDGE('',*,*,#50308,.F.);
#71270=ORIENTED_EDGE('',*,*,#51493,.F.);
#71271=ORIENTED_EDGE('',*,*,#46577,.F.);
#71272=ORIENTED_EDGE('',*,*,#51492,.T.);
#71273=ORIENTED_EDGE('',*,*,#47255,.F.);
#71274=ORIENTED_EDGE('',*,*,#51494,.F.);
#71275=ORIENTED_EDGE('',*,*,#49601,.F.);
#71276=ORIENTED_EDGE('',*,*,#51493,.T.);
#71277=ORIENTED_EDGE('',*,*,#49596,.F.);
#71278=ORIENTED_EDGE('',*,*,#51495,.F.);
#71279=ORIENTED_EDGE('',*,*,#46578,.F.);
#71280=ORIENTED_EDGE('',*,*,#51494,.T.);
#71281=ORIENTED_EDGE('',*,*,#47267,.F.);
#71282=ORIENTED_EDGE('',*,*,#51496,.F.);
#71283=ORIENTED_EDGE('',*,*,#49602,.F.);
#71284=ORIENTED_EDGE('',*,*,#51495,.T.);
#71285=ORIENTED_EDGE('',*,*,#49595,.F.);
#71286=ORIENTED_EDGE('',*,*,#51497,.F.);
#71287=ORIENTED_EDGE('',*,*,#47263,.F.);
#71288=ORIENTED_EDGE('',*,*,#51496,.T.);
#71289=ORIENTED_EDGE('',*,*,#47251,.F.);
#71290=ORIENTED_EDGE('',*,*,#51498,.F.);
#71291=ORIENTED_EDGE('',*,*,#49603,.F.);
#71292=ORIENTED_EDGE('',*,*,#51497,.T.);
#71293=ORIENTED_EDGE('',*,*,#49606,.F.);
#71294=ORIENTED_EDGE('',*,*,#51499,.F.);
#71295=ORIENTED_EDGE('',*,*,#47242,.F.);
#71296=ORIENTED_EDGE('',*,*,#51498,.T.);
#71297=ORIENTED_EDGE('',*,*,#47269,.F.);
#71298=ORIENTED_EDGE('',*,*,#51500,.F.);
#71299=ORIENTED_EDGE('',*,*,#49604,.F.);
#71300=ORIENTED_EDGE('',*,*,#51499,.T.);
#71301=ORIENTED_EDGE('',*,*,#49605,.F.);
#71302=ORIENTED_EDGE('',*,*,#51500,.T.);
#71303=ORIENTED_EDGE('',*,*,#47247,.F.);
#71304=ORIENTED_EDGE('',*,*,#47243,.T.);
#71305=ORIENTED_EDGE('',*,*,#51501,.F.);
#71306=ORIENTED_EDGE('',*,*,#49645,.F.);
#71307=ORIENTED_EDGE('',*,*,#51502,.F.);
#71308=ORIENTED_EDGE('',*,*,#47199,.F.);
#71309=ORIENTED_EDGE('',*,*,#51502,.T.);
#71310=ORIENTED_EDGE('',*,*,#49644,.F.);
#71311=ORIENTED_EDGE('',*,*,#51503,.F.);
#71312=ORIENTED_EDGE('',*,*,#47208,.F.);
#71313=ORIENTED_EDGE('',*,*,#47198,.T.);
#71314=ORIENTED_EDGE('',*,*,#47202,.F.);
#71315=ORIENTED_EDGE('',*,*,#51504,.F.);
#71316=ORIENTED_EDGE('',*,*,#49646,.F.);
#71317=ORIENTED_EDGE('',*,*,#51501,.T.);
#71318=ORIENTED_EDGE('',*,*,#51503,.T.);
#71319=ORIENTED_EDGE('',*,*,#49643,.F.);
#71320=ORIENTED_EDGE('',*,*,#51505,.F.);
#71321=ORIENTED_EDGE('',*,*,#47193,.F.);
#71322=ORIENTED_EDGE('',*,*,#51504,.T.);
#71323=ORIENTED_EDGE('',*,*,#47206,.F.);
#71324=ORIENTED_EDGE('',*,*,#51506,.F.);
#71325=ORIENTED_EDGE('',*,*,#49635,.F.);
#71326=ORIENTED_EDGE('',*,*,#51505,.T.);
#71327=ORIENTED_EDGE('',*,*,#49642,.F.);
#71328=ORIENTED_EDGE('',*,*,#51507,.F.);
#71329=ORIENTED_EDGE('',*,*,#47210,.F.);
#71330=ORIENTED_EDGE('',*,*,#51506,.T.);
#71331=ORIENTED_EDGE('',*,*,#46165,.F.);
#71332=ORIENTED_EDGE('',*,*,#51508,.F.);
#71333=ORIENTED_EDGE('',*,*,#49636,.F.);
#71334=ORIENTED_EDGE('',*,*,#51507,.T.);
#71335=ORIENTED_EDGE('',*,*,#49641,.F.);
#71336=ORIENTED_EDGE('',*,*,#51509,.F.);
#71337=ORIENTED_EDGE('',*,*,#47185,.T.);
#71338=ORIENTED_EDGE('',*,*,#47189,.F.);
#71339=ORIENTED_EDGE('',*,*,#51508,.T.);
#71340=ORIENTED_EDGE('',*,*,#46164,.F.);
#71341=ORIENTED_EDGE('',*,*,#51510,.F.);
#71342=ORIENTED_EDGE('',*,*,#50309,.F.);
#71343=ORIENTED_EDGE('',*,*,#51509,.T.);
#71344=ORIENTED_EDGE('',*,*,#49640,.F.);
#71345=ORIENTED_EDGE('',*,*,#51511,.F.);
#71346=ORIENTED_EDGE('',*,*,#47186,.F.);
#71347=ORIENTED_EDGE('',*,*,#51510,.T.);
#71348=ORIENTED_EDGE('',*,*,#46163,.F.);
#71349=ORIENTED_EDGE('',*,*,#51512,.F.);
#71350=ORIENTED_EDGE('',*,*,#49620,.F.);
#71351=ORIENTED_EDGE('',*,*,#51511,.T.);
#71352=ORIENTED_EDGE('',*,*,#49639,.F.);
#71353=ORIENTED_EDGE('',*,*,#51513,.F.);
#71354=ORIENTED_EDGE('',*,*,#47204,.F.);
#71355=ORIENTED_EDGE('',*,*,#51512,.T.);
#71356=ORIENTED_EDGE('',*,*,#46162,.F.);
#71357=ORIENTED_EDGE('',*,*,#51514,.F.);
#71358=ORIENTED_EDGE('',*,*,#50311,.F.);
#71359=ORIENTED_EDGE('',*,*,#51513,.T.);
#71360=ORIENTED_EDGE('',*,*,#49638,.F.);
#71361=ORIENTED_EDGE('',*,*,#51515,.F.);
#71362=ORIENTED_EDGE('',*,*,#46568,.F.);
#71363=ORIENTED_EDGE('',*,*,#51514,.T.);
#71364=ORIENTED_EDGE('',*,*,#46161,.F.);
#71365=ORIENTED_EDGE('',*,*,#51516,.F.);
#71366=ORIENTED_EDGE('',*,*,#49626,.F.);
#71367=ORIENTED_EDGE('',*,*,#51515,.T.);
#71368=ORIENTED_EDGE('',*,*,#50310,.F.);
#71369=ORIENTED_EDGE('',*,*,#51517,.F.);
#71370=ORIENTED_EDGE('',*,*,#46569,.F.);
#71371=ORIENTED_EDGE('',*,*,#51516,.T.);
#71372=ORIENTED_EDGE('',*,*,#47235,.F.);
#71373=ORIENTED_EDGE('',*,*,#51518,.F.);
#71374=ORIENTED_EDGE('',*,*,#49627,.F.);
#71375=ORIENTED_EDGE('',*,*,#51517,.T.);
#71376=ORIENTED_EDGE('',*,*,#49622,.F.);
#71377=ORIENTED_EDGE('',*,*,#51519,.F.);
#71378=ORIENTED_EDGE('',*,*,#46570,.F.);
#71379=ORIENTED_EDGE('',*,*,#47230,.F.);
#71380=ORIENTED_EDGE('',*,*,#47226,.T.);
#71381=ORIENTED_EDGE('',*,*,#51520,.F.);
#71382=ORIENTED_EDGE('',*,*,#49628,.F.);
#71383=ORIENTED_EDGE('',*,*,#51518,.T.);
#71384=ORIENTED_EDGE('',*,*,#51519,.T.);
#71385=ORIENTED_EDGE('',*,*,#50312,.F.);
#71386=ORIENTED_EDGE('',*,*,#51521,.F.);
#71387=ORIENTED_EDGE('',*,*,#46571,.F.);
#71388=ORIENTED_EDGE('',*,*,#51520,.T.);
#71389=ORIENTED_EDGE('',*,*,#47225,.F.);
#71390=ORIENTED_EDGE('',*,*,#51522,.F.);
#71391=ORIENTED_EDGE('',*,*,#49629,.F.);
#71392=ORIENTED_EDGE('',*,*,#51521,.T.);
#71393=ORIENTED_EDGE('',*,*,#49624,.F.);
#71394=ORIENTED_EDGE('',*,*,#51523,.F.);
#71395=ORIENTED_EDGE('',*,*,#46572,.F.);
#71396=ORIENTED_EDGE('',*,*,#51522,.T.);
#71397=ORIENTED_EDGE('',*,*,#47237,.F.);
#71398=ORIENTED_EDGE('',*,*,#51524,.F.);
#71399=ORIENTED_EDGE('',*,*,#49630,.F.);
#71400=ORIENTED_EDGE('',*,*,#51523,.T.);
#71401=ORIENTED_EDGE('',*,*,#49623,.F.);
#71402=ORIENTED_EDGE('',*,*,#51525,.F.);
#71403=ORIENTED_EDGE('',*,*,#47233,.F.);
#71404=ORIENTED_EDGE('',*,*,#51524,.T.);
#71405=ORIENTED_EDGE('',*,*,#47221,.F.);
#71406=ORIENTED_EDGE('',*,*,#51526,.F.);
#71407=ORIENTED_EDGE('',*,*,#49631,.F.);
#71408=ORIENTED_EDGE('',*,*,#51525,.T.);
#71409=ORIENTED_EDGE('',*,*,#49634,.F.);
#71410=ORIENTED_EDGE('',*,*,#51527,.F.);
#71411=ORIENTED_EDGE('',*,*,#47212,.F.);
#71412=ORIENTED_EDGE('',*,*,#51526,.T.);
#71413=ORIENTED_EDGE('',*,*,#47239,.F.);
#71414=ORIENTED_EDGE('',*,*,#51528,.F.);
#71415=ORIENTED_EDGE('',*,*,#49632,.F.);
#71416=ORIENTED_EDGE('',*,*,#51527,.T.);
#71417=ORIENTED_EDGE('',*,*,#49633,.F.);
#71418=ORIENTED_EDGE('',*,*,#51528,.T.);
#71419=ORIENTED_EDGE('',*,*,#47217,.F.);
#71420=ORIENTED_EDGE('',*,*,#47213,.T.);
#71421=ORIENTED_EDGE('',*,*,#51529,.F.);
#71422=ORIENTED_EDGE('',*,*,#49673,.F.);
#71423=ORIENTED_EDGE('',*,*,#51530,.F.);
#71424=ORIENTED_EDGE('',*,*,#47169,.F.);
#71425=ORIENTED_EDGE('',*,*,#51530,.T.);
#71426=ORIENTED_EDGE('',*,*,#49672,.F.);
#71427=ORIENTED_EDGE('',*,*,#51531,.F.);
#71428=ORIENTED_EDGE('',*,*,#47178,.F.);
#71429=ORIENTED_EDGE('',*,*,#47168,.T.);
#71430=ORIENTED_EDGE('',*,*,#47172,.F.);
#71431=ORIENTED_EDGE('',*,*,#51532,.F.);
#71432=ORIENTED_EDGE('',*,*,#49674,.F.);
#71433=ORIENTED_EDGE('',*,*,#51529,.T.);
#71434=ORIENTED_EDGE('',*,*,#51531,.T.);
#71435=ORIENTED_EDGE('',*,*,#49671,.F.);
#71436=ORIENTED_EDGE('',*,*,#51533,.F.);
#71437=ORIENTED_EDGE('',*,*,#47163,.F.);
#71438=ORIENTED_EDGE('',*,*,#51532,.T.);
#71439=ORIENTED_EDGE('',*,*,#47176,.F.);
#71440=ORIENTED_EDGE('',*,*,#51534,.F.);
#71441=ORIENTED_EDGE('',*,*,#49663,.F.);
#71442=ORIENTED_EDGE('',*,*,#51533,.T.);
#71443=ORIENTED_EDGE('',*,*,#49670,.F.);
#71444=ORIENTED_EDGE('',*,*,#51535,.F.);
#71445=ORIENTED_EDGE('',*,*,#47180,.F.);
#71446=ORIENTED_EDGE('',*,*,#51534,.T.);
#71447=ORIENTED_EDGE('',*,*,#46171,.F.);
#71448=ORIENTED_EDGE('',*,*,#51536,.F.);
#71449=ORIENTED_EDGE('',*,*,#49664,.F.);
#71450=ORIENTED_EDGE('',*,*,#51535,.T.);
#71451=ORIENTED_EDGE('',*,*,#49669,.F.);
#71452=ORIENTED_EDGE('',*,*,#51537,.F.);
#71453=ORIENTED_EDGE('',*,*,#47155,.T.);
#71454=ORIENTED_EDGE('',*,*,#47159,.F.);
#71455=ORIENTED_EDGE('',*,*,#51536,.T.);
#71456=ORIENTED_EDGE('',*,*,#46170,.F.);
#71457=ORIENTED_EDGE('',*,*,#51538,.F.);
#71458=ORIENTED_EDGE('',*,*,#50313,.F.);
#71459=ORIENTED_EDGE('',*,*,#51537,.T.);
#71460=ORIENTED_EDGE('',*,*,#49668,.F.);
#71461=ORIENTED_EDGE('',*,*,#51539,.F.);
#71462=ORIENTED_EDGE('',*,*,#47156,.F.);
#71463=ORIENTED_EDGE('',*,*,#51538,.T.);
#71464=ORIENTED_EDGE('',*,*,#46169,.F.);
#71465=ORIENTED_EDGE('',*,*,#51540,.F.);
#71466=ORIENTED_EDGE('',*,*,#49648,.F.);
#71467=ORIENTED_EDGE('',*,*,#51539,.T.);
#71468=ORIENTED_EDGE('',*,*,#49667,.F.);
#71469=ORIENTED_EDGE('',*,*,#51541,.F.);
#71470=ORIENTED_EDGE('',*,*,#47174,.F.);
#71471=ORIENTED_EDGE('',*,*,#51540,.T.);
#71472=ORIENTED_EDGE('',*,*,#46168,.F.);
#71473=ORIENTED_EDGE('',*,*,#51542,.F.);
#71474=ORIENTED_EDGE('',*,*,#50315,.F.);
#71475=ORIENTED_EDGE('',*,*,#51541,.T.);
#71476=ORIENTED_EDGE('',*,*,#49666,.F.);
#71477=ORIENTED_EDGE('',*,*,#51543,.F.);
#71478=ORIENTED_EDGE('',*,*,#46562,.F.);
#71479=ORIENTED_EDGE('',*,*,#51542,.T.);
#71480=ORIENTED_EDGE('',*,*,#46167,.F.);
#71481=ORIENTED_EDGE('',*,*,#51544,.F.);
#71482=ORIENTED_EDGE('',*,*,#49654,.F.);
#71483=ORIENTED_EDGE('',*,*,#51543,.T.);
#71484=ORIENTED_EDGE('',*,*,#50314,.F.);
#71485=ORIENTED_EDGE('',*,*,#51545,.F.);
#71486=ORIENTED_EDGE('',*,*,#46563,.F.);
#71487=ORIENTED_EDGE('',*,*,#51544,.T.);
#71488=ORIENTED_EDGE('',*,*,#47205,.F.);
#71489=ORIENTED_EDGE('',*,*,#51546,.F.);
#71490=ORIENTED_EDGE('',*,*,#49655,.F.);
#71491=ORIENTED_EDGE('',*,*,#51545,.T.);
#71492=ORIENTED_EDGE('',*,*,#49650,.F.);
#71493=ORIENTED_EDGE('',*,*,#51547,.F.);
#71494=ORIENTED_EDGE('',*,*,#46564,.F.);
#71495=ORIENTED_EDGE('',*,*,#47200,.F.);
#71496=ORIENTED_EDGE('',*,*,#47196,.T.);
#71497=ORIENTED_EDGE('',*,*,#51548,.F.);
#71498=ORIENTED_EDGE('',*,*,#49656,.F.);
#71499=ORIENTED_EDGE('',*,*,#51546,.T.);
#71500=ORIENTED_EDGE('',*,*,#51547,.T.);
#71501=ORIENTED_EDGE('',*,*,#50316,.F.);
#71502=ORIENTED_EDGE('',*,*,#51549,.F.);
#71503=ORIENTED_EDGE('',*,*,#46565,.F.);
#71504=ORIENTED_EDGE('',*,*,#51548,.T.);
#71505=ORIENTED_EDGE('',*,*,#47195,.F.);
#71506=ORIENTED_EDGE('',*,*,#51550,.F.);
#71507=ORIENTED_EDGE('',*,*,#49657,.F.);
#71508=ORIENTED_EDGE('',*,*,#51549,.T.);
#71509=ORIENTED_EDGE('',*,*,#49652,.F.);
#71510=ORIENTED_EDGE('',*,*,#51551,.F.);
#71511=ORIENTED_EDGE('',*,*,#46566,.F.);
#71512=ORIENTED_EDGE('',*,*,#51550,.T.);
#71513=ORIENTED_EDGE('',*,*,#47207,.F.);
#71514=ORIENTED_EDGE('',*,*,#51552,.F.);
#71515=ORIENTED_EDGE('',*,*,#49658,.F.);
#71516=ORIENTED_EDGE('',*,*,#51551,.T.);
#71517=ORIENTED_EDGE('',*,*,#49651,.F.);
#71518=ORIENTED_EDGE('',*,*,#51553,.F.);
#71519=ORIENTED_EDGE('',*,*,#47203,.F.);
#71520=ORIENTED_EDGE('',*,*,#51552,.T.);
#71521=ORIENTED_EDGE('',*,*,#47191,.F.);
#71522=ORIENTED_EDGE('',*,*,#51554,.F.);
#71523=ORIENTED_EDGE('',*,*,#49659,.F.);
#71524=ORIENTED_EDGE('',*,*,#51553,.T.);
#71525=ORIENTED_EDGE('',*,*,#49662,.F.);
#71526=ORIENTED_EDGE('',*,*,#51555,.F.);
#71527=ORIENTED_EDGE('',*,*,#47182,.F.);
#71528=ORIENTED_EDGE('',*,*,#51554,.T.);
#71529=ORIENTED_EDGE('',*,*,#47209,.F.);
#71530=ORIENTED_EDGE('',*,*,#51556,.F.);
#71531=ORIENTED_EDGE('',*,*,#49660,.F.);
#71532=ORIENTED_EDGE('',*,*,#51555,.T.);
#71533=ORIENTED_EDGE('',*,*,#49661,.F.);
#71534=ORIENTED_EDGE('',*,*,#51556,.T.);
#71535=ORIENTED_EDGE('',*,*,#47187,.F.);
#71536=ORIENTED_EDGE('',*,*,#47183,.T.);
#71537=ORIENTED_EDGE('',*,*,#51557,.F.);
#71538=ORIENTED_EDGE('',*,*,#49701,.F.);
#71539=ORIENTED_EDGE('',*,*,#51558,.F.);
#71540=ORIENTED_EDGE('',*,*,#47139,.F.);
#71541=ORIENTED_EDGE('',*,*,#51558,.T.);
#71542=ORIENTED_EDGE('',*,*,#49700,.F.);
#71543=ORIENTED_EDGE('',*,*,#51559,.F.);
#71544=ORIENTED_EDGE('',*,*,#47148,.F.);
#71545=ORIENTED_EDGE('',*,*,#47138,.T.);
#71546=ORIENTED_EDGE('',*,*,#47142,.F.);
#71547=ORIENTED_EDGE('',*,*,#51560,.F.);
#71548=ORIENTED_EDGE('',*,*,#49702,.F.);
#71549=ORIENTED_EDGE('',*,*,#51557,.T.);
#71550=ORIENTED_EDGE('',*,*,#51559,.T.);
#71551=ORIENTED_EDGE('',*,*,#49699,.F.);
#71552=ORIENTED_EDGE('',*,*,#51561,.F.);
#71553=ORIENTED_EDGE('',*,*,#47133,.F.);
#71554=ORIENTED_EDGE('',*,*,#51560,.T.);
#71555=ORIENTED_EDGE('',*,*,#47146,.F.);
#71556=ORIENTED_EDGE('',*,*,#51562,.F.);
#71557=ORIENTED_EDGE('',*,*,#49691,.F.);
#71558=ORIENTED_EDGE('',*,*,#51561,.T.);
#71559=ORIENTED_EDGE('',*,*,#49698,.F.);
#71560=ORIENTED_EDGE('',*,*,#51563,.F.);
#71561=ORIENTED_EDGE('',*,*,#47150,.F.);
#71562=ORIENTED_EDGE('',*,*,#51562,.T.);
#71563=ORIENTED_EDGE('',*,*,#46177,.F.);
#71564=ORIENTED_EDGE('',*,*,#51564,.F.);
#71565=ORIENTED_EDGE('',*,*,#49692,.F.);
#71566=ORIENTED_EDGE('',*,*,#51563,.T.);
#71567=ORIENTED_EDGE('',*,*,#49697,.F.);
#71568=ORIENTED_EDGE('',*,*,#51565,.F.);
#71569=ORIENTED_EDGE('',*,*,#47125,.T.);
#71570=ORIENTED_EDGE('',*,*,#47129,.F.);
#71571=ORIENTED_EDGE('',*,*,#51564,.T.);
#71572=ORIENTED_EDGE('',*,*,#46176,.F.);
#71573=ORIENTED_EDGE('',*,*,#51566,.F.);
#71574=ORIENTED_EDGE('',*,*,#50317,.F.);
#71575=ORIENTED_EDGE('',*,*,#51565,.T.);
#71576=ORIENTED_EDGE('',*,*,#49696,.F.);
#71577=ORIENTED_EDGE('',*,*,#51567,.F.);
#71578=ORIENTED_EDGE('',*,*,#47126,.F.);
#71579=ORIENTED_EDGE('',*,*,#51566,.T.);
#71580=ORIENTED_EDGE('',*,*,#46175,.F.);
#71581=ORIENTED_EDGE('',*,*,#51568,.F.);
#71582=ORIENTED_EDGE('',*,*,#49676,.F.);
#71583=ORIENTED_EDGE('',*,*,#51567,.T.);
#71584=ORIENTED_EDGE('',*,*,#49695,.F.);
#71585=ORIENTED_EDGE('',*,*,#51569,.F.);
#71586=ORIENTED_EDGE('',*,*,#47144,.F.);
#71587=ORIENTED_EDGE('',*,*,#51568,.T.);
#71588=ORIENTED_EDGE('',*,*,#46174,.F.);
#71589=ORIENTED_EDGE('',*,*,#51570,.F.);
#71590=ORIENTED_EDGE('',*,*,#50319,.F.);
#71591=ORIENTED_EDGE('',*,*,#51569,.T.);
#71592=ORIENTED_EDGE('',*,*,#49694,.F.);
#71593=ORIENTED_EDGE('',*,*,#51571,.F.);
#71594=ORIENTED_EDGE('',*,*,#46556,.F.);
#71595=ORIENTED_EDGE('',*,*,#51570,.T.);
#71596=ORIENTED_EDGE('',*,*,#46173,.F.);
#71597=ORIENTED_EDGE('',*,*,#51572,.F.);
#71598=ORIENTED_EDGE('',*,*,#49682,.F.);
#71599=ORIENTED_EDGE('',*,*,#51571,.T.);
#71600=ORIENTED_EDGE('',*,*,#50318,.F.);
#71601=ORIENTED_EDGE('',*,*,#51573,.F.);
#71602=ORIENTED_EDGE('',*,*,#46557,.F.);
#71603=ORIENTED_EDGE('',*,*,#51572,.T.);
#71604=ORIENTED_EDGE('',*,*,#47175,.F.);
#71605=ORIENTED_EDGE('',*,*,#51574,.F.);
#71606=ORIENTED_EDGE('',*,*,#49683,.F.);
#71607=ORIENTED_EDGE('',*,*,#51573,.T.);
#71608=ORIENTED_EDGE('',*,*,#49678,.F.);
#71609=ORIENTED_EDGE('',*,*,#51575,.F.);
#71610=ORIENTED_EDGE('',*,*,#46558,.F.);
#71611=ORIENTED_EDGE('',*,*,#47170,.F.);
#71612=ORIENTED_EDGE('',*,*,#47166,.T.);
#71613=ORIENTED_EDGE('',*,*,#51576,.F.);
#71614=ORIENTED_EDGE('',*,*,#49684,.F.);
#71615=ORIENTED_EDGE('',*,*,#51574,.T.);
#71616=ORIENTED_EDGE('',*,*,#51575,.T.);
#71617=ORIENTED_EDGE('',*,*,#50320,.F.);
#71618=ORIENTED_EDGE('',*,*,#51577,.F.);
#71619=ORIENTED_EDGE('',*,*,#46559,.F.);
#71620=ORIENTED_EDGE('',*,*,#51576,.T.);
#71621=ORIENTED_EDGE('',*,*,#47165,.F.);
#71622=ORIENTED_EDGE('',*,*,#51578,.F.);
#71623=ORIENTED_EDGE('',*,*,#49685,.F.);
#71624=ORIENTED_EDGE('',*,*,#51577,.T.);
#71625=ORIENTED_EDGE('',*,*,#49680,.F.);
#71626=ORIENTED_EDGE('',*,*,#51579,.F.);
#71627=ORIENTED_EDGE('',*,*,#46560,.F.);
#71628=ORIENTED_EDGE('',*,*,#51578,.T.);
#71629=ORIENTED_EDGE('',*,*,#47177,.F.);
#71630=ORIENTED_EDGE('',*,*,#51580,.F.);
#71631=ORIENTED_EDGE('',*,*,#49686,.F.);
#71632=ORIENTED_EDGE('',*,*,#51579,.T.);
#71633=ORIENTED_EDGE('',*,*,#49679,.F.);
#71634=ORIENTED_EDGE('',*,*,#51581,.F.);
#71635=ORIENTED_EDGE('',*,*,#47173,.F.);
#71636=ORIENTED_EDGE('',*,*,#51580,.T.);
#71637=ORIENTED_EDGE('',*,*,#47161,.F.);
#71638=ORIENTED_EDGE('',*,*,#51582,.F.);
#71639=ORIENTED_EDGE('',*,*,#49687,.F.);
#71640=ORIENTED_EDGE('',*,*,#51581,.T.);
#71641=ORIENTED_EDGE('',*,*,#49690,.F.);
#71642=ORIENTED_EDGE('',*,*,#51583,.F.);
#71643=ORIENTED_EDGE('',*,*,#47152,.F.);
#71644=ORIENTED_EDGE('',*,*,#51582,.T.);
#71645=ORIENTED_EDGE('',*,*,#47179,.F.);
#71646=ORIENTED_EDGE('',*,*,#51584,.F.);
#71647=ORIENTED_EDGE('',*,*,#49688,.F.);
#71648=ORIENTED_EDGE('',*,*,#51583,.T.);
#71649=ORIENTED_EDGE('',*,*,#49689,.F.);
#71650=ORIENTED_EDGE('',*,*,#51584,.T.);
#71651=ORIENTED_EDGE('',*,*,#47157,.F.);
#71652=ORIENTED_EDGE('',*,*,#47153,.T.);
#71653=ORIENTED_EDGE('',*,*,#51585,.F.);
#71654=ORIENTED_EDGE('',*,*,#49729,.F.);
#71655=ORIENTED_EDGE('',*,*,#51586,.F.);
#71656=ORIENTED_EDGE('',*,*,#47109,.F.);
#71657=ORIENTED_EDGE('',*,*,#51586,.T.);
#71658=ORIENTED_EDGE('',*,*,#49728,.F.);
#71659=ORIENTED_EDGE('',*,*,#51587,.F.);
#71660=ORIENTED_EDGE('',*,*,#47118,.F.);
#71661=ORIENTED_EDGE('',*,*,#47108,.T.);
#71662=ORIENTED_EDGE('',*,*,#47112,.F.);
#71663=ORIENTED_EDGE('',*,*,#51588,.F.);
#71664=ORIENTED_EDGE('',*,*,#49730,.F.);
#71665=ORIENTED_EDGE('',*,*,#51585,.T.);
#71666=ORIENTED_EDGE('',*,*,#51587,.T.);
#71667=ORIENTED_EDGE('',*,*,#49727,.F.);
#71668=ORIENTED_EDGE('',*,*,#51589,.F.);
#71669=ORIENTED_EDGE('',*,*,#47103,.F.);
#71670=ORIENTED_EDGE('',*,*,#51588,.T.);
#71671=ORIENTED_EDGE('',*,*,#47116,.F.);
#71672=ORIENTED_EDGE('',*,*,#51590,.F.);
#71673=ORIENTED_EDGE('',*,*,#49719,.F.);
#71674=ORIENTED_EDGE('',*,*,#51589,.T.);
#71675=ORIENTED_EDGE('',*,*,#49726,.F.);
#71676=ORIENTED_EDGE('',*,*,#51591,.F.);
#71677=ORIENTED_EDGE('',*,*,#47120,.F.);
#71678=ORIENTED_EDGE('',*,*,#51590,.T.);
#71679=ORIENTED_EDGE('',*,*,#46183,.F.);
#71680=ORIENTED_EDGE('',*,*,#51592,.F.);
#71681=ORIENTED_EDGE('',*,*,#49720,.F.);
#71682=ORIENTED_EDGE('',*,*,#51591,.T.);
#71683=ORIENTED_EDGE('',*,*,#49725,.F.);
#71684=ORIENTED_EDGE('',*,*,#51593,.F.);
#71685=ORIENTED_EDGE('',*,*,#47095,.T.);
#71686=ORIENTED_EDGE('',*,*,#47099,.F.);
#71687=ORIENTED_EDGE('',*,*,#51592,.T.);
#71688=ORIENTED_EDGE('',*,*,#46182,.F.);
#71689=ORIENTED_EDGE('',*,*,#51594,.F.);
#71690=ORIENTED_EDGE('',*,*,#50321,.F.);
#71691=ORIENTED_EDGE('',*,*,#51593,.T.);
#71692=ORIENTED_EDGE('',*,*,#49724,.F.);
#71693=ORIENTED_EDGE('',*,*,#51595,.F.);
#71694=ORIENTED_EDGE('',*,*,#47096,.F.);
#71695=ORIENTED_EDGE('',*,*,#51594,.T.);
#71696=ORIENTED_EDGE('',*,*,#46181,.F.);
#71697=ORIENTED_EDGE('',*,*,#51596,.F.);
#71698=ORIENTED_EDGE('',*,*,#49704,.F.);
#71699=ORIENTED_EDGE('',*,*,#51595,.T.);
#71700=ORIENTED_EDGE('',*,*,#49723,.F.);
#71701=ORIENTED_EDGE('',*,*,#51597,.F.);
#71702=ORIENTED_EDGE('',*,*,#47114,.F.);
#71703=ORIENTED_EDGE('',*,*,#51596,.T.);
#71704=ORIENTED_EDGE('',*,*,#46180,.F.);
#71705=ORIENTED_EDGE('',*,*,#51598,.F.);
#71706=ORIENTED_EDGE('',*,*,#50323,.F.);
#71707=ORIENTED_EDGE('',*,*,#51597,.T.);
#71708=ORIENTED_EDGE('',*,*,#49722,.F.);
#71709=ORIENTED_EDGE('',*,*,#51599,.F.);
#71710=ORIENTED_EDGE('',*,*,#46550,.F.);
#71711=ORIENTED_EDGE('',*,*,#51598,.T.);
#71712=ORIENTED_EDGE('',*,*,#46179,.F.);
#71713=ORIENTED_EDGE('',*,*,#51600,.F.);
#71714=ORIENTED_EDGE('',*,*,#49710,.F.);
#71715=ORIENTED_EDGE('',*,*,#51599,.T.);
#71716=ORIENTED_EDGE('',*,*,#50322,.F.);
#71717=ORIENTED_EDGE('',*,*,#51601,.F.);
#71718=ORIENTED_EDGE('',*,*,#46551,.F.);
#71719=ORIENTED_EDGE('',*,*,#51600,.T.);
#71720=ORIENTED_EDGE('',*,*,#47145,.F.);
#71721=ORIENTED_EDGE('',*,*,#51602,.F.);
#71722=ORIENTED_EDGE('',*,*,#49711,.F.);
#71723=ORIENTED_EDGE('',*,*,#51601,.T.);
#71724=ORIENTED_EDGE('',*,*,#49706,.F.);
#71725=ORIENTED_EDGE('',*,*,#51603,.F.);
#71726=ORIENTED_EDGE('',*,*,#46552,.F.);
#71727=ORIENTED_EDGE('',*,*,#47140,.F.);
#71728=ORIENTED_EDGE('',*,*,#47136,.T.);
#71729=ORIENTED_EDGE('',*,*,#51604,.F.);
#71730=ORIENTED_EDGE('',*,*,#49712,.F.);
#71731=ORIENTED_EDGE('',*,*,#51602,.T.);
#71732=ORIENTED_EDGE('',*,*,#51603,.T.);
#71733=ORIENTED_EDGE('',*,*,#50324,.F.);
#71734=ORIENTED_EDGE('',*,*,#51605,.F.);
#71735=ORIENTED_EDGE('',*,*,#46553,.F.);
#71736=ORIENTED_EDGE('',*,*,#51604,.T.);
#71737=ORIENTED_EDGE('',*,*,#47135,.F.);
#71738=ORIENTED_EDGE('',*,*,#51606,.F.);
#71739=ORIENTED_EDGE('',*,*,#49713,.F.);
#71740=ORIENTED_EDGE('',*,*,#51605,.T.);
#71741=ORIENTED_EDGE('',*,*,#49708,.F.);
#71742=ORIENTED_EDGE('',*,*,#51607,.F.);
#71743=ORIENTED_EDGE('',*,*,#46554,.F.);
#71744=ORIENTED_EDGE('',*,*,#51606,.T.);
#71745=ORIENTED_EDGE('',*,*,#47147,.F.);
#71746=ORIENTED_EDGE('',*,*,#51608,.F.);
#71747=ORIENTED_EDGE('',*,*,#49714,.F.);
#71748=ORIENTED_EDGE('',*,*,#51607,.T.);
#71749=ORIENTED_EDGE('',*,*,#49707,.F.);
#71750=ORIENTED_EDGE('',*,*,#51609,.F.);
#71751=ORIENTED_EDGE('',*,*,#47143,.F.);
#71752=ORIENTED_EDGE('',*,*,#51608,.T.);
#71753=ORIENTED_EDGE('',*,*,#47131,.F.);
#71754=ORIENTED_EDGE('',*,*,#51610,.F.);
#71755=ORIENTED_EDGE('',*,*,#49715,.F.);
#71756=ORIENTED_EDGE('',*,*,#51609,.T.);
#71757=ORIENTED_EDGE('',*,*,#49718,.F.);
#71758=ORIENTED_EDGE('',*,*,#51611,.F.);
#71759=ORIENTED_EDGE('',*,*,#47122,.F.);
#71760=ORIENTED_EDGE('',*,*,#51610,.T.);
#71761=ORIENTED_EDGE('',*,*,#47149,.F.);
#71762=ORIENTED_EDGE('',*,*,#51612,.F.);
#71763=ORIENTED_EDGE('',*,*,#49716,.F.);
#71764=ORIENTED_EDGE('',*,*,#51611,.T.);
#71765=ORIENTED_EDGE('',*,*,#49717,.F.);
#71766=ORIENTED_EDGE('',*,*,#51612,.T.);
#71767=ORIENTED_EDGE('',*,*,#47127,.F.);
#71768=ORIENTED_EDGE('',*,*,#47123,.T.);
#71769=ORIENTED_EDGE('',*,*,#51613,.F.);
#71770=ORIENTED_EDGE('',*,*,#49755,.F.);
#71771=ORIENTED_EDGE('',*,*,#51614,.F.);
#71772=ORIENTED_EDGE('',*,*,#47079,.F.);
#71773=ORIENTED_EDGE('',*,*,#51614,.T.);
#71774=ORIENTED_EDGE('',*,*,#49754,.F.);
#71775=ORIENTED_EDGE('',*,*,#51615,.F.);
#71776=ORIENTED_EDGE('',*,*,#47088,.F.);
#71777=ORIENTED_EDGE('',*,*,#47078,.T.);
#71778=ORIENTED_EDGE('',*,*,#47082,.F.);
#71779=ORIENTED_EDGE('',*,*,#51616,.F.);
#71780=ORIENTED_EDGE('',*,*,#49756,.F.);
#71781=ORIENTED_EDGE('',*,*,#51613,.T.);
#71782=ORIENTED_EDGE('',*,*,#51615,.T.);
#71783=ORIENTED_EDGE('',*,*,#49753,.F.);
#71784=ORIENTED_EDGE('',*,*,#51617,.F.);
#71785=ORIENTED_EDGE('',*,*,#47073,.F.);
#71786=ORIENTED_EDGE('',*,*,#51616,.T.);
#71787=ORIENTED_EDGE('',*,*,#47086,.F.);
#71788=ORIENTED_EDGE('',*,*,#51618,.F.);
#71789=ORIENTED_EDGE('',*,*,#49745,.F.);
#71790=ORIENTED_EDGE('',*,*,#51617,.T.);
#71791=ORIENTED_EDGE('',*,*,#49752,.F.);
#71792=ORIENTED_EDGE('',*,*,#51619,.F.);
#71793=ORIENTED_EDGE('',*,*,#47090,.F.);
#71794=ORIENTED_EDGE('',*,*,#51618,.T.);
#71795=ORIENTED_EDGE('',*,*,#46188,.F.);
#71796=ORIENTED_EDGE('',*,*,#51620,.F.);
#71797=ORIENTED_EDGE('',*,*,#49746,.F.);
#71798=ORIENTED_EDGE('',*,*,#51619,.T.);
#71799=ORIENTED_EDGE('',*,*,#49751,.F.);
#71800=ORIENTED_EDGE('',*,*,#51621,.F.);
#71801=ORIENTED_EDGE('',*,*,#47065,.T.);
#71802=ORIENTED_EDGE('',*,*,#47069,.F.);
#71803=ORIENTED_EDGE('',*,*,#51620,.T.);
#71804=ORIENTED_EDGE('',*,*,#46187,.F.);
#71805=ORIENTED_EDGE('',*,*,#45889,.F.);
#71806=ORIENTED_EDGE('',*,*,#50325,.F.);
#71807=ORIENTED_EDGE('',*,*,#51621,.T.);
#71808=ORIENTED_EDGE('',*,*,#49750,.F.);
#71809=ORIENTED_EDGE('',*,*,#51622,.F.);
#71810=ORIENTED_EDGE('',*,*,#47066,.F.);
#71811=ORIENTED_EDGE('',*,*,#51622,.T.);
#71812=ORIENTED_EDGE('',*,*,#49749,.F.);
#71813=ORIENTED_EDGE('',*,*,#51623,.F.);
#71814=ORIENTED_EDGE('',*,*,#47084,.F.);
#71815=ORIENTED_EDGE('',*,*,#45887,.T.);
#71816=ORIENTED_EDGE('',*,*,#46186,.F.);
#71817=ORIENTED_EDGE('',*,*,#51624,.F.);
#71818=ORIENTED_EDGE('',*,*,#50327,.F.);
#71819=ORIENTED_EDGE('',*,*,#51623,.T.);
#71820=ORIENTED_EDGE('',*,*,#49748,.F.);
#71821=ORIENTED_EDGE('',*,*,#51625,.F.);
#71822=ORIENTED_EDGE('',*,*,#46545,.F.);
#71823=ORIENTED_EDGE('',*,*,#51624,.T.);
#71824=ORIENTED_EDGE('',*,*,#46185,.F.);
#71825=ORIENTED_EDGE('',*,*,#51626,.F.);
#71826=ORIENTED_EDGE('',*,*,#49736,.F.);
#71827=ORIENTED_EDGE('',*,*,#51625,.T.);
#71828=ORIENTED_EDGE('',*,*,#50326,.F.);
#71829=ORIENTED_EDGE('',*,*,#45885,.F.);
#71830=ORIENTED_EDGE('',*,*,#46546,.F.);
#71831=ORIENTED_EDGE('',*,*,#51626,.T.);
#71832=ORIENTED_EDGE('',*,*,#47115,.F.);
#71833=ORIENTED_EDGE('',*,*,#51627,.F.);
#71834=ORIENTED_EDGE('',*,*,#49737,.F.);
#71835=ORIENTED_EDGE('',*,*,#47110,.F.);
#71836=ORIENTED_EDGE('',*,*,#47106,.T.);
#71837=ORIENTED_EDGE('',*,*,#51628,.F.);
#71838=ORIENTED_EDGE('',*,*,#49738,.F.);
#71839=ORIENTED_EDGE('',*,*,#51627,.T.);
#71840=ORIENTED_EDGE('',*,*,#45883,.T.);
#71841=ORIENTED_EDGE('',*,*,#50328,.F.);
#71842=ORIENTED_EDGE('',*,*,#51629,.F.);
#71843=ORIENTED_EDGE('',*,*,#46547,.F.);
#71844=ORIENTED_EDGE('',*,*,#51628,.T.);
#71845=ORIENTED_EDGE('',*,*,#47105,.F.);
#71846=ORIENTED_EDGE('',*,*,#51630,.F.);
#71847=ORIENTED_EDGE('',*,*,#49739,.F.);
#71848=ORIENTED_EDGE('',*,*,#51629,.T.);
#71849=ORIENTED_EDGE('',*,*,#49734,.F.);
#71850=ORIENTED_EDGE('',*,*,#51631,.F.);
#71851=ORIENTED_EDGE('',*,*,#46548,.F.);
#71852=ORIENTED_EDGE('',*,*,#51630,.T.);
#71853=ORIENTED_EDGE('',*,*,#47117,.F.);
#71854=ORIENTED_EDGE('',*,*,#51632,.F.);
#71855=ORIENTED_EDGE('',*,*,#49740,.F.);
#71856=ORIENTED_EDGE('',*,*,#51631,.T.);
#71857=ORIENTED_EDGE('',*,*,#49733,.F.);
#71858=ORIENTED_EDGE('',*,*,#51633,.F.);
#71859=ORIENTED_EDGE('',*,*,#47113,.F.);
#71860=ORIENTED_EDGE('',*,*,#51632,.T.);
#71861=ORIENTED_EDGE('',*,*,#47101,.F.);
#71862=ORIENTED_EDGE('',*,*,#51634,.F.);
#71863=ORIENTED_EDGE('',*,*,#49741,.F.);
#71864=ORIENTED_EDGE('',*,*,#51633,.T.);
#71865=ORIENTED_EDGE('',*,*,#49744,.F.);
#71866=ORIENTED_EDGE('',*,*,#51635,.F.);
#71867=ORIENTED_EDGE('',*,*,#47092,.F.);
#71868=ORIENTED_EDGE('',*,*,#51634,.T.);
#71869=ORIENTED_EDGE('',*,*,#47119,.F.);
#71870=ORIENTED_EDGE('',*,*,#51636,.F.);
#71871=ORIENTED_EDGE('',*,*,#49742,.F.);
#71872=ORIENTED_EDGE('',*,*,#51635,.T.);
#71873=ORIENTED_EDGE('',*,*,#49743,.F.);
#71874=ORIENTED_EDGE('',*,*,#51636,.T.);
#71875=ORIENTED_EDGE('',*,*,#47097,.F.);
#71876=ORIENTED_EDGE('',*,*,#47093,.T.);
#71877=ORIENTED_EDGE('',*,*,#51637,.F.);
#71878=ORIENTED_EDGE('',*,*,#49783,.F.);
#71879=ORIENTED_EDGE('',*,*,#51638,.F.);
#71880=ORIENTED_EDGE('',*,*,#47049,.F.);
#71881=ORIENTED_EDGE('',*,*,#51638,.T.);
#71882=ORIENTED_EDGE('',*,*,#49782,.F.);
#71883=ORIENTED_EDGE('',*,*,#51639,.F.);
#71884=ORIENTED_EDGE('',*,*,#47058,.F.);
#71885=ORIENTED_EDGE('',*,*,#47048,.T.);
#71886=ORIENTED_EDGE('',*,*,#47052,.F.);
#71887=ORIENTED_EDGE('',*,*,#51640,.F.);
#71888=ORIENTED_EDGE('',*,*,#49784,.F.);
#71889=ORIENTED_EDGE('',*,*,#51637,.T.);
#71890=ORIENTED_EDGE('',*,*,#51639,.T.);
#71891=ORIENTED_EDGE('',*,*,#49781,.F.);
#71892=ORIENTED_EDGE('',*,*,#51641,.F.);
#71893=ORIENTED_EDGE('',*,*,#47043,.F.);
#71894=ORIENTED_EDGE('',*,*,#51640,.T.);
#71895=ORIENTED_EDGE('',*,*,#47056,.F.);
#71896=ORIENTED_EDGE('',*,*,#51642,.F.);
#71897=ORIENTED_EDGE('',*,*,#49773,.F.);
#71898=ORIENTED_EDGE('',*,*,#51641,.T.);
#71899=ORIENTED_EDGE('',*,*,#49780,.F.);
#71900=ORIENTED_EDGE('',*,*,#51643,.F.);
#71901=ORIENTED_EDGE('',*,*,#47060,.F.);
#71902=ORIENTED_EDGE('',*,*,#51642,.T.);
#71903=ORIENTED_EDGE('',*,*,#46194,.F.);
#71904=ORIENTED_EDGE('',*,*,#51644,.F.);
#71905=ORIENTED_EDGE('',*,*,#49774,.F.);
#71906=ORIENTED_EDGE('',*,*,#51643,.T.);
#71907=ORIENTED_EDGE('',*,*,#49779,.F.);
#71908=ORIENTED_EDGE('',*,*,#51645,.F.);
#71909=ORIENTED_EDGE('',*,*,#47035,.T.);
#71910=ORIENTED_EDGE('',*,*,#47039,.F.);
#71911=ORIENTED_EDGE('',*,*,#51644,.T.);
#71912=ORIENTED_EDGE('',*,*,#46193,.F.);
#71913=ORIENTED_EDGE('',*,*,#51646,.F.);
#71914=ORIENTED_EDGE('',*,*,#50329,.F.);
#71915=ORIENTED_EDGE('',*,*,#51645,.T.);
#71916=ORIENTED_EDGE('',*,*,#49778,.F.);
#71917=ORIENTED_EDGE('',*,*,#51647,.F.);
#71918=ORIENTED_EDGE('',*,*,#47036,.F.);
#71919=ORIENTED_EDGE('',*,*,#51646,.T.);
#71920=ORIENTED_EDGE('',*,*,#46192,.F.);
#71921=ORIENTED_EDGE('',*,*,#51648,.F.);
#71922=ORIENTED_EDGE('',*,*,#49758,.F.);
#71923=ORIENTED_EDGE('',*,*,#51647,.T.);
#71924=ORIENTED_EDGE('',*,*,#49777,.F.);
#71925=ORIENTED_EDGE('',*,*,#51649,.F.);
#71926=ORIENTED_EDGE('',*,*,#47054,.F.);
#71927=ORIENTED_EDGE('',*,*,#51648,.T.);
#71928=ORIENTED_EDGE('',*,*,#46191,.F.);
#71929=ORIENTED_EDGE('',*,*,#51650,.F.);
#71930=ORIENTED_EDGE('',*,*,#50331,.F.);
#71931=ORIENTED_EDGE('',*,*,#51649,.T.);
#71932=ORIENTED_EDGE('',*,*,#49776,.F.);
#71933=ORIENTED_EDGE('',*,*,#51651,.F.);
#71934=ORIENTED_EDGE('',*,*,#46539,.F.);
#71935=ORIENTED_EDGE('',*,*,#51650,.T.);
#71936=ORIENTED_EDGE('',*,*,#46190,.F.);
#71937=ORIENTED_EDGE('',*,*,#51652,.F.);
#71938=ORIENTED_EDGE('',*,*,#49764,.F.);
#71939=ORIENTED_EDGE('',*,*,#51651,.T.);
#71940=ORIENTED_EDGE('',*,*,#50330,.F.);
#71941=ORIENTED_EDGE('',*,*,#51653,.F.);
#71942=ORIENTED_EDGE('',*,*,#46540,.F.);
#71943=ORIENTED_EDGE('',*,*,#51652,.T.);
#71944=ORIENTED_EDGE('',*,*,#47085,.F.);
#71945=ORIENTED_EDGE('',*,*,#51654,.F.);
#71946=ORIENTED_EDGE('',*,*,#49765,.F.);
#71947=ORIENTED_EDGE('',*,*,#51653,.T.);
#71948=ORIENTED_EDGE('',*,*,#49760,.F.);
#71949=ORIENTED_EDGE('',*,*,#51655,.F.);
#71950=ORIENTED_EDGE('',*,*,#46541,.F.);
#71951=ORIENTED_EDGE('',*,*,#47080,.F.);
#71952=ORIENTED_EDGE('',*,*,#47076,.T.);
#71953=ORIENTED_EDGE('',*,*,#51656,.F.);
#71954=ORIENTED_EDGE('',*,*,#49766,.F.);
#71955=ORIENTED_EDGE('',*,*,#51654,.T.);
#71956=ORIENTED_EDGE('',*,*,#51655,.T.);
#71957=ORIENTED_EDGE('',*,*,#50332,.F.);
#71958=ORIENTED_EDGE('',*,*,#51657,.F.);
#71959=ORIENTED_EDGE('',*,*,#46542,.F.);
#71960=ORIENTED_EDGE('',*,*,#51656,.T.);
#71961=ORIENTED_EDGE('',*,*,#47075,.F.);
#71962=ORIENTED_EDGE('',*,*,#51658,.F.);
#71963=ORIENTED_EDGE('',*,*,#49767,.F.);
#71964=ORIENTED_EDGE('',*,*,#51657,.T.);
#71965=ORIENTED_EDGE('',*,*,#49762,.F.);
#71966=ORIENTED_EDGE('',*,*,#51659,.F.);
#71967=ORIENTED_EDGE('',*,*,#46543,.F.);
#71968=ORIENTED_EDGE('',*,*,#51658,.T.);
#71969=ORIENTED_EDGE('',*,*,#47087,.F.);
#71970=ORIENTED_EDGE('',*,*,#51660,.F.);
#71971=ORIENTED_EDGE('',*,*,#49768,.F.);
#71972=ORIENTED_EDGE('',*,*,#51659,.T.);
#71973=ORIENTED_EDGE('',*,*,#49761,.F.);
#71974=ORIENTED_EDGE('',*,*,#51661,.F.);
#71975=ORIENTED_EDGE('',*,*,#47083,.F.);
#71976=ORIENTED_EDGE('',*,*,#51660,.T.);
#71977=ORIENTED_EDGE('',*,*,#47071,.F.);
#71978=ORIENTED_EDGE('',*,*,#51662,.F.);
#71979=ORIENTED_EDGE('',*,*,#49769,.F.);
#71980=ORIENTED_EDGE('',*,*,#51661,.T.);
#71981=ORIENTED_EDGE('',*,*,#49772,.F.);
#71982=ORIENTED_EDGE('',*,*,#51663,.F.);
#71983=ORIENTED_EDGE('',*,*,#47062,.F.);
#71984=ORIENTED_EDGE('',*,*,#51662,.T.);
#71985=ORIENTED_EDGE('',*,*,#47089,.F.);
#71986=ORIENTED_EDGE('',*,*,#51664,.F.);
#71987=ORIENTED_EDGE('',*,*,#49770,.F.);
#71988=ORIENTED_EDGE('',*,*,#51663,.T.);
#71989=ORIENTED_EDGE('',*,*,#49771,.F.);
#71990=ORIENTED_EDGE('',*,*,#51664,.T.);
#71991=ORIENTED_EDGE('',*,*,#47067,.F.);
#71992=ORIENTED_EDGE('',*,*,#47063,.T.);
#71993=ORIENTED_EDGE('',*,*,#51665,.F.);
#71994=ORIENTED_EDGE('',*,*,#49811,.F.);
#71995=ORIENTED_EDGE('',*,*,#51666,.F.);
#71996=ORIENTED_EDGE('',*,*,#47019,.F.);
#71997=ORIENTED_EDGE('',*,*,#51666,.T.);
#71998=ORIENTED_EDGE('',*,*,#49810,.F.);
#71999=ORIENTED_EDGE('',*,*,#51667,.F.);
#72000=ORIENTED_EDGE('',*,*,#47028,.F.);
#72001=ORIENTED_EDGE('',*,*,#47018,.T.);
#72002=ORIENTED_EDGE('',*,*,#47022,.F.);
#72003=ORIENTED_EDGE('',*,*,#51668,.F.);
#72004=ORIENTED_EDGE('',*,*,#49812,.F.);
#72005=ORIENTED_EDGE('',*,*,#51665,.T.);
#72006=ORIENTED_EDGE('',*,*,#51667,.T.);
#72007=ORIENTED_EDGE('',*,*,#49809,.F.);
#72008=ORIENTED_EDGE('',*,*,#51669,.F.);
#72009=ORIENTED_EDGE('',*,*,#47013,.F.);
#72010=ORIENTED_EDGE('',*,*,#51668,.T.);
#72011=ORIENTED_EDGE('',*,*,#47026,.F.);
#72012=ORIENTED_EDGE('',*,*,#51670,.F.);
#72013=ORIENTED_EDGE('',*,*,#49801,.F.);
#72014=ORIENTED_EDGE('',*,*,#51669,.T.);
#72015=ORIENTED_EDGE('',*,*,#49808,.F.);
#72016=ORIENTED_EDGE('',*,*,#51671,.F.);
#72017=ORIENTED_EDGE('',*,*,#47030,.F.);
#72018=ORIENTED_EDGE('',*,*,#51670,.T.);
#72019=ORIENTED_EDGE('',*,*,#46200,.F.);
#72020=ORIENTED_EDGE('',*,*,#51672,.F.);
#72021=ORIENTED_EDGE('',*,*,#49802,.F.);
#72022=ORIENTED_EDGE('',*,*,#51671,.T.);
#72023=ORIENTED_EDGE('',*,*,#49807,.F.);
#72024=ORIENTED_EDGE('',*,*,#51673,.F.);
#72025=ORIENTED_EDGE('',*,*,#47005,.T.);
#72026=ORIENTED_EDGE('',*,*,#47009,.F.);
#72027=ORIENTED_EDGE('',*,*,#51672,.T.);
#72028=ORIENTED_EDGE('',*,*,#46199,.F.);
#72029=ORIENTED_EDGE('',*,*,#51674,.F.);
#72030=ORIENTED_EDGE('',*,*,#50333,.F.);
#72031=ORIENTED_EDGE('',*,*,#51673,.T.);
#72032=ORIENTED_EDGE('',*,*,#49806,.F.);
#72033=ORIENTED_EDGE('',*,*,#51675,.F.);
#72034=ORIENTED_EDGE('',*,*,#47006,.F.);
#72035=ORIENTED_EDGE('',*,*,#51674,.T.);
#72036=ORIENTED_EDGE('',*,*,#46198,.F.);
#72037=ORIENTED_EDGE('',*,*,#51676,.F.);
#72038=ORIENTED_EDGE('',*,*,#49786,.F.);
#72039=ORIENTED_EDGE('',*,*,#51675,.T.);
#72040=ORIENTED_EDGE('',*,*,#49805,.F.);
#72041=ORIENTED_EDGE('',*,*,#51677,.F.);
#72042=ORIENTED_EDGE('',*,*,#47024,.F.);
#72043=ORIENTED_EDGE('',*,*,#51676,.T.);
#72044=ORIENTED_EDGE('',*,*,#46197,.F.);
#72045=ORIENTED_EDGE('',*,*,#51678,.F.);
#72046=ORIENTED_EDGE('',*,*,#50335,.F.);
#72047=ORIENTED_EDGE('',*,*,#51677,.T.);
#72048=ORIENTED_EDGE('',*,*,#49804,.F.);
#72049=ORIENTED_EDGE('',*,*,#51679,.F.);
#72050=ORIENTED_EDGE('',*,*,#46533,.F.);
#72051=ORIENTED_EDGE('',*,*,#51678,.T.);
#72052=ORIENTED_EDGE('',*,*,#46196,.F.);
#72053=ORIENTED_EDGE('',*,*,#51680,.F.);
#72054=ORIENTED_EDGE('',*,*,#49792,.F.);
#72055=ORIENTED_EDGE('',*,*,#51679,.T.);
#72056=ORIENTED_EDGE('',*,*,#50334,.F.);
#72057=ORIENTED_EDGE('',*,*,#51681,.F.);
#72058=ORIENTED_EDGE('',*,*,#46534,.F.);
#72059=ORIENTED_EDGE('',*,*,#51680,.T.);
#72060=ORIENTED_EDGE('',*,*,#47055,.F.);
#72061=ORIENTED_EDGE('',*,*,#51682,.F.);
#72062=ORIENTED_EDGE('',*,*,#49793,.F.);
#72063=ORIENTED_EDGE('',*,*,#51681,.T.);
#72064=ORIENTED_EDGE('',*,*,#49788,.F.);
#72065=ORIENTED_EDGE('',*,*,#51683,.F.);
#72066=ORIENTED_EDGE('',*,*,#46535,.F.);
#72067=ORIENTED_EDGE('',*,*,#47050,.F.);
#72068=ORIENTED_EDGE('',*,*,#47046,.T.);
#72069=ORIENTED_EDGE('',*,*,#51684,.F.);
#72070=ORIENTED_EDGE('',*,*,#49794,.F.);
#72071=ORIENTED_EDGE('',*,*,#51682,.T.);
#72072=ORIENTED_EDGE('',*,*,#51683,.T.);
#72073=ORIENTED_EDGE('',*,*,#50336,.F.);
#72074=ORIENTED_EDGE('',*,*,#51685,.F.);
#72075=ORIENTED_EDGE('',*,*,#46536,.F.);
#72076=ORIENTED_EDGE('',*,*,#51684,.T.);
#72077=ORIENTED_EDGE('',*,*,#47045,.F.);
#72078=ORIENTED_EDGE('',*,*,#51686,.F.);
#72079=ORIENTED_EDGE('',*,*,#49795,.F.);
#72080=ORIENTED_EDGE('',*,*,#51685,.T.);
#72081=ORIENTED_EDGE('',*,*,#49790,.F.);
#72082=ORIENTED_EDGE('',*,*,#51687,.F.);
#72083=ORIENTED_EDGE('',*,*,#46537,.F.);
#72084=ORIENTED_EDGE('',*,*,#51686,.T.);
#72085=ORIENTED_EDGE('',*,*,#47057,.F.);
#72086=ORIENTED_EDGE('',*,*,#51688,.F.);
#72087=ORIENTED_EDGE('',*,*,#49796,.F.);
#72088=ORIENTED_EDGE('',*,*,#51687,.T.);
#72089=ORIENTED_EDGE('',*,*,#49789,.F.);
#72090=ORIENTED_EDGE('',*,*,#51689,.F.);
#72091=ORIENTED_EDGE('',*,*,#47053,.F.);
#72092=ORIENTED_EDGE('',*,*,#51688,.T.);
#72093=ORIENTED_EDGE('',*,*,#47041,.F.);
#72094=ORIENTED_EDGE('',*,*,#51690,.F.);
#72095=ORIENTED_EDGE('',*,*,#49797,.F.);
#72096=ORIENTED_EDGE('',*,*,#51689,.T.);
#72097=ORIENTED_EDGE('',*,*,#49800,.F.);
#72098=ORIENTED_EDGE('',*,*,#51691,.F.);
#72099=ORIENTED_EDGE('',*,*,#47032,.F.);
#72100=ORIENTED_EDGE('',*,*,#51690,.T.);
#72101=ORIENTED_EDGE('',*,*,#47059,.F.);
#72102=ORIENTED_EDGE('',*,*,#51692,.F.);
#72103=ORIENTED_EDGE('',*,*,#49798,.F.);
#72104=ORIENTED_EDGE('',*,*,#51691,.T.);
#72105=ORIENTED_EDGE('',*,*,#49799,.F.);
#72106=ORIENTED_EDGE('',*,*,#51692,.T.);
#72107=ORIENTED_EDGE('',*,*,#47037,.F.);
#72108=ORIENTED_EDGE('',*,*,#47033,.T.);
#72109=ORIENTED_EDGE('',*,*,#51693,.F.);
#72110=ORIENTED_EDGE('',*,*,#49839,.F.);
#72111=ORIENTED_EDGE('',*,*,#51694,.F.);
#72112=ORIENTED_EDGE('',*,*,#46989,.F.);
#72113=ORIENTED_EDGE('',*,*,#51694,.T.);
#72114=ORIENTED_EDGE('',*,*,#49838,.F.);
#72115=ORIENTED_EDGE('',*,*,#51695,.F.);
#72116=ORIENTED_EDGE('',*,*,#46998,.F.);
#72117=ORIENTED_EDGE('',*,*,#46988,.T.);
#72118=ORIENTED_EDGE('',*,*,#46992,.F.);
#72119=ORIENTED_EDGE('',*,*,#51696,.F.);
#72120=ORIENTED_EDGE('',*,*,#49840,.F.);
#72121=ORIENTED_EDGE('',*,*,#51693,.T.);
#72122=ORIENTED_EDGE('',*,*,#51695,.T.);
#72123=ORIENTED_EDGE('',*,*,#49837,.F.);
#72124=ORIENTED_EDGE('',*,*,#51697,.F.);
#72125=ORIENTED_EDGE('',*,*,#46983,.F.);
#72126=ORIENTED_EDGE('',*,*,#51696,.T.);
#72127=ORIENTED_EDGE('',*,*,#46996,.F.);
#72128=ORIENTED_EDGE('',*,*,#51698,.F.);
#72129=ORIENTED_EDGE('',*,*,#49829,.F.);
#72130=ORIENTED_EDGE('',*,*,#51697,.T.);
#72131=ORIENTED_EDGE('',*,*,#49836,.F.);
#72132=ORIENTED_EDGE('',*,*,#51699,.F.);
#72133=ORIENTED_EDGE('',*,*,#47000,.F.);
#72134=ORIENTED_EDGE('',*,*,#51698,.T.);
#72135=ORIENTED_EDGE('',*,*,#46206,.F.);
#72136=ORIENTED_EDGE('',*,*,#51700,.F.);
#72137=ORIENTED_EDGE('',*,*,#49830,.F.);
#72138=ORIENTED_EDGE('',*,*,#51699,.T.);
#72139=ORIENTED_EDGE('',*,*,#49835,.F.);
#72140=ORIENTED_EDGE('',*,*,#51701,.F.);
#72141=ORIENTED_EDGE('',*,*,#46975,.T.);
#72142=ORIENTED_EDGE('',*,*,#46979,.F.);
#72143=ORIENTED_EDGE('',*,*,#51700,.T.);
#72144=ORIENTED_EDGE('',*,*,#46205,.F.);
#72145=ORIENTED_EDGE('',*,*,#51702,.F.);
#72146=ORIENTED_EDGE('',*,*,#50337,.F.);
#72147=ORIENTED_EDGE('',*,*,#51701,.T.);
#72148=ORIENTED_EDGE('',*,*,#49834,.F.);
#72149=ORIENTED_EDGE('',*,*,#51703,.F.);
#72150=ORIENTED_EDGE('',*,*,#46976,.F.);
#72151=ORIENTED_EDGE('',*,*,#51702,.T.);
#72152=ORIENTED_EDGE('',*,*,#46204,.F.);
#72153=ORIENTED_EDGE('',*,*,#51704,.F.);
#72154=ORIENTED_EDGE('',*,*,#49814,.F.);
#72155=ORIENTED_EDGE('',*,*,#51703,.T.);
#72156=ORIENTED_EDGE('',*,*,#49833,.F.);
#72157=ORIENTED_EDGE('',*,*,#51705,.F.);
#72158=ORIENTED_EDGE('',*,*,#46994,.F.);
#72159=ORIENTED_EDGE('',*,*,#51704,.T.);
#72160=ORIENTED_EDGE('',*,*,#46203,.F.);
#72161=ORIENTED_EDGE('',*,*,#51706,.F.);
#72162=ORIENTED_EDGE('',*,*,#50339,.F.);
#72163=ORIENTED_EDGE('',*,*,#51705,.T.);
#72164=ORIENTED_EDGE('',*,*,#49832,.F.);
#72165=ORIENTED_EDGE('',*,*,#51707,.F.);
#72166=ORIENTED_EDGE('',*,*,#46527,.F.);
#72167=ORIENTED_EDGE('',*,*,#51706,.T.);
#72168=ORIENTED_EDGE('',*,*,#46202,.F.);
#72169=ORIENTED_EDGE('',*,*,#51708,.F.);
#72170=ORIENTED_EDGE('',*,*,#49820,.F.);
#72171=ORIENTED_EDGE('',*,*,#51707,.T.);
#72172=ORIENTED_EDGE('',*,*,#50338,.F.);
#72173=ORIENTED_EDGE('',*,*,#51709,.F.);
#72174=ORIENTED_EDGE('',*,*,#46528,.F.);
#72175=ORIENTED_EDGE('',*,*,#51708,.T.);
#72176=ORIENTED_EDGE('',*,*,#47025,.F.);
#72177=ORIENTED_EDGE('',*,*,#51710,.F.);
#72178=ORIENTED_EDGE('',*,*,#49821,.F.);
#72179=ORIENTED_EDGE('',*,*,#51709,.T.);
#72180=ORIENTED_EDGE('',*,*,#49816,.F.);
#72181=ORIENTED_EDGE('',*,*,#51711,.F.);
#72182=ORIENTED_EDGE('',*,*,#46529,.F.);
#72183=ORIENTED_EDGE('',*,*,#47020,.F.);
#72184=ORIENTED_EDGE('',*,*,#47016,.T.);
#72185=ORIENTED_EDGE('',*,*,#51712,.F.);
#72186=ORIENTED_EDGE('',*,*,#49822,.F.);
#72187=ORIENTED_EDGE('',*,*,#51710,.T.);
#72188=ORIENTED_EDGE('',*,*,#51711,.T.);
#72189=ORIENTED_EDGE('',*,*,#50340,.F.);
#72190=ORIENTED_EDGE('',*,*,#51713,.F.);
#72191=ORIENTED_EDGE('',*,*,#46530,.F.);
#72192=ORIENTED_EDGE('',*,*,#51712,.T.);
#72193=ORIENTED_EDGE('',*,*,#47015,.F.);
#72194=ORIENTED_EDGE('',*,*,#51714,.F.);
#72195=ORIENTED_EDGE('',*,*,#49823,.F.);
#72196=ORIENTED_EDGE('',*,*,#51713,.T.);
#72197=ORIENTED_EDGE('',*,*,#49818,.F.);
#72198=ORIENTED_EDGE('',*,*,#51715,.F.);
#72199=ORIENTED_EDGE('',*,*,#46531,.F.);
#72200=ORIENTED_EDGE('',*,*,#51714,.T.);
#72201=ORIENTED_EDGE('',*,*,#47027,.F.);
#72202=ORIENTED_EDGE('',*,*,#51716,.F.);
#72203=ORIENTED_EDGE('',*,*,#49824,.F.);
#72204=ORIENTED_EDGE('',*,*,#51715,.T.);
#72205=ORIENTED_EDGE('',*,*,#49817,.F.);
#72206=ORIENTED_EDGE('',*,*,#51717,.F.);
#72207=ORIENTED_EDGE('',*,*,#47023,.F.);
#72208=ORIENTED_EDGE('',*,*,#51716,.T.);
#72209=ORIENTED_EDGE('',*,*,#47011,.F.);
#72210=ORIENTED_EDGE('',*,*,#51718,.F.);
#72211=ORIENTED_EDGE('',*,*,#49825,.F.);
#72212=ORIENTED_EDGE('',*,*,#51717,.T.);
#72213=ORIENTED_EDGE('',*,*,#49828,.F.);
#72214=ORIENTED_EDGE('',*,*,#51719,.F.);
#72215=ORIENTED_EDGE('',*,*,#47002,.F.);
#72216=ORIENTED_EDGE('',*,*,#51718,.T.);
#72217=ORIENTED_EDGE('',*,*,#47029,.F.);
#72218=ORIENTED_EDGE('',*,*,#51720,.F.);
#72219=ORIENTED_EDGE('',*,*,#49826,.F.);
#72220=ORIENTED_EDGE('',*,*,#51719,.T.);
#72221=ORIENTED_EDGE('',*,*,#49827,.F.);
#72222=ORIENTED_EDGE('',*,*,#51720,.T.);
#72223=ORIENTED_EDGE('',*,*,#47007,.F.);
#72224=ORIENTED_EDGE('',*,*,#47003,.T.);
#72225=ORIENTED_EDGE('',*,*,#51721,.F.);
#72226=ORIENTED_EDGE('',*,*,#49867,.F.);
#72227=ORIENTED_EDGE('',*,*,#51722,.F.);
#72228=ORIENTED_EDGE('',*,*,#46959,.F.);
#72229=ORIENTED_EDGE('',*,*,#51722,.T.);
#72230=ORIENTED_EDGE('',*,*,#49866,.F.);
#72231=ORIENTED_EDGE('',*,*,#51723,.F.);
#72232=ORIENTED_EDGE('',*,*,#46968,.F.);
#72233=ORIENTED_EDGE('',*,*,#46958,.T.);
#72234=ORIENTED_EDGE('',*,*,#46962,.F.);
#72235=ORIENTED_EDGE('',*,*,#51724,.F.);
#72236=ORIENTED_EDGE('',*,*,#49868,.F.);
#72237=ORIENTED_EDGE('',*,*,#51721,.T.);
#72238=ORIENTED_EDGE('',*,*,#51723,.T.);
#72239=ORIENTED_EDGE('',*,*,#49865,.F.);
#72240=ORIENTED_EDGE('',*,*,#51725,.F.);
#72241=ORIENTED_EDGE('',*,*,#46953,.F.);
#72242=ORIENTED_EDGE('',*,*,#51724,.T.);
#72243=ORIENTED_EDGE('',*,*,#46966,.F.);
#72244=ORIENTED_EDGE('',*,*,#51726,.F.);
#72245=ORIENTED_EDGE('',*,*,#49857,.F.);
#72246=ORIENTED_EDGE('',*,*,#51725,.T.);
#72247=ORIENTED_EDGE('',*,*,#49864,.F.);
#72248=ORIENTED_EDGE('',*,*,#51727,.F.);
#72249=ORIENTED_EDGE('',*,*,#46970,.F.);
#72250=ORIENTED_EDGE('',*,*,#51726,.T.);
#72251=ORIENTED_EDGE('',*,*,#46212,.F.);
#72252=ORIENTED_EDGE('',*,*,#51728,.F.);
#72253=ORIENTED_EDGE('',*,*,#49858,.F.);
#72254=ORIENTED_EDGE('',*,*,#51727,.T.);
#72255=ORIENTED_EDGE('',*,*,#49863,.F.);
#72256=ORIENTED_EDGE('',*,*,#51729,.F.);
#72257=ORIENTED_EDGE('',*,*,#46945,.T.);
#72258=ORIENTED_EDGE('',*,*,#46949,.F.);
#72259=ORIENTED_EDGE('',*,*,#51728,.T.);
#72260=ORIENTED_EDGE('',*,*,#46211,.F.);
#72261=ORIENTED_EDGE('',*,*,#51730,.F.);
#72262=ORIENTED_EDGE('',*,*,#50341,.F.);
#72263=ORIENTED_EDGE('',*,*,#51729,.T.);
#72264=ORIENTED_EDGE('',*,*,#49862,.F.);
#72265=ORIENTED_EDGE('',*,*,#51731,.F.);
#72266=ORIENTED_EDGE('',*,*,#46946,.F.);
#72267=ORIENTED_EDGE('',*,*,#51730,.T.);
#72268=ORIENTED_EDGE('',*,*,#46210,.F.);
#72269=ORIENTED_EDGE('',*,*,#51732,.F.);
#72270=ORIENTED_EDGE('',*,*,#49842,.F.);
#72271=ORIENTED_EDGE('',*,*,#51731,.T.);
#72272=ORIENTED_EDGE('',*,*,#49861,.F.);
#72273=ORIENTED_EDGE('',*,*,#51733,.F.);
#72274=ORIENTED_EDGE('',*,*,#46964,.F.);
#72275=ORIENTED_EDGE('',*,*,#51732,.T.);
#72276=ORIENTED_EDGE('',*,*,#46209,.F.);
#72277=ORIENTED_EDGE('',*,*,#51734,.F.);
#72278=ORIENTED_EDGE('',*,*,#50343,.F.);
#72279=ORIENTED_EDGE('',*,*,#51733,.T.);
#72280=ORIENTED_EDGE('',*,*,#49860,.F.);
#72281=ORIENTED_EDGE('',*,*,#51735,.F.);
#72282=ORIENTED_EDGE('',*,*,#46521,.F.);
#72283=ORIENTED_EDGE('',*,*,#51734,.T.);
#72284=ORIENTED_EDGE('',*,*,#46208,.F.);
#72285=ORIENTED_EDGE('',*,*,#51736,.F.);
#72286=ORIENTED_EDGE('',*,*,#49848,.F.);
#72287=ORIENTED_EDGE('',*,*,#51735,.T.);
#72288=ORIENTED_EDGE('',*,*,#50342,.F.);
#72289=ORIENTED_EDGE('',*,*,#51737,.F.);
#72290=ORIENTED_EDGE('',*,*,#46522,.F.);
#72291=ORIENTED_EDGE('',*,*,#51736,.T.);
#72292=ORIENTED_EDGE('',*,*,#46995,.F.);
#72293=ORIENTED_EDGE('',*,*,#51738,.F.);
#72294=ORIENTED_EDGE('',*,*,#49849,.F.);
#72295=ORIENTED_EDGE('',*,*,#51737,.T.);
#72296=ORIENTED_EDGE('',*,*,#49844,.F.);
#72297=ORIENTED_EDGE('',*,*,#51739,.F.);
#72298=ORIENTED_EDGE('',*,*,#46523,.F.);
#72299=ORIENTED_EDGE('',*,*,#46990,.F.);
#72300=ORIENTED_EDGE('',*,*,#46986,.T.);
#72301=ORIENTED_EDGE('',*,*,#51740,.F.);
#72302=ORIENTED_EDGE('',*,*,#49850,.F.);
#72303=ORIENTED_EDGE('',*,*,#51738,.T.);
#72304=ORIENTED_EDGE('',*,*,#51739,.T.);
#72305=ORIENTED_EDGE('',*,*,#50344,.F.);
#72306=ORIENTED_EDGE('',*,*,#51741,.F.);
#72307=ORIENTED_EDGE('',*,*,#46524,.F.);
#72308=ORIENTED_EDGE('',*,*,#51740,.T.);
#72309=ORIENTED_EDGE('',*,*,#46985,.F.);
#72310=ORIENTED_EDGE('',*,*,#51742,.F.);
#72311=ORIENTED_EDGE('',*,*,#49851,.F.);
#72312=ORIENTED_EDGE('',*,*,#51741,.T.);
#72313=ORIENTED_EDGE('',*,*,#49846,.F.);
#72314=ORIENTED_EDGE('',*,*,#51743,.F.);
#72315=ORIENTED_EDGE('',*,*,#46525,.F.);
#72316=ORIENTED_EDGE('',*,*,#51742,.T.);
#72317=ORIENTED_EDGE('',*,*,#46997,.F.);
#72318=ORIENTED_EDGE('',*,*,#51744,.F.);
#72319=ORIENTED_EDGE('',*,*,#49852,.F.);
#72320=ORIENTED_EDGE('',*,*,#51743,.T.);
#72321=ORIENTED_EDGE('',*,*,#49845,.F.);
#72322=ORIENTED_EDGE('',*,*,#51745,.F.);
#72323=ORIENTED_EDGE('',*,*,#46993,.F.);
#72324=ORIENTED_EDGE('',*,*,#51744,.T.);
#72325=ORIENTED_EDGE('',*,*,#46981,.F.);
#72326=ORIENTED_EDGE('',*,*,#51746,.F.);
#72327=ORIENTED_EDGE('',*,*,#49853,.F.);
#72328=ORIENTED_EDGE('',*,*,#51745,.T.);
#72329=ORIENTED_EDGE('',*,*,#49856,.F.);
#72330=ORIENTED_EDGE('',*,*,#51747,.F.);
#72331=ORIENTED_EDGE('',*,*,#46972,.F.);
#72332=ORIENTED_EDGE('',*,*,#51746,.T.);
#72333=ORIENTED_EDGE('',*,*,#46999,.F.);
#72334=ORIENTED_EDGE('',*,*,#51748,.F.);
#72335=ORIENTED_EDGE('',*,*,#49854,.F.);
#72336=ORIENTED_EDGE('',*,*,#51747,.T.);
#72337=ORIENTED_EDGE('',*,*,#49855,.F.);
#72338=ORIENTED_EDGE('',*,*,#51748,.T.);
#72339=ORIENTED_EDGE('',*,*,#46977,.F.);
#72340=ORIENTED_EDGE('',*,*,#46973,.T.);
#72341=ORIENTED_EDGE('',*,*,#51749,.F.);
#72342=ORIENTED_EDGE('',*,*,#49895,.F.);
#72343=ORIENTED_EDGE('',*,*,#51750,.F.);
#72344=ORIENTED_EDGE('',*,*,#46929,.F.);
#72345=ORIENTED_EDGE('',*,*,#51750,.T.);
#72346=ORIENTED_EDGE('',*,*,#49894,.F.);
#72347=ORIENTED_EDGE('',*,*,#51751,.F.);
#72348=ORIENTED_EDGE('',*,*,#46938,.F.);
#72349=ORIENTED_EDGE('',*,*,#46928,.T.);
#72350=ORIENTED_EDGE('',*,*,#46932,.F.);
#72351=ORIENTED_EDGE('',*,*,#51752,.F.);
#72352=ORIENTED_EDGE('',*,*,#49896,.F.);
#72353=ORIENTED_EDGE('',*,*,#51749,.T.);
#72354=ORIENTED_EDGE('',*,*,#51751,.T.);
#72355=ORIENTED_EDGE('',*,*,#49893,.F.);
#72356=ORIENTED_EDGE('',*,*,#51753,.F.);
#72357=ORIENTED_EDGE('',*,*,#46923,.F.);
#72358=ORIENTED_EDGE('',*,*,#51752,.T.);
#72359=ORIENTED_EDGE('',*,*,#46936,.F.);
#72360=ORIENTED_EDGE('',*,*,#51754,.F.);
#72361=ORIENTED_EDGE('',*,*,#49885,.F.);
#72362=ORIENTED_EDGE('',*,*,#51753,.T.);
#72363=ORIENTED_EDGE('',*,*,#49892,.F.);
#72364=ORIENTED_EDGE('',*,*,#51755,.F.);
#72365=ORIENTED_EDGE('',*,*,#46940,.F.);
#72366=ORIENTED_EDGE('',*,*,#51754,.T.);
#72367=ORIENTED_EDGE('',*,*,#46218,.F.);
#72368=ORIENTED_EDGE('',*,*,#51756,.F.);
#72369=ORIENTED_EDGE('',*,*,#49886,.F.);
#72370=ORIENTED_EDGE('',*,*,#51755,.T.);
#72371=ORIENTED_EDGE('',*,*,#49891,.F.);
#72372=ORIENTED_EDGE('',*,*,#51757,.F.);
#72373=ORIENTED_EDGE('',*,*,#46915,.T.);
#72374=ORIENTED_EDGE('',*,*,#46919,.F.);
#72375=ORIENTED_EDGE('',*,*,#51756,.T.);
#72376=ORIENTED_EDGE('',*,*,#46217,.F.);
#72377=ORIENTED_EDGE('',*,*,#51758,.F.);
#72378=ORIENTED_EDGE('',*,*,#50345,.F.);
#72379=ORIENTED_EDGE('',*,*,#51757,.T.);
#72380=ORIENTED_EDGE('',*,*,#49890,.F.);
#72381=ORIENTED_EDGE('',*,*,#51759,.F.);
#72382=ORIENTED_EDGE('',*,*,#46916,.F.);
#72383=ORIENTED_EDGE('',*,*,#51758,.T.);
#72384=ORIENTED_EDGE('',*,*,#46216,.F.);
#72385=ORIENTED_EDGE('',*,*,#51760,.F.);
#72386=ORIENTED_EDGE('',*,*,#49870,.F.);
#72387=ORIENTED_EDGE('',*,*,#51759,.T.);
#72388=ORIENTED_EDGE('',*,*,#49889,.F.);
#72389=ORIENTED_EDGE('',*,*,#51761,.F.);
#72390=ORIENTED_EDGE('',*,*,#46934,.F.);
#72391=ORIENTED_EDGE('',*,*,#51760,.T.);
#72392=ORIENTED_EDGE('',*,*,#46215,.F.);
#72393=ORIENTED_EDGE('',*,*,#51762,.F.);
#72394=ORIENTED_EDGE('',*,*,#50347,.F.);
#72395=ORIENTED_EDGE('',*,*,#51761,.T.);
#72396=ORIENTED_EDGE('',*,*,#49888,.F.);
#72397=ORIENTED_EDGE('',*,*,#51763,.F.);
#72398=ORIENTED_EDGE('',*,*,#46515,.F.);
#72399=ORIENTED_EDGE('',*,*,#51762,.T.);
#72400=ORIENTED_EDGE('',*,*,#46214,.F.);
#72401=ORIENTED_EDGE('',*,*,#51764,.F.);
#72402=ORIENTED_EDGE('',*,*,#49876,.F.);
#72403=ORIENTED_EDGE('',*,*,#51763,.T.);
#72404=ORIENTED_EDGE('',*,*,#50346,.F.);
#72405=ORIENTED_EDGE('',*,*,#51765,.F.);
#72406=ORIENTED_EDGE('',*,*,#46516,.F.);
#72407=ORIENTED_EDGE('',*,*,#51764,.T.);
#72408=ORIENTED_EDGE('',*,*,#46965,.F.);
#72409=ORIENTED_EDGE('',*,*,#51766,.F.);
#72410=ORIENTED_EDGE('',*,*,#49877,.F.);
#72411=ORIENTED_EDGE('',*,*,#51765,.T.);
#72412=ORIENTED_EDGE('',*,*,#49872,.F.);
#72413=ORIENTED_EDGE('',*,*,#51767,.F.);
#72414=ORIENTED_EDGE('',*,*,#46517,.F.);
#72415=ORIENTED_EDGE('',*,*,#46960,.F.);
#72416=ORIENTED_EDGE('',*,*,#46956,.T.);
#72417=ORIENTED_EDGE('',*,*,#51768,.F.);
#72418=ORIENTED_EDGE('',*,*,#49878,.F.);
#72419=ORIENTED_EDGE('',*,*,#51766,.T.);
#72420=ORIENTED_EDGE('',*,*,#51767,.T.);
#72421=ORIENTED_EDGE('',*,*,#50348,.F.);
#72422=ORIENTED_EDGE('',*,*,#51769,.F.);
#72423=ORIENTED_EDGE('',*,*,#46518,.F.);
#72424=ORIENTED_EDGE('',*,*,#51768,.T.);
#72425=ORIENTED_EDGE('',*,*,#46955,.F.);
#72426=ORIENTED_EDGE('',*,*,#51770,.F.);
#72427=ORIENTED_EDGE('',*,*,#49879,.F.);
#72428=ORIENTED_EDGE('',*,*,#51769,.T.);
#72429=ORIENTED_EDGE('',*,*,#49874,.F.);
#72430=ORIENTED_EDGE('',*,*,#51771,.F.);
#72431=ORIENTED_EDGE('',*,*,#46519,.F.);
#72432=ORIENTED_EDGE('',*,*,#51770,.T.);
#72433=ORIENTED_EDGE('',*,*,#46967,.F.);
#72434=ORIENTED_EDGE('',*,*,#51772,.F.);
#72435=ORIENTED_EDGE('',*,*,#49880,.F.);
#72436=ORIENTED_EDGE('',*,*,#51771,.T.);
#72437=ORIENTED_EDGE('',*,*,#49873,.F.);
#72438=ORIENTED_EDGE('',*,*,#51773,.F.);
#72439=ORIENTED_EDGE('',*,*,#46963,.F.);
#72440=ORIENTED_EDGE('',*,*,#51772,.T.);
#72441=ORIENTED_EDGE('',*,*,#46951,.F.);
#72442=ORIENTED_EDGE('',*,*,#51774,.F.);
#72443=ORIENTED_EDGE('',*,*,#49881,.F.);
#72444=ORIENTED_EDGE('',*,*,#51773,.T.);
#72445=ORIENTED_EDGE('',*,*,#49884,.F.);
#72446=ORIENTED_EDGE('',*,*,#51775,.F.);
#72447=ORIENTED_EDGE('',*,*,#46942,.F.);
#72448=ORIENTED_EDGE('',*,*,#51774,.T.);
#72449=ORIENTED_EDGE('',*,*,#46969,.F.);
#72450=ORIENTED_EDGE('',*,*,#51776,.F.);
#72451=ORIENTED_EDGE('',*,*,#49882,.F.);
#72452=ORIENTED_EDGE('',*,*,#51775,.T.);
#72453=ORIENTED_EDGE('',*,*,#49883,.F.);
#72454=ORIENTED_EDGE('',*,*,#51776,.T.);
#72455=ORIENTED_EDGE('',*,*,#46947,.F.);
#72456=ORIENTED_EDGE('',*,*,#46943,.T.);
#72457=ORIENTED_EDGE('',*,*,#51777,.F.);
#72458=ORIENTED_EDGE('',*,*,#49923,.F.);
#72459=ORIENTED_EDGE('',*,*,#51778,.F.);
#72460=ORIENTED_EDGE('',*,*,#46899,.F.);
#72461=ORIENTED_EDGE('',*,*,#51778,.T.);
#72462=ORIENTED_EDGE('',*,*,#49922,.F.);
#72463=ORIENTED_EDGE('',*,*,#51779,.F.);
#72464=ORIENTED_EDGE('',*,*,#46908,.F.);
#72465=ORIENTED_EDGE('',*,*,#46898,.T.);
#72466=ORIENTED_EDGE('',*,*,#46902,.F.);
#72467=ORIENTED_EDGE('',*,*,#51780,.F.);
#72468=ORIENTED_EDGE('',*,*,#49924,.F.);
#72469=ORIENTED_EDGE('',*,*,#51777,.T.);
#72470=ORIENTED_EDGE('',*,*,#51779,.T.);
#72471=ORIENTED_EDGE('',*,*,#49921,.F.);
#72472=ORIENTED_EDGE('',*,*,#51781,.F.);
#72473=ORIENTED_EDGE('',*,*,#46893,.F.);
#72474=ORIENTED_EDGE('',*,*,#51780,.T.);
#72475=ORIENTED_EDGE('',*,*,#46906,.F.);
#72476=ORIENTED_EDGE('',*,*,#51782,.F.);
#72477=ORIENTED_EDGE('',*,*,#49913,.F.);
#72478=ORIENTED_EDGE('',*,*,#51781,.T.);
#72479=ORIENTED_EDGE('',*,*,#49920,.F.);
#72480=ORIENTED_EDGE('',*,*,#51783,.F.);
#72481=ORIENTED_EDGE('',*,*,#46910,.F.);
#72482=ORIENTED_EDGE('',*,*,#51782,.T.);
#72483=ORIENTED_EDGE('',*,*,#46224,.F.);
#72484=ORIENTED_EDGE('',*,*,#51784,.F.);
#72485=ORIENTED_EDGE('',*,*,#49914,.F.);
#72486=ORIENTED_EDGE('',*,*,#51783,.T.);
#72487=ORIENTED_EDGE('',*,*,#49919,.F.);
#72488=ORIENTED_EDGE('',*,*,#51785,.F.);
#72489=ORIENTED_EDGE('',*,*,#46885,.T.);
#72490=ORIENTED_EDGE('',*,*,#46889,.F.);
#72491=ORIENTED_EDGE('',*,*,#51784,.T.);
#72492=ORIENTED_EDGE('',*,*,#46223,.F.);
#72493=ORIENTED_EDGE('',*,*,#51786,.F.);
#72494=ORIENTED_EDGE('',*,*,#50349,.F.);
#72495=ORIENTED_EDGE('',*,*,#51785,.T.);
#72496=ORIENTED_EDGE('',*,*,#49918,.F.);
#72497=ORIENTED_EDGE('',*,*,#51787,.F.);
#72498=ORIENTED_EDGE('',*,*,#46886,.F.);
#72499=ORIENTED_EDGE('',*,*,#51786,.T.);
#72500=ORIENTED_EDGE('',*,*,#46222,.F.);
#72501=ORIENTED_EDGE('',*,*,#51788,.F.);
#72502=ORIENTED_EDGE('',*,*,#49898,.F.);
#72503=ORIENTED_EDGE('',*,*,#51787,.T.);
#72504=ORIENTED_EDGE('',*,*,#49917,.F.);
#72505=ORIENTED_EDGE('',*,*,#51789,.F.);
#72506=ORIENTED_EDGE('',*,*,#46904,.F.);
#72507=ORIENTED_EDGE('',*,*,#51788,.T.);
#72508=ORIENTED_EDGE('',*,*,#46221,.F.);
#72509=ORIENTED_EDGE('',*,*,#51790,.F.);
#72510=ORIENTED_EDGE('',*,*,#50351,.F.);
#72511=ORIENTED_EDGE('',*,*,#51789,.T.);
#72512=ORIENTED_EDGE('',*,*,#49916,.F.);
#72513=ORIENTED_EDGE('',*,*,#51791,.F.);
#72514=ORIENTED_EDGE('',*,*,#46509,.F.);
#72515=ORIENTED_EDGE('',*,*,#51790,.T.);
#72516=ORIENTED_EDGE('',*,*,#46220,.F.);
#72517=ORIENTED_EDGE('',*,*,#51792,.F.);
#72518=ORIENTED_EDGE('',*,*,#49904,.F.);
#72519=ORIENTED_EDGE('',*,*,#51791,.T.);
#72520=ORIENTED_EDGE('',*,*,#50350,.F.);
#72521=ORIENTED_EDGE('',*,*,#51793,.F.);
#72522=ORIENTED_EDGE('',*,*,#46510,.F.);
#72523=ORIENTED_EDGE('',*,*,#51792,.T.);
#72524=ORIENTED_EDGE('',*,*,#46935,.F.);
#72525=ORIENTED_EDGE('',*,*,#51794,.F.);
#72526=ORIENTED_EDGE('',*,*,#49905,.F.);
#72527=ORIENTED_EDGE('',*,*,#51793,.T.);
#72528=ORIENTED_EDGE('',*,*,#49900,.F.);
#72529=ORIENTED_EDGE('',*,*,#51795,.F.);
#72530=ORIENTED_EDGE('',*,*,#46511,.F.);
#72531=ORIENTED_EDGE('',*,*,#46930,.F.);
#72532=ORIENTED_EDGE('',*,*,#46926,.T.);
#72533=ORIENTED_EDGE('',*,*,#51796,.F.);
#72534=ORIENTED_EDGE('',*,*,#49906,.F.);
#72535=ORIENTED_EDGE('',*,*,#51794,.T.);
#72536=ORIENTED_EDGE('',*,*,#51795,.T.);
#72537=ORIENTED_EDGE('',*,*,#50352,.F.);
#72538=ORIENTED_EDGE('',*,*,#51797,.F.);
#72539=ORIENTED_EDGE('',*,*,#46512,.F.);
#72540=ORIENTED_EDGE('',*,*,#51796,.T.);
#72541=ORIENTED_EDGE('',*,*,#46925,.F.);
#72542=ORIENTED_EDGE('',*,*,#51798,.F.);
#72543=ORIENTED_EDGE('',*,*,#49907,.F.);
#72544=ORIENTED_EDGE('',*,*,#51797,.T.);
#72545=ORIENTED_EDGE('',*,*,#49902,.F.);
#72546=ORIENTED_EDGE('',*,*,#51799,.F.);
#72547=ORIENTED_EDGE('',*,*,#46513,.F.);
#72548=ORIENTED_EDGE('',*,*,#51798,.T.);
#72549=ORIENTED_EDGE('',*,*,#46937,.F.);
#72550=ORIENTED_EDGE('',*,*,#51800,.F.);
#72551=ORIENTED_EDGE('',*,*,#49908,.F.);
#72552=ORIENTED_EDGE('',*,*,#51799,.T.);
#72553=ORIENTED_EDGE('',*,*,#49901,.F.);
#72554=ORIENTED_EDGE('',*,*,#51801,.F.);
#72555=ORIENTED_EDGE('',*,*,#46933,.F.);
#72556=ORIENTED_EDGE('',*,*,#51800,.T.);
#72557=ORIENTED_EDGE('',*,*,#46921,.F.);
#72558=ORIENTED_EDGE('',*,*,#51802,.F.);
#72559=ORIENTED_EDGE('',*,*,#49909,.F.);
#72560=ORIENTED_EDGE('',*,*,#51801,.T.);
#72561=ORIENTED_EDGE('',*,*,#49912,.F.);
#72562=ORIENTED_EDGE('',*,*,#51803,.F.);
#72563=ORIENTED_EDGE('',*,*,#46912,.F.);
#72564=ORIENTED_EDGE('',*,*,#51802,.T.);
#72565=ORIENTED_EDGE('',*,*,#46939,.F.);
#72566=ORIENTED_EDGE('',*,*,#51804,.F.);
#72567=ORIENTED_EDGE('',*,*,#49910,.F.);
#72568=ORIENTED_EDGE('',*,*,#51803,.T.);
#72569=ORIENTED_EDGE('',*,*,#49911,.F.);
#72570=ORIENTED_EDGE('',*,*,#51804,.T.);
#72571=ORIENTED_EDGE('',*,*,#46917,.F.);
#72572=ORIENTED_EDGE('',*,*,#46913,.T.);
#72573=ORIENTED_EDGE('',*,*,#51805,.F.);
#72574=ORIENTED_EDGE('',*,*,#49951,.F.);
#72575=ORIENTED_EDGE('',*,*,#51806,.F.);
#72576=ORIENTED_EDGE('',*,*,#46869,.F.);
#72577=ORIENTED_EDGE('',*,*,#51806,.T.);
#72578=ORIENTED_EDGE('',*,*,#49950,.F.);
#72579=ORIENTED_EDGE('',*,*,#51807,.F.);
#72580=ORIENTED_EDGE('',*,*,#46878,.F.);
#72581=ORIENTED_EDGE('',*,*,#46868,.T.);
#72582=ORIENTED_EDGE('',*,*,#46872,.F.);
#72583=ORIENTED_EDGE('',*,*,#51808,.F.);
#72584=ORIENTED_EDGE('',*,*,#49952,.F.);
#72585=ORIENTED_EDGE('',*,*,#51805,.T.);
#72586=ORIENTED_EDGE('',*,*,#51807,.T.);
#72587=ORIENTED_EDGE('',*,*,#49949,.F.);
#72588=ORIENTED_EDGE('',*,*,#51809,.F.);
#72589=ORIENTED_EDGE('',*,*,#46863,.F.);
#72590=ORIENTED_EDGE('',*,*,#51808,.T.);
#72591=ORIENTED_EDGE('',*,*,#46876,.F.);
#72592=ORIENTED_EDGE('',*,*,#51810,.F.);
#72593=ORIENTED_EDGE('',*,*,#49941,.F.);
#72594=ORIENTED_EDGE('',*,*,#51809,.T.);
#72595=ORIENTED_EDGE('',*,*,#49948,.F.);
#72596=ORIENTED_EDGE('',*,*,#51811,.F.);
#72597=ORIENTED_EDGE('',*,*,#46880,.F.);
#72598=ORIENTED_EDGE('',*,*,#51810,.T.);
#72599=ORIENTED_EDGE('',*,*,#46230,.F.);
#72600=ORIENTED_EDGE('',*,*,#51812,.F.);
#72601=ORIENTED_EDGE('',*,*,#49942,.F.);
#72602=ORIENTED_EDGE('',*,*,#51811,.T.);
#72603=ORIENTED_EDGE('',*,*,#49947,.F.);
#72604=ORIENTED_EDGE('',*,*,#51813,.F.);
#72605=ORIENTED_EDGE('',*,*,#46855,.T.);
#72606=ORIENTED_EDGE('',*,*,#46859,.F.);
#72607=ORIENTED_EDGE('',*,*,#51812,.T.);
#72608=ORIENTED_EDGE('',*,*,#46229,.F.);
#72609=ORIENTED_EDGE('',*,*,#51814,.F.);
#72610=ORIENTED_EDGE('',*,*,#50353,.F.);
#72611=ORIENTED_EDGE('',*,*,#51813,.T.);
#72612=ORIENTED_EDGE('',*,*,#49946,.F.);
#72613=ORIENTED_EDGE('',*,*,#51815,.F.);
#72614=ORIENTED_EDGE('',*,*,#46856,.F.);
#72615=ORIENTED_EDGE('',*,*,#51814,.T.);
#72616=ORIENTED_EDGE('',*,*,#46228,.F.);
#72617=ORIENTED_EDGE('',*,*,#51816,.F.);
#72618=ORIENTED_EDGE('',*,*,#49926,.F.);
#72619=ORIENTED_EDGE('',*,*,#51815,.T.);
#72620=ORIENTED_EDGE('',*,*,#49945,.F.);
#72621=ORIENTED_EDGE('',*,*,#51817,.F.);
#72622=ORIENTED_EDGE('',*,*,#46874,.F.);
#72623=ORIENTED_EDGE('',*,*,#51816,.T.);
#72624=ORIENTED_EDGE('',*,*,#46227,.F.);
#72625=ORIENTED_EDGE('',*,*,#51818,.F.);
#72626=ORIENTED_EDGE('',*,*,#50355,.F.);
#72627=ORIENTED_EDGE('',*,*,#51817,.T.);
#72628=ORIENTED_EDGE('',*,*,#49944,.F.);
#72629=ORIENTED_EDGE('',*,*,#51819,.F.);
#72630=ORIENTED_EDGE('',*,*,#46503,.F.);
#72631=ORIENTED_EDGE('',*,*,#51818,.T.);
#72632=ORIENTED_EDGE('',*,*,#46226,.F.);
#72633=ORIENTED_EDGE('',*,*,#51820,.F.);
#72634=ORIENTED_EDGE('',*,*,#49932,.F.);
#72635=ORIENTED_EDGE('',*,*,#51819,.T.);
#72636=ORIENTED_EDGE('',*,*,#50354,.F.);
#72637=ORIENTED_EDGE('',*,*,#51821,.F.);
#72638=ORIENTED_EDGE('',*,*,#46504,.F.);
#72639=ORIENTED_EDGE('',*,*,#51820,.T.);
#72640=ORIENTED_EDGE('',*,*,#46905,.F.);
#72641=ORIENTED_EDGE('',*,*,#51822,.F.);
#72642=ORIENTED_EDGE('',*,*,#49933,.F.);
#72643=ORIENTED_EDGE('',*,*,#51821,.T.);
#72644=ORIENTED_EDGE('',*,*,#49928,.F.);
#72645=ORIENTED_EDGE('',*,*,#51823,.F.);
#72646=ORIENTED_EDGE('',*,*,#46505,.F.);
#72647=ORIENTED_EDGE('',*,*,#46900,.F.);
#72648=ORIENTED_EDGE('',*,*,#46896,.T.);
#72649=ORIENTED_EDGE('',*,*,#51824,.F.);
#72650=ORIENTED_EDGE('',*,*,#49934,.F.);
#72651=ORIENTED_EDGE('',*,*,#51822,.T.);
#72652=ORIENTED_EDGE('',*,*,#51823,.T.);
#72653=ORIENTED_EDGE('',*,*,#50356,.F.);
#72654=ORIENTED_EDGE('',*,*,#51825,.F.);
#72655=ORIENTED_EDGE('',*,*,#46506,.F.);
#72656=ORIENTED_EDGE('',*,*,#51824,.T.);
#72657=ORIENTED_EDGE('',*,*,#46895,.F.);
#72658=ORIENTED_EDGE('',*,*,#51826,.F.);
#72659=ORIENTED_EDGE('',*,*,#49935,.F.);
#72660=ORIENTED_EDGE('',*,*,#51825,.T.);
#72661=ORIENTED_EDGE('',*,*,#49930,.F.);
#72662=ORIENTED_EDGE('',*,*,#51827,.F.);
#72663=ORIENTED_EDGE('',*,*,#46507,.F.);
#72664=ORIENTED_EDGE('',*,*,#51826,.T.);
#72665=ORIENTED_EDGE('',*,*,#46907,.F.);
#72666=ORIENTED_EDGE('',*,*,#51828,.F.);
#72667=ORIENTED_EDGE('',*,*,#49936,.F.);
#72668=ORIENTED_EDGE('',*,*,#51827,.T.);
#72669=ORIENTED_EDGE('',*,*,#49929,.F.);
#72670=ORIENTED_EDGE('',*,*,#51829,.F.);
#72671=ORIENTED_EDGE('',*,*,#46903,.F.);
#72672=ORIENTED_EDGE('',*,*,#51828,.T.);
#72673=ORIENTED_EDGE('',*,*,#46891,.F.);
#72674=ORIENTED_EDGE('',*,*,#51830,.F.);
#72675=ORIENTED_EDGE('',*,*,#49937,.F.);
#72676=ORIENTED_EDGE('',*,*,#51829,.T.);
#72677=ORIENTED_EDGE('',*,*,#49940,.F.);
#72678=ORIENTED_EDGE('',*,*,#51831,.F.);
#72679=ORIENTED_EDGE('',*,*,#46882,.F.);
#72680=ORIENTED_EDGE('',*,*,#51830,.T.);
#72681=ORIENTED_EDGE('',*,*,#46909,.F.);
#72682=ORIENTED_EDGE('',*,*,#51832,.F.);
#72683=ORIENTED_EDGE('',*,*,#49938,.F.);
#72684=ORIENTED_EDGE('',*,*,#51831,.T.);
#72685=ORIENTED_EDGE('',*,*,#49939,.F.);
#72686=ORIENTED_EDGE('',*,*,#51832,.T.);
#72687=ORIENTED_EDGE('',*,*,#46887,.F.);
#72688=ORIENTED_EDGE('',*,*,#46883,.T.);
#72689=ORIENTED_EDGE('',*,*,#51833,.F.);
#72690=ORIENTED_EDGE('',*,*,#49979,.F.);
#72691=ORIENTED_EDGE('',*,*,#51834,.F.);
#72692=ORIENTED_EDGE('',*,*,#46839,.F.);
#72693=ORIENTED_EDGE('',*,*,#51834,.T.);
#72694=ORIENTED_EDGE('',*,*,#49978,.F.);
#72695=ORIENTED_EDGE('',*,*,#51835,.F.);
#72696=ORIENTED_EDGE('',*,*,#46848,.F.);
#72697=ORIENTED_EDGE('',*,*,#46838,.T.);
#72698=ORIENTED_EDGE('',*,*,#46842,.F.);
#72699=ORIENTED_EDGE('',*,*,#51836,.F.);
#72700=ORIENTED_EDGE('',*,*,#49980,.F.);
#72701=ORIENTED_EDGE('',*,*,#51833,.T.);
#72702=ORIENTED_EDGE('',*,*,#51835,.T.);
#72703=ORIENTED_EDGE('',*,*,#49977,.F.);
#72704=ORIENTED_EDGE('',*,*,#51837,.F.);
#72705=ORIENTED_EDGE('',*,*,#46833,.F.);
#72706=ORIENTED_EDGE('',*,*,#51836,.T.);
#72707=ORIENTED_EDGE('',*,*,#46846,.F.);
#72708=ORIENTED_EDGE('',*,*,#51838,.F.);
#72709=ORIENTED_EDGE('',*,*,#49969,.F.);
#72710=ORIENTED_EDGE('',*,*,#51837,.T.);
#72711=ORIENTED_EDGE('',*,*,#49976,.F.);
#72712=ORIENTED_EDGE('',*,*,#51839,.F.);
#72713=ORIENTED_EDGE('',*,*,#46850,.F.);
#72714=ORIENTED_EDGE('',*,*,#51838,.T.);
#72715=ORIENTED_EDGE('',*,*,#46236,.F.);
#72716=ORIENTED_EDGE('',*,*,#51840,.F.);
#72717=ORIENTED_EDGE('',*,*,#49970,.F.);
#72718=ORIENTED_EDGE('',*,*,#51839,.T.);
#72719=ORIENTED_EDGE('',*,*,#49975,.F.);
#72720=ORIENTED_EDGE('',*,*,#51841,.F.);
#72721=ORIENTED_EDGE('',*,*,#46825,.T.);
#72722=ORIENTED_EDGE('',*,*,#46829,.F.);
#72723=ORIENTED_EDGE('',*,*,#51840,.T.);
#72724=ORIENTED_EDGE('',*,*,#46235,.F.);
#72725=ORIENTED_EDGE('',*,*,#51842,.F.);
#72726=ORIENTED_EDGE('',*,*,#50357,.F.);
#72727=ORIENTED_EDGE('',*,*,#51841,.T.);
#72728=ORIENTED_EDGE('',*,*,#49974,.F.);
#72729=ORIENTED_EDGE('',*,*,#51843,.F.);
#72730=ORIENTED_EDGE('',*,*,#46826,.F.);
#72731=ORIENTED_EDGE('',*,*,#51842,.T.);
#72732=ORIENTED_EDGE('',*,*,#46234,.F.);
#72733=ORIENTED_EDGE('',*,*,#51844,.F.);
#72734=ORIENTED_EDGE('',*,*,#49954,.F.);
#72735=ORIENTED_EDGE('',*,*,#51843,.T.);
#72736=ORIENTED_EDGE('',*,*,#49973,.F.);
#72737=ORIENTED_EDGE('',*,*,#51845,.F.);
#72738=ORIENTED_EDGE('',*,*,#46844,.F.);
#72739=ORIENTED_EDGE('',*,*,#51844,.T.);
#72740=ORIENTED_EDGE('',*,*,#46233,.F.);
#72741=ORIENTED_EDGE('',*,*,#51846,.F.);
#72742=ORIENTED_EDGE('',*,*,#50359,.F.);
#72743=ORIENTED_EDGE('',*,*,#51845,.T.);
#72744=ORIENTED_EDGE('',*,*,#49972,.F.);
#72745=ORIENTED_EDGE('',*,*,#51847,.F.);
#72746=ORIENTED_EDGE('',*,*,#46497,.F.);
#72747=ORIENTED_EDGE('',*,*,#51846,.T.);
#72748=ORIENTED_EDGE('',*,*,#46232,.F.);
#72749=ORIENTED_EDGE('',*,*,#51848,.F.);
#72750=ORIENTED_EDGE('',*,*,#49960,.F.);
#72751=ORIENTED_EDGE('',*,*,#51847,.T.);
#72752=ORIENTED_EDGE('',*,*,#50358,.F.);
#72753=ORIENTED_EDGE('',*,*,#51849,.F.);
#72754=ORIENTED_EDGE('',*,*,#46498,.F.);
#72755=ORIENTED_EDGE('',*,*,#51848,.T.);
#72756=ORIENTED_EDGE('',*,*,#46875,.F.);
#72757=ORIENTED_EDGE('',*,*,#51850,.F.);
#72758=ORIENTED_EDGE('',*,*,#49961,.F.);
#72759=ORIENTED_EDGE('',*,*,#51849,.T.);
#72760=ORIENTED_EDGE('',*,*,#49956,.F.);
#72761=ORIENTED_EDGE('',*,*,#51851,.F.);
#72762=ORIENTED_EDGE('',*,*,#46499,.F.);
#72763=ORIENTED_EDGE('',*,*,#46870,.F.);
#72764=ORIENTED_EDGE('',*,*,#46866,.T.);
#72765=ORIENTED_EDGE('',*,*,#51852,.F.);
#72766=ORIENTED_EDGE('',*,*,#49962,.F.);
#72767=ORIENTED_EDGE('',*,*,#51850,.T.);
#72768=ORIENTED_EDGE('',*,*,#51851,.T.);
#72769=ORIENTED_EDGE('',*,*,#50360,.F.);
#72770=ORIENTED_EDGE('',*,*,#51853,.F.);
#72771=ORIENTED_EDGE('',*,*,#46500,.F.);
#72772=ORIENTED_EDGE('',*,*,#51852,.T.);
#72773=ORIENTED_EDGE('',*,*,#46865,.F.);
#72774=ORIENTED_EDGE('',*,*,#51854,.F.);
#72775=ORIENTED_EDGE('',*,*,#49963,.F.);
#72776=ORIENTED_EDGE('',*,*,#51853,.T.);
#72777=ORIENTED_EDGE('',*,*,#49958,.F.);
#72778=ORIENTED_EDGE('',*,*,#51855,.F.);
#72779=ORIENTED_EDGE('',*,*,#46501,.F.);
#72780=ORIENTED_EDGE('',*,*,#51854,.T.);
#72781=ORIENTED_EDGE('',*,*,#46877,.F.);
#72782=ORIENTED_EDGE('',*,*,#51856,.F.);
#72783=ORIENTED_EDGE('',*,*,#49964,.F.);
#72784=ORIENTED_EDGE('',*,*,#51855,.T.);
#72785=ORIENTED_EDGE('',*,*,#49957,.F.);
#72786=ORIENTED_EDGE('',*,*,#51857,.F.);
#72787=ORIENTED_EDGE('',*,*,#46873,.F.);
#72788=ORIENTED_EDGE('',*,*,#51856,.T.);
#72789=ORIENTED_EDGE('',*,*,#46861,.F.);
#72790=ORIENTED_EDGE('',*,*,#51858,.F.);
#72791=ORIENTED_EDGE('',*,*,#49965,.F.);
#72792=ORIENTED_EDGE('',*,*,#51857,.T.);
#72793=ORIENTED_EDGE('',*,*,#49968,.F.);
#72794=ORIENTED_EDGE('',*,*,#51859,.F.);
#72795=ORIENTED_EDGE('',*,*,#46852,.F.);
#72796=ORIENTED_EDGE('',*,*,#51858,.T.);
#72797=ORIENTED_EDGE('',*,*,#46879,.F.);
#72798=ORIENTED_EDGE('',*,*,#51860,.F.);
#72799=ORIENTED_EDGE('',*,*,#49966,.F.);
#72800=ORIENTED_EDGE('',*,*,#51859,.T.);
#72801=ORIENTED_EDGE('',*,*,#49967,.F.);
#72802=ORIENTED_EDGE('',*,*,#51860,.T.);
#72803=ORIENTED_EDGE('',*,*,#46857,.F.);
#72804=ORIENTED_EDGE('',*,*,#46853,.T.);
#72805=ORIENTED_EDGE('',*,*,#51861,.F.);
#72806=ORIENTED_EDGE('',*,*,#50007,.F.);
#72807=ORIENTED_EDGE('',*,*,#51862,.F.);
#72808=ORIENTED_EDGE('',*,*,#46809,.F.);
#72809=ORIENTED_EDGE('',*,*,#51862,.T.);
#72810=ORIENTED_EDGE('',*,*,#50006,.F.);
#72811=ORIENTED_EDGE('',*,*,#51863,.F.);
#72812=ORIENTED_EDGE('',*,*,#46818,.F.);
#72813=ORIENTED_EDGE('',*,*,#46808,.T.);
#72814=ORIENTED_EDGE('',*,*,#46812,.F.);
#72815=ORIENTED_EDGE('',*,*,#51864,.F.);
#72816=ORIENTED_EDGE('',*,*,#50008,.F.);
#72817=ORIENTED_EDGE('',*,*,#51861,.T.);
#72818=ORIENTED_EDGE('',*,*,#51863,.T.);
#72819=ORIENTED_EDGE('',*,*,#50005,.F.);
#72820=ORIENTED_EDGE('',*,*,#51865,.F.);
#72821=ORIENTED_EDGE('',*,*,#46803,.F.);
#72822=ORIENTED_EDGE('',*,*,#51864,.T.);
#72823=ORIENTED_EDGE('',*,*,#46816,.F.);
#72824=ORIENTED_EDGE('',*,*,#51866,.F.);
#72825=ORIENTED_EDGE('',*,*,#49997,.F.);
#72826=ORIENTED_EDGE('',*,*,#51865,.T.);
#72827=ORIENTED_EDGE('',*,*,#50004,.F.);
#72828=ORIENTED_EDGE('',*,*,#51867,.F.);
#72829=ORIENTED_EDGE('',*,*,#46820,.F.);
#72830=ORIENTED_EDGE('',*,*,#51866,.T.);
#72831=ORIENTED_EDGE('',*,*,#46242,.F.);
#72832=ORIENTED_EDGE('',*,*,#51868,.F.);
#72833=ORIENTED_EDGE('',*,*,#49998,.F.);
#72834=ORIENTED_EDGE('',*,*,#51867,.T.);
#72835=ORIENTED_EDGE('',*,*,#50003,.F.);
#72836=ORIENTED_EDGE('',*,*,#51869,.F.);
#72837=ORIENTED_EDGE('',*,*,#46795,.T.);
#72838=ORIENTED_EDGE('',*,*,#46799,.F.);
#72839=ORIENTED_EDGE('',*,*,#51868,.T.);
#72840=ORIENTED_EDGE('',*,*,#46241,.F.);
#72841=ORIENTED_EDGE('',*,*,#51870,.F.);
#72842=ORIENTED_EDGE('',*,*,#50361,.F.);
#72843=ORIENTED_EDGE('',*,*,#51869,.T.);
#72844=ORIENTED_EDGE('',*,*,#50002,.F.);
#72845=ORIENTED_EDGE('',*,*,#51871,.F.);
#72846=ORIENTED_EDGE('',*,*,#46796,.F.);
#72847=ORIENTED_EDGE('',*,*,#51870,.T.);
#72848=ORIENTED_EDGE('',*,*,#46240,.F.);
#72849=ORIENTED_EDGE('',*,*,#51872,.F.);
#72850=ORIENTED_EDGE('',*,*,#49982,.F.);
#72851=ORIENTED_EDGE('',*,*,#51871,.T.);
#72852=ORIENTED_EDGE('',*,*,#50001,.F.);
#72853=ORIENTED_EDGE('',*,*,#51873,.F.);
#72854=ORIENTED_EDGE('',*,*,#46814,.F.);
#72855=ORIENTED_EDGE('',*,*,#51872,.T.);
#72856=ORIENTED_EDGE('',*,*,#46239,.F.);
#72857=ORIENTED_EDGE('',*,*,#51874,.F.);
#72858=ORIENTED_EDGE('',*,*,#50363,.F.);
#72859=ORIENTED_EDGE('',*,*,#51873,.T.);
#72860=ORIENTED_EDGE('',*,*,#50000,.F.);
#72861=ORIENTED_EDGE('',*,*,#51875,.F.);
#72862=ORIENTED_EDGE('',*,*,#46491,.F.);
#72863=ORIENTED_EDGE('',*,*,#51874,.T.);
#72864=ORIENTED_EDGE('',*,*,#46238,.F.);
#72865=ORIENTED_EDGE('',*,*,#51876,.F.);
#72866=ORIENTED_EDGE('',*,*,#49988,.F.);
#72867=ORIENTED_EDGE('',*,*,#51875,.T.);
#72868=ORIENTED_EDGE('',*,*,#50362,.F.);
#72869=ORIENTED_EDGE('',*,*,#51877,.F.);
#72870=ORIENTED_EDGE('',*,*,#46492,.F.);
#72871=ORIENTED_EDGE('',*,*,#51876,.T.);
#72872=ORIENTED_EDGE('',*,*,#46845,.F.);
#72873=ORIENTED_EDGE('',*,*,#51878,.F.);
#72874=ORIENTED_EDGE('',*,*,#49989,.F.);
#72875=ORIENTED_EDGE('',*,*,#51877,.T.);
#72876=ORIENTED_EDGE('',*,*,#49984,.F.);
#72877=ORIENTED_EDGE('',*,*,#51879,.F.);
#72878=ORIENTED_EDGE('',*,*,#46493,.F.);
#72879=ORIENTED_EDGE('',*,*,#46840,.F.);
#72880=ORIENTED_EDGE('',*,*,#46836,.T.);
#72881=ORIENTED_EDGE('',*,*,#51880,.F.);
#72882=ORIENTED_EDGE('',*,*,#49990,.F.);
#72883=ORIENTED_EDGE('',*,*,#51878,.T.);
#72884=ORIENTED_EDGE('',*,*,#51879,.T.);
#72885=ORIENTED_EDGE('',*,*,#50364,.F.);
#72886=ORIENTED_EDGE('',*,*,#51881,.F.);
#72887=ORIENTED_EDGE('',*,*,#46494,.F.);
#72888=ORIENTED_EDGE('',*,*,#51880,.T.);
#72889=ORIENTED_EDGE('',*,*,#46835,.F.);
#72890=ORIENTED_EDGE('',*,*,#51882,.F.);
#72891=ORIENTED_EDGE('',*,*,#49991,.F.);
#72892=ORIENTED_EDGE('',*,*,#51881,.T.);
#72893=ORIENTED_EDGE('',*,*,#49986,.F.);
#72894=ORIENTED_EDGE('',*,*,#51883,.F.);
#72895=ORIENTED_EDGE('',*,*,#46495,.F.);
#72896=ORIENTED_EDGE('',*,*,#51882,.T.);
#72897=ORIENTED_EDGE('',*,*,#46847,.F.);
#72898=ORIENTED_EDGE('',*,*,#51884,.F.);
#72899=ORIENTED_EDGE('',*,*,#49992,.F.);
#72900=ORIENTED_EDGE('',*,*,#51883,.T.);
#72901=ORIENTED_EDGE('',*,*,#49985,.F.);
#72902=ORIENTED_EDGE('',*,*,#51885,.F.);
#72903=ORIENTED_EDGE('',*,*,#46843,.F.);
#72904=ORIENTED_EDGE('',*,*,#51884,.T.);
#72905=ORIENTED_EDGE('',*,*,#46831,.F.);
#72906=ORIENTED_EDGE('',*,*,#51886,.F.);
#72907=ORIENTED_EDGE('',*,*,#49993,.F.);
#72908=ORIENTED_EDGE('',*,*,#51885,.T.);
#72909=ORIENTED_EDGE('',*,*,#49996,.F.);
#72910=ORIENTED_EDGE('',*,*,#51887,.F.);
#72911=ORIENTED_EDGE('',*,*,#46822,.F.);
#72912=ORIENTED_EDGE('',*,*,#51886,.T.);
#72913=ORIENTED_EDGE('',*,*,#46849,.F.);
#72914=ORIENTED_EDGE('',*,*,#51888,.F.);
#72915=ORIENTED_EDGE('',*,*,#49994,.F.);
#72916=ORIENTED_EDGE('',*,*,#51887,.T.);
#72917=ORIENTED_EDGE('',*,*,#49995,.F.);
#72918=ORIENTED_EDGE('',*,*,#51888,.T.);
#72919=ORIENTED_EDGE('',*,*,#46827,.F.);
#72920=ORIENTED_EDGE('',*,*,#46823,.T.);
#72921=ORIENTED_EDGE('',*,*,#51889,.F.);
#72922=ORIENTED_EDGE('',*,*,#50035,.F.);
#72923=ORIENTED_EDGE('',*,*,#51890,.F.);
#72924=ORIENTED_EDGE('',*,*,#46779,.F.);
#72925=ORIENTED_EDGE('',*,*,#51890,.T.);
#72926=ORIENTED_EDGE('',*,*,#50034,.F.);
#72927=ORIENTED_EDGE('',*,*,#51891,.F.);
#72928=ORIENTED_EDGE('',*,*,#46788,.F.);
#72929=ORIENTED_EDGE('',*,*,#46778,.T.);
#72930=ORIENTED_EDGE('',*,*,#46782,.F.);
#72931=ORIENTED_EDGE('',*,*,#51892,.F.);
#72932=ORIENTED_EDGE('',*,*,#50036,.F.);
#72933=ORIENTED_EDGE('',*,*,#51889,.T.);
#72934=ORIENTED_EDGE('',*,*,#51891,.T.);
#72935=ORIENTED_EDGE('',*,*,#50033,.F.);
#72936=ORIENTED_EDGE('',*,*,#51893,.F.);
#72937=ORIENTED_EDGE('',*,*,#46773,.F.);
#72938=ORIENTED_EDGE('',*,*,#51892,.T.);
#72939=ORIENTED_EDGE('',*,*,#46786,.F.);
#72940=ORIENTED_EDGE('',*,*,#51894,.F.);
#72941=ORIENTED_EDGE('',*,*,#50025,.F.);
#72942=ORIENTED_EDGE('',*,*,#51893,.T.);
#72943=ORIENTED_EDGE('',*,*,#50032,.F.);
#72944=ORIENTED_EDGE('',*,*,#51895,.F.);
#72945=ORIENTED_EDGE('',*,*,#46790,.F.);
#72946=ORIENTED_EDGE('',*,*,#51894,.T.);
#72947=ORIENTED_EDGE('',*,*,#46248,.F.);
#72948=ORIENTED_EDGE('',*,*,#51896,.F.);
#72949=ORIENTED_EDGE('',*,*,#50026,.F.);
#72950=ORIENTED_EDGE('',*,*,#51895,.T.);
#72951=ORIENTED_EDGE('',*,*,#50031,.F.);
#72952=ORIENTED_EDGE('',*,*,#51897,.F.);
#72953=ORIENTED_EDGE('',*,*,#46765,.T.);
#72954=ORIENTED_EDGE('',*,*,#46769,.F.);
#72955=ORIENTED_EDGE('',*,*,#51896,.T.);
#72956=ORIENTED_EDGE('',*,*,#46247,.F.);
#72957=ORIENTED_EDGE('',*,*,#51898,.F.);
#72958=ORIENTED_EDGE('',*,*,#50365,.F.);
#72959=ORIENTED_EDGE('',*,*,#51897,.T.);
#72960=ORIENTED_EDGE('',*,*,#50030,.F.);
#72961=ORIENTED_EDGE('',*,*,#51899,.F.);
#72962=ORIENTED_EDGE('',*,*,#46766,.F.);
#72963=ORIENTED_EDGE('',*,*,#51898,.T.);
#72964=ORIENTED_EDGE('',*,*,#46246,.F.);
#72965=ORIENTED_EDGE('',*,*,#51900,.F.);
#72966=ORIENTED_EDGE('',*,*,#50010,.F.);
#72967=ORIENTED_EDGE('',*,*,#51899,.T.);
#72968=ORIENTED_EDGE('',*,*,#50029,.F.);
#72969=ORIENTED_EDGE('',*,*,#51901,.F.);
#72970=ORIENTED_EDGE('',*,*,#46784,.F.);
#72971=ORIENTED_EDGE('',*,*,#51900,.T.);
#72972=ORIENTED_EDGE('',*,*,#46245,.F.);
#72973=ORIENTED_EDGE('',*,*,#51902,.F.);
#72974=ORIENTED_EDGE('',*,*,#50367,.F.);
#72975=ORIENTED_EDGE('',*,*,#51901,.T.);
#72976=ORIENTED_EDGE('',*,*,#50028,.F.);
#72977=ORIENTED_EDGE('',*,*,#51903,.F.);
#72978=ORIENTED_EDGE('',*,*,#46485,.F.);
#72979=ORIENTED_EDGE('',*,*,#51902,.T.);
#72980=ORIENTED_EDGE('',*,*,#46244,.F.);
#72981=ORIENTED_EDGE('',*,*,#51904,.F.);
#72982=ORIENTED_EDGE('',*,*,#50016,.F.);
#72983=ORIENTED_EDGE('',*,*,#51903,.T.);
#72984=ORIENTED_EDGE('',*,*,#50366,.F.);
#72985=ORIENTED_EDGE('',*,*,#51905,.F.);
#72986=ORIENTED_EDGE('',*,*,#46486,.F.);
#72987=ORIENTED_EDGE('',*,*,#51904,.T.);
#72988=ORIENTED_EDGE('',*,*,#46815,.F.);
#72989=ORIENTED_EDGE('',*,*,#51906,.F.);
#72990=ORIENTED_EDGE('',*,*,#50017,.F.);
#72991=ORIENTED_EDGE('',*,*,#51905,.T.);
#72992=ORIENTED_EDGE('',*,*,#50012,.F.);
#72993=ORIENTED_EDGE('',*,*,#51907,.F.);
#72994=ORIENTED_EDGE('',*,*,#46487,.F.);
#72995=ORIENTED_EDGE('',*,*,#46810,.F.);
#72996=ORIENTED_EDGE('',*,*,#46806,.T.);
#72997=ORIENTED_EDGE('',*,*,#51908,.F.);
#72998=ORIENTED_EDGE('',*,*,#50018,.F.);
#72999=ORIENTED_EDGE('',*,*,#51906,.T.);
#73000=ORIENTED_EDGE('',*,*,#51907,.T.);
#73001=ORIENTED_EDGE('',*,*,#50368,.F.);
#73002=ORIENTED_EDGE('',*,*,#51909,.F.);
#73003=ORIENTED_EDGE('',*,*,#46488,.F.);
#73004=ORIENTED_EDGE('',*,*,#51908,.T.);
#73005=ORIENTED_EDGE('',*,*,#46805,.F.);
#73006=ORIENTED_EDGE('',*,*,#51910,.F.);
#73007=ORIENTED_EDGE('',*,*,#50019,.F.);
#73008=ORIENTED_EDGE('',*,*,#51909,.T.);
#73009=ORIENTED_EDGE('',*,*,#50014,.F.);
#73010=ORIENTED_EDGE('',*,*,#51911,.F.);
#73011=ORIENTED_EDGE('',*,*,#46489,.F.);
#73012=ORIENTED_EDGE('',*,*,#51910,.T.);
#73013=ORIENTED_EDGE('',*,*,#46817,.F.);
#73014=ORIENTED_EDGE('',*,*,#51912,.F.);
#73015=ORIENTED_EDGE('',*,*,#50020,.F.);
#73016=ORIENTED_EDGE('',*,*,#51911,.T.);
#73017=ORIENTED_EDGE('',*,*,#50013,.F.);
#73018=ORIENTED_EDGE('',*,*,#51913,.F.);
#73019=ORIENTED_EDGE('',*,*,#46813,.F.);
#73020=ORIENTED_EDGE('',*,*,#51912,.T.);
#73021=ORIENTED_EDGE('',*,*,#46801,.F.);
#73022=ORIENTED_EDGE('',*,*,#51914,.F.);
#73023=ORIENTED_EDGE('',*,*,#50021,.F.);
#73024=ORIENTED_EDGE('',*,*,#51913,.T.);
#73025=ORIENTED_EDGE('',*,*,#50024,.F.);
#73026=ORIENTED_EDGE('',*,*,#51915,.F.);
#73027=ORIENTED_EDGE('',*,*,#46792,.F.);
#73028=ORIENTED_EDGE('',*,*,#51914,.T.);
#73029=ORIENTED_EDGE('',*,*,#46819,.F.);
#73030=ORIENTED_EDGE('',*,*,#51916,.F.);
#73031=ORIENTED_EDGE('',*,*,#50022,.F.);
#73032=ORIENTED_EDGE('',*,*,#51915,.T.);
#73033=ORIENTED_EDGE('',*,*,#50023,.F.);
#73034=ORIENTED_EDGE('',*,*,#51916,.T.);
#73035=ORIENTED_EDGE('',*,*,#46797,.F.);
#73036=ORIENTED_EDGE('',*,*,#46793,.T.);
#73037=ORIENTED_EDGE('',*,*,#51917,.F.);
#73038=ORIENTED_EDGE('',*,*,#50063,.F.);
#73039=ORIENTED_EDGE('',*,*,#51918,.F.);
#73040=ORIENTED_EDGE('',*,*,#46749,.F.);
#73041=ORIENTED_EDGE('',*,*,#51918,.T.);
#73042=ORIENTED_EDGE('',*,*,#50062,.F.);
#73043=ORIENTED_EDGE('',*,*,#51919,.F.);
#73044=ORIENTED_EDGE('',*,*,#46758,.F.);
#73045=ORIENTED_EDGE('',*,*,#46748,.T.);
#73046=ORIENTED_EDGE('',*,*,#46752,.F.);
#73047=ORIENTED_EDGE('',*,*,#51920,.F.);
#73048=ORIENTED_EDGE('',*,*,#50064,.F.);
#73049=ORIENTED_EDGE('',*,*,#51917,.T.);
#73050=ORIENTED_EDGE('',*,*,#51919,.T.);
#73051=ORIENTED_EDGE('',*,*,#50061,.F.);
#73052=ORIENTED_EDGE('',*,*,#51921,.F.);
#73053=ORIENTED_EDGE('',*,*,#46743,.F.);
#73054=ORIENTED_EDGE('',*,*,#51920,.T.);
#73055=ORIENTED_EDGE('',*,*,#46756,.F.);
#73056=ORIENTED_EDGE('',*,*,#51922,.F.);
#73057=ORIENTED_EDGE('',*,*,#50053,.F.);
#73058=ORIENTED_EDGE('',*,*,#51921,.T.);
#73059=ORIENTED_EDGE('',*,*,#50060,.F.);
#73060=ORIENTED_EDGE('',*,*,#51923,.F.);
#73061=ORIENTED_EDGE('',*,*,#46760,.F.);
#73062=ORIENTED_EDGE('',*,*,#51922,.T.);
#73063=ORIENTED_EDGE('',*,*,#46254,.F.);
#73064=ORIENTED_EDGE('',*,*,#51924,.F.);
#73065=ORIENTED_EDGE('',*,*,#50054,.F.);
#73066=ORIENTED_EDGE('',*,*,#51923,.T.);
#73067=ORIENTED_EDGE('',*,*,#50059,.F.);
#73068=ORIENTED_EDGE('',*,*,#51925,.F.);
#73069=ORIENTED_EDGE('',*,*,#46735,.T.);
#73070=ORIENTED_EDGE('',*,*,#46739,.F.);
#73071=ORIENTED_EDGE('',*,*,#51924,.T.);
#73072=ORIENTED_EDGE('',*,*,#46253,.F.);
#73073=ORIENTED_EDGE('',*,*,#51926,.F.);
#73074=ORIENTED_EDGE('',*,*,#50369,.F.);
#73075=ORIENTED_EDGE('',*,*,#51925,.T.);
#73076=ORIENTED_EDGE('',*,*,#50058,.F.);
#73077=ORIENTED_EDGE('',*,*,#51927,.F.);
#73078=ORIENTED_EDGE('',*,*,#46736,.F.);
#73079=ORIENTED_EDGE('',*,*,#51926,.T.);
#73080=ORIENTED_EDGE('',*,*,#46252,.F.);
#73081=ORIENTED_EDGE('',*,*,#51928,.F.);
#73082=ORIENTED_EDGE('',*,*,#50038,.F.);
#73083=ORIENTED_EDGE('',*,*,#51927,.T.);
#73084=ORIENTED_EDGE('',*,*,#50057,.F.);
#73085=ORIENTED_EDGE('',*,*,#51929,.F.);
#73086=ORIENTED_EDGE('',*,*,#46754,.F.);
#73087=ORIENTED_EDGE('',*,*,#51928,.T.);
#73088=ORIENTED_EDGE('',*,*,#46251,.F.);
#73089=ORIENTED_EDGE('',*,*,#51930,.F.);
#73090=ORIENTED_EDGE('',*,*,#50371,.F.);
#73091=ORIENTED_EDGE('',*,*,#51929,.T.);
#73092=ORIENTED_EDGE('',*,*,#50056,.F.);
#73093=ORIENTED_EDGE('',*,*,#51931,.F.);
#73094=ORIENTED_EDGE('',*,*,#46479,.F.);
#73095=ORIENTED_EDGE('',*,*,#51930,.T.);
#73096=ORIENTED_EDGE('',*,*,#46250,.F.);
#73097=ORIENTED_EDGE('',*,*,#51932,.F.);
#73098=ORIENTED_EDGE('',*,*,#50044,.F.);
#73099=ORIENTED_EDGE('',*,*,#51931,.T.);
#73100=ORIENTED_EDGE('',*,*,#50370,.F.);
#73101=ORIENTED_EDGE('',*,*,#51933,.F.);
#73102=ORIENTED_EDGE('',*,*,#46480,.F.);
#73103=ORIENTED_EDGE('',*,*,#51932,.T.);
#73104=ORIENTED_EDGE('',*,*,#46785,.F.);
#73105=ORIENTED_EDGE('',*,*,#51934,.F.);
#73106=ORIENTED_EDGE('',*,*,#50045,.F.);
#73107=ORIENTED_EDGE('',*,*,#51933,.T.);
#73108=ORIENTED_EDGE('',*,*,#50040,.F.);
#73109=ORIENTED_EDGE('',*,*,#51935,.F.);
#73110=ORIENTED_EDGE('',*,*,#46481,.F.);
#73111=ORIENTED_EDGE('',*,*,#46780,.F.);
#73112=ORIENTED_EDGE('',*,*,#46776,.T.);
#73113=ORIENTED_EDGE('',*,*,#51936,.F.);
#73114=ORIENTED_EDGE('',*,*,#50046,.F.);
#73115=ORIENTED_EDGE('',*,*,#51934,.T.);
#73116=ORIENTED_EDGE('',*,*,#51935,.T.);
#73117=ORIENTED_EDGE('',*,*,#50372,.F.);
#73118=ORIENTED_EDGE('',*,*,#51937,.F.);
#73119=ORIENTED_EDGE('',*,*,#46482,.F.);
#73120=ORIENTED_EDGE('',*,*,#51936,.T.);
#73121=ORIENTED_EDGE('',*,*,#46775,.F.);
#73122=ORIENTED_EDGE('',*,*,#51938,.F.);
#73123=ORIENTED_EDGE('',*,*,#50047,.F.);
#73124=ORIENTED_EDGE('',*,*,#51937,.T.);
#73125=ORIENTED_EDGE('',*,*,#50042,.F.);
#73126=ORIENTED_EDGE('',*,*,#51939,.F.);
#73127=ORIENTED_EDGE('',*,*,#46483,.F.);
#73128=ORIENTED_EDGE('',*,*,#51938,.T.);
#73129=ORIENTED_EDGE('',*,*,#46787,.F.);
#73130=ORIENTED_EDGE('',*,*,#51940,.F.);
#73131=ORIENTED_EDGE('',*,*,#50048,.F.);
#73132=ORIENTED_EDGE('',*,*,#51939,.T.);
#73133=ORIENTED_EDGE('',*,*,#50041,.F.);
#73134=ORIENTED_EDGE('',*,*,#51941,.F.);
#73135=ORIENTED_EDGE('',*,*,#46783,.F.);
#73136=ORIENTED_EDGE('',*,*,#51940,.T.);
#73137=ORIENTED_EDGE('',*,*,#46771,.F.);
#73138=ORIENTED_EDGE('',*,*,#51942,.F.);
#73139=ORIENTED_EDGE('',*,*,#50049,.F.);
#73140=ORIENTED_EDGE('',*,*,#51941,.T.);
#73141=ORIENTED_EDGE('',*,*,#50052,.F.);
#73142=ORIENTED_EDGE('',*,*,#51943,.F.);
#73143=ORIENTED_EDGE('',*,*,#46762,.F.);
#73144=ORIENTED_EDGE('',*,*,#51942,.T.);
#73145=ORIENTED_EDGE('',*,*,#46789,.F.);
#73146=ORIENTED_EDGE('',*,*,#51944,.F.);
#73147=ORIENTED_EDGE('',*,*,#50050,.F.);
#73148=ORIENTED_EDGE('',*,*,#51943,.T.);
#73149=ORIENTED_EDGE('',*,*,#50051,.F.);
#73150=ORIENTED_EDGE('',*,*,#51944,.T.);
#73151=ORIENTED_EDGE('',*,*,#46767,.F.);
#73152=ORIENTED_EDGE('',*,*,#46763,.T.);
#73153=ORIENTED_EDGE('',*,*,#51945,.F.);
#73154=ORIENTED_EDGE('',*,*,#50091,.F.);
#73155=ORIENTED_EDGE('',*,*,#51946,.F.);
#73156=ORIENTED_EDGE('',*,*,#46719,.F.);
#73157=ORIENTED_EDGE('',*,*,#51946,.T.);
#73158=ORIENTED_EDGE('',*,*,#50090,.F.);
#73159=ORIENTED_EDGE('',*,*,#51947,.F.);
#73160=ORIENTED_EDGE('',*,*,#46728,.F.);
#73161=ORIENTED_EDGE('',*,*,#46718,.T.);
#73162=ORIENTED_EDGE('',*,*,#46722,.F.);
#73163=ORIENTED_EDGE('',*,*,#51948,.F.);
#73164=ORIENTED_EDGE('',*,*,#50092,.F.);
#73165=ORIENTED_EDGE('',*,*,#51945,.T.);
#73166=ORIENTED_EDGE('',*,*,#51947,.T.);
#73167=ORIENTED_EDGE('',*,*,#50089,.F.);
#73168=ORIENTED_EDGE('',*,*,#51949,.F.);
#73169=ORIENTED_EDGE('',*,*,#46713,.F.);
#73170=ORIENTED_EDGE('',*,*,#51948,.T.);
#73171=ORIENTED_EDGE('',*,*,#46726,.F.);
#73172=ORIENTED_EDGE('',*,*,#51950,.F.);
#73173=ORIENTED_EDGE('',*,*,#50081,.F.);
#73174=ORIENTED_EDGE('',*,*,#51949,.T.);
#73175=ORIENTED_EDGE('',*,*,#50088,.F.);
#73176=ORIENTED_EDGE('',*,*,#51951,.F.);
#73177=ORIENTED_EDGE('',*,*,#46730,.F.);
#73178=ORIENTED_EDGE('',*,*,#51950,.T.);
#73179=ORIENTED_EDGE('',*,*,#46260,.F.);
#73180=ORIENTED_EDGE('',*,*,#51952,.F.);
#73181=ORIENTED_EDGE('',*,*,#50082,.F.);
#73182=ORIENTED_EDGE('',*,*,#51951,.T.);
#73183=ORIENTED_EDGE('',*,*,#50087,.F.);
#73184=ORIENTED_EDGE('',*,*,#51953,.F.);
#73185=ORIENTED_EDGE('',*,*,#46705,.T.);
#73186=ORIENTED_EDGE('',*,*,#46709,.F.);
#73187=ORIENTED_EDGE('',*,*,#51952,.T.);
#73188=ORIENTED_EDGE('',*,*,#46259,.F.);
#73189=ORIENTED_EDGE('',*,*,#51954,.F.);
#73190=ORIENTED_EDGE('',*,*,#50373,.F.);
#73191=ORIENTED_EDGE('',*,*,#51953,.T.);
#73192=ORIENTED_EDGE('',*,*,#50086,.F.);
#73193=ORIENTED_EDGE('',*,*,#51955,.F.);
#73194=ORIENTED_EDGE('',*,*,#46706,.F.);
#73195=ORIENTED_EDGE('',*,*,#51954,.T.);
#73196=ORIENTED_EDGE('',*,*,#46258,.F.);
#73197=ORIENTED_EDGE('',*,*,#51956,.F.);
#73198=ORIENTED_EDGE('',*,*,#50066,.F.);
#73199=ORIENTED_EDGE('',*,*,#51955,.T.);
#73200=ORIENTED_EDGE('',*,*,#50085,.F.);
#73201=ORIENTED_EDGE('',*,*,#51957,.F.);
#73202=ORIENTED_EDGE('',*,*,#46724,.F.);
#73203=ORIENTED_EDGE('',*,*,#51956,.T.);
#73204=ORIENTED_EDGE('',*,*,#46257,.F.);
#73205=ORIENTED_EDGE('',*,*,#51958,.F.);
#73206=ORIENTED_EDGE('',*,*,#50375,.F.);
#73207=ORIENTED_EDGE('',*,*,#51957,.T.);
#73208=ORIENTED_EDGE('',*,*,#50084,.F.);
#73209=ORIENTED_EDGE('',*,*,#51959,.F.);
#73210=ORIENTED_EDGE('',*,*,#46473,.F.);
#73211=ORIENTED_EDGE('',*,*,#51958,.T.);
#73212=ORIENTED_EDGE('',*,*,#46256,.F.);
#73213=ORIENTED_EDGE('',*,*,#51960,.F.);
#73214=ORIENTED_EDGE('',*,*,#50072,.F.);
#73215=ORIENTED_EDGE('',*,*,#51959,.T.);
#73216=ORIENTED_EDGE('',*,*,#50374,.F.);
#73217=ORIENTED_EDGE('',*,*,#51961,.F.);
#73218=ORIENTED_EDGE('',*,*,#46474,.F.);
#73219=ORIENTED_EDGE('',*,*,#51960,.T.);
#73220=ORIENTED_EDGE('',*,*,#46755,.F.);
#73221=ORIENTED_EDGE('',*,*,#51962,.F.);
#73222=ORIENTED_EDGE('',*,*,#50073,.F.);
#73223=ORIENTED_EDGE('',*,*,#51961,.T.);
#73224=ORIENTED_EDGE('',*,*,#50068,.F.);
#73225=ORIENTED_EDGE('',*,*,#51963,.F.);
#73226=ORIENTED_EDGE('',*,*,#46475,.F.);
#73227=ORIENTED_EDGE('',*,*,#46750,.F.);
#73228=ORIENTED_EDGE('',*,*,#46746,.T.);
#73229=ORIENTED_EDGE('',*,*,#51964,.F.);
#73230=ORIENTED_EDGE('',*,*,#50074,.F.);
#73231=ORIENTED_EDGE('',*,*,#51962,.T.);
#73232=ORIENTED_EDGE('',*,*,#51963,.T.);
#73233=ORIENTED_EDGE('',*,*,#50376,.F.);
#73234=ORIENTED_EDGE('',*,*,#51965,.F.);
#73235=ORIENTED_EDGE('',*,*,#46476,.F.);
#73236=ORIENTED_EDGE('',*,*,#51964,.T.);
#73237=ORIENTED_EDGE('',*,*,#46745,.F.);
#73238=ORIENTED_EDGE('',*,*,#51966,.F.);
#73239=ORIENTED_EDGE('',*,*,#50075,.F.);
#73240=ORIENTED_EDGE('',*,*,#51965,.T.);
#73241=ORIENTED_EDGE('',*,*,#50070,.F.);
#73242=ORIENTED_EDGE('',*,*,#51967,.F.);
#73243=ORIENTED_EDGE('',*,*,#46477,.F.);
#73244=ORIENTED_EDGE('',*,*,#51966,.T.);
#73245=ORIENTED_EDGE('',*,*,#46757,.F.);
#73246=ORIENTED_EDGE('',*,*,#51968,.F.);
#73247=ORIENTED_EDGE('',*,*,#50076,.F.);
#73248=ORIENTED_EDGE('',*,*,#51967,.T.);
#73249=ORIENTED_EDGE('',*,*,#50069,.F.);
#73250=ORIENTED_EDGE('',*,*,#51969,.F.);
#73251=ORIENTED_EDGE('',*,*,#46753,.F.);
#73252=ORIENTED_EDGE('',*,*,#51968,.T.);
#73253=ORIENTED_EDGE('',*,*,#46741,.F.);
#73254=ORIENTED_EDGE('',*,*,#51970,.F.);
#73255=ORIENTED_EDGE('',*,*,#50077,.F.);
#73256=ORIENTED_EDGE('',*,*,#51969,.T.);
#73257=ORIENTED_EDGE('',*,*,#50080,.F.);
#73258=ORIENTED_EDGE('',*,*,#51971,.F.);
#73259=ORIENTED_EDGE('',*,*,#46732,.F.);
#73260=ORIENTED_EDGE('',*,*,#51970,.T.);
#73261=ORIENTED_EDGE('',*,*,#46759,.F.);
#73262=ORIENTED_EDGE('',*,*,#51972,.F.);
#73263=ORIENTED_EDGE('',*,*,#50078,.F.);
#73264=ORIENTED_EDGE('',*,*,#51971,.T.);
#73265=ORIENTED_EDGE('',*,*,#50079,.F.);
#73266=ORIENTED_EDGE('',*,*,#51972,.T.);
#73267=ORIENTED_EDGE('',*,*,#46737,.F.);
#73268=ORIENTED_EDGE('',*,*,#46733,.T.);
#73269=ORIENTED_EDGE('',*,*,#51973,.F.);
#73270=ORIENTED_EDGE('',*,*,#50119,.F.);
#73271=ORIENTED_EDGE('',*,*,#51974,.F.);
#73272=ORIENTED_EDGE('',*,*,#46689,.F.);
#73273=ORIENTED_EDGE('',*,*,#51974,.T.);
#73274=ORIENTED_EDGE('',*,*,#50118,.F.);
#73275=ORIENTED_EDGE('',*,*,#51975,.F.);
#73276=ORIENTED_EDGE('',*,*,#46698,.F.);
#73277=ORIENTED_EDGE('',*,*,#46688,.T.);
#73278=ORIENTED_EDGE('',*,*,#46692,.F.);
#73279=ORIENTED_EDGE('',*,*,#51976,.F.);
#73280=ORIENTED_EDGE('',*,*,#50120,.F.);
#73281=ORIENTED_EDGE('',*,*,#51973,.T.);
#73282=ORIENTED_EDGE('',*,*,#51975,.T.);
#73283=ORIENTED_EDGE('',*,*,#50117,.F.);
#73284=ORIENTED_EDGE('',*,*,#51977,.F.);
#73285=ORIENTED_EDGE('',*,*,#46683,.F.);
#73286=ORIENTED_EDGE('',*,*,#51976,.T.);
#73287=ORIENTED_EDGE('',*,*,#46696,.F.);
#73288=ORIENTED_EDGE('',*,*,#51978,.F.);
#73289=ORIENTED_EDGE('',*,*,#50109,.F.);
#73290=ORIENTED_EDGE('',*,*,#51977,.T.);
#73291=ORIENTED_EDGE('',*,*,#50116,.F.);
#73292=ORIENTED_EDGE('',*,*,#51979,.F.);
#73293=ORIENTED_EDGE('',*,*,#46700,.F.);
#73294=ORIENTED_EDGE('',*,*,#51978,.T.);
#73295=ORIENTED_EDGE('',*,*,#46266,.F.);
#73296=ORIENTED_EDGE('',*,*,#51980,.F.);
#73297=ORIENTED_EDGE('',*,*,#50110,.F.);
#73298=ORIENTED_EDGE('',*,*,#51979,.T.);
#73299=ORIENTED_EDGE('',*,*,#50115,.F.);
#73300=ORIENTED_EDGE('',*,*,#51981,.F.);
#73301=ORIENTED_EDGE('',*,*,#46675,.T.);
#73302=ORIENTED_EDGE('',*,*,#46679,.F.);
#73303=ORIENTED_EDGE('',*,*,#51980,.T.);
#73304=ORIENTED_EDGE('',*,*,#46265,.F.);
#73305=ORIENTED_EDGE('',*,*,#51982,.F.);
#73306=ORIENTED_EDGE('',*,*,#50377,.F.);
#73307=ORIENTED_EDGE('',*,*,#51981,.T.);
#73308=ORIENTED_EDGE('',*,*,#50114,.F.);
#73309=ORIENTED_EDGE('',*,*,#51983,.F.);
#73310=ORIENTED_EDGE('',*,*,#46676,.F.);
#73311=ORIENTED_EDGE('',*,*,#51982,.T.);
#73312=ORIENTED_EDGE('',*,*,#46264,.F.);
#73313=ORIENTED_EDGE('',*,*,#51984,.F.);
#73314=ORIENTED_EDGE('',*,*,#50094,.F.);
#73315=ORIENTED_EDGE('',*,*,#51983,.T.);
#73316=ORIENTED_EDGE('',*,*,#50113,.F.);
#73317=ORIENTED_EDGE('',*,*,#51985,.F.);
#73318=ORIENTED_EDGE('',*,*,#46694,.F.);
#73319=ORIENTED_EDGE('',*,*,#51984,.T.);
#73320=ORIENTED_EDGE('',*,*,#46263,.F.);
#73321=ORIENTED_EDGE('',*,*,#51986,.F.);
#73322=ORIENTED_EDGE('',*,*,#50379,.F.);
#73323=ORIENTED_EDGE('',*,*,#51985,.T.);
#73324=ORIENTED_EDGE('',*,*,#50112,.F.);
#73325=ORIENTED_EDGE('',*,*,#51987,.F.);
#73326=ORIENTED_EDGE('',*,*,#46467,.F.);
#73327=ORIENTED_EDGE('',*,*,#51986,.T.);
#73328=ORIENTED_EDGE('',*,*,#46262,.F.);
#73329=ORIENTED_EDGE('',*,*,#51988,.F.);
#73330=ORIENTED_EDGE('',*,*,#50100,.F.);
#73331=ORIENTED_EDGE('',*,*,#51987,.T.);
#73332=ORIENTED_EDGE('',*,*,#50378,.F.);
#73333=ORIENTED_EDGE('',*,*,#51989,.F.);
#73334=ORIENTED_EDGE('',*,*,#46468,.F.);
#73335=ORIENTED_EDGE('',*,*,#51988,.T.);
#73336=ORIENTED_EDGE('',*,*,#46725,.F.);
#73337=ORIENTED_EDGE('',*,*,#51990,.F.);
#73338=ORIENTED_EDGE('',*,*,#50101,.F.);
#73339=ORIENTED_EDGE('',*,*,#51989,.T.);
#73340=ORIENTED_EDGE('',*,*,#50096,.F.);
#73341=ORIENTED_EDGE('',*,*,#51991,.F.);
#73342=ORIENTED_EDGE('',*,*,#46469,.F.);
#73343=ORIENTED_EDGE('',*,*,#46720,.F.);
#73344=ORIENTED_EDGE('',*,*,#46716,.T.);
#73345=ORIENTED_EDGE('',*,*,#51992,.F.);
#73346=ORIENTED_EDGE('',*,*,#50102,.F.);
#73347=ORIENTED_EDGE('',*,*,#51990,.T.);
#73348=ORIENTED_EDGE('',*,*,#51991,.T.);
#73349=ORIENTED_EDGE('',*,*,#50380,.F.);
#73350=ORIENTED_EDGE('',*,*,#51993,.F.);
#73351=ORIENTED_EDGE('',*,*,#46470,.F.);
#73352=ORIENTED_EDGE('',*,*,#51992,.T.);
#73353=ORIENTED_EDGE('',*,*,#46715,.F.);
#73354=ORIENTED_EDGE('',*,*,#51994,.F.);
#73355=ORIENTED_EDGE('',*,*,#50103,.F.);
#73356=ORIENTED_EDGE('',*,*,#51993,.T.);
#73357=ORIENTED_EDGE('',*,*,#50098,.F.);
#73358=ORIENTED_EDGE('',*,*,#51995,.F.);
#73359=ORIENTED_EDGE('',*,*,#46471,.F.);
#73360=ORIENTED_EDGE('',*,*,#51994,.T.);
#73361=ORIENTED_EDGE('',*,*,#46727,.F.);
#73362=ORIENTED_EDGE('',*,*,#51996,.F.);
#73363=ORIENTED_EDGE('',*,*,#50104,.F.);
#73364=ORIENTED_EDGE('',*,*,#51995,.T.);
#73365=ORIENTED_EDGE('',*,*,#50097,.F.);
#73366=ORIENTED_EDGE('',*,*,#51997,.F.);
#73367=ORIENTED_EDGE('',*,*,#46723,.F.);
#73368=ORIENTED_EDGE('',*,*,#51996,.T.);
#73369=ORIENTED_EDGE('',*,*,#46711,.F.);
#73370=ORIENTED_EDGE('',*,*,#51998,.F.);
#73371=ORIENTED_EDGE('',*,*,#50105,.F.);
#73372=ORIENTED_EDGE('',*,*,#51997,.T.);
#73373=ORIENTED_EDGE('',*,*,#50108,.F.);
#73374=ORIENTED_EDGE('',*,*,#51999,.F.);
#73375=ORIENTED_EDGE('',*,*,#46702,.F.);
#73376=ORIENTED_EDGE('',*,*,#51998,.T.);
#73377=ORIENTED_EDGE('',*,*,#46729,.F.);
#73378=ORIENTED_EDGE('',*,*,#52000,.F.);
#73379=ORIENTED_EDGE('',*,*,#50106,.F.);
#73380=ORIENTED_EDGE('',*,*,#51999,.T.);
#73381=ORIENTED_EDGE('',*,*,#50107,.F.);
#73382=ORIENTED_EDGE('',*,*,#52000,.T.);
#73383=ORIENTED_EDGE('',*,*,#46707,.F.);
#73384=ORIENTED_EDGE('',*,*,#46703,.T.);
#73385=ORIENTED_EDGE('',*,*,#52001,.F.);
#73386=ORIENTED_EDGE('',*,*,#50147,.F.);
#73387=ORIENTED_EDGE('',*,*,#52002,.F.);
#73388=ORIENTED_EDGE('',*,*,#46655,.F.);
#73389=ORIENTED_EDGE('',*,*,#52002,.T.);
#73390=ORIENTED_EDGE('',*,*,#50146,.F.);
#73391=ORIENTED_EDGE('',*,*,#52003,.F.);
#73392=ORIENTED_EDGE('',*,*,#46667,.F.);
#73393=ORIENTED_EDGE('',*,*,#46654,.T.);
#73394=ORIENTED_EDGE('',*,*,#46661,.F.);
#73395=ORIENTED_EDGE('',*,*,#52004,.F.);
#73396=ORIENTED_EDGE('',*,*,#50148,.F.);
#73397=ORIENTED_EDGE('',*,*,#52001,.T.);
#73398=ORIENTED_EDGE('',*,*,#52003,.T.);
#73399=ORIENTED_EDGE('',*,*,#50145,.F.);
#73400=ORIENTED_EDGE('',*,*,#52005,.F.);
#73401=ORIENTED_EDGE('',*,*,#46651,.F.);
#73402=ORIENTED_EDGE('',*,*,#52004,.T.);
#73403=ORIENTED_EDGE('',*,*,#46665,.F.);
#73404=ORIENTED_EDGE('',*,*,#52006,.F.);
#73405=ORIENTED_EDGE('',*,*,#50137,.F.);
#73406=ORIENTED_EDGE('',*,*,#52005,.T.);
#73407=ORIENTED_EDGE('',*,*,#50144,.F.);
#73408=ORIENTED_EDGE('',*,*,#52007,.F.);
#73409=ORIENTED_EDGE('',*,*,#46669,.F.);
#73410=ORIENTED_EDGE('',*,*,#52006,.T.);
#73411=ORIENTED_EDGE('',*,*,#46272,.F.);
#73412=ORIENTED_EDGE('',*,*,#52008,.F.);
#73413=ORIENTED_EDGE('',*,*,#50138,.F.);
#73414=ORIENTED_EDGE('',*,*,#52007,.T.);
#73415=ORIENTED_EDGE('',*,*,#50143,.F.);
#73416=ORIENTED_EDGE('',*,*,#52009,.F.);
#73417=ORIENTED_EDGE('',*,*,#46641,.T.);
#73418=ORIENTED_EDGE('',*,*,#46648,.F.);
#73419=ORIENTED_EDGE('',*,*,#52008,.T.);
#73420=ORIENTED_EDGE('',*,*,#46271,.F.);
#73421=ORIENTED_EDGE('',*,*,#52010,.F.);
#73422=ORIENTED_EDGE('',*,*,#50381,.F.);
#73423=ORIENTED_EDGE('',*,*,#52009,.T.);
#73424=ORIENTED_EDGE('',*,*,#50142,.F.);
#73425=ORIENTED_EDGE('',*,*,#52011,.F.);
#73426=ORIENTED_EDGE('',*,*,#46642,.F.);
#73427=ORIENTED_EDGE('',*,*,#52010,.T.);
#73428=ORIENTED_EDGE('',*,*,#46270,.F.);
#73429=ORIENTED_EDGE('',*,*,#52012,.F.);
#73430=ORIENTED_EDGE('',*,*,#50122,.F.);
#73431=ORIENTED_EDGE('',*,*,#52011,.T.);
#73432=ORIENTED_EDGE('',*,*,#50141,.F.);
#73433=ORIENTED_EDGE('',*,*,#52013,.F.);
#73434=ORIENTED_EDGE('',*,*,#46663,.F.);
#73435=ORIENTED_EDGE('',*,*,#52012,.T.);
#73436=ORIENTED_EDGE('',*,*,#46269,.F.);
#73437=ORIENTED_EDGE('',*,*,#52014,.F.);
#73438=ORIENTED_EDGE('',*,*,#50383,.F.);
#73439=ORIENTED_EDGE('',*,*,#52013,.T.);
#73440=ORIENTED_EDGE('',*,*,#50140,.F.);
#73441=ORIENTED_EDGE('',*,*,#52015,.F.);
#73442=ORIENTED_EDGE('',*,*,#46461,.F.);
#73443=ORIENTED_EDGE('',*,*,#52014,.T.);
#73444=ORIENTED_EDGE('',*,*,#46268,.F.);
#73445=ORIENTED_EDGE('',*,*,#52016,.F.);
#73446=ORIENTED_EDGE('',*,*,#50128,.F.);
#73447=ORIENTED_EDGE('',*,*,#52015,.T.);
#73448=ORIENTED_EDGE('',*,*,#50382,.F.);
#73449=ORIENTED_EDGE('',*,*,#52017,.F.);
#73450=ORIENTED_EDGE('',*,*,#46462,.F.);
#73451=ORIENTED_EDGE('',*,*,#52016,.T.);
#73452=ORIENTED_EDGE('',*,*,#46695,.F.);
#73453=ORIENTED_EDGE('',*,*,#52018,.F.);
#73454=ORIENTED_EDGE('',*,*,#50129,.F.);
#73455=ORIENTED_EDGE('',*,*,#52017,.T.);
#73456=ORIENTED_EDGE('',*,*,#50124,.F.);
#73457=ORIENTED_EDGE('',*,*,#52019,.F.);
#73458=ORIENTED_EDGE('',*,*,#46463,.F.);
#73459=ORIENTED_EDGE('',*,*,#46690,.F.);
#73460=ORIENTED_EDGE('',*,*,#46686,.T.);
#73461=ORIENTED_EDGE('',*,*,#52020,.F.);
#73462=ORIENTED_EDGE('',*,*,#50130,.F.);
#73463=ORIENTED_EDGE('',*,*,#52018,.T.);
#73464=ORIENTED_EDGE('',*,*,#52019,.T.);
#73465=ORIENTED_EDGE('',*,*,#50384,.F.);
#73466=ORIENTED_EDGE('',*,*,#52021,.F.);
#73467=ORIENTED_EDGE('',*,*,#46464,.F.);
#73468=ORIENTED_EDGE('',*,*,#52020,.T.);
#73469=ORIENTED_EDGE('',*,*,#46685,.F.);
#73470=ORIENTED_EDGE('',*,*,#52022,.F.);
#73471=ORIENTED_EDGE('',*,*,#50131,.F.);
#73472=ORIENTED_EDGE('',*,*,#52021,.T.);
#73473=ORIENTED_EDGE('',*,*,#50126,.F.);
#73474=ORIENTED_EDGE('',*,*,#52023,.F.);
#73475=ORIENTED_EDGE('',*,*,#46465,.F.);
#73476=ORIENTED_EDGE('',*,*,#52022,.T.);
#73477=ORIENTED_EDGE('',*,*,#46697,.F.);
#73478=ORIENTED_EDGE('',*,*,#52024,.F.);
#73479=ORIENTED_EDGE('',*,*,#50132,.F.);
#73480=ORIENTED_EDGE('',*,*,#52023,.T.);
#73481=ORIENTED_EDGE('',*,*,#50125,.F.);
#73482=ORIENTED_EDGE('',*,*,#52025,.F.);
#73483=ORIENTED_EDGE('',*,*,#46693,.F.);
#73484=ORIENTED_EDGE('',*,*,#52024,.T.);
#73485=ORIENTED_EDGE('',*,*,#46681,.F.);
#73486=ORIENTED_EDGE('',*,*,#52026,.F.);
#73487=ORIENTED_EDGE('',*,*,#50133,.F.);
#73488=ORIENTED_EDGE('',*,*,#52025,.T.);
#73489=ORIENTED_EDGE('',*,*,#50136,.F.);
#73490=ORIENTED_EDGE('',*,*,#52027,.F.);
#73491=ORIENTED_EDGE('',*,*,#46672,.F.);
#73492=ORIENTED_EDGE('',*,*,#52026,.T.);
#73493=ORIENTED_EDGE('',*,*,#46699,.F.);
#73494=ORIENTED_EDGE('',*,*,#52028,.F.);
#73495=ORIENTED_EDGE('',*,*,#50134,.F.);
#73496=ORIENTED_EDGE('',*,*,#52027,.T.);
#73497=ORIENTED_EDGE('',*,*,#50135,.F.);
#73498=ORIENTED_EDGE('',*,*,#52028,.T.);
#73499=ORIENTED_EDGE('',*,*,#46677,.F.);
#73500=ORIENTED_EDGE('',*,*,#46673,.T.);
#73501=ORIENTED_EDGE('',*,*,#52029,.F.);
#73502=ORIENTED_EDGE('',*,*,#52030,.F.);
#73503=ORIENTED_EDGE('',*,*,#52031,.F.);
#73504=ORIENTED_EDGE('',*,*,#52032,.T.);
#73505=ORIENTED_EDGE('',*,*,#52033,.F.);
#73506=ORIENTED_EDGE('',*,*,#52034,.F.);
#73507=ORIENTED_EDGE('',*,*,#52035,.F.);
#73508=ORIENTED_EDGE('',*,*,#52036,.T.);
#73509=ORIENTED_EDGE('',*,*,#52037,.F.);
#73510=ORIENTED_EDGE('',*,*,#52038,.F.);
#73511=ORIENTED_EDGE('',*,*,#52039,.F.);
#73512=ORIENTED_EDGE('',*,*,#52040,.T.);
#73513=ORIENTED_EDGE('',*,*,#52041,.F.);
#73514=ORIENTED_EDGE('',*,*,#52042,.F.);
#73515=ORIENTED_EDGE('',*,*,#52043,.F.);
#73516=ORIENTED_EDGE('',*,*,#52044,.T.);
#73517=ORIENTED_EDGE('',*,*,#52045,.F.);
#73518=ORIENTED_EDGE('',*,*,#52046,.F.);
#73519=ORIENTED_EDGE('',*,*,#52047,.T.);
#73520=ORIENTED_EDGE('',*,*,#52048,.F.);
#73521=ORIENTED_EDGE('',*,*,#52049,.F.);
#73522=ORIENTED_EDGE('',*,*,#52047,.F.);
#73523=ORIENTED_EDGE('',*,*,#52050,.F.);
#73524=ORIENTED_EDGE('',*,*,#52051,.T.);
#73525=ORIENTED_EDGE('',*,*,#52052,.F.);
#73526=ORIENTED_EDGE('',*,*,#52051,.F.);
#73527=ORIENTED_EDGE('',*,*,#52053,.F.);
#73528=ORIENTED_EDGE('',*,*,#52054,.T.);
#73529=ORIENTED_EDGE('',*,*,#52055,.F.);
#73530=ORIENTED_EDGE('',*,*,#52056,.F.);
#73531=ORIENTED_EDGE('',*,*,#52054,.F.);
#73532=ORIENTED_EDGE('',*,*,#52057,.F.);
#73533=ORIENTED_EDGE('',*,*,#52058,.T.);
#73534=ORIENTED_EDGE('',*,*,#52059,.F.);
#73535=ORIENTED_EDGE('',*,*,#52058,.F.);
#73536=ORIENTED_EDGE('',*,*,#52060,.F.);
#73537=ORIENTED_EDGE('',*,*,#52061,.T.);
#73538=ORIENTED_EDGE('',*,*,#52062,.T.);
#73539=ORIENTED_EDGE('',*,*,#52061,.F.);
#73540=ORIENTED_EDGE('',*,*,#52062,.F.);
#73541=ORIENTED_EDGE('',*,*,#52063,.T.);
#73542=ORIENTED_EDGE('',*,*,#52057,.T.);
#73543=ORIENTED_EDGE('',*,*,#52063,.F.);
#73544=ORIENTED_EDGE('',*,*,#52064,.T.);
#73545=ORIENTED_EDGE('',*,*,#52065,.T.);
#73546=ORIENTED_EDGE('',*,*,#52066,.T.);
#73547=ORIENTED_EDGE('',*,*,#52067,.T.);
#73548=ORIENTED_EDGE('',*,*,#52068,.T.);
#73549=ORIENTED_EDGE('',*,*,#52069,.T.);
#73550=ORIENTED_EDGE('',*,*,#52070,.T.);
#73551=ORIENTED_EDGE('',*,*,#52071,.T.);
#73552=ORIENTED_EDGE('',*,*,#52072,.T.);
#73553=ORIENTED_EDGE('',*,*,#52073,.T.);
#73554=ORIENTED_EDGE('',*,*,#52074,.T.);
#73555=ORIENTED_EDGE('',*,*,#52075,.T.);
#73556=ORIENTED_EDGE('',*,*,#52076,.T.);
#73557=ORIENTED_EDGE('',*,*,#52077,.T.);
#73558=ORIENTED_EDGE('',*,*,#52078,.T.);
#73559=ORIENTED_EDGE('',*,*,#52079,.T.);
#73560=ORIENTED_EDGE('',*,*,#52080,.T.);
#73561=ORIENTED_EDGE('',*,*,#52081,.T.);
#73562=ORIENTED_EDGE('',*,*,#52082,.T.);
#73563=ORIENTED_EDGE('',*,*,#52083,.T.);
#73564=ORIENTED_EDGE('',*,*,#52084,.T.);
#73565=ORIENTED_EDGE('',*,*,#52085,.T.);
#73566=ORIENTED_EDGE('',*,*,#52086,.T.);
#73567=ORIENTED_EDGE('',*,*,#52087,.T.);
#73568=ORIENTED_EDGE('',*,*,#52088,.T.);
#73569=ORIENTED_EDGE('',*,*,#52089,.T.);
#73570=ORIENTED_EDGE('',*,*,#52090,.T.);
#73571=ORIENTED_EDGE('',*,*,#52091,.T.);
#73572=ORIENTED_EDGE('',*,*,#52092,.T.);
#73573=ORIENTED_EDGE('',*,*,#52093,.T.);
#73574=ORIENTED_EDGE('',*,*,#52094,.T.);
#73575=ORIENTED_EDGE('',*,*,#52095,.T.);
#73576=ORIENTED_EDGE('',*,*,#52096,.T.);
#73577=ORIENTED_EDGE('',*,*,#52097,.T.);
#73578=ORIENTED_EDGE('',*,*,#52098,.T.);
#73579=ORIENTED_EDGE('',*,*,#52099,.T.);
#73580=ORIENTED_EDGE('',*,*,#52100,.T.);
#73581=ORIENTED_EDGE('',*,*,#52101,.T.);
#73582=ORIENTED_EDGE('',*,*,#52102,.T.);
#73583=ORIENTED_EDGE('',*,*,#52103,.T.);
#73584=ORIENTED_EDGE('',*,*,#52104,.T.);
#73585=ORIENTED_EDGE('',*,*,#52105,.T.);
#73586=ORIENTED_EDGE('',*,*,#52106,.T.);
#73587=ORIENTED_EDGE('',*,*,#52107,.T.);
#73588=ORIENTED_EDGE('',*,*,#52108,.T.);
#73589=ORIENTED_EDGE('',*,*,#52109,.T.);
#73590=ORIENTED_EDGE('',*,*,#52110,.T.);
#73591=ORIENTED_EDGE('',*,*,#52111,.T.);
#73592=ORIENTED_EDGE('',*,*,#52112,.T.);
#73593=ORIENTED_EDGE('',*,*,#52113,.T.);
#73594=ORIENTED_EDGE('',*,*,#52114,.T.);
#73595=ORIENTED_EDGE('',*,*,#52115,.T.);
#73596=ORIENTED_EDGE('',*,*,#52116,.T.);
#73597=ORIENTED_EDGE('',*,*,#52117,.T.);
#73598=ORIENTED_EDGE('',*,*,#52118,.T.);
#73599=ORIENTED_EDGE('',*,*,#52119,.T.);
#73600=ORIENTED_EDGE('',*,*,#52120,.T.);
#73601=ORIENTED_EDGE('',*,*,#52121,.T.);
#73602=ORIENTED_EDGE('',*,*,#52122,.T.);
#73603=ORIENTED_EDGE('',*,*,#52123,.T.);
#73604=ORIENTED_EDGE('',*,*,#52124,.T.);
#73605=ORIENTED_EDGE('',*,*,#52125,.T.);
#73606=ORIENTED_EDGE('',*,*,#52126,.T.);
#73607=ORIENTED_EDGE('',*,*,#52127,.T.);
#73608=ORIENTED_EDGE('',*,*,#52128,.T.);
#73609=ORIENTED_EDGE('',*,*,#52129,.T.);
#73610=ORIENTED_EDGE('',*,*,#52130,.T.);
#73611=ORIENTED_EDGE('',*,*,#52131,.T.);
#73612=ORIENTED_EDGE('',*,*,#52132,.T.);
#73613=ORIENTED_EDGE('',*,*,#52133,.T.);
#73614=ORIENTED_EDGE('',*,*,#52134,.T.);
#73615=ORIENTED_EDGE('',*,*,#52135,.T.);
#73616=ORIENTED_EDGE('',*,*,#52136,.T.);
#73617=ORIENTED_EDGE('',*,*,#52137,.T.);
#73618=ORIENTED_EDGE('',*,*,#52138,.T.);
#73619=ORIENTED_EDGE('',*,*,#52139,.T.);
#73620=ORIENTED_EDGE('',*,*,#52140,.T.);
#73621=ORIENTED_EDGE('',*,*,#52141,.T.);
#73622=ORIENTED_EDGE('',*,*,#52142,.T.);
#73623=ORIENTED_EDGE('',*,*,#52143,.T.);
#73624=ORIENTED_EDGE('',*,*,#52144,.T.);
#73625=ORIENTED_EDGE('',*,*,#52145,.T.);
#73626=ORIENTED_EDGE('',*,*,#52146,.T.);
#73627=ORIENTED_EDGE('',*,*,#52147,.T.);
#73628=ORIENTED_EDGE('',*,*,#52148,.T.);
#73629=ORIENTED_EDGE('',*,*,#52149,.T.);
#73630=ORIENTED_EDGE('',*,*,#52150,.T.);
#73631=ORIENTED_EDGE('',*,*,#52151,.T.);
#73632=ORIENTED_EDGE('',*,*,#52152,.T.);
#73633=ORIENTED_EDGE('',*,*,#52153,.T.);
#73634=ORIENTED_EDGE('',*,*,#52154,.T.);
#73635=ORIENTED_EDGE('',*,*,#52155,.T.);
#73636=ORIENTED_EDGE('',*,*,#52156,.T.);
#73637=ORIENTED_EDGE('',*,*,#52157,.T.);
#73638=ORIENTED_EDGE('',*,*,#52158,.T.);
#73639=ORIENTED_EDGE('',*,*,#52159,.T.);
#73640=ORIENTED_EDGE('',*,*,#52160,.T.);
#73641=ORIENTED_EDGE('',*,*,#52161,.T.);
#73642=ORIENTED_EDGE('',*,*,#52162,.T.);
#73643=ORIENTED_EDGE('',*,*,#52163,.T.);
#73644=ORIENTED_EDGE('',*,*,#52164,.T.);
#73645=ORIENTED_EDGE('',*,*,#52165,.T.);
#73646=ORIENTED_EDGE('',*,*,#52166,.T.);
#73647=ORIENTED_EDGE('',*,*,#52167,.T.);
#73648=ORIENTED_EDGE('',*,*,#52168,.T.);
#73649=ORIENTED_EDGE('',*,*,#52169,.T.);
#73650=ORIENTED_EDGE('',*,*,#52170,.T.);
#73651=ORIENTED_EDGE('',*,*,#52171,.T.);
#73652=ORIENTED_EDGE('',*,*,#52172,.T.);
#73653=ORIENTED_EDGE('',*,*,#52173,.T.);
#73654=ORIENTED_EDGE('',*,*,#52174,.T.);
#73655=ORIENTED_EDGE('',*,*,#52175,.T.);
#73656=ORIENTED_EDGE('',*,*,#52176,.T.);
#73657=ORIENTED_EDGE('',*,*,#52177,.T.);
#73658=ORIENTED_EDGE('',*,*,#52178,.T.);
#73659=ORIENTED_EDGE('',*,*,#52179,.T.);
#73660=ORIENTED_EDGE('',*,*,#52180,.T.);
#73661=ORIENTED_EDGE('',*,*,#52181,.T.);
#73662=ORIENTED_EDGE('',*,*,#52182,.T.);
#73663=ORIENTED_EDGE('',*,*,#52183,.T.);
#73664=ORIENTED_EDGE('',*,*,#52184,.T.);
#73665=ORIENTED_EDGE('',*,*,#52185,.T.);
#73666=ORIENTED_EDGE('',*,*,#52186,.T.);
#73667=ORIENTED_EDGE('',*,*,#52187,.T.);
#73668=ORIENTED_EDGE('',*,*,#52188,.T.);
#73669=ORIENTED_EDGE('',*,*,#52189,.T.);
#73670=ORIENTED_EDGE('',*,*,#52190,.T.);
#73671=ORIENTED_EDGE('',*,*,#52191,.T.);
#73672=ORIENTED_EDGE('',*,*,#52192,.T.);
#73673=ORIENTED_EDGE('',*,*,#52193,.T.);
#73674=ORIENTED_EDGE('',*,*,#52194,.T.);
#73675=ORIENTED_EDGE('',*,*,#52195,.T.);
#73676=ORIENTED_EDGE('',*,*,#52196,.T.);
#73677=ORIENTED_EDGE('',*,*,#52197,.T.);
#73678=ORIENTED_EDGE('',*,*,#52198,.T.);
#73679=ORIENTED_EDGE('',*,*,#52199,.T.);
#73680=ORIENTED_EDGE('',*,*,#52200,.T.);
#73681=ORIENTED_EDGE('',*,*,#52201,.T.);
#73682=ORIENTED_EDGE('',*,*,#52202,.T.);
#73683=ORIENTED_EDGE('',*,*,#52203,.T.);
#73684=ORIENTED_EDGE('',*,*,#52204,.T.);
#73685=ORIENTED_EDGE('',*,*,#52205,.T.);
#73686=ORIENTED_EDGE('',*,*,#52206,.T.);
#73687=ORIENTED_EDGE('',*,*,#52207,.T.);
#73688=ORIENTED_EDGE('',*,*,#52208,.T.);
#73689=ORIENTED_EDGE('',*,*,#52209,.T.);
#73690=ORIENTED_EDGE('',*,*,#52210,.T.);
#73691=ORIENTED_EDGE('',*,*,#52211,.T.);
#73692=ORIENTED_EDGE('',*,*,#52212,.T.);
#73693=ORIENTED_EDGE('',*,*,#52213,.T.);
#73694=ORIENTED_EDGE('',*,*,#52214,.T.);
#73695=ORIENTED_EDGE('',*,*,#52215,.T.);
#73696=ORIENTED_EDGE('',*,*,#52216,.T.);
#73697=ORIENTED_EDGE('',*,*,#52217,.T.);
#73698=ORIENTED_EDGE('',*,*,#52218,.T.);
#73699=ORIENTED_EDGE('',*,*,#52219,.T.);
#73700=ORIENTED_EDGE('',*,*,#52220,.T.);
#73701=ORIENTED_EDGE('',*,*,#52221,.T.);
#73702=ORIENTED_EDGE('',*,*,#52222,.T.);
#73703=ORIENTED_EDGE('',*,*,#52223,.T.);
#73704=ORIENTED_EDGE('',*,*,#52224,.T.);
#73705=ORIENTED_EDGE('',*,*,#52225,.T.);
#73706=ORIENTED_EDGE('',*,*,#52226,.T.);
#73707=ORIENTED_EDGE('',*,*,#52227,.T.);
#73708=ORIENTED_EDGE('',*,*,#52228,.T.);
#73709=ORIENTED_EDGE('',*,*,#52229,.T.);
#73710=ORIENTED_EDGE('',*,*,#52230,.T.);
#73711=ORIENTED_EDGE('',*,*,#52231,.T.);
#73712=ORIENTED_EDGE('',*,*,#52232,.T.);
#73713=ORIENTED_EDGE('',*,*,#52233,.T.);
#73714=ORIENTED_EDGE('',*,*,#52234,.T.);
#73715=ORIENTED_EDGE('',*,*,#52235,.T.);
#73716=ORIENTED_EDGE('',*,*,#52236,.T.);
#73717=ORIENTED_EDGE('',*,*,#52237,.T.);
#73718=ORIENTED_EDGE('',*,*,#52238,.T.);
#73719=ORIENTED_EDGE('',*,*,#52239,.T.);
#73720=ORIENTED_EDGE('',*,*,#52240,.T.);
#73721=ORIENTED_EDGE('',*,*,#52241,.T.);
#73722=ORIENTED_EDGE('',*,*,#52242,.T.);
#73723=ORIENTED_EDGE('',*,*,#52243,.T.);
#73724=ORIENTED_EDGE('',*,*,#52041,.T.);
#73725=ORIENTED_EDGE('',*,*,#52244,.T.);
#73726=ORIENTED_EDGE('',*,*,#52055,.T.);
#73727=ORIENTED_EDGE('',*,*,#52056,.T.);
#73728=ORIENTED_EDGE('',*,*,#52244,.F.);
#73729=ORIENTED_EDGE('',*,*,#52045,.T.);
#73730=ORIENTED_EDGE('',*,*,#52245,.T.);
#73731=ORIENTED_EDGE('',*,*,#52246,.T.);
#73732=ORIENTED_EDGE('',*,*,#52247,.T.);
#73733=ORIENTED_EDGE('',*,*,#52248,.T.);
#73734=ORIENTED_EDGE('',*,*,#52249,.T.);
#73735=ORIENTED_EDGE('',*,*,#52250,.T.);
#73736=ORIENTED_EDGE('',*,*,#52251,.T.);
#73737=ORIENTED_EDGE('',*,*,#52252,.T.);
#73738=ORIENTED_EDGE('',*,*,#52253,.T.);
#73739=ORIENTED_EDGE('',*,*,#52254,.T.);
#73740=ORIENTED_EDGE('',*,*,#52255,.T.);
#73741=ORIENTED_EDGE('',*,*,#52256,.T.);
#73742=ORIENTED_EDGE('',*,*,#52257,.T.);
#73743=ORIENTED_EDGE('',*,*,#52258,.T.);
#73744=ORIENTED_EDGE('',*,*,#52259,.T.);
#73745=ORIENTED_EDGE('',*,*,#52260,.T.);
#73746=ORIENTED_EDGE('',*,*,#52261,.T.);
#73747=ORIENTED_EDGE('',*,*,#52262,.T.);
#73748=ORIENTED_EDGE('',*,*,#52263,.T.);
#73749=ORIENTED_EDGE('',*,*,#52264,.T.);
#73750=ORIENTED_EDGE('',*,*,#52265,.T.);
#73751=ORIENTED_EDGE('',*,*,#52266,.T.);
#73752=ORIENTED_EDGE('',*,*,#52267,.T.);
#73753=ORIENTED_EDGE('',*,*,#52268,.T.);
#73754=ORIENTED_EDGE('',*,*,#52269,.T.);
#73755=ORIENTED_EDGE('',*,*,#52270,.T.);
#73756=ORIENTED_EDGE('',*,*,#52271,.T.);
#73757=ORIENTED_EDGE('',*,*,#52272,.T.);
#73758=ORIENTED_EDGE('',*,*,#52273,.T.);
#73759=ORIENTED_EDGE('',*,*,#52274,.T.);
#73760=ORIENTED_EDGE('',*,*,#52275,.T.);
#73761=ORIENTED_EDGE('',*,*,#52276,.T.);
#73762=ORIENTED_EDGE('',*,*,#52277,.T.);
#73763=ORIENTED_EDGE('',*,*,#52278,.T.);
#73764=ORIENTED_EDGE('',*,*,#52279,.T.);
#73765=ORIENTED_EDGE('',*,*,#52280,.T.);
#73766=ORIENTED_EDGE('',*,*,#52281,.T.);
#73767=ORIENTED_EDGE('',*,*,#52282,.T.);
#73768=ORIENTED_EDGE('',*,*,#52283,.T.);
#73769=ORIENTED_EDGE('',*,*,#52284,.T.);
#73770=ORIENTED_EDGE('',*,*,#52285,.T.);
#73771=ORIENTED_EDGE('',*,*,#52286,.T.);
#73772=ORIENTED_EDGE('',*,*,#52287,.T.);
#73773=ORIENTED_EDGE('',*,*,#52288,.T.);
#73774=ORIENTED_EDGE('',*,*,#52289,.T.);
#73775=ORIENTED_EDGE('',*,*,#52290,.T.);
#73776=ORIENTED_EDGE('',*,*,#52291,.T.);
#73777=ORIENTED_EDGE('',*,*,#52292,.T.);
#73778=ORIENTED_EDGE('',*,*,#52293,.T.);
#73779=ORIENTED_EDGE('',*,*,#52294,.T.);
#73780=ORIENTED_EDGE('',*,*,#52295,.T.);
#73781=ORIENTED_EDGE('',*,*,#52296,.T.);
#73782=ORIENTED_EDGE('',*,*,#52297,.T.);
#73783=ORIENTED_EDGE('',*,*,#52298,.T.);
#73784=ORIENTED_EDGE('',*,*,#52299,.T.);
#73785=ORIENTED_EDGE('',*,*,#52300,.T.);
#73786=ORIENTED_EDGE('',*,*,#52301,.T.);
#73787=ORIENTED_EDGE('',*,*,#52302,.T.);
#73788=ORIENTED_EDGE('',*,*,#52303,.T.);
#73789=ORIENTED_EDGE('',*,*,#52304,.T.);
#73790=ORIENTED_EDGE('',*,*,#52305,.T.);
#73791=ORIENTED_EDGE('',*,*,#52306,.T.);
#73792=ORIENTED_EDGE('',*,*,#52307,.T.);
#73793=ORIENTED_EDGE('',*,*,#52308,.T.);
#73794=ORIENTED_EDGE('',*,*,#52309,.T.);
#73795=ORIENTED_EDGE('',*,*,#52310,.T.);
#73796=ORIENTED_EDGE('',*,*,#52311,.T.);
#73797=ORIENTED_EDGE('',*,*,#52312,.T.);
#73798=ORIENTED_EDGE('',*,*,#52313,.T.);
#73799=ORIENTED_EDGE('',*,*,#52314,.T.);
#73800=ORIENTED_EDGE('',*,*,#52315,.T.);
#73801=ORIENTED_EDGE('',*,*,#52316,.T.);
#73802=ORIENTED_EDGE('',*,*,#52317,.T.);
#73803=ORIENTED_EDGE('',*,*,#52318,.T.);
#73804=ORIENTED_EDGE('',*,*,#52319,.T.);
#73805=ORIENTED_EDGE('',*,*,#52320,.T.);
#73806=ORIENTED_EDGE('',*,*,#52321,.T.);
#73807=ORIENTED_EDGE('',*,*,#52322,.T.);
#73808=ORIENTED_EDGE('',*,*,#52323,.T.);
#73809=ORIENTED_EDGE('',*,*,#52324,.T.);
#73810=ORIENTED_EDGE('',*,*,#52325,.T.);
#73811=ORIENTED_EDGE('',*,*,#52326,.T.);
#73812=ORIENTED_EDGE('',*,*,#52327,.T.);
#73813=ORIENTED_EDGE('',*,*,#52328,.T.);
#73814=ORIENTED_EDGE('',*,*,#52329,.T.);
#73815=ORIENTED_EDGE('',*,*,#52330,.T.);
#73816=ORIENTED_EDGE('',*,*,#52331,.T.);
#73817=ORIENTED_EDGE('',*,*,#52332,.T.);
#73818=ORIENTED_EDGE('',*,*,#52333,.T.);
#73819=ORIENTED_EDGE('',*,*,#52033,.T.);
#73820=ORIENTED_EDGE('',*,*,#52334,.T.);
#73821=ORIENTED_EDGE('',*,*,#52335,.T.);
#73822=ORIENTED_EDGE('',*,*,#52336,.T.);
#73823=ORIENTED_EDGE('',*,*,#52337,.T.);
#73824=ORIENTED_EDGE('',*,*,#52338,.T.);
#73825=ORIENTED_EDGE('',*,*,#52339,.T.);
#73826=ORIENTED_EDGE('',*,*,#52340,.T.);
#73827=ORIENTED_EDGE('',*,*,#52341,.T.);
#73828=ORIENTED_EDGE('',*,*,#52342,.T.);
#73829=ORIENTED_EDGE('',*,*,#52343,.T.);
#73830=ORIENTED_EDGE('',*,*,#52344,.T.);
#73831=ORIENTED_EDGE('',*,*,#52345,.T.);
#73832=ORIENTED_EDGE('',*,*,#52346,.T.);
#73833=ORIENTED_EDGE('',*,*,#52347,.T.);
#73834=ORIENTED_EDGE('',*,*,#52348,.T.);
#73835=ORIENTED_EDGE('',*,*,#52349,.T.);
#73836=ORIENTED_EDGE('',*,*,#52350,.T.);
#73837=ORIENTED_EDGE('',*,*,#52351,.T.);
#73838=ORIENTED_EDGE('',*,*,#52352,.T.);
#73839=ORIENTED_EDGE('',*,*,#52353,.T.);
#73840=ORIENTED_EDGE('',*,*,#52354,.T.);
#73841=ORIENTED_EDGE('',*,*,#52355,.T.);
#73842=ORIENTED_EDGE('',*,*,#52356,.T.);
#73843=ORIENTED_EDGE('',*,*,#52357,.T.);
#73844=ORIENTED_EDGE('',*,*,#52358,.T.);
#73845=ORIENTED_EDGE('',*,*,#52359,.T.);
#73846=ORIENTED_EDGE('',*,*,#52360,.T.);
#73847=ORIENTED_EDGE('',*,*,#52361,.T.);
#73848=ORIENTED_EDGE('',*,*,#52362,.T.);
#73849=ORIENTED_EDGE('',*,*,#52363,.T.);
#73850=ORIENTED_EDGE('',*,*,#52364,.T.);
#73851=ORIENTED_EDGE('',*,*,#52365,.T.);
#73852=ORIENTED_EDGE('',*,*,#52366,.T.);
#73853=ORIENTED_EDGE('',*,*,#52367,.T.);
#73854=ORIENTED_EDGE('',*,*,#52368,.T.);
#73855=ORIENTED_EDGE('',*,*,#52369,.T.);
#73856=ORIENTED_EDGE('',*,*,#52370,.T.);
#73857=ORIENTED_EDGE('',*,*,#52371,.T.);
#73858=ORIENTED_EDGE('',*,*,#52372,.T.);
#73859=ORIENTED_EDGE('',*,*,#52373,.T.);
#73860=ORIENTED_EDGE('',*,*,#52374,.T.);
#73861=ORIENTED_EDGE('',*,*,#52375,.T.);
#73862=ORIENTED_EDGE('',*,*,#52376,.T.);
#73863=ORIENTED_EDGE('',*,*,#52377,.T.);
#73864=ORIENTED_EDGE('',*,*,#52378,.T.);
#73865=ORIENTED_EDGE('',*,*,#52379,.T.);
#73866=ORIENTED_EDGE('',*,*,#52380,.T.);
#73867=ORIENTED_EDGE('',*,*,#52381,.T.);
#73868=ORIENTED_EDGE('',*,*,#52382,.T.);
#73869=ORIENTED_EDGE('',*,*,#52383,.T.);
#73870=ORIENTED_EDGE('',*,*,#52384,.T.);
#73871=ORIENTED_EDGE('',*,*,#52385,.T.);
#73872=ORIENTED_EDGE('',*,*,#52386,.T.);
#73873=ORIENTED_EDGE('',*,*,#52387,.T.);
#73874=ORIENTED_EDGE('',*,*,#52388,.T.);
#73875=ORIENTED_EDGE('',*,*,#52389,.T.);
#73876=ORIENTED_EDGE('',*,*,#52390,.T.);
#73877=ORIENTED_EDGE('',*,*,#52391,.T.);
#73878=ORIENTED_EDGE('',*,*,#52392,.T.);
#73879=ORIENTED_EDGE('',*,*,#52393,.T.);
#73880=ORIENTED_EDGE('',*,*,#52394,.T.);
#73881=ORIENTED_EDGE('',*,*,#52395,.T.);
#73882=ORIENTED_EDGE('',*,*,#52396,.T.);
#73883=ORIENTED_EDGE('',*,*,#52397,.T.);
#73884=ORIENTED_EDGE('',*,*,#52398,.T.);
#73885=ORIENTED_EDGE('',*,*,#52399,.T.);
#73886=ORIENTED_EDGE('',*,*,#52400,.T.);
#73887=ORIENTED_EDGE('',*,*,#52401,.T.);
#73888=ORIENTED_EDGE('',*,*,#52402,.T.);
#73889=ORIENTED_EDGE('',*,*,#52403,.T.);
#73890=ORIENTED_EDGE('',*,*,#52404,.T.);
#73891=ORIENTED_EDGE('',*,*,#52405,.T.);
#73892=ORIENTED_EDGE('',*,*,#52406,.T.);
#73893=ORIENTED_EDGE('',*,*,#52407,.T.);
#73894=ORIENTED_EDGE('',*,*,#52408,.T.);
#73895=ORIENTED_EDGE('',*,*,#52409,.T.);
#73896=ORIENTED_EDGE('',*,*,#52410,.T.);
#73897=ORIENTED_EDGE('',*,*,#52411,.T.);
#73898=ORIENTED_EDGE('',*,*,#52412,.T.);
#73899=ORIENTED_EDGE('',*,*,#52413,.T.);
#73900=ORIENTED_EDGE('',*,*,#52414,.T.);
#73901=ORIENTED_EDGE('',*,*,#52415,.T.);
#73902=ORIENTED_EDGE('',*,*,#52416,.T.);
#73903=ORIENTED_EDGE('',*,*,#52417,.T.);
#73904=ORIENTED_EDGE('',*,*,#52418,.T.);
#73905=ORIENTED_EDGE('',*,*,#52419,.T.);
#73906=ORIENTED_EDGE('',*,*,#52420,.T.);
#73907=ORIENTED_EDGE('',*,*,#52421,.T.);
#73908=ORIENTED_EDGE('',*,*,#52422,.T.);
#73909=ORIENTED_EDGE('',*,*,#52039,.T.);
#73910=ORIENTED_EDGE('',*,*,#52423,.T.);
#73911=ORIENTED_EDGE('',*,*,#52424,.T.);
#73912=ORIENTED_EDGE('',*,*,#52425,.T.);
#73913=ORIENTED_EDGE('',*,*,#52426,.T.);
#73914=ORIENTED_EDGE('',*,*,#52427,.T.);
#73915=ORIENTED_EDGE('',*,*,#52428,.T.);
#73916=ORIENTED_EDGE('',*,*,#52429,.T.);
#73917=ORIENTED_EDGE('',*,*,#52430,.T.);
#73918=ORIENTED_EDGE('',*,*,#52431,.T.);
#73919=ORIENTED_EDGE('',*,*,#52432,.T.);
#73920=ORIENTED_EDGE('',*,*,#52433,.T.);
#73921=ORIENTED_EDGE('',*,*,#52434,.T.);
#73922=ORIENTED_EDGE('',*,*,#52435,.T.);
#73923=ORIENTED_EDGE('',*,*,#52436,.T.);
#73924=ORIENTED_EDGE('',*,*,#52437,.T.);
#73925=ORIENTED_EDGE('',*,*,#52438,.T.);
#73926=ORIENTED_EDGE('',*,*,#52439,.T.);
#73927=ORIENTED_EDGE('',*,*,#52440,.T.);
#73928=ORIENTED_EDGE('',*,*,#52441,.T.);
#73929=ORIENTED_EDGE('',*,*,#52442,.T.);
#73930=ORIENTED_EDGE('',*,*,#52443,.T.);
#73931=ORIENTED_EDGE('',*,*,#52444,.T.);
#73932=ORIENTED_EDGE('',*,*,#52445,.T.);
#73933=ORIENTED_EDGE('',*,*,#52446,.T.);
#73934=ORIENTED_EDGE('',*,*,#52447,.T.);
#73935=ORIENTED_EDGE('',*,*,#52448,.T.);
#73936=ORIENTED_EDGE('',*,*,#52449,.T.);
#73937=ORIENTED_EDGE('',*,*,#52450,.T.);
#73938=ORIENTED_EDGE('',*,*,#52451,.T.);
#73939=ORIENTED_EDGE('',*,*,#52452,.T.);
#73940=ORIENTED_EDGE('',*,*,#52453,.T.);
#73941=ORIENTED_EDGE('',*,*,#52454,.T.);
#73942=ORIENTED_EDGE('',*,*,#52455,.T.);
#73943=ORIENTED_EDGE('',*,*,#52456,.T.);
#73944=ORIENTED_EDGE('',*,*,#52457,.T.);
#73945=ORIENTED_EDGE('',*,*,#52458,.T.);
#73946=ORIENTED_EDGE('',*,*,#52459,.T.);
#73947=ORIENTED_EDGE('',*,*,#52460,.T.);
#73948=ORIENTED_EDGE('',*,*,#52461,.T.);
#73949=ORIENTED_EDGE('',*,*,#52462,.T.);
#73950=ORIENTED_EDGE('',*,*,#52463,.T.);
#73951=ORIENTED_EDGE('',*,*,#52464,.T.);
#73952=ORIENTED_EDGE('',*,*,#52465,.T.);
#73953=ORIENTED_EDGE('',*,*,#52466,.T.);
#73954=ORIENTED_EDGE('',*,*,#52467,.T.);
#73955=ORIENTED_EDGE('',*,*,#52468,.T.);
#73956=ORIENTED_EDGE('',*,*,#52469,.T.);
#73957=ORIENTED_EDGE('',*,*,#52470,.T.);
#73958=ORIENTED_EDGE('',*,*,#52471,.T.);
#73959=ORIENTED_EDGE('',*,*,#52472,.T.);
#73960=ORIENTED_EDGE('',*,*,#52473,.T.);
#73961=ORIENTED_EDGE('',*,*,#52474,.T.);
#73962=ORIENTED_EDGE('',*,*,#52475,.T.);
#73963=ORIENTED_EDGE('',*,*,#52476,.T.);
#73964=ORIENTED_EDGE('',*,*,#52477,.T.);
#73965=ORIENTED_EDGE('',*,*,#52478,.T.);
#73966=ORIENTED_EDGE('',*,*,#52479,.T.);
#73967=ORIENTED_EDGE('',*,*,#52480,.T.);
#73968=ORIENTED_EDGE('',*,*,#52481,.T.);
#73969=ORIENTED_EDGE('',*,*,#52482,.T.);
#73970=ORIENTED_EDGE('',*,*,#52483,.T.);
#73971=ORIENTED_EDGE('',*,*,#52484,.T.);
#73972=ORIENTED_EDGE('',*,*,#52485,.T.);
#73973=ORIENTED_EDGE('',*,*,#52486,.T.);
#73974=ORIENTED_EDGE('',*,*,#52487,.T.);
#73975=ORIENTED_EDGE('',*,*,#52488,.T.);
#73976=ORIENTED_EDGE('',*,*,#52489,.T.);
#73977=ORIENTED_EDGE('',*,*,#52490,.T.);
#73978=ORIENTED_EDGE('',*,*,#52491,.T.);
#73979=ORIENTED_EDGE('',*,*,#52492,.T.);
#73980=ORIENTED_EDGE('',*,*,#52493,.T.);
#73981=ORIENTED_EDGE('',*,*,#52494,.T.);
#73982=ORIENTED_EDGE('',*,*,#52495,.T.);
#73983=ORIENTED_EDGE('',*,*,#52496,.T.);
#73984=ORIENTED_EDGE('',*,*,#52497,.T.);
#73985=ORIENTED_EDGE('',*,*,#52498,.T.);
#73986=ORIENTED_EDGE('',*,*,#52499,.T.);
#73987=ORIENTED_EDGE('',*,*,#52500,.T.);
#73988=ORIENTED_EDGE('',*,*,#52501,.T.);
#73989=ORIENTED_EDGE('',*,*,#52502,.T.);
#73990=ORIENTED_EDGE('',*,*,#52503,.T.);
#73991=ORIENTED_EDGE('',*,*,#52504,.T.);
#73992=ORIENTED_EDGE('',*,*,#52505,.T.);
#73993=ORIENTED_EDGE('',*,*,#52506,.T.);
#73994=ORIENTED_EDGE('',*,*,#52507,.T.);
#73995=ORIENTED_EDGE('',*,*,#52508,.T.);
#73996=ORIENTED_EDGE('',*,*,#52509,.T.);
#73997=ORIENTED_EDGE('',*,*,#52510,.T.);
#73998=ORIENTED_EDGE('',*,*,#52511,.T.);
#73999=ORIENTED_EDGE('',*,*,#52512,.T.);
#74000=ORIENTED_EDGE('',*,*,#52513,.T.);
#74001=ORIENTED_EDGE('',*,*,#52514,.T.);
#74002=ORIENTED_EDGE('',*,*,#52515,.T.);
#74003=ORIENTED_EDGE('',*,*,#52516,.T.);
#74004=ORIENTED_EDGE('',*,*,#52517,.T.);
#74005=ORIENTED_EDGE('',*,*,#52518,.T.);
#74006=ORIENTED_EDGE('',*,*,#52519,.T.);
#74007=ORIENTED_EDGE('',*,*,#52520,.T.);
#74008=ORIENTED_EDGE('',*,*,#52521,.T.);
#74009=ORIENTED_EDGE('',*,*,#52522,.T.);
#74010=ORIENTED_EDGE('',*,*,#52523,.T.);
#74011=ORIENTED_EDGE('',*,*,#52524,.T.);
#74012=ORIENTED_EDGE('',*,*,#52525,.T.);
#74013=ORIENTED_EDGE('',*,*,#52526,.T.);
#74014=ORIENTED_EDGE('',*,*,#52527,.T.);
#74015=ORIENTED_EDGE('',*,*,#52528,.T.);
#74016=ORIENTED_EDGE('',*,*,#52529,.T.);
#74017=ORIENTED_EDGE('',*,*,#52530,.T.);
#74018=ORIENTED_EDGE('',*,*,#52531,.T.);
#74019=ORIENTED_EDGE('',*,*,#52532,.T.);
#74020=ORIENTED_EDGE('',*,*,#52533,.T.);
#74021=ORIENTED_EDGE('',*,*,#52534,.T.);
#74022=ORIENTED_EDGE('',*,*,#52535,.T.);
#74023=ORIENTED_EDGE('',*,*,#52536,.T.);
#74024=ORIENTED_EDGE('',*,*,#52537,.T.);
#74025=ORIENTED_EDGE('',*,*,#52538,.T.);
#74026=ORIENTED_EDGE('',*,*,#52539,.T.);
#74027=ORIENTED_EDGE('',*,*,#52540,.T.);
#74028=ORIENTED_EDGE('',*,*,#52541,.T.);
#74029=ORIENTED_EDGE('',*,*,#52542,.T.);
#74030=ORIENTED_EDGE('',*,*,#52543,.T.);
#74031=ORIENTED_EDGE('',*,*,#52544,.T.);
#74032=ORIENTED_EDGE('',*,*,#52545,.T.);
#74033=ORIENTED_EDGE('',*,*,#52546,.T.);
#74034=ORIENTED_EDGE('',*,*,#52547,.T.);
#74035=ORIENTED_EDGE('',*,*,#52548,.T.);
#74036=ORIENTED_EDGE('',*,*,#52549,.T.);
#74037=ORIENTED_EDGE('',*,*,#52550,.T.);
#74038=ORIENTED_EDGE('',*,*,#52551,.T.);
#74039=ORIENTED_EDGE('',*,*,#52552,.T.);
#74040=ORIENTED_EDGE('',*,*,#52553,.T.);
#74041=ORIENTED_EDGE('',*,*,#52554,.T.);
#74042=ORIENTED_EDGE('',*,*,#52555,.T.);
#74043=ORIENTED_EDGE('',*,*,#52556,.T.);
#74044=ORIENTED_EDGE('',*,*,#52557,.T.);
#74045=ORIENTED_EDGE('',*,*,#52558,.T.);
#74046=ORIENTED_EDGE('',*,*,#52559,.T.);
#74047=ORIENTED_EDGE('',*,*,#52560,.T.);
#74048=ORIENTED_EDGE('',*,*,#52561,.T.);
#74049=ORIENTED_EDGE('',*,*,#52562,.T.);
#74050=ORIENTED_EDGE('',*,*,#52563,.T.);
#74051=ORIENTED_EDGE('',*,*,#52564,.T.);
#74052=ORIENTED_EDGE('',*,*,#52565,.T.);
#74053=ORIENTED_EDGE('',*,*,#52566,.T.);
#74054=ORIENTED_EDGE('',*,*,#52567,.T.);
#74055=ORIENTED_EDGE('',*,*,#52568,.T.);
#74056=ORIENTED_EDGE('',*,*,#52569,.T.);
#74057=ORIENTED_EDGE('',*,*,#52570,.T.);
#74058=ORIENTED_EDGE('',*,*,#52571,.T.);
#74059=ORIENTED_EDGE('',*,*,#52572,.T.);
#74060=ORIENTED_EDGE('',*,*,#52573,.T.);
#74061=ORIENTED_EDGE('',*,*,#52574,.T.);
#74062=ORIENTED_EDGE('',*,*,#52575,.T.);
#74063=ORIENTED_EDGE('',*,*,#52576,.T.);
#74064=ORIENTED_EDGE('',*,*,#52577,.T.);
#74065=ORIENTED_EDGE('',*,*,#52578,.T.);
#74066=ORIENTED_EDGE('',*,*,#52579,.T.);
#74067=ORIENTED_EDGE('',*,*,#52580,.T.);
#74068=ORIENTED_EDGE('',*,*,#52581,.T.);
#74069=ORIENTED_EDGE('',*,*,#52582,.T.);
#74070=ORIENTED_EDGE('',*,*,#52583,.T.);
#74071=ORIENTED_EDGE('',*,*,#52584,.T.);
#74072=ORIENTED_EDGE('',*,*,#52585,.T.);
#74073=ORIENTED_EDGE('',*,*,#52586,.T.);
#74074=ORIENTED_EDGE('',*,*,#52587,.T.);
#74075=ORIENTED_EDGE('',*,*,#52588,.T.);
#74076=ORIENTED_EDGE('',*,*,#52589,.T.);
#74077=ORIENTED_EDGE('',*,*,#52590,.T.);
#74078=ORIENTED_EDGE('',*,*,#52591,.T.);
#74079=ORIENTED_EDGE('',*,*,#52592,.T.);
#74080=ORIENTED_EDGE('',*,*,#52593,.T.);
#74081=ORIENTED_EDGE('',*,*,#52594,.T.);
#74082=ORIENTED_EDGE('',*,*,#52595,.T.);
#74083=ORIENTED_EDGE('',*,*,#52596,.T.);
#74084=ORIENTED_EDGE('',*,*,#52597,.T.);
#74085=ORIENTED_EDGE('',*,*,#52598,.T.);
#74086=ORIENTED_EDGE('',*,*,#52599,.T.);
#74087=ORIENTED_EDGE('',*,*,#52600,.T.);
#74088=ORIENTED_EDGE('',*,*,#52601,.T.);
#74089=ORIENTED_EDGE('',*,*,#52602,.T.);
#74090=ORIENTED_EDGE('',*,*,#52603,.T.);
#74091=ORIENTED_EDGE('',*,*,#52050,.T.);
#74092=ORIENTED_EDGE('',*,*,#52603,.F.);
#74093=ORIENTED_EDGE('',*,*,#52604,.T.);
#74094=ORIENTED_EDGE('',*,*,#52605,.T.);
#74095=ORIENTED_EDGE('',*,*,#52606,.T.);
#74096=ORIENTED_EDGE('',*,*,#52607,.T.);
#74097=ORIENTED_EDGE('',*,*,#52608,.T.);
#74098=ORIENTED_EDGE('',*,*,#52609,.T.);
#74099=ORIENTED_EDGE('',*,*,#52610,.T.);
#74100=ORIENTED_EDGE('',*,*,#52611,.T.);
#74101=ORIENTED_EDGE('',*,*,#52612,.T.);
#74102=ORIENTED_EDGE('',*,*,#52613,.T.);
#74103=ORIENTED_EDGE('',*,*,#52614,.T.);
#74104=ORIENTED_EDGE('',*,*,#52615,.T.);
#74105=ORIENTED_EDGE('',*,*,#52616,.T.);
#74106=ORIENTED_EDGE('',*,*,#52617,.T.);
#74107=ORIENTED_EDGE('',*,*,#52618,.T.);
#74108=ORIENTED_EDGE('',*,*,#52619,.T.);
#74109=ORIENTED_EDGE('',*,*,#52620,.T.);
#74110=ORIENTED_EDGE('',*,*,#52621,.T.);
#74111=ORIENTED_EDGE('',*,*,#52622,.T.);
#74112=ORIENTED_EDGE('',*,*,#52623,.T.);
#74113=ORIENTED_EDGE('',*,*,#52624,.T.);
#74114=ORIENTED_EDGE('',*,*,#52625,.T.);
#74115=ORIENTED_EDGE('',*,*,#52626,.T.);
#74116=ORIENTED_EDGE('',*,*,#52627,.T.);
#74117=ORIENTED_EDGE('',*,*,#52628,.T.);
#74118=ORIENTED_EDGE('',*,*,#52629,.T.);
#74119=ORIENTED_EDGE('',*,*,#52630,.T.);
#74120=ORIENTED_EDGE('',*,*,#52631,.T.);
#74121=ORIENTED_EDGE('',*,*,#52632,.T.);
#74122=ORIENTED_EDGE('',*,*,#52633,.T.);
#74123=ORIENTED_EDGE('',*,*,#52634,.T.);
#74124=ORIENTED_EDGE('',*,*,#52635,.T.);
#74125=ORIENTED_EDGE('',*,*,#52636,.T.);
#74126=ORIENTED_EDGE('',*,*,#52637,.T.);
#74127=ORIENTED_EDGE('',*,*,#52638,.T.);
#74128=ORIENTED_EDGE('',*,*,#52639,.T.);
#74129=ORIENTED_EDGE('',*,*,#52640,.T.);
#74130=ORIENTED_EDGE('',*,*,#52641,.T.);
#74131=ORIENTED_EDGE('',*,*,#52642,.T.);
#74132=ORIENTED_EDGE('',*,*,#52643,.T.);
#74133=ORIENTED_EDGE('',*,*,#52644,.T.);
#74134=ORIENTED_EDGE('',*,*,#52645,.T.);
#74135=ORIENTED_EDGE('',*,*,#52646,.T.);
#74136=ORIENTED_EDGE('',*,*,#52647,.T.);
#74137=ORIENTED_EDGE('',*,*,#52648,.T.);
#74138=ORIENTED_EDGE('',*,*,#52649,.T.);
#74139=ORIENTED_EDGE('',*,*,#52650,.T.);
#74140=ORIENTED_EDGE('',*,*,#52651,.T.);
#74141=ORIENTED_EDGE('',*,*,#52652,.T.);
#74142=ORIENTED_EDGE('',*,*,#52653,.T.);
#74143=ORIENTED_EDGE('',*,*,#52654,.T.);
#74144=ORIENTED_EDGE('',*,*,#52655,.T.);
#74145=ORIENTED_EDGE('',*,*,#52656,.T.);
#74146=ORIENTED_EDGE('',*,*,#52657,.T.);
#74147=ORIENTED_EDGE('',*,*,#52658,.T.);
#74148=ORIENTED_EDGE('',*,*,#52659,.T.);
#74149=ORIENTED_EDGE('',*,*,#52660,.T.);
#74150=ORIENTED_EDGE('',*,*,#52661,.T.);
#74151=ORIENTED_EDGE('',*,*,#52662,.T.);
#74152=ORIENTED_EDGE('',*,*,#52663,.T.);
#74153=ORIENTED_EDGE('',*,*,#52664,.T.);
#74154=ORIENTED_EDGE('',*,*,#52665,.T.);
#74155=ORIENTED_EDGE('',*,*,#52666,.T.);
#74156=ORIENTED_EDGE('',*,*,#52667,.T.);
#74157=ORIENTED_EDGE('',*,*,#52668,.T.);
#74158=ORIENTED_EDGE('',*,*,#52669,.T.);
#74159=ORIENTED_EDGE('',*,*,#52670,.T.);
#74160=ORIENTED_EDGE('',*,*,#52671,.T.);
#74161=ORIENTED_EDGE('',*,*,#52672,.T.);
#74162=ORIENTED_EDGE('',*,*,#52673,.T.);
#74163=ORIENTED_EDGE('',*,*,#52674,.T.);
#74164=ORIENTED_EDGE('',*,*,#52675,.T.);
#74165=ORIENTED_EDGE('',*,*,#52676,.T.);
#74166=ORIENTED_EDGE('',*,*,#52677,.T.);
#74167=ORIENTED_EDGE('',*,*,#52678,.T.);
#74168=ORIENTED_EDGE('',*,*,#52679,.T.);
#74169=ORIENTED_EDGE('',*,*,#52680,.T.);
#74170=ORIENTED_EDGE('',*,*,#52681,.T.);
#74171=ORIENTED_EDGE('',*,*,#52682,.T.);
#74172=ORIENTED_EDGE('',*,*,#52683,.T.);
#74173=ORIENTED_EDGE('',*,*,#52684,.T.);
#74174=ORIENTED_EDGE('',*,*,#52685,.T.);
#74175=ORIENTED_EDGE('',*,*,#52686,.T.);
#74176=ORIENTED_EDGE('',*,*,#52687,.T.);
#74177=ORIENTED_EDGE('',*,*,#52688,.T.);
#74178=ORIENTED_EDGE('',*,*,#52689,.T.);
#74179=ORIENTED_EDGE('',*,*,#52690,.T.);
#74180=ORIENTED_EDGE('',*,*,#52691,.T.);
#74181=ORIENTED_EDGE('',*,*,#52692,.T.);
#74182=ORIENTED_EDGE('',*,*,#52693,.T.);
#74183=ORIENTED_EDGE('',*,*,#52031,.T.);
#74184=ORIENTED_EDGE('',*,*,#52694,.T.);
#74185=ORIENTED_EDGE('',*,*,#52695,.T.);
#74186=ORIENTED_EDGE('',*,*,#52696,.T.);
#74187=ORIENTED_EDGE('',*,*,#52697,.T.);
#74188=ORIENTED_EDGE('',*,*,#52698,.T.);
#74189=ORIENTED_EDGE('',*,*,#52699,.T.);
#74190=ORIENTED_EDGE('',*,*,#52700,.T.);
#74191=ORIENTED_EDGE('',*,*,#52701,.T.);
#74192=ORIENTED_EDGE('',*,*,#52702,.T.);
#74193=ORIENTED_EDGE('',*,*,#52703,.T.);
#74194=ORIENTED_EDGE('',*,*,#52704,.T.);
#74195=ORIENTED_EDGE('',*,*,#52705,.T.);
#74196=ORIENTED_EDGE('',*,*,#52706,.T.);
#74197=ORIENTED_EDGE('',*,*,#52707,.T.);
#74198=ORIENTED_EDGE('',*,*,#52708,.T.);
#74199=ORIENTED_EDGE('',*,*,#52709,.T.);
#74200=ORIENTED_EDGE('',*,*,#52710,.T.);
#74201=ORIENTED_EDGE('',*,*,#52711,.T.);
#74202=ORIENTED_EDGE('',*,*,#52712,.T.);
#74203=ORIENTED_EDGE('',*,*,#52713,.T.);
#74204=ORIENTED_EDGE('',*,*,#52714,.T.);
#74205=ORIENTED_EDGE('',*,*,#52715,.T.);
#74206=ORIENTED_EDGE('',*,*,#52716,.T.);
#74207=ORIENTED_EDGE('',*,*,#52717,.T.);
#74208=ORIENTED_EDGE('',*,*,#52718,.T.);
#74209=ORIENTED_EDGE('',*,*,#52719,.T.);
#74210=ORIENTED_EDGE('',*,*,#52720,.T.);
#74211=ORIENTED_EDGE('',*,*,#52721,.T.);
#74212=ORIENTED_EDGE('',*,*,#52722,.T.);
#74213=ORIENTED_EDGE('',*,*,#52723,.T.);
#74214=ORIENTED_EDGE('',*,*,#52724,.T.);
#74215=ORIENTED_EDGE('',*,*,#52725,.T.);
#74216=ORIENTED_EDGE('',*,*,#52726,.T.);
#74217=ORIENTED_EDGE('',*,*,#52727,.T.);
#74218=ORIENTED_EDGE('',*,*,#52728,.T.);
#74219=ORIENTED_EDGE('',*,*,#52729,.T.);
#74220=ORIENTED_EDGE('',*,*,#52730,.T.);
#74221=ORIENTED_EDGE('',*,*,#52731,.T.);
#74222=ORIENTED_EDGE('',*,*,#52732,.T.);
#74223=ORIENTED_EDGE('',*,*,#52733,.T.);
#74224=ORIENTED_EDGE('',*,*,#52734,.T.);
#74225=ORIENTED_EDGE('',*,*,#52735,.T.);
#74226=ORIENTED_EDGE('',*,*,#52736,.T.);
#74227=ORIENTED_EDGE('',*,*,#52737,.T.);
#74228=ORIENTED_EDGE('',*,*,#52738,.T.);
#74229=ORIENTED_EDGE('',*,*,#52739,.T.);
#74230=ORIENTED_EDGE('',*,*,#52740,.T.);
#74231=ORIENTED_EDGE('',*,*,#52741,.T.);
#74232=ORIENTED_EDGE('',*,*,#52742,.T.);
#74233=ORIENTED_EDGE('',*,*,#52743,.T.);
#74234=ORIENTED_EDGE('',*,*,#52744,.T.);
#74235=ORIENTED_EDGE('',*,*,#52745,.T.);
#74236=ORIENTED_EDGE('',*,*,#52746,.T.);
#74237=ORIENTED_EDGE('',*,*,#52747,.T.);
#74238=ORIENTED_EDGE('',*,*,#52748,.T.);
#74239=ORIENTED_EDGE('',*,*,#52749,.T.);
#74240=ORIENTED_EDGE('',*,*,#52750,.T.);
#74241=ORIENTED_EDGE('',*,*,#52751,.T.);
#74242=ORIENTED_EDGE('',*,*,#52752,.T.);
#74243=ORIENTED_EDGE('',*,*,#52753,.T.);
#74244=ORIENTED_EDGE('',*,*,#52754,.T.);
#74245=ORIENTED_EDGE('',*,*,#52755,.T.);
#74246=ORIENTED_EDGE('',*,*,#52756,.T.);
#74247=ORIENTED_EDGE('',*,*,#52757,.T.);
#74248=ORIENTED_EDGE('',*,*,#52758,.T.);
#74249=ORIENTED_EDGE('',*,*,#52759,.T.);
#74250=ORIENTED_EDGE('',*,*,#52760,.T.);
#74251=ORIENTED_EDGE('',*,*,#52761,.T.);
#74252=ORIENTED_EDGE('',*,*,#52762,.T.);
#74253=ORIENTED_EDGE('',*,*,#52763,.T.);
#74254=ORIENTED_EDGE('',*,*,#52764,.T.);
#74255=ORIENTED_EDGE('',*,*,#52765,.T.);
#74256=ORIENTED_EDGE('',*,*,#52766,.T.);
#74257=ORIENTED_EDGE('',*,*,#52767,.T.);
#74258=ORIENTED_EDGE('',*,*,#52768,.T.);
#74259=ORIENTED_EDGE('',*,*,#52769,.T.);
#74260=ORIENTED_EDGE('',*,*,#52770,.T.);
#74261=ORIENTED_EDGE('',*,*,#52771,.T.);
#74262=ORIENTED_EDGE('',*,*,#52772,.T.);
#74263=ORIENTED_EDGE('',*,*,#52773,.T.);
#74264=ORIENTED_EDGE('',*,*,#52774,.T.);
#74265=ORIENTED_EDGE('',*,*,#52775,.T.);
#74266=ORIENTED_EDGE('',*,*,#52776,.T.);
#74267=ORIENTED_EDGE('',*,*,#52777,.T.);
#74268=ORIENTED_EDGE('',*,*,#52778,.T.);
#74269=ORIENTED_EDGE('',*,*,#52779,.T.);
#74270=ORIENTED_EDGE('',*,*,#52780,.T.);
#74271=ORIENTED_EDGE('',*,*,#52781,.T.);
#74272=ORIENTED_EDGE('',*,*,#52782,.T.);
#74273=ORIENTED_EDGE('',*,*,#52783,.T.);
#74274=ORIENTED_EDGE('',*,*,#52784,.T.);
#74275=ORIENTED_EDGE('',*,*,#52048,.T.);
#74276=ORIENTED_EDGE('',*,*,#52049,.T.);
#74277=ORIENTED_EDGE('',*,*,#52784,.F.);
#74278=ORIENTED_EDGE('',*,*,#52785,.T.);
#74279=ORIENTED_EDGE('',*,*,#52783,.F.);
#74280=ORIENTED_EDGE('',*,*,#52786,.T.);
#74281=ORIENTED_EDGE('',*,*,#52787,.T.);
#74282=ORIENTED_EDGE('',*,*,#52786,.F.);
#74283=ORIENTED_EDGE('',*,*,#52785,.F.);
#74284=ORIENTED_EDGE('',*,*,#52788,.F.);
#74285=ORIENTED_EDGE('',*,*,#52789,.T.);
#74286=ORIENTED_EDGE('',*,*,#52790,.T.);
#74287=ORIENTED_EDGE('',*,*,#52791,.T.);
#74288=ORIENTED_EDGE('',*,*,#52792,.F.);
#74289=ORIENTED_EDGE('',*,*,#52793,.F.);
#74290=ORIENTED_EDGE('',*,*,#52794,.T.);
#74291=ORIENTED_EDGE('',*,*,#52795,.T.);
#74292=ORIENTED_EDGE('',*,*,#52793,.T.);
#74293=ORIENTED_EDGE('',*,*,#52796,.T.);
#74294=ORIENTED_EDGE('',*,*,#52797,.T.);
#74295=ORIENTED_EDGE('',*,*,#52798,.T.);
#74296=ORIENTED_EDGE('',*,*,#52799,.T.);
#74297=ORIENTED_EDGE('',*,*,#52800,.T.);
#74298=ORIENTED_EDGE('',*,*,#52801,.F.);
#74299=ORIENTED_EDGE('',*,*,#52802,.T.);
#74300=ORIENTED_EDGE('',*,*,#52803,.T.);
#74301=ORIENTED_EDGE('',*,*,#52804,.T.);
#74302=ORIENTED_EDGE('',*,*,#52805,.F.);
#74303=ORIENTED_EDGE('',*,*,#52806,.F.);
#74304=ORIENTED_EDGE('',*,*,#52807,.T.);
#74305=ORIENTED_EDGE('',*,*,#52808,.T.);
#74306=ORIENTED_EDGE('',*,*,#52806,.T.);
#74307=ORIENTED_EDGE('',*,*,#52809,.T.);
#74308=ORIENTED_EDGE('',*,*,#52790,.F.);
#74309=ORIENTED_EDGE('',*,*,#52810,.T.);
#74310=ORIENTED_EDGE('',*,*,#52607,.F.);
#74311=ORIENTED_EDGE('',*,*,#52811,.T.);
#74312=ORIENTED_EDGE('',*,*,#52420,.F.);
#74313=ORIENTED_EDGE('',*,*,#52812,.T.);
#74314=ORIENTED_EDGE('',*,*,#52807,.F.);
#74315=ORIENTED_EDGE('',*,*,#52813,.T.);
#74316=ORIENTED_EDGE('',*,*,#52803,.F.);
#74317=ORIENTED_EDGE('',*,*,#52814,.T.);
#74318=ORIENTED_EDGE('',*,*,#52797,.F.);
#74319=ORIENTED_EDGE('',*,*,#52815,.T.);
#74320=ORIENTED_EDGE('',*,*,#52799,.F.);
#74321=ORIENTED_EDGE('',*,*,#52816,.T.);
#74322=ORIENTED_EDGE('',*,*,#52794,.F.);
#74323=ORIENTED_EDGE('',*,*,#52817,.T.);
#74324=ORIENTED_EDGE('',*,*,#52818,.T.);
#74325=ORIENTED_EDGE('',*,*,#52819,.T.);
#74326=ORIENTED_EDGE('',*,*,#52820,.F.);
#74327=ORIENTED_EDGE('',*,*,#52821,.F.);
#74328=ORIENTED_EDGE('',*,*,#52822,.F.);
#74329=ORIENTED_EDGE('',*,*,#52823,.T.);
#74330=ORIENTED_EDGE('',*,*,#52821,.T.);
#74331=ORIENTED_EDGE('',*,*,#52824,.T.);
#74332=ORIENTED_EDGE('',*,*,#52825,.T.);
#74333=ORIENTED_EDGE('',*,*,#52826,.T.);
#74334=ORIENTED_EDGE('',*,*,#52827,.T.);
#74335=ORIENTED_EDGE('',*,*,#52828,.T.);
#74336=ORIENTED_EDGE('',*,*,#52829,.T.);
#74337=ORIENTED_EDGE('',*,*,#52830,.T.);
#74338=ORIENTED_EDGE('',*,*,#52831,.T.);
#74339=ORIENTED_EDGE('',*,*,#52832,.T.);
#74340=ORIENTED_EDGE('',*,*,#52833,.F.);
#74341=ORIENTED_EDGE('',*,*,#52834,.F.);
#74342=ORIENTED_EDGE('',*,*,#52835,.F.);
#74343=ORIENTED_EDGE('',*,*,#52836,.T.);
#74344=ORIENTED_EDGE('',*,*,#52834,.T.);
#74345=ORIENTED_EDGE('',*,*,#52837,.T.);
#74346=ORIENTED_EDGE('',*,*,#52838,.T.);
#74347=ORIENTED_EDGE('',*,*,#52839,.T.);
#74348=ORIENTED_EDGE('',*,*,#52613,.F.);
#74349=ORIENTED_EDGE('',*,*,#52840,.T.);
#74350=ORIENTED_EDGE('',*,*,#52818,.F.);
#74351=ORIENTED_EDGE('',*,*,#52841,.T.);
#74352=ORIENTED_EDGE('',*,*,#52838,.F.);
#74353=ORIENTED_EDGE('',*,*,#52842,.T.);
#74354=ORIENTED_EDGE('',*,*,#52414,.F.);
#74355=ORIENTED_EDGE('',*,*,#52843,.T.);
#74356=ORIENTED_EDGE('',*,*,#52829,.F.);
#74357=ORIENTED_EDGE('',*,*,#52844,.T.);
#74358=ORIENTED_EDGE('',*,*,#52831,.F.);
#74359=ORIENTED_EDGE('',*,*,#52845,.T.);
#74360=ORIENTED_EDGE('',*,*,#52825,.F.);
#74361=ORIENTED_EDGE('',*,*,#52846,.T.);
#74362=ORIENTED_EDGE('',*,*,#52827,.F.);
#74363=ORIENTED_EDGE('',*,*,#52847,.T.);
#74364=ORIENTED_EDGE('',*,*,#52848,.T.);
#74365=ORIENTED_EDGE('',*,*,#52849,.T.);
#74366=ORIENTED_EDGE('',*,*,#52850,.F.);
#74367=ORIENTED_EDGE('',*,*,#52851,.F.);
#74368=ORIENTED_EDGE('',*,*,#52852,.F.);
#74369=ORIENTED_EDGE('',*,*,#52853,.T.);
#74370=ORIENTED_EDGE('',*,*,#52851,.T.);
#74371=ORIENTED_EDGE('',*,*,#52854,.T.);
#74372=ORIENTED_EDGE('',*,*,#52855,.T.);
#74373=ORIENTED_EDGE('',*,*,#52856,.T.);
#74374=ORIENTED_EDGE('',*,*,#52857,.T.);
#74375=ORIENTED_EDGE('',*,*,#52858,.T.);
#74376=ORIENTED_EDGE('',*,*,#52859,.T.);
#74377=ORIENTED_EDGE('',*,*,#52860,.T.);
#74378=ORIENTED_EDGE('',*,*,#52861,.T.);
#74379=ORIENTED_EDGE('',*,*,#52862,.T.);
#74380=ORIENTED_EDGE('',*,*,#52863,.F.);
#74381=ORIENTED_EDGE('',*,*,#52864,.F.);
#74382=ORIENTED_EDGE('',*,*,#52865,.F.);
#74383=ORIENTED_EDGE('',*,*,#52866,.T.);
#74384=ORIENTED_EDGE('',*,*,#52864,.T.);
#74385=ORIENTED_EDGE('',*,*,#52867,.T.);
#74386=ORIENTED_EDGE('',*,*,#52868,.T.);
#74387=ORIENTED_EDGE('',*,*,#52869,.T.);
#74388=ORIENTED_EDGE('',*,*,#52619,.F.);
#74389=ORIENTED_EDGE('',*,*,#52870,.T.);
#74390=ORIENTED_EDGE('',*,*,#52848,.F.);
#74391=ORIENTED_EDGE('',*,*,#52871,.T.);
#74392=ORIENTED_EDGE('',*,*,#52868,.F.);
#74393=ORIENTED_EDGE('',*,*,#52872,.T.);
#74394=ORIENTED_EDGE('',*,*,#52408,.F.);
#74395=ORIENTED_EDGE('',*,*,#52873,.T.);
#74396=ORIENTED_EDGE('',*,*,#52859,.F.);
#74397=ORIENTED_EDGE('',*,*,#52874,.T.);
#74398=ORIENTED_EDGE('',*,*,#52861,.F.);
#74399=ORIENTED_EDGE('',*,*,#52875,.T.);
#74400=ORIENTED_EDGE('',*,*,#52855,.F.);
#74401=ORIENTED_EDGE('',*,*,#52876,.T.);
#74402=ORIENTED_EDGE('',*,*,#52857,.F.);
#74403=ORIENTED_EDGE('',*,*,#52877,.T.);
#74404=ORIENTED_EDGE('',*,*,#52878,.T.);
#74405=ORIENTED_EDGE('',*,*,#52879,.T.);
#74406=ORIENTED_EDGE('',*,*,#52880,.F.);
#74407=ORIENTED_EDGE('',*,*,#52881,.F.);
#74408=ORIENTED_EDGE('',*,*,#52882,.F.);
#74409=ORIENTED_EDGE('',*,*,#52883,.T.);
#74410=ORIENTED_EDGE('',*,*,#52881,.T.);
#74411=ORIENTED_EDGE('',*,*,#52884,.T.);
#74412=ORIENTED_EDGE('',*,*,#52885,.T.);
#74413=ORIENTED_EDGE('',*,*,#52886,.T.);
#74414=ORIENTED_EDGE('',*,*,#52887,.T.);
#74415=ORIENTED_EDGE('',*,*,#52888,.T.);
#74416=ORIENTED_EDGE('',*,*,#52889,.T.);
#74417=ORIENTED_EDGE('',*,*,#52890,.T.);
#74418=ORIENTED_EDGE('',*,*,#52891,.T.);
#74419=ORIENTED_EDGE('',*,*,#52892,.T.);
#74420=ORIENTED_EDGE('',*,*,#52893,.F.);
#74421=ORIENTED_EDGE('',*,*,#52894,.F.);
#74422=ORIENTED_EDGE('',*,*,#52895,.F.);
#74423=ORIENTED_EDGE('',*,*,#52896,.T.);
#74424=ORIENTED_EDGE('',*,*,#52894,.T.);
#74425=ORIENTED_EDGE('',*,*,#52897,.T.);
#74426=ORIENTED_EDGE('',*,*,#52898,.T.);
#74427=ORIENTED_EDGE('',*,*,#52899,.T.);
#74428=ORIENTED_EDGE('',*,*,#52625,.F.);
#74429=ORIENTED_EDGE('',*,*,#52900,.T.);
#74430=ORIENTED_EDGE('',*,*,#52878,.F.);
#74431=ORIENTED_EDGE('',*,*,#52901,.T.);
#74432=ORIENTED_EDGE('',*,*,#52898,.F.);
#74433=ORIENTED_EDGE('',*,*,#52902,.T.);
#74434=ORIENTED_EDGE('',*,*,#52402,.F.);
#74435=ORIENTED_EDGE('',*,*,#52903,.T.);
#74436=ORIENTED_EDGE('',*,*,#52889,.F.);
#74437=ORIENTED_EDGE('',*,*,#52904,.T.);
#74438=ORIENTED_EDGE('',*,*,#52891,.F.);
#74439=ORIENTED_EDGE('',*,*,#52905,.T.);
#74440=ORIENTED_EDGE('',*,*,#52885,.F.);
#74441=ORIENTED_EDGE('',*,*,#52906,.T.);
#74442=ORIENTED_EDGE('',*,*,#52887,.F.);
#74443=ORIENTED_EDGE('',*,*,#52907,.T.);
#74444=ORIENTED_EDGE('',*,*,#52908,.T.);
#74445=ORIENTED_EDGE('',*,*,#52909,.T.);
#74446=ORIENTED_EDGE('',*,*,#52910,.F.);
#74447=ORIENTED_EDGE('',*,*,#52911,.F.);
#74448=ORIENTED_EDGE('',*,*,#52912,.F.);
#74449=ORIENTED_EDGE('',*,*,#52913,.T.);
#74450=ORIENTED_EDGE('',*,*,#52911,.T.);
#74451=ORIENTED_EDGE('',*,*,#52914,.T.);
#74452=ORIENTED_EDGE('',*,*,#52915,.T.);
#74453=ORIENTED_EDGE('',*,*,#52916,.T.);
#74454=ORIENTED_EDGE('',*,*,#52917,.T.);
#74455=ORIENTED_EDGE('',*,*,#52918,.T.);
#74456=ORIENTED_EDGE('',*,*,#52919,.T.);
#74457=ORIENTED_EDGE('',*,*,#52920,.T.);
#74458=ORIENTED_EDGE('',*,*,#52921,.T.);
#74459=ORIENTED_EDGE('',*,*,#52922,.T.);
#74460=ORIENTED_EDGE('',*,*,#52923,.F.);
#74461=ORIENTED_EDGE('',*,*,#52924,.F.);
#74462=ORIENTED_EDGE('',*,*,#52925,.F.);
#74463=ORIENTED_EDGE('',*,*,#52926,.T.);
#74464=ORIENTED_EDGE('',*,*,#52924,.T.);
#74465=ORIENTED_EDGE('',*,*,#52927,.T.);
#74466=ORIENTED_EDGE('',*,*,#52928,.T.);
#74467=ORIENTED_EDGE('',*,*,#52929,.T.);
#74468=ORIENTED_EDGE('',*,*,#52631,.F.);
#74469=ORIENTED_EDGE('',*,*,#52930,.T.);
#74470=ORIENTED_EDGE('',*,*,#52908,.F.);
#74471=ORIENTED_EDGE('',*,*,#52931,.T.);
#74472=ORIENTED_EDGE('',*,*,#52928,.F.);
#74473=ORIENTED_EDGE('',*,*,#52932,.T.);
#74474=ORIENTED_EDGE('',*,*,#52396,.F.);
#74475=ORIENTED_EDGE('',*,*,#52933,.T.);
#74476=ORIENTED_EDGE('',*,*,#52919,.F.);
#74477=ORIENTED_EDGE('',*,*,#52934,.T.);
#74478=ORIENTED_EDGE('',*,*,#52921,.F.);
#74479=ORIENTED_EDGE('',*,*,#52935,.T.);
#74480=ORIENTED_EDGE('',*,*,#52915,.F.);
#74481=ORIENTED_EDGE('',*,*,#52936,.T.);
#74482=ORIENTED_EDGE('',*,*,#52917,.F.);
#74483=ORIENTED_EDGE('',*,*,#52937,.T.);
#74484=ORIENTED_EDGE('',*,*,#52938,.T.);
#74485=ORIENTED_EDGE('',*,*,#52939,.T.);
#74486=ORIENTED_EDGE('',*,*,#52940,.F.);
#74487=ORIENTED_EDGE('',*,*,#52941,.F.);
#74488=ORIENTED_EDGE('',*,*,#52942,.F.);
#74489=ORIENTED_EDGE('',*,*,#52943,.T.);
#74490=ORIENTED_EDGE('',*,*,#52941,.T.);
#74491=ORIENTED_EDGE('',*,*,#52944,.T.);
#74492=ORIENTED_EDGE('',*,*,#52945,.T.);
#74493=ORIENTED_EDGE('',*,*,#52946,.T.);
#74494=ORIENTED_EDGE('',*,*,#52947,.T.);
#74495=ORIENTED_EDGE('',*,*,#52948,.T.);
#74496=ORIENTED_EDGE('',*,*,#52949,.T.);
#74497=ORIENTED_EDGE('',*,*,#52950,.T.);
#74498=ORIENTED_EDGE('',*,*,#52951,.T.);
#74499=ORIENTED_EDGE('',*,*,#52952,.T.);
#74500=ORIENTED_EDGE('',*,*,#52953,.F.);
#74501=ORIENTED_EDGE('',*,*,#52954,.F.);
#74502=ORIENTED_EDGE('',*,*,#52955,.F.);
#74503=ORIENTED_EDGE('',*,*,#52956,.T.);
#74504=ORIENTED_EDGE('',*,*,#52954,.T.);
#74505=ORIENTED_EDGE('',*,*,#52957,.T.);
#74506=ORIENTED_EDGE('',*,*,#52958,.T.);
#74507=ORIENTED_EDGE('',*,*,#52959,.T.);
#74508=ORIENTED_EDGE('',*,*,#52637,.F.);
#74509=ORIENTED_EDGE('',*,*,#52960,.T.);
#74510=ORIENTED_EDGE('',*,*,#52938,.F.);
#74511=ORIENTED_EDGE('',*,*,#52961,.T.);
#74512=ORIENTED_EDGE('',*,*,#52958,.F.);
#74513=ORIENTED_EDGE('',*,*,#52962,.T.);
#74514=ORIENTED_EDGE('',*,*,#52390,.F.);
#74515=ORIENTED_EDGE('',*,*,#52963,.T.);
#74516=ORIENTED_EDGE('',*,*,#52949,.F.);
#74517=ORIENTED_EDGE('',*,*,#52964,.T.);
#74518=ORIENTED_EDGE('',*,*,#52951,.F.);
#74519=ORIENTED_EDGE('',*,*,#52965,.T.);
#74520=ORIENTED_EDGE('',*,*,#52945,.F.);
#74521=ORIENTED_EDGE('',*,*,#52966,.T.);
#74522=ORIENTED_EDGE('',*,*,#52947,.F.);
#74523=ORIENTED_EDGE('',*,*,#52967,.T.);
#74524=ORIENTED_EDGE('',*,*,#52968,.T.);
#74525=ORIENTED_EDGE('',*,*,#52969,.T.);
#74526=ORIENTED_EDGE('',*,*,#52970,.F.);
#74527=ORIENTED_EDGE('',*,*,#52971,.F.);
#74528=ORIENTED_EDGE('',*,*,#52972,.F.);
#74529=ORIENTED_EDGE('',*,*,#52973,.T.);
#74530=ORIENTED_EDGE('',*,*,#52971,.T.);
#74531=ORIENTED_EDGE('',*,*,#52974,.T.);
#74532=ORIENTED_EDGE('',*,*,#52975,.T.);
#74533=ORIENTED_EDGE('',*,*,#52976,.T.);
#74534=ORIENTED_EDGE('',*,*,#52977,.T.);
#74535=ORIENTED_EDGE('',*,*,#52978,.T.);
#74536=ORIENTED_EDGE('',*,*,#52979,.T.);
#74537=ORIENTED_EDGE('',*,*,#52980,.T.);
#74538=ORIENTED_EDGE('',*,*,#52981,.T.);
#74539=ORIENTED_EDGE('',*,*,#52982,.T.);
#74540=ORIENTED_EDGE('',*,*,#52983,.F.);
#74541=ORIENTED_EDGE('',*,*,#52984,.F.);
#74542=ORIENTED_EDGE('',*,*,#52985,.F.);
#74543=ORIENTED_EDGE('',*,*,#52986,.T.);
#74544=ORIENTED_EDGE('',*,*,#52984,.T.);
#74545=ORIENTED_EDGE('',*,*,#52987,.T.);
#74546=ORIENTED_EDGE('',*,*,#52988,.T.);
#74547=ORIENTED_EDGE('',*,*,#52989,.T.);
#74548=ORIENTED_EDGE('',*,*,#52643,.F.);
#74549=ORIENTED_EDGE('',*,*,#52990,.T.);
#74550=ORIENTED_EDGE('',*,*,#52968,.F.);
#74551=ORIENTED_EDGE('',*,*,#52991,.T.);
#74552=ORIENTED_EDGE('',*,*,#52988,.F.);
#74553=ORIENTED_EDGE('',*,*,#52992,.T.);
#74554=ORIENTED_EDGE('',*,*,#52384,.F.);
#74555=ORIENTED_EDGE('',*,*,#52993,.T.);
#74556=ORIENTED_EDGE('',*,*,#52979,.F.);
#74557=ORIENTED_EDGE('',*,*,#52994,.T.);
#74558=ORIENTED_EDGE('',*,*,#52981,.F.);
#74559=ORIENTED_EDGE('',*,*,#52995,.T.);
#74560=ORIENTED_EDGE('',*,*,#52975,.F.);
#74561=ORIENTED_EDGE('',*,*,#52996,.T.);
#74562=ORIENTED_EDGE('',*,*,#52977,.F.);
#74563=ORIENTED_EDGE('',*,*,#52997,.T.);
#74564=ORIENTED_EDGE('',*,*,#52998,.T.);
#74565=ORIENTED_EDGE('',*,*,#52999,.T.);
#74566=ORIENTED_EDGE('',*,*,#53000,.F.);
#74567=ORIENTED_EDGE('',*,*,#53001,.F.);
#74568=ORIENTED_EDGE('',*,*,#53002,.F.);
#74569=ORIENTED_EDGE('',*,*,#53003,.T.);
#74570=ORIENTED_EDGE('',*,*,#53001,.T.);
#74571=ORIENTED_EDGE('',*,*,#53004,.T.);
#74572=ORIENTED_EDGE('',*,*,#53005,.T.);
#74573=ORIENTED_EDGE('',*,*,#53006,.T.);
#74574=ORIENTED_EDGE('',*,*,#53007,.T.);
#74575=ORIENTED_EDGE('',*,*,#53008,.T.);
#74576=ORIENTED_EDGE('',*,*,#53009,.T.);
#74577=ORIENTED_EDGE('',*,*,#53010,.T.);
#74578=ORIENTED_EDGE('',*,*,#53011,.T.);
#74579=ORIENTED_EDGE('',*,*,#53012,.T.);
#74580=ORIENTED_EDGE('',*,*,#53013,.F.);
#74581=ORIENTED_EDGE('',*,*,#53014,.F.);
#74582=ORIENTED_EDGE('',*,*,#53015,.F.);
#74583=ORIENTED_EDGE('',*,*,#53016,.T.);
#74584=ORIENTED_EDGE('',*,*,#53014,.T.);
#74585=ORIENTED_EDGE('',*,*,#53017,.T.);
#74586=ORIENTED_EDGE('',*,*,#53018,.T.);
#74587=ORIENTED_EDGE('',*,*,#53019,.T.);
#74588=ORIENTED_EDGE('',*,*,#52649,.F.);
#74589=ORIENTED_EDGE('',*,*,#53020,.T.);
#74590=ORIENTED_EDGE('',*,*,#52998,.F.);
#74591=ORIENTED_EDGE('',*,*,#53021,.T.);
#74592=ORIENTED_EDGE('',*,*,#53018,.F.);
#74593=ORIENTED_EDGE('',*,*,#53022,.T.);
#74594=ORIENTED_EDGE('',*,*,#52378,.F.);
#74595=ORIENTED_EDGE('',*,*,#53023,.T.);
#74596=ORIENTED_EDGE('',*,*,#53009,.F.);
#74597=ORIENTED_EDGE('',*,*,#53024,.T.);
#74598=ORIENTED_EDGE('',*,*,#53011,.F.);
#74599=ORIENTED_EDGE('',*,*,#53025,.T.);
#74600=ORIENTED_EDGE('',*,*,#53005,.F.);
#74601=ORIENTED_EDGE('',*,*,#53026,.T.);
#74602=ORIENTED_EDGE('',*,*,#53007,.F.);
#74603=ORIENTED_EDGE('',*,*,#53027,.T.);
#74604=ORIENTED_EDGE('',*,*,#53028,.T.);
#74605=ORIENTED_EDGE('',*,*,#53029,.T.);
#74606=ORIENTED_EDGE('',*,*,#53030,.F.);
#74607=ORIENTED_EDGE('',*,*,#53031,.F.);
#74608=ORIENTED_EDGE('',*,*,#53032,.F.);
#74609=ORIENTED_EDGE('',*,*,#53033,.T.);
#74610=ORIENTED_EDGE('',*,*,#53031,.T.);
#74611=ORIENTED_EDGE('',*,*,#53034,.T.);
#74612=ORIENTED_EDGE('',*,*,#53035,.T.);
#74613=ORIENTED_EDGE('',*,*,#53036,.T.);
#74614=ORIENTED_EDGE('',*,*,#53037,.T.);
#74615=ORIENTED_EDGE('',*,*,#53038,.T.);
#74616=ORIENTED_EDGE('',*,*,#53039,.T.);
#74617=ORIENTED_EDGE('',*,*,#53040,.T.);
#74618=ORIENTED_EDGE('',*,*,#53041,.T.);
#74619=ORIENTED_EDGE('',*,*,#53042,.T.);
#74620=ORIENTED_EDGE('',*,*,#53043,.F.);
#74621=ORIENTED_EDGE('',*,*,#53044,.F.);
#74622=ORIENTED_EDGE('',*,*,#53045,.F.);
#74623=ORIENTED_EDGE('',*,*,#53046,.T.);
#74624=ORIENTED_EDGE('',*,*,#53044,.T.);
#74625=ORIENTED_EDGE('',*,*,#53047,.T.);
#74626=ORIENTED_EDGE('',*,*,#53048,.T.);
#74627=ORIENTED_EDGE('',*,*,#53049,.T.);
#74628=ORIENTED_EDGE('',*,*,#52655,.F.);
#74629=ORIENTED_EDGE('',*,*,#53050,.T.);
#74630=ORIENTED_EDGE('',*,*,#53028,.F.);
#74631=ORIENTED_EDGE('',*,*,#53051,.T.);
#74632=ORIENTED_EDGE('',*,*,#53048,.F.);
#74633=ORIENTED_EDGE('',*,*,#53052,.T.);
#74634=ORIENTED_EDGE('',*,*,#52372,.F.);
#74635=ORIENTED_EDGE('',*,*,#53053,.T.);
#74636=ORIENTED_EDGE('',*,*,#53039,.F.);
#74637=ORIENTED_EDGE('',*,*,#53054,.T.);
#74638=ORIENTED_EDGE('',*,*,#53041,.F.);
#74639=ORIENTED_EDGE('',*,*,#53055,.T.);
#74640=ORIENTED_EDGE('',*,*,#53035,.F.);
#74641=ORIENTED_EDGE('',*,*,#53056,.T.);
#74642=ORIENTED_EDGE('',*,*,#53037,.F.);
#74643=ORIENTED_EDGE('',*,*,#53057,.T.);
#74644=ORIENTED_EDGE('',*,*,#53058,.T.);
#74645=ORIENTED_EDGE('',*,*,#53059,.T.);
#74646=ORIENTED_EDGE('',*,*,#53060,.F.);
#74647=ORIENTED_EDGE('',*,*,#53061,.F.);
#74648=ORIENTED_EDGE('',*,*,#53062,.F.);
#74649=ORIENTED_EDGE('',*,*,#53063,.T.);
#74650=ORIENTED_EDGE('',*,*,#53061,.T.);
#74651=ORIENTED_EDGE('',*,*,#53064,.T.);
#74652=ORIENTED_EDGE('',*,*,#53065,.T.);
#74653=ORIENTED_EDGE('',*,*,#53066,.T.);
#74654=ORIENTED_EDGE('',*,*,#53067,.T.);
#74655=ORIENTED_EDGE('',*,*,#53068,.T.);
#74656=ORIENTED_EDGE('',*,*,#53069,.T.);
#74657=ORIENTED_EDGE('',*,*,#53070,.T.);
#74658=ORIENTED_EDGE('',*,*,#53071,.T.);
#74659=ORIENTED_EDGE('',*,*,#53072,.T.);
#74660=ORIENTED_EDGE('',*,*,#53073,.F.);
#74661=ORIENTED_EDGE('',*,*,#53074,.F.);
#74662=ORIENTED_EDGE('',*,*,#53075,.F.);
#74663=ORIENTED_EDGE('',*,*,#53076,.T.);
#74664=ORIENTED_EDGE('',*,*,#53074,.T.);
#74665=ORIENTED_EDGE('',*,*,#53077,.T.);
#74666=ORIENTED_EDGE('',*,*,#53078,.T.);
#74667=ORIENTED_EDGE('',*,*,#53079,.T.);
#74668=ORIENTED_EDGE('',*,*,#52661,.F.);
#74669=ORIENTED_EDGE('',*,*,#53080,.T.);
#74670=ORIENTED_EDGE('',*,*,#53058,.F.);
#74671=ORIENTED_EDGE('',*,*,#53081,.T.);
#74672=ORIENTED_EDGE('',*,*,#53078,.F.);
#74673=ORIENTED_EDGE('',*,*,#53082,.T.);
#74674=ORIENTED_EDGE('',*,*,#52366,.F.);
#74675=ORIENTED_EDGE('',*,*,#53083,.T.);
#74676=ORIENTED_EDGE('',*,*,#53069,.F.);
#74677=ORIENTED_EDGE('',*,*,#53084,.T.);
#74678=ORIENTED_EDGE('',*,*,#53071,.F.);
#74679=ORIENTED_EDGE('',*,*,#53085,.T.);
#74680=ORIENTED_EDGE('',*,*,#53065,.F.);
#74681=ORIENTED_EDGE('',*,*,#53086,.T.);
#74682=ORIENTED_EDGE('',*,*,#53067,.F.);
#74683=ORIENTED_EDGE('',*,*,#53087,.T.);
#74684=ORIENTED_EDGE('',*,*,#53088,.T.);
#74685=ORIENTED_EDGE('',*,*,#53089,.T.);
#74686=ORIENTED_EDGE('',*,*,#53090,.F.);
#74687=ORIENTED_EDGE('',*,*,#53091,.F.);
#74688=ORIENTED_EDGE('',*,*,#53092,.F.);
#74689=ORIENTED_EDGE('',*,*,#53093,.T.);
#74690=ORIENTED_EDGE('',*,*,#53091,.T.);
#74691=ORIENTED_EDGE('',*,*,#53094,.T.);
#74692=ORIENTED_EDGE('',*,*,#53095,.T.);
#74693=ORIENTED_EDGE('',*,*,#53096,.T.);
#74694=ORIENTED_EDGE('',*,*,#53097,.T.);
#74695=ORIENTED_EDGE('',*,*,#53098,.T.);
#74696=ORIENTED_EDGE('',*,*,#53099,.T.);
#74697=ORIENTED_EDGE('',*,*,#53100,.T.);
#74698=ORIENTED_EDGE('',*,*,#53101,.T.);
#74699=ORIENTED_EDGE('',*,*,#53102,.T.);
#74700=ORIENTED_EDGE('',*,*,#53103,.F.);
#74701=ORIENTED_EDGE('',*,*,#53104,.F.);
#74702=ORIENTED_EDGE('',*,*,#53105,.F.);
#74703=ORIENTED_EDGE('',*,*,#53106,.T.);
#74704=ORIENTED_EDGE('',*,*,#53104,.T.);
#74705=ORIENTED_EDGE('',*,*,#53107,.T.);
#74706=ORIENTED_EDGE('',*,*,#53108,.T.);
#74707=ORIENTED_EDGE('',*,*,#53109,.T.);
#74708=ORIENTED_EDGE('',*,*,#52667,.F.);
#74709=ORIENTED_EDGE('',*,*,#53110,.T.);
#74710=ORIENTED_EDGE('',*,*,#53088,.F.);
#74711=ORIENTED_EDGE('',*,*,#53111,.T.);
#74712=ORIENTED_EDGE('',*,*,#53108,.F.);
#74713=ORIENTED_EDGE('',*,*,#53112,.T.);
#74714=ORIENTED_EDGE('',*,*,#52360,.F.);
#74715=ORIENTED_EDGE('',*,*,#53113,.T.);
#74716=ORIENTED_EDGE('',*,*,#53099,.F.);
#74717=ORIENTED_EDGE('',*,*,#53114,.T.);
#74718=ORIENTED_EDGE('',*,*,#53101,.F.);
#74719=ORIENTED_EDGE('',*,*,#53115,.T.);
#74720=ORIENTED_EDGE('',*,*,#53095,.F.);
#74721=ORIENTED_EDGE('',*,*,#53116,.T.);
#74722=ORIENTED_EDGE('',*,*,#53097,.F.);
#74723=ORIENTED_EDGE('',*,*,#53117,.T.);
#74724=ORIENTED_EDGE('',*,*,#53118,.T.);
#74725=ORIENTED_EDGE('',*,*,#53119,.T.);
#74726=ORIENTED_EDGE('',*,*,#53120,.F.);
#74727=ORIENTED_EDGE('',*,*,#53121,.F.);
#74728=ORIENTED_EDGE('',*,*,#53122,.F.);
#74729=ORIENTED_EDGE('',*,*,#53123,.T.);
#74730=ORIENTED_EDGE('',*,*,#53121,.T.);
#74731=ORIENTED_EDGE('',*,*,#53124,.T.);
#74732=ORIENTED_EDGE('',*,*,#53125,.T.);
#74733=ORIENTED_EDGE('',*,*,#53126,.T.);
#74734=ORIENTED_EDGE('',*,*,#53127,.T.);
#74735=ORIENTED_EDGE('',*,*,#53128,.T.);
#74736=ORIENTED_EDGE('',*,*,#53129,.T.);
#74737=ORIENTED_EDGE('',*,*,#53130,.T.);
#74738=ORIENTED_EDGE('',*,*,#53131,.T.);
#74739=ORIENTED_EDGE('',*,*,#53132,.T.);
#74740=ORIENTED_EDGE('',*,*,#53133,.F.);
#74741=ORIENTED_EDGE('',*,*,#53134,.F.);
#74742=ORIENTED_EDGE('',*,*,#53135,.F.);
#74743=ORIENTED_EDGE('',*,*,#53136,.T.);
#74744=ORIENTED_EDGE('',*,*,#53134,.T.);
#74745=ORIENTED_EDGE('',*,*,#53137,.T.);
#74746=ORIENTED_EDGE('',*,*,#53138,.T.);
#74747=ORIENTED_EDGE('',*,*,#53139,.T.);
#74748=ORIENTED_EDGE('',*,*,#52673,.F.);
#74749=ORIENTED_EDGE('',*,*,#53140,.T.);
#74750=ORIENTED_EDGE('',*,*,#53118,.F.);
#74751=ORIENTED_EDGE('',*,*,#53141,.T.);
#74752=ORIENTED_EDGE('',*,*,#53138,.F.);
#74753=ORIENTED_EDGE('',*,*,#53142,.T.);
#74754=ORIENTED_EDGE('',*,*,#52354,.F.);
#74755=ORIENTED_EDGE('',*,*,#53143,.T.);
#74756=ORIENTED_EDGE('',*,*,#53129,.F.);
#74757=ORIENTED_EDGE('',*,*,#53144,.T.);
#74758=ORIENTED_EDGE('',*,*,#53131,.F.);
#74759=ORIENTED_EDGE('',*,*,#53145,.T.);
#74760=ORIENTED_EDGE('',*,*,#53125,.F.);
#74761=ORIENTED_EDGE('',*,*,#53146,.T.);
#74762=ORIENTED_EDGE('',*,*,#53127,.F.);
#74763=ORIENTED_EDGE('',*,*,#53147,.T.);
#74764=ORIENTED_EDGE('',*,*,#53148,.T.);
#74765=ORIENTED_EDGE('',*,*,#53149,.T.);
#74766=ORIENTED_EDGE('',*,*,#53150,.F.);
#74767=ORIENTED_EDGE('',*,*,#53151,.F.);
#74768=ORIENTED_EDGE('',*,*,#53152,.F.);
#74769=ORIENTED_EDGE('',*,*,#53153,.T.);
#74770=ORIENTED_EDGE('',*,*,#53151,.T.);
#74771=ORIENTED_EDGE('',*,*,#53154,.T.);
#74772=ORIENTED_EDGE('',*,*,#53155,.T.);
#74773=ORIENTED_EDGE('',*,*,#53156,.T.);
#74774=ORIENTED_EDGE('',*,*,#53157,.T.);
#74775=ORIENTED_EDGE('',*,*,#53158,.T.);
#74776=ORIENTED_EDGE('',*,*,#53159,.T.);
#74777=ORIENTED_EDGE('',*,*,#53160,.T.);
#74778=ORIENTED_EDGE('',*,*,#53161,.T.);
#74779=ORIENTED_EDGE('',*,*,#53162,.T.);
#74780=ORIENTED_EDGE('',*,*,#53163,.F.);
#74781=ORIENTED_EDGE('',*,*,#53164,.F.);
#74782=ORIENTED_EDGE('',*,*,#53165,.F.);
#74783=ORIENTED_EDGE('',*,*,#53166,.T.);
#74784=ORIENTED_EDGE('',*,*,#53164,.T.);
#74785=ORIENTED_EDGE('',*,*,#53167,.T.);
#74786=ORIENTED_EDGE('',*,*,#53168,.T.);
#74787=ORIENTED_EDGE('',*,*,#53169,.T.);
#74788=ORIENTED_EDGE('',*,*,#52679,.F.);
#74789=ORIENTED_EDGE('',*,*,#53170,.T.);
#74790=ORIENTED_EDGE('',*,*,#53148,.F.);
#74791=ORIENTED_EDGE('',*,*,#53171,.T.);
#74792=ORIENTED_EDGE('',*,*,#53168,.F.);
#74793=ORIENTED_EDGE('',*,*,#53172,.T.);
#74794=ORIENTED_EDGE('',*,*,#52348,.F.);
#74795=ORIENTED_EDGE('',*,*,#53173,.T.);
#74796=ORIENTED_EDGE('',*,*,#53159,.F.);
#74797=ORIENTED_EDGE('',*,*,#53174,.T.);
#74798=ORIENTED_EDGE('',*,*,#53161,.F.);
#74799=ORIENTED_EDGE('',*,*,#53175,.T.);
#74800=ORIENTED_EDGE('',*,*,#53155,.F.);
#74801=ORIENTED_EDGE('',*,*,#53176,.T.);
#74802=ORIENTED_EDGE('',*,*,#53157,.F.);
#74803=ORIENTED_EDGE('',*,*,#53177,.T.);
#74804=ORIENTED_EDGE('',*,*,#53178,.T.);
#74805=ORIENTED_EDGE('',*,*,#53179,.T.);
#74806=ORIENTED_EDGE('',*,*,#53180,.F.);
#74807=ORIENTED_EDGE('',*,*,#53181,.F.);
#74808=ORIENTED_EDGE('',*,*,#53182,.F.);
#74809=ORIENTED_EDGE('',*,*,#53183,.T.);
#74810=ORIENTED_EDGE('',*,*,#53181,.T.);
#74811=ORIENTED_EDGE('',*,*,#53184,.T.);
#74812=ORIENTED_EDGE('',*,*,#53185,.T.);
#74813=ORIENTED_EDGE('',*,*,#53186,.T.);
#74814=ORIENTED_EDGE('',*,*,#53187,.T.);
#74815=ORIENTED_EDGE('',*,*,#53188,.T.);
#74816=ORIENTED_EDGE('',*,*,#53189,.T.);
#74817=ORIENTED_EDGE('',*,*,#53190,.T.);
#74818=ORIENTED_EDGE('',*,*,#53191,.T.);
#74819=ORIENTED_EDGE('',*,*,#53192,.T.);
#74820=ORIENTED_EDGE('',*,*,#53193,.F.);
#74821=ORIENTED_EDGE('',*,*,#53194,.F.);
#74822=ORIENTED_EDGE('',*,*,#53195,.F.);
#74823=ORIENTED_EDGE('',*,*,#53196,.T.);
#74824=ORIENTED_EDGE('',*,*,#53194,.T.);
#74825=ORIENTED_EDGE('',*,*,#53197,.T.);
#74826=ORIENTED_EDGE('',*,*,#53198,.T.);
#74827=ORIENTED_EDGE('',*,*,#53199,.T.);
#74828=ORIENTED_EDGE('',*,*,#52685,.F.);
#74829=ORIENTED_EDGE('',*,*,#53200,.T.);
#74830=ORIENTED_EDGE('',*,*,#53178,.F.);
#74831=ORIENTED_EDGE('',*,*,#53201,.T.);
#74832=ORIENTED_EDGE('',*,*,#53198,.F.);
#74833=ORIENTED_EDGE('',*,*,#53202,.T.);
#74834=ORIENTED_EDGE('',*,*,#52342,.F.);
#74835=ORIENTED_EDGE('',*,*,#53203,.T.);
#74836=ORIENTED_EDGE('',*,*,#53189,.F.);
#74837=ORIENTED_EDGE('',*,*,#53204,.T.);
#74838=ORIENTED_EDGE('',*,*,#53191,.F.);
#74839=ORIENTED_EDGE('',*,*,#53205,.T.);
#74840=ORIENTED_EDGE('',*,*,#53185,.F.);
#74841=ORIENTED_EDGE('',*,*,#53206,.T.);
#74842=ORIENTED_EDGE('',*,*,#53187,.F.);
#74843=ORIENTED_EDGE('',*,*,#53207,.T.);
#74844=ORIENTED_EDGE('',*,*,#53208,.T.);
#74845=ORIENTED_EDGE('',*,*,#53209,.T.);
#74846=ORIENTED_EDGE('',*,*,#53210,.F.);
#74847=ORIENTED_EDGE('',*,*,#53211,.F.);
#74848=ORIENTED_EDGE('',*,*,#53212,.F.);
#74849=ORIENTED_EDGE('',*,*,#53213,.T.);
#74850=ORIENTED_EDGE('',*,*,#53211,.T.);
#74851=ORIENTED_EDGE('',*,*,#53214,.T.);
#74852=ORIENTED_EDGE('',*,*,#53215,.T.);
#74853=ORIENTED_EDGE('',*,*,#53216,.T.);
#74854=ORIENTED_EDGE('',*,*,#53217,.T.);
#74855=ORIENTED_EDGE('',*,*,#53218,.T.);
#74856=ORIENTED_EDGE('',*,*,#53219,.T.);
#74857=ORIENTED_EDGE('',*,*,#53220,.T.);
#74858=ORIENTED_EDGE('',*,*,#53221,.T.);
#74859=ORIENTED_EDGE('',*,*,#53222,.T.);
#74860=ORIENTED_EDGE('',*,*,#53223,.F.);
#74861=ORIENTED_EDGE('',*,*,#53224,.F.);
#74862=ORIENTED_EDGE('',*,*,#53225,.F.);
#74863=ORIENTED_EDGE('',*,*,#53226,.T.);
#74864=ORIENTED_EDGE('',*,*,#53224,.T.);
#74865=ORIENTED_EDGE('',*,*,#53227,.T.);
#74866=ORIENTED_EDGE('',*,*,#53228,.T.);
#74867=ORIENTED_EDGE('',*,*,#53229,.T.);
#74868=ORIENTED_EDGE('',*,*,#52691,.F.);
#74869=ORIENTED_EDGE('',*,*,#53230,.T.);
#74870=ORIENTED_EDGE('',*,*,#53208,.F.);
#74871=ORIENTED_EDGE('',*,*,#53231,.T.);
#74872=ORIENTED_EDGE('',*,*,#53228,.F.);
#74873=ORIENTED_EDGE('',*,*,#53232,.T.);
#74874=ORIENTED_EDGE('',*,*,#52336,.F.);
#74875=ORIENTED_EDGE('',*,*,#53233,.T.);
#74876=ORIENTED_EDGE('',*,*,#53219,.F.);
#74877=ORIENTED_EDGE('',*,*,#53234,.T.);
#74878=ORIENTED_EDGE('',*,*,#53221,.F.);
#74879=ORIENTED_EDGE('',*,*,#53235,.T.);
#74880=ORIENTED_EDGE('',*,*,#53215,.F.);
#74881=ORIENTED_EDGE('',*,*,#53236,.T.);
#74882=ORIENTED_EDGE('',*,*,#53217,.F.);
#74883=ORIENTED_EDGE('',*,*,#53237,.T.);
#74884=ORIENTED_EDGE('',*,*,#53238,.T.);
#74885=ORIENTED_EDGE('',*,*,#53239,.T.);
#74886=ORIENTED_EDGE('',*,*,#53240,.F.);
#74887=ORIENTED_EDGE('',*,*,#53241,.F.);
#74888=ORIENTED_EDGE('',*,*,#53242,.F.);
#74889=ORIENTED_EDGE('',*,*,#53243,.T.);
#74890=ORIENTED_EDGE('',*,*,#53241,.T.);
#74891=ORIENTED_EDGE('',*,*,#53244,.T.);
#74892=ORIENTED_EDGE('',*,*,#53245,.T.);
#74893=ORIENTED_EDGE('',*,*,#53246,.T.);
#74894=ORIENTED_EDGE('',*,*,#53247,.T.);
#74895=ORIENTED_EDGE('',*,*,#53248,.T.);
#74896=ORIENTED_EDGE('',*,*,#53249,.T.);
#74897=ORIENTED_EDGE('',*,*,#53250,.T.);
#74898=ORIENTED_EDGE('',*,*,#53251,.T.);
#74899=ORIENTED_EDGE('',*,*,#53252,.T.);
#74900=ORIENTED_EDGE('',*,*,#53253,.F.);
#74901=ORIENTED_EDGE('',*,*,#53254,.F.);
#74902=ORIENTED_EDGE('',*,*,#53255,.F.);
#74903=ORIENTED_EDGE('',*,*,#53256,.T.);
#74904=ORIENTED_EDGE('',*,*,#53254,.T.);
#74905=ORIENTED_EDGE('',*,*,#53257,.T.);
#74906=ORIENTED_EDGE('',*,*,#53258,.T.);
#74907=ORIENTED_EDGE('',*,*,#53259,.T.);
#74908=ORIENTED_EDGE('',*,*,#52696,.F.);
#74909=ORIENTED_EDGE('',*,*,#53260,.T.);
#74910=ORIENTED_EDGE('',*,*,#53238,.F.);
#74911=ORIENTED_EDGE('',*,*,#53261,.T.);
#74912=ORIENTED_EDGE('',*,*,#53258,.F.);
#74913=ORIENTED_EDGE('',*,*,#53262,.T.);
#74914=ORIENTED_EDGE('',*,*,#52331,.F.);
#74915=ORIENTED_EDGE('',*,*,#53263,.T.);
#74916=ORIENTED_EDGE('',*,*,#53249,.F.);
#74917=ORIENTED_EDGE('',*,*,#53264,.T.);
#74918=ORIENTED_EDGE('',*,*,#53251,.F.);
#74919=ORIENTED_EDGE('',*,*,#53265,.T.);
#74920=ORIENTED_EDGE('',*,*,#53245,.F.);
#74921=ORIENTED_EDGE('',*,*,#53266,.T.);
#74922=ORIENTED_EDGE('',*,*,#53247,.F.);
#74923=ORIENTED_EDGE('',*,*,#53267,.T.);
#74924=ORIENTED_EDGE('',*,*,#53268,.T.);
#74925=ORIENTED_EDGE('',*,*,#53269,.T.);
#74926=ORIENTED_EDGE('',*,*,#53270,.F.);
#74927=ORIENTED_EDGE('',*,*,#53271,.F.);
#74928=ORIENTED_EDGE('',*,*,#53272,.F.);
#74929=ORIENTED_EDGE('',*,*,#53273,.T.);
#74930=ORIENTED_EDGE('',*,*,#53271,.T.);
#74931=ORIENTED_EDGE('',*,*,#53274,.T.);
#74932=ORIENTED_EDGE('',*,*,#53275,.T.);
#74933=ORIENTED_EDGE('',*,*,#53276,.T.);
#74934=ORIENTED_EDGE('',*,*,#53277,.T.);
#74935=ORIENTED_EDGE('',*,*,#53278,.T.);
#74936=ORIENTED_EDGE('',*,*,#53279,.T.);
#74937=ORIENTED_EDGE('',*,*,#53280,.T.);
#74938=ORIENTED_EDGE('',*,*,#53281,.T.);
#74939=ORIENTED_EDGE('',*,*,#53282,.T.);
#74940=ORIENTED_EDGE('',*,*,#53283,.F.);
#74941=ORIENTED_EDGE('',*,*,#53284,.F.);
#74942=ORIENTED_EDGE('',*,*,#53285,.F.);
#74943=ORIENTED_EDGE('',*,*,#53286,.T.);
#74944=ORIENTED_EDGE('',*,*,#53284,.T.);
#74945=ORIENTED_EDGE('',*,*,#53287,.T.);
#74946=ORIENTED_EDGE('',*,*,#53288,.T.);
#74947=ORIENTED_EDGE('',*,*,#53289,.T.);
#74948=ORIENTED_EDGE('',*,*,#52702,.F.);
#74949=ORIENTED_EDGE('',*,*,#53290,.T.);
#74950=ORIENTED_EDGE('',*,*,#53268,.F.);
#74951=ORIENTED_EDGE('',*,*,#53291,.T.);
#74952=ORIENTED_EDGE('',*,*,#53288,.F.);
#74953=ORIENTED_EDGE('',*,*,#53292,.T.);
#74954=ORIENTED_EDGE('',*,*,#52325,.F.);
#74955=ORIENTED_EDGE('',*,*,#53293,.T.);
#74956=ORIENTED_EDGE('',*,*,#53279,.F.);
#74957=ORIENTED_EDGE('',*,*,#53294,.T.);
#74958=ORIENTED_EDGE('',*,*,#53281,.F.);
#74959=ORIENTED_EDGE('',*,*,#53295,.T.);
#74960=ORIENTED_EDGE('',*,*,#53275,.F.);
#74961=ORIENTED_EDGE('',*,*,#53296,.T.);
#74962=ORIENTED_EDGE('',*,*,#53277,.F.);
#74963=ORIENTED_EDGE('',*,*,#53297,.T.);
#74964=ORIENTED_EDGE('',*,*,#53298,.T.);
#74965=ORIENTED_EDGE('',*,*,#53299,.T.);
#74966=ORIENTED_EDGE('',*,*,#53300,.F.);
#74967=ORIENTED_EDGE('',*,*,#53301,.F.);
#74968=ORIENTED_EDGE('',*,*,#53302,.F.);
#74969=ORIENTED_EDGE('',*,*,#53303,.T.);
#74970=ORIENTED_EDGE('',*,*,#53301,.T.);
#74971=ORIENTED_EDGE('',*,*,#53304,.T.);
#74972=ORIENTED_EDGE('',*,*,#53305,.T.);
#74973=ORIENTED_EDGE('',*,*,#53306,.T.);
#74974=ORIENTED_EDGE('',*,*,#53307,.T.);
#74975=ORIENTED_EDGE('',*,*,#53308,.T.);
#74976=ORIENTED_EDGE('',*,*,#53309,.T.);
#74977=ORIENTED_EDGE('',*,*,#53310,.T.);
#74978=ORIENTED_EDGE('',*,*,#53311,.T.);
#74979=ORIENTED_EDGE('',*,*,#53312,.T.);
#74980=ORIENTED_EDGE('',*,*,#53313,.F.);
#74981=ORIENTED_EDGE('',*,*,#53314,.F.);
#74982=ORIENTED_EDGE('',*,*,#53315,.F.);
#74983=ORIENTED_EDGE('',*,*,#53316,.T.);
#74984=ORIENTED_EDGE('',*,*,#53314,.T.);
#74985=ORIENTED_EDGE('',*,*,#53317,.T.);
#74986=ORIENTED_EDGE('',*,*,#53318,.T.);
#74987=ORIENTED_EDGE('',*,*,#53319,.T.);
#74988=ORIENTED_EDGE('',*,*,#52708,.F.);
#74989=ORIENTED_EDGE('',*,*,#53320,.T.);
#74990=ORIENTED_EDGE('',*,*,#53298,.F.);
#74991=ORIENTED_EDGE('',*,*,#53321,.T.);
#74992=ORIENTED_EDGE('',*,*,#53318,.F.);
#74993=ORIENTED_EDGE('',*,*,#53322,.T.);
#74994=ORIENTED_EDGE('',*,*,#52319,.F.);
#74995=ORIENTED_EDGE('',*,*,#53323,.T.);
#74996=ORIENTED_EDGE('',*,*,#53309,.F.);
#74997=ORIENTED_EDGE('',*,*,#53324,.T.);
#74998=ORIENTED_EDGE('',*,*,#53311,.F.);
#74999=ORIENTED_EDGE('',*,*,#53325,.T.);
#75000=ORIENTED_EDGE('',*,*,#53305,.F.);
#75001=ORIENTED_EDGE('',*,*,#53326,.T.);
#75002=ORIENTED_EDGE('',*,*,#53307,.F.);
#75003=ORIENTED_EDGE('',*,*,#53327,.T.);
#75004=ORIENTED_EDGE('',*,*,#53328,.T.);
#75005=ORIENTED_EDGE('',*,*,#53329,.T.);
#75006=ORIENTED_EDGE('',*,*,#53330,.F.);
#75007=ORIENTED_EDGE('',*,*,#53331,.F.);
#75008=ORIENTED_EDGE('',*,*,#53332,.F.);
#75009=ORIENTED_EDGE('',*,*,#53333,.T.);
#75010=ORIENTED_EDGE('',*,*,#53331,.T.);
#75011=ORIENTED_EDGE('',*,*,#53334,.T.);
#75012=ORIENTED_EDGE('',*,*,#53335,.T.);
#75013=ORIENTED_EDGE('',*,*,#53336,.T.);
#75014=ORIENTED_EDGE('',*,*,#53337,.T.);
#75015=ORIENTED_EDGE('',*,*,#53338,.T.);
#75016=ORIENTED_EDGE('',*,*,#53339,.T.);
#75017=ORIENTED_EDGE('',*,*,#53340,.T.);
#75018=ORIENTED_EDGE('',*,*,#53341,.T.);
#75019=ORIENTED_EDGE('',*,*,#53342,.T.);
#75020=ORIENTED_EDGE('',*,*,#53343,.F.);
#75021=ORIENTED_EDGE('',*,*,#53344,.F.);
#75022=ORIENTED_EDGE('',*,*,#53345,.F.);
#75023=ORIENTED_EDGE('',*,*,#53346,.T.);
#75024=ORIENTED_EDGE('',*,*,#53344,.T.);
#75025=ORIENTED_EDGE('',*,*,#53347,.T.);
#75026=ORIENTED_EDGE('',*,*,#53348,.T.);
#75027=ORIENTED_EDGE('',*,*,#53349,.T.);
#75028=ORIENTED_EDGE('',*,*,#52714,.F.);
#75029=ORIENTED_EDGE('',*,*,#53350,.T.);
#75030=ORIENTED_EDGE('',*,*,#53328,.F.);
#75031=ORIENTED_EDGE('',*,*,#53351,.T.);
#75032=ORIENTED_EDGE('',*,*,#53348,.F.);
#75033=ORIENTED_EDGE('',*,*,#53352,.T.);
#75034=ORIENTED_EDGE('',*,*,#52313,.F.);
#75035=ORIENTED_EDGE('',*,*,#53353,.T.);
#75036=ORIENTED_EDGE('',*,*,#53339,.F.);
#75037=ORIENTED_EDGE('',*,*,#53354,.T.);
#75038=ORIENTED_EDGE('',*,*,#53341,.F.);
#75039=ORIENTED_EDGE('',*,*,#53355,.T.);
#75040=ORIENTED_EDGE('',*,*,#53335,.F.);
#75041=ORIENTED_EDGE('',*,*,#53356,.T.);
#75042=ORIENTED_EDGE('',*,*,#53337,.F.);
#75043=ORIENTED_EDGE('',*,*,#53357,.T.);
#75044=ORIENTED_EDGE('',*,*,#53358,.T.);
#75045=ORIENTED_EDGE('',*,*,#53359,.T.);
#75046=ORIENTED_EDGE('',*,*,#53360,.F.);
#75047=ORIENTED_EDGE('',*,*,#53361,.F.);
#75048=ORIENTED_EDGE('',*,*,#53362,.F.);
#75049=ORIENTED_EDGE('',*,*,#53363,.T.);
#75050=ORIENTED_EDGE('',*,*,#53361,.T.);
#75051=ORIENTED_EDGE('',*,*,#53364,.T.);
#75052=ORIENTED_EDGE('',*,*,#53365,.T.);
#75053=ORIENTED_EDGE('',*,*,#53366,.T.);
#75054=ORIENTED_EDGE('',*,*,#53367,.T.);
#75055=ORIENTED_EDGE('',*,*,#53368,.T.);
#75056=ORIENTED_EDGE('',*,*,#53369,.T.);
#75057=ORIENTED_EDGE('',*,*,#53370,.T.);
#75058=ORIENTED_EDGE('',*,*,#53371,.T.);
#75059=ORIENTED_EDGE('',*,*,#53372,.T.);
#75060=ORIENTED_EDGE('',*,*,#53373,.F.);
#75061=ORIENTED_EDGE('',*,*,#53374,.F.);
#75062=ORIENTED_EDGE('',*,*,#53375,.F.);
#75063=ORIENTED_EDGE('',*,*,#53376,.T.);
#75064=ORIENTED_EDGE('',*,*,#53374,.T.);
#75065=ORIENTED_EDGE('',*,*,#53377,.T.);
#75066=ORIENTED_EDGE('',*,*,#53378,.T.);
#75067=ORIENTED_EDGE('',*,*,#53379,.T.);
#75068=ORIENTED_EDGE('',*,*,#52720,.F.);
#75069=ORIENTED_EDGE('',*,*,#53380,.T.);
#75070=ORIENTED_EDGE('',*,*,#53358,.F.);
#75071=ORIENTED_EDGE('',*,*,#53381,.T.);
#75072=ORIENTED_EDGE('',*,*,#53378,.F.);
#75073=ORIENTED_EDGE('',*,*,#53382,.T.);
#75074=ORIENTED_EDGE('',*,*,#52307,.F.);
#75075=ORIENTED_EDGE('',*,*,#53383,.T.);
#75076=ORIENTED_EDGE('',*,*,#53369,.F.);
#75077=ORIENTED_EDGE('',*,*,#53384,.T.);
#75078=ORIENTED_EDGE('',*,*,#53371,.F.);
#75079=ORIENTED_EDGE('',*,*,#53385,.T.);
#75080=ORIENTED_EDGE('',*,*,#53365,.F.);
#75081=ORIENTED_EDGE('',*,*,#53386,.T.);
#75082=ORIENTED_EDGE('',*,*,#53367,.F.);
#75083=ORIENTED_EDGE('',*,*,#53387,.T.);
#75084=ORIENTED_EDGE('',*,*,#53388,.T.);
#75085=ORIENTED_EDGE('',*,*,#53389,.T.);
#75086=ORIENTED_EDGE('',*,*,#53390,.F.);
#75087=ORIENTED_EDGE('',*,*,#53391,.F.);
#75088=ORIENTED_EDGE('',*,*,#53392,.F.);
#75089=ORIENTED_EDGE('',*,*,#53393,.T.);
#75090=ORIENTED_EDGE('',*,*,#53391,.T.);
#75091=ORIENTED_EDGE('',*,*,#53394,.T.);
#75092=ORIENTED_EDGE('',*,*,#53395,.T.);
#75093=ORIENTED_EDGE('',*,*,#53396,.T.);
#75094=ORIENTED_EDGE('',*,*,#53397,.T.);
#75095=ORIENTED_EDGE('',*,*,#53398,.T.);
#75096=ORIENTED_EDGE('',*,*,#53399,.T.);
#75097=ORIENTED_EDGE('',*,*,#53400,.T.);
#75098=ORIENTED_EDGE('',*,*,#53401,.T.);
#75099=ORIENTED_EDGE('',*,*,#53402,.T.);
#75100=ORIENTED_EDGE('',*,*,#53403,.F.);
#75101=ORIENTED_EDGE('',*,*,#53404,.F.);
#75102=ORIENTED_EDGE('',*,*,#53405,.F.);
#75103=ORIENTED_EDGE('',*,*,#53406,.T.);
#75104=ORIENTED_EDGE('',*,*,#53404,.T.);
#75105=ORIENTED_EDGE('',*,*,#53407,.T.);
#75106=ORIENTED_EDGE('',*,*,#53408,.T.);
#75107=ORIENTED_EDGE('',*,*,#53409,.T.);
#75108=ORIENTED_EDGE('',*,*,#52726,.F.);
#75109=ORIENTED_EDGE('',*,*,#53410,.T.);
#75110=ORIENTED_EDGE('',*,*,#53388,.F.);
#75111=ORIENTED_EDGE('',*,*,#53411,.T.);
#75112=ORIENTED_EDGE('',*,*,#53408,.F.);
#75113=ORIENTED_EDGE('',*,*,#53412,.T.);
#75114=ORIENTED_EDGE('',*,*,#52301,.F.);
#75115=ORIENTED_EDGE('',*,*,#53413,.T.);
#75116=ORIENTED_EDGE('',*,*,#53399,.F.);
#75117=ORIENTED_EDGE('',*,*,#53414,.T.);
#75118=ORIENTED_EDGE('',*,*,#53401,.F.);
#75119=ORIENTED_EDGE('',*,*,#53415,.T.);
#75120=ORIENTED_EDGE('',*,*,#53395,.F.);
#75121=ORIENTED_EDGE('',*,*,#53416,.T.);
#75122=ORIENTED_EDGE('',*,*,#53397,.F.);
#75123=ORIENTED_EDGE('',*,*,#53417,.T.);
#75124=ORIENTED_EDGE('',*,*,#53418,.T.);
#75125=ORIENTED_EDGE('',*,*,#53419,.T.);
#75126=ORIENTED_EDGE('',*,*,#53420,.F.);
#75127=ORIENTED_EDGE('',*,*,#53421,.F.);
#75128=ORIENTED_EDGE('',*,*,#53422,.F.);
#75129=ORIENTED_EDGE('',*,*,#53423,.T.);
#75130=ORIENTED_EDGE('',*,*,#53421,.T.);
#75131=ORIENTED_EDGE('',*,*,#53424,.T.);
#75132=ORIENTED_EDGE('',*,*,#53425,.T.);
#75133=ORIENTED_EDGE('',*,*,#53426,.T.);
#75134=ORIENTED_EDGE('',*,*,#53427,.T.);
#75135=ORIENTED_EDGE('',*,*,#53428,.T.);
#75136=ORIENTED_EDGE('',*,*,#53429,.T.);
#75137=ORIENTED_EDGE('',*,*,#53430,.T.);
#75138=ORIENTED_EDGE('',*,*,#53431,.T.);
#75139=ORIENTED_EDGE('',*,*,#53432,.T.);
#75140=ORIENTED_EDGE('',*,*,#53433,.F.);
#75141=ORIENTED_EDGE('',*,*,#53434,.F.);
#75142=ORIENTED_EDGE('',*,*,#53435,.F.);
#75143=ORIENTED_EDGE('',*,*,#53436,.T.);
#75144=ORIENTED_EDGE('',*,*,#53434,.T.);
#75145=ORIENTED_EDGE('',*,*,#53437,.T.);
#75146=ORIENTED_EDGE('',*,*,#53438,.T.);
#75147=ORIENTED_EDGE('',*,*,#53439,.T.);
#75148=ORIENTED_EDGE('',*,*,#52732,.F.);
#75149=ORIENTED_EDGE('',*,*,#53440,.T.);
#75150=ORIENTED_EDGE('',*,*,#53418,.F.);
#75151=ORIENTED_EDGE('',*,*,#53441,.T.);
#75152=ORIENTED_EDGE('',*,*,#53438,.F.);
#75153=ORIENTED_EDGE('',*,*,#53442,.T.);
#75154=ORIENTED_EDGE('',*,*,#52295,.F.);
#75155=ORIENTED_EDGE('',*,*,#53443,.T.);
#75156=ORIENTED_EDGE('',*,*,#53429,.F.);
#75157=ORIENTED_EDGE('',*,*,#53444,.T.);
#75158=ORIENTED_EDGE('',*,*,#53431,.F.);
#75159=ORIENTED_EDGE('',*,*,#53445,.T.);
#75160=ORIENTED_EDGE('',*,*,#53425,.F.);
#75161=ORIENTED_EDGE('',*,*,#53446,.T.);
#75162=ORIENTED_EDGE('',*,*,#53427,.F.);
#75163=ORIENTED_EDGE('',*,*,#53447,.T.);
#75164=ORIENTED_EDGE('',*,*,#53448,.T.);
#75165=ORIENTED_EDGE('',*,*,#53449,.T.);
#75166=ORIENTED_EDGE('',*,*,#53450,.F.);
#75167=ORIENTED_EDGE('',*,*,#53451,.F.);
#75168=ORIENTED_EDGE('',*,*,#53452,.F.);
#75169=ORIENTED_EDGE('',*,*,#53453,.T.);
#75170=ORIENTED_EDGE('',*,*,#53451,.T.);
#75171=ORIENTED_EDGE('',*,*,#53454,.T.);
#75172=ORIENTED_EDGE('',*,*,#53455,.T.);
#75173=ORIENTED_EDGE('',*,*,#53456,.T.);
#75174=ORIENTED_EDGE('',*,*,#53457,.T.);
#75175=ORIENTED_EDGE('',*,*,#53458,.T.);
#75176=ORIENTED_EDGE('',*,*,#53459,.T.);
#75177=ORIENTED_EDGE('',*,*,#53460,.T.);
#75178=ORIENTED_EDGE('',*,*,#53461,.T.);
#75179=ORIENTED_EDGE('',*,*,#53462,.T.);
#75180=ORIENTED_EDGE('',*,*,#53463,.F.);
#75181=ORIENTED_EDGE('',*,*,#53464,.F.);
#75182=ORIENTED_EDGE('',*,*,#53465,.F.);
#75183=ORIENTED_EDGE('',*,*,#53466,.T.);
#75184=ORIENTED_EDGE('',*,*,#53464,.T.);
#75185=ORIENTED_EDGE('',*,*,#53467,.T.);
#75186=ORIENTED_EDGE('',*,*,#53468,.T.);
#75187=ORIENTED_EDGE('',*,*,#53469,.T.);
#75188=ORIENTED_EDGE('',*,*,#52738,.F.);
#75189=ORIENTED_EDGE('',*,*,#53470,.T.);
#75190=ORIENTED_EDGE('',*,*,#53448,.F.);
#75191=ORIENTED_EDGE('',*,*,#53471,.T.);
#75192=ORIENTED_EDGE('',*,*,#53468,.F.);
#75193=ORIENTED_EDGE('',*,*,#53472,.T.);
#75194=ORIENTED_EDGE('',*,*,#52289,.F.);
#75195=ORIENTED_EDGE('',*,*,#53473,.T.);
#75196=ORIENTED_EDGE('',*,*,#53459,.F.);
#75197=ORIENTED_EDGE('',*,*,#53474,.T.);
#75198=ORIENTED_EDGE('',*,*,#53461,.F.);
#75199=ORIENTED_EDGE('',*,*,#53475,.T.);
#75200=ORIENTED_EDGE('',*,*,#53455,.F.);
#75201=ORIENTED_EDGE('',*,*,#53476,.T.);
#75202=ORIENTED_EDGE('',*,*,#53457,.F.);
#75203=ORIENTED_EDGE('',*,*,#53477,.T.);
#75204=ORIENTED_EDGE('',*,*,#53478,.T.);
#75205=ORIENTED_EDGE('',*,*,#53479,.T.);
#75206=ORIENTED_EDGE('',*,*,#53480,.F.);
#75207=ORIENTED_EDGE('',*,*,#53481,.F.);
#75208=ORIENTED_EDGE('',*,*,#53482,.F.);
#75209=ORIENTED_EDGE('',*,*,#53483,.T.);
#75210=ORIENTED_EDGE('',*,*,#53481,.T.);
#75211=ORIENTED_EDGE('',*,*,#53484,.T.);
#75212=ORIENTED_EDGE('',*,*,#53485,.T.);
#75213=ORIENTED_EDGE('',*,*,#53486,.T.);
#75214=ORIENTED_EDGE('',*,*,#53487,.T.);
#75215=ORIENTED_EDGE('',*,*,#53488,.T.);
#75216=ORIENTED_EDGE('',*,*,#53489,.T.);
#75217=ORIENTED_EDGE('',*,*,#53490,.T.);
#75218=ORIENTED_EDGE('',*,*,#53491,.T.);
#75219=ORIENTED_EDGE('',*,*,#53492,.T.);
#75220=ORIENTED_EDGE('',*,*,#53493,.F.);
#75221=ORIENTED_EDGE('',*,*,#53494,.F.);
#75222=ORIENTED_EDGE('',*,*,#53495,.F.);
#75223=ORIENTED_EDGE('',*,*,#53496,.T.);
#75224=ORIENTED_EDGE('',*,*,#53494,.T.);
#75225=ORIENTED_EDGE('',*,*,#53497,.T.);
#75226=ORIENTED_EDGE('',*,*,#53498,.T.);
#75227=ORIENTED_EDGE('',*,*,#53499,.T.);
#75228=ORIENTED_EDGE('',*,*,#52744,.F.);
#75229=ORIENTED_EDGE('',*,*,#53500,.T.);
#75230=ORIENTED_EDGE('',*,*,#53478,.F.);
#75231=ORIENTED_EDGE('',*,*,#53501,.T.);
#75232=ORIENTED_EDGE('',*,*,#53498,.F.);
#75233=ORIENTED_EDGE('',*,*,#53502,.T.);
#75234=ORIENTED_EDGE('',*,*,#52283,.F.);
#75235=ORIENTED_EDGE('',*,*,#53503,.T.);
#75236=ORIENTED_EDGE('',*,*,#53489,.F.);
#75237=ORIENTED_EDGE('',*,*,#53504,.T.);
#75238=ORIENTED_EDGE('',*,*,#53491,.F.);
#75239=ORIENTED_EDGE('',*,*,#53505,.T.);
#75240=ORIENTED_EDGE('',*,*,#53485,.F.);
#75241=ORIENTED_EDGE('',*,*,#53506,.T.);
#75242=ORIENTED_EDGE('',*,*,#53487,.F.);
#75243=ORIENTED_EDGE('',*,*,#53507,.T.);
#75244=ORIENTED_EDGE('',*,*,#53508,.T.);
#75245=ORIENTED_EDGE('',*,*,#53509,.T.);
#75246=ORIENTED_EDGE('',*,*,#53510,.F.);
#75247=ORIENTED_EDGE('',*,*,#53511,.F.);
#75248=ORIENTED_EDGE('',*,*,#53512,.F.);
#75249=ORIENTED_EDGE('',*,*,#53513,.T.);
#75250=ORIENTED_EDGE('',*,*,#53511,.T.);
#75251=ORIENTED_EDGE('',*,*,#53514,.T.);
#75252=ORIENTED_EDGE('',*,*,#53515,.T.);
#75253=ORIENTED_EDGE('',*,*,#53516,.T.);
#75254=ORIENTED_EDGE('',*,*,#53517,.T.);
#75255=ORIENTED_EDGE('',*,*,#53518,.T.);
#75256=ORIENTED_EDGE('',*,*,#53519,.T.);
#75257=ORIENTED_EDGE('',*,*,#53520,.T.);
#75258=ORIENTED_EDGE('',*,*,#53521,.T.);
#75259=ORIENTED_EDGE('',*,*,#53522,.T.);
#75260=ORIENTED_EDGE('',*,*,#53523,.F.);
#75261=ORIENTED_EDGE('',*,*,#53524,.F.);
#75262=ORIENTED_EDGE('',*,*,#53525,.F.);
#75263=ORIENTED_EDGE('',*,*,#53526,.T.);
#75264=ORIENTED_EDGE('',*,*,#53524,.T.);
#75265=ORIENTED_EDGE('',*,*,#53527,.T.);
#75266=ORIENTED_EDGE('',*,*,#53528,.T.);
#75267=ORIENTED_EDGE('',*,*,#53529,.T.);
#75268=ORIENTED_EDGE('',*,*,#52750,.F.);
#75269=ORIENTED_EDGE('',*,*,#53530,.T.);
#75270=ORIENTED_EDGE('',*,*,#53508,.F.);
#75271=ORIENTED_EDGE('',*,*,#53531,.T.);
#75272=ORIENTED_EDGE('',*,*,#53528,.F.);
#75273=ORIENTED_EDGE('',*,*,#53532,.T.);
#75274=ORIENTED_EDGE('',*,*,#52277,.F.);
#75275=ORIENTED_EDGE('',*,*,#53533,.T.);
#75276=ORIENTED_EDGE('',*,*,#53519,.F.);
#75277=ORIENTED_EDGE('',*,*,#53534,.T.);
#75278=ORIENTED_EDGE('',*,*,#53521,.F.);
#75279=ORIENTED_EDGE('',*,*,#53535,.T.);
#75280=ORIENTED_EDGE('',*,*,#53515,.F.);
#75281=ORIENTED_EDGE('',*,*,#53536,.T.);
#75282=ORIENTED_EDGE('',*,*,#53517,.F.);
#75283=ORIENTED_EDGE('',*,*,#53537,.T.);
#75284=ORIENTED_EDGE('',*,*,#53538,.T.);
#75285=ORIENTED_EDGE('',*,*,#53539,.T.);
#75286=ORIENTED_EDGE('',*,*,#53540,.F.);
#75287=ORIENTED_EDGE('',*,*,#53541,.F.);
#75288=ORIENTED_EDGE('',*,*,#53542,.F.);
#75289=ORIENTED_EDGE('',*,*,#53543,.T.);
#75290=ORIENTED_EDGE('',*,*,#53541,.T.);
#75291=ORIENTED_EDGE('',*,*,#53544,.T.);
#75292=ORIENTED_EDGE('',*,*,#53545,.T.);
#75293=ORIENTED_EDGE('',*,*,#53546,.T.);
#75294=ORIENTED_EDGE('',*,*,#53547,.T.);
#75295=ORIENTED_EDGE('',*,*,#53548,.T.);
#75296=ORIENTED_EDGE('',*,*,#53549,.T.);
#75297=ORIENTED_EDGE('',*,*,#53550,.T.);
#75298=ORIENTED_EDGE('',*,*,#53551,.T.);
#75299=ORIENTED_EDGE('',*,*,#53552,.T.);
#75300=ORIENTED_EDGE('',*,*,#53553,.F.);
#75301=ORIENTED_EDGE('',*,*,#53554,.F.);
#75302=ORIENTED_EDGE('',*,*,#53555,.F.);
#75303=ORIENTED_EDGE('',*,*,#53556,.T.);
#75304=ORIENTED_EDGE('',*,*,#53554,.T.);
#75305=ORIENTED_EDGE('',*,*,#53557,.T.);
#75306=ORIENTED_EDGE('',*,*,#53558,.T.);
#75307=ORIENTED_EDGE('',*,*,#53559,.T.);
#75308=ORIENTED_EDGE('',*,*,#52756,.F.);
#75309=ORIENTED_EDGE('',*,*,#53560,.T.);
#75310=ORIENTED_EDGE('',*,*,#53538,.F.);
#75311=ORIENTED_EDGE('',*,*,#53561,.T.);
#75312=ORIENTED_EDGE('',*,*,#53558,.F.);
#75313=ORIENTED_EDGE('',*,*,#53562,.T.);
#75314=ORIENTED_EDGE('',*,*,#52271,.F.);
#75315=ORIENTED_EDGE('',*,*,#53563,.T.);
#75316=ORIENTED_EDGE('',*,*,#53549,.F.);
#75317=ORIENTED_EDGE('',*,*,#53564,.T.);
#75318=ORIENTED_EDGE('',*,*,#53551,.F.);
#75319=ORIENTED_EDGE('',*,*,#53565,.T.);
#75320=ORIENTED_EDGE('',*,*,#53545,.F.);
#75321=ORIENTED_EDGE('',*,*,#53566,.T.);
#75322=ORIENTED_EDGE('',*,*,#53547,.F.);
#75323=ORIENTED_EDGE('',*,*,#53567,.T.);
#75324=ORIENTED_EDGE('',*,*,#53568,.T.);
#75325=ORIENTED_EDGE('',*,*,#53569,.T.);
#75326=ORIENTED_EDGE('',*,*,#53570,.F.);
#75327=ORIENTED_EDGE('',*,*,#53571,.F.);
#75328=ORIENTED_EDGE('',*,*,#53572,.F.);
#75329=ORIENTED_EDGE('',*,*,#53573,.T.);
#75330=ORIENTED_EDGE('',*,*,#53571,.T.);
#75331=ORIENTED_EDGE('',*,*,#53574,.T.);
#75332=ORIENTED_EDGE('',*,*,#53575,.T.);
#75333=ORIENTED_EDGE('',*,*,#53576,.T.);
#75334=ORIENTED_EDGE('',*,*,#53577,.T.);
#75335=ORIENTED_EDGE('',*,*,#53578,.T.);
#75336=ORIENTED_EDGE('',*,*,#53579,.T.);
#75337=ORIENTED_EDGE('',*,*,#53580,.T.);
#75338=ORIENTED_EDGE('',*,*,#53581,.T.);
#75339=ORIENTED_EDGE('',*,*,#53582,.T.);
#75340=ORIENTED_EDGE('',*,*,#53583,.F.);
#75341=ORIENTED_EDGE('',*,*,#53584,.F.);
#75342=ORIENTED_EDGE('',*,*,#53585,.F.);
#75343=ORIENTED_EDGE('',*,*,#53586,.T.);
#75344=ORIENTED_EDGE('',*,*,#53584,.T.);
#75345=ORIENTED_EDGE('',*,*,#53587,.T.);
#75346=ORIENTED_EDGE('',*,*,#53588,.T.);
#75347=ORIENTED_EDGE('',*,*,#53589,.T.);
#75348=ORIENTED_EDGE('',*,*,#52762,.F.);
#75349=ORIENTED_EDGE('',*,*,#53590,.T.);
#75350=ORIENTED_EDGE('',*,*,#53568,.F.);
#75351=ORIENTED_EDGE('',*,*,#53591,.T.);
#75352=ORIENTED_EDGE('',*,*,#53588,.F.);
#75353=ORIENTED_EDGE('',*,*,#53592,.T.);
#75354=ORIENTED_EDGE('',*,*,#52265,.F.);
#75355=ORIENTED_EDGE('',*,*,#53593,.T.);
#75356=ORIENTED_EDGE('',*,*,#53579,.F.);
#75357=ORIENTED_EDGE('',*,*,#53594,.T.);
#75358=ORIENTED_EDGE('',*,*,#53581,.F.);
#75359=ORIENTED_EDGE('',*,*,#53595,.T.);
#75360=ORIENTED_EDGE('',*,*,#53575,.F.);
#75361=ORIENTED_EDGE('',*,*,#53596,.T.);
#75362=ORIENTED_EDGE('',*,*,#53577,.F.);
#75363=ORIENTED_EDGE('',*,*,#53597,.T.);
#75364=ORIENTED_EDGE('',*,*,#53598,.T.);
#75365=ORIENTED_EDGE('',*,*,#53599,.T.);
#75366=ORIENTED_EDGE('',*,*,#53600,.F.);
#75367=ORIENTED_EDGE('',*,*,#53601,.F.);
#75368=ORIENTED_EDGE('',*,*,#53602,.F.);
#75369=ORIENTED_EDGE('',*,*,#53603,.T.);
#75370=ORIENTED_EDGE('',*,*,#53601,.T.);
#75371=ORIENTED_EDGE('',*,*,#53604,.T.);
#75372=ORIENTED_EDGE('',*,*,#53605,.T.);
#75373=ORIENTED_EDGE('',*,*,#53606,.T.);
#75374=ORIENTED_EDGE('',*,*,#53607,.T.);
#75375=ORIENTED_EDGE('',*,*,#53608,.T.);
#75376=ORIENTED_EDGE('',*,*,#53609,.T.);
#75377=ORIENTED_EDGE('',*,*,#53610,.T.);
#75378=ORIENTED_EDGE('',*,*,#53611,.T.);
#75379=ORIENTED_EDGE('',*,*,#53612,.T.);
#75380=ORIENTED_EDGE('',*,*,#53613,.F.);
#75381=ORIENTED_EDGE('',*,*,#53614,.F.);
#75382=ORIENTED_EDGE('',*,*,#53615,.F.);
#75383=ORIENTED_EDGE('',*,*,#53616,.T.);
#75384=ORIENTED_EDGE('',*,*,#53614,.T.);
#75385=ORIENTED_EDGE('',*,*,#53617,.T.);
#75386=ORIENTED_EDGE('',*,*,#53618,.T.);
#75387=ORIENTED_EDGE('',*,*,#53619,.T.);
#75388=ORIENTED_EDGE('',*,*,#52768,.F.);
#75389=ORIENTED_EDGE('',*,*,#53620,.T.);
#75390=ORIENTED_EDGE('',*,*,#53598,.F.);
#75391=ORIENTED_EDGE('',*,*,#53621,.T.);
#75392=ORIENTED_EDGE('',*,*,#53618,.F.);
#75393=ORIENTED_EDGE('',*,*,#53622,.T.);
#75394=ORIENTED_EDGE('',*,*,#52259,.F.);
#75395=ORIENTED_EDGE('',*,*,#53623,.T.);
#75396=ORIENTED_EDGE('',*,*,#53609,.F.);
#75397=ORIENTED_EDGE('',*,*,#53624,.T.);
#75398=ORIENTED_EDGE('',*,*,#53611,.F.);
#75399=ORIENTED_EDGE('',*,*,#53625,.T.);
#75400=ORIENTED_EDGE('',*,*,#53605,.F.);
#75401=ORIENTED_EDGE('',*,*,#53626,.T.);
#75402=ORIENTED_EDGE('',*,*,#53607,.F.);
#75403=ORIENTED_EDGE('',*,*,#53627,.T.);
#75404=ORIENTED_EDGE('',*,*,#53628,.T.);
#75405=ORIENTED_EDGE('',*,*,#53629,.T.);
#75406=ORIENTED_EDGE('',*,*,#53630,.F.);
#75407=ORIENTED_EDGE('',*,*,#53631,.F.);
#75408=ORIENTED_EDGE('',*,*,#53632,.F.);
#75409=ORIENTED_EDGE('',*,*,#53633,.T.);
#75410=ORIENTED_EDGE('',*,*,#53631,.T.);
#75411=ORIENTED_EDGE('',*,*,#53634,.T.);
#75412=ORIENTED_EDGE('',*,*,#53635,.T.);
#75413=ORIENTED_EDGE('',*,*,#53636,.T.);
#75414=ORIENTED_EDGE('',*,*,#53637,.T.);
#75415=ORIENTED_EDGE('',*,*,#53638,.T.);
#75416=ORIENTED_EDGE('',*,*,#53639,.T.);
#75417=ORIENTED_EDGE('',*,*,#53640,.T.);
#75418=ORIENTED_EDGE('',*,*,#53641,.T.);
#75419=ORIENTED_EDGE('',*,*,#53642,.T.);
#75420=ORIENTED_EDGE('',*,*,#53643,.F.);
#75421=ORIENTED_EDGE('',*,*,#53644,.F.);
#75422=ORIENTED_EDGE('',*,*,#53645,.F.);
#75423=ORIENTED_EDGE('',*,*,#53646,.T.);
#75424=ORIENTED_EDGE('',*,*,#53644,.T.);
#75425=ORIENTED_EDGE('',*,*,#53647,.T.);
#75426=ORIENTED_EDGE('',*,*,#53648,.T.);
#75427=ORIENTED_EDGE('',*,*,#53649,.T.);
#75428=ORIENTED_EDGE('',*,*,#52774,.F.);
#75429=ORIENTED_EDGE('',*,*,#53650,.T.);
#75430=ORIENTED_EDGE('',*,*,#53628,.F.);
#75431=ORIENTED_EDGE('',*,*,#53651,.T.);
#75432=ORIENTED_EDGE('',*,*,#53648,.F.);
#75433=ORIENTED_EDGE('',*,*,#53652,.T.);
#75434=ORIENTED_EDGE('',*,*,#52253,.F.);
#75435=ORIENTED_EDGE('',*,*,#53653,.T.);
#75436=ORIENTED_EDGE('',*,*,#53639,.F.);
#75437=ORIENTED_EDGE('',*,*,#53654,.T.);
#75438=ORIENTED_EDGE('',*,*,#53641,.F.);
#75439=ORIENTED_EDGE('',*,*,#53655,.T.);
#75440=ORIENTED_EDGE('',*,*,#53635,.F.);
#75441=ORIENTED_EDGE('',*,*,#53656,.T.);
#75442=ORIENTED_EDGE('',*,*,#53637,.F.);
#75443=ORIENTED_EDGE('',*,*,#53657,.T.);
#75444=ORIENTED_EDGE('',*,*,#53658,.T.);
#75445=ORIENTED_EDGE('',*,*,#53659,.T.);
#75446=ORIENTED_EDGE('',*,*,#53660,.F.);
#75447=ORIENTED_EDGE('',*,*,#53661,.F.);
#75448=ORIENTED_EDGE('',*,*,#53662,.F.);
#75449=ORIENTED_EDGE('',*,*,#53663,.T.);
#75450=ORIENTED_EDGE('',*,*,#53661,.T.);
#75451=ORIENTED_EDGE('',*,*,#53664,.T.);
#75452=ORIENTED_EDGE('',*,*,#53665,.T.);
#75453=ORIENTED_EDGE('',*,*,#53666,.T.);
#75454=ORIENTED_EDGE('',*,*,#53667,.T.);
#75455=ORIENTED_EDGE('',*,*,#53668,.T.);
#75456=ORIENTED_EDGE('',*,*,#53669,.T.);
#75457=ORIENTED_EDGE('',*,*,#53670,.T.);
#75458=ORIENTED_EDGE('',*,*,#53671,.T.);
#75459=ORIENTED_EDGE('',*,*,#53672,.T.);
#75460=ORIENTED_EDGE('',*,*,#53673,.F.);
#75461=ORIENTED_EDGE('',*,*,#53674,.F.);
#75462=ORIENTED_EDGE('',*,*,#53675,.F.);
#75463=ORIENTED_EDGE('',*,*,#53676,.T.);
#75464=ORIENTED_EDGE('',*,*,#53674,.T.);
#75465=ORIENTED_EDGE('',*,*,#53677,.T.);
#75466=ORIENTED_EDGE('',*,*,#53678,.T.);
#75467=ORIENTED_EDGE('',*,*,#53679,.T.);
#75468=ORIENTED_EDGE('',*,*,#52780,.F.);
#75469=ORIENTED_EDGE('',*,*,#53680,.T.);
#75470=ORIENTED_EDGE('',*,*,#53658,.F.);
#75471=ORIENTED_EDGE('',*,*,#53681,.T.);
#75472=ORIENTED_EDGE('',*,*,#53678,.F.);
#75473=ORIENTED_EDGE('',*,*,#53682,.T.);
#75474=ORIENTED_EDGE('',*,*,#52247,.F.);
#75475=ORIENTED_EDGE('',*,*,#53683,.T.);
#75476=ORIENTED_EDGE('',*,*,#53669,.F.);
#75477=ORIENTED_EDGE('',*,*,#53684,.T.);
#75478=ORIENTED_EDGE('',*,*,#53671,.F.);
#75479=ORIENTED_EDGE('',*,*,#53685,.T.);
#75480=ORIENTED_EDGE('',*,*,#53665,.F.);
#75481=ORIENTED_EDGE('',*,*,#53686,.T.);
#75482=ORIENTED_EDGE('',*,*,#53667,.F.);
#75483=ORIENTED_EDGE('',*,*,#53687,.T.);
#75484=ORIENTED_EDGE('',*,*,#53688,.T.);
#75485=ORIENTED_EDGE('',*,*,#53689,.T.);
#75486=ORIENTED_EDGE('',*,*,#53690,.F.);
#75487=ORIENTED_EDGE('',*,*,#53691,.F.);
#75488=ORIENTED_EDGE('',*,*,#53692,.F.);
#75489=ORIENTED_EDGE('',*,*,#53693,.T.);
#75490=ORIENTED_EDGE('',*,*,#53691,.T.);
#75491=ORIENTED_EDGE('',*,*,#53694,.T.);
#75492=ORIENTED_EDGE('',*,*,#53695,.T.);
#75493=ORIENTED_EDGE('',*,*,#53696,.T.);
#75494=ORIENTED_EDGE('',*,*,#53697,.T.);
#75495=ORIENTED_EDGE('',*,*,#53698,.T.);
#75496=ORIENTED_EDGE('',*,*,#53699,.T.);
#75497=ORIENTED_EDGE('',*,*,#53700,.T.);
#75498=ORIENTED_EDGE('',*,*,#53701,.T.);
#75499=ORIENTED_EDGE('',*,*,#53702,.T.);
#75500=ORIENTED_EDGE('',*,*,#53703,.F.);
#75501=ORIENTED_EDGE('',*,*,#53704,.F.);
#75502=ORIENTED_EDGE('',*,*,#53705,.F.);
#75503=ORIENTED_EDGE('',*,*,#53706,.T.);
#75504=ORIENTED_EDGE('',*,*,#53704,.T.);
#75505=ORIENTED_EDGE('',*,*,#53707,.T.);
#75506=ORIENTED_EDGE('',*,*,#53708,.T.);
#75507=ORIENTED_EDGE('',*,*,#53709,.T.);
#75508=ORIENTED_EDGE('',*,*,#52425,.F.);
#75509=ORIENTED_EDGE('',*,*,#53710,.T.);
#75510=ORIENTED_EDGE('',*,*,#53688,.F.);
#75511=ORIENTED_EDGE('',*,*,#53711,.T.);
#75512=ORIENTED_EDGE('',*,*,#53708,.F.);
#75513=ORIENTED_EDGE('',*,*,#53712,.T.);
#75514=ORIENTED_EDGE('',*,*,#52241,.F.);
#75515=ORIENTED_EDGE('',*,*,#53713,.T.);
#75516=ORIENTED_EDGE('',*,*,#53699,.F.);
#75517=ORIENTED_EDGE('',*,*,#53714,.T.);
#75518=ORIENTED_EDGE('',*,*,#53701,.F.);
#75519=ORIENTED_EDGE('',*,*,#53715,.T.);
#75520=ORIENTED_EDGE('',*,*,#53695,.F.);
#75521=ORIENTED_EDGE('',*,*,#53716,.T.);
#75522=ORIENTED_EDGE('',*,*,#53697,.F.);
#75523=ORIENTED_EDGE('',*,*,#53717,.T.);
#75524=ORIENTED_EDGE('',*,*,#53718,.T.);
#75525=ORIENTED_EDGE('',*,*,#53719,.T.);
#75526=ORIENTED_EDGE('',*,*,#53720,.F.);
#75527=ORIENTED_EDGE('',*,*,#53721,.F.);
#75528=ORIENTED_EDGE('',*,*,#53722,.F.);
#75529=ORIENTED_EDGE('',*,*,#53723,.T.);
#75530=ORIENTED_EDGE('',*,*,#53721,.T.);
#75531=ORIENTED_EDGE('',*,*,#53724,.T.);
#75532=ORIENTED_EDGE('',*,*,#53725,.T.);
#75533=ORIENTED_EDGE('',*,*,#53726,.T.);
#75534=ORIENTED_EDGE('',*,*,#53727,.T.);
#75535=ORIENTED_EDGE('',*,*,#53728,.T.);
#75536=ORIENTED_EDGE('',*,*,#53729,.T.);
#75537=ORIENTED_EDGE('',*,*,#53730,.T.);
#75538=ORIENTED_EDGE('',*,*,#53731,.T.);
#75539=ORIENTED_EDGE('',*,*,#53732,.T.);
#75540=ORIENTED_EDGE('',*,*,#53733,.F.);
#75541=ORIENTED_EDGE('',*,*,#53734,.F.);
#75542=ORIENTED_EDGE('',*,*,#53735,.F.);
#75543=ORIENTED_EDGE('',*,*,#53736,.T.);
#75544=ORIENTED_EDGE('',*,*,#53734,.T.);
#75545=ORIENTED_EDGE('',*,*,#53737,.T.);
#75546=ORIENTED_EDGE('',*,*,#53738,.T.);
#75547=ORIENTED_EDGE('',*,*,#53739,.T.);
#75548=ORIENTED_EDGE('',*,*,#52431,.F.);
#75549=ORIENTED_EDGE('',*,*,#53740,.T.);
#75550=ORIENTED_EDGE('',*,*,#53718,.F.);
#75551=ORIENTED_EDGE('',*,*,#53741,.T.);
#75552=ORIENTED_EDGE('',*,*,#53738,.F.);
#75553=ORIENTED_EDGE('',*,*,#53742,.T.);
#75554=ORIENTED_EDGE('',*,*,#52235,.F.);
#75555=ORIENTED_EDGE('',*,*,#53743,.T.);
#75556=ORIENTED_EDGE('',*,*,#53729,.F.);
#75557=ORIENTED_EDGE('',*,*,#53744,.T.);
#75558=ORIENTED_EDGE('',*,*,#53731,.F.);
#75559=ORIENTED_EDGE('',*,*,#53745,.T.);
#75560=ORIENTED_EDGE('',*,*,#53725,.F.);
#75561=ORIENTED_EDGE('',*,*,#53746,.T.);
#75562=ORIENTED_EDGE('',*,*,#53727,.F.);
#75563=ORIENTED_EDGE('',*,*,#53747,.T.);
#75564=ORIENTED_EDGE('',*,*,#53748,.T.);
#75565=ORIENTED_EDGE('',*,*,#53749,.T.);
#75566=ORIENTED_EDGE('',*,*,#53750,.F.);
#75567=ORIENTED_EDGE('',*,*,#53751,.F.);
#75568=ORIENTED_EDGE('',*,*,#53752,.F.);
#75569=ORIENTED_EDGE('',*,*,#53753,.T.);
#75570=ORIENTED_EDGE('',*,*,#53751,.T.);
#75571=ORIENTED_EDGE('',*,*,#53754,.T.);
#75572=ORIENTED_EDGE('',*,*,#53755,.T.);
#75573=ORIENTED_EDGE('',*,*,#53756,.T.);
#75574=ORIENTED_EDGE('',*,*,#53757,.T.);
#75575=ORIENTED_EDGE('',*,*,#53758,.T.);
#75576=ORIENTED_EDGE('',*,*,#53759,.T.);
#75577=ORIENTED_EDGE('',*,*,#53760,.T.);
#75578=ORIENTED_EDGE('',*,*,#53761,.T.);
#75579=ORIENTED_EDGE('',*,*,#53762,.T.);
#75580=ORIENTED_EDGE('',*,*,#53763,.F.);
#75581=ORIENTED_EDGE('',*,*,#53764,.F.);
#75582=ORIENTED_EDGE('',*,*,#53765,.F.);
#75583=ORIENTED_EDGE('',*,*,#53766,.T.);
#75584=ORIENTED_EDGE('',*,*,#53764,.T.);
#75585=ORIENTED_EDGE('',*,*,#53767,.T.);
#75586=ORIENTED_EDGE('',*,*,#53768,.T.);
#75587=ORIENTED_EDGE('',*,*,#53769,.T.);
#75588=ORIENTED_EDGE('',*,*,#52437,.F.);
#75589=ORIENTED_EDGE('',*,*,#53770,.T.);
#75590=ORIENTED_EDGE('',*,*,#53748,.F.);
#75591=ORIENTED_EDGE('',*,*,#53771,.T.);
#75592=ORIENTED_EDGE('',*,*,#53768,.F.);
#75593=ORIENTED_EDGE('',*,*,#53772,.T.);
#75594=ORIENTED_EDGE('',*,*,#52229,.F.);
#75595=ORIENTED_EDGE('',*,*,#53773,.T.);
#75596=ORIENTED_EDGE('',*,*,#53759,.F.);
#75597=ORIENTED_EDGE('',*,*,#53774,.T.);
#75598=ORIENTED_EDGE('',*,*,#53761,.F.);
#75599=ORIENTED_EDGE('',*,*,#53775,.T.);
#75600=ORIENTED_EDGE('',*,*,#53755,.F.);
#75601=ORIENTED_EDGE('',*,*,#53776,.T.);
#75602=ORIENTED_EDGE('',*,*,#53757,.F.);
#75603=ORIENTED_EDGE('',*,*,#53777,.T.);
#75604=ORIENTED_EDGE('',*,*,#53778,.T.);
#75605=ORIENTED_EDGE('',*,*,#53779,.T.);
#75606=ORIENTED_EDGE('',*,*,#53780,.F.);
#75607=ORIENTED_EDGE('',*,*,#53781,.F.);
#75608=ORIENTED_EDGE('',*,*,#53782,.F.);
#75609=ORIENTED_EDGE('',*,*,#53783,.T.);
#75610=ORIENTED_EDGE('',*,*,#53781,.T.);
#75611=ORIENTED_EDGE('',*,*,#53784,.T.);
#75612=ORIENTED_EDGE('',*,*,#53785,.T.);
#75613=ORIENTED_EDGE('',*,*,#53786,.T.);
#75614=ORIENTED_EDGE('',*,*,#53787,.T.);
#75615=ORIENTED_EDGE('',*,*,#53788,.T.);
#75616=ORIENTED_EDGE('',*,*,#53789,.T.);
#75617=ORIENTED_EDGE('',*,*,#53790,.T.);
#75618=ORIENTED_EDGE('',*,*,#53791,.T.);
#75619=ORIENTED_EDGE('',*,*,#53792,.T.);
#75620=ORIENTED_EDGE('',*,*,#53793,.F.);
#75621=ORIENTED_EDGE('',*,*,#53794,.F.);
#75622=ORIENTED_EDGE('',*,*,#53795,.F.);
#75623=ORIENTED_EDGE('',*,*,#53796,.T.);
#75624=ORIENTED_EDGE('',*,*,#53794,.T.);
#75625=ORIENTED_EDGE('',*,*,#53797,.T.);
#75626=ORIENTED_EDGE('',*,*,#53798,.T.);
#75627=ORIENTED_EDGE('',*,*,#53799,.T.);
#75628=ORIENTED_EDGE('',*,*,#52443,.F.);
#75629=ORIENTED_EDGE('',*,*,#53800,.T.);
#75630=ORIENTED_EDGE('',*,*,#53778,.F.);
#75631=ORIENTED_EDGE('',*,*,#53801,.T.);
#75632=ORIENTED_EDGE('',*,*,#53798,.F.);
#75633=ORIENTED_EDGE('',*,*,#53802,.T.);
#75634=ORIENTED_EDGE('',*,*,#52223,.F.);
#75635=ORIENTED_EDGE('',*,*,#53803,.T.);
#75636=ORIENTED_EDGE('',*,*,#53789,.F.);
#75637=ORIENTED_EDGE('',*,*,#53804,.T.);
#75638=ORIENTED_EDGE('',*,*,#53791,.F.);
#75639=ORIENTED_EDGE('',*,*,#53805,.T.);
#75640=ORIENTED_EDGE('',*,*,#53785,.F.);
#75641=ORIENTED_EDGE('',*,*,#53806,.T.);
#75642=ORIENTED_EDGE('',*,*,#53787,.F.);
#75643=ORIENTED_EDGE('',*,*,#53807,.T.);
#75644=ORIENTED_EDGE('',*,*,#53808,.T.);
#75645=ORIENTED_EDGE('',*,*,#53809,.T.);
#75646=ORIENTED_EDGE('',*,*,#53810,.F.);
#75647=ORIENTED_EDGE('',*,*,#53811,.F.);
#75648=ORIENTED_EDGE('',*,*,#53812,.F.);
#75649=ORIENTED_EDGE('',*,*,#53813,.T.);
#75650=ORIENTED_EDGE('',*,*,#53811,.T.);
#75651=ORIENTED_EDGE('',*,*,#53814,.T.);
#75652=ORIENTED_EDGE('',*,*,#53815,.T.);
#75653=ORIENTED_EDGE('',*,*,#53816,.T.);
#75654=ORIENTED_EDGE('',*,*,#53817,.T.);
#75655=ORIENTED_EDGE('',*,*,#53818,.T.);
#75656=ORIENTED_EDGE('',*,*,#53819,.T.);
#75657=ORIENTED_EDGE('',*,*,#53820,.T.);
#75658=ORIENTED_EDGE('',*,*,#53821,.T.);
#75659=ORIENTED_EDGE('',*,*,#53822,.T.);
#75660=ORIENTED_EDGE('',*,*,#53823,.F.);
#75661=ORIENTED_EDGE('',*,*,#53824,.F.);
#75662=ORIENTED_EDGE('',*,*,#53825,.F.);
#75663=ORIENTED_EDGE('',*,*,#53826,.T.);
#75664=ORIENTED_EDGE('',*,*,#53824,.T.);
#75665=ORIENTED_EDGE('',*,*,#53827,.T.);
#75666=ORIENTED_EDGE('',*,*,#53828,.T.);
#75667=ORIENTED_EDGE('',*,*,#53829,.T.);
#75668=ORIENTED_EDGE('',*,*,#52449,.F.);
#75669=ORIENTED_EDGE('',*,*,#53830,.T.);
#75670=ORIENTED_EDGE('',*,*,#53808,.F.);
#75671=ORIENTED_EDGE('',*,*,#53831,.T.);
#75672=ORIENTED_EDGE('',*,*,#53828,.F.);
#75673=ORIENTED_EDGE('',*,*,#53832,.T.);
#75674=ORIENTED_EDGE('',*,*,#52217,.F.);
#75675=ORIENTED_EDGE('',*,*,#53833,.T.);
#75676=ORIENTED_EDGE('',*,*,#53819,.F.);
#75677=ORIENTED_EDGE('',*,*,#53834,.T.);
#75678=ORIENTED_EDGE('',*,*,#53821,.F.);
#75679=ORIENTED_EDGE('',*,*,#53835,.T.);
#75680=ORIENTED_EDGE('',*,*,#53815,.F.);
#75681=ORIENTED_EDGE('',*,*,#53836,.T.);
#75682=ORIENTED_EDGE('',*,*,#53817,.F.);
#75683=ORIENTED_EDGE('',*,*,#53837,.T.);
#75684=ORIENTED_EDGE('',*,*,#53838,.T.);
#75685=ORIENTED_EDGE('',*,*,#53839,.T.);
#75686=ORIENTED_EDGE('',*,*,#53840,.F.);
#75687=ORIENTED_EDGE('',*,*,#53841,.F.);
#75688=ORIENTED_EDGE('',*,*,#53842,.F.);
#75689=ORIENTED_EDGE('',*,*,#53843,.T.);
#75690=ORIENTED_EDGE('',*,*,#53841,.T.);
#75691=ORIENTED_EDGE('',*,*,#53844,.T.);
#75692=ORIENTED_EDGE('',*,*,#53845,.T.);
#75693=ORIENTED_EDGE('',*,*,#53846,.T.);
#75694=ORIENTED_EDGE('',*,*,#53847,.T.);
#75695=ORIENTED_EDGE('',*,*,#53848,.T.);
#75696=ORIENTED_EDGE('',*,*,#53849,.T.);
#75697=ORIENTED_EDGE('',*,*,#53850,.T.);
#75698=ORIENTED_EDGE('',*,*,#53851,.T.);
#75699=ORIENTED_EDGE('',*,*,#53852,.T.);
#75700=ORIENTED_EDGE('',*,*,#53853,.F.);
#75701=ORIENTED_EDGE('',*,*,#53854,.F.);
#75702=ORIENTED_EDGE('',*,*,#53855,.F.);
#75703=ORIENTED_EDGE('',*,*,#53856,.T.);
#75704=ORIENTED_EDGE('',*,*,#53854,.T.);
#75705=ORIENTED_EDGE('',*,*,#53857,.T.);
#75706=ORIENTED_EDGE('',*,*,#53858,.T.);
#75707=ORIENTED_EDGE('',*,*,#53859,.T.);
#75708=ORIENTED_EDGE('',*,*,#52455,.F.);
#75709=ORIENTED_EDGE('',*,*,#53860,.T.);
#75710=ORIENTED_EDGE('',*,*,#53838,.F.);
#75711=ORIENTED_EDGE('',*,*,#53861,.T.);
#75712=ORIENTED_EDGE('',*,*,#53858,.F.);
#75713=ORIENTED_EDGE('',*,*,#53862,.T.);
#75714=ORIENTED_EDGE('',*,*,#52211,.F.);
#75715=ORIENTED_EDGE('',*,*,#53863,.T.);
#75716=ORIENTED_EDGE('',*,*,#53849,.F.);
#75717=ORIENTED_EDGE('',*,*,#53864,.T.);
#75718=ORIENTED_EDGE('',*,*,#53851,.F.);
#75719=ORIENTED_EDGE('',*,*,#53865,.T.);
#75720=ORIENTED_EDGE('',*,*,#53845,.F.);
#75721=ORIENTED_EDGE('',*,*,#53866,.T.);
#75722=ORIENTED_EDGE('',*,*,#53847,.F.);
#75723=ORIENTED_EDGE('',*,*,#53867,.T.);
#75724=ORIENTED_EDGE('',*,*,#53868,.T.);
#75725=ORIENTED_EDGE('',*,*,#53869,.T.);
#75726=ORIENTED_EDGE('',*,*,#53870,.F.);
#75727=ORIENTED_EDGE('',*,*,#53871,.F.);
#75728=ORIENTED_EDGE('',*,*,#53872,.F.);
#75729=ORIENTED_EDGE('',*,*,#53873,.T.);
#75730=ORIENTED_EDGE('',*,*,#53871,.T.);
#75731=ORIENTED_EDGE('',*,*,#53874,.T.);
#75732=ORIENTED_EDGE('',*,*,#53875,.T.);
#75733=ORIENTED_EDGE('',*,*,#53876,.T.);
#75734=ORIENTED_EDGE('',*,*,#53877,.T.);
#75735=ORIENTED_EDGE('',*,*,#53878,.T.);
#75736=ORIENTED_EDGE('',*,*,#53879,.T.);
#75737=ORIENTED_EDGE('',*,*,#53880,.T.);
#75738=ORIENTED_EDGE('',*,*,#53881,.T.);
#75739=ORIENTED_EDGE('',*,*,#53882,.T.);
#75740=ORIENTED_EDGE('',*,*,#53883,.F.);
#75741=ORIENTED_EDGE('',*,*,#53884,.F.);
#75742=ORIENTED_EDGE('',*,*,#53885,.F.);
#75743=ORIENTED_EDGE('',*,*,#53886,.T.);
#75744=ORIENTED_EDGE('',*,*,#53884,.T.);
#75745=ORIENTED_EDGE('',*,*,#53887,.T.);
#75746=ORIENTED_EDGE('',*,*,#53888,.T.);
#75747=ORIENTED_EDGE('',*,*,#53889,.T.);
#75748=ORIENTED_EDGE('',*,*,#52461,.F.);
#75749=ORIENTED_EDGE('',*,*,#53890,.T.);
#75750=ORIENTED_EDGE('',*,*,#53868,.F.);
#75751=ORIENTED_EDGE('',*,*,#53891,.T.);
#75752=ORIENTED_EDGE('',*,*,#53888,.F.);
#75753=ORIENTED_EDGE('',*,*,#53892,.T.);
#75754=ORIENTED_EDGE('',*,*,#52205,.F.);
#75755=ORIENTED_EDGE('',*,*,#53893,.T.);
#75756=ORIENTED_EDGE('',*,*,#53879,.F.);
#75757=ORIENTED_EDGE('',*,*,#53894,.T.);
#75758=ORIENTED_EDGE('',*,*,#53881,.F.);
#75759=ORIENTED_EDGE('',*,*,#53895,.T.);
#75760=ORIENTED_EDGE('',*,*,#53875,.F.);
#75761=ORIENTED_EDGE('',*,*,#53896,.T.);
#75762=ORIENTED_EDGE('',*,*,#53877,.F.);
#75763=ORIENTED_EDGE('',*,*,#53897,.T.);
#75764=ORIENTED_EDGE('',*,*,#53898,.T.);
#75765=ORIENTED_EDGE('',*,*,#53899,.T.);
#75766=ORIENTED_EDGE('',*,*,#53900,.F.);
#75767=ORIENTED_EDGE('',*,*,#53901,.F.);
#75768=ORIENTED_EDGE('',*,*,#53902,.F.);
#75769=ORIENTED_EDGE('',*,*,#53903,.T.);
#75770=ORIENTED_EDGE('',*,*,#53901,.T.);
#75771=ORIENTED_EDGE('',*,*,#53904,.T.);
#75772=ORIENTED_EDGE('',*,*,#53905,.T.);
#75773=ORIENTED_EDGE('',*,*,#53906,.T.);
#75774=ORIENTED_EDGE('',*,*,#53907,.T.);
#75775=ORIENTED_EDGE('',*,*,#53908,.T.);
#75776=ORIENTED_EDGE('',*,*,#53909,.T.);
#75777=ORIENTED_EDGE('',*,*,#53910,.T.);
#75778=ORIENTED_EDGE('',*,*,#53911,.T.);
#75779=ORIENTED_EDGE('',*,*,#53912,.T.);
#75780=ORIENTED_EDGE('',*,*,#53913,.F.);
#75781=ORIENTED_EDGE('',*,*,#53914,.F.);
#75782=ORIENTED_EDGE('',*,*,#53915,.F.);
#75783=ORIENTED_EDGE('',*,*,#53916,.T.);
#75784=ORIENTED_EDGE('',*,*,#53914,.T.);
#75785=ORIENTED_EDGE('',*,*,#53917,.T.);
#75786=ORIENTED_EDGE('',*,*,#53918,.T.);
#75787=ORIENTED_EDGE('',*,*,#53919,.T.);
#75788=ORIENTED_EDGE('',*,*,#52467,.F.);
#75789=ORIENTED_EDGE('',*,*,#53920,.T.);
#75790=ORIENTED_EDGE('',*,*,#53898,.F.);
#75791=ORIENTED_EDGE('',*,*,#53921,.T.);
#75792=ORIENTED_EDGE('',*,*,#53918,.F.);
#75793=ORIENTED_EDGE('',*,*,#53922,.T.);
#75794=ORIENTED_EDGE('',*,*,#52199,.F.);
#75795=ORIENTED_EDGE('',*,*,#53923,.T.);
#75796=ORIENTED_EDGE('',*,*,#53909,.F.);
#75797=ORIENTED_EDGE('',*,*,#53924,.T.);
#75798=ORIENTED_EDGE('',*,*,#53911,.F.);
#75799=ORIENTED_EDGE('',*,*,#53925,.T.);
#75800=ORIENTED_EDGE('',*,*,#53905,.F.);
#75801=ORIENTED_EDGE('',*,*,#53926,.T.);
#75802=ORIENTED_EDGE('',*,*,#53907,.F.);
#75803=ORIENTED_EDGE('',*,*,#53927,.T.);
#75804=ORIENTED_EDGE('',*,*,#53928,.T.);
#75805=ORIENTED_EDGE('',*,*,#53929,.T.);
#75806=ORIENTED_EDGE('',*,*,#53930,.F.);
#75807=ORIENTED_EDGE('',*,*,#53931,.F.);
#75808=ORIENTED_EDGE('',*,*,#53932,.F.);
#75809=ORIENTED_EDGE('',*,*,#53933,.T.);
#75810=ORIENTED_EDGE('',*,*,#53931,.T.);
#75811=ORIENTED_EDGE('',*,*,#53934,.T.);
#75812=ORIENTED_EDGE('',*,*,#53935,.T.);
#75813=ORIENTED_EDGE('',*,*,#53936,.T.);
#75814=ORIENTED_EDGE('',*,*,#53937,.T.);
#75815=ORIENTED_EDGE('',*,*,#53938,.T.);
#75816=ORIENTED_EDGE('',*,*,#53939,.T.);
#75817=ORIENTED_EDGE('',*,*,#53940,.T.);
#75818=ORIENTED_EDGE('',*,*,#53941,.T.);
#75819=ORIENTED_EDGE('',*,*,#53942,.T.);
#75820=ORIENTED_EDGE('',*,*,#53943,.F.);
#75821=ORIENTED_EDGE('',*,*,#53944,.F.);
#75822=ORIENTED_EDGE('',*,*,#53945,.F.);
#75823=ORIENTED_EDGE('',*,*,#53946,.T.);
#75824=ORIENTED_EDGE('',*,*,#53944,.T.);
#75825=ORIENTED_EDGE('',*,*,#53947,.T.);
#75826=ORIENTED_EDGE('',*,*,#53948,.T.);
#75827=ORIENTED_EDGE('',*,*,#53949,.T.);
#75828=ORIENTED_EDGE('',*,*,#52473,.F.);
#75829=ORIENTED_EDGE('',*,*,#53950,.T.);
#75830=ORIENTED_EDGE('',*,*,#53928,.F.);
#75831=ORIENTED_EDGE('',*,*,#53951,.T.);
#75832=ORIENTED_EDGE('',*,*,#53948,.F.);
#75833=ORIENTED_EDGE('',*,*,#53952,.T.);
#75834=ORIENTED_EDGE('',*,*,#52193,.F.);
#75835=ORIENTED_EDGE('',*,*,#53953,.T.);
#75836=ORIENTED_EDGE('',*,*,#53939,.F.);
#75837=ORIENTED_EDGE('',*,*,#53954,.T.);
#75838=ORIENTED_EDGE('',*,*,#53941,.F.);
#75839=ORIENTED_EDGE('',*,*,#53955,.T.);
#75840=ORIENTED_EDGE('',*,*,#53935,.F.);
#75841=ORIENTED_EDGE('',*,*,#53956,.T.);
#75842=ORIENTED_EDGE('',*,*,#53937,.F.);
#75843=ORIENTED_EDGE('',*,*,#53957,.T.);
#75844=ORIENTED_EDGE('',*,*,#53958,.T.);
#75845=ORIENTED_EDGE('',*,*,#53959,.T.);
#75846=ORIENTED_EDGE('',*,*,#53960,.F.);
#75847=ORIENTED_EDGE('',*,*,#53961,.F.);
#75848=ORIENTED_EDGE('',*,*,#53962,.F.);
#75849=ORIENTED_EDGE('',*,*,#53963,.T.);
#75850=ORIENTED_EDGE('',*,*,#53961,.T.);
#75851=ORIENTED_EDGE('',*,*,#53964,.T.);
#75852=ORIENTED_EDGE('',*,*,#53965,.T.);
#75853=ORIENTED_EDGE('',*,*,#53966,.T.);
#75854=ORIENTED_EDGE('',*,*,#53967,.T.);
#75855=ORIENTED_EDGE('',*,*,#53968,.T.);
#75856=ORIENTED_EDGE('',*,*,#53969,.T.);
#75857=ORIENTED_EDGE('',*,*,#53970,.T.);
#75858=ORIENTED_EDGE('',*,*,#53971,.T.);
#75859=ORIENTED_EDGE('',*,*,#53972,.T.);
#75860=ORIENTED_EDGE('',*,*,#53973,.F.);
#75861=ORIENTED_EDGE('',*,*,#53974,.F.);
#75862=ORIENTED_EDGE('',*,*,#53975,.F.);
#75863=ORIENTED_EDGE('',*,*,#53976,.T.);
#75864=ORIENTED_EDGE('',*,*,#53974,.T.);
#75865=ORIENTED_EDGE('',*,*,#53977,.T.);
#75866=ORIENTED_EDGE('',*,*,#53978,.T.);
#75867=ORIENTED_EDGE('',*,*,#53979,.T.);
#75868=ORIENTED_EDGE('',*,*,#52479,.F.);
#75869=ORIENTED_EDGE('',*,*,#53980,.T.);
#75870=ORIENTED_EDGE('',*,*,#53958,.F.);
#75871=ORIENTED_EDGE('',*,*,#53981,.T.);
#75872=ORIENTED_EDGE('',*,*,#53978,.F.);
#75873=ORIENTED_EDGE('',*,*,#53982,.T.);
#75874=ORIENTED_EDGE('',*,*,#52187,.F.);
#75875=ORIENTED_EDGE('',*,*,#53983,.T.);
#75876=ORIENTED_EDGE('',*,*,#53969,.F.);
#75877=ORIENTED_EDGE('',*,*,#53984,.T.);
#75878=ORIENTED_EDGE('',*,*,#53971,.F.);
#75879=ORIENTED_EDGE('',*,*,#53985,.T.);
#75880=ORIENTED_EDGE('',*,*,#53965,.F.);
#75881=ORIENTED_EDGE('',*,*,#53986,.T.);
#75882=ORIENTED_EDGE('',*,*,#53967,.F.);
#75883=ORIENTED_EDGE('',*,*,#53987,.T.);
#75884=ORIENTED_EDGE('',*,*,#53988,.T.);
#75885=ORIENTED_EDGE('',*,*,#53989,.T.);
#75886=ORIENTED_EDGE('',*,*,#53990,.F.);
#75887=ORIENTED_EDGE('',*,*,#53991,.F.);
#75888=ORIENTED_EDGE('',*,*,#53992,.F.);
#75889=ORIENTED_EDGE('',*,*,#53993,.T.);
#75890=ORIENTED_EDGE('',*,*,#53991,.T.);
#75891=ORIENTED_EDGE('',*,*,#53994,.T.);
#75892=ORIENTED_EDGE('',*,*,#53995,.T.);
#75893=ORIENTED_EDGE('',*,*,#53996,.T.);
#75894=ORIENTED_EDGE('',*,*,#53997,.T.);
#75895=ORIENTED_EDGE('',*,*,#53998,.T.);
#75896=ORIENTED_EDGE('',*,*,#53999,.T.);
#75897=ORIENTED_EDGE('',*,*,#54000,.T.);
#75898=ORIENTED_EDGE('',*,*,#54001,.T.);
#75899=ORIENTED_EDGE('',*,*,#54002,.T.);
#75900=ORIENTED_EDGE('',*,*,#54003,.F.);
#75901=ORIENTED_EDGE('',*,*,#54004,.F.);
#75902=ORIENTED_EDGE('',*,*,#54005,.F.);
#75903=ORIENTED_EDGE('',*,*,#54006,.T.);
#75904=ORIENTED_EDGE('',*,*,#54004,.T.);
#75905=ORIENTED_EDGE('',*,*,#54007,.T.);
#75906=ORIENTED_EDGE('',*,*,#54008,.T.);
#75907=ORIENTED_EDGE('',*,*,#54009,.T.);
#75908=ORIENTED_EDGE('',*,*,#52485,.F.);
#75909=ORIENTED_EDGE('',*,*,#54010,.T.);
#75910=ORIENTED_EDGE('',*,*,#53988,.F.);
#75911=ORIENTED_EDGE('',*,*,#54011,.T.);
#75912=ORIENTED_EDGE('',*,*,#54008,.F.);
#75913=ORIENTED_EDGE('',*,*,#54012,.T.);
#75914=ORIENTED_EDGE('',*,*,#52181,.F.);
#75915=ORIENTED_EDGE('',*,*,#54013,.T.);
#75916=ORIENTED_EDGE('',*,*,#53999,.F.);
#75917=ORIENTED_EDGE('',*,*,#54014,.T.);
#75918=ORIENTED_EDGE('',*,*,#54001,.F.);
#75919=ORIENTED_EDGE('',*,*,#54015,.T.);
#75920=ORIENTED_EDGE('',*,*,#53995,.F.);
#75921=ORIENTED_EDGE('',*,*,#54016,.T.);
#75922=ORIENTED_EDGE('',*,*,#53997,.F.);
#75923=ORIENTED_EDGE('',*,*,#54017,.T.);
#75924=ORIENTED_EDGE('',*,*,#54018,.T.);
#75925=ORIENTED_EDGE('',*,*,#54019,.T.);
#75926=ORIENTED_EDGE('',*,*,#54020,.F.);
#75927=ORIENTED_EDGE('',*,*,#54021,.F.);
#75928=ORIENTED_EDGE('',*,*,#54022,.F.);
#75929=ORIENTED_EDGE('',*,*,#54023,.T.);
#75930=ORIENTED_EDGE('',*,*,#54021,.T.);
#75931=ORIENTED_EDGE('',*,*,#54024,.T.);
#75932=ORIENTED_EDGE('',*,*,#54025,.T.);
#75933=ORIENTED_EDGE('',*,*,#54026,.T.);
#75934=ORIENTED_EDGE('',*,*,#54027,.T.);
#75935=ORIENTED_EDGE('',*,*,#54028,.T.);
#75936=ORIENTED_EDGE('',*,*,#54029,.T.);
#75937=ORIENTED_EDGE('',*,*,#54030,.T.);
#75938=ORIENTED_EDGE('',*,*,#54031,.T.);
#75939=ORIENTED_EDGE('',*,*,#54032,.T.);
#75940=ORIENTED_EDGE('',*,*,#54033,.F.);
#75941=ORIENTED_EDGE('',*,*,#54034,.F.);
#75942=ORIENTED_EDGE('',*,*,#54035,.F.);
#75943=ORIENTED_EDGE('',*,*,#54036,.T.);
#75944=ORIENTED_EDGE('',*,*,#54034,.T.);
#75945=ORIENTED_EDGE('',*,*,#54037,.T.);
#75946=ORIENTED_EDGE('',*,*,#54038,.T.);
#75947=ORIENTED_EDGE('',*,*,#54039,.T.);
#75948=ORIENTED_EDGE('',*,*,#52491,.F.);
#75949=ORIENTED_EDGE('',*,*,#54040,.T.);
#75950=ORIENTED_EDGE('',*,*,#54018,.F.);
#75951=ORIENTED_EDGE('',*,*,#54041,.T.);
#75952=ORIENTED_EDGE('',*,*,#54038,.F.);
#75953=ORIENTED_EDGE('',*,*,#54042,.T.);
#75954=ORIENTED_EDGE('',*,*,#52175,.F.);
#75955=ORIENTED_EDGE('',*,*,#54043,.T.);
#75956=ORIENTED_EDGE('',*,*,#54029,.F.);
#75957=ORIENTED_EDGE('',*,*,#54044,.T.);
#75958=ORIENTED_EDGE('',*,*,#54031,.F.);
#75959=ORIENTED_EDGE('',*,*,#54045,.T.);
#75960=ORIENTED_EDGE('',*,*,#54025,.F.);
#75961=ORIENTED_EDGE('',*,*,#54046,.T.);
#75962=ORIENTED_EDGE('',*,*,#54027,.F.);
#75963=ORIENTED_EDGE('',*,*,#54047,.T.);
#75964=ORIENTED_EDGE('',*,*,#54048,.T.);
#75965=ORIENTED_EDGE('',*,*,#54049,.T.);
#75966=ORIENTED_EDGE('',*,*,#54050,.F.);
#75967=ORIENTED_EDGE('',*,*,#54051,.F.);
#75968=ORIENTED_EDGE('',*,*,#54052,.F.);
#75969=ORIENTED_EDGE('',*,*,#54053,.T.);
#75970=ORIENTED_EDGE('',*,*,#54051,.T.);
#75971=ORIENTED_EDGE('',*,*,#54054,.T.);
#75972=ORIENTED_EDGE('',*,*,#54055,.T.);
#75973=ORIENTED_EDGE('',*,*,#54056,.T.);
#75974=ORIENTED_EDGE('',*,*,#54057,.T.);
#75975=ORIENTED_EDGE('',*,*,#54058,.T.);
#75976=ORIENTED_EDGE('',*,*,#54059,.T.);
#75977=ORIENTED_EDGE('',*,*,#54060,.T.);
#75978=ORIENTED_EDGE('',*,*,#54061,.T.);
#75979=ORIENTED_EDGE('',*,*,#54062,.T.);
#75980=ORIENTED_EDGE('',*,*,#54063,.F.);
#75981=ORIENTED_EDGE('',*,*,#54064,.F.);
#75982=ORIENTED_EDGE('',*,*,#54065,.F.);
#75983=ORIENTED_EDGE('',*,*,#54066,.T.);
#75984=ORIENTED_EDGE('',*,*,#54064,.T.);
#75985=ORIENTED_EDGE('',*,*,#54067,.T.);
#75986=ORIENTED_EDGE('',*,*,#54068,.T.);
#75987=ORIENTED_EDGE('',*,*,#54069,.T.);
#75988=ORIENTED_EDGE('',*,*,#52497,.F.);
#75989=ORIENTED_EDGE('',*,*,#54070,.T.);
#75990=ORIENTED_EDGE('',*,*,#54048,.F.);
#75991=ORIENTED_EDGE('',*,*,#54071,.T.);
#75992=ORIENTED_EDGE('',*,*,#54068,.F.);
#75993=ORIENTED_EDGE('',*,*,#54072,.T.);
#75994=ORIENTED_EDGE('',*,*,#52169,.F.);
#75995=ORIENTED_EDGE('',*,*,#54073,.T.);
#75996=ORIENTED_EDGE('',*,*,#54059,.F.);
#75997=ORIENTED_EDGE('',*,*,#54074,.T.);
#75998=ORIENTED_EDGE('',*,*,#54061,.F.);
#75999=ORIENTED_EDGE('',*,*,#54075,.T.);
#76000=ORIENTED_EDGE('',*,*,#54055,.F.);
#76001=ORIENTED_EDGE('',*,*,#54076,.T.);
#76002=ORIENTED_EDGE('',*,*,#54057,.F.);
#76003=ORIENTED_EDGE('',*,*,#54077,.T.);
#76004=ORIENTED_EDGE('',*,*,#54078,.T.);
#76005=ORIENTED_EDGE('',*,*,#54079,.T.);
#76006=ORIENTED_EDGE('',*,*,#54080,.F.);
#76007=ORIENTED_EDGE('',*,*,#54081,.F.);
#76008=ORIENTED_EDGE('',*,*,#54082,.F.);
#76009=ORIENTED_EDGE('',*,*,#54083,.T.);
#76010=ORIENTED_EDGE('',*,*,#54081,.T.);
#76011=ORIENTED_EDGE('',*,*,#54084,.T.);
#76012=ORIENTED_EDGE('',*,*,#54085,.T.);
#76013=ORIENTED_EDGE('',*,*,#54086,.T.);
#76014=ORIENTED_EDGE('',*,*,#54087,.T.);
#76015=ORIENTED_EDGE('',*,*,#54088,.T.);
#76016=ORIENTED_EDGE('',*,*,#54089,.T.);
#76017=ORIENTED_EDGE('',*,*,#54090,.T.);
#76018=ORIENTED_EDGE('',*,*,#54091,.T.);
#76019=ORIENTED_EDGE('',*,*,#54092,.T.);
#76020=ORIENTED_EDGE('',*,*,#54093,.F.);
#76021=ORIENTED_EDGE('',*,*,#54094,.F.);
#76022=ORIENTED_EDGE('',*,*,#54095,.F.);
#76023=ORIENTED_EDGE('',*,*,#54096,.T.);
#76024=ORIENTED_EDGE('',*,*,#54094,.T.);
#76025=ORIENTED_EDGE('',*,*,#54097,.T.);
#76026=ORIENTED_EDGE('',*,*,#54098,.T.);
#76027=ORIENTED_EDGE('',*,*,#54099,.T.);
#76028=ORIENTED_EDGE('',*,*,#52503,.F.);
#76029=ORIENTED_EDGE('',*,*,#54100,.T.);
#76030=ORIENTED_EDGE('',*,*,#54078,.F.);
#76031=ORIENTED_EDGE('',*,*,#54101,.T.);
#76032=ORIENTED_EDGE('',*,*,#54098,.F.);
#76033=ORIENTED_EDGE('',*,*,#54102,.T.);
#76034=ORIENTED_EDGE('',*,*,#52163,.F.);
#76035=ORIENTED_EDGE('',*,*,#54103,.T.);
#76036=ORIENTED_EDGE('',*,*,#54089,.F.);
#76037=ORIENTED_EDGE('',*,*,#54104,.T.);
#76038=ORIENTED_EDGE('',*,*,#54091,.F.);
#76039=ORIENTED_EDGE('',*,*,#54105,.T.);
#76040=ORIENTED_EDGE('',*,*,#54085,.F.);
#76041=ORIENTED_EDGE('',*,*,#54106,.T.);
#76042=ORIENTED_EDGE('',*,*,#54087,.F.);
#76043=ORIENTED_EDGE('',*,*,#54107,.T.);
#76044=ORIENTED_EDGE('',*,*,#54108,.T.);
#76045=ORIENTED_EDGE('',*,*,#54109,.T.);
#76046=ORIENTED_EDGE('',*,*,#54110,.F.);
#76047=ORIENTED_EDGE('',*,*,#54111,.F.);
#76048=ORIENTED_EDGE('',*,*,#54112,.F.);
#76049=ORIENTED_EDGE('',*,*,#54113,.T.);
#76050=ORIENTED_EDGE('',*,*,#54111,.T.);
#76051=ORIENTED_EDGE('',*,*,#54114,.T.);
#76052=ORIENTED_EDGE('',*,*,#54115,.T.);
#76053=ORIENTED_EDGE('',*,*,#54116,.T.);
#76054=ORIENTED_EDGE('',*,*,#54117,.T.);
#76055=ORIENTED_EDGE('',*,*,#54118,.T.);
#76056=ORIENTED_EDGE('',*,*,#54119,.T.);
#76057=ORIENTED_EDGE('',*,*,#54120,.T.);
#76058=ORIENTED_EDGE('',*,*,#54121,.T.);
#76059=ORIENTED_EDGE('',*,*,#54122,.T.);
#76060=ORIENTED_EDGE('',*,*,#54123,.F.);
#76061=ORIENTED_EDGE('',*,*,#54124,.F.);
#76062=ORIENTED_EDGE('',*,*,#54125,.F.);
#76063=ORIENTED_EDGE('',*,*,#54126,.T.);
#76064=ORIENTED_EDGE('',*,*,#54124,.T.);
#76065=ORIENTED_EDGE('',*,*,#54127,.T.);
#76066=ORIENTED_EDGE('',*,*,#54128,.T.);
#76067=ORIENTED_EDGE('',*,*,#54129,.T.);
#76068=ORIENTED_EDGE('',*,*,#52509,.F.);
#76069=ORIENTED_EDGE('',*,*,#54130,.T.);
#76070=ORIENTED_EDGE('',*,*,#54108,.F.);
#76071=ORIENTED_EDGE('',*,*,#54131,.T.);
#76072=ORIENTED_EDGE('',*,*,#54128,.F.);
#76073=ORIENTED_EDGE('',*,*,#54132,.T.);
#76074=ORIENTED_EDGE('',*,*,#52157,.F.);
#76075=ORIENTED_EDGE('',*,*,#54133,.T.);
#76076=ORIENTED_EDGE('',*,*,#54119,.F.);
#76077=ORIENTED_EDGE('',*,*,#54134,.T.);
#76078=ORIENTED_EDGE('',*,*,#54121,.F.);
#76079=ORIENTED_EDGE('',*,*,#54135,.T.);
#76080=ORIENTED_EDGE('',*,*,#54115,.F.);
#76081=ORIENTED_EDGE('',*,*,#54136,.T.);
#76082=ORIENTED_EDGE('',*,*,#54117,.F.);
#76083=ORIENTED_EDGE('',*,*,#54137,.T.);
#76084=ORIENTED_EDGE('',*,*,#54138,.T.);
#76085=ORIENTED_EDGE('',*,*,#54139,.T.);
#76086=ORIENTED_EDGE('',*,*,#54140,.F.);
#76087=ORIENTED_EDGE('',*,*,#54141,.F.);
#76088=ORIENTED_EDGE('',*,*,#54142,.F.);
#76089=ORIENTED_EDGE('',*,*,#54143,.T.);
#76090=ORIENTED_EDGE('',*,*,#54141,.T.);
#76091=ORIENTED_EDGE('',*,*,#54144,.T.);
#76092=ORIENTED_EDGE('',*,*,#54145,.T.);
#76093=ORIENTED_EDGE('',*,*,#54146,.T.);
#76094=ORIENTED_EDGE('',*,*,#54147,.T.);
#76095=ORIENTED_EDGE('',*,*,#54148,.T.);
#76096=ORIENTED_EDGE('',*,*,#54149,.T.);
#76097=ORIENTED_EDGE('',*,*,#54150,.T.);
#76098=ORIENTED_EDGE('',*,*,#54151,.T.);
#76099=ORIENTED_EDGE('',*,*,#54152,.T.);
#76100=ORIENTED_EDGE('',*,*,#54153,.F.);
#76101=ORIENTED_EDGE('',*,*,#54154,.F.);
#76102=ORIENTED_EDGE('',*,*,#54155,.F.);
#76103=ORIENTED_EDGE('',*,*,#54156,.T.);
#76104=ORIENTED_EDGE('',*,*,#54154,.T.);
#76105=ORIENTED_EDGE('',*,*,#54157,.T.);
#76106=ORIENTED_EDGE('',*,*,#54158,.T.);
#76107=ORIENTED_EDGE('',*,*,#54159,.T.);
#76108=ORIENTED_EDGE('',*,*,#52515,.F.);
#76109=ORIENTED_EDGE('',*,*,#54160,.T.);
#76110=ORIENTED_EDGE('',*,*,#54138,.F.);
#76111=ORIENTED_EDGE('',*,*,#54161,.T.);
#76112=ORIENTED_EDGE('',*,*,#54158,.F.);
#76113=ORIENTED_EDGE('',*,*,#54162,.T.);
#76114=ORIENTED_EDGE('',*,*,#52151,.F.);
#76115=ORIENTED_EDGE('',*,*,#54163,.T.);
#76116=ORIENTED_EDGE('',*,*,#54149,.F.);
#76117=ORIENTED_EDGE('',*,*,#54164,.T.);
#76118=ORIENTED_EDGE('',*,*,#54151,.F.);
#76119=ORIENTED_EDGE('',*,*,#54165,.T.);
#76120=ORIENTED_EDGE('',*,*,#54145,.F.);
#76121=ORIENTED_EDGE('',*,*,#54166,.T.);
#76122=ORIENTED_EDGE('',*,*,#54147,.F.);
#76123=ORIENTED_EDGE('',*,*,#54167,.T.);
#76124=ORIENTED_EDGE('',*,*,#54168,.T.);
#76125=ORIENTED_EDGE('',*,*,#54169,.T.);
#76126=ORIENTED_EDGE('',*,*,#54170,.F.);
#76127=ORIENTED_EDGE('',*,*,#54171,.F.);
#76128=ORIENTED_EDGE('',*,*,#54172,.F.);
#76129=ORIENTED_EDGE('',*,*,#54173,.T.);
#76130=ORIENTED_EDGE('',*,*,#54171,.T.);
#76131=ORIENTED_EDGE('',*,*,#54174,.T.);
#76132=ORIENTED_EDGE('',*,*,#54175,.T.);
#76133=ORIENTED_EDGE('',*,*,#54176,.T.);
#76134=ORIENTED_EDGE('',*,*,#54177,.T.);
#76135=ORIENTED_EDGE('',*,*,#54178,.T.);
#76136=ORIENTED_EDGE('',*,*,#54179,.T.);
#76137=ORIENTED_EDGE('',*,*,#54180,.T.);
#76138=ORIENTED_EDGE('',*,*,#54181,.T.);
#76139=ORIENTED_EDGE('',*,*,#54182,.T.);
#76140=ORIENTED_EDGE('',*,*,#54183,.F.);
#76141=ORIENTED_EDGE('',*,*,#54184,.F.);
#76142=ORIENTED_EDGE('',*,*,#54185,.F.);
#76143=ORIENTED_EDGE('',*,*,#54186,.T.);
#76144=ORIENTED_EDGE('',*,*,#54184,.T.);
#76145=ORIENTED_EDGE('',*,*,#54187,.T.);
#76146=ORIENTED_EDGE('',*,*,#54188,.T.);
#76147=ORIENTED_EDGE('',*,*,#54189,.T.);
#76148=ORIENTED_EDGE('',*,*,#52521,.F.);
#76149=ORIENTED_EDGE('',*,*,#54190,.T.);
#76150=ORIENTED_EDGE('',*,*,#54168,.F.);
#76151=ORIENTED_EDGE('',*,*,#54191,.T.);
#76152=ORIENTED_EDGE('',*,*,#54188,.F.);
#76153=ORIENTED_EDGE('',*,*,#54192,.T.);
#76154=ORIENTED_EDGE('',*,*,#52145,.F.);
#76155=ORIENTED_EDGE('',*,*,#54193,.T.);
#76156=ORIENTED_EDGE('',*,*,#54179,.F.);
#76157=ORIENTED_EDGE('',*,*,#54194,.T.);
#76158=ORIENTED_EDGE('',*,*,#54181,.F.);
#76159=ORIENTED_EDGE('',*,*,#54195,.T.);
#76160=ORIENTED_EDGE('',*,*,#54175,.F.);
#76161=ORIENTED_EDGE('',*,*,#54196,.T.);
#76162=ORIENTED_EDGE('',*,*,#54177,.F.);
#76163=ORIENTED_EDGE('',*,*,#54197,.T.);
#76164=ORIENTED_EDGE('',*,*,#54198,.T.);
#76165=ORIENTED_EDGE('',*,*,#54199,.T.);
#76166=ORIENTED_EDGE('',*,*,#54200,.F.);
#76167=ORIENTED_EDGE('',*,*,#54201,.F.);
#76168=ORIENTED_EDGE('',*,*,#54202,.F.);
#76169=ORIENTED_EDGE('',*,*,#54203,.T.);
#76170=ORIENTED_EDGE('',*,*,#54201,.T.);
#76171=ORIENTED_EDGE('',*,*,#54204,.T.);
#76172=ORIENTED_EDGE('',*,*,#54205,.T.);
#76173=ORIENTED_EDGE('',*,*,#54206,.T.);
#76174=ORIENTED_EDGE('',*,*,#54207,.T.);
#76175=ORIENTED_EDGE('',*,*,#54208,.T.);
#76176=ORIENTED_EDGE('',*,*,#54209,.T.);
#76177=ORIENTED_EDGE('',*,*,#54210,.T.);
#76178=ORIENTED_EDGE('',*,*,#54211,.T.);
#76179=ORIENTED_EDGE('',*,*,#54212,.T.);
#76180=ORIENTED_EDGE('',*,*,#54213,.F.);
#76181=ORIENTED_EDGE('',*,*,#54214,.F.);
#76182=ORIENTED_EDGE('',*,*,#54215,.F.);
#76183=ORIENTED_EDGE('',*,*,#54216,.T.);
#76184=ORIENTED_EDGE('',*,*,#54214,.T.);
#76185=ORIENTED_EDGE('',*,*,#54217,.T.);
#76186=ORIENTED_EDGE('',*,*,#54218,.T.);
#76187=ORIENTED_EDGE('',*,*,#54219,.T.);
#76188=ORIENTED_EDGE('',*,*,#52527,.F.);
#76189=ORIENTED_EDGE('',*,*,#54220,.T.);
#76190=ORIENTED_EDGE('',*,*,#54198,.F.);
#76191=ORIENTED_EDGE('',*,*,#54221,.T.);
#76192=ORIENTED_EDGE('',*,*,#54218,.F.);
#76193=ORIENTED_EDGE('',*,*,#54222,.T.);
#76194=ORIENTED_EDGE('',*,*,#52139,.F.);
#76195=ORIENTED_EDGE('',*,*,#54223,.T.);
#76196=ORIENTED_EDGE('',*,*,#54209,.F.);
#76197=ORIENTED_EDGE('',*,*,#54224,.T.);
#76198=ORIENTED_EDGE('',*,*,#54211,.F.);
#76199=ORIENTED_EDGE('',*,*,#54225,.T.);
#76200=ORIENTED_EDGE('',*,*,#54205,.F.);
#76201=ORIENTED_EDGE('',*,*,#54226,.T.);
#76202=ORIENTED_EDGE('',*,*,#54207,.F.);
#76203=ORIENTED_EDGE('',*,*,#54227,.T.);
#76204=ORIENTED_EDGE('',*,*,#54228,.T.);
#76205=ORIENTED_EDGE('',*,*,#54229,.T.);
#76206=ORIENTED_EDGE('',*,*,#54230,.F.);
#76207=ORIENTED_EDGE('',*,*,#54231,.F.);
#76208=ORIENTED_EDGE('',*,*,#54232,.F.);
#76209=ORIENTED_EDGE('',*,*,#54233,.T.);
#76210=ORIENTED_EDGE('',*,*,#54231,.T.);
#76211=ORIENTED_EDGE('',*,*,#54234,.T.);
#76212=ORIENTED_EDGE('',*,*,#54235,.T.);
#76213=ORIENTED_EDGE('',*,*,#54236,.T.);
#76214=ORIENTED_EDGE('',*,*,#54237,.T.);
#76215=ORIENTED_EDGE('',*,*,#54238,.T.);
#76216=ORIENTED_EDGE('',*,*,#54239,.T.);
#76217=ORIENTED_EDGE('',*,*,#54240,.T.);
#76218=ORIENTED_EDGE('',*,*,#54241,.T.);
#76219=ORIENTED_EDGE('',*,*,#54242,.T.);
#76220=ORIENTED_EDGE('',*,*,#54243,.F.);
#76221=ORIENTED_EDGE('',*,*,#54244,.F.);
#76222=ORIENTED_EDGE('',*,*,#54245,.F.);
#76223=ORIENTED_EDGE('',*,*,#54246,.T.);
#76224=ORIENTED_EDGE('',*,*,#54244,.T.);
#76225=ORIENTED_EDGE('',*,*,#54247,.T.);
#76226=ORIENTED_EDGE('',*,*,#54248,.T.);
#76227=ORIENTED_EDGE('',*,*,#54249,.T.);
#76228=ORIENTED_EDGE('',*,*,#52533,.F.);
#76229=ORIENTED_EDGE('',*,*,#54250,.T.);
#76230=ORIENTED_EDGE('',*,*,#54228,.F.);
#76231=ORIENTED_EDGE('',*,*,#54251,.T.);
#76232=ORIENTED_EDGE('',*,*,#54248,.F.);
#76233=ORIENTED_EDGE('',*,*,#54252,.T.);
#76234=ORIENTED_EDGE('',*,*,#52133,.F.);
#76235=ORIENTED_EDGE('',*,*,#54253,.T.);
#76236=ORIENTED_EDGE('',*,*,#54239,.F.);
#76237=ORIENTED_EDGE('',*,*,#54254,.T.);
#76238=ORIENTED_EDGE('',*,*,#54241,.F.);
#76239=ORIENTED_EDGE('',*,*,#54255,.T.);
#76240=ORIENTED_EDGE('',*,*,#54235,.F.);
#76241=ORIENTED_EDGE('',*,*,#54256,.T.);
#76242=ORIENTED_EDGE('',*,*,#54237,.F.);
#76243=ORIENTED_EDGE('',*,*,#54257,.T.);
#76244=ORIENTED_EDGE('',*,*,#54258,.T.);
#76245=ORIENTED_EDGE('',*,*,#54259,.T.);
#76246=ORIENTED_EDGE('',*,*,#54260,.F.);
#76247=ORIENTED_EDGE('',*,*,#54261,.F.);
#76248=ORIENTED_EDGE('',*,*,#54262,.F.);
#76249=ORIENTED_EDGE('',*,*,#54263,.T.);
#76250=ORIENTED_EDGE('',*,*,#54261,.T.);
#76251=ORIENTED_EDGE('',*,*,#54264,.T.);
#76252=ORIENTED_EDGE('',*,*,#54265,.T.);
#76253=ORIENTED_EDGE('',*,*,#54266,.T.);
#76254=ORIENTED_EDGE('',*,*,#54267,.T.);
#76255=ORIENTED_EDGE('',*,*,#54268,.T.);
#76256=ORIENTED_EDGE('',*,*,#54269,.T.);
#76257=ORIENTED_EDGE('',*,*,#54270,.T.);
#76258=ORIENTED_EDGE('',*,*,#54271,.T.);
#76259=ORIENTED_EDGE('',*,*,#54272,.T.);
#76260=ORIENTED_EDGE('',*,*,#54273,.F.);
#76261=ORIENTED_EDGE('',*,*,#54274,.F.);
#76262=ORIENTED_EDGE('',*,*,#54275,.F.);
#76263=ORIENTED_EDGE('',*,*,#54276,.T.);
#76264=ORIENTED_EDGE('',*,*,#54274,.T.);
#76265=ORIENTED_EDGE('',*,*,#54277,.T.);
#76266=ORIENTED_EDGE('',*,*,#54278,.T.);
#76267=ORIENTED_EDGE('',*,*,#54279,.T.);
#76268=ORIENTED_EDGE('',*,*,#52539,.F.);
#76269=ORIENTED_EDGE('',*,*,#54280,.T.);
#76270=ORIENTED_EDGE('',*,*,#54258,.F.);
#76271=ORIENTED_EDGE('',*,*,#54281,.T.);
#76272=ORIENTED_EDGE('',*,*,#54278,.F.);
#76273=ORIENTED_EDGE('',*,*,#54282,.T.);
#76274=ORIENTED_EDGE('',*,*,#52127,.F.);
#76275=ORIENTED_EDGE('',*,*,#54283,.T.);
#76276=ORIENTED_EDGE('',*,*,#54269,.F.);
#76277=ORIENTED_EDGE('',*,*,#54284,.T.);
#76278=ORIENTED_EDGE('',*,*,#54271,.F.);
#76279=ORIENTED_EDGE('',*,*,#54285,.T.);
#76280=ORIENTED_EDGE('',*,*,#54265,.F.);
#76281=ORIENTED_EDGE('',*,*,#54286,.T.);
#76282=ORIENTED_EDGE('',*,*,#54267,.F.);
#76283=ORIENTED_EDGE('',*,*,#54287,.T.);
#76284=ORIENTED_EDGE('',*,*,#54288,.T.);
#76285=ORIENTED_EDGE('',*,*,#54289,.T.);
#76286=ORIENTED_EDGE('',*,*,#54290,.F.);
#76287=ORIENTED_EDGE('',*,*,#54291,.F.);
#76288=ORIENTED_EDGE('',*,*,#54292,.F.);
#76289=ORIENTED_EDGE('',*,*,#54293,.T.);
#76290=ORIENTED_EDGE('',*,*,#54291,.T.);
#76291=ORIENTED_EDGE('',*,*,#54294,.T.);
#76292=ORIENTED_EDGE('',*,*,#54295,.T.);
#76293=ORIENTED_EDGE('',*,*,#54296,.T.);
#76294=ORIENTED_EDGE('',*,*,#54297,.T.);
#76295=ORIENTED_EDGE('',*,*,#54298,.T.);
#76296=ORIENTED_EDGE('',*,*,#54299,.T.);
#76297=ORIENTED_EDGE('',*,*,#54300,.T.);
#76298=ORIENTED_EDGE('',*,*,#54301,.T.);
#76299=ORIENTED_EDGE('',*,*,#54302,.T.);
#76300=ORIENTED_EDGE('',*,*,#54303,.F.);
#76301=ORIENTED_EDGE('',*,*,#54304,.F.);
#76302=ORIENTED_EDGE('',*,*,#54305,.F.);
#76303=ORIENTED_EDGE('',*,*,#54306,.T.);
#76304=ORIENTED_EDGE('',*,*,#54304,.T.);
#76305=ORIENTED_EDGE('',*,*,#54307,.T.);
#76306=ORIENTED_EDGE('',*,*,#54308,.T.);
#76307=ORIENTED_EDGE('',*,*,#54309,.T.);
#76308=ORIENTED_EDGE('',*,*,#52545,.F.);
#76309=ORIENTED_EDGE('',*,*,#54310,.T.);
#76310=ORIENTED_EDGE('',*,*,#54288,.F.);
#76311=ORIENTED_EDGE('',*,*,#54311,.T.);
#76312=ORIENTED_EDGE('',*,*,#54308,.F.);
#76313=ORIENTED_EDGE('',*,*,#54312,.T.);
#76314=ORIENTED_EDGE('',*,*,#52121,.F.);
#76315=ORIENTED_EDGE('',*,*,#54313,.T.);
#76316=ORIENTED_EDGE('',*,*,#54299,.F.);
#76317=ORIENTED_EDGE('',*,*,#54314,.T.);
#76318=ORIENTED_EDGE('',*,*,#54301,.F.);
#76319=ORIENTED_EDGE('',*,*,#54315,.T.);
#76320=ORIENTED_EDGE('',*,*,#54295,.F.);
#76321=ORIENTED_EDGE('',*,*,#54316,.T.);
#76322=ORIENTED_EDGE('',*,*,#54297,.F.);
#76323=ORIENTED_EDGE('',*,*,#54317,.T.);
#76324=ORIENTED_EDGE('',*,*,#54318,.T.);
#76325=ORIENTED_EDGE('',*,*,#54319,.T.);
#76326=ORIENTED_EDGE('',*,*,#54320,.F.);
#76327=ORIENTED_EDGE('',*,*,#54321,.F.);
#76328=ORIENTED_EDGE('',*,*,#54322,.F.);
#76329=ORIENTED_EDGE('',*,*,#54323,.T.);
#76330=ORIENTED_EDGE('',*,*,#54321,.T.);
#76331=ORIENTED_EDGE('',*,*,#54324,.T.);
#76332=ORIENTED_EDGE('',*,*,#54325,.T.);
#76333=ORIENTED_EDGE('',*,*,#54326,.T.);
#76334=ORIENTED_EDGE('',*,*,#54327,.T.);
#76335=ORIENTED_EDGE('',*,*,#54328,.T.);
#76336=ORIENTED_EDGE('',*,*,#54329,.T.);
#76337=ORIENTED_EDGE('',*,*,#54330,.T.);
#76338=ORIENTED_EDGE('',*,*,#54331,.T.);
#76339=ORIENTED_EDGE('',*,*,#54332,.T.);
#76340=ORIENTED_EDGE('',*,*,#54333,.F.);
#76341=ORIENTED_EDGE('',*,*,#54334,.F.);
#76342=ORIENTED_EDGE('',*,*,#54335,.F.);
#76343=ORIENTED_EDGE('',*,*,#54336,.T.);
#76344=ORIENTED_EDGE('',*,*,#54334,.T.);
#76345=ORIENTED_EDGE('',*,*,#54337,.T.);
#76346=ORIENTED_EDGE('',*,*,#54338,.T.);
#76347=ORIENTED_EDGE('',*,*,#54339,.T.);
#76348=ORIENTED_EDGE('',*,*,#52551,.F.);
#76349=ORIENTED_EDGE('',*,*,#54340,.T.);
#76350=ORIENTED_EDGE('',*,*,#54318,.F.);
#76351=ORIENTED_EDGE('',*,*,#54341,.T.);
#76352=ORIENTED_EDGE('',*,*,#54338,.F.);
#76353=ORIENTED_EDGE('',*,*,#54342,.T.);
#76354=ORIENTED_EDGE('',*,*,#52115,.F.);
#76355=ORIENTED_EDGE('',*,*,#54343,.T.);
#76356=ORIENTED_EDGE('',*,*,#54329,.F.);
#76357=ORIENTED_EDGE('',*,*,#54344,.T.);
#76358=ORIENTED_EDGE('',*,*,#54331,.F.);
#76359=ORIENTED_EDGE('',*,*,#54345,.T.);
#76360=ORIENTED_EDGE('',*,*,#54325,.F.);
#76361=ORIENTED_EDGE('',*,*,#54346,.T.);
#76362=ORIENTED_EDGE('',*,*,#54327,.F.);
#76363=ORIENTED_EDGE('',*,*,#54347,.T.);
#76364=ORIENTED_EDGE('',*,*,#54348,.T.);
#76365=ORIENTED_EDGE('',*,*,#54349,.T.);
#76366=ORIENTED_EDGE('',*,*,#54350,.F.);
#76367=ORIENTED_EDGE('',*,*,#54351,.F.);
#76368=ORIENTED_EDGE('',*,*,#54352,.F.);
#76369=ORIENTED_EDGE('',*,*,#54353,.T.);
#76370=ORIENTED_EDGE('',*,*,#54351,.T.);
#76371=ORIENTED_EDGE('',*,*,#54354,.T.);
#76372=ORIENTED_EDGE('',*,*,#54355,.T.);
#76373=ORIENTED_EDGE('',*,*,#54356,.T.);
#76374=ORIENTED_EDGE('',*,*,#54357,.T.);
#76375=ORIENTED_EDGE('',*,*,#54358,.T.);
#76376=ORIENTED_EDGE('',*,*,#54359,.T.);
#76377=ORIENTED_EDGE('',*,*,#54360,.T.);
#76378=ORIENTED_EDGE('',*,*,#54361,.T.);
#76379=ORIENTED_EDGE('',*,*,#54362,.T.);
#76380=ORIENTED_EDGE('',*,*,#54363,.F.);
#76381=ORIENTED_EDGE('',*,*,#54364,.F.);
#76382=ORIENTED_EDGE('',*,*,#54365,.F.);
#76383=ORIENTED_EDGE('',*,*,#54366,.T.);
#76384=ORIENTED_EDGE('',*,*,#54364,.T.);
#76385=ORIENTED_EDGE('',*,*,#54367,.T.);
#76386=ORIENTED_EDGE('',*,*,#54368,.T.);
#76387=ORIENTED_EDGE('',*,*,#54369,.T.);
#76388=ORIENTED_EDGE('',*,*,#52557,.F.);
#76389=ORIENTED_EDGE('',*,*,#54370,.T.);
#76390=ORIENTED_EDGE('',*,*,#54348,.F.);
#76391=ORIENTED_EDGE('',*,*,#54371,.T.);
#76392=ORIENTED_EDGE('',*,*,#54368,.F.);
#76393=ORIENTED_EDGE('',*,*,#54372,.T.);
#76394=ORIENTED_EDGE('',*,*,#52109,.F.);
#76395=ORIENTED_EDGE('',*,*,#54373,.T.);
#76396=ORIENTED_EDGE('',*,*,#54359,.F.);
#76397=ORIENTED_EDGE('',*,*,#54374,.T.);
#76398=ORIENTED_EDGE('',*,*,#54361,.F.);
#76399=ORIENTED_EDGE('',*,*,#54375,.T.);
#76400=ORIENTED_EDGE('',*,*,#54355,.F.);
#76401=ORIENTED_EDGE('',*,*,#54376,.T.);
#76402=ORIENTED_EDGE('',*,*,#54357,.F.);
#76403=ORIENTED_EDGE('',*,*,#54377,.T.);
#76404=ORIENTED_EDGE('',*,*,#54378,.T.);
#76405=ORIENTED_EDGE('',*,*,#54379,.T.);
#76406=ORIENTED_EDGE('',*,*,#54380,.F.);
#76407=ORIENTED_EDGE('',*,*,#54381,.F.);
#76408=ORIENTED_EDGE('',*,*,#54382,.F.);
#76409=ORIENTED_EDGE('',*,*,#54383,.T.);
#76410=ORIENTED_EDGE('',*,*,#54381,.T.);
#76411=ORIENTED_EDGE('',*,*,#54384,.T.);
#76412=ORIENTED_EDGE('',*,*,#54385,.T.);
#76413=ORIENTED_EDGE('',*,*,#54386,.T.);
#76414=ORIENTED_EDGE('',*,*,#54387,.T.);
#76415=ORIENTED_EDGE('',*,*,#54388,.T.);
#76416=ORIENTED_EDGE('',*,*,#54389,.T.);
#76417=ORIENTED_EDGE('',*,*,#54390,.T.);
#76418=ORIENTED_EDGE('',*,*,#54391,.T.);
#76419=ORIENTED_EDGE('',*,*,#54392,.T.);
#76420=ORIENTED_EDGE('',*,*,#54393,.F.);
#76421=ORIENTED_EDGE('',*,*,#54394,.F.);
#76422=ORIENTED_EDGE('',*,*,#54395,.F.);
#76423=ORIENTED_EDGE('',*,*,#54396,.T.);
#76424=ORIENTED_EDGE('',*,*,#54394,.T.);
#76425=ORIENTED_EDGE('',*,*,#54397,.T.);
#76426=ORIENTED_EDGE('',*,*,#54398,.T.);
#76427=ORIENTED_EDGE('',*,*,#54399,.T.);
#76428=ORIENTED_EDGE('',*,*,#52563,.F.);
#76429=ORIENTED_EDGE('',*,*,#54400,.T.);
#76430=ORIENTED_EDGE('',*,*,#54378,.F.);
#76431=ORIENTED_EDGE('',*,*,#54401,.T.);
#76432=ORIENTED_EDGE('',*,*,#54398,.F.);
#76433=ORIENTED_EDGE('',*,*,#54402,.T.);
#76434=ORIENTED_EDGE('',*,*,#52103,.F.);
#76435=ORIENTED_EDGE('',*,*,#54403,.T.);
#76436=ORIENTED_EDGE('',*,*,#54389,.F.);
#76437=ORIENTED_EDGE('',*,*,#54404,.T.);
#76438=ORIENTED_EDGE('',*,*,#54391,.F.);
#76439=ORIENTED_EDGE('',*,*,#54405,.T.);
#76440=ORIENTED_EDGE('',*,*,#54385,.F.);
#76441=ORIENTED_EDGE('',*,*,#54406,.T.);
#76442=ORIENTED_EDGE('',*,*,#54387,.F.);
#76443=ORIENTED_EDGE('',*,*,#54407,.T.);
#76444=ORIENTED_EDGE('',*,*,#54408,.T.);
#76445=ORIENTED_EDGE('',*,*,#54409,.T.);
#76446=ORIENTED_EDGE('',*,*,#54410,.F.);
#76447=ORIENTED_EDGE('',*,*,#54411,.F.);
#76448=ORIENTED_EDGE('',*,*,#54412,.F.);
#76449=ORIENTED_EDGE('',*,*,#54413,.T.);
#76450=ORIENTED_EDGE('',*,*,#54411,.T.);
#76451=ORIENTED_EDGE('',*,*,#54414,.T.);
#76452=ORIENTED_EDGE('',*,*,#54415,.T.);
#76453=ORIENTED_EDGE('',*,*,#54416,.T.);
#76454=ORIENTED_EDGE('',*,*,#54417,.T.);
#76455=ORIENTED_EDGE('',*,*,#54418,.T.);
#76456=ORIENTED_EDGE('',*,*,#54419,.T.);
#76457=ORIENTED_EDGE('',*,*,#54420,.T.);
#76458=ORIENTED_EDGE('',*,*,#54421,.T.);
#76459=ORIENTED_EDGE('',*,*,#54422,.T.);
#76460=ORIENTED_EDGE('',*,*,#54423,.F.);
#76461=ORIENTED_EDGE('',*,*,#54424,.F.);
#76462=ORIENTED_EDGE('',*,*,#54425,.F.);
#76463=ORIENTED_EDGE('',*,*,#54426,.T.);
#76464=ORIENTED_EDGE('',*,*,#54424,.T.);
#76465=ORIENTED_EDGE('',*,*,#54427,.T.);
#76466=ORIENTED_EDGE('',*,*,#54428,.T.);
#76467=ORIENTED_EDGE('',*,*,#54429,.T.);
#76468=ORIENTED_EDGE('',*,*,#52569,.F.);
#76469=ORIENTED_EDGE('',*,*,#54430,.T.);
#76470=ORIENTED_EDGE('',*,*,#54408,.F.);
#76471=ORIENTED_EDGE('',*,*,#54431,.T.);
#76472=ORIENTED_EDGE('',*,*,#54428,.F.);
#76473=ORIENTED_EDGE('',*,*,#54432,.T.);
#76474=ORIENTED_EDGE('',*,*,#52097,.F.);
#76475=ORIENTED_EDGE('',*,*,#54433,.T.);
#76476=ORIENTED_EDGE('',*,*,#54419,.F.);
#76477=ORIENTED_EDGE('',*,*,#54434,.T.);
#76478=ORIENTED_EDGE('',*,*,#54421,.F.);
#76479=ORIENTED_EDGE('',*,*,#54435,.T.);
#76480=ORIENTED_EDGE('',*,*,#54415,.F.);
#76481=ORIENTED_EDGE('',*,*,#54436,.T.);
#76482=ORIENTED_EDGE('',*,*,#54417,.F.);
#76483=ORIENTED_EDGE('',*,*,#54437,.T.);
#76484=ORIENTED_EDGE('',*,*,#54438,.T.);
#76485=ORIENTED_EDGE('',*,*,#54439,.T.);
#76486=ORIENTED_EDGE('',*,*,#54440,.F.);
#76487=ORIENTED_EDGE('',*,*,#54441,.F.);
#76488=ORIENTED_EDGE('',*,*,#54442,.F.);
#76489=ORIENTED_EDGE('',*,*,#54443,.T.);
#76490=ORIENTED_EDGE('',*,*,#54441,.T.);
#76491=ORIENTED_EDGE('',*,*,#54444,.T.);
#76492=ORIENTED_EDGE('',*,*,#54445,.T.);
#76493=ORIENTED_EDGE('',*,*,#54446,.T.);
#76494=ORIENTED_EDGE('',*,*,#54447,.T.);
#76495=ORIENTED_EDGE('',*,*,#54448,.T.);
#76496=ORIENTED_EDGE('',*,*,#54449,.T.);
#76497=ORIENTED_EDGE('',*,*,#54450,.T.);
#76498=ORIENTED_EDGE('',*,*,#54451,.T.);
#76499=ORIENTED_EDGE('',*,*,#54452,.T.);
#76500=ORIENTED_EDGE('',*,*,#54453,.F.);
#76501=ORIENTED_EDGE('',*,*,#54454,.F.);
#76502=ORIENTED_EDGE('',*,*,#54455,.F.);
#76503=ORIENTED_EDGE('',*,*,#54456,.T.);
#76504=ORIENTED_EDGE('',*,*,#54454,.T.);
#76505=ORIENTED_EDGE('',*,*,#54457,.T.);
#76506=ORIENTED_EDGE('',*,*,#54458,.T.);
#76507=ORIENTED_EDGE('',*,*,#54459,.T.);
#76508=ORIENTED_EDGE('',*,*,#52575,.F.);
#76509=ORIENTED_EDGE('',*,*,#54460,.T.);
#76510=ORIENTED_EDGE('',*,*,#54438,.F.);
#76511=ORIENTED_EDGE('',*,*,#54461,.T.);
#76512=ORIENTED_EDGE('',*,*,#54458,.F.);
#76513=ORIENTED_EDGE('',*,*,#54462,.T.);
#76514=ORIENTED_EDGE('',*,*,#52091,.F.);
#76515=ORIENTED_EDGE('',*,*,#54463,.T.);
#76516=ORIENTED_EDGE('',*,*,#54449,.F.);
#76517=ORIENTED_EDGE('',*,*,#54464,.T.);
#76518=ORIENTED_EDGE('',*,*,#54451,.F.);
#76519=ORIENTED_EDGE('',*,*,#54465,.T.);
#76520=ORIENTED_EDGE('',*,*,#54445,.F.);
#76521=ORIENTED_EDGE('',*,*,#54466,.T.);
#76522=ORIENTED_EDGE('',*,*,#54447,.F.);
#76523=ORIENTED_EDGE('',*,*,#54467,.T.);
#76524=ORIENTED_EDGE('',*,*,#54468,.T.);
#76525=ORIENTED_EDGE('',*,*,#54469,.T.);
#76526=ORIENTED_EDGE('',*,*,#54470,.F.);
#76527=ORIENTED_EDGE('',*,*,#54471,.F.);
#76528=ORIENTED_EDGE('',*,*,#54472,.F.);
#76529=ORIENTED_EDGE('',*,*,#54473,.T.);
#76530=ORIENTED_EDGE('',*,*,#54471,.T.);
#76531=ORIENTED_EDGE('',*,*,#54474,.T.);
#76532=ORIENTED_EDGE('',*,*,#54475,.T.);
#76533=ORIENTED_EDGE('',*,*,#54476,.T.);
#76534=ORIENTED_EDGE('',*,*,#54477,.T.);
#76535=ORIENTED_EDGE('',*,*,#54478,.T.);
#76536=ORIENTED_EDGE('',*,*,#54479,.T.);
#76537=ORIENTED_EDGE('',*,*,#54480,.T.);
#76538=ORIENTED_EDGE('',*,*,#54481,.T.);
#76539=ORIENTED_EDGE('',*,*,#54482,.T.);
#76540=ORIENTED_EDGE('',*,*,#54483,.F.);
#76541=ORIENTED_EDGE('',*,*,#54484,.F.);
#76542=ORIENTED_EDGE('',*,*,#54485,.F.);
#76543=ORIENTED_EDGE('',*,*,#54486,.T.);
#76544=ORIENTED_EDGE('',*,*,#54484,.T.);
#76545=ORIENTED_EDGE('',*,*,#54487,.T.);
#76546=ORIENTED_EDGE('',*,*,#54488,.T.);
#76547=ORIENTED_EDGE('',*,*,#54489,.T.);
#76548=ORIENTED_EDGE('',*,*,#52581,.F.);
#76549=ORIENTED_EDGE('',*,*,#54490,.T.);
#76550=ORIENTED_EDGE('',*,*,#54468,.F.);
#76551=ORIENTED_EDGE('',*,*,#54491,.T.);
#76552=ORIENTED_EDGE('',*,*,#54488,.F.);
#76553=ORIENTED_EDGE('',*,*,#54492,.T.);
#76554=ORIENTED_EDGE('',*,*,#52085,.F.);
#76555=ORIENTED_EDGE('',*,*,#54493,.T.);
#76556=ORIENTED_EDGE('',*,*,#54479,.F.);
#76557=ORIENTED_EDGE('',*,*,#54494,.T.);
#76558=ORIENTED_EDGE('',*,*,#54481,.F.);
#76559=ORIENTED_EDGE('',*,*,#54495,.T.);
#76560=ORIENTED_EDGE('',*,*,#54475,.F.);
#76561=ORIENTED_EDGE('',*,*,#54496,.T.);
#76562=ORIENTED_EDGE('',*,*,#54477,.F.);
#76563=ORIENTED_EDGE('',*,*,#54497,.T.);
#76564=ORIENTED_EDGE('',*,*,#54498,.T.);
#76565=ORIENTED_EDGE('',*,*,#54499,.T.);
#76566=ORIENTED_EDGE('',*,*,#54500,.F.);
#76567=ORIENTED_EDGE('',*,*,#54501,.F.);
#76568=ORIENTED_EDGE('',*,*,#54502,.F.);
#76569=ORIENTED_EDGE('',*,*,#54503,.T.);
#76570=ORIENTED_EDGE('',*,*,#54501,.T.);
#76571=ORIENTED_EDGE('',*,*,#54504,.T.);
#76572=ORIENTED_EDGE('',*,*,#54505,.T.);
#76573=ORIENTED_EDGE('',*,*,#54506,.T.);
#76574=ORIENTED_EDGE('',*,*,#54507,.T.);
#76575=ORIENTED_EDGE('',*,*,#54508,.T.);
#76576=ORIENTED_EDGE('',*,*,#54509,.T.);
#76577=ORIENTED_EDGE('',*,*,#54510,.T.);
#76578=ORIENTED_EDGE('',*,*,#54511,.T.);
#76579=ORIENTED_EDGE('',*,*,#54512,.T.);
#76580=ORIENTED_EDGE('',*,*,#54513,.F.);
#76581=ORIENTED_EDGE('',*,*,#54514,.F.);
#76582=ORIENTED_EDGE('',*,*,#54515,.F.);
#76583=ORIENTED_EDGE('',*,*,#54516,.T.);
#76584=ORIENTED_EDGE('',*,*,#54514,.T.);
#76585=ORIENTED_EDGE('',*,*,#54517,.T.);
#76586=ORIENTED_EDGE('',*,*,#54518,.T.);
#76587=ORIENTED_EDGE('',*,*,#54519,.T.);
#76588=ORIENTED_EDGE('',*,*,#52587,.F.);
#76589=ORIENTED_EDGE('',*,*,#54520,.T.);
#76590=ORIENTED_EDGE('',*,*,#54498,.F.);
#76591=ORIENTED_EDGE('',*,*,#54521,.T.);
#76592=ORIENTED_EDGE('',*,*,#54518,.F.);
#76593=ORIENTED_EDGE('',*,*,#54522,.T.);
#76594=ORIENTED_EDGE('',*,*,#52079,.F.);
#76595=ORIENTED_EDGE('',*,*,#54523,.T.);
#76596=ORIENTED_EDGE('',*,*,#54509,.F.);
#76597=ORIENTED_EDGE('',*,*,#54524,.T.);
#76598=ORIENTED_EDGE('',*,*,#54511,.F.);
#76599=ORIENTED_EDGE('',*,*,#54525,.T.);
#76600=ORIENTED_EDGE('',*,*,#54505,.F.);
#76601=ORIENTED_EDGE('',*,*,#54526,.T.);
#76602=ORIENTED_EDGE('',*,*,#54507,.F.);
#76603=ORIENTED_EDGE('',*,*,#54527,.T.);
#76604=ORIENTED_EDGE('',*,*,#54528,.T.);
#76605=ORIENTED_EDGE('',*,*,#54529,.T.);
#76606=ORIENTED_EDGE('',*,*,#54530,.F.);
#76607=ORIENTED_EDGE('',*,*,#54531,.F.);
#76608=ORIENTED_EDGE('',*,*,#54532,.F.);
#76609=ORIENTED_EDGE('',*,*,#54533,.T.);
#76610=ORIENTED_EDGE('',*,*,#54531,.T.);
#76611=ORIENTED_EDGE('',*,*,#54534,.T.);
#76612=ORIENTED_EDGE('',*,*,#54535,.T.);
#76613=ORIENTED_EDGE('',*,*,#54536,.T.);
#76614=ORIENTED_EDGE('',*,*,#54537,.T.);
#76615=ORIENTED_EDGE('',*,*,#54538,.T.);
#76616=ORIENTED_EDGE('',*,*,#54539,.T.);
#76617=ORIENTED_EDGE('',*,*,#54540,.T.);
#76618=ORIENTED_EDGE('',*,*,#54541,.T.);
#76619=ORIENTED_EDGE('',*,*,#54542,.T.);
#76620=ORIENTED_EDGE('',*,*,#54543,.F.);
#76621=ORIENTED_EDGE('',*,*,#54544,.F.);
#76622=ORIENTED_EDGE('',*,*,#54545,.F.);
#76623=ORIENTED_EDGE('',*,*,#54546,.T.);
#76624=ORIENTED_EDGE('',*,*,#54544,.T.);
#76625=ORIENTED_EDGE('',*,*,#54547,.T.);
#76626=ORIENTED_EDGE('',*,*,#54548,.T.);
#76627=ORIENTED_EDGE('',*,*,#54549,.T.);
#76628=ORIENTED_EDGE('',*,*,#52593,.F.);
#76629=ORIENTED_EDGE('',*,*,#54550,.T.);
#76630=ORIENTED_EDGE('',*,*,#54528,.F.);
#76631=ORIENTED_EDGE('',*,*,#54551,.T.);
#76632=ORIENTED_EDGE('',*,*,#54548,.F.);
#76633=ORIENTED_EDGE('',*,*,#54552,.T.);
#76634=ORIENTED_EDGE('',*,*,#52073,.F.);
#76635=ORIENTED_EDGE('',*,*,#54553,.T.);
#76636=ORIENTED_EDGE('',*,*,#54539,.F.);
#76637=ORIENTED_EDGE('',*,*,#54554,.T.);
#76638=ORIENTED_EDGE('',*,*,#54541,.F.);
#76639=ORIENTED_EDGE('',*,*,#54555,.T.);
#76640=ORIENTED_EDGE('',*,*,#54535,.F.);
#76641=ORIENTED_EDGE('',*,*,#54556,.T.);
#76642=ORIENTED_EDGE('',*,*,#54537,.F.);
#76643=ORIENTED_EDGE('',*,*,#54557,.T.);
#76644=ORIENTED_EDGE('',*,*,#52052,.T.);
#76645=ORIENTED_EDGE('',*,*,#52046,.T.);
#76646=ORIENTED_EDGE('',*,*,#54558,.T.);
#76647=ORIENTED_EDGE('',*,*,#54559,.T.);
#76648=ORIENTED_EDGE('',*,*,#54560,.F.);
#76649=ORIENTED_EDGE('',*,*,#54561,.F.);
#76650=ORIENTED_EDGE('',*,*,#54562,.F.);
#76651=ORIENTED_EDGE('',*,*,#54563,.T.);
#76652=ORIENTED_EDGE('',*,*,#54561,.T.);
#76653=ORIENTED_EDGE('',*,*,#54564,.T.);
#76654=ORIENTED_EDGE('',*,*,#54565,.T.);
#76655=ORIENTED_EDGE('',*,*,#54566,.T.);
#76656=ORIENTED_EDGE('',*,*,#54567,.T.);
#76657=ORIENTED_EDGE('',*,*,#54568,.T.);
#76658=ORIENTED_EDGE('',*,*,#54569,.T.);
#76659=ORIENTED_EDGE('',*,*,#54570,.T.);
#76660=ORIENTED_EDGE('',*,*,#54571,.T.);
#76661=ORIENTED_EDGE('',*,*,#54572,.T.);
#76662=ORIENTED_EDGE('',*,*,#54573,.F.);
#76663=ORIENTED_EDGE('',*,*,#54574,.F.);
#76664=ORIENTED_EDGE('',*,*,#54575,.F.);
#76665=ORIENTED_EDGE('',*,*,#54576,.T.);
#76666=ORIENTED_EDGE('',*,*,#54574,.T.);
#76667=ORIENTED_EDGE('',*,*,#54577,.T.);
#76668=ORIENTED_EDGE('',*,*,#54578,.T.);
#76669=ORIENTED_EDGE('',*,*,#54579,.T.);
#76670=ORIENTED_EDGE('',*,*,#52059,.T.);
#76671=ORIENTED_EDGE('',*,*,#52053,.T.);
#76672=ORIENTED_EDGE('',*,*,#52060,.T.);
#76673=ORIENTED_EDGE('',*,*,#52787,.F.);
#76674=ORIENTED_EDGE('',*,*,#52599,.F.);
#76675=ORIENTED_EDGE('',*,*,#54580,.T.);
#76676=ORIENTED_EDGE('',*,*,#54558,.F.);
#76677=ORIENTED_EDGE('',*,*,#54581,.T.);
#76678=ORIENTED_EDGE('',*,*,#54578,.F.);
#76679=ORIENTED_EDGE('',*,*,#54582,.T.);
#76680=ORIENTED_EDGE('',*,*,#52067,.F.);
#76681=ORIENTED_EDGE('',*,*,#54583,.T.);
#76682=ORIENTED_EDGE('',*,*,#54569,.F.);
#76683=ORIENTED_EDGE('',*,*,#54584,.T.);
#76684=ORIENTED_EDGE('',*,*,#54571,.F.);
#76685=ORIENTED_EDGE('',*,*,#54585,.T.);
#76686=ORIENTED_EDGE('',*,*,#54565,.F.);
#76687=ORIENTED_EDGE('',*,*,#54586,.T.);
#76688=ORIENTED_EDGE('',*,*,#54567,.F.);
#76689=ORIENTED_EDGE('',*,*,#54587,.T.);
#76690=ORIENTED_EDGE('',*,*,#54588,.T.);
#76691=ORIENTED_EDGE('',*,*,#54589,.T.);
#76692=ORIENTED_EDGE('',*,*,#54590,.T.);
#76693=ORIENTED_EDGE('',*,*,#54591,.T.);
#76694=ORIENTED_EDGE('',*,*,#54592,.T.);
#76695=ORIENTED_EDGE('',*,*,#54593,.T.);
#76696=ORIENTED_EDGE('',*,*,#54594,.T.);
#76697=ORIENTED_EDGE('',*,*,#54595,.T.);
#76698=ORIENTED_EDGE('',*,*,#54596,.T.);
#76699=ORIENTED_EDGE('',*,*,#54597,.T.);
#76700=ORIENTED_EDGE('',*,*,#54598,.T.);
#76701=ORIENTED_EDGE('',*,*,#54599,.T.);
#76702=ORIENTED_EDGE('',*,*,#54600,.T.);
#76703=ORIENTED_EDGE('',*,*,#54601,.T.);
#76704=ORIENTED_EDGE('',*,*,#54602,.T.);
#76705=ORIENTED_EDGE('',*,*,#54603,.T.);
#76706=ORIENTED_EDGE('',*,*,#54604,.T.);
#76707=ORIENTED_EDGE('',*,*,#54605,.T.);
#76708=ORIENTED_EDGE('',*,*,#54606,.T.);
#76709=ORIENTED_EDGE('',*,*,#54607,.T.);
#76710=ORIENTED_EDGE('',*,*,#54608,.T.);
#76711=ORIENTED_EDGE('',*,*,#54609,.T.);
#76712=ORIENTED_EDGE('',*,*,#54610,.T.);
#76713=ORIENTED_EDGE('',*,*,#54611,.T.);
#76714=ORIENTED_EDGE('',*,*,#54612,.T.);
#76715=ORIENTED_EDGE('',*,*,#54613,.T.);
#76716=ORIENTED_EDGE('',*,*,#54614,.T.);
#76717=ORIENTED_EDGE('',*,*,#54615,.T.);
#76718=ORIENTED_EDGE('',*,*,#54606,.F.);
#76719=ORIENTED_EDGE('',*,*,#54616,.T.);
#76720=ORIENTED_EDGE('',*,*,#54588,.F.);
#76721=ORIENTED_EDGE('',*,*,#54617,.T.);
#76722=ORIENTED_EDGE('',*,*,#54590,.F.);
#76723=ORIENTED_EDGE('',*,*,#54618,.T.);
#76724=ORIENTED_EDGE('',*,*,#54594,.F.);
#76725=ORIENTED_EDGE('',*,*,#54619,.T.);
#76726=ORIENTED_EDGE('',*,*,#54620,.F.);
#76727=ORIENTED_EDGE('',*,*,#54614,.F.);
#76728=ORIENTED_EDGE('',*,*,#54621,.F.);
#76729=ORIENTED_EDGE('',*,*,#54576,.F.);
#76730=ORIENTED_EDGE('',*,*,#54621,.T.);
#76731=ORIENTED_EDGE('',*,*,#54613,.F.);
#76732=ORIENTED_EDGE('',*,*,#54622,.F.);
#76733=ORIENTED_EDGE('',*,*,#54585,.F.);
#76734=ORIENTED_EDGE('',*,*,#54575,.T.);
#76735=ORIENTED_EDGE('',*,*,#54579,.F.);
#76736=ORIENTED_EDGE('',*,*,#54623,.F.);
#76737=ORIENTED_EDGE('',*,*,#54615,.F.);
#76738=ORIENTED_EDGE('',*,*,#54620,.T.);
#76739=ORIENTED_EDGE('',*,*,#54622,.T.);
#76740=ORIENTED_EDGE('',*,*,#54612,.F.);
#76741=ORIENTED_EDGE('',*,*,#54624,.F.);
#76742=ORIENTED_EDGE('',*,*,#54570,.F.);
#76743=ORIENTED_EDGE('',*,*,#54623,.T.);
#76744=ORIENTED_EDGE('',*,*,#54583,.F.);
#76745=ORIENTED_EDGE('',*,*,#54625,.F.);
#76746=ORIENTED_EDGE('',*,*,#54604,.F.);
#76747=ORIENTED_EDGE('',*,*,#54624,.T.);
#76748=ORIENTED_EDGE('',*,*,#54611,.F.);
#76749=ORIENTED_EDGE('',*,*,#54626,.F.);
#76750=ORIENTED_EDGE('',*,*,#54587,.F.);
#76751=ORIENTED_EDGE('',*,*,#54625,.T.);
#76752=ORIENTED_EDGE('',*,*,#52066,.F.);
#76753=ORIENTED_EDGE('',*,*,#54627,.F.);
#76754=ORIENTED_EDGE('',*,*,#54605,.F.);
#76755=ORIENTED_EDGE('',*,*,#54626,.T.);
#76756=ORIENTED_EDGE('',*,*,#54610,.F.);
#76757=ORIENTED_EDGE('',*,*,#54628,.F.);
#76758=ORIENTED_EDGE('',*,*,#54562,.T.);
#76759=ORIENTED_EDGE('',*,*,#54566,.F.);
#76760=ORIENTED_EDGE('',*,*,#54627,.T.);
#76761=ORIENTED_EDGE('',*,*,#52065,.F.);
#76762=ORIENTED_EDGE('',*,*,#54629,.F.);
#76763=ORIENTED_EDGE('',*,*,#54616,.F.);
#76764=ORIENTED_EDGE('',*,*,#54628,.T.);
#76765=ORIENTED_EDGE('',*,*,#54609,.F.);
#76766=ORIENTED_EDGE('',*,*,#54630,.F.);
#76767=ORIENTED_EDGE('',*,*,#54563,.F.);
#76768=ORIENTED_EDGE('',*,*,#54629,.T.);
#76769=ORIENTED_EDGE('',*,*,#52064,.F.);
#76770=ORIENTED_EDGE('',*,*,#54631,.F.);
#76771=ORIENTED_EDGE('',*,*,#54589,.F.);
#76772=ORIENTED_EDGE('',*,*,#54630,.T.);
#76773=ORIENTED_EDGE('',*,*,#54608,.F.);
#76774=ORIENTED_EDGE('',*,*,#54632,.F.);
#76775=ORIENTED_EDGE('',*,*,#54581,.F.);
#76776=ORIENTED_EDGE('',*,*,#54631,.T.);
#76777=ORIENTED_EDGE('',*,*,#52422,.F.);
#76778=ORIENTED_EDGE('',*,*,#54633,.F.);
#76779=ORIENTED_EDGE('',*,*,#54618,.F.);
#76780=ORIENTED_EDGE('',*,*,#54632,.T.);
#76781=ORIENTED_EDGE('',*,*,#54607,.F.);
#76782=ORIENTED_EDGE('',*,*,#54634,.F.);
#76783=ORIENTED_EDGE('',*,*,#52600,.F.);
#76784=ORIENTED_EDGE('',*,*,#54633,.T.);
#76785=ORIENTED_EDGE('',*,*,#52421,.F.);
#76786=ORIENTED_EDGE('',*,*,#54635,.F.);
#76787=ORIENTED_EDGE('',*,*,#54595,.F.);
#76788=ORIENTED_EDGE('',*,*,#54634,.T.);
#76789=ORIENTED_EDGE('',*,*,#54617,.F.);
#76790=ORIENTED_EDGE('',*,*,#54636,.F.);
#76791=ORIENTED_EDGE('',*,*,#52601,.F.);
#76792=ORIENTED_EDGE('',*,*,#54635,.T.);
#76793=ORIENTED_EDGE('',*,*,#52813,.F.);
#76794=ORIENTED_EDGE('',*,*,#54637,.F.);
#76795=ORIENTED_EDGE('',*,*,#54596,.F.);
#76796=ORIENTED_EDGE('',*,*,#54636,.T.);
#76797=ORIENTED_EDGE('',*,*,#54591,.F.);
#76798=ORIENTED_EDGE('',*,*,#54638,.F.);
#76799=ORIENTED_EDGE('',*,*,#52604,.F.);
#76800=ORIENTED_EDGE('',*,*,#52602,.F.);
#76801=ORIENTED_EDGE('',*,*,#52809,.F.);
#76802=ORIENTED_EDGE('',*,*,#52805,.T.);
#76803=ORIENTED_EDGE('',*,*,#54639,.F.);
#76804=ORIENTED_EDGE('',*,*,#54597,.F.);
#76805=ORIENTED_EDGE('',*,*,#54637,.T.);
#76806=ORIENTED_EDGE('',*,*,#54638,.T.);
#76807=ORIENTED_EDGE('',*,*,#54619,.F.);
#76808=ORIENTED_EDGE('',*,*,#54640,.F.);
#76809=ORIENTED_EDGE('',*,*,#52605,.F.);
#76810=ORIENTED_EDGE('',*,*,#54639,.T.);
#76811=ORIENTED_EDGE('',*,*,#52804,.F.);
#76812=ORIENTED_EDGE('',*,*,#54641,.F.);
#76813=ORIENTED_EDGE('',*,*,#54598,.F.);
#76814=ORIENTED_EDGE('',*,*,#54640,.T.);
#76815=ORIENTED_EDGE('',*,*,#54593,.F.);
#76816=ORIENTED_EDGE('',*,*,#54642,.F.);
#76817=ORIENTED_EDGE('',*,*,#52606,.F.);
#76818=ORIENTED_EDGE('',*,*,#54641,.T.);
#76819=ORIENTED_EDGE('',*,*,#52815,.F.);
#76820=ORIENTED_EDGE('',*,*,#54643,.F.);
#76821=ORIENTED_EDGE('',*,*,#54599,.F.);
#76822=ORIENTED_EDGE('',*,*,#54642,.T.);
#76823=ORIENTED_EDGE('',*,*,#54592,.F.);
#76824=ORIENTED_EDGE('',*,*,#54644,.F.);
#76825=ORIENTED_EDGE('',*,*,#52811,.F.);
#76826=ORIENTED_EDGE('',*,*,#54643,.T.);
#76827=ORIENTED_EDGE('',*,*,#52800,.F.);
#76828=ORIENTED_EDGE('',*,*,#54645,.F.);
#76829=ORIENTED_EDGE('',*,*,#54600,.F.);
#76830=ORIENTED_EDGE('',*,*,#54644,.T.);
#76831=ORIENTED_EDGE('',*,*,#54603,.F.);
#76832=ORIENTED_EDGE('',*,*,#54646,.F.);
#76833=ORIENTED_EDGE('',*,*,#52791,.F.);
#76834=ORIENTED_EDGE('',*,*,#54645,.T.);
#76835=ORIENTED_EDGE('',*,*,#52817,.F.);
#76836=ORIENTED_EDGE('',*,*,#54647,.F.);
#76837=ORIENTED_EDGE('',*,*,#54601,.F.);
#76838=ORIENTED_EDGE('',*,*,#54646,.T.);
#76839=ORIENTED_EDGE('',*,*,#54602,.F.);
#76840=ORIENTED_EDGE('',*,*,#54647,.T.);
#76841=ORIENTED_EDGE('',*,*,#52796,.F.);
#76842=ORIENTED_EDGE('',*,*,#52792,.T.);
#76843=ORIENTED_EDGE('',*,*,#54648,.T.);
#76844=ORIENTED_EDGE('',*,*,#54649,.T.);
#76845=ORIENTED_EDGE('',*,*,#54650,.T.);
#76846=ORIENTED_EDGE('',*,*,#54651,.T.);
#76847=ORIENTED_EDGE('',*,*,#54652,.T.);
#76848=ORIENTED_EDGE('',*,*,#54653,.T.);
#76849=ORIENTED_EDGE('',*,*,#54654,.T.);
#76850=ORIENTED_EDGE('',*,*,#54655,.T.);
#76851=ORIENTED_EDGE('',*,*,#54656,.T.);
#76852=ORIENTED_EDGE('',*,*,#54657,.T.);
#76853=ORIENTED_EDGE('',*,*,#54658,.T.);
#76854=ORIENTED_EDGE('',*,*,#54659,.T.);
#76855=ORIENTED_EDGE('',*,*,#54660,.T.);
#76856=ORIENTED_EDGE('',*,*,#54661,.T.);
#76857=ORIENTED_EDGE('',*,*,#54662,.T.);
#76858=ORIENTED_EDGE('',*,*,#54663,.T.);
#76859=ORIENTED_EDGE('',*,*,#54664,.T.);
#76860=ORIENTED_EDGE('',*,*,#54665,.T.);
#76861=ORIENTED_EDGE('',*,*,#54666,.T.);
#76862=ORIENTED_EDGE('',*,*,#54667,.T.);
#76863=ORIENTED_EDGE('',*,*,#54668,.T.);
#76864=ORIENTED_EDGE('',*,*,#54669,.T.);
#76865=ORIENTED_EDGE('',*,*,#54670,.T.);
#76866=ORIENTED_EDGE('',*,*,#54671,.T.);
#76867=ORIENTED_EDGE('',*,*,#54672,.T.);
#76868=ORIENTED_EDGE('',*,*,#54673,.T.);
#76869=ORIENTED_EDGE('',*,*,#54674,.T.);
#76870=ORIENTED_EDGE('',*,*,#54675,.T.);
#76871=ORIENTED_EDGE('',*,*,#54676,.T.);
#76872=ORIENTED_EDGE('',*,*,#54677,.T.);
#76873=ORIENTED_EDGE('',*,*,#54678,.T.);
#76874=ORIENTED_EDGE('',*,*,#54679,.T.);
#76875=ORIENTED_EDGE('',*,*,#54680,.T.);
#76876=ORIENTED_EDGE('',*,*,#54681,.T.);
#76877=ORIENTED_EDGE('',*,*,#54682,.T.);
#76878=ORIENTED_EDGE('',*,*,#54683,.T.);
#76879=ORIENTED_EDGE('',*,*,#54684,.T.);
#76880=ORIENTED_EDGE('',*,*,#54685,.T.);
#76881=ORIENTED_EDGE('',*,*,#54686,.T.);
#76882=ORIENTED_EDGE('',*,*,#54687,.T.);
#76883=ORIENTED_EDGE('',*,*,#54688,.T.);
#76884=ORIENTED_EDGE('',*,*,#54689,.T.);
#76885=ORIENTED_EDGE('',*,*,#54690,.T.);
#76886=ORIENTED_EDGE('',*,*,#54691,.T.);
#76887=ORIENTED_EDGE('',*,*,#54692,.T.);
#76888=ORIENTED_EDGE('',*,*,#54693,.T.);
#76889=ORIENTED_EDGE('',*,*,#54694,.T.);
#76890=ORIENTED_EDGE('',*,*,#54695,.T.);
#76891=ORIENTED_EDGE('',*,*,#54696,.T.);
#76892=ORIENTED_EDGE('',*,*,#54697,.T.);
#76893=ORIENTED_EDGE('',*,*,#54698,.T.);
#76894=ORIENTED_EDGE('',*,*,#54699,.T.);
#76895=ORIENTED_EDGE('',*,*,#54700,.T.);
#76896=ORIENTED_EDGE('',*,*,#54701,.T.);
#76897=ORIENTED_EDGE('',*,*,#54702,.T.);
#76898=ORIENTED_EDGE('',*,*,#54703,.T.);
#76899=ORIENTED_EDGE('',*,*,#54704,.T.);
#76900=ORIENTED_EDGE('',*,*,#54705,.T.);
#76901=ORIENTED_EDGE('',*,*,#54706,.T.);
#76902=ORIENTED_EDGE('',*,*,#54707,.T.);
#76903=ORIENTED_EDGE('',*,*,#54708,.T.);
#76904=ORIENTED_EDGE('',*,*,#54709,.T.);
#76905=ORIENTED_EDGE('',*,*,#54710,.T.);
#76906=ORIENTED_EDGE('',*,*,#54711,.T.);
#76907=ORIENTED_EDGE('',*,*,#54712,.T.);
#76908=ORIENTED_EDGE('',*,*,#54713,.T.);
#76909=ORIENTED_EDGE('',*,*,#54714,.T.);
#76910=ORIENTED_EDGE('',*,*,#54715,.T.);
#76911=ORIENTED_EDGE('',*,*,#54716,.T.);
#76912=ORIENTED_EDGE('',*,*,#54717,.T.);
#76913=ORIENTED_EDGE('',*,*,#54718,.T.);
#76914=ORIENTED_EDGE('',*,*,#54719,.T.);
#76915=ORIENTED_EDGE('',*,*,#54720,.T.);
#76916=ORIENTED_EDGE('',*,*,#54721,.T.);
#76917=ORIENTED_EDGE('',*,*,#54722,.T.);
#76918=ORIENTED_EDGE('',*,*,#54723,.T.);
#76919=ORIENTED_EDGE('',*,*,#54724,.T.);
#76920=ORIENTED_EDGE('',*,*,#54725,.T.);
#76921=ORIENTED_EDGE('',*,*,#54726,.T.);
#76922=ORIENTED_EDGE('',*,*,#54727,.T.);
#76923=ORIENTED_EDGE('',*,*,#54728,.T.);
#76924=ORIENTED_EDGE('',*,*,#54729,.T.);
#76925=ORIENTED_EDGE('',*,*,#54730,.T.);
#76926=ORIENTED_EDGE('',*,*,#54731,.T.);
#76927=ORIENTED_EDGE('',*,*,#54732,.T.);
#76928=ORIENTED_EDGE('',*,*,#54733,.T.);
#76929=ORIENTED_EDGE('',*,*,#54734,.T.);
#76930=ORIENTED_EDGE('',*,*,#54735,.T.);
#76931=ORIENTED_EDGE('',*,*,#54736,.T.);
#76932=ORIENTED_EDGE('',*,*,#54737,.T.);
#76933=ORIENTED_EDGE('',*,*,#54738,.T.);
#76934=ORIENTED_EDGE('',*,*,#54739,.T.);
#76935=ORIENTED_EDGE('',*,*,#54740,.T.);
#76936=ORIENTED_EDGE('',*,*,#54741,.T.);
#76937=ORIENTED_EDGE('',*,*,#54742,.T.);
#76938=ORIENTED_EDGE('',*,*,#54743,.T.);
#76939=ORIENTED_EDGE('',*,*,#54744,.T.);
#76940=ORIENTED_EDGE('',*,*,#54745,.T.);
#76941=ORIENTED_EDGE('',*,*,#54746,.T.);
#76942=ORIENTED_EDGE('',*,*,#54747,.T.);
#76943=ORIENTED_EDGE('',*,*,#54748,.T.);
#76944=ORIENTED_EDGE('',*,*,#54749,.T.);
#76945=ORIENTED_EDGE('',*,*,#54750,.T.);
#76946=ORIENTED_EDGE('',*,*,#54751,.T.);
#76947=ORIENTED_EDGE('',*,*,#54752,.T.);
#76948=ORIENTED_EDGE('',*,*,#54753,.T.);
#76949=ORIENTED_EDGE('',*,*,#54754,.T.);
#76950=ORIENTED_EDGE('',*,*,#54755,.T.);
#76951=ORIENTED_EDGE('',*,*,#54756,.T.);
#76952=ORIENTED_EDGE('',*,*,#54757,.T.);
#76953=ORIENTED_EDGE('',*,*,#54758,.T.);
#76954=ORIENTED_EDGE('',*,*,#54759,.T.);
#76955=ORIENTED_EDGE('',*,*,#54760,.T.);
#76956=ORIENTED_EDGE('',*,*,#54761,.T.);
#76957=ORIENTED_EDGE('',*,*,#54762,.T.);
#76958=ORIENTED_EDGE('',*,*,#54763,.T.);
#76959=ORIENTED_EDGE('',*,*,#54764,.T.);
#76960=ORIENTED_EDGE('',*,*,#54765,.T.);
#76961=ORIENTED_EDGE('',*,*,#54766,.T.);
#76962=ORIENTED_EDGE('',*,*,#54767,.T.);
#76963=ORIENTED_EDGE('',*,*,#54768,.T.);
#76964=ORIENTED_EDGE('',*,*,#54769,.T.);
#76965=ORIENTED_EDGE('',*,*,#54770,.T.);
#76966=ORIENTED_EDGE('',*,*,#54771,.T.);
#76967=ORIENTED_EDGE('',*,*,#54772,.T.);
#76968=ORIENTED_EDGE('',*,*,#54773,.T.);
#76969=ORIENTED_EDGE('',*,*,#54774,.T.);
#76970=ORIENTED_EDGE('',*,*,#54775,.T.);
#76971=ORIENTED_EDGE('',*,*,#54776,.T.);
#76972=ORIENTED_EDGE('',*,*,#54777,.T.);
#76973=ORIENTED_EDGE('',*,*,#54778,.T.);
#76974=ORIENTED_EDGE('',*,*,#54779,.T.);
#76975=ORIENTED_EDGE('',*,*,#54780,.T.);
#76976=ORIENTED_EDGE('',*,*,#54781,.T.);
#76977=ORIENTED_EDGE('',*,*,#54782,.T.);
#76978=ORIENTED_EDGE('',*,*,#54783,.T.);
#76979=ORIENTED_EDGE('',*,*,#54784,.T.);
#76980=ORIENTED_EDGE('',*,*,#54785,.T.);
#76981=ORIENTED_EDGE('',*,*,#54786,.T.);
#76982=ORIENTED_EDGE('',*,*,#54787,.T.);
#76983=ORIENTED_EDGE('',*,*,#54788,.T.);
#76984=ORIENTED_EDGE('',*,*,#54789,.T.);
#76985=ORIENTED_EDGE('',*,*,#54790,.T.);
#76986=ORIENTED_EDGE('',*,*,#54791,.T.);
#76987=ORIENTED_EDGE('',*,*,#54792,.T.);
#76988=ORIENTED_EDGE('',*,*,#54793,.T.);
#76989=ORIENTED_EDGE('',*,*,#54794,.T.);
#76990=ORIENTED_EDGE('',*,*,#54795,.T.);
#76991=ORIENTED_EDGE('',*,*,#54796,.T.);
#76992=ORIENTED_EDGE('',*,*,#54797,.T.);
#76993=ORIENTED_EDGE('',*,*,#54798,.T.);
#76994=ORIENTED_EDGE('',*,*,#54799,.T.);
#76995=ORIENTED_EDGE('',*,*,#54800,.T.);
#76996=ORIENTED_EDGE('',*,*,#54801,.T.);
#76997=ORIENTED_EDGE('',*,*,#54802,.T.);
#76998=ORIENTED_EDGE('',*,*,#54803,.T.);
#76999=ORIENTED_EDGE('',*,*,#54804,.T.);
#77000=ORIENTED_EDGE('',*,*,#54805,.T.);
#77001=ORIENTED_EDGE('',*,*,#54806,.T.);
#77002=ORIENTED_EDGE('',*,*,#54807,.T.);
#77003=ORIENTED_EDGE('',*,*,#54808,.T.);
#77004=ORIENTED_EDGE('',*,*,#54809,.T.);
#77005=ORIENTED_EDGE('',*,*,#54810,.T.);
#77006=ORIENTED_EDGE('',*,*,#54811,.T.);
#77007=ORIENTED_EDGE('',*,*,#54812,.T.);
#77008=ORIENTED_EDGE('',*,*,#54813,.T.);
#77009=ORIENTED_EDGE('',*,*,#54814,.T.);
#77010=ORIENTED_EDGE('',*,*,#54815,.T.);
#77011=ORIENTED_EDGE('',*,*,#54816,.T.);
#77012=ORIENTED_EDGE('',*,*,#54817,.T.);
#77013=ORIENTED_EDGE('',*,*,#54818,.T.);
#77014=ORIENTED_EDGE('',*,*,#54819,.T.);
#77015=ORIENTED_EDGE('',*,*,#54820,.T.);
#77016=ORIENTED_EDGE('',*,*,#54821,.T.);
#77017=ORIENTED_EDGE('',*,*,#54822,.T.);
#77018=ORIENTED_EDGE('',*,*,#54823,.T.);
#77019=ORIENTED_EDGE('',*,*,#54824,.T.);
#77020=ORIENTED_EDGE('',*,*,#54825,.T.);
#77021=ORIENTED_EDGE('',*,*,#54826,.T.);
#77022=ORIENTED_EDGE('',*,*,#54827,.T.);
#77023=ORIENTED_EDGE('',*,*,#54828,.T.);
#77024=ORIENTED_EDGE('',*,*,#54829,.T.);
#77025=ORIENTED_EDGE('',*,*,#54830,.T.);
#77026=ORIENTED_EDGE('',*,*,#54831,.T.);
#77027=ORIENTED_EDGE('',*,*,#54832,.T.);
#77028=ORIENTED_EDGE('',*,*,#54833,.T.);
#77029=ORIENTED_EDGE('',*,*,#54834,.T.);
#77030=ORIENTED_EDGE('',*,*,#54835,.T.);
#77031=ORIENTED_EDGE('',*,*,#54836,.T.);
#77032=ORIENTED_EDGE('',*,*,#54837,.T.);
#77033=ORIENTED_EDGE('',*,*,#54838,.T.);
#77034=ORIENTED_EDGE('',*,*,#54839,.T.);
#77035=ORIENTED_EDGE('',*,*,#54840,.T.);
#77036=ORIENTED_EDGE('',*,*,#54841,.T.);
#77037=ORIENTED_EDGE('',*,*,#54842,.T.);
#77038=ORIENTED_EDGE('',*,*,#54843,.T.);
#77039=ORIENTED_EDGE('',*,*,#54844,.T.);
#77040=ORIENTED_EDGE('',*,*,#54845,.T.);
#77041=ORIENTED_EDGE('',*,*,#54846,.T.);
#77042=ORIENTED_EDGE('',*,*,#54847,.T.);
#77043=ORIENTED_EDGE('',*,*,#54848,.T.);
#77044=ORIENTED_EDGE('',*,*,#54849,.T.);
#77045=ORIENTED_EDGE('',*,*,#54850,.T.);
#77046=ORIENTED_EDGE('',*,*,#54851,.T.);
#77047=ORIENTED_EDGE('',*,*,#54852,.T.);
#77048=ORIENTED_EDGE('',*,*,#54853,.T.);
#77049=ORIENTED_EDGE('',*,*,#54854,.T.);
#77050=ORIENTED_EDGE('',*,*,#54855,.T.);
#77051=ORIENTED_EDGE('',*,*,#54856,.T.);
#77052=ORIENTED_EDGE('',*,*,#54857,.T.);
#77053=ORIENTED_EDGE('',*,*,#54858,.T.);
#77054=ORIENTED_EDGE('',*,*,#54859,.T.);
#77055=ORIENTED_EDGE('',*,*,#54860,.T.);
#77056=ORIENTED_EDGE('',*,*,#54861,.T.);
#77057=ORIENTED_EDGE('',*,*,#54862,.T.);
#77058=ORIENTED_EDGE('',*,*,#54863,.T.);
#77059=ORIENTED_EDGE('',*,*,#54864,.T.);
#77060=ORIENTED_EDGE('',*,*,#54865,.T.);
#77061=ORIENTED_EDGE('',*,*,#54866,.T.);
#77062=ORIENTED_EDGE('',*,*,#54867,.T.);
#77063=ORIENTED_EDGE('',*,*,#54868,.T.);
#77064=ORIENTED_EDGE('',*,*,#54869,.T.);
#77065=ORIENTED_EDGE('',*,*,#54870,.T.);
#77066=ORIENTED_EDGE('',*,*,#54871,.T.);
#77067=ORIENTED_EDGE('',*,*,#54872,.T.);
#77068=ORIENTED_EDGE('',*,*,#54873,.T.);
#77069=ORIENTED_EDGE('',*,*,#54874,.T.);
#77070=ORIENTED_EDGE('',*,*,#54875,.T.);
#77071=ORIENTED_EDGE('',*,*,#54876,.T.);
#77072=ORIENTED_EDGE('',*,*,#54877,.T.);
#77073=ORIENTED_EDGE('',*,*,#54878,.T.);
#77074=ORIENTED_EDGE('',*,*,#54879,.T.);
#77075=ORIENTED_EDGE('',*,*,#54880,.T.);
#77076=ORIENTED_EDGE('',*,*,#54881,.T.);
#77077=ORIENTED_EDGE('',*,*,#54882,.T.);
#77078=ORIENTED_EDGE('',*,*,#54883,.T.);
#77079=ORIENTED_EDGE('',*,*,#54884,.T.);
#77080=ORIENTED_EDGE('',*,*,#54885,.T.);
#77081=ORIENTED_EDGE('',*,*,#54886,.T.);
#77082=ORIENTED_EDGE('',*,*,#54887,.T.);
#77083=ORIENTED_EDGE('',*,*,#54888,.T.);
#77084=ORIENTED_EDGE('',*,*,#54889,.T.);
#77085=ORIENTED_EDGE('',*,*,#54890,.T.);
#77086=ORIENTED_EDGE('',*,*,#54891,.T.);
#77087=ORIENTED_EDGE('',*,*,#54892,.T.);
#77088=ORIENTED_EDGE('',*,*,#54893,.T.);
#77089=ORIENTED_EDGE('',*,*,#54894,.T.);
#77090=ORIENTED_EDGE('',*,*,#54895,.T.);
#77091=ORIENTED_EDGE('',*,*,#54896,.T.);
#77092=ORIENTED_EDGE('',*,*,#54897,.T.);
#77093=ORIENTED_EDGE('',*,*,#54898,.T.);
#77094=ORIENTED_EDGE('',*,*,#54899,.T.);
#77095=ORIENTED_EDGE('',*,*,#54900,.T.);
#77096=ORIENTED_EDGE('',*,*,#54901,.T.);
#77097=ORIENTED_EDGE('',*,*,#54902,.T.);
#77098=ORIENTED_EDGE('',*,*,#54903,.T.);
#77099=ORIENTED_EDGE('',*,*,#54904,.T.);
#77100=ORIENTED_EDGE('',*,*,#54905,.T.);
#77101=ORIENTED_EDGE('',*,*,#54906,.T.);
#77102=ORIENTED_EDGE('',*,*,#54907,.T.);
#77103=ORIENTED_EDGE('',*,*,#54908,.T.);
#77104=ORIENTED_EDGE('',*,*,#54909,.T.);
#77105=ORIENTED_EDGE('',*,*,#54910,.T.);
#77106=ORIENTED_EDGE('',*,*,#54911,.T.);
#77107=ORIENTED_EDGE('',*,*,#54912,.T.);
#77108=ORIENTED_EDGE('',*,*,#54913,.T.);
#77109=ORIENTED_EDGE('',*,*,#54914,.T.);
#77110=ORIENTED_EDGE('',*,*,#54915,.T.);
#77111=ORIENTED_EDGE('',*,*,#54916,.T.);
#77112=ORIENTED_EDGE('',*,*,#54917,.T.);
#77113=ORIENTED_EDGE('',*,*,#54918,.T.);
#77114=ORIENTED_EDGE('',*,*,#54919,.T.);
#77115=ORIENTED_EDGE('',*,*,#54920,.T.);
#77116=ORIENTED_EDGE('',*,*,#54921,.T.);
#77117=ORIENTED_EDGE('',*,*,#54922,.T.);
#77118=ORIENTED_EDGE('',*,*,#54923,.T.);
#77119=ORIENTED_EDGE('',*,*,#54924,.T.);
#77120=ORIENTED_EDGE('',*,*,#54925,.T.);
#77121=ORIENTED_EDGE('',*,*,#54926,.T.);
#77122=ORIENTED_EDGE('',*,*,#54927,.T.);
#77123=ORIENTED_EDGE('',*,*,#54928,.T.);
#77124=ORIENTED_EDGE('',*,*,#54929,.T.);
#77125=ORIENTED_EDGE('',*,*,#54930,.T.);
#77126=ORIENTED_EDGE('',*,*,#54931,.T.);
#77127=ORIENTED_EDGE('',*,*,#54932,.T.);
#77128=ORIENTED_EDGE('',*,*,#54933,.T.);
#77129=ORIENTED_EDGE('',*,*,#54934,.T.);
#77130=ORIENTED_EDGE('',*,*,#54935,.T.);
#77131=ORIENTED_EDGE('',*,*,#54936,.T.);
#77132=ORIENTED_EDGE('',*,*,#54937,.T.);
#77133=ORIENTED_EDGE('',*,*,#54938,.T.);
#77134=ORIENTED_EDGE('',*,*,#54939,.T.);
#77135=ORIENTED_EDGE('',*,*,#54940,.T.);
#77136=ORIENTED_EDGE('',*,*,#54941,.T.);
#77137=ORIENTED_EDGE('',*,*,#54942,.T.);
#77138=ORIENTED_EDGE('',*,*,#54943,.T.);
#77139=ORIENTED_EDGE('',*,*,#54944,.T.);
#77140=ORIENTED_EDGE('',*,*,#54945,.T.);
#77141=ORIENTED_EDGE('',*,*,#54946,.T.);
#77142=ORIENTED_EDGE('',*,*,#54947,.T.);
#77143=ORIENTED_EDGE('',*,*,#54948,.T.);
#77144=ORIENTED_EDGE('',*,*,#54949,.T.);
#77145=ORIENTED_EDGE('',*,*,#54950,.T.);
#77146=ORIENTED_EDGE('',*,*,#54951,.T.);
#77147=ORIENTED_EDGE('',*,*,#54952,.T.);
#77148=ORIENTED_EDGE('',*,*,#54953,.T.);
#77149=ORIENTED_EDGE('',*,*,#54954,.T.);
#77150=ORIENTED_EDGE('',*,*,#54955,.T.);
#77151=ORIENTED_EDGE('',*,*,#54956,.T.);
#77152=ORIENTED_EDGE('',*,*,#54957,.T.);
#77153=ORIENTED_EDGE('',*,*,#54958,.T.);
#77154=ORIENTED_EDGE('',*,*,#54959,.T.);
#77155=ORIENTED_EDGE('',*,*,#54960,.T.);
#77156=ORIENTED_EDGE('',*,*,#54961,.T.);
#77157=ORIENTED_EDGE('',*,*,#54962,.T.);
#77158=ORIENTED_EDGE('',*,*,#54963,.T.);
#77159=ORIENTED_EDGE('',*,*,#54964,.T.);
#77160=ORIENTED_EDGE('',*,*,#54965,.T.);
#77161=ORIENTED_EDGE('',*,*,#54966,.T.);
#77162=ORIENTED_EDGE('',*,*,#54967,.T.);
#77163=ORIENTED_EDGE('',*,*,#54968,.T.);
#77164=ORIENTED_EDGE('',*,*,#54969,.T.);
#77165=ORIENTED_EDGE('',*,*,#54970,.T.);
#77166=ORIENTED_EDGE('',*,*,#54971,.T.);
#77167=ORIENTED_EDGE('',*,*,#54972,.T.);
#77168=ORIENTED_EDGE('',*,*,#54973,.T.);
#77169=ORIENTED_EDGE('',*,*,#54974,.T.);
#77170=ORIENTED_EDGE('',*,*,#54975,.T.);
#77171=ORIENTED_EDGE('',*,*,#54976,.T.);
#77172=ORIENTED_EDGE('',*,*,#54977,.T.);
#77173=ORIENTED_EDGE('',*,*,#54978,.T.);
#77174=ORIENTED_EDGE('',*,*,#54979,.T.);
#77175=ORIENTED_EDGE('',*,*,#54980,.T.);
#77176=ORIENTED_EDGE('',*,*,#54981,.T.);
#77177=ORIENTED_EDGE('',*,*,#54982,.T.);
#77178=ORIENTED_EDGE('',*,*,#54983,.T.);
#77179=ORIENTED_EDGE('',*,*,#54984,.T.);
#77180=ORIENTED_EDGE('',*,*,#54985,.T.);
#77181=ORIENTED_EDGE('',*,*,#54986,.T.);
#77182=ORIENTED_EDGE('',*,*,#54987,.T.);
#77183=ORIENTED_EDGE('',*,*,#54988,.T.);
#77184=ORIENTED_EDGE('',*,*,#54989,.T.);
#77185=ORIENTED_EDGE('',*,*,#54990,.T.);
#77186=ORIENTED_EDGE('',*,*,#54991,.T.);
#77187=ORIENTED_EDGE('',*,*,#54992,.T.);
#77188=ORIENTED_EDGE('',*,*,#54993,.T.);
#77189=ORIENTED_EDGE('',*,*,#54994,.T.);
#77190=ORIENTED_EDGE('',*,*,#54995,.T.);
#77191=ORIENTED_EDGE('',*,*,#54996,.T.);
#77192=ORIENTED_EDGE('',*,*,#54997,.T.);
#77193=ORIENTED_EDGE('',*,*,#54998,.T.);
#77194=ORIENTED_EDGE('',*,*,#54999,.T.);
#77195=ORIENTED_EDGE('',*,*,#55000,.T.);
#77196=ORIENTED_EDGE('',*,*,#55001,.T.);
#77197=ORIENTED_EDGE('',*,*,#55002,.T.);
#77198=ORIENTED_EDGE('',*,*,#55003,.T.);
#77199=ORIENTED_EDGE('',*,*,#55004,.T.);
#77200=ORIENTED_EDGE('',*,*,#55005,.T.);
#77201=ORIENTED_EDGE('',*,*,#55006,.T.);
#77202=ORIENTED_EDGE('',*,*,#55007,.T.);
#77203=ORIENTED_EDGE('',*,*,#55008,.T.);
#77204=ORIENTED_EDGE('',*,*,#55009,.T.);
#77205=ORIENTED_EDGE('',*,*,#55010,.T.);
#77206=ORIENTED_EDGE('',*,*,#55011,.T.);
#77207=ORIENTED_EDGE('',*,*,#55012,.T.);
#77208=ORIENTED_EDGE('',*,*,#55013,.T.);
#77209=ORIENTED_EDGE('',*,*,#55014,.T.);
#77210=ORIENTED_EDGE('',*,*,#55015,.T.);
#77211=ORIENTED_EDGE('',*,*,#55016,.T.);
#77212=ORIENTED_EDGE('',*,*,#55017,.T.);
#77213=ORIENTED_EDGE('',*,*,#55018,.T.);
#77214=ORIENTED_EDGE('',*,*,#55019,.T.);
#77215=ORIENTED_EDGE('',*,*,#55020,.T.);
#77216=ORIENTED_EDGE('',*,*,#55021,.T.);
#77217=ORIENTED_EDGE('',*,*,#55022,.T.);
#77218=ORIENTED_EDGE('',*,*,#55023,.T.);
#77219=ORIENTED_EDGE('',*,*,#55024,.T.);
#77220=ORIENTED_EDGE('',*,*,#55025,.T.);
#77221=ORIENTED_EDGE('',*,*,#55026,.T.);
#77222=ORIENTED_EDGE('',*,*,#55027,.T.);
#77223=ORIENTED_EDGE('',*,*,#55028,.T.);
#77224=ORIENTED_EDGE('',*,*,#55029,.T.);
#77225=ORIENTED_EDGE('',*,*,#55030,.T.);
#77226=ORIENTED_EDGE('',*,*,#55031,.T.);
#77227=ORIENTED_EDGE('',*,*,#55032,.T.);
#77228=ORIENTED_EDGE('',*,*,#55033,.T.);
#77229=ORIENTED_EDGE('',*,*,#55034,.T.);
#77230=ORIENTED_EDGE('',*,*,#55035,.T.);
#77231=ORIENTED_EDGE('',*,*,#55036,.T.);
#77232=ORIENTED_EDGE('',*,*,#55037,.T.);
#77233=ORIENTED_EDGE('',*,*,#55038,.T.);
#77234=ORIENTED_EDGE('',*,*,#55039,.T.);
#77235=ORIENTED_EDGE('',*,*,#55040,.T.);
#77236=ORIENTED_EDGE('',*,*,#55041,.T.);
#77237=ORIENTED_EDGE('',*,*,#55042,.T.);
#77238=ORIENTED_EDGE('',*,*,#55043,.T.);
#77239=ORIENTED_EDGE('',*,*,#55044,.T.);
#77240=ORIENTED_EDGE('',*,*,#55045,.T.);
#77241=ORIENTED_EDGE('',*,*,#55046,.T.);
#77242=ORIENTED_EDGE('',*,*,#55047,.T.);
#77243=ORIENTED_EDGE('',*,*,#55048,.T.);
#77244=ORIENTED_EDGE('',*,*,#55049,.T.);
#77245=ORIENTED_EDGE('',*,*,#55050,.T.);
#77246=ORIENTED_EDGE('',*,*,#55051,.T.);
#77247=ORIENTED_EDGE('',*,*,#55052,.T.);
#77248=ORIENTED_EDGE('',*,*,#55053,.T.);
#77249=ORIENTED_EDGE('',*,*,#55054,.T.);
#77250=ORIENTED_EDGE('',*,*,#55055,.T.);
#77251=ORIENTED_EDGE('',*,*,#55056,.T.);
#77252=ORIENTED_EDGE('',*,*,#55057,.T.);
#77253=ORIENTED_EDGE('',*,*,#55058,.T.);
#77254=ORIENTED_EDGE('',*,*,#55059,.T.);
#77255=ORIENTED_EDGE('',*,*,#55060,.T.);
#77256=ORIENTED_EDGE('',*,*,#55061,.T.);
#77257=ORIENTED_EDGE('',*,*,#55062,.T.);
#77258=ORIENTED_EDGE('',*,*,#55063,.T.);
#77259=ORIENTED_EDGE('',*,*,#55064,.T.);
#77260=ORIENTED_EDGE('',*,*,#55065,.T.);
#77261=ORIENTED_EDGE('',*,*,#55066,.T.);
#77262=ORIENTED_EDGE('',*,*,#55067,.T.);
#77263=ORIENTED_EDGE('',*,*,#55068,.T.);
#77264=ORIENTED_EDGE('',*,*,#55069,.T.);
#77265=ORIENTED_EDGE('',*,*,#55070,.T.);
#77266=ORIENTED_EDGE('',*,*,#55071,.T.);
#77267=ORIENTED_EDGE('',*,*,#55072,.T.);
#77268=ORIENTED_EDGE('',*,*,#55073,.T.);
#77269=ORIENTED_EDGE('',*,*,#55074,.T.);
#77270=ORIENTED_EDGE('',*,*,#55075,.T.);
#77271=ORIENTED_EDGE('',*,*,#55076,.T.);
#77272=ORIENTED_EDGE('',*,*,#55077,.T.);
#77273=ORIENTED_EDGE('',*,*,#55078,.T.);
#77274=ORIENTED_EDGE('',*,*,#55079,.T.);
#77275=ORIENTED_EDGE('',*,*,#55080,.T.);
#77276=ORIENTED_EDGE('',*,*,#55081,.T.);
#77277=ORIENTED_EDGE('',*,*,#55082,.T.);
#77278=ORIENTED_EDGE('',*,*,#55083,.T.);
#77279=ORIENTED_EDGE('',*,*,#55084,.T.);
#77280=ORIENTED_EDGE('',*,*,#55085,.T.);
#77281=ORIENTED_EDGE('',*,*,#55086,.T.);
#77282=ORIENTED_EDGE('',*,*,#55087,.T.);
#77283=ORIENTED_EDGE('',*,*,#55088,.T.);
#77284=ORIENTED_EDGE('',*,*,#55089,.T.);
#77285=ORIENTED_EDGE('',*,*,#55090,.T.);
#77286=ORIENTED_EDGE('',*,*,#55091,.T.);
#77287=ORIENTED_EDGE('',*,*,#55092,.T.);
#77288=ORIENTED_EDGE('',*,*,#55093,.T.);
#77289=ORIENTED_EDGE('',*,*,#55094,.T.);
#77290=ORIENTED_EDGE('',*,*,#55095,.T.);
#77291=ORIENTED_EDGE('',*,*,#55096,.T.);
#77292=ORIENTED_EDGE('',*,*,#55097,.T.);
#77293=ORIENTED_EDGE('',*,*,#55098,.T.);
#77294=ORIENTED_EDGE('',*,*,#55099,.T.);
#77295=ORIENTED_EDGE('',*,*,#55100,.T.);
#77296=ORIENTED_EDGE('',*,*,#55101,.T.);
#77297=ORIENTED_EDGE('',*,*,#55102,.T.);
#77298=ORIENTED_EDGE('',*,*,#55103,.T.);
#77299=ORIENTED_EDGE('',*,*,#55104,.T.);
#77300=ORIENTED_EDGE('',*,*,#55105,.T.);
#77301=ORIENTED_EDGE('',*,*,#55106,.T.);
#77302=ORIENTED_EDGE('',*,*,#55107,.T.);
#77303=ORIENTED_EDGE('',*,*,#55108,.T.);
#77304=ORIENTED_EDGE('',*,*,#55109,.T.);
#77305=ORIENTED_EDGE('',*,*,#55110,.T.);
#77306=ORIENTED_EDGE('',*,*,#55111,.T.);
#77307=ORIENTED_EDGE('',*,*,#55112,.T.);
#77308=ORIENTED_EDGE('',*,*,#55113,.T.);
#77309=ORIENTED_EDGE('',*,*,#55114,.T.);
#77310=ORIENTED_EDGE('',*,*,#55115,.T.);
#77311=ORIENTED_EDGE('',*,*,#55116,.T.);
#77312=ORIENTED_EDGE('',*,*,#55117,.T.);
#77313=ORIENTED_EDGE('',*,*,#55118,.T.);
#77314=ORIENTED_EDGE('',*,*,#55119,.T.);
#77315=ORIENTED_EDGE('',*,*,#55120,.T.);
#77316=ORIENTED_EDGE('',*,*,#55121,.T.);
#77317=ORIENTED_EDGE('',*,*,#55122,.T.);
#77318=ORIENTED_EDGE('',*,*,#55123,.T.);
#77319=ORIENTED_EDGE('',*,*,#55124,.T.);
#77320=ORIENTED_EDGE('',*,*,#55125,.T.);
#77321=ORIENTED_EDGE('',*,*,#55126,.T.);
#77322=ORIENTED_EDGE('',*,*,#55127,.T.);
#77323=ORIENTED_EDGE('',*,*,#55128,.T.);
#77324=ORIENTED_EDGE('',*,*,#55129,.T.);
#77325=ORIENTED_EDGE('',*,*,#55130,.T.);
#77326=ORIENTED_EDGE('',*,*,#55131,.T.);
#77327=ORIENTED_EDGE('',*,*,#55132,.T.);
#77328=ORIENTED_EDGE('',*,*,#55133,.T.);
#77329=ORIENTED_EDGE('',*,*,#55134,.T.);
#77330=ORIENTED_EDGE('',*,*,#55135,.T.);
#77331=ORIENTED_EDGE('',*,*,#55136,.T.);
#77332=ORIENTED_EDGE('',*,*,#55137,.T.);
#77333=ORIENTED_EDGE('',*,*,#55138,.T.);
#77334=ORIENTED_EDGE('',*,*,#55139,.T.);
#77335=ORIENTED_EDGE('',*,*,#55140,.T.);
#77336=ORIENTED_EDGE('',*,*,#55141,.T.);
#77337=ORIENTED_EDGE('',*,*,#55142,.T.);
#77338=ORIENTED_EDGE('',*,*,#55143,.T.);
#77339=ORIENTED_EDGE('',*,*,#55144,.T.);
#77340=ORIENTED_EDGE('',*,*,#55145,.T.);
#77341=ORIENTED_EDGE('',*,*,#55146,.T.);
#77342=ORIENTED_EDGE('',*,*,#55147,.T.);
#77343=ORIENTED_EDGE('',*,*,#55148,.T.);
#77344=ORIENTED_EDGE('',*,*,#55149,.T.);
#77345=ORIENTED_EDGE('',*,*,#55150,.T.);
#77346=ORIENTED_EDGE('',*,*,#55151,.T.);
#77347=ORIENTED_EDGE('',*,*,#55152,.T.);
#77348=ORIENTED_EDGE('',*,*,#55153,.T.);
#77349=ORIENTED_EDGE('',*,*,#55154,.T.);
#77350=ORIENTED_EDGE('',*,*,#55155,.T.);
#77351=ORIENTED_EDGE('',*,*,#55156,.T.);
#77352=ORIENTED_EDGE('',*,*,#55157,.T.);
#77353=ORIENTED_EDGE('',*,*,#55158,.T.);
#77354=ORIENTED_EDGE('',*,*,#55159,.T.);
#77355=ORIENTED_EDGE('',*,*,#55160,.T.);
#77356=ORIENTED_EDGE('',*,*,#55161,.T.);
#77357=ORIENTED_EDGE('',*,*,#55162,.T.);
#77358=ORIENTED_EDGE('',*,*,#55163,.T.);
#77359=ORIENTED_EDGE('',*,*,#55164,.T.);
#77360=ORIENTED_EDGE('',*,*,#55165,.T.);
#77361=ORIENTED_EDGE('',*,*,#55166,.T.);
#77362=ORIENTED_EDGE('',*,*,#55167,.T.);
#77363=ORIENTED_EDGE('',*,*,#55168,.T.);
#77364=ORIENTED_EDGE('',*,*,#55169,.T.);
#77365=ORIENTED_EDGE('',*,*,#55170,.T.);
#77366=ORIENTED_EDGE('',*,*,#55171,.T.);
#77367=ORIENTED_EDGE('',*,*,#55172,.T.);
#77368=ORIENTED_EDGE('',*,*,#55173,.T.);
#77369=ORIENTED_EDGE('',*,*,#55174,.T.);
#77370=ORIENTED_EDGE('',*,*,#55175,.T.);
#77371=ORIENTED_EDGE('',*,*,#55176,.T.);
#77372=ORIENTED_EDGE('',*,*,#55177,.T.);
#77373=ORIENTED_EDGE('',*,*,#55178,.T.);
#77374=ORIENTED_EDGE('',*,*,#55179,.T.);
#77375=ORIENTED_EDGE('',*,*,#55180,.T.);
#77376=ORIENTED_EDGE('',*,*,#55181,.T.);
#77377=ORIENTED_EDGE('',*,*,#55182,.T.);
#77378=ORIENTED_EDGE('',*,*,#55183,.T.);
#77379=ORIENTED_EDGE('',*,*,#55184,.T.);
#77380=ORIENTED_EDGE('',*,*,#55185,.T.);
#77381=ORIENTED_EDGE('',*,*,#55186,.T.);
#77382=ORIENTED_EDGE('',*,*,#55187,.T.);
#77383=ORIENTED_EDGE('',*,*,#55188,.T.);
#77384=ORIENTED_EDGE('',*,*,#55189,.T.);
#77385=ORIENTED_EDGE('',*,*,#55190,.T.);
#77386=ORIENTED_EDGE('',*,*,#55191,.T.);
#77387=ORIENTED_EDGE('',*,*,#55192,.T.);
#77388=ORIENTED_EDGE('',*,*,#55193,.T.);
#77389=ORIENTED_EDGE('',*,*,#55194,.T.);
#77390=ORIENTED_EDGE('',*,*,#55195,.T.);
#77391=ORIENTED_EDGE('',*,*,#55196,.T.);
#77392=ORIENTED_EDGE('',*,*,#55197,.T.);
#77393=ORIENTED_EDGE('',*,*,#55198,.T.);
#77394=ORIENTED_EDGE('',*,*,#55199,.T.);
#77395=ORIENTED_EDGE('',*,*,#55200,.T.);
#77396=ORIENTED_EDGE('',*,*,#55201,.T.);
#77397=ORIENTED_EDGE('',*,*,#55202,.T.);
#77398=ORIENTED_EDGE('',*,*,#55203,.T.);
#77399=ORIENTED_EDGE('',*,*,#55204,.T.);
#77400=ORIENTED_EDGE('',*,*,#55205,.T.);
#77401=ORIENTED_EDGE('',*,*,#55206,.T.);
#77402=ORIENTED_EDGE('',*,*,#55207,.T.);
#77403=ORIENTED_EDGE('',*,*,#55208,.T.);
#77404=ORIENTED_EDGE('',*,*,#55209,.T.);
#77405=ORIENTED_EDGE('',*,*,#55210,.T.);
#77406=ORIENTED_EDGE('',*,*,#55211,.T.);
#77407=ORIENTED_EDGE('',*,*,#55212,.T.);
#77408=ORIENTED_EDGE('',*,*,#55213,.T.);
#77409=ORIENTED_EDGE('',*,*,#55214,.T.);
#77410=ORIENTED_EDGE('',*,*,#55215,.T.);
#77411=ORIENTED_EDGE('',*,*,#55216,.T.);
#77412=ORIENTED_EDGE('',*,*,#55217,.T.);
#77413=ORIENTED_EDGE('',*,*,#55218,.T.);
#77414=ORIENTED_EDGE('',*,*,#55219,.T.);
#77415=ORIENTED_EDGE('',*,*,#55220,.T.);
#77416=ORIENTED_EDGE('',*,*,#55221,.T.);
#77417=ORIENTED_EDGE('',*,*,#55222,.T.);
#77418=ORIENTED_EDGE('',*,*,#55223,.T.);
#77419=ORIENTED_EDGE('',*,*,#55224,.T.);
#77420=ORIENTED_EDGE('',*,*,#55225,.T.);
#77421=ORIENTED_EDGE('',*,*,#55226,.T.);
#77422=ORIENTED_EDGE('',*,*,#55227,.T.);
#77423=ORIENTED_EDGE('',*,*,#55228,.T.);
#77424=ORIENTED_EDGE('',*,*,#55229,.T.);
#77425=ORIENTED_EDGE('',*,*,#55230,.T.);
#77426=ORIENTED_EDGE('',*,*,#55231,.T.);
#77427=ORIENTED_EDGE('',*,*,#55232,.T.);
#77428=ORIENTED_EDGE('',*,*,#55233,.T.);
#77429=ORIENTED_EDGE('',*,*,#55234,.T.);
#77430=ORIENTED_EDGE('',*,*,#55235,.T.);
#77431=ORIENTED_EDGE('',*,*,#55236,.T.);
#77432=ORIENTED_EDGE('',*,*,#55237,.T.);
#77433=ORIENTED_EDGE('',*,*,#55238,.T.);
#77434=ORIENTED_EDGE('',*,*,#55239,.T.);
#77435=ORIENTED_EDGE('',*,*,#55240,.T.);
#77436=ORIENTED_EDGE('',*,*,#55241,.T.);
#77437=ORIENTED_EDGE('',*,*,#55242,.T.);
#77438=ORIENTED_EDGE('',*,*,#55243,.T.);
#77439=ORIENTED_EDGE('',*,*,#55244,.T.);
#77440=ORIENTED_EDGE('',*,*,#55245,.T.);
#77441=ORIENTED_EDGE('',*,*,#55246,.T.);
#77442=ORIENTED_EDGE('',*,*,#55247,.T.);
#77443=ORIENTED_EDGE('',*,*,#55248,.T.);
#77444=ORIENTED_EDGE('',*,*,#55249,.T.);
#77445=ORIENTED_EDGE('',*,*,#55250,.T.);
#77446=ORIENTED_EDGE('',*,*,#55251,.T.);
#77447=ORIENTED_EDGE('',*,*,#55252,.T.);
#77448=ORIENTED_EDGE('',*,*,#55253,.T.);
#77449=ORIENTED_EDGE('',*,*,#55254,.T.);
#77450=ORIENTED_EDGE('',*,*,#55255,.T.);
#77451=ORIENTED_EDGE('',*,*,#55256,.T.);
#77452=ORIENTED_EDGE('',*,*,#55257,.T.);
#77453=ORIENTED_EDGE('',*,*,#55258,.T.);
#77454=ORIENTED_EDGE('',*,*,#55259,.T.);
#77455=ORIENTED_EDGE('',*,*,#55260,.T.);
#77456=ORIENTED_EDGE('',*,*,#55261,.T.);
#77457=ORIENTED_EDGE('',*,*,#55262,.T.);
#77458=ORIENTED_EDGE('',*,*,#55263,.T.);
#77459=ORIENTED_EDGE('',*,*,#55264,.T.);
#77460=ORIENTED_EDGE('',*,*,#55265,.T.);
#77461=ORIENTED_EDGE('',*,*,#55266,.T.);
#77462=ORIENTED_EDGE('',*,*,#55267,.T.);
#77463=ORIENTED_EDGE('',*,*,#55268,.T.);
#77464=ORIENTED_EDGE('',*,*,#55269,.T.);
#77465=ORIENTED_EDGE('',*,*,#55270,.T.);
#77466=ORIENTED_EDGE('',*,*,#55271,.T.);
#77467=ORIENTED_EDGE('',*,*,#55272,.T.);
#77468=ORIENTED_EDGE('',*,*,#55273,.T.);
#77469=ORIENTED_EDGE('',*,*,#55274,.T.);
#77470=ORIENTED_EDGE('',*,*,#55275,.T.);
#77471=ORIENTED_EDGE('',*,*,#55276,.T.);
#77472=ORIENTED_EDGE('',*,*,#55277,.T.);
#77473=ORIENTED_EDGE('',*,*,#55278,.T.);
#77474=ORIENTED_EDGE('',*,*,#55279,.T.);
#77475=ORIENTED_EDGE('',*,*,#55280,.T.);
#77476=ORIENTED_EDGE('',*,*,#55281,.T.);
#77477=ORIENTED_EDGE('',*,*,#55282,.T.);
#77478=ORIENTED_EDGE('',*,*,#55283,.T.);
#77479=ORIENTED_EDGE('',*,*,#55284,.T.);
#77480=ORIENTED_EDGE('',*,*,#55285,.T.);
#77481=ORIENTED_EDGE('',*,*,#55286,.T.);
#77482=ORIENTED_EDGE('',*,*,#55287,.T.);
#77483=ORIENTED_EDGE('',*,*,#55288,.T.);
#77484=ORIENTED_EDGE('',*,*,#55289,.T.);
#77485=ORIENTED_EDGE('',*,*,#55290,.T.);
#77486=ORIENTED_EDGE('',*,*,#55291,.T.);
#77487=ORIENTED_EDGE('',*,*,#55292,.T.);
#77488=ORIENTED_EDGE('',*,*,#55293,.T.);
#77489=ORIENTED_EDGE('',*,*,#55294,.T.);
#77490=ORIENTED_EDGE('',*,*,#55295,.T.);
#77491=ORIENTED_EDGE('',*,*,#55296,.T.);
#77492=ORIENTED_EDGE('',*,*,#55297,.T.);
#77493=ORIENTED_EDGE('',*,*,#55298,.T.);
#77494=ORIENTED_EDGE('',*,*,#55299,.T.);
#77495=ORIENTED_EDGE('',*,*,#55300,.T.);
#77496=ORIENTED_EDGE('',*,*,#55301,.T.);
#77497=ORIENTED_EDGE('',*,*,#55302,.T.);
#77498=ORIENTED_EDGE('',*,*,#55303,.T.);
#77499=ORIENTED_EDGE('',*,*,#55304,.T.);
#77500=ORIENTED_EDGE('',*,*,#55305,.T.);
#77501=ORIENTED_EDGE('',*,*,#55306,.T.);
#77502=ORIENTED_EDGE('',*,*,#55307,.T.);
#77503=ORIENTED_EDGE('',*,*,#55308,.T.);
#77504=ORIENTED_EDGE('',*,*,#55309,.T.);
#77505=ORIENTED_EDGE('',*,*,#55310,.T.);
#77506=ORIENTED_EDGE('',*,*,#55311,.T.);
#77507=ORIENTED_EDGE('',*,*,#55312,.T.);
#77508=ORIENTED_EDGE('',*,*,#55313,.T.);
#77509=ORIENTED_EDGE('',*,*,#55314,.T.);
#77510=ORIENTED_EDGE('',*,*,#55315,.T.);
#77511=ORIENTED_EDGE('',*,*,#55316,.T.);
#77512=ORIENTED_EDGE('',*,*,#55317,.T.);
#77513=ORIENTED_EDGE('',*,*,#55318,.T.);
#77514=ORIENTED_EDGE('',*,*,#55319,.T.);
#77515=ORIENTED_EDGE('',*,*,#55320,.T.);
#77516=ORIENTED_EDGE('',*,*,#55321,.T.);
#77517=ORIENTED_EDGE('',*,*,#55322,.T.);
#77518=ORIENTED_EDGE('',*,*,#55323,.T.);
#77519=ORIENTED_EDGE('',*,*,#55324,.T.);
#77520=ORIENTED_EDGE('',*,*,#55325,.T.);
#77521=ORIENTED_EDGE('',*,*,#55326,.T.);
#77522=ORIENTED_EDGE('',*,*,#55327,.T.);
#77523=ORIENTED_EDGE('',*,*,#55328,.T.);
#77524=ORIENTED_EDGE('',*,*,#55329,.T.);
#77525=ORIENTED_EDGE('',*,*,#55330,.T.);
#77526=ORIENTED_EDGE('',*,*,#55331,.T.);
#77527=ORIENTED_EDGE('',*,*,#55332,.T.);
#77528=ORIENTED_EDGE('',*,*,#55333,.T.);
#77529=ORIENTED_EDGE('',*,*,#55334,.T.);
#77530=ORIENTED_EDGE('',*,*,#55335,.T.);
#77531=ORIENTED_EDGE('',*,*,#55336,.T.);
#77532=ORIENTED_EDGE('',*,*,#55337,.T.);
#77533=ORIENTED_EDGE('',*,*,#55338,.T.);
#77534=ORIENTED_EDGE('',*,*,#55339,.T.);
#77535=ORIENTED_EDGE('',*,*,#55340,.T.);
#77536=ORIENTED_EDGE('',*,*,#55341,.T.);
#77537=ORIENTED_EDGE('',*,*,#55342,.T.);
#77538=ORIENTED_EDGE('',*,*,#55343,.T.);
#77539=ORIENTED_EDGE('',*,*,#55344,.T.);
#77540=ORIENTED_EDGE('',*,*,#55345,.T.);
#77541=ORIENTED_EDGE('',*,*,#55346,.T.);
#77542=ORIENTED_EDGE('',*,*,#55347,.T.);
#77543=ORIENTED_EDGE('',*,*,#55348,.T.);
#77544=ORIENTED_EDGE('',*,*,#55349,.T.);
#77545=ORIENTED_EDGE('',*,*,#55350,.T.);
#77546=ORIENTED_EDGE('',*,*,#55351,.T.);
#77547=ORIENTED_EDGE('',*,*,#55352,.T.);
#77548=ORIENTED_EDGE('',*,*,#55353,.T.);
#77549=ORIENTED_EDGE('',*,*,#55354,.T.);
#77550=ORIENTED_EDGE('',*,*,#55355,.T.);
#77551=ORIENTED_EDGE('',*,*,#55356,.T.);
#77552=ORIENTED_EDGE('',*,*,#55357,.T.);
#77553=ORIENTED_EDGE('',*,*,#55358,.T.);
#77554=ORIENTED_EDGE('',*,*,#55359,.T.);
#77555=ORIENTED_EDGE('',*,*,#55360,.T.);
#77556=ORIENTED_EDGE('',*,*,#55361,.T.);
#77557=ORIENTED_EDGE('',*,*,#55362,.T.);
#77558=ORIENTED_EDGE('',*,*,#55363,.T.);
#77559=ORIENTED_EDGE('',*,*,#55364,.T.);
#77560=ORIENTED_EDGE('',*,*,#55365,.T.);
#77561=ORIENTED_EDGE('',*,*,#55366,.T.);
#77562=ORIENTED_EDGE('',*,*,#55367,.T.);
#77563=ORIENTED_EDGE('',*,*,#55368,.T.);
#77564=ORIENTED_EDGE('',*,*,#55369,.T.);
#77565=ORIENTED_EDGE('',*,*,#55370,.T.);
#77566=ORIENTED_EDGE('',*,*,#55371,.T.);
#77567=ORIENTED_EDGE('',*,*,#55372,.T.);
#77568=ORIENTED_EDGE('',*,*,#55373,.T.);
#77569=ORIENTED_EDGE('',*,*,#55374,.T.);
#77570=ORIENTED_EDGE('',*,*,#55375,.T.);
#77571=ORIENTED_EDGE('',*,*,#55376,.T.);
#77572=ORIENTED_EDGE('',*,*,#55377,.T.);
#77573=ORIENTED_EDGE('',*,*,#55378,.T.);
#77574=ORIENTED_EDGE('',*,*,#55379,.T.);
#77575=ORIENTED_EDGE('',*,*,#55380,.T.);
#77576=ORIENTED_EDGE('',*,*,#55381,.T.);
#77577=ORIENTED_EDGE('',*,*,#55382,.T.);
#77578=ORIENTED_EDGE('',*,*,#55383,.T.);
#77579=ORIENTED_EDGE('',*,*,#55384,.T.);
#77580=ORIENTED_EDGE('',*,*,#55385,.T.);
#77581=ORIENTED_EDGE('',*,*,#55386,.T.);
#77582=ORIENTED_EDGE('',*,*,#55387,.T.);
#77583=ORIENTED_EDGE('',*,*,#55388,.T.);
#77584=ORIENTED_EDGE('',*,*,#55389,.T.);
#77585=ORIENTED_EDGE('',*,*,#55390,.T.);
#77586=ORIENTED_EDGE('',*,*,#55391,.T.);
#77587=ORIENTED_EDGE('',*,*,#55392,.T.);
#77588=ORIENTED_EDGE('',*,*,#55393,.T.);
#77589=ORIENTED_EDGE('',*,*,#55394,.T.);
#77590=ORIENTED_EDGE('',*,*,#55395,.T.);
#77591=ORIENTED_EDGE('',*,*,#55396,.T.);
#77592=ORIENTED_EDGE('',*,*,#55397,.T.);
#77593=ORIENTED_EDGE('',*,*,#55398,.T.);
#77594=ORIENTED_EDGE('',*,*,#55399,.T.);
#77595=ORIENTED_EDGE('',*,*,#55400,.T.);
#77596=ORIENTED_EDGE('',*,*,#55401,.T.);
#77597=ORIENTED_EDGE('',*,*,#55402,.T.);
#77598=ORIENTED_EDGE('',*,*,#55403,.T.);
#77599=ORIENTED_EDGE('',*,*,#55404,.T.);
#77600=ORIENTED_EDGE('',*,*,#55405,.T.);
#77601=ORIENTED_EDGE('',*,*,#55406,.T.);
#77602=ORIENTED_EDGE('',*,*,#55407,.T.);
#77603=ORIENTED_EDGE('',*,*,#55408,.T.);
#77604=ORIENTED_EDGE('',*,*,#55409,.T.);
#77605=ORIENTED_EDGE('',*,*,#55410,.T.);
#77606=ORIENTED_EDGE('',*,*,#55411,.T.);
#77607=ORIENTED_EDGE('',*,*,#55412,.T.);
#77608=ORIENTED_EDGE('',*,*,#55413,.T.);
#77609=ORIENTED_EDGE('',*,*,#55414,.T.);
#77610=ORIENTED_EDGE('',*,*,#55415,.T.);
#77611=ORIENTED_EDGE('',*,*,#55416,.T.);
#77612=ORIENTED_EDGE('',*,*,#55417,.T.);
#77613=ORIENTED_EDGE('',*,*,#55418,.T.);
#77614=ORIENTED_EDGE('',*,*,#55419,.T.);
#77615=ORIENTED_EDGE('',*,*,#55420,.T.);
#77616=ORIENTED_EDGE('',*,*,#55421,.T.);
#77617=ORIENTED_EDGE('',*,*,#55422,.T.);
#77618=ORIENTED_EDGE('',*,*,#55423,.T.);
#77619=ORIENTED_EDGE('',*,*,#55424,.T.);
#77620=ORIENTED_EDGE('',*,*,#55425,.T.);
#77621=ORIENTED_EDGE('',*,*,#55426,.T.);
#77622=ORIENTED_EDGE('',*,*,#55427,.T.);
#77623=ORIENTED_EDGE('',*,*,#55428,.T.);
#77624=ORIENTED_EDGE('',*,*,#55429,.T.);
#77625=ORIENTED_EDGE('',*,*,#55430,.T.);
#77626=ORIENTED_EDGE('',*,*,#55431,.T.);
#77627=ORIENTED_EDGE('',*,*,#55432,.T.);
#77628=ORIENTED_EDGE('',*,*,#55433,.T.);
#77629=ORIENTED_EDGE('',*,*,#55434,.T.);
#77630=ORIENTED_EDGE('',*,*,#55435,.T.);
#77631=ORIENTED_EDGE('',*,*,#55436,.T.);
#77632=ORIENTED_EDGE('',*,*,#55437,.T.);
#77633=ORIENTED_EDGE('',*,*,#55438,.T.);
#77634=ORIENTED_EDGE('',*,*,#55439,.T.);
#77635=ORIENTED_EDGE('',*,*,#55440,.T.);
#77636=ORIENTED_EDGE('',*,*,#55441,.T.);
#77637=ORIENTED_EDGE('',*,*,#55442,.T.);
#77638=ORIENTED_EDGE('',*,*,#55443,.T.);
#77639=ORIENTED_EDGE('',*,*,#55444,.T.);
#77640=ORIENTED_EDGE('',*,*,#55445,.T.);
#77641=ORIENTED_EDGE('',*,*,#55446,.T.);
#77642=ORIENTED_EDGE('',*,*,#55447,.T.);
#77643=ORIENTED_EDGE('',*,*,#55448,.T.);
#77644=ORIENTED_EDGE('',*,*,#55449,.T.);
#77645=ORIENTED_EDGE('',*,*,#55450,.T.);
#77646=ORIENTED_EDGE('',*,*,#55451,.T.);
#77647=ORIENTED_EDGE('',*,*,#55452,.T.);
#77648=ORIENTED_EDGE('',*,*,#55453,.T.);
#77649=ORIENTED_EDGE('',*,*,#55454,.T.);
#77650=ORIENTED_EDGE('',*,*,#55455,.T.);
#77651=ORIENTED_EDGE('',*,*,#55456,.T.);
#77652=ORIENTED_EDGE('',*,*,#55457,.T.);
#77653=ORIENTED_EDGE('',*,*,#55458,.T.);
#77654=ORIENTED_EDGE('',*,*,#55459,.T.);
#77655=ORIENTED_EDGE('',*,*,#55460,.T.);
#77656=ORIENTED_EDGE('',*,*,#52043,.T.);
#77657=ORIENTED_EDGE('',*,*,#55461,.T.);
#77658=ORIENTED_EDGE('',*,*,#52037,.T.);
#77659=ORIENTED_EDGE('',*,*,#55462,.T.);
#77660=ORIENTED_EDGE('',*,*,#55463,.T.);
#77661=ORIENTED_EDGE('',*,*,#55464,.T.);
#77662=ORIENTED_EDGE('',*,*,#55465,.T.);
#77663=ORIENTED_EDGE('',*,*,#55466,.T.);
#77664=ORIENTED_EDGE('',*,*,#55467,.T.);
#77665=ORIENTED_EDGE('',*,*,#55468,.T.);
#77666=ORIENTED_EDGE('',*,*,#55469,.T.);
#77667=ORIENTED_EDGE('',*,*,#55470,.T.);
#77668=ORIENTED_EDGE('',*,*,#55471,.T.);
#77669=ORIENTED_EDGE('',*,*,#55472,.T.);
#77670=ORIENTED_EDGE('',*,*,#55473,.T.);
#77671=ORIENTED_EDGE('',*,*,#55474,.T.);
#77672=ORIENTED_EDGE('',*,*,#55475,.T.);
#77673=ORIENTED_EDGE('',*,*,#55476,.T.);
#77674=ORIENTED_EDGE('',*,*,#55477,.T.);
#77675=ORIENTED_EDGE('',*,*,#55478,.T.);
#77676=ORIENTED_EDGE('',*,*,#55479,.T.);
#77677=ORIENTED_EDGE('',*,*,#55480,.T.);
#77678=ORIENTED_EDGE('',*,*,#55481,.T.);
#77679=ORIENTED_EDGE('',*,*,#55482,.T.);
#77680=ORIENTED_EDGE('',*,*,#55483,.T.);
#77681=ORIENTED_EDGE('',*,*,#55484,.T.);
#77682=ORIENTED_EDGE('',*,*,#55485,.T.);
#77683=ORIENTED_EDGE('',*,*,#55486,.T.);
#77684=ORIENTED_EDGE('',*,*,#55487,.T.);
#77685=ORIENTED_EDGE('',*,*,#55488,.T.);
#77686=ORIENTED_EDGE('',*,*,#55489,.T.);
#77687=ORIENTED_EDGE('',*,*,#55490,.T.);
#77688=ORIENTED_EDGE('',*,*,#55491,.T.);
#77689=ORIENTED_EDGE('',*,*,#55492,.T.);
#77690=ORIENTED_EDGE('',*,*,#55493,.T.);
#77691=ORIENTED_EDGE('',*,*,#55494,.T.);
#77692=ORIENTED_EDGE('',*,*,#55495,.T.);
#77693=ORIENTED_EDGE('',*,*,#55496,.T.);
#77694=ORIENTED_EDGE('',*,*,#55497,.T.);
#77695=ORIENTED_EDGE('',*,*,#55498,.T.);
#77696=ORIENTED_EDGE('',*,*,#55499,.T.);
#77697=ORIENTED_EDGE('',*,*,#55500,.T.);
#77698=ORIENTED_EDGE('',*,*,#55501,.T.);
#77699=ORIENTED_EDGE('',*,*,#55502,.T.);
#77700=ORIENTED_EDGE('',*,*,#55503,.T.);
#77701=ORIENTED_EDGE('',*,*,#55504,.T.);
#77702=ORIENTED_EDGE('',*,*,#55505,.T.);
#77703=ORIENTED_EDGE('',*,*,#55506,.T.);
#77704=ORIENTED_EDGE('',*,*,#55507,.T.);
#77705=ORIENTED_EDGE('',*,*,#55508,.T.);
#77706=ORIENTED_EDGE('',*,*,#55509,.T.);
#77707=ORIENTED_EDGE('',*,*,#55510,.T.);
#77708=ORIENTED_EDGE('',*,*,#55511,.T.);
#77709=ORIENTED_EDGE('',*,*,#55512,.T.);
#77710=ORIENTED_EDGE('',*,*,#55513,.T.);
#77711=ORIENTED_EDGE('',*,*,#55514,.T.);
#77712=ORIENTED_EDGE('',*,*,#55515,.T.);
#77713=ORIENTED_EDGE('',*,*,#55516,.T.);
#77714=ORIENTED_EDGE('',*,*,#55517,.T.);
#77715=ORIENTED_EDGE('',*,*,#55518,.T.);
#77716=ORIENTED_EDGE('',*,*,#55519,.T.);
#77717=ORIENTED_EDGE('',*,*,#55520,.T.);
#77718=ORIENTED_EDGE('',*,*,#55521,.T.);
#77719=ORIENTED_EDGE('',*,*,#55522,.T.);
#77720=ORIENTED_EDGE('',*,*,#55523,.T.);
#77721=ORIENTED_EDGE('',*,*,#55524,.T.);
#77722=ORIENTED_EDGE('',*,*,#55525,.T.);
#77723=ORIENTED_EDGE('',*,*,#55526,.T.);
#77724=ORIENTED_EDGE('',*,*,#55527,.T.);
#77725=ORIENTED_EDGE('',*,*,#55528,.T.);
#77726=ORIENTED_EDGE('',*,*,#55529,.T.);
#77727=ORIENTED_EDGE('',*,*,#55530,.T.);
#77728=ORIENTED_EDGE('',*,*,#55531,.T.);
#77729=ORIENTED_EDGE('',*,*,#55532,.T.);
#77730=ORIENTED_EDGE('',*,*,#55533,.T.);
#77731=ORIENTED_EDGE('',*,*,#55534,.T.);
#77732=ORIENTED_EDGE('',*,*,#55535,.T.);
#77733=ORIENTED_EDGE('',*,*,#55536,.T.);
#77734=ORIENTED_EDGE('',*,*,#55537,.T.);
#77735=ORIENTED_EDGE('',*,*,#55538,.T.);
#77736=ORIENTED_EDGE('',*,*,#55539,.T.);
#77737=ORIENTED_EDGE('',*,*,#55540,.T.);
#77738=ORIENTED_EDGE('',*,*,#55541,.T.);
#77739=ORIENTED_EDGE('',*,*,#55542,.T.);
#77740=ORIENTED_EDGE('',*,*,#55543,.T.);
#77741=ORIENTED_EDGE('',*,*,#55544,.T.);
#77742=ORIENTED_EDGE('',*,*,#55545,.T.);
#77743=ORIENTED_EDGE('',*,*,#55546,.T.);
#77744=ORIENTED_EDGE('',*,*,#55547,.T.);
#77745=ORIENTED_EDGE('',*,*,#55548,.T.);
#77746=ORIENTED_EDGE('',*,*,#55549,.T.);
#77747=ORIENTED_EDGE('',*,*,#55550,.T.);
#77748=ORIENTED_EDGE('',*,*,#55551,.T.);
#77749=ORIENTED_EDGE('',*,*,#55552,.T.);
#77750=ORIENTED_EDGE('',*,*,#55553,.T.);
#77751=ORIENTED_EDGE('',*,*,#55554,.T.);
#77752=ORIENTED_EDGE('',*,*,#55555,.T.);
#77753=ORIENTED_EDGE('',*,*,#55556,.T.);
#77754=ORIENTED_EDGE('',*,*,#55557,.T.);
#77755=ORIENTED_EDGE('',*,*,#55558,.T.);
#77756=ORIENTED_EDGE('',*,*,#55559,.T.);
#77757=ORIENTED_EDGE('',*,*,#55560,.T.);
#77758=ORIENTED_EDGE('',*,*,#55561,.T.);
#77759=ORIENTED_EDGE('',*,*,#55562,.T.);
#77760=ORIENTED_EDGE('',*,*,#55563,.T.);
#77761=ORIENTED_EDGE('',*,*,#55564,.T.);
#77762=ORIENTED_EDGE('',*,*,#55565,.T.);
#77763=ORIENTED_EDGE('',*,*,#55566,.T.);
#77764=ORIENTED_EDGE('',*,*,#55567,.T.);
#77765=ORIENTED_EDGE('',*,*,#55568,.T.);
#77766=ORIENTED_EDGE('',*,*,#55569,.T.);
#77767=ORIENTED_EDGE('',*,*,#55570,.T.);
#77768=ORIENTED_EDGE('',*,*,#55571,.T.);
#77769=ORIENTED_EDGE('',*,*,#55572,.T.);
#77770=ORIENTED_EDGE('',*,*,#55573,.T.);
#77771=ORIENTED_EDGE('',*,*,#55574,.T.);
#77772=ORIENTED_EDGE('',*,*,#55575,.T.);
#77773=ORIENTED_EDGE('',*,*,#55576,.T.);
#77774=ORIENTED_EDGE('',*,*,#55577,.T.);
#77775=ORIENTED_EDGE('',*,*,#55578,.T.);
#77776=ORIENTED_EDGE('',*,*,#55579,.T.);
#77777=ORIENTED_EDGE('',*,*,#55580,.T.);
#77778=ORIENTED_EDGE('',*,*,#55581,.T.);
#77779=ORIENTED_EDGE('',*,*,#55582,.T.);
#77780=ORIENTED_EDGE('',*,*,#55583,.T.);
#77781=ORIENTED_EDGE('',*,*,#55584,.T.);
#77782=ORIENTED_EDGE('',*,*,#55585,.T.);
#77783=ORIENTED_EDGE('',*,*,#55586,.T.);
#77784=ORIENTED_EDGE('',*,*,#55587,.T.);
#77785=ORIENTED_EDGE('',*,*,#55588,.T.);
#77786=ORIENTED_EDGE('',*,*,#55589,.T.);
#77787=ORIENTED_EDGE('',*,*,#55590,.T.);
#77788=ORIENTED_EDGE('',*,*,#55591,.T.);
#77789=ORIENTED_EDGE('',*,*,#55592,.T.);
#77790=ORIENTED_EDGE('',*,*,#55593,.T.);
#77791=ORIENTED_EDGE('',*,*,#55594,.T.);
#77792=ORIENTED_EDGE('',*,*,#55595,.T.);
#77793=ORIENTED_EDGE('',*,*,#55596,.T.);
#77794=ORIENTED_EDGE('',*,*,#55597,.T.);
#77795=ORIENTED_EDGE('',*,*,#55598,.T.);
#77796=ORIENTED_EDGE('',*,*,#55599,.T.);
#77797=ORIENTED_EDGE('',*,*,#55600,.T.);
#77798=ORIENTED_EDGE('',*,*,#55601,.T.);
#77799=ORIENTED_EDGE('',*,*,#55602,.T.);
#77800=ORIENTED_EDGE('',*,*,#55603,.T.);
#77801=ORIENTED_EDGE('',*,*,#55604,.T.);
#77802=ORIENTED_EDGE('',*,*,#55605,.T.);
#77803=ORIENTED_EDGE('',*,*,#55606,.T.);
#77804=ORIENTED_EDGE('',*,*,#55607,.T.);
#77805=ORIENTED_EDGE('',*,*,#55608,.T.);
#77806=ORIENTED_EDGE('',*,*,#55609,.T.);
#77807=ORIENTED_EDGE('',*,*,#55610,.T.);
#77808=ORIENTED_EDGE('',*,*,#55611,.T.);
#77809=ORIENTED_EDGE('',*,*,#55612,.T.);
#77810=ORIENTED_EDGE('',*,*,#55613,.T.);
#77811=ORIENTED_EDGE('',*,*,#55614,.T.);
#77812=ORIENTED_EDGE('',*,*,#55615,.T.);
#77813=ORIENTED_EDGE('',*,*,#55616,.T.);
#77814=ORIENTED_EDGE('',*,*,#55617,.T.);
#77815=ORIENTED_EDGE('',*,*,#55618,.T.);
#77816=ORIENTED_EDGE('',*,*,#55619,.T.);
#77817=ORIENTED_EDGE('',*,*,#55620,.T.);
#77818=ORIENTED_EDGE('',*,*,#55621,.T.);
#77819=ORIENTED_EDGE('',*,*,#55622,.T.);
#77820=ORIENTED_EDGE('',*,*,#55623,.T.);
#77821=ORIENTED_EDGE('',*,*,#55624,.T.);
#77822=ORIENTED_EDGE('',*,*,#55625,.T.);
#77823=ORIENTED_EDGE('',*,*,#55626,.T.);
#77824=ORIENTED_EDGE('',*,*,#55627,.T.);
#77825=ORIENTED_EDGE('',*,*,#55628,.T.);
#77826=ORIENTED_EDGE('',*,*,#55629,.T.);
#77827=ORIENTED_EDGE('',*,*,#55630,.T.);
#77828=ORIENTED_EDGE('',*,*,#55631,.T.);
#77829=ORIENTED_EDGE('',*,*,#55632,.T.);
#77830=ORIENTED_EDGE('',*,*,#55633,.T.);
#77831=ORIENTED_EDGE('',*,*,#55634,.T.);
#77832=ORIENTED_EDGE('',*,*,#55635,.T.);
#77833=ORIENTED_EDGE('',*,*,#55636,.T.);
#77834=ORIENTED_EDGE('',*,*,#55637,.T.);
#77835=ORIENTED_EDGE('',*,*,#55638,.T.);
#77836=ORIENTED_EDGE('',*,*,#55639,.T.);
#77837=ORIENTED_EDGE('',*,*,#55640,.T.);
#77838=ORIENTED_EDGE('',*,*,#55641,.T.);
#77839=ORIENTED_EDGE('',*,*,#55642,.T.);
#77840=ORIENTED_EDGE('',*,*,#55643,.T.);
#77841=ORIENTED_EDGE('',*,*,#55644,.T.);
#77842=ORIENTED_EDGE('',*,*,#55645,.T.);
#77843=ORIENTED_EDGE('',*,*,#55646,.T.);
#77844=ORIENTED_EDGE('',*,*,#55647,.T.);
#77845=ORIENTED_EDGE('',*,*,#55648,.T.);
#77846=ORIENTED_EDGE('',*,*,#55649,.T.);
#77847=ORIENTED_EDGE('',*,*,#55650,.T.);
#77848=ORIENTED_EDGE('',*,*,#55651,.T.);
#77849=ORIENTED_EDGE('',*,*,#55652,.T.);
#77850=ORIENTED_EDGE('',*,*,#55653,.T.);
#77851=ORIENTED_EDGE('',*,*,#55654,.T.);
#77852=ORIENTED_EDGE('',*,*,#55655,.T.);
#77853=ORIENTED_EDGE('',*,*,#55656,.T.);
#77854=ORIENTED_EDGE('',*,*,#55657,.T.);
#77855=ORIENTED_EDGE('',*,*,#55658,.T.);
#77856=ORIENTED_EDGE('',*,*,#55659,.T.);
#77857=ORIENTED_EDGE('',*,*,#55660,.T.);
#77858=ORIENTED_EDGE('',*,*,#55661,.T.);
#77859=ORIENTED_EDGE('',*,*,#55662,.T.);
#77860=ORIENTED_EDGE('',*,*,#55663,.T.);
#77861=ORIENTED_EDGE('',*,*,#55664,.T.);
#77862=ORIENTED_EDGE('',*,*,#55665,.T.);
#77863=ORIENTED_EDGE('',*,*,#55666,.T.);
#77864=ORIENTED_EDGE('',*,*,#55667,.T.);
#77865=ORIENTED_EDGE('',*,*,#55668,.T.);
#77866=ORIENTED_EDGE('',*,*,#55669,.T.);
#77867=ORIENTED_EDGE('',*,*,#55670,.T.);
#77868=ORIENTED_EDGE('',*,*,#55671,.T.);
#77869=ORIENTED_EDGE('',*,*,#55672,.T.);
#77870=ORIENTED_EDGE('',*,*,#55673,.T.);
#77871=ORIENTED_EDGE('',*,*,#55674,.T.);
#77872=ORIENTED_EDGE('',*,*,#55675,.T.);
#77873=ORIENTED_EDGE('',*,*,#55676,.T.);
#77874=ORIENTED_EDGE('',*,*,#55677,.T.);
#77875=ORIENTED_EDGE('',*,*,#55678,.T.);
#77876=ORIENTED_EDGE('',*,*,#55679,.T.);
#77877=ORIENTED_EDGE('',*,*,#55680,.T.);
#77878=ORIENTED_EDGE('',*,*,#55681,.T.);
#77879=ORIENTED_EDGE('',*,*,#55682,.T.);
#77880=ORIENTED_EDGE('',*,*,#55683,.T.);
#77881=ORIENTED_EDGE('',*,*,#55684,.T.);
#77882=ORIENTED_EDGE('',*,*,#55685,.T.);
#77883=ORIENTED_EDGE('',*,*,#55686,.T.);
#77884=ORIENTED_EDGE('',*,*,#55687,.T.);
#77885=ORIENTED_EDGE('',*,*,#55688,.T.);
#77886=ORIENTED_EDGE('',*,*,#55689,.T.);
#77887=ORIENTED_EDGE('',*,*,#55690,.T.);
#77888=ORIENTED_EDGE('',*,*,#55691,.T.);
#77889=ORIENTED_EDGE('',*,*,#55692,.T.);
#77890=ORIENTED_EDGE('',*,*,#55693,.T.);
#77891=ORIENTED_EDGE('',*,*,#55694,.T.);
#77892=ORIENTED_EDGE('',*,*,#55695,.T.);
#77893=ORIENTED_EDGE('',*,*,#55696,.T.);
#77894=ORIENTED_EDGE('',*,*,#55697,.T.);
#77895=ORIENTED_EDGE('',*,*,#55698,.T.);
#77896=ORIENTED_EDGE('',*,*,#55699,.T.);
#77897=ORIENTED_EDGE('',*,*,#55700,.T.);
#77898=ORIENTED_EDGE('',*,*,#55701,.T.);
#77899=ORIENTED_EDGE('',*,*,#55702,.T.);
#77900=ORIENTED_EDGE('',*,*,#55703,.T.);
#77901=ORIENTED_EDGE('',*,*,#55704,.T.);
#77902=ORIENTED_EDGE('',*,*,#55705,.T.);
#77903=ORIENTED_EDGE('',*,*,#55706,.T.);
#77904=ORIENTED_EDGE('',*,*,#55707,.T.);
#77905=ORIENTED_EDGE('',*,*,#55708,.T.);
#77906=ORIENTED_EDGE('',*,*,#55709,.T.);
#77907=ORIENTED_EDGE('',*,*,#55710,.T.);
#77908=ORIENTED_EDGE('',*,*,#55711,.T.);
#77909=ORIENTED_EDGE('',*,*,#55712,.T.);
#77910=ORIENTED_EDGE('',*,*,#55713,.T.);
#77911=ORIENTED_EDGE('',*,*,#55714,.T.);
#77912=ORIENTED_EDGE('',*,*,#55715,.T.);
#77913=ORIENTED_EDGE('',*,*,#55716,.T.);
#77914=ORIENTED_EDGE('',*,*,#55717,.T.);
#77915=ORIENTED_EDGE('',*,*,#55718,.T.);
#77916=ORIENTED_EDGE('',*,*,#55719,.T.);
#77917=ORIENTED_EDGE('',*,*,#55720,.T.);
#77918=ORIENTED_EDGE('',*,*,#55721,.T.);
#77919=ORIENTED_EDGE('',*,*,#55722,.T.);
#77920=ORIENTED_EDGE('',*,*,#55723,.T.);
#77921=ORIENTED_EDGE('',*,*,#55724,.T.);
#77922=ORIENTED_EDGE('',*,*,#55725,.T.);
#77923=ORIENTED_EDGE('',*,*,#55726,.T.);
#77924=ORIENTED_EDGE('',*,*,#55727,.T.);
#77925=ORIENTED_EDGE('',*,*,#55728,.T.);
#77926=ORIENTED_EDGE('',*,*,#55729,.T.);
#77927=ORIENTED_EDGE('',*,*,#55730,.T.);
#77928=ORIENTED_EDGE('',*,*,#55731,.T.);
#77929=ORIENTED_EDGE('',*,*,#55732,.T.);
#77930=ORIENTED_EDGE('',*,*,#55733,.T.);
#77931=ORIENTED_EDGE('',*,*,#55734,.T.);
#77932=ORIENTED_EDGE('',*,*,#55735,.T.);
#77933=ORIENTED_EDGE('',*,*,#55736,.T.);
#77934=ORIENTED_EDGE('',*,*,#55737,.T.);
#77935=ORIENTED_EDGE('',*,*,#55738,.T.);
#77936=ORIENTED_EDGE('',*,*,#55739,.T.);
#77937=ORIENTED_EDGE('',*,*,#55740,.T.);
#77938=ORIENTED_EDGE('',*,*,#55741,.T.);
#77939=ORIENTED_EDGE('',*,*,#55742,.T.);
#77940=ORIENTED_EDGE('',*,*,#55743,.T.);
#77941=ORIENTED_EDGE('',*,*,#55744,.T.);
#77942=ORIENTED_EDGE('',*,*,#55745,.T.);
#77943=ORIENTED_EDGE('',*,*,#55746,.T.);
#77944=ORIENTED_EDGE('',*,*,#55747,.T.);
#77945=ORIENTED_EDGE('',*,*,#55748,.T.);
#77946=ORIENTED_EDGE('',*,*,#55749,.T.);
#77947=ORIENTED_EDGE('',*,*,#55750,.T.);
#77948=ORIENTED_EDGE('',*,*,#55751,.T.);
#77949=ORIENTED_EDGE('',*,*,#55752,.T.);
#77950=ORIENTED_EDGE('',*,*,#55753,.T.);
#77951=ORIENTED_EDGE('',*,*,#55754,.T.);
#77952=ORIENTED_EDGE('',*,*,#55755,.T.);
#77953=ORIENTED_EDGE('',*,*,#55756,.T.);
#77954=ORIENTED_EDGE('',*,*,#55757,.T.);
#77955=ORIENTED_EDGE('',*,*,#55758,.T.);
#77956=ORIENTED_EDGE('',*,*,#55759,.T.);
#77957=ORIENTED_EDGE('',*,*,#55760,.T.);
#77958=ORIENTED_EDGE('',*,*,#55761,.T.);
#77959=ORIENTED_EDGE('',*,*,#55762,.T.);
#77960=ORIENTED_EDGE('',*,*,#55763,.T.);
#77961=ORIENTED_EDGE('',*,*,#55764,.T.);
#77962=ORIENTED_EDGE('',*,*,#55765,.T.);
#77963=ORIENTED_EDGE('',*,*,#55766,.T.);
#77964=ORIENTED_EDGE('',*,*,#55767,.T.);
#77965=ORIENTED_EDGE('',*,*,#55768,.T.);
#77966=ORIENTED_EDGE('',*,*,#55769,.T.);
#77967=ORIENTED_EDGE('',*,*,#55770,.T.);
#77968=ORIENTED_EDGE('',*,*,#55771,.T.);
#77969=ORIENTED_EDGE('',*,*,#55772,.T.);
#77970=ORIENTED_EDGE('',*,*,#55773,.T.);
#77971=ORIENTED_EDGE('',*,*,#55774,.T.);
#77972=ORIENTED_EDGE('',*,*,#55775,.T.);
#77973=ORIENTED_EDGE('',*,*,#55776,.T.);
#77974=ORIENTED_EDGE('',*,*,#55777,.T.);
#77975=ORIENTED_EDGE('',*,*,#55778,.T.);
#77976=ORIENTED_EDGE('',*,*,#55779,.T.);
#77977=ORIENTED_EDGE('',*,*,#55780,.T.);
#77978=ORIENTED_EDGE('',*,*,#55781,.T.);
#77979=ORIENTED_EDGE('',*,*,#55782,.T.);
#77980=ORIENTED_EDGE('',*,*,#55783,.T.);
#77981=ORIENTED_EDGE('',*,*,#55784,.T.);
#77982=ORIENTED_EDGE('',*,*,#55785,.T.);
#77983=ORIENTED_EDGE('',*,*,#55786,.T.);
#77984=ORIENTED_EDGE('',*,*,#55787,.T.);
#77985=ORIENTED_EDGE('',*,*,#55788,.T.);
#77986=ORIENTED_EDGE('',*,*,#55789,.T.);
#77987=ORIENTED_EDGE('',*,*,#55790,.T.);
#77988=ORIENTED_EDGE('',*,*,#55791,.T.);
#77989=ORIENTED_EDGE('',*,*,#55792,.T.);
#77990=ORIENTED_EDGE('',*,*,#55793,.T.);
#77991=ORIENTED_EDGE('',*,*,#55794,.T.);
#77992=ORIENTED_EDGE('',*,*,#55795,.T.);
#77993=ORIENTED_EDGE('',*,*,#55796,.T.);
#77994=ORIENTED_EDGE('',*,*,#55797,.T.);
#77995=ORIENTED_EDGE('',*,*,#55798,.T.);
#77996=ORIENTED_EDGE('',*,*,#55799,.T.);
#77997=ORIENTED_EDGE('',*,*,#55800,.T.);
#77998=ORIENTED_EDGE('',*,*,#55801,.T.);
#77999=ORIENTED_EDGE('',*,*,#55802,.T.);
#78000=ORIENTED_EDGE('',*,*,#55803,.T.);
#78001=ORIENTED_EDGE('',*,*,#55804,.T.);
#78002=ORIENTED_EDGE('',*,*,#55805,.T.);
#78003=ORIENTED_EDGE('',*,*,#55806,.T.);
#78004=ORIENTED_EDGE('',*,*,#55807,.T.);
#78005=ORIENTED_EDGE('',*,*,#55808,.T.);
#78006=ORIENTED_EDGE('',*,*,#55809,.T.);
#78007=ORIENTED_EDGE('',*,*,#55810,.T.);
#78008=ORIENTED_EDGE('',*,*,#55811,.T.);
#78009=ORIENTED_EDGE('',*,*,#55812,.T.);
#78010=ORIENTED_EDGE('',*,*,#55813,.T.);
#78011=ORIENTED_EDGE('',*,*,#55814,.T.);
#78012=ORIENTED_EDGE('',*,*,#55815,.T.);
#78013=ORIENTED_EDGE('',*,*,#55816,.T.);
#78014=ORIENTED_EDGE('',*,*,#55817,.T.);
#78015=ORIENTED_EDGE('',*,*,#55818,.T.);
#78016=ORIENTED_EDGE('',*,*,#55819,.T.);
#78017=ORIENTED_EDGE('',*,*,#55820,.T.);
#78018=ORIENTED_EDGE('',*,*,#55821,.T.);
#78019=ORIENTED_EDGE('',*,*,#55822,.T.);
#78020=ORIENTED_EDGE('',*,*,#55823,.T.);
#78021=ORIENTED_EDGE('',*,*,#55824,.T.);
#78022=ORIENTED_EDGE('',*,*,#55825,.T.);
#78023=ORIENTED_EDGE('',*,*,#55826,.T.);
#78024=ORIENTED_EDGE('',*,*,#55827,.T.);
#78025=ORIENTED_EDGE('',*,*,#55828,.T.);
#78026=ORIENTED_EDGE('',*,*,#55829,.T.);
#78027=ORIENTED_EDGE('',*,*,#55830,.T.);
#78028=ORIENTED_EDGE('',*,*,#55831,.T.);
#78029=ORIENTED_EDGE('',*,*,#55832,.T.);
#78030=ORIENTED_EDGE('',*,*,#55833,.T.);
#78031=ORIENTED_EDGE('',*,*,#55834,.T.);
#78032=ORIENTED_EDGE('',*,*,#55835,.T.);
#78033=ORIENTED_EDGE('',*,*,#55836,.T.);
#78034=ORIENTED_EDGE('',*,*,#55837,.T.);
#78035=ORIENTED_EDGE('',*,*,#55838,.T.);
#78036=ORIENTED_EDGE('',*,*,#55839,.T.);
#78037=ORIENTED_EDGE('',*,*,#55840,.T.);
#78038=ORIENTED_EDGE('',*,*,#55841,.T.);
#78039=ORIENTED_EDGE('',*,*,#55842,.T.);
#78040=ORIENTED_EDGE('',*,*,#55843,.T.);
#78041=ORIENTED_EDGE('',*,*,#55844,.T.);
#78042=ORIENTED_EDGE('',*,*,#55845,.T.);
#78043=ORIENTED_EDGE('',*,*,#55846,.T.);
#78044=ORIENTED_EDGE('',*,*,#55847,.T.);
#78045=ORIENTED_EDGE('',*,*,#55848,.T.);
#78046=ORIENTED_EDGE('',*,*,#55849,.T.);
#78047=ORIENTED_EDGE('',*,*,#55850,.T.);
#78048=ORIENTED_EDGE('',*,*,#55851,.T.);
#78049=ORIENTED_EDGE('',*,*,#55852,.T.);
#78050=ORIENTED_EDGE('',*,*,#55853,.T.);
#78051=ORIENTED_EDGE('',*,*,#55854,.T.);
#78052=ORIENTED_EDGE('',*,*,#55855,.T.);
#78053=ORIENTED_EDGE('',*,*,#55856,.T.);
#78054=ORIENTED_EDGE('',*,*,#55857,.T.);
#78055=ORIENTED_EDGE('',*,*,#55858,.T.);
#78056=ORIENTED_EDGE('',*,*,#55859,.T.);
#78057=ORIENTED_EDGE('',*,*,#55860,.T.);
#78058=ORIENTED_EDGE('',*,*,#55861,.T.);
#78059=ORIENTED_EDGE('',*,*,#55862,.T.);
#78060=ORIENTED_EDGE('',*,*,#55863,.T.);
#78061=ORIENTED_EDGE('',*,*,#55864,.T.);
#78062=ORIENTED_EDGE('',*,*,#55865,.T.);
#78063=ORIENTED_EDGE('',*,*,#55866,.T.);
#78064=ORIENTED_EDGE('',*,*,#55867,.T.);
#78065=ORIENTED_EDGE('',*,*,#55868,.T.);
#78066=ORIENTED_EDGE('',*,*,#55869,.T.);
#78067=ORIENTED_EDGE('',*,*,#55870,.T.);
#78068=ORIENTED_EDGE('',*,*,#55871,.T.);
#78069=ORIENTED_EDGE('',*,*,#55872,.T.);
#78070=ORIENTED_EDGE('',*,*,#55873,.T.);
#78071=ORIENTED_EDGE('',*,*,#55874,.T.);
#78072=ORIENTED_EDGE('',*,*,#55875,.T.);
#78073=ORIENTED_EDGE('',*,*,#55876,.T.);
#78074=ORIENTED_EDGE('',*,*,#55877,.T.);
#78075=ORIENTED_EDGE('',*,*,#55878,.T.);
#78076=ORIENTED_EDGE('',*,*,#52035,.T.);
#78077=ORIENTED_EDGE('',*,*,#55879,.T.);
#78078=ORIENTED_EDGE('',*,*,#52029,.T.);
#78079=ORIENTED_EDGE('',*,*,#55880,.T.);
#78080=ORIENTED_EDGE('',*,*,#55881,.T.);
#78081=ORIENTED_EDGE('',*,*,#55882,.T.);
#78082=ORIENTED_EDGE('',*,*,#55883,.T.);
#78083=ORIENTED_EDGE('',*,*,#55884,.T.);
#78084=ORIENTED_EDGE('',*,*,#55885,.T.);
#78085=ORIENTED_EDGE('',*,*,#55886,.T.);
#78086=ORIENTED_EDGE('',*,*,#55887,.T.);
#78087=ORIENTED_EDGE('',*,*,#55888,.T.);
#78088=ORIENTED_EDGE('',*,*,#55889,.T.);
#78089=ORIENTED_EDGE('',*,*,#55890,.T.);
#78090=ORIENTED_EDGE('',*,*,#55891,.T.);
#78091=ORIENTED_EDGE('',*,*,#55892,.T.);
#78092=ORIENTED_EDGE('',*,*,#55893,.T.);
#78093=ORIENTED_EDGE('',*,*,#55894,.T.);
#78094=ORIENTED_EDGE('',*,*,#55895,.T.);
#78095=ORIENTED_EDGE('',*,*,#55896,.T.);
#78096=ORIENTED_EDGE('',*,*,#55897,.T.);
#78097=ORIENTED_EDGE('',*,*,#55898,.T.);
#78098=ORIENTED_EDGE('',*,*,#55899,.T.);
#78099=ORIENTED_EDGE('',*,*,#55900,.T.);
#78100=ORIENTED_EDGE('',*,*,#55901,.T.);
#78101=ORIENTED_EDGE('',*,*,#55902,.T.);
#78102=ORIENTED_EDGE('',*,*,#55903,.T.);
#78103=ORIENTED_EDGE('',*,*,#55904,.T.);
#78104=ORIENTED_EDGE('',*,*,#55905,.T.);
#78105=ORIENTED_EDGE('',*,*,#55906,.T.);
#78106=ORIENTED_EDGE('',*,*,#55907,.T.);
#78107=ORIENTED_EDGE('',*,*,#55908,.T.);
#78108=ORIENTED_EDGE('',*,*,#55909,.T.);
#78109=ORIENTED_EDGE('',*,*,#55910,.T.);
#78110=ORIENTED_EDGE('',*,*,#55911,.T.);
#78111=ORIENTED_EDGE('',*,*,#55912,.T.);
#78112=ORIENTED_EDGE('',*,*,#55913,.T.);
#78113=ORIENTED_EDGE('',*,*,#55914,.T.);
#78114=ORIENTED_EDGE('',*,*,#55915,.T.);
#78115=ORIENTED_EDGE('',*,*,#55916,.T.);
#78116=ORIENTED_EDGE('',*,*,#55917,.T.);
#78117=ORIENTED_EDGE('',*,*,#55918,.T.);
#78118=ORIENTED_EDGE('',*,*,#55919,.T.);
#78119=ORIENTED_EDGE('',*,*,#55920,.T.);
#78120=ORIENTED_EDGE('',*,*,#55921,.T.);
#78121=ORIENTED_EDGE('',*,*,#55922,.T.);
#78122=ORIENTED_EDGE('',*,*,#55923,.T.);
#78123=ORIENTED_EDGE('',*,*,#55924,.T.);
#78124=ORIENTED_EDGE('',*,*,#55925,.T.);
#78125=ORIENTED_EDGE('',*,*,#55926,.T.);
#78126=ORIENTED_EDGE('',*,*,#55927,.T.);
#78127=ORIENTED_EDGE('',*,*,#55928,.T.);
#78128=ORIENTED_EDGE('',*,*,#55929,.T.);
#78129=ORIENTED_EDGE('',*,*,#55930,.T.);
#78130=ORIENTED_EDGE('',*,*,#55931,.T.);
#78131=ORIENTED_EDGE('',*,*,#55932,.T.);
#78132=ORIENTED_EDGE('',*,*,#55933,.T.);
#78133=ORIENTED_EDGE('',*,*,#55934,.T.);
#78134=ORIENTED_EDGE('',*,*,#55935,.T.);
#78135=ORIENTED_EDGE('',*,*,#55936,.T.);
#78136=ORIENTED_EDGE('',*,*,#55937,.T.);
#78137=ORIENTED_EDGE('',*,*,#55938,.T.);
#78138=ORIENTED_EDGE('',*,*,#55939,.T.);
#78139=ORIENTED_EDGE('',*,*,#55940,.T.);
#78140=ORIENTED_EDGE('',*,*,#55941,.T.);
#78141=ORIENTED_EDGE('',*,*,#55942,.T.);
#78142=ORIENTED_EDGE('',*,*,#55943,.T.);
#78143=ORIENTED_EDGE('',*,*,#55944,.T.);
#78144=ORIENTED_EDGE('',*,*,#55945,.T.);
#78145=ORIENTED_EDGE('',*,*,#55946,.T.);
#78146=ORIENTED_EDGE('',*,*,#55947,.T.);
#78147=ORIENTED_EDGE('',*,*,#55948,.T.);
#78148=ORIENTED_EDGE('',*,*,#55949,.T.);
#78149=ORIENTED_EDGE('',*,*,#55950,.T.);
#78150=ORIENTED_EDGE('',*,*,#55951,.T.);
#78151=ORIENTED_EDGE('',*,*,#55952,.T.);
#78152=ORIENTED_EDGE('',*,*,#55953,.T.);
#78153=ORIENTED_EDGE('',*,*,#55954,.T.);
#78154=ORIENTED_EDGE('',*,*,#55955,.T.);
#78155=ORIENTED_EDGE('',*,*,#55956,.T.);
#78156=ORIENTED_EDGE('',*,*,#55957,.T.);
#78157=ORIENTED_EDGE('',*,*,#55958,.T.);
#78158=ORIENTED_EDGE('',*,*,#55959,.T.);
#78159=ORIENTED_EDGE('',*,*,#55960,.T.);
#78160=ORIENTED_EDGE('',*,*,#55961,.T.);
#78161=ORIENTED_EDGE('',*,*,#55962,.T.);
#78162=ORIENTED_EDGE('',*,*,#55963,.T.);
#78163=ORIENTED_EDGE('',*,*,#55964,.T.);
#78164=ORIENTED_EDGE('',*,*,#55965,.T.);
#78165=ORIENTED_EDGE('',*,*,#55966,.T.);
#78166=ORIENTED_EDGE('',*,*,#55967,.T.);
#78167=ORIENTED_EDGE('',*,*,#55968,.T.);
#78168=ORIENTED_EDGE('',*,*,#55969,.T.);
#78169=ORIENTED_EDGE('',*,*,#55970,.T.);
#78170=ORIENTED_EDGE('',*,*,#55971,.T.);
#78171=ORIENTED_EDGE('',*,*,#55972,.T.);
#78172=ORIENTED_EDGE('',*,*,#55973,.T.);
#78173=ORIENTED_EDGE('',*,*,#55974,.T.);
#78174=ORIENTED_EDGE('',*,*,#55975,.T.);
#78175=ORIENTED_EDGE('',*,*,#55976,.T.);
#78176=ORIENTED_EDGE('',*,*,#55977,.T.);
#78177=ORIENTED_EDGE('',*,*,#55978,.T.);
#78178=ORIENTED_EDGE('',*,*,#55979,.T.);
#78179=ORIENTED_EDGE('',*,*,#55980,.T.);
#78180=ORIENTED_EDGE('',*,*,#55981,.T.);
#78181=ORIENTED_EDGE('',*,*,#55982,.T.);
#78182=ORIENTED_EDGE('',*,*,#55983,.T.);
#78183=ORIENTED_EDGE('',*,*,#55984,.T.);
#78184=ORIENTED_EDGE('',*,*,#55985,.T.);
#78185=ORIENTED_EDGE('',*,*,#55986,.T.);
#78186=ORIENTED_EDGE('',*,*,#55987,.T.);
#78187=ORIENTED_EDGE('',*,*,#55988,.T.);
#78188=ORIENTED_EDGE('',*,*,#55989,.T.);
#78189=ORIENTED_EDGE('',*,*,#55990,.T.);
#78190=ORIENTED_EDGE('',*,*,#55991,.T.);
#78191=ORIENTED_EDGE('',*,*,#55992,.T.);
#78192=ORIENTED_EDGE('',*,*,#55993,.T.);
#78193=ORIENTED_EDGE('',*,*,#55994,.T.);
#78194=ORIENTED_EDGE('',*,*,#55995,.T.);
#78195=ORIENTED_EDGE('',*,*,#55996,.T.);
#78196=ORIENTED_EDGE('',*,*,#55997,.T.);
#78197=ORIENTED_EDGE('',*,*,#55998,.T.);
#78198=ORIENTED_EDGE('',*,*,#55999,.T.);
#78199=ORIENTED_EDGE('',*,*,#56000,.T.);
#78200=ORIENTED_EDGE('',*,*,#56001,.T.);
#78201=ORIENTED_EDGE('',*,*,#56002,.T.);
#78202=ORIENTED_EDGE('',*,*,#56003,.T.);
#78203=ORIENTED_EDGE('',*,*,#56004,.T.);
#78204=ORIENTED_EDGE('',*,*,#56005,.T.);
#78205=ORIENTED_EDGE('',*,*,#56006,.T.);
#78206=ORIENTED_EDGE('',*,*,#56007,.T.);
#78207=ORIENTED_EDGE('',*,*,#56008,.T.);
#78208=ORIENTED_EDGE('',*,*,#56009,.T.);
#78209=ORIENTED_EDGE('',*,*,#56010,.T.);
#78210=ORIENTED_EDGE('',*,*,#56011,.T.);
#78211=ORIENTED_EDGE('',*,*,#56012,.T.);
#78212=ORIENTED_EDGE('',*,*,#56013,.T.);
#78213=ORIENTED_EDGE('',*,*,#56014,.T.);
#78214=ORIENTED_EDGE('',*,*,#56015,.T.);
#78215=ORIENTED_EDGE('',*,*,#56016,.T.);
#78216=ORIENTED_EDGE('',*,*,#56017,.T.);
#78217=ORIENTED_EDGE('',*,*,#56018,.T.);
#78218=ORIENTED_EDGE('',*,*,#56019,.T.);
#78219=ORIENTED_EDGE('',*,*,#56020,.T.);
#78220=ORIENTED_EDGE('',*,*,#56021,.T.);
#78221=ORIENTED_EDGE('',*,*,#56022,.T.);
#78222=ORIENTED_EDGE('',*,*,#56023,.T.);
#78223=ORIENTED_EDGE('',*,*,#56024,.T.);
#78224=ORIENTED_EDGE('',*,*,#56025,.T.);
#78225=ORIENTED_EDGE('',*,*,#56026,.T.);
#78226=ORIENTED_EDGE('',*,*,#56027,.T.);
#78227=ORIENTED_EDGE('',*,*,#56028,.T.);
#78228=ORIENTED_EDGE('',*,*,#56029,.T.);
#78229=ORIENTED_EDGE('',*,*,#56030,.T.);
#78230=ORIENTED_EDGE('',*,*,#56031,.T.);
#78231=ORIENTED_EDGE('',*,*,#56032,.T.);
#78232=ORIENTED_EDGE('',*,*,#56033,.T.);
#78233=ORIENTED_EDGE('',*,*,#56034,.T.);
#78234=ORIENTED_EDGE('',*,*,#56035,.T.);
#78235=ORIENTED_EDGE('',*,*,#56036,.T.);
#78236=ORIENTED_EDGE('',*,*,#56037,.T.);
#78237=ORIENTED_EDGE('',*,*,#56038,.T.);
#78238=ORIENTED_EDGE('',*,*,#56039,.T.);
#78239=ORIENTED_EDGE('',*,*,#56040,.T.);
#78240=ORIENTED_EDGE('',*,*,#56041,.T.);
#78241=ORIENTED_EDGE('',*,*,#56042,.T.);
#78242=ORIENTED_EDGE('',*,*,#56043,.T.);
#78243=ORIENTED_EDGE('',*,*,#56044,.T.);
#78244=ORIENTED_EDGE('',*,*,#56045,.T.);
#78245=ORIENTED_EDGE('',*,*,#56046,.T.);
#78246=ORIENTED_EDGE('',*,*,#56047,.T.);
#78247=ORIENTED_EDGE('',*,*,#56048,.T.);
#78248=ORIENTED_EDGE('',*,*,#56049,.T.);
#78249=ORIENTED_EDGE('',*,*,#56050,.T.);
#78250=ORIENTED_EDGE('',*,*,#56051,.T.);
#78251=ORIENTED_EDGE('',*,*,#56052,.T.);
#78252=ORIENTED_EDGE('',*,*,#56053,.T.);
#78253=ORIENTED_EDGE('',*,*,#56054,.T.);
#78254=ORIENTED_EDGE('',*,*,#56055,.T.);
#78255=ORIENTED_EDGE('',*,*,#56056,.T.);
#78256=ORIENTED_EDGE('',*,*,#56057,.T.);
#78257=ORIENTED_EDGE('',*,*,#56058,.T.);
#78258=ORIENTED_EDGE('',*,*,#56059,.T.);
#78259=ORIENTED_EDGE('',*,*,#56060,.T.);
#78260=ORIENTED_EDGE('',*,*,#56061,.T.);
#78261=ORIENTED_EDGE('',*,*,#56062,.T.);
#78262=ORIENTED_EDGE('',*,*,#56063,.T.);
#78263=ORIENTED_EDGE('',*,*,#56064,.T.);
#78264=ORIENTED_EDGE('',*,*,#56065,.T.);
#78265=ORIENTED_EDGE('',*,*,#56066,.T.);
#78266=ORIENTED_EDGE('',*,*,#56067,.T.);
#78267=ORIENTED_EDGE('',*,*,#56068,.T.);
#78268=ORIENTED_EDGE('',*,*,#56069,.T.);
#78269=ORIENTED_EDGE('',*,*,#56070,.T.);
#78270=ORIENTED_EDGE('',*,*,#56071,.T.);
#78271=ORIENTED_EDGE('',*,*,#56072,.T.);
#78272=ORIENTED_EDGE('',*,*,#56073,.T.);
#78273=ORIENTED_EDGE('',*,*,#56074,.T.);
#78274=ORIENTED_EDGE('',*,*,#56075,.T.);
#78275=ORIENTED_EDGE('',*,*,#56076,.T.);
#78276=ORIENTED_EDGE('',*,*,#56077,.T.);
#78277=ORIENTED_EDGE('',*,*,#56078,.T.);
#78278=ORIENTED_EDGE('',*,*,#56079,.T.);
#78279=ORIENTED_EDGE('',*,*,#56080,.T.);
#78280=ORIENTED_EDGE('',*,*,#56081,.T.);
#78281=ORIENTED_EDGE('',*,*,#56082,.T.);
#78282=ORIENTED_EDGE('',*,*,#56083,.T.);
#78283=ORIENTED_EDGE('',*,*,#56084,.T.);
#78284=ORIENTED_EDGE('',*,*,#56085,.T.);
#78285=ORIENTED_EDGE('',*,*,#56086,.T.);
#78286=ORIENTED_EDGE('',*,*,#56087,.T.);
#78287=ORIENTED_EDGE('',*,*,#56088,.T.);
#78288=ORIENTED_EDGE('',*,*,#56089,.T.);
#78289=ORIENTED_EDGE('',*,*,#56090,.T.);
#78290=ORIENTED_EDGE('',*,*,#56091,.T.);
#78291=ORIENTED_EDGE('',*,*,#56092,.T.);
#78292=ORIENTED_EDGE('',*,*,#56093,.T.);
#78293=ORIENTED_EDGE('',*,*,#56094,.T.);
#78294=ORIENTED_EDGE('',*,*,#56095,.T.);
#78295=ORIENTED_EDGE('',*,*,#56096,.T.);
#78296=ORIENTED_EDGE('',*,*,#56097,.T.);
#78297=ORIENTED_EDGE('',*,*,#56098,.T.);
#78298=ORIENTED_EDGE('',*,*,#56099,.T.);
#78299=ORIENTED_EDGE('',*,*,#56100,.T.);
#78300=ORIENTED_EDGE('',*,*,#56101,.T.);
#78301=ORIENTED_EDGE('',*,*,#56102,.T.);
#78302=ORIENTED_EDGE('',*,*,#56103,.T.);
#78303=ORIENTED_EDGE('',*,*,#56104,.T.);
#78304=ORIENTED_EDGE('',*,*,#56105,.T.);
#78305=ORIENTED_EDGE('',*,*,#56106,.T.);
#78306=ORIENTED_EDGE('',*,*,#56107,.T.);
#78307=ORIENTED_EDGE('',*,*,#56108,.T.);
#78308=ORIENTED_EDGE('',*,*,#56109,.T.);
#78309=ORIENTED_EDGE('',*,*,#56110,.T.);
#78310=ORIENTED_EDGE('',*,*,#56111,.T.);
#78311=ORIENTED_EDGE('',*,*,#56112,.T.);
#78312=ORIENTED_EDGE('',*,*,#56113,.T.);
#78313=ORIENTED_EDGE('',*,*,#56114,.T.);
#78314=ORIENTED_EDGE('',*,*,#56115,.T.);
#78315=ORIENTED_EDGE('',*,*,#56116,.T.);
#78316=ORIENTED_EDGE('',*,*,#56117,.T.);
#78317=ORIENTED_EDGE('',*,*,#56118,.T.);
#78318=ORIENTED_EDGE('',*,*,#56119,.T.);
#78319=ORIENTED_EDGE('',*,*,#56120,.T.);
#78320=ORIENTED_EDGE('',*,*,#56121,.T.);
#78321=ORIENTED_EDGE('',*,*,#56122,.T.);
#78322=ORIENTED_EDGE('',*,*,#56123,.T.);
#78323=ORIENTED_EDGE('',*,*,#56124,.T.);
#78324=ORIENTED_EDGE('',*,*,#56125,.T.);
#78325=ORIENTED_EDGE('',*,*,#56126,.T.);
#78326=ORIENTED_EDGE('',*,*,#56127,.T.);
#78327=ORIENTED_EDGE('',*,*,#56128,.T.);
#78328=ORIENTED_EDGE('',*,*,#56129,.T.);
#78329=ORIENTED_EDGE('',*,*,#56130,.T.);
#78330=ORIENTED_EDGE('',*,*,#56131,.T.);
#78331=ORIENTED_EDGE('',*,*,#56132,.T.);
#78332=ORIENTED_EDGE('',*,*,#56133,.T.);
#78333=ORIENTED_EDGE('',*,*,#56134,.T.);
#78334=ORIENTED_EDGE('',*,*,#56135,.T.);
#78335=ORIENTED_EDGE('',*,*,#56136,.T.);
#78336=ORIENTED_EDGE('',*,*,#56137,.T.);
#78337=ORIENTED_EDGE('',*,*,#56138,.T.);
#78338=ORIENTED_EDGE('',*,*,#56139,.T.);
#78339=ORIENTED_EDGE('',*,*,#56140,.T.);
#78340=ORIENTED_EDGE('',*,*,#56141,.T.);
#78341=ORIENTED_EDGE('',*,*,#56142,.T.);
#78342=ORIENTED_EDGE('',*,*,#56143,.T.);
#78343=ORIENTED_EDGE('',*,*,#56144,.T.);
#78344=ORIENTED_EDGE('',*,*,#56145,.T.);
#78345=ORIENTED_EDGE('',*,*,#56146,.T.);
#78346=ORIENTED_EDGE('',*,*,#56147,.T.);
#78347=ORIENTED_EDGE('',*,*,#56148,.T.);
#78348=ORIENTED_EDGE('',*,*,#56149,.T.);
#78349=ORIENTED_EDGE('',*,*,#56150,.T.);
#78350=ORIENTED_EDGE('',*,*,#56151,.T.);
#78351=ORIENTED_EDGE('',*,*,#56152,.T.);
#78352=ORIENTED_EDGE('',*,*,#56153,.T.);
#78353=ORIENTED_EDGE('',*,*,#56154,.T.);
#78354=ORIENTED_EDGE('',*,*,#56155,.T.);
#78355=ORIENTED_EDGE('',*,*,#56156,.T.);
#78356=ORIENTED_EDGE('',*,*,#56157,.T.);
#78357=ORIENTED_EDGE('',*,*,#56158,.T.);
#78358=ORIENTED_EDGE('',*,*,#56159,.T.);
#78359=ORIENTED_EDGE('',*,*,#56160,.T.);
#78360=ORIENTED_EDGE('',*,*,#56161,.T.);
#78361=ORIENTED_EDGE('',*,*,#56162,.T.);
#78362=ORIENTED_EDGE('',*,*,#56163,.T.);
#78363=ORIENTED_EDGE('',*,*,#56164,.T.);
#78364=ORIENTED_EDGE('',*,*,#56165,.T.);
#78365=ORIENTED_EDGE('',*,*,#56166,.T.);
#78366=ORIENTED_EDGE('',*,*,#56167,.T.);
#78367=ORIENTED_EDGE('',*,*,#56168,.T.);
#78368=ORIENTED_EDGE('',*,*,#56169,.T.);
#78369=ORIENTED_EDGE('',*,*,#56170,.T.);
#78370=ORIENTED_EDGE('',*,*,#56171,.T.);
#78371=ORIENTED_EDGE('',*,*,#56172,.T.);
#78372=ORIENTED_EDGE('',*,*,#56173,.T.);
#78373=ORIENTED_EDGE('',*,*,#56174,.T.);
#78374=ORIENTED_EDGE('',*,*,#56175,.T.);
#78375=ORIENTED_EDGE('',*,*,#56176,.T.);
#78376=ORIENTED_EDGE('',*,*,#56177,.T.);
#78377=ORIENTED_EDGE('',*,*,#56178,.T.);
#78378=ORIENTED_EDGE('',*,*,#56179,.T.);
#78379=ORIENTED_EDGE('',*,*,#56180,.T.);
#78380=ORIENTED_EDGE('',*,*,#56181,.T.);
#78381=ORIENTED_EDGE('',*,*,#56182,.T.);
#78382=ORIENTED_EDGE('',*,*,#56183,.T.);
#78383=ORIENTED_EDGE('',*,*,#56184,.T.);
#78384=ORIENTED_EDGE('',*,*,#56185,.T.);
#78385=ORIENTED_EDGE('',*,*,#56186,.T.);
#78386=ORIENTED_EDGE('',*,*,#56187,.T.);
#78387=ORIENTED_EDGE('',*,*,#56188,.T.);
#78388=ORIENTED_EDGE('',*,*,#56189,.T.);
#78389=ORIENTED_EDGE('',*,*,#56190,.T.);
#78390=ORIENTED_EDGE('',*,*,#56191,.T.);
#78391=ORIENTED_EDGE('',*,*,#56192,.T.);
#78392=ORIENTED_EDGE('',*,*,#56193,.T.);
#78393=ORIENTED_EDGE('',*,*,#56194,.T.);
#78394=ORIENTED_EDGE('',*,*,#56195,.T.);
#78395=ORIENTED_EDGE('',*,*,#56196,.T.);
#78396=ORIENTED_EDGE('',*,*,#56197,.T.);
#78397=ORIENTED_EDGE('',*,*,#56198,.T.);
#78398=ORIENTED_EDGE('',*,*,#56199,.T.);
#78399=ORIENTED_EDGE('',*,*,#56200,.T.);
#78400=ORIENTED_EDGE('',*,*,#56201,.T.);
#78401=ORIENTED_EDGE('',*,*,#56202,.T.);
#78402=ORIENTED_EDGE('',*,*,#56203,.T.);
#78403=ORIENTED_EDGE('',*,*,#56204,.T.);
#78404=ORIENTED_EDGE('',*,*,#56205,.T.);
#78405=ORIENTED_EDGE('',*,*,#56206,.T.);
#78406=ORIENTED_EDGE('',*,*,#56207,.T.);
#78407=ORIENTED_EDGE('',*,*,#56208,.T.);
#78408=ORIENTED_EDGE('',*,*,#56209,.T.);
#78409=ORIENTED_EDGE('',*,*,#56210,.T.);
#78410=ORIENTED_EDGE('',*,*,#56211,.T.);
#78411=ORIENTED_EDGE('',*,*,#56212,.T.);
#78412=ORIENTED_EDGE('',*,*,#56213,.T.);
#78413=ORIENTED_EDGE('',*,*,#56214,.T.);
#78414=ORIENTED_EDGE('',*,*,#56215,.T.);
#78415=ORIENTED_EDGE('',*,*,#56216,.T.);
#78416=ORIENTED_EDGE('',*,*,#56217,.T.);
#78417=ORIENTED_EDGE('',*,*,#56218,.T.);
#78418=ORIENTED_EDGE('',*,*,#56219,.T.);
#78419=ORIENTED_EDGE('',*,*,#56220,.T.);
#78420=ORIENTED_EDGE('',*,*,#56221,.T.);
#78421=ORIENTED_EDGE('',*,*,#56222,.T.);
#78422=ORIENTED_EDGE('',*,*,#56223,.T.);
#78423=ORIENTED_EDGE('',*,*,#56224,.T.);
#78424=ORIENTED_EDGE('',*,*,#56225,.T.);
#78425=ORIENTED_EDGE('',*,*,#56226,.T.);
#78426=ORIENTED_EDGE('',*,*,#56227,.T.);
#78427=ORIENTED_EDGE('',*,*,#56228,.T.);
#78428=ORIENTED_EDGE('',*,*,#56229,.T.);
#78429=ORIENTED_EDGE('',*,*,#56230,.T.);
#78430=ORIENTED_EDGE('',*,*,#56231,.T.);
#78431=ORIENTED_EDGE('',*,*,#56232,.T.);
#78432=ORIENTED_EDGE('',*,*,#56233,.T.);
#78433=ORIENTED_EDGE('',*,*,#56234,.T.);
#78434=ORIENTED_EDGE('',*,*,#56235,.T.);
#78435=ORIENTED_EDGE('',*,*,#56236,.T.);
#78436=ORIENTED_EDGE('',*,*,#56237,.T.);
#78437=ORIENTED_EDGE('',*,*,#56238,.T.);
#78438=ORIENTED_EDGE('',*,*,#56239,.T.);
#78439=ORIENTED_EDGE('',*,*,#56240,.T.);
#78440=ORIENTED_EDGE('',*,*,#56241,.T.);
#78441=ORIENTED_EDGE('',*,*,#56242,.T.);
#78442=ORIENTED_EDGE('',*,*,#56243,.T.);
#78443=ORIENTED_EDGE('',*,*,#56244,.T.);
#78444=ORIENTED_EDGE('',*,*,#56245,.T.);
#78445=ORIENTED_EDGE('',*,*,#56246,.T.);
#78446=ORIENTED_EDGE('',*,*,#56247,.T.);
#78447=ORIENTED_EDGE('',*,*,#56248,.T.);
#78448=ORIENTED_EDGE('',*,*,#56249,.T.);
#78449=ORIENTED_EDGE('',*,*,#56250,.T.);
#78450=ORIENTED_EDGE('',*,*,#56251,.T.);
#78451=ORIENTED_EDGE('',*,*,#56252,.T.);
#78452=ORIENTED_EDGE('',*,*,#56253,.T.);
#78453=ORIENTED_EDGE('',*,*,#56254,.T.);
#78454=ORIENTED_EDGE('',*,*,#56255,.T.);
#78455=ORIENTED_EDGE('',*,*,#56256,.T.);
#78456=ORIENTED_EDGE('',*,*,#56257,.T.);
#78457=ORIENTED_EDGE('',*,*,#56258,.T.);
#78458=ORIENTED_EDGE('',*,*,#56259,.T.);
#78459=ORIENTED_EDGE('',*,*,#56260,.T.);
#78460=ORIENTED_EDGE('',*,*,#56261,.T.);
#78461=ORIENTED_EDGE('',*,*,#56262,.T.);
#78462=ORIENTED_EDGE('',*,*,#56263,.T.);
#78463=ORIENTED_EDGE('',*,*,#56264,.T.);
#78464=ORIENTED_EDGE('',*,*,#56265,.T.);
#78465=ORIENTED_EDGE('',*,*,#56266,.T.);
#78466=ORIENTED_EDGE('',*,*,#56267,.T.);
#78467=ORIENTED_EDGE('',*,*,#56268,.T.);
#78468=ORIENTED_EDGE('',*,*,#56269,.T.);
#78469=ORIENTED_EDGE('',*,*,#56270,.T.);
#78470=ORIENTED_EDGE('',*,*,#56271,.T.);
#78471=ORIENTED_EDGE('',*,*,#56272,.T.);
#78472=ORIENTED_EDGE('',*,*,#56273,.T.);
#78473=ORIENTED_EDGE('',*,*,#56274,.T.);
#78474=ORIENTED_EDGE('',*,*,#56275,.T.);
#78475=ORIENTED_EDGE('',*,*,#56276,.T.);
#78476=ORIENTED_EDGE('',*,*,#56277,.T.);
#78477=ORIENTED_EDGE('',*,*,#56278,.T.);
#78478=ORIENTED_EDGE('',*,*,#56279,.T.);
#78479=ORIENTED_EDGE('',*,*,#56280,.T.);
#78480=ORIENTED_EDGE('',*,*,#56281,.T.);
#78481=ORIENTED_EDGE('',*,*,#56282,.T.);
#78482=ORIENTED_EDGE('',*,*,#56283,.T.);
#78483=ORIENTED_EDGE('',*,*,#56284,.T.);
#78484=ORIENTED_EDGE('',*,*,#56285,.T.);
#78485=ORIENTED_EDGE('',*,*,#56286,.T.);
#78486=ORIENTED_EDGE('',*,*,#56287,.T.);
#78487=ORIENTED_EDGE('',*,*,#56288,.T.);
#78488=ORIENTED_EDGE('',*,*,#56289,.T.);
#78489=ORIENTED_EDGE('',*,*,#56290,.T.);
#78490=ORIENTED_EDGE('',*,*,#56291,.T.);
#78491=ORIENTED_EDGE('',*,*,#56292,.T.);
#78492=ORIENTED_EDGE('',*,*,#56293,.T.);
#78493=ORIENTED_EDGE('',*,*,#56294,.T.);
#78494=ORIENTED_EDGE('',*,*,#56295,.T.);
#78495=ORIENTED_EDGE('',*,*,#54666,.F.);
#78496=ORIENTED_EDGE('',*,*,#56296,.T.);
#78497=ORIENTED_EDGE('',*,*,#54648,.F.);
#78498=ORIENTED_EDGE('',*,*,#56297,.T.);
#78499=ORIENTED_EDGE('',*,*,#54650,.F.);
#78500=ORIENTED_EDGE('',*,*,#56298,.T.);
#78501=ORIENTED_EDGE('',*,*,#54654,.F.);
#78502=ORIENTED_EDGE('',*,*,#56299,.T.);
#78503=ORIENTED_EDGE('',*,*,#54694,.F.);
#78504=ORIENTED_EDGE('',*,*,#56300,.T.);
#78505=ORIENTED_EDGE('',*,*,#54676,.F.);
#78506=ORIENTED_EDGE('',*,*,#56301,.T.);
#78507=ORIENTED_EDGE('',*,*,#54678,.F.);
#78508=ORIENTED_EDGE('',*,*,#56302,.T.);
#78509=ORIENTED_EDGE('',*,*,#54682,.F.);
#78510=ORIENTED_EDGE('',*,*,#56303,.T.);
#78511=ORIENTED_EDGE('',*,*,#54722,.F.);
#78512=ORIENTED_EDGE('',*,*,#56304,.T.);
#78513=ORIENTED_EDGE('',*,*,#54704,.F.);
#78514=ORIENTED_EDGE('',*,*,#56305,.T.);
#78515=ORIENTED_EDGE('',*,*,#54706,.F.);
#78516=ORIENTED_EDGE('',*,*,#56306,.T.);
#78517=ORIENTED_EDGE('',*,*,#54710,.F.);
#78518=ORIENTED_EDGE('',*,*,#56307,.T.);
#78519=ORIENTED_EDGE('',*,*,#54750,.F.);
#78520=ORIENTED_EDGE('',*,*,#56308,.T.);
#78521=ORIENTED_EDGE('',*,*,#54732,.F.);
#78522=ORIENTED_EDGE('',*,*,#56309,.T.);
#78523=ORIENTED_EDGE('',*,*,#54734,.F.);
#78524=ORIENTED_EDGE('',*,*,#56310,.T.);
#78525=ORIENTED_EDGE('',*,*,#54738,.F.);
#78526=ORIENTED_EDGE('',*,*,#56311,.T.);
#78527=ORIENTED_EDGE('',*,*,#54778,.F.);
#78528=ORIENTED_EDGE('',*,*,#56312,.T.);
#78529=ORIENTED_EDGE('',*,*,#54760,.F.);
#78530=ORIENTED_EDGE('',*,*,#56313,.T.);
#78531=ORIENTED_EDGE('',*,*,#54762,.F.);
#78532=ORIENTED_EDGE('',*,*,#56314,.T.);
#78533=ORIENTED_EDGE('',*,*,#54766,.F.);
#78534=ORIENTED_EDGE('',*,*,#56315,.T.);
#78535=ORIENTED_EDGE('',*,*,#54806,.F.);
#78536=ORIENTED_EDGE('',*,*,#56316,.T.);
#78537=ORIENTED_EDGE('',*,*,#54788,.F.);
#78538=ORIENTED_EDGE('',*,*,#56317,.T.);
#78539=ORIENTED_EDGE('',*,*,#54790,.F.);
#78540=ORIENTED_EDGE('',*,*,#56318,.T.);
#78541=ORIENTED_EDGE('',*,*,#54794,.F.);
#78542=ORIENTED_EDGE('',*,*,#56319,.T.);
#78543=ORIENTED_EDGE('',*,*,#54834,.F.);
#78544=ORIENTED_EDGE('',*,*,#56320,.T.);
#78545=ORIENTED_EDGE('',*,*,#54816,.F.);
#78546=ORIENTED_EDGE('',*,*,#56321,.T.);
#78547=ORIENTED_EDGE('',*,*,#54818,.F.);
#78548=ORIENTED_EDGE('',*,*,#56322,.T.);
#78549=ORIENTED_EDGE('',*,*,#54822,.F.);
#78550=ORIENTED_EDGE('',*,*,#56323,.T.);
#78551=ORIENTED_EDGE('',*,*,#54862,.F.);
#78552=ORIENTED_EDGE('',*,*,#56324,.T.);
#78553=ORIENTED_EDGE('',*,*,#54844,.F.);
#78554=ORIENTED_EDGE('',*,*,#56325,.T.);
#78555=ORIENTED_EDGE('',*,*,#54846,.F.);
#78556=ORIENTED_EDGE('',*,*,#56326,.T.);
#78557=ORIENTED_EDGE('',*,*,#54850,.F.);
#78558=ORIENTED_EDGE('',*,*,#56327,.T.);
#78559=ORIENTED_EDGE('',*,*,#54890,.F.);
#78560=ORIENTED_EDGE('',*,*,#56328,.T.);
#78561=ORIENTED_EDGE('',*,*,#54872,.F.);
#78562=ORIENTED_EDGE('',*,*,#56329,.T.);
#78563=ORIENTED_EDGE('',*,*,#54874,.F.);
#78564=ORIENTED_EDGE('',*,*,#56330,.T.);
#78565=ORIENTED_EDGE('',*,*,#54878,.F.);
#78566=ORIENTED_EDGE('',*,*,#56331,.T.);
#78567=ORIENTED_EDGE('',*,*,#54918,.F.);
#78568=ORIENTED_EDGE('',*,*,#56332,.T.);
#78569=ORIENTED_EDGE('',*,*,#54900,.F.);
#78570=ORIENTED_EDGE('',*,*,#56333,.T.);
#78571=ORIENTED_EDGE('',*,*,#54902,.F.);
#78572=ORIENTED_EDGE('',*,*,#56334,.T.);
#78573=ORIENTED_EDGE('',*,*,#54906,.F.);
#78574=ORIENTED_EDGE('',*,*,#56335,.T.);
#78575=ORIENTED_EDGE('',*,*,#54946,.F.);
#78576=ORIENTED_EDGE('',*,*,#56336,.T.);
#78577=ORIENTED_EDGE('',*,*,#54928,.F.);
#78578=ORIENTED_EDGE('',*,*,#56337,.T.);
#78579=ORIENTED_EDGE('',*,*,#54930,.F.);
#78580=ORIENTED_EDGE('',*,*,#56338,.T.);
#78581=ORIENTED_EDGE('',*,*,#54934,.F.);
#78582=ORIENTED_EDGE('',*,*,#56339,.T.);
#78583=ORIENTED_EDGE('',*,*,#54974,.F.);
#78584=ORIENTED_EDGE('',*,*,#56340,.T.);
#78585=ORIENTED_EDGE('',*,*,#54956,.F.);
#78586=ORIENTED_EDGE('',*,*,#56341,.T.);
#78587=ORIENTED_EDGE('',*,*,#54958,.F.);
#78588=ORIENTED_EDGE('',*,*,#56342,.T.);
#78589=ORIENTED_EDGE('',*,*,#54962,.F.);
#78590=ORIENTED_EDGE('',*,*,#56343,.T.);
#78591=ORIENTED_EDGE('',*,*,#55002,.F.);
#78592=ORIENTED_EDGE('',*,*,#56344,.T.);
#78593=ORIENTED_EDGE('',*,*,#54984,.F.);
#78594=ORIENTED_EDGE('',*,*,#56345,.T.);
#78595=ORIENTED_EDGE('',*,*,#54986,.F.);
#78596=ORIENTED_EDGE('',*,*,#56346,.T.);
#78597=ORIENTED_EDGE('',*,*,#54990,.F.);
#78598=ORIENTED_EDGE('',*,*,#56347,.T.);
#78599=ORIENTED_EDGE('',*,*,#55030,.F.);
#78600=ORIENTED_EDGE('',*,*,#56348,.T.);
#78601=ORIENTED_EDGE('',*,*,#55012,.F.);
#78602=ORIENTED_EDGE('',*,*,#56349,.T.);
#78603=ORIENTED_EDGE('',*,*,#55014,.F.);
#78604=ORIENTED_EDGE('',*,*,#56350,.T.);
#78605=ORIENTED_EDGE('',*,*,#55018,.F.);
#78606=ORIENTED_EDGE('',*,*,#56351,.T.);
#78607=ORIENTED_EDGE('',*,*,#55058,.F.);
#78608=ORIENTED_EDGE('',*,*,#56352,.T.);
#78609=ORIENTED_EDGE('',*,*,#55040,.F.);
#78610=ORIENTED_EDGE('',*,*,#56353,.T.);
#78611=ORIENTED_EDGE('',*,*,#55042,.F.);
#78612=ORIENTED_EDGE('',*,*,#56354,.T.);
#78613=ORIENTED_EDGE('',*,*,#55046,.F.);
#78614=ORIENTED_EDGE('',*,*,#56355,.T.);
#78615=ORIENTED_EDGE('',*,*,#55086,.F.);
#78616=ORIENTED_EDGE('',*,*,#56356,.T.);
#78617=ORIENTED_EDGE('',*,*,#55068,.F.);
#78618=ORIENTED_EDGE('',*,*,#56357,.T.);
#78619=ORIENTED_EDGE('',*,*,#55070,.F.);
#78620=ORIENTED_EDGE('',*,*,#56358,.T.);
#78621=ORIENTED_EDGE('',*,*,#55074,.F.);
#78622=ORIENTED_EDGE('',*,*,#56359,.T.);
#78623=ORIENTED_EDGE('',*,*,#55114,.F.);
#78624=ORIENTED_EDGE('',*,*,#56360,.T.);
#78625=ORIENTED_EDGE('',*,*,#55096,.F.);
#78626=ORIENTED_EDGE('',*,*,#56361,.T.);
#78627=ORIENTED_EDGE('',*,*,#55098,.F.);
#78628=ORIENTED_EDGE('',*,*,#56362,.T.);
#78629=ORIENTED_EDGE('',*,*,#55102,.F.);
#78630=ORIENTED_EDGE('',*,*,#56363,.T.);
#78631=ORIENTED_EDGE('',*,*,#55142,.F.);
#78632=ORIENTED_EDGE('',*,*,#56364,.T.);
#78633=ORIENTED_EDGE('',*,*,#55124,.F.);
#78634=ORIENTED_EDGE('',*,*,#56365,.T.);
#78635=ORIENTED_EDGE('',*,*,#55126,.F.);
#78636=ORIENTED_EDGE('',*,*,#56366,.T.);
#78637=ORIENTED_EDGE('',*,*,#55130,.F.);
#78638=ORIENTED_EDGE('',*,*,#56367,.T.);
#78639=ORIENTED_EDGE('',*,*,#55170,.F.);
#78640=ORIENTED_EDGE('',*,*,#56368,.T.);
#78641=ORIENTED_EDGE('',*,*,#55152,.F.);
#78642=ORIENTED_EDGE('',*,*,#56369,.T.);
#78643=ORIENTED_EDGE('',*,*,#55154,.F.);
#78644=ORIENTED_EDGE('',*,*,#56370,.T.);
#78645=ORIENTED_EDGE('',*,*,#55158,.F.);
#78646=ORIENTED_EDGE('',*,*,#56371,.T.);
#78647=ORIENTED_EDGE('',*,*,#55198,.F.);
#78648=ORIENTED_EDGE('',*,*,#56372,.T.);
#78649=ORIENTED_EDGE('',*,*,#55180,.F.);
#78650=ORIENTED_EDGE('',*,*,#56373,.T.);
#78651=ORIENTED_EDGE('',*,*,#55182,.F.);
#78652=ORIENTED_EDGE('',*,*,#56374,.T.);
#78653=ORIENTED_EDGE('',*,*,#55186,.F.);
#78654=ORIENTED_EDGE('',*,*,#56375,.T.);
#78655=ORIENTED_EDGE('',*,*,#55226,.F.);
#78656=ORIENTED_EDGE('',*,*,#56376,.T.);
#78657=ORIENTED_EDGE('',*,*,#55208,.F.);
#78658=ORIENTED_EDGE('',*,*,#56377,.T.);
#78659=ORIENTED_EDGE('',*,*,#55210,.F.);
#78660=ORIENTED_EDGE('',*,*,#56378,.T.);
#78661=ORIENTED_EDGE('',*,*,#55214,.F.);
#78662=ORIENTED_EDGE('',*,*,#56379,.T.);
#78663=ORIENTED_EDGE('',*,*,#55254,.F.);
#78664=ORIENTED_EDGE('',*,*,#56380,.T.);
#78665=ORIENTED_EDGE('',*,*,#55236,.F.);
#78666=ORIENTED_EDGE('',*,*,#56381,.T.);
#78667=ORIENTED_EDGE('',*,*,#55238,.F.);
#78668=ORIENTED_EDGE('',*,*,#56382,.T.);
#78669=ORIENTED_EDGE('',*,*,#55242,.F.);
#78670=ORIENTED_EDGE('',*,*,#56383,.T.);
#78671=ORIENTED_EDGE('',*,*,#55282,.F.);
#78672=ORIENTED_EDGE('',*,*,#56384,.T.);
#78673=ORIENTED_EDGE('',*,*,#55264,.F.);
#78674=ORIENTED_EDGE('',*,*,#56385,.T.);
#78675=ORIENTED_EDGE('',*,*,#55266,.F.);
#78676=ORIENTED_EDGE('',*,*,#56386,.T.);
#78677=ORIENTED_EDGE('',*,*,#55270,.F.);
#78678=ORIENTED_EDGE('',*,*,#56387,.T.);
#78679=ORIENTED_EDGE('',*,*,#55310,.F.);
#78680=ORIENTED_EDGE('',*,*,#56388,.T.);
#78681=ORIENTED_EDGE('',*,*,#55292,.F.);
#78682=ORIENTED_EDGE('',*,*,#56389,.T.);
#78683=ORIENTED_EDGE('',*,*,#55294,.F.);
#78684=ORIENTED_EDGE('',*,*,#56390,.T.);
#78685=ORIENTED_EDGE('',*,*,#55298,.F.);
#78686=ORIENTED_EDGE('',*,*,#56391,.T.);
#78687=ORIENTED_EDGE('',*,*,#55338,.F.);
#78688=ORIENTED_EDGE('',*,*,#56392,.T.);
#78689=ORIENTED_EDGE('',*,*,#55320,.F.);
#78690=ORIENTED_EDGE('',*,*,#56393,.T.);
#78691=ORIENTED_EDGE('',*,*,#55322,.F.);
#78692=ORIENTED_EDGE('',*,*,#56394,.T.);
#78693=ORIENTED_EDGE('',*,*,#55326,.F.);
#78694=ORIENTED_EDGE('',*,*,#56395,.T.);
#78695=ORIENTED_EDGE('',*,*,#55366,.F.);
#78696=ORIENTED_EDGE('',*,*,#56396,.T.);
#78697=ORIENTED_EDGE('',*,*,#55348,.F.);
#78698=ORIENTED_EDGE('',*,*,#56397,.T.);
#78699=ORIENTED_EDGE('',*,*,#55350,.F.);
#78700=ORIENTED_EDGE('',*,*,#56398,.T.);
#78701=ORIENTED_EDGE('',*,*,#55354,.F.);
#78702=ORIENTED_EDGE('',*,*,#56399,.T.);
#78703=ORIENTED_EDGE('',*,*,#55394,.F.);
#78704=ORIENTED_EDGE('',*,*,#56400,.T.);
#78705=ORIENTED_EDGE('',*,*,#55376,.F.);
#78706=ORIENTED_EDGE('',*,*,#56401,.T.);
#78707=ORIENTED_EDGE('',*,*,#55378,.F.);
#78708=ORIENTED_EDGE('',*,*,#56402,.T.);
#78709=ORIENTED_EDGE('',*,*,#55382,.F.);
#78710=ORIENTED_EDGE('',*,*,#56403,.T.);
#78711=ORIENTED_EDGE('',*,*,#55422,.F.);
#78712=ORIENTED_EDGE('',*,*,#56404,.T.);
#78713=ORIENTED_EDGE('',*,*,#55404,.F.);
#78714=ORIENTED_EDGE('',*,*,#56405,.T.);
#78715=ORIENTED_EDGE('',*,*,#55406,.F.);
#78716=ORIENTED_EDGE('',*,*,#56406,.T.);
#78717=ORIENTED_EDGE('',*,*,#55410,.F.);
#78718=ORIENTED_EDGE('',*,*,#56407,.T.);
#78719=ORIENTED_EDGE('',*,*,#55450,.F.);
#78720=ORIENTED_EDGE('',*,*,#56408,.T.);
#78721=ORIENTED_EDGE('',*,*,#55432,.F.);
#78722=ORIENTED_EDGE('',*,*,#56409,.T.);
#78723=ORIENTED_EDGE('',*,*,#55434,.F.);
#78724=ORIENTED_EDGE('',*,*,#56410,.T.);
#78725=ORIENTED_EDGE('',*,*,#55438,.F.);
#78726=ORIENTED_EDGE('',*,*,#56411,.T.);
#78727=ORIENTED_EDGE('',*,*,#55476,.F.);
#78728=ORIENTED_EDGE('',*,*,#56412,.T.);
#78729=ORIENTED_EDGE('',*,*,#55460,.F.);
#78730=ORIENTED_EDGE('',*,*,#56413,.T.);
#78731=ORIENTED_EDGE('',*,*,#55461,.F.);
#78732=ORIENTED_EDGE('',*,*,#56414,.T.);
#78733=ORIENTED_EDGE('',*,*,#55464,.F.);
#78734=ORIENTED_EDGE('',*,*,#56415,.T.);
#78735=ORIENTED_EDGE('',*,*,#55504,.F.);
#78736=ORIENTED_EDGE('',*,*,#56416,.T.);
#78737=ORIENTED_EDGE('',*,*,#55486,.F.);
#78738=ORIENTED_EDGE('',*,*,#56417,.T.);
#78739=ORIENTED_EDGE('',*,*,#55488,.F.);
#78740=ORIENTED_EDGE('',*,*,#56418,.T.);
#78741=ORIENTED_EDGE('',*,*,#55492,.F.);
#78742=ORIENTED_EDGE('',*,*,#56419,.T.);
#78743=ORIENTED_EDGE('',*,*,#55532,.F.);
#78744=ORIENTED_EDGE('',*,*,#56420,.T.);
#78745=ORIENTED_EDGE('',*,*,#55514,.F.);
#78746=ORIENTED_EDGE('',*,*,#56421,.T.);
#78747=ORIENTED_EDGE('',*,*,#55516,.F.);
#78748=ORIENTED_EDGE('',*,*,#56422,.T.);
#78749=ORIENTED_EDGE('',*,*,#55520,.F.);
#78750=ORIENTED_EDGE('',*,*,#56423,.T.);
#78751=ORIENTED_EDGE('',*,*,#55560,.F.);
#78752=ORIENTED_EDGE('',*,*,#56424,.T.);
#78753=ORIENTED_EDGE('',*,*,#55542,.F.);
#78754=ORIENTED_EDGE('',*,*,#56425,.T.);
#78755=ORIENTED_EDGE('',*,*,#55544,.F.);
#78756=ORIENTED_EDGE('',*,*,#56426,.T.);
#78757=ORIENTED_EDGE('',*,*,#55548,.F.);
#78758=ORIENTED_EDGE('',*,*,#56427,.T.);
#78759=ORIENTED_EDGE('',*,*,#55588,.F.);
#78760=ORIENTED_EDGE('',*,*,#56428,.T.);
#78761=ORIENTED_EDGE('',*,*,#55570,.F.);
#78762=ORIENTED_EDGE('',*,*,#56429,.T.);
#78763=ORIENTED_EDGE('',*,*,#55572,.F.);
#78764=ORIENTED_EDGE('',*,*,#56430,.T.);
#78765=ORIENTED_EDGE('',*,*,#55576,.F.);
#78766=ORIENTED_EDGE('',*,*,#56431,.T.);
#78767=ORIENTED_EDGE('',*,*,#55616,.F.);
#78768=ORIENTED_EDGE('',*,*,#56432,.T.);
#78769=ORIENTED_EDGE('',*,*,#55598,.F.);
#78770=ORIENTED_EDGE('',*,*,#56433,.T.);
#78771=ORIENTED_EDGE('',*,*,#55600,.F.);
#78772=ORIENTED_EDGE('',*,*,#56434,.T.);
#78773=ORIENTED_EDGE('',*,*,#55604,.F.);
#78774=ORIENTED_EDGE('',*,*,#56435,.T.);
#78775=ORIENTED_EDGE('',*,*,#55644,.F.);
#78776=ORIENTED_EDGE('',*,*,#56436,.T.);
#78777=ORIENTED_EDGE('',*,*,#55626,.F.);
#78778=ORIENTED_EDGE('',*,*,#56437,.T.);
#78779=ORIENTED_EDGE('',*,*,#55628,.F.);
#78780=ORIENTED_EDGE('',*,*,#56438,.T.);
#78781=ORIENTED_EDGE('',*,*,#55632,.F.);
#78782=ORIENTED_EDGE('',*,*,#56439,.T.);
#78783=ORIENTED_EDGE('',*,*,#55672,.F.);
#78784=ORIENTED_EDGE('',*,*,#56440,.T.);
#78785=ORIENTED_EDGE('',*,*,#55654,.F.);
#78786=ORIENTED_EDGE('',*,*,#56441,.T.);
#78787=ORIENTED_EDGE('',*,*,#55656,.F.);
#78788=ORIENTED_EDGE('',*,*,#56442,.T.);
#78789=ORIENTED_EDGE('',*,*,#55660,.F.);
#78790=ORIENTED_EDGE('',*,*,#56443,.T.);
#78791=ORIENTED_EDGE('',*,*,#55700,.F.);
#78792=ORIENTED_EDGE('',*,*,#56444,.T.);
#78793=ORIENTED_EDGE('',*,*,#55682,.F.);
#78794=ORIENTED_EDGE('',*,*,#56445,.T.);
#78795=ORIENTED_EDGE('',*,*,#55684,.F.);
#78796=ORIENTED_EDGE('',*,*,#56446,.T.);
#78797=ORIENTED_EDGE('',*,*,#55688,.F.);
#78798=ORIENTED_EDGE('',*,*,#56447,.T.);
#78799=ORIENTED_EDGE('',*,*,#55728,.F.);
#78800=ORIENTED_EDGE('',*,*,#56448,.T.);
#78801=ORIENTED_EDGE('',*,*,#55710,.F.);
#78802=ORIENTED_EDGE('',*,*,#56449,.T.);
#78803=ORIENTED_EDGE('',*,*,#55712,.F.);
#78804=ORIENTED_EDGE('',*,*,#56450,.T.);
#78805=ORIENTED_EDGE('',*,*,#55716,.F.);
#78806=ORIENTED_EDGE('',*,*,#56451,.T.);
#78807=ORIENTED_EDGE('',*,*,#55756,.F.);
#78808=ORIENTED_EDGE('',*,*,#56452,.T.);
#78809=ORIENTED_EDGE('',*,*,#55738,.F.);
#78810=ORIENTED_EDGE('',*,*,#56453,.T.);
#78811=ORIENTED_EDGE('',*,*,#55740,.F.);
#78812=ORIENTED_EDGE('',*,*,#56454,.T.);
#78813=ORIENTED_EDGE('',*,*,#55744,.F.);
#78814=ORIENTED_EDGE('',*,*,#56455,.T.);
#78815=ORIENTED_EDGE('',*,*,#55784,.F.);
#78816=ORIENTED_EDGE('',*,*,#56456,.T.);
#78817=ORIENTED_EDGE('',*,*,#55766,.F.);
#78818=ORIENTED_EDGE('',*,*,#56457,.T.);
#78819=ORIENTED_EDGE('',*,*,#55768,.F.);
#78820=ORIENTED_EDGE('',*,*,#56458,.T.);
#78821=ORIENTED_EDGE('',*,*,#55772,.F.);
#78822=ORIENTED_EDGE('',*,*,#56459,.T.);
#78823=ORIENTED_EDGE('',*,*,#55812,.F.);
#78824=ORIENTED_EDGE('',*,*,#56460,.T.);
#78825=ORIENTED_EDGE('',*,*,#55794,.F.);
#78826=ORIENTED_EDGE('',*,*,#56461,.T.);
#78827=ORIENTED_EDGE('',*,*,#55796,.F.);
#78828=ORIENTED_EDGE('',*,*,#56462,.T.);
#78829=ORIENTED_EDGE('',*,*,#55800,.F.);
#78830=ORIENTED_EDGE('',*,*,#56463,.T.);
#78831=ORIENTED_EDGE('',*,*,#55840,.F.);
#78832=ORIENTED_EDGE('',*,*,#56464,.T.);
#78833=ORIENTED_EDGE('',*,*,#55822,.F.);
#78834=ORIENTED_EDGE('',*,*,#56465,.T.);
#78835=ORIENTED_EDGE('',*,*,#55824,.F.);
#78836=ORIENTED_EDGE('',*,*,#56466,.T.);
#78837=ORIENTED_EDGE('',*,*,#55828,.F.);
#78838=ORIENTED_EDGE('',*,*,#56467,.T.);
#78839=ORIENTED_EDGE('',*,*,#55868,.F.);
#78840=ORIENTED_EDGE('',*,*,#56468,.T.);
#78841=ORIENTED_EDGE('',*,*,#55850,.F.);
#78842=ORIENTED_EDGE('',*,*,#56469,.T.);
#78843=ORIENTED_EDGE('',*,*,#55852,.F.);
#78844=ORIENTED_EDGE('',*,*,#56470,.T.);
#78845=ORIENTED_EDGE('',*,*,#55856,.F.);
#78846=ORIENTED_EDGE('',*,*,#56471,.T.);
#78847=ORIENTED_EDGE('',*,*,#55894,.F.);
#78848=ORIENTED_EDGE('',*,*,#56472,.T.);
#78849=ORIENTED_EDGE('',*,*,#55878,.F.);
#78850=ORIENTED_EDGE('',*,*,#56473,.T.);
#78851=ORIENTED_EDGE('',*,*,#55879,.F.);
#78852=ORIENTED_EDGE('',*,*,#56474,.T.);
#78853=ORIENTED_EDGE('',*,*,#55882,.F.);
#78854=ORIENTED_EDGE('',*,*,#56475,.T.);
#78855=ORIENTED_EDGE('',*,*,#55922,.F.);
#78856=ORIENTED_EDGE('',*,*,#56476,.T.);
#78857=ORIENTED_EDGE('',*,*,#55904,.F.);
#78858=ORIENTED_EDGE('',*,*,#56477,.T.);
#78859=ORIENTED_EDGE('',*,*,#55906,.F.);
#78860=ORIENTED_EDGE('',*,*,#56478,.T.);
#78861=ORIENTED_EDGE('',*,*,#55910,.F.);
#78862=ORIENTED_EDGE('',*,*,#56479,.T.);
#78863=ORIENTED_EDGE('',*,*,#55950,.F.);
#78864=ORIENTED_EDGE('',*,*,#56480,.T.);
#78865=ORIENTED_EDGE('',*,*,#55932,.F.);
#78866=ORIENTED_EDGE('',*,*,#56481,.T.);
#78867=ORIENTED_EDGE('',*,*,#55934,.F.);
#78868=ORIENTED_EDGE('',*,*,#56482,.T.);
#78869=ORIENTED_EDGE('',*,*,#55938,.F.);
#78870=ORIENTED_EDGE('',*,*,#56483,.T.);
#78871=ORIENTED_EDGE('',*,*,#55978,.F.);
#78872=ORIENTED_EDGE('',*,*,#56484,.T.);
#78873=ORIENTED_EDGE('',*,*,#55960,.F.);
#78874=ORIENTED_EDGE('',*,*,#56485,.T.);
#78875=ORIENTED_EDGE('',*,*,#55962,.F.);
#78876=ORIENTED_EDGE('',*,*,#56486,.T.);
#78877=ORIENTED_EDGE('',*,*,#55966,.F.);
#78878=ORIENTED_EDGE('',*,*,#56487,.T.);
#78879=ORIENTED_EDGE('',*,*,#56006,.F.);
#78880=ORIENTED_EDGE('',*,*,#56488,.T.);
#78881=ORIENTED_EDGE('',*,*,#55988,.F.);
#78882=ORIENTED_EDGE('',*,*,#56489,.T.);
#78883=ORIENTED_EDGE('',*,*,#55990,.F.);
#78884=ORIENTED_EDGE('',*,*,#56490,.T.);
#78885=ORIENTED_EDGE('',*,*,#55994,.F.);
#78886=ORIENTED_EDGE('',*,*,#56491,.T.);
#78887=ORIENTED_EDGE('',*,*,#56034,.F.);
#78888=ORIENTED_EDGE('',*,*,#56492,.T.);
#78889=ORIENTED_EDGE('',*,*,#56016,.F.);
#78890=ORIENTED_EDGE('',*,*,#56493,.T.);
#78891=ORIENTED_EDGE('',*,*,#56018,.F.);
#78892=ORIENTED_EDGE('',*,*,#56494,.T.);
#78893=ORIENTED_EDGE('',*,*,#56022,.F.);
#78894=ORIENTED_EDGE('',*,*,#56495,.T.);
#78895=ORIENTED_EDGE('',*,*,#56062,.F.);
#78896=ORIENTED_EDGE('',*,*,#56496,.T.);
#78897=ORIENTED_EDGE('',*,*,#56044,.F.);
#78898=ORIENTED_EDGE('',*,*,#56497,.T.);
#78899=ORIENTED_EDGE('',*,*,#56046,.F.);
#78900=ORIENTED_EDGE('',*,*,#56498,.T.);
#78901=ORIENTED_EDGE('',*,*,#56050,.F.);
#78902=ORIENTED_EDGE('',*,*,#56499,.T.);
#78903=ORIENTED_EDGE('',*,*,#56090,.F.);
#78904=ORIENTED_EDGE('',*,*,#56500,.T.);
#78905=ORIENTED_EDGE('',*,*,#56072,.F.);
#78906=ORIENTED_EDGE('',*,*,#56501,.T.);
#78907=ORIENTED_EDGE('',*,*,#56074,.F.);
#78908=ORIENTED_EDGE('',*,*,#56502,.T.);
#78909=ORIENTED_EDGE('',*,*,#56078,.F.);
#78910=ORIENTED_EDGE('',*,*,#56503,.T.);
#78911=ORIENTED_EDGE('',*,*,#56118,.F.);
#78912=ORIENTED_EDGE('',*,*,#56504,.T.);
#78913=ORIENTED_EDGE('',*,*,#56100,.F.);
#78914=ORIENTED_EDGE('',*,*,#56505,.T.);
#78915=ORIENTED_EDGE('',*,*,#56102,.F.);
#78916=ORIENTED_EDGE('',*,*,#56506,.T.);
#78917=ORIENTED_EDGE('',*,*,#56106,.F.);
#78918=ORIENTED_EDGE('',*,*,#56507,.T.);
#78919=ORIENTED_EDGE('',*,*,#56146,.F.);
#78920=ORIENTED_EDGE('',*,*,#56508,.T.);
#78921=ORIENTED_EDGE('',*,*,#56128,.F.);
#78922=ORIENTED_EDGE('',*,*,#56509,.T.);
#78923=ORIENTED_EDGE('',*,*,#56130,.F.);
#78924=ORIENTED_EDGE('',*,*,#56510,.T.);
#78925=ORIENTED_EDGE('',*,*,#56134,.F.);
#78926=ORIENTED_EDGE('',*,*,#56511,.T.);
#78927=ORIENTED_EDGE('',*,*,#56174,.F.);
#78928=ORIENTED_EDGE('',*,*,#56512,.T.);
#78929=ORIENTED_EDGE('',*,*,#56156,.F.);
#78930=ORIENTED_EDGE('',*,*,#56513,.T.);
#78931=ORIENTED_EDGE('',*,*,#56158,.F.);
#78932=ORIENTED_EDGE('',*,*,#56514,.T.);
#78933=ORIENTED_EDGE('',*,*,#56162,.F.);
#78934=ORIENTED_EDGE('',*,*,#56515,.T.);
#78935=ORIENTED_EDGE('',*,*,#56202,.F.);
#78936=ORIENTED_EDGE('',*,*,#56516,.T.);
#78937=ORIENTED_EDGE('',*,*,#56184,.F.);
#78938=ORIENTED_EDGE('',*,*,#56517,.T.);
#78939=ORIENTED_EDGE('',*,*,#56186,.F.);
#78940=ORIENTED_EDGE('',*,*,#56518,.T.);
#78941=ORIENTED_EDGE('',*,*,#56190,.F.);
#78942=ORIENTED_EDGE('',*,*,#56519,.T.);
#78943=ORIENTED_EDGE('',*,*,#56230,.F.);
#78944=ORIENTED_EDGE('',*,*,#56520,.T.);
#78945=ORIENTED_EDGE('',*,*,#56212,.F.);
#78946=ORIENTED_EDGE('',*,*,#56521,.T.);
#78947=ORIENTED_EDGE('',*,*,#56214,.F.);
#78948=ORIENTED_EDGE('',*,*,#56522,.T.);
#78949=ORIENTED_EDGE('',*,*,#56218,.F.);
#78950=ORIENTED_EDGE('',*,*,#56523,.T.);
#78951=ORIENTED_EDGE('',*,*,#56258,.F.);
#78952=ORIENTED_EDGE('',*,*,#56524,.T.);
#78953=ORIENTED_EDGE('',*,*,#56240,.F.);
#78954=ORIENTED_EDGE('',*,*,#56525,.T.);
#78955=ORIENTED_EDGE('',*,*,#56242,.F.);
#78956=ORIENTED_EDGE('',*,*,#56526,.T.);
#78957=ORIENTED_EDGE('',*,*,#56246,.F.);
#78958=ORIENTED_EDGE('',*,*,#56527,.T.);
#78959=ORIENTED_EDGE('',*,*,#56286,.F.);
#78960=ORIENTED_EDGE('',*,*,#56528,.T.);
#78961=ORIENTED_EDGE('',*,*,#56268,.F.);
#78962=ORIENTED_EDGE('',*,*,#56529,.T.);
#78963=ORIENTED_EDGE('',*,*,#56270,.F.);
#78964=ORIENTED_EDGE('',*,*,#56530,.T.);
#78965=ORIENTED_EDGE('',*,*,#56274,.F.);
#78966=ORIENTED_EDGE('',*,*,#56531,.T.);
#78967=ORIENTED_EDGE('',*,*,#56532,.F.);
#78968=ORIENTED_EDGE('',*,*,#54674,.F.);
#78969=ORIENTED_EDGE('',*,*,#56533,.F.);
#78970=ORIENTED_EDGE('',*,*,#54546,.F.);
#78971=ORIENTED_EDGE('',*,*,#56533,.T.);
#78972=ORIENTED_EDGE('',*,*,#54673,.F.);
#78973=ORIENTED_EDGE('',*,*,#56534,.F.);
#78974=ORIENTED_EDGE('',*,*,#54555,.F.);
#78975=ORIENTED_EDGE('',*,*,#54545,.T.);
#78976=ORIENTED_EDGE('',*,*,#54549,.F.);
#78977=ORIENTED_EDGE('',*,*,#56535,.F.);
#78978=ORIENTED_EDGE('',*,*,#54675,.F.);
#78979=ORIENTED_EDGE('',*,*,#56532,.T.);
#78980=ORIENTED_EDGE('',*,*,#56534,.T.);
#78981=ORIENTED_EDGE('',*,*,#54672,.F.);
#78982=ORIENTED_EDGE('',*,*,#56536,.F.);
#78983=ORIENTED_EDGE('',*,*,#54540,.F.);
#78984=ORIENTED_EDGE('',*,*,#56535,.T.);
#78985=ORIENTED_EDGE('',*,*,#54553,.F.);
#78986=ORIENTED_EDGE('',*,*,#56537,.F.);
#78987=ORIENTED_EDGE('',*,*,#54664,.F.);
#78988=ORIENTED_EDGE('',*,*,#56536,.T.);
#78989=ORIENTED_EDGE('',*,*,#54671,.F.);
#78990=ORIENTED_EDGE('',*,*,#56538,.F.);
#78991=ORIENTED_EDGE('',*,*,#54557,.F.);
#78992=ORIENTED_EDGE('',*,*,#56537,.T.);
#78993=ORIENTED_EDGE('',*,*,#52072,.F.);
#78994=ORIENTED_EDGE('',*,*,#56539,.F.);
#78995=ORIENTED_EDGE('',*,*,#54665,.F.);
#78996=ORIENTED_EDGE('',*,*,#56538,.T.);
#78997=ORIENTED_EDGE('',*,*,#54670,.F.);
#78998=ORIENTED_EDGE('',*,*,#56540,.F.);
#78999=ORIENTED_EDGE('',*,*,#54532,.T.);
#79000=ORIENTED_EDGE('',*,*,#54536,.F.);
#79001=ORIENTED_EDGE('',*,*,#56539,.T.);
#79002=ORIENTED_EDGE('',*,*,#52071,.F.);
#79003=ORIENTED_EDGE('',*,*,#56541,.F.);
#79004=ORIENTED_EDGE('',*,*,#56296,.F.);
#79005=ORIENTED_EDGE('',*,*,#56540,.T.);
#79006=ORIENTED_EDGE('',*,*,#54669,.F.);
#79007=ORIENTED_EDGE('',*,*,#56542,.F.);
#79008=ORIENTED_EDGE('',*,*,#54533,.F.);
#79009=ORIENTED_EDGE('',*,*,#56541,.T.);
#79010=ORIENTED_EDGE('',*,*,#52070,.F.);
#79011=ORIENTED_EDGE('',*,*,#56543,.F.);
#79012=ORIENTED_EDGE('',*,*,#54649,.F.);
#79013=ORIENTED_EDGE('',*,*,#56542,.T.);
#79014=ORIENTED_EDGE('',*,*,#54668,.F.);
#79015=ORIENTED_EDGE('',*,*,#56544,.F.);
#79016=ORIENTED_EDGE('',*,*,#54551,.F.);
#79017=ORIENTED_EDGE('',*,*,#56543,.T.);
#79018=ORIENTED_EDGE('',*,*,#52069,.F.);
#79019=ORIENTED_EDGE('',*,*,#56545,.F.);
#79020=ORIENTED_EDGE('',*,*,#56298,.F.);
#79021=ORIENTED_EDGE('',*,*,#56544,.T.);
#79022=ORIENTED_EDGE('',*,*,#54667,.F.);
#79023=ORIENTED_EDGE('',*,*,#56546,.F.);
#79024=ORIENTED_EDGE('',*,*,#52594,.F.);
#79025=ORIENTED_EDGE('',*,*,#56545,.T.);
#79026=ORIENTED_EDGE('',*,*,#52068,.F.);
#79027=ORIENTED_EDGE('',*,*,#56547,.F.);
#79028=ORIENTED_EDGE('',*,*,#54655,.F.);
#79029=ORIENTED_EDGE('',*,*,#56546,.T.);
#79030=ORIENTED_EDGE('',*,*,#56297,.F.);
#79031=ORIENTED_EDGE('',*,*,#56548,.F.);
#79032=ORIENTED_EDGE('',*,*,#52595,.F.);
#79033=ORIENTED_EDGE('',*,*,#56547,.T.);
#79034=ORIENTED_EDGE('',*,*,#54582,.F.);
#79035=ORIENTED_EDGE('',*,*,#56549,.F.);
#79036=ORIENTED_EDGE('',*,*,#54656,.F.);
#79037=ORIENTED_EDGE('',*,*,#56548,.T.);
#79038=ORIENTED_EDGE('',*,*,#54651,.F.);
#79039=ORIENTED_EDGE('',*,*,#56550,.F.);
#79040=ORIENTED_EDGE('',*,*,#52596,.F.);
#79041=ORIENTED_EDGE('',*,*,#54577,.F.);
#79042=ORIENTED_EDGE('',*,*,#54573,.T.);
#79043=ORIENTED_EDGE('',*,*,#56551,.F.);
#79044=ORIENTED_EDGE('',*,*,#54657,.F.);
#79045=ORIENTED_EDGE('',*,*,#56549,.T.);
#79046=ORIENTED_EDGE('',*,*,#56550,.T.);
#79047=ORIENTED_EDGE('',*,*,#56299,.F.);
#79048=ORIENTED_EDGE('',*,*,#56552,.F.);
#79049=ORIENTED_EDGE('',*,*,#52597,.F.);
#79050=ORIENTED_EDGE('',*,*,#56551,.T.);
#79051=ORIENTED_EDGE('',*,*,#54572,.F.);
#79052=ORIENTED_EDGE('',*,*,#56553,.F.);
#79053=ORIENTED_EDGE('',*,*,#54658,.F.);
#79054=ORIENTED_EDGE('',*,*,#56552,.T.);
#79055=ORIENTED_EDGE('',*,*,#54653,.F.);
#79056=ORIENTED_EDGE('',*,*,#56554,.F.);
#79057=ORIENTED_EDGE('',*,*,#52598,.F.);
#79058=ORIENTED_EDGE('',*,*,#56553,.T.);
#79059=ORIENTED_EDGE('',*,*,#54584,.F.);
#79060=ORIENTED_EDGE('',*,*,#56555,.F.);
#79061=ORIENTED_EDGE('',*,*,#54659,.F.);
#79062=ORIENTED_EDGE('',*,*,#56554,.T.);
#79063=ORIENTED_EDGE('',*,*,#54652,.F.);
#79064=ORIENTED_EDGE('',*,*,#56556,.F.);
#79065=ORIENTED_EDGE('',*,*,#54580,.F.);
#79066=ORIENTED_EDGE('',*,*,#56555,.T.);
#79067=ORIENTED_EDGE('',*,*,#54568,.F.);
#79068=ORIENTED_EDGE('',*,*,#56557,.F.);
#79069=ORIENTED_EDGE('',*,*,#54660,.F.);
#79070=ORIENTED_EDGE('',*,*,#56556,.T.);
#79071=ORIENTED_EDGE('',*,*,#54663,.F.);
#79072=ORIENTED_EDGE('',*,*,#56558,.F.);
#79073=ORIENTED_EDGE('',*,*,#54559,.F.);
#79074=ORIENTED_EDGE('',*,*,#56557,.T.);
#79075=ORIENTED_EDGE('',*,*,#54586,.F.);
#79076=ORIENTED_EDGE('',*,*,#56559,.F.);
#79077=ORIENTED_EDGE('',*,*,#54661,.F.);
#79078=ORIENTED_EDGE('',*,*,#56558,.T.);
#79079=ORIENTED_EDGE('',*,*,#54662,.F.);
#79080=ORIENTED_EDGE('',*,*,#56559,.T.);
#79081=ORIENTED_EDGE('',*,*,#54564,.F.);
#79082=ORIENTED_EDGE('',*,*,#54560,.T.);
#79083=ORIENTED_EDGE('',*,*,#56560,.F.);
#79084=ORIENTED_EDGE('',*,*,#54702,.F.);
#79085=ORIENTED_EDGE('',*,*,#56561,.F.);
#79086=ORIENTED_EDGE('',*,*,#54516,.F.);
#79087=ORIENTED_EDGE('',*,*,#56561,.T.);
#79088=ORIENTED_EDGE('',*,*,#54701,.F.);
#79089=ORIENTED_EDGE('',*,*,#56562,.F.);
#79090=ORIENTED_EDGE('',*,*,#54525,.F.);
#79091=ORIENTED_EDGE('',*,*,#54515,.T.);
#79092=ORIENTED_EDGE('',*,*,#54519,.F.);
#79093=ORIENTED_EDGE('',*,*,#56563,.F.);
#79094=ORIENTED_EDGE('',*,*,#54703,.F.);
#79095=ORIENTED_EDGE('',*,*,#56560,.T.);
#79096=ORIENTED_EDGE('',*,*,#56562,.T.);
#79097=ORIENTED_EDGE('',*,*,#54700,.F.);
#79098=ORIENTED_EDGE('',*,*,#56564,.F.);
#79099=ORIENTED_EDGE('',*,*,#54510,.F.);
#79100=ORIENTED_EDGE('',*,*,#56563,.T.);
#79101=ORIENTED_EDGE('',*,*,#54523,.F.);
#79102=ORIENTED_EDGE('',*,*,#56565,.F.);
#79103=ORIENTED_EDGE('',*,*,#54692,.F.);
#79104=ORIENTED_EDGE('',*,*,#56564,.T.);
#79105=ORIENTED_EDGE('',*,*,#54699,.F.);
#79106=ORIENTED_EDGE('',*,*,#56566,.F.);
#79107=ORIENTED_EDGE('',*,*,#54527,.F.);
#79108=ORIENTED_EDGE('',*,*,#56565,.T.);
#79109=ORIENTED_EDGE('',*,*,#52078,.F.);
#79110=ORIENTED_EDGE('',*,*,#56567,.F.);
#79111=ORIENTED_EDGE('',*,*,#54693,.F.);
#79112=ORIENTED_EDGE('',*,*,#56566,.T.);
#79113=ORIENTED_EDGE('',*,*,#54698,.F.);
#79114=ORIENTED_EDGE('',*,*,#56568,.F.);
#79115=ORIENTED_EDGE('',*,*,#54502,.T.);
#79116=ORIENTED_EDGE('',*,*,#54506,.F.);
#79117=ORIENTED_EDGE('',*,*,#56567,.T.);
#79118=ORIENTED_EDGE('',*,*,#52077,.F.);
#79119=ORIENTED_EDGE('',*,*,#56569,.F.);
#79120=ORIENTED_EDGE('',*,*,#56300,.F.);
#79121=ORIENTED_EDGE('',*,*,#56568,.T.);
#79122=ORIENTED_EDGE('',*,*,#54697,.F.);
#79123=ORIENTED_EDGE('',*,*,#56570,.F.);
#79124=ORIENTED_EDGE('',*,*,#54503,.F.);
#79125=ORIENTED_EDGE('',*,*,#56569,.T.);
#79126=ORIENTED_EDGE('',*,*,#52076,.F.);
#79127=ORIENTED_EDGE('',*,*,#56571,.F.);
#79128=ORIENTED_EDGE('',*,*,#54677,.F.);
#79129=ORIENTED_EDGE('',*,*,#56570,.T.);
#79130=ORIENTED_EDGE('',*,*,#54696,.F.);
#79131=ORIENTED_EDGE('',*,*,#56572,.F.);
#79132=ORIENTED_EDGE('',*,*,#54521,.F.);
#79133=ORIENTED_EDGE('',*,*,#56571,.T.);
#79134=ORIENTED_EDGE('',*,*,#52075,.F.);
#79135=ORIENTED_EDGE('',*,*,#56573,.F.);
#79136=ORIENTED_EDGE('',*,*,#56302,.F.);
#79137=ORIENTED_EDGE('',*,*,#56572,.T.);
#79138=ORIENTED_EDGE('',*,*,#54695,.F.);
#79139=ORIENTED_EDGE('',*,*,#56574,.F.);
#79140=ORIENTED_EDGE('',*,*,#52588,.F.);
#79141=ORIENTED_EDGE('',*,*,#56573,.T.);
#79142=ORIENTED_EDGE('',*,*,#52074,.F.);
#79143=ORIENTED_EDGE('',*,*,#56575,.F.);
#79144=ORIENTED_EDGE('',*,*,#54683,.F.);
#79145=ORIENTED_EDGE('',*,*,#56574,.T.);
#79146=ORIENTED_EDGE('',*,*,#56301,.F.);
#79147=ORIENTED_EDGE('',*,*,#56576,.F.);
#79148=ORIENTED_EDGE('',*,*,#52589,.F.);
#79149=ORIENTED_EDGE('',*,*,#56575,.T.);
#79150=ORIENTED_EDGE('',*,*,#54552,.F.);
#79151=ORIENTED_EDGE('',*,*,#56577,.F.);
#79152=ORIENTED_EDGE('',*,*,#54684,.F.);
#79153=ORIENTED_EDGE('',*,*,#56576,.T.);
#79154=ORIENTED_EDGE('',*,*,#54679,.F.);
#79155=ORIENTED_EDGE('',*,*,#56578,.F.);
#79156=ORIENTED_EDGE('',*,*,#52590,.F.);
#79157=ORIENTED_EDGE('',*,*,#54547,.F.);
#79158=ORIENTED_EDGE('',*,*,#54543,.T.);
#79159=ORIENTED_EDGE('',*,*,#56579,.F.);
#79160=ORIENTED_EDGE('',*,*,#54685,.F.);
#79161=ORIENTED_EDGE('',*,*,#56577,.T.);
#79162=ORIENTED_EDGE('',*,*,#56578,.T.);
#79163=ORIENTED_EDGE('',*,*,#56303,.F.);
#79164=ORIENTED_EDGE('',*,*,#56580,.F.);
#79165=ORIENTED_EDGE('',*,*,#52591,.F.);
#79166=ORIENTED_EDGE('',*,*,#56579,.T.);
#79167=ORIENTED_EDGE('',*,*,#54542,.F.);
#79168=ORIENTED_EDGE('',*,*,#56581,.F.);
#79169=ORIENTED_EDGE('',*,*,#54686,.F.);
#79170=ORIENTED_EDGE('',*,*,#56580,.T.);
#79171=ORIENTED_EDGE('',*,*,#54681,.F.);
#79172=ORIENTED_EDGE('',*,*,#56582,.F.);
#79173=ORIENTED_EDGE('',*,*,#52592,.F.);
#79174=ORIENTED_EDGE('',*,*,#56581,.T.);
#79175=ORIENTED_EDGE('',*,*,#54554,.F.);
#79176=ORIENTED_EDGE('',*,*,#56583,.F.);
#79177=ORIENTED_EDGE('',*,*,#54687,.F.);
#79178=ORIENTED_EDGE('',*,*,#56582,.T.);
#79179=ORIENTED_EDGE('',*,*,#54680,.F.);
#79180=ORIENTED_EDGE('',*,*,#56584,.F.);
#79181=ORIENTED_EDGE('',*,*,#54550,.F.);
#79182=ORIENTED_EDGE('',*,*,#56583,.T.);
#79183=ORIENTED_EDGE('',*,*,#54538,.F.);
#79184=ORIENTED_EDGE('',*,*,#56585,.F.);
#79185=ORIENTED_EDGE('',*,*,#54688,.F.);
#79186=ORIENTED_EDGE('',*,*,#56584,.T.);
#79187=ORIENTED_EDGE('',*,*,#54691,.F.);
#79188=ORIENTED_EDGE('',*,*,#56586,.F.);
#79189=ORIENTED_EDGE('',*,*,#54529,.F.);
#79190=ORIENTED_EDGE('',*,*,#56585,.T.);
#79191=ORIENTED_EDGE('',*,*,#54556,.F.);
#79192=ORIENTED_EDGE('',*,*,#56587,.F.);
#79193=ORIENTED_EDGE('',*,*,#54689,.F.);
#79194=ORIENTED_EDGE('',*,*,#56586,.T.);
#79195=ORIENTED_EDGE('',*,*,#54690,.F.);
#79196=ORIENTED_EDGE('',*,*,#56587,.T.);
#79197=ORIENTED_EDGE('',*,*,#54534,.F.);
#79198=ORIENTED_EDGE('',*,*,#54530,.T.);
#79199=ORIENTED_EDGE('',*,*,#56588,.F.);
#79200=ORIENTED_EDGE('',*,*,#54730,.F.);
#79201=ORIENTED_EDGE('',*,*,#56589,.F.);
#79202=ORIENTED_EDGE('',*,*,#54486,.F.);
#79203=ORIENTED_EDGE('',*,*,#56589,.T.);
#79204=ORIENTED_EDGE('',*,*,#54729,.F.);
#79205=ORIENTED_EDGE('',*,*,#56590,.F.);
#79206=ORIENTED_EDGE('',*,*,#54495,.F.);
#79207=ORIENTED_EDGE('',*,*,#54485,.T.);
#79208=ORIENTED_EDGE('',*,*,#54489,.F.);
#79209=ORIENTED_EDGE('',*,*,#56591,.F.);
#79210=ORIENTED_EDGE('',*,*,#54731,.F.);
#79211=ORIENTED_EDGE('',*,*,#56588,.T.);
#79212=ORIENTED_EDGE('',*,*,#56590,.T.);
#79213=ORIENTED_EDGE('',*,*,#54728,.F.);
#79214=ORIENTED_EDGE('',*,*,#56592,.F.);
#79215=ORIENTED_EDGE('',*,*,#54480,.F.);
#79216=ORIENTED_EDGE('',*,*,#56591,.T.);
#79217=ORIENTED_EDGE('',*,*,#54493,.F.);
#79218=ORIENTED_EDGE('',*,*,#56593,.F.);
#79219=ORIENTED_EDGE('',*,*,#54720,.F.);
#79220=ORIENTED_EDGE('',*,*,#56592,.T.);
#79221=ORIENTED_EDGE('',*,*,#54727,.F.);
#79222=ORIENTED_EDGE('',*,*,#56594,.F.);
#79223=ORIENTED_EDGE('',*,*,#54497,.F.);
#79224=ORIENTED_EDGE('',*,*,#56593,.T.);
#79225=ORIENTED_EDGE('',*,*,#52084,.F.);
#79226=ORIENTED_EDGE('',*,*,#56595,.F.);
#79227=ORIENTED_EDGE('',*,*,#54721,.F.);
#79228=ORIENTED_EDGE('',*,*,#56594,.T.);
#79229=ORIENTED_EDGE('',*,*,#54726,.F.);
#79230=ORIENTED_EDGE('',*,*,#56596,.F.);
#79231=ORIENTED_EDGE('',*,*,#54472,.T.);
#79232=ORIENTED_EDGE('',*,*,#54476,.F.);
#79233=ORIENTED_EDGE('',*,*,#56595,.T.);
#79234=ORIENTED_EDGE('',*,*,#52083,.F.);
#79235=ORIENTED_EDGE('',*,*,#56597,.F.);
#79236=ORIENTED_EDGE('',*,*,#56304,.F.);
#79237=ORIENTED_EDGE('',*,*,#56596,.T.);
#79238=ORIENTED_EDGE('',*,*,#54725,.F.);
#79239=ORIENTED_EDGE('',*,*,#56598,.F.);
#79240=ORIENTED_EDGE('',*,*,#54473,.F.);
#79241=ORIENTED_EDGE('',*,*,#56597,.T.);
#79242=ORIENTED_EDGE('',*,*,#52082,.F.);
#79243=ORIENTED_EDGE('',*,*,#56599,.F.);
#79244=ORIENTED_EDGE('',*,*,#54705,.F.);
#79245=ORIENTED_EDGE('',*,*,#56598,.T.);
#79246=ORIENTED_EDGE('',*,*,#54724,.F.);
#79247=ORIENTED_EDGE('',*,*,#56600,.F.);
#79248=ORIENTED_EDGE('',*,*,#54491,.F.);
#79249=ORIENTED_EDGE('',*,*,#56599,.T.);
#79250=ORIENTED_EDGE('',*,*,#52081,.F.);
#79251=ORIENTED_EDGE('',*,*,#56601,.F.);
#79252=ORIENTED_EDGE('',*,*,#56306,.F.);
#79253=ORIENTED_EDGE('',*,*,#56600,.T.);
#79254=ORIENTED_EDGE('',*,*,#54723,.F.);
#79255=ORIENTED_EDGE('',*,*,#56602,.F.);
#79256=ORIENTED_EDGE('',*,*,#52582,.F.);
#79257=ORIENTED_EDGE('',*,*,#56601,.T.);
#79258=ORIENTED_EDGE('',*,*,#52080,.F.);
#79259=ORIENTED_EDGE('',*,*,#56603,.F.);
#79260=ORIENTED_EDGE('',*,*,#54711,.F.);
#79261=ORIENTED_EDGE('',*,*,#56602,.T.);
#79262=ORIENTED_EDGE('',*,*,#56305,.F.);
#79263=ORIENTED_EDGE('',*,*,#56604,.F.);
#79264=ORIENTED_EDGE('',*,*,#52583,.F.);
#79265=ORIENTED_EDGE('',*,*,#56603,.T.);
#79266=ORIENTED_EDGE('',*,*,#54522,.F.);
#79267=ORIENTED_EDGE('',*,*,#56605,.F.);
#79268=ORIENTED_EDGE('',*,*,#54712,.F.);
#79269=ORIENTED_EDGE('',*,*,#56604,.T.);
#79270=ORIENTED_EDGE('',*,*,#54707,.F.);
#79271=ORIENTED_EDGE('',*,*,#56606,.F.);
#79272=ORIENTED_EDGE('',*,*,#52584,.F.);
#79273=ORIENTED_EDGE('',*,*,#54517,.F.);
#79274=ORIENTED_EDGE('',*,*,#54513,.T.);
#79275=ORIENTED_EDGE('',*,*,#56607,.F.);
#79276=ORIENTED_EDGE('',*,*,#54713,.F.);
#79277=ORIENTED_EDGE('',*,*,#56605,.T.);
#79278=ORIENTED_EDGE('',*,*,#56606,.T.);
#79279=ORIENTED_EDGE('',*,*,#56307,.F.);
#79280=ORIENTED_EDGE('',*,*,#56608,.F.);
#79281=ORIENTED_EDGE('',*,*,#52585,.F.);
#79282=ORIENTED_EDGE('',*,*,#56607,.T.);
#79283=ORIENTED_EDGE('',*,*,#54512,.F.);
#79284=ORIENTED_EDGE('',*,*,#56609,.F.);
#79285=ORIENTED_EDGE('',*,*,#54714,.F.);
#79286=ORIENTED_EDGE('',*,*,#56608,.T.);
#79287=ORIENTED_EDGE('',*,*,#54709,.F.);
#79288=ORIENTED_EDGE('',*,*,#56610,.F.);
#79289=ORIENTED_EDGE('',*,*,#52586,.F.);
#79290=ORIENTED_EDGE('',*,*,#56609,.T.);
#79291=ORIENTED_EDGE('',*,*,#54524,.F.);
#79292=ORIENTED_EDGE('',*,*,#56611,.F.);
#79293=ORIENTED_EDGE('',*,*,#54715,.F.);
#79294=ORIENTED_EDGE('',*,*,#56610,.T.);
#79295=ORIENTED_EDGE('',*,*,#54708,.F.);
#79296=ORIENTED_EDGE('',*,*,#56612,.F.);
#79297=ORIENTED_EDGE('',*,*,#54520,.F.);
#79298=ORIENTED_EDGE('',*,*,#56611,.T.);
#79299=ORIENTED_EDGE('',*,*,#54508,.F.);
#79300=ORIENTED_EDGE('',*,*,#56613,.F.);
#79301=ORIENTED_EDGE('',*,*,#54716,.F.);
#79302=ORIENTED_EDGE('',*,*,#56612,.T.);
#79303=ORIENTED_EDGE('',*,*,#54719,.F.);
#79304=ORIENTED_EDGE('',*,*,#56614,.F.);
#79305=ORIENTED_EDGE('',*,*,#54499,.F.);
#79306=ORIENTED_EDGE('',*,*,#56613,.T.);
#79307=ORIENTED_EDGE('',*,*,#54526,.F.);
#79308=ORIENTED_EDGE('',*,*,#56615,.F.);
#79309=ORIENTED_EDGE('',*,*,#54717,.F.);
#79310=ORIENTED_EDGE('',*,*,#56614,.T.);
#79311=ORIENTED_EDGE('',*,*,#54718,.F.);
#79312=ORIENTED_EDGE('',*,*,#56615,.T.);
#79313=ORIENTED_EDGE('',*,*,#54504,.F.);
#79314=ORIENTED_EDGE('',*,*,#54500,.T.);
#79315=ORIENTED_EDGE('',*,*,#56616,.F.);
#79316=ORIENTED_EDGE('',*,*,#54758,.F.);
#79317=ORIENTED_EDGE('',*,*,#56617,.F.);
#79318=ORIENTED_EDGE('',*,*,#54456,.F.);
#79319=ORIENTED_EDGE('',*,*,#56617,.T.);
#79320=ORIENTED_EDGE('',*,*,#54757,.F.);
#79321=ORIENTED_EDGE('',*,*,#56618,.F.);
#79322=ORIENTED_EDGE('',*,*,#54465,.F.);
#79323=ORIENTED_EDGE('',*,*,#54455,.T.);
#79324=ORIENTED_EDGE('',*,*,#54459,.F.);
#79325=ORIENTED_EDGE('',*,*,#56619,.F.);
#79326=ORIENTED_EDGE('',*,*,#54759,.F.);
#79327=ORIENTED_EDGE('',*,*,#56616,.T.);
#79328=ORIENTED_EDGE('',*,*,#56618,.T.);
#79329=ORIENTED_EDGE('',*,*,#54756,.F.);
#79330=ORIENTED_EDGE('',*,*,#56620,.F.);
#79331=ORIENTED_EDGE('',*,*,#54450,.F.);
#79332=ORIENTED_EDGE('',*,*,#56619,.T.);
#79333=ORIENTED_EDGE('',*,*,#54463,.F.);
#79334=ORIENTED_EDGE('',*,*,#56621,.F.);
#79335=ORIENTED_EDGE('',*,*,#54748,.F.);
#79336=ORIENTED_EDGE('',*,*,#56620,.T.);
#79337=ORIENTED_EDGE('',*,*,#54755,.F.);
#79338=ORIENTED_EDGE('',*,*,#56622,.F.);
#79339=ORIENTED_EDGE('',*,*,#54467,.F.);
#79340=ORIENTED_EDGE('',*,*,#56621,.T.);
#79341=ORIENTED_EDGE('',*,*,#52090,.F.);
#79342=ORIENTED_EDGE('',*,*,#56623,.F.);
#79343=ORIENTED_EDGE('',*,*,#54749,.F.);
#79344=ORIENTED_EDGE('',*,*,#56622,.T.);
#79345=ORIENTED_EDGE('',*,*,#54754,.F.);
#79346=ORIENTED_EDGE('',*,*,#56624,.F.);
#79347=ORIENTED_EDGE('',*,*,#54442,.T.);
#79348=ORIENTED_EDGE('',*,*,#54446,.F.);
#79349=ORIENTED_EDGE('',*,*,#56623,.T.);
#79350=ORIENTED_EDGE('',*,*,#52089,.F.);
#79351=ORIENTED_EDGE('',*,*,#56625,.F.);
#79352=ORIENTED_EDGE('',*,*,#56308,.F.);
#79353=ORIENTED_EDGE('',*,*,#56624,.T.);
#79354=ORIENTED_EDGE('',*,*,#54753,.F.);
#79355=ORIENTED_EDGE('',*,*,#56626,.F.);
#79356=ORIENTED_EDGE('',*,*,#54443,.F.);
#79357=ORIENTED_EDGE('',*,*,#56625,.T.);
#79358=ORIENTED_EDGE('',*,*,#52088,.F.);
#79359=ORIENTED_EDGE('',*,*,#56627,.F.);
#79360=ORIENTED_EDGE('',*,*,#54733,.F.);
#79361=ORIENTED_EDGE('',*,*,#56626,.T.);
#79362=ORIENTED_EDGE('',*,*,#54752,.F.);
#79363=ORIENTED_EDGE('',*,*,#56628,.F.);
#79364=ORIENTED_EDGE('',*,*,#54461,.F.);
#79365=ORIENTED_EDGE('',*,*,#56627,.T.);
#79366=ORIENTED_EDGE('',*,*,#52087,.F.);
#79367=ORIENTED_EDGE('',*,*,#56629,.F.);
#79368=ORIENTED_EDGE('',*,*,#56310,.F.);
#79369=ORIENTED_EDGE('',*,*,#56628,.T.);
#79370=ORIENTED_EDGE('',*,*,#54751,.F.);
#79371=ORIENTED_EDGE('',*,*,#56630,.F.);
#79372=ORIENTED_EDGE('',*,*,#52576,.F.);
#79373=ORIENTED_EDGE('',*,*,#56629,.T.);
#79374=ORIENTED_EDGE('',*,*,#52086,.F.);
#79375=ORIENTED_EDGE('',*,*,#56631,.F.);
#79376=ORIENTED_EDGE('',*,*,#54739,.F.);
#79377=ORIENTED_EDGE('',*,*,#56630,.T.);
#79378=ORIENTED_EDGE('',*,*,#56309,.F.);
#79379=ORIENTED_EDGE('',*,*,#56632,.F.);
#79380=ORIENTED_EDGE('',*,*,#52577,.F.);
#79381=ORIENTED_EDGE('',*,*,#56631,.T.);
#79382=ORIENTED_EDGE('',*,*,#54492,.F.);
#79383=ORIENTED_EDGE('',*,*,#56633,.F.);
#79384=ORIENTED_EDGE('',*,*,#54740,.F.);
#79385=ORIENTED_EDGE('',*,*,#56632,.T.);
#79386=ORIENTED_EDGE('',*,*,#54735,.F.);
#79387=ORIENTED_EDGE('',*,*,#56634,.F.);
#79388=ORIENTED_EDGE('',*,*,#52578,.F.);
#79389=ORIENTED_EDGE('',*,*,#54487,.F.);
#79390=ORIENTED_EDGE('',*,*,#54483,.T.);
#79391=ORIENTED_EDGE('',*,*,#56635,.F.);
#79392=ORIENTED_EDGE('',*,*,#54741,.F.);
#79393=ORIENTED_EDGE('',*,*,#56633,.T.);
#79394=ORIENTED_EDGE('',*,*,#56634,.T.);
#79395=ORIENTED_EDGE('',*,*,#56311,.F.);
#79396=ORIENTED_EDGE('',*,*,#56636,.F.);
#79397=ORIENTED_EDGE('',*,*,#52579,.F.);
#79398=ORIENTED_EDGE('',*,*,#56635,.T.);
#79399=ORIENTED_EDGE('',*,*,#54482,.F.);
#79400=ORIENTED_EDGE('',*,*,#56637,.F.);
#79401=ORIENTED_EDGE('',*,*,#54742,.F.);
#79402=ORIENTED_EDGE('',*,*,#56636,.T.);
#79403=ORIENTED_EDGE('',*,*,#54737,.F.);
#79404=ORIENTED_EDGE('',*,*,#56638,.F.);
#79405=ORIENTED_EDGE('',*,*,#52580,.F.);
#79406=ORIENTED_EDGE('',*,*,#56637,.T.);
#79407=ORIENTED_EDGE('',*,*,#54494,.F.);
#79408=ORIENTED_EDGE('',*,*,#56639,.F.);
#79409=ORIENTED_EDGE('',*,*,#54743,.F.);
#79410=ORIENTED_EDGE('',*,*,#56638,.T.);
#79411=ORIENTED_EDGE('',*,*,#54736,.F.);
#79412=ORIENTED_EDGE('',*,*,#56640,.F.);
#79413=ORIENTED_EDGE('',*,*,#54490,.F.);
#79414=ORIENTED_EDGE('',*,*,#56639,.T.);
#79415=ORIENTED_EDGE('',*,*,#54478,.F.);
#79416=ORIENTED_EDGE('',*,*,#56641,.F.);
#79417=ORIENTED_EDGE('',*,*,#54744,.F.);
#79418=ORIENTED_EDGE('',*,*,#56640,.T.);
#79419=ORIENTED_EDGE('',*,*,#54747,.F.);
#79420=ORIENTED_EDGE('',*,*,#56642,.F.);
#79421=ORIENTED_EDGE('',*,*,#54469,.F.);
#79422=ORIENTED_EDGE('',*,*,#56641,.T.);
#79423=ORIENTED_EDGE('',*,*,#54496,.F.);
#79424=ORIENTED_EDGE('',*,*,#56643,.F.);
#79425=ORIENTED_EDGE('',*,*,#54745,.F.);
#79426=ORIENTED_EDGE('',*,*,#56642,.T.);
#79427=ORIENTED_EDGE('',*,*,#54746,.F.);
#79428=ORIENTED_EDGE('',*,*,#56643,.T.);
#79429=ORIENTED_EDGE('',*,*,#54474,.F.);
#79430=ORIENTED_EDGE('',*,*,#54470,.T.);
#79431=ORIENTED_EDGE('',*,*,#56644,.F.);
#79432=ORIENTED_EDGE('',*,*,#54786,.F.);
#79433=ORIENTED_EDGE('',*,*,#56645,.F.);
#79434=ORIENTED_EDGE('',*,*,#54426,.F.);
#79435=ORIENTED_EDGE('',*,*,#56645,.T.);
#79436=ORIENTED_EDGE('',*,*,#54785,.F.);
#79437=ORIENTED_EDGE('',*,*,#56646,.F.);
#79438=ORIENTED_EDGE('',*,*,#54435,.F.);
#79439=ORIENTED_EDGE('',*,*,#54425,.T.);
#79440=ORIENTED_EDGE('',*,*,#54429,.F.);
#79441=ORIENTED_EDGE('',*,*,#56647,.F.);
#79442=ORIENTED_EDGE('',*,*,#54787,.F.);
#79443=ORIENTED_EDGE('',*,*,#56644,.T.);
#79444=ORIENTED_EDGE('',*,*,#56646,.T.);
#79445=ORIENTED_EDGE('',*,*,#54784,.F.);
#79446=ORIENTED_EDGE('',*,*,#56648,.F.);
#79447=ORIENTED_EDGE('',*,*,#54420,.F.);
#79448=ORIENTED_EDGE('',*,*,#56647,.T.);
#79449=ORIENTED_EDGE('',*,*,#54433,.F.);
#79450=ORIENTED_EDGE('',*,*,#56649,.F.);
#79451=ORIENTED_EDGE('',*,*,#54776,.F.);
#79452=ORIENTED_EDGE('',*,*,#56648,.T.);
#79453=ORIENTED_EDGE('',*,*,#54783,.F.);
#79454=ORIENTED_EDGE('',*,*,#56650,.F.);
#79455=ORIENTED_EDGE('',*,*,#54437,.F.);
#79456=ORIENTED_EDGE('',*,*,#56649,.T.);
#79457=ORIENTED_EDGE('',*,*,#52096,.F.);
#79458=ORIENTED_EDGE('',*,*,#56651,.F.);
#79459=ORIENTED_EDGE('',*,*,#54777,.F.);
#79460=ORIENTED_EDGE('',*,*,#56650,.T.);
#79461=ORIENTED_EDGE('',*,*,#54782,.F.);
#79462=ORIENTED_EDGE('',*,*,#56652,.F.);
#79463=ORIENTED_EDGE('',*,*,#54412,.T.);
#79464=ORIENTED_EDGE('',*,*,#54416,.F.);
#79465=ORIENTED_EDGE('',*,*,#56651,.T.);
#79466=ORIENTED_EDGE('',*,*,#52095,.F.);
#79467=ORIENTED_EDGE('',*,*,#56653,.F.);
#79468=ORIENTED_EDGE('',*,*,#56312,.F.);
#79469=ORIENTED_EDGE('',*,*,#56652,.T.);
#79470=ORIENTED_EDGE('',*,*,#54781,.F.);
#79471=ORIENTED_EDGE('',*,*,#56654,.F.);
#79472=ORIENTED_EDGE('',*,*,#54413,.F.);
#79473=ORIENTED_EDGE('',*,*,#56653,.T.);
#79474=ORIENTED_EDGE('',*,*,#52094,.F.);
#79475=ORIENTED_EDGE('',*,*,#56655,.F.);
#79476=ORIENTED_EDGE('',*,*,#54761,.F.);
#79477=ORIENTED_EDGE('',*,*,#56654,.T.);
#79478=ORIENTED_EDGE('',*,*,#54780,.F.);
#79479=ORIENTED_EDGE('',*,*,#56656,.F.);
#79480=ORIENTED_EDGE('',*,*,#54431,.F.);
#79481=ORIENTED_EDGE('',*,*,#56655,.T.);
#79482=ORIENTED_EDGE('',*,*,#52093,.F.);
#79483=ORIENTED_EDGE('',*,*,#56657,.F.);
#79484=ORIENTED_EDGE('',*,*,#56314,.F.);
#79485=ORIENTED_EDGE('',*,*,#56656,.T.);
#79486=ORIENTED_EDGE('',*,*,#54779,.F.);
#79487=ORIENTED_EDGE('',*,*,#56658,.F.);
#79488=ORIENTED_EDGE('',*,*,#52570,.F.);
#79489=ORIENTED_EDGE('',*,*,#56657,.T.);
#79490=ORIENTED_EDGE('',*,*,#52092,.F.);
#79491=ORIENTED_EDGE('',*,*,#56659,.F.);
#79492=ORIENTED_EDGE('',*,*,#54767,.F.);
#79493=ORIENTED_EDGE('',*,*,#56658,.T.);
#79494=ORIENTED_EDGE('',*,*,#56313,.F.);
#79495=ORIENTED_EDGE('',*,*,#56660,.F.);
#79496=ORIENTED_EDGE('',*,*,#52571,.F.);
#79497=ORIENTED_EDGE('',*,*,#56659,.T.);
#79498=ORIENTED_EDGE('',*,*,#54462,.F.);
#79499=ORIENTED_EDGE('',*,*,#56661,.F.);
#79500=ORIENTED_EDGE('',*,*,#54768,.F.);
#79501=ORIENTED_EDGE('',*,*,#56660,.T.);
#79502=ORIENTED_EDGE('',*,*,#54763,.F.);
#79503=ORIENTED_EDGE('',*,*,#56662,.F.);
#79504=ORIENTED_EDGE('',*,*,#52572,.F.);
#79505=ORIENTED_EDGE('',*,*,#54457,.F.);
#79506=ORIENTED_EDGE('',*,*,#54453,.T.);
#79507=ORIENTED_EDGE('',*,*,#56663,.F.);
#79508=ORIENTED_EDGE('',*,*,#54769,.F.);
#79509=ORIENTED_EDGE('',*,*,#56661,.T.);
#79510=ORIENTED_EDGE('',*,*,#56662,.T.);
#79511=ORIENTED_EDGE('',*,*,#56315,.F.);
#79512=ORIENTED_EDGE('',*,*,#56664,.F.);
#79513=ORIENTED_EDGE('',*,*,#52573,.F.);
#79514=ORIENTED_EDGE('',*,*,#56663,.T.);
#79515=ORIENTED_EDGE('',*,*,#54452,.F.);
#79516=ORIENTED_EDGE('',*,*,#56665,.F.);
#79517=ORIENTED_EDGE('',*,*,#54770,.F.);
#79518=ORIENTED_EDGE('',*,*,#56664,.T.);
#79519=ORIENTED_EDGE('',*,*,#54765,.F.);
#79520=ORIENTED_EDGE('',*,*,#56666,.F.);
#79521=ORIENTED_EDGE('',*,*,#52574,.F.);
#79522=ORIENTED_EDGE('',*,*,#56665,.T.);
#79523=ORIENTED_EDGE('',*,*,#54464,.F.);
#79524=ORIENTED_EDGE('',*,*,#56667,.F.);
#79525=ORIENTED_EDGE('',*,*,#54771,.F.);
#79526=ORIENTED_EDGE('',*,*,#56666,.T.);
#79527=ORIENTED_EDGE('',*,*,#54764,.F.);
#79528=ORIENTED_EDGE('',*,*,#56668,.F.);
#79529=ORIENTED_EDGE('',*,*,#54460,.F.);
#79530=ORIENTED_EDGE('',*,*,#56667,.T.);
#79531=ORIENTED_EDGE('',*,*,#54448,.F.);
#79532=ORIENTED_EDGE('',*,*,#56669,.F.);
#79533=ORIENTED_EDGE('',*,*,#54772,.F.);
#79534=ORIENTED_EDGE('',*,*,#56668,.T.);
#79535=ORIENTED_EDGE('',*,*,#54775,.F.);
#79536=ORIENTED_EDGE('',*,*,#56670,.F.);
#79537=ORIENTED_EDGE('',*,*,#54439,.F.);
#79538=ORIENTED_EDGE('',*,*,#56669,.T.);
#79539=ORIENTED_EDGE('',*,*,#54466,.F.);
#79540=ORIENTED_EDGE('',*,*,#56671,.F.);
#79541=ORIENTED_EDGE('',*,*,#54773,.F.);
#79542=ORIENTED_EDGE('',*,*,#56670,.T.);
#79543=ORIENTED_EDGE('',*,*,#54774,.F.);
#79544=ORIENTED_EDGE('',*,*,#56671,.T.);
#79545=ORIENTED_EDGE('',*,*,#54444,.F.);
#79546=ORIENTED_EDGE('',*,*,#54440,.T.);
#79547=ORIENTED_EDGE('',*,*,#56672,.F.);
#79548=ORIENTED_EDGE('',*,*,#54814,.F.);
#79549=ORIENTED_EDGE('',*,*,#56673,.F.);
#79550=ORIENTED_EDGE('',*,*,#54396,.F.);
#79551=ORIENTED_EDGE('',*,*,#56673,.T.);
#79552=ORIENTED_EDGE('',*,*,#54813,.F.);
#79553=ORIENTED_EDGE('',*,*,#56674,.F.);
#79554=ORIENTED_EDGE('',*,*,#54405,.F.);
#79555=ORIENTED_EDGE('',*,*,#54395,.T.);
#79556=ORIENTED_EDGE('',*,*,#54399,.F.);
#79557=ORIENTED_EDGE('',*,*,#56675,.F.);
#79558=ORIENTED_EDGE('',*,*,#54815,.F.);
#79559=ORIENTED_EDGE('',*,*,#56672,.T.);
#79560=ORIENTED_EDGE('',*,*,#56674,.T.);
#79561=ORIENTED_EDGE('',*,*,#54812,.F.);
#79562=ORIENTED_EDGE('',*,*,#56676,.F.);
#79563=ORIENTED_EDGE('',*,*,#54390,.F.);
#79564=ORIENTED_EDGE('',*,*,#56675,.T.);
#79565=ORIENTED_EDGE('',*,*,#54403,.F.);
#79566=ORIENTED_EDGE('',*,*,#56677,.F.);
#79567=ORIENTED_EDGE('',*,*,#54804,.F.);
#79568=ORIENTED_EDGE('',*,*,#56676,.T.);
#79569=ORIENTED_EDGE('',*,*,#54811,.F.);
#79570=ORIENTED_EDGE('',*,*,#56678,.F.);
#79571=ORIENTED_EDGE('',*,*,#54407,.F.);
#79572=ORIENTED_EDGE('',*,*,#56677,.T.);
#79573=ORIENTED_EDGE('',*,*,#52102,.F.);
#79574=ORIENTED_EDGE('',*,*,#56679,.F.);
#79575=ORIENTED_EDGE('',*,*,#54805,.F.);
#79576=ORIENTED_EDGE('',*,*,#56678,.T.);
#79577=ORIENTED_EDGE('',*,*,#54810,.F.);
#79578=ORIENTED_EDGE('',*,*,#56680,.F.);
#79579=ORIENTED_EDGE('',*,*,#54382,.T.);
#79580=ORIENTED_EDGE('',*,*,#54386,.F.);
#79581=ORIENTED_EDGE('',*,*,#56679,.T.);
#79582=ORIENTED_EDGE('',*,*,#52101,.F.);
#79583=ORIENTED_EDGE('',*,*,#56681,.F.);
#79584=ORIENTED_EDGE('',*,*,#56316,.F.);
#79585=ORIENTED_EDGE('',*,*,#56680,.T.);
#79586=ORIENTED_EDGE('',*,*,#54809,.F.);
#79587=ORIENTED_EDGE('',*,*,#56682,.F.);
#79588=ORIENTED_EDGE('',*,*,#54383,.F.);
#79589=ORIENTED_EDGE('',*,*,#56681,.T.);
#79590=ORIENTED_EDGE('',*,*,#52100,.F.);
#79591=ORIENTED_EDGE('',*,*,#56683,.F.);
#79592=ORIENTED_EDGE('',*,*,#54789,.F.);
#79593=ORIENTED_EDGE('',*,*,#56682,.T.);
#79594=ORIENTED_EDGE('',*,*,#54808,.F.);
#79595=ORIENTED_EDGE('',*,*,#56684,.F.);
#79596=ORIENTED_EDGE('',*,*,#54401,.F.);
#79597=ORIENTED_EDGE('',*,*,#56683,.T.);
#79598=ORIENTED_EDGE('',*,*,#52099,.F.);
#79599=ORIENTED_EDGE('',*,*,#56685,.F.);
#79600=ORIENTED_EDGE('',*,*,#56318,.F.);
#79601=ORIENTED_EDGE('',*,*,#56684,.T.);
#79602=ORIENTED_EDGE('',*,*,#54807,.F.);
#79603=ORIENTED_EDGE('',*,*,#56686,.F.);
#79604=ORIENTED_EDGE('',*,*,#52564,.F.);
#79605=ORIENTED_EDGE('',*,*,#56685,.T.);
#79606=ORIENTED_EDGE('',*,*,#52098,.F.);
#79607=ORIENTED_EDGE('',*,*,#56687,.F.);
#79608=ORIENTED_EDGE('',*,*,#54795,.F.);
#79609=ORIENTED_EDGE('',*,*,#56686,.T.);
#79610=ORIENTED_EDGE('',*,*,#56317,.F.);
#79611=ORIENTED_EDGE('',*,*,#56688,.F.);
#79612=ORIENTED_EDGE('',*,*,#52565,.F.);
#79613=ORIENTED_EDGE('',*,*,#56687,.T.);
#79614=ORIENTED_EDGE('',*,*,#54432,.F.);
#79615=ORIENTED_EDGE('',*,*,#56689,.F.);
#79616=ORIENTED_EDGE('',*,*,#54796,.F.);
#79617=ORIENTED_EDGE('',*,*,#56688,.T.);
#79618=ORIENTED_EDGE('',*,*,#54791,.F.);
#79619=ORIENTED_EDGE('',*,*,#56690,.F.);
#79620=ORIENTED_EDGE('',*,*,#52566,.F.);
#79621=ORIENTED_EDGE('',*,*,#54427,.F.);
#79622=ORIENTED_EDGE('',*,*,#54423,.T.);
#79623=ORIENTED_EDGE('',*,*,#56691,.F.);
#79624=ORIENTED_EDGE('',*,*,#54797,.F.);
#79625=ORIENTED_EDGE('',*,*,#56689,.T.);
#79626=ORIENTED_EDGE('',*,*,#56690,.T.);
#79627=ORIENTED_EDGE('',*,*,#56319,.F.);
#79628=ORIENTED_EDGE('',*,*,#56692,.F.);
#79629=ORIENTED_EDGE('',*,*,#52567,.F.);
#79630=ORIENTED_EDGE('',*,*,#56691,.T.);
#79631=ORIENTED_EDGE('',*,*,#54422,.F.);
#79632=ORIENTED_EDGE('',*,*,#56693,.F.);
#79633=ORIENTED_EDGE('',*,*,#54798,.F.);
#79634=ORIENTED_EDGE('',*,*,#56692,.T.);
#79635=ORIENTED_EDGE('',*,*,#54793,.F.);
#79636=ORIENTED_EDGE('',*,*,#56694,.F.);
#79637=ORIENTED_EDGE('',*,*,#52568,.F.);
#79638=ORIENTED_EDGE('',*,*,#56693,.T.);
#79639=ORIENTED_EDGE('',*,*,#54434,.F.);
#79640=ORIENTED_EDGE('',*,*,#56695,.F.);
#79641=ORIENTED_EDGE('',*,*,#54799,.F.);
#79642=ORIENTED_EDGE('',*,*,#56694,.T.);
#79643=ORIENTED_EDGE('',*,*,#54792,.F.);
#79644=ORIENTED_EDGE('',*,*,#56696,.F.);
#79645=ORIENTED_EDGE('',*,*,#54430,.F.);
#79646=ORIENTED_EDGE('',*,*,#56695,.T.);
#79647=ORIENTED_EDGE('',*,*,#54418,.F.);
#79648=ORIENTED_EDGE('',*,*,#56697,.F.);
#79649=ORIENTED_EDGE('',*,*,#54800,.F.);
#79650=ORIENTED_EDGE('',*,*,#56696,.T.);
#79651=ORIENTED_EDGE('',*,*,#54803,.F.);
#79652=ORIENTED_EDGE('',*,*,#56698,.F.);
#79653=ORIENTED_EDGE('',*,*,#54409,.F.);
#79654=ORIENTED_EDGE('',*,*,#56697,.T.);
#79655=ORIENTED_EDGE('',*,*,#54436,.F.);
#79656=ORIENTED_EDGE('',*,*,#56699,.F.);
#79657=ORIENTED_EDGE('',*,*,#54801,.F.);
#79658=ORIENTED_EDGE('',*,*,#56698,.T.);
#79659=ORIENTED_EDGE('',*,*,#54802,.F.);
#79660=ORIENTED_EDGE('',*,*,#56699,.T.);
#79661=ORIENTED_EDGE('',*,*,#54414,.F.);
#79662=ORIENTED_EDGE('',*,*,#54410,.T.);
#79663=ORIENTED_EDGE('',*,*,#56700,.F.);
#79664=ORIENTED_EDGE('',*,*,#54842,.F.);
#79665=ORIENTED_EDGE('',*,*,#56701,.F.);
#79666=ORIENTED_EDGE('',*,*,#54366,.F.);
#79667=ORIENTED_EDGE('',*,*,#56701,.T.);
#79668=ORIENTED_EDGE('',*,*,#54841,.F.);
#79669=ORIENTED_EDGE('',*,*,#56702,.F.);
#79670=ORIENTED_EDGE('',*,*,#54375,.F.);
#79671=ORIENTED_EDGE('',*,*,#54365,.T.);
#79672=ORIENTED_EDGE('',*,*,#54369,.F.);
#79673=ORIENTED_EDGE('',*,*,#56703,.F.);
#79674=ORIENTED_EDGE('',*,*,#54843,.F.);
#79675=ORIENTED_EDGE('',*,*,#56700,.T.);
#79676=ORIENTED_EDGE('',*,*,#56702,.T.);
#79677=ORIENTED_EDGE('',*,*,#54840,.F.);
#79678=ORIENTED_EDGE('',*,*,#56704,.F.);
#79679=ORIENTED_EDGE('',*,*,#54360,.F.);
#79680=ORIENTED_EDGE('',*,*,#56703,.T.);
#79681=ORIENTED_EDGE('',*,*,#54373,.F.);
#79682=ORIENTED_EDGE('',*,*,#56705,.F.);
#79683=ORIENTED_EDGE('',*,*,#54832,.F.);
#79684=ORIENTED_EDGE('',*,*,#56704,.T.);
#79685=ORIENTED_EDGE('',*,*,#54839,.F.);
#79686=ORIENTED_EDGE('',*,*,#56706,.F.);
#79687=ORIENTED_EDGE('',*,*,#54377,.F.);
#79688=ORIENTED_EDGE('',*,*,#56705,.T.);
#79689=ORIENTED_EDGE('',*,*,#52108,.F.);
#79690=ORIENTED_EDGE('',*,*,#56707,.F.);
#79691=ORIENTED_EDGE('',*,*,#54833,.F.);
#79692=ORIENTED_EDGE('',*,*,#56706,.T.);
#79693=ORIENTED_EDGE('',*,*,#54838,.F.);
#79694=ORIENTED_EDGE('',*,*,#56708,.F.);
#79695=ORIENTED_EDGE('',*,*,#54352,.T.);
#79696=ORIENTED_EDGE('',*,*,#54356,.F.);
#79697=ORIENTED_EDGE('',*,*,#56707,.T.);
#79698=ORIENTED_EDGE('',*,*,#52107,.F.);
#79699=ORIENTED_EDGE('',*,*,#56709,.F.);
#79700=ORIENTED_EDGE('',*,*,#56320,.F.);
#79701=ORIENTED_EDGE('',*,*,#56708,.T.);
#79702=ORIENTED_EDGE('',*,*,#54837,.F.);
#79703=ORIENTED_EDGE('',*,*,#56710,.F.);
#79704=ORIENTED_EDGE('',*,*,#54353,.F.);
#79705=ORIENTED_EDGE('',*,*,#56709,.T.);
#79706=ORIENTED_EDGE('',*,*,#52106,.F.);
#79707=ORIENTED_EDGE('',*,*,#56711,.F.);
#79708=ORIENTED_EDGE('',*,*,#54817,.F.);
#79709=ORIENTED_EDGE('',*,*,#56710,.T.);
#79710=ORIENTED_EDGE('',*,*,#54836,.F.);
#79711=ORIENTED_EDGE('',*,*,#56712,.F.);
#79712=ORIENTED_EDGE('',*,*,#54371,.F.);
#79713=ORIENTED_EDGE('',*,*,#56711,.T.);
#79714=ORIENTED_EDGE('',*,*,#52105,.F.);
#79715=ORIENTED_EDGE('',*,*,#56713,.F.);
#79716=ORIENTED_EDGE('',*,*,#56322,.F.);
#79717=ORIENTED_EDGE('',*,*,#56712,.T.);
#79718=ORIENTED_EDGE('',*,*,#54835,.F.);
#79719=ORIENTED_EDGE('',*,*,#56714,.F.);
#79720=ORIENTED_EDGE('',*,*,#52558,.F.);
#79721=ORIENTED_EDGE('',*,*,#56713,.T.);
#79722=ORIENTED_EDGE('',*,*,#52104,.F.);
#79723=ORIENTED_EDGE('',*,*,#56715,.F.);
#79724=ORIENTED_EDGE('',*,*,#54823,.F.);
#79725=ORIENTED_EDGE('',*,*,#56714,.T.);
#79726=ORIENTED_EDGE('',*,*,#56321,.F.);
#79727=ORIENTED_EDGE('',*,*,#56716,.F.);
#79728=ORIENTED_EDGE('',*,*,#52559,.F.);
#79729=ORIENTED_EDGE('',*,*,#56715,.T.);
#79730=ORIENTED_EDGE('',*,*,#54402,.F.);
#79731=ORIENTED_EDGE('',*,*,#56717,.F.);
#79732=ORIENTED_EDGE('',*,*,#54824,.F.);
#79733=ORIENTED_EDGE('',*,*,#56716,.T.);
#79734=ORIENTED_EDGE('',*,*,#54819,.F.);
#79735=ORIENTED_EDGE('',*,*,#56718,.F.);
#79736=ORIENTED_EDGE('',*,*,#52560,.F.);
#79737=ORIENTED_EDGE('',*,*,#54397,.F.);
#79738=ORIENTED_EDGE('',*,*,#54393,.T.);
#79739=ORIENTED_EDGE('',*,*,#56719,.F.);
#79740=ORIENTED_EDGE('',*,*,#54825,.F.);
#79741=ORIENTED_EDGE('',*,*,#56717,.T.);
#79742=ORIENTED_EDGE('',*,*,#56718,.T.);
#79743=ORIENTED_EDGE('',*,*,#56323,.F.);
#79744=ORIENTED_EDGE('',*,*,#56720,.F.);
#79745=ORIENTED_EDGE('',*,*,#52561,.F.);
#79746=ORIENTED_EDGE('',*,*,#56719,.T.);
#79747=ORIENTED_EDGE('',*,*,#54392,.F.);
#79748=ORIENTED_EDGE('',*,*,#56721,.F.);
#79749=ORIENTED_EDGE('',*,*,#54826,.F.);
#79750=ORIENTED_EDGE('',*,*,#56720,.T.);
#79751=ORIENTED_EDGE('',*,*,#54821,.F.);
#79752=ORIENTED_EDGE('',*,*,#56722,.F.);
#79753=ORIENTED_EDGE('',*,*,#52562,.F.);
#79754=ORIENTED_EDGE('',*,*,#56721,.T.);
#79755=ORIENTED_EDGE('',*,*,#54404,.F.);
#79756=ORIENTED_EDGE('',*,*,#56723,.F.);
#79757=ORIENTED_EDGE('',*,*,#54827,.F.);
#79758=ORIENTED_EDGE('',*,*,#56722,.T.);
#79759=ORIENTED_EDGE('',*,*,#54820,.F.);
#79760=ORIENTED_EDGE('',*,*,#56724,.F.);
#79761=ORIENTED_EDGE('',*,*,#54400,.F.);
#79762=ORIENTED_EDGE('',*,*,#56723,.T.);
#79763=ORIENTED_EDGE('',*,*,#54388,.F.);
#79764=ORIENTED_EDGE('',*,*,#56725,.F.);
#79765=ORIENTED_EDGE('',*,*,#54828,.F.);
#79766=ORIENTED_EDGE('',*,*,#56724,.T.);
#79767=ORIENTED_EDGE('',*,*,#54831,.F.);
#79768=ORIENTED_EDGE('',*,*,#56726,.F.);
#79769=ORIENTED_EDGE('',*,*,#54379,.F.);
#79770=ORIENTED_EDGE('',*,*,#56725,.T.);
#79771=ORIENTED_EDGE('',*,*,#54406,.F.);
#79772=ORIENTED_EDGE('',*,*,#56727,.F.);
#79773=ORIENTED_EDGE('',*,*,#54829,.F.);
#79774=ORIENTED_EDGE('',*,*,#56726,.T.);
#79775=ORIENTED_EDGE('',*,*,#54830,.F.);
#79776=ORIENTED_EDGE('',*,*,#56727,.T.);
#79777=ORIENTED_EDGE('',*,*,#54384,.F.);
#79778=ORIENTED_EDGE('',*,*,#54380,.T.);
#79779=ORIENTED_EDGE('',*,*,#56728,.F.);
#79780=ORIENTED_EDGE('',*,*,#54870,.F.);
#79781=ORIENTED_EDGE('',*,*,#56729,.F.);
#79782=ORIENTED_EDGE('',*,*,#54336,.F.);
#79783=ORIENTED_EDGE('',*,*,#56729,.T.);
#79784=ORIENTED_EDGE('',*,*,#54869,.F.);
#79785=ORIENTED_EDGE('',*,*,#56730,.F.);
#79786=ORIENTED_EDGE('',*,*,#54345,.F.);
#79787=ORIENTED_EDGE('',*,*,#54335,.T.);
#79788=ORIENTED_EDGE('',*,*,#54339,.F.);
#79789=ORIENTED_EDGE('',*,*,#56731,.F.);
#79790=ORIENTED_EDGE('',*,*,#54871,.F.);
#79791=ORIENTED_EDGE('',*,*,#56728,.T.);
#79792=ORIENTED_EDGE('',*,*,#56730,.T.);
#79793=ORIENTED_EDGE('',*,*,#54868,.F.);
#79794=ORIENTED_EDGE('',*,*,#56732,.F.);
#79795=ORIENTED_EDGE('',*,*,#54330,.F.);
#79796=ORIENTED_EDGE('',*,*,#56731,.T.);
#79797=ORIENTED_EDGE('',*,*,#54343,.F.);
#79798=ORIENTED_EDGE('',*,*,#56733,.F.);
#79799=ORIENTED_EDGE('',*,*,#54860,.F.);
#79800=ORIENTED_EDGE('',*,*,#56732,.T.);
#79801=ORIENTED_EDGE('',*,*,#54867,.F.);
#79802=ORIENTED_EDGE('',*,*,#56734,.F.);
#79803=ORIENTED_EDGE('',*,*,#54347,.F.);
#79804=ORIENTED_EDGE('',*,*,#56733,.T.);
#79805=ORIENTED_EDGE('',*,*,#52114,.F.);
#79806=ORIENTED_EDGE('',*,*,#56735,.F.);
#79807=ORIENTED_EDGE('',*,*,#54861,.F.);
#79808=ORIENTED_EDGE('',*,*,#56734,.T.);
#79809=ORIENTED_EDGE('',*,*,#54866,.F.);
#79810=ORIENTED_EDGE('',*,*,#56736,.F.);
#79811=ORIENTED_EDGE('',*,*,#54322,.T.);
#79812=ORIENTED_EDGE('',*,*,#54326,.F.);
#79813=ORIENTED_EDGE('',*,*,#56735,.T.);
#79814=ORIENTED_EDGE('',*,*,#52113,.F.);
#79815=ORIENTED_EDGE('',*,*,#56737,.F.);
#79816=ORIENTED_EDGE('',*,*,#56324,.F.);
#79817=ORIENTED_EDGE('',*,*,#56736,.T.);
#79818=ORIENTED_EDGE('',*,*,#54865,.F.);
#79819=ORIENTED_EDGE('',*,*,#56738,.F.);
#79820=ORIENTED_EDGE('',*,*,#54323,.F.);
#79821=ORIENTED_EDGE('',*,*,#56737,.T.);
#79822=ORIENTED_EDGE('',*,*,#52112,.F.);
#79823=ORIENTED_EDGE('',*,*,#56739,.F.);
#79824=ORIENTED_EDGE('',*,*,#54845,.F.);
#79825=ORIENTED_EDGE('',*,*,#56738,.T.);
#79826=ORIENTED_EDGE('',*,*,#54864,.F.);
#79827=ORIENTED_EDGE('',*,*,#56740,.F.);
#79828=ORIENTED_EDGE('',*,*,#54341,.F.);
#79829=ORIENTED_EDGE('',*,*,#56739,.T.);
#79830=ORIENTED_EDGE('',*,*,#52111,.F.);
#79831=ORIENTED_EDGE('',*,*,#56741,.F.);
#79832=ORIENTED_EDGE('',*,*,#56326,.F.);
#79833=ORIENTED_EDGE('',*,*,#56740,.T.);
#79834=ORIENTED_EDGE('',*,*,#54863,.F.);
#79835=ORIENTED_EDGE('',*,*,#56742,.F.);
#79836=ORIENTED_EDGE('',*,*,#52552,.F.);
#79837=ORIENTED_EDGE('',*,*,#56741,.T.);
#79838=ORIENTED_EDGE('',*,*,#52110,.F.);
#79839=ORIENTED_EDGE('',*,*,#56743,.F.);
#79840=ORIENTED_EDGE('',*,*,#54851,.F.);
#79841=ORIENTED_EDGE('',*,*,#56742,.T.);
#79842=ORIENTED_EDGE('',*,*,#56325,.F.);
#79843=ORIENTED_EDGE('',*,*,#56744,.F.);
#79844=ORIENTED_EDGE('',*,*,#52553,.F.);
#79845=ORIENTED_EDGE('',*,*,#56743,.T.);
#79846=ORIENTED_EDGE('',*,*,#54372,.F.);
#79847=ORIENTED_EDGE('',*,*,#56745,.F.);
#79848=ORIENTED_EDGE('',*,*,#54852,.F.);
#79849=ORIENTED_EDGE('',*,*,#56744,.T.);
#79850=ORIENTED_EDGE('',*,*,#54847,.F.);
#79851=ORIENTED_EDGE('',*,*,#56746,.F.);
#79852=ORIENTED_EDGE('',*,*,#52554,.F.);
#79853=ORIENTED_EDGE('',*,*,#54367,.F.);
#79854=ORIENTED_EDGE('',*,*,#54363,.T.);
#79855=ORIENTED_EDGE('',*,*,#56747,.F.);
#79856=ORIENTED_EDGE('',*,*,#54853,.F.);
#79857=ORIENTED_EDGE('',*,*,#56745,.T.);
#79858=ORIENTED_EDGE('',*,*,#56746,.T.);
#79859=ORIENTED_EDGE('',*,*,#56327,.F.);
#79860=ORIENTED_EDGE('',*,*,#56748,.F.);
#79861=ORIENTED_EDGE('',*,*,#52555,.F.);
#79862=ORIENTED_EDGE('',*,*,#56747,.T.);
#79863=ORIENTED_EDGE('',*,*,#54362,.F.);
#79864=ORIENTED_EDGE('',*,*,#56749,.F.);
#79865=ORIENTED_EDGE('',*,*,#54854,.F.);
#79866=ORIENTED_EDGE('',*,*,#56748,.T.);
#79867=ORIENTED_EDGE('',*,*,#54849,.F.);
#79868=ORIENTED_EDGE('',*,*,#56750,.F.);
#79869=ORIENTED_EDGE('',*,*,#52556,.F.);
#79870=ORIENTED_EDGE('',*,*,#56749,.T.);
#79871=ORIENTED_EDGE('',*,*,#54374,.F.);
#79872=ORIENTED_EDGE('',*,*,#56751,.F.);
#79873=ORIENTED_EDGE('',*,*,#54855,.F.);
#79874=ORIENTED_EDGE('',*,*,#56750,.T.);
#79875=ORIENTED_EDGE('',*,*,#54848,.F.);
#79876=ORIENTED_EDGE('',*,*,#56752,.F.);
#79877=ORIENTED_EDGE('',*,*,#54370,.F.);
#79878=ORIENTED_EDGE('',*,*,#56751,.T.);
#79879=ORIENTED_EDGE('',*,*,#54358,.F.);
#79880=ORIENTED_EDGE('',*,*,#56753,.F.);
#79881=ORIENTED_EDGE('',*,*,#54856,.F.);
#79882=ORIENTED_EDGE('',*,*,#56752,.T.);
#79883=ORIENTED_EDGE('',*,*,#54859,.F.);
#79884=ORIENTED_EDGE('',*,*,#56754,.F.);
#79885=ORIENTED_EDGE('',*,*,#54349,.F.);
#79886=ORIENTED_EDGE('',*,*,#56753,.T.);
#79887=ORIENTED_EDGE('',*,*,#54376,.F.);
#79888=ORIENTED_EDGE('',*,*,#56755,.F.);
#79889=ORIENTED_EDGE('',*,*,#54857,.F.);
#79890=ORIENTED_EDGE('',*,*,#56754,.T.);
#79891=ORIENTED_EDGE('',*,*,#54858,.F.);
#79892=ORIENTED_EDGE('',*,*,#56755,.T.);
#79893=ORIENTED_EDGE('',*,*,#54354,.F.);
#79894=ORIENTED_EDGE('',*,*,#54350,.T.);
#79895=ORIENTED_EDGE('',*,*,#56756,.F.);
#79896=ORIENTED_EDGE('',*,*,#54898,.F.);
#79897=ORIENTED_EDGE('',*,*,#56757,.F.);
#79898=ORIENTED_EDGE('',*,*,#54306,.F.);
#79899=ORIENTED_EDGE('',*,*,#56757,.T.);
#79900=ORIENTED_EDGE('',*,*,#54897,.F.);
#79901=ORIENTED_EDGE('',*,*,#56758,.F.);
#79902=ORIENTED_EDGE('',*,*,#54315,.F.);
#79903=ORIENTED_EDGE('',*,*,#54305,.T.);
#79904=ORIENTED_EDGE('',*,*,#54309,.F.);
#79905=ORIENTED_EDGE('',*,*,#56759,.F.);
#79906=ORIENTED_EDGE('',*,*,#54899,.F.);
#79907=ORIENTED_EDGE('',*,*,#56756,.T.);
#79908=ORIENTED_EDGE('',*,*,#56758,.T.);
#79909=ORIENTED_EDGE('',*,*,#54896,.F.);
#79910=ORIENTED_EDGE('',*,*,#56760,.F.);
#79911=ORIENTED_EDGE('',*,*,#54300,.F.);
#79912=ORIENTED_EDGE('',*,*,#56759,.T.);
#79913=ORIENTED_EDGE('',*,*,#54313,.F.);
#79914=ORIENTED_EDGE('',*,*,#56761,.F.);
#79915=ORIENTED_EDGE('',*,*,#54888,.F.);
#79916=ORIENTED_EDGE('',*,*,#56760,.T.);
#79917=ORIENTED_EDGE('',*,*,#54895,.F.);
#79918=ORIENTED_EDGE('',*,*,#56762,.F.);
#79919=ORIENTED_EDGE('',*,*,#54317,.F.);
#79920=ORIENTED_EDGE('',*,*,#56761,.T.);
#79921=ORIENTED_EDGE('',*,*,#52120,.F.);
#79922=ORIENTED_EDGE('',*,*,#56763,.F.);
#79923=ORIENTED_EDGE('',*,*,#54889,.F.);
#79924=ORIENTED_EDGE('',*,*,#56762,.T.);
#79925=ORIENTED_EDGE('',*,*,#54894,.F.);
#79926=ORIENTED_EDGE('',*,*,#56764,.F.);
#79927=ORIENTED_EDGE('',*,*,#54292,.T.);
#79928=ORIENTED_EDGE('',*,*,#54296,.F.);
#79929=ORIENTED_EDGE('',*,*,#56763,.T.);
#79930=ORIENTED_EDGE('',*,*,#52119,.F.);
#79931=ORIENTED_EDGE('',*,*,#56765,.F.);
#79932=ORIENTED_EDGE('',*,*,#56328,.F.);
#79933=ORIENTED_EDGE('',*,*,#56764,.T.);
#79934=ORIENTED_EDGE('',*,*,#54893,.F.);
#79935=ORIENTED_EDGE('',*,*,#56766,.F.);
#79936=ORIENTED_EDGE('',*,*,#54293,.F.);
#79937=ORIENTED_EDGE('',*,*,#56765,.T.);
#79938=ORIENTED_EDGE('',*,*,#52118,.F.);
#79939=ORIENTED_EDGE('',*,*,#56767,.F.);
#79940=ORIENTED_EDGE('',*,*,#54873,.F.);
#79941=ORIENTED_EDGE('',*,*,#56766,.T.);
#79942=ORIENTED_EDGE('',*,*,#54892,.F.);
#79943=ORIENTED_EDGE('',*,*,#56768,.F.);
#79944=ORIENTED_EDGE('',*,*,#54311,.F.);
#79945=ORIENTED_EDGE('',*,*,#56767,.T.);
#79946=ORIENTED_EDGE('',*,*,#52117,.F.);
#79947=ORIENTED_EDGE('',*,*,#56769,.F.);
#79948=ORIENTED_EDGE('',*,*,#56330,.F.);
#79949=ORIENTED_EDGE('',*,*,#56768,.T.);
#79950=ORIENTED_EDGE('',*,*,#54891,.F.);
#79951=ORIENTED_EDGE('',*,*,#56770,.F.);
#79952=ORIENTED_EDGE('',*,*,#52546,.F.);
#79953=ORIENTED_EDGE('',*,*,#56769,.T.);
#79954=ORIENTED_EDGE('',*,*,#52116,.F.);
#79955=ORIENTED_EDGE('',*,*,#56771,.F.);
#79956=ORIENTED_EDGE('',*,*,#54879,.F.);
#79957=ORIENTED_EDGE('',*,*,#56770,.T.);
#79958=ORIENTED_EDGE('',*,*,#56329,.F.);
#79959=ORIENTED_EDGE('',*,*,#56772,.F.);
#79960=ORIENTED_EDGE('',*,*,#52547,.F.);
#79961=ORIENTED_EDGE('',*,*,#56771,.T.);
#79962=ORIENTED_EDGE('',*,*,#54342,.F.);
#79963=ORIENTED_EDGE('',*,*,#56773,.F.);
#79964=ORIENTED_EDGE('',*,*,#54880,.F.);
#79965=ORIENTED_EDGE('',*,*,#56772,.T.);
#79966=ORIENTED_EDGE('',*,*,#54875,.F.);
#79967=ORIENTED_EDGE('',*,*,#56774,.F.);
#79968=ORIENTED_EDGE('',*,*,#52548,.F.);
#79969=ORIENTED_EDGE('',*,*,#54337,.F.);
#79970=ORIENTED_EDGE('',*,*,#54333,.T.);
#79971=ORIENTED_EDGE('',*,*,#56775,.F.);
#79972=ORIENTED_EDGE('',*,*,#54881,.F.);
#79973=ORIENTED_EDGE('',*,*,#56773,.T.);
#79974=ORIENTED_EDGE('',*,*,#56774,.T.);
#79975=ORIENTED_EDGE('',*,*,#56331,.F.);
#79976=ORIENTED_EDGE('',*,*,#56776,.F.);
#79977=ORIENTED_EDGE('',*,*,#52549,.F.);
#79978=ORIENTED_EDGE('',*,*,#56775,.T.);
#79979=ORIENTED_EDGE('',*,*,#54332,.F.);
#79980=ORIENTED_EDGE('',*,*,#56777,.F.);
#79981=ORIENTED_EDGE('',*,*,#54882,.F.);
#79982=ORIENTED_EDGE('',*,*,#56776,.T.);
#79983=ORIENTED_EDGE('',*,*,#54877,.F.);
#79984=ORIENTED_EDGE('',*,*,#56778,.F.);
#79985=ORIENTED_EDGE('',*,*,#52550,.F.);
#79986=ORIENTED_EDGE('',*,*,#56777,.T.);
#79987=ORIENTED_EDGE('',*,*,#54344,.F.);
#79988=ORIENTED_EDGE('',*,*,#56779,.F.);
#79989=ORIENTED_EDGE('',*,*,#54883,.F.);
#79990=ORIENTED_EDGE('',*,*,#56778,.T.);
#79991=ORIENTED_EDGE('',*,*,#54876,.F.);
#79992=ORIENTED_EDGE('',*,*,#56780,.F.);
#79993=ORIENTED_EDGE('',*,*,#54340,.F.);
#79994=ORIENTED_EDGE('',*,*,#56779,.T.);
#79995=ORIENTED_EDGE('',*,*,#54328,.F.);
#79996=ORIENTED_EDGE('',*,*,#56781,.F.);
#79997=ORIENTED_EDGE('',*,*,#54884,.F.);
#79998=ORIENTED_EDGE('',*,*,#56780,.T.);
#79999=ORIENTED_EDGE('',*,*,#54887,.F.);
#80000=ORIENTED_EDGE('',*,*,#56782,.F.);
#80001=ORIENTED_EDGE('',*,*,#54319,.F.);
#80002=ORIENTED_EDGE('',*,*,#56781,.T.);
#80003=ORIENTED_EDGE('',*,*,#54346,.F.);
#80004=ORIENTED_EDGE('',*,*,#56783,.F.);
#80005=ORIENTED_EDGE('',*,*,#54885,.F.);
#80006=ORIENTED_EDGE('',*,*,#56782,.T.);
#80007=ORIENTED_EDGE('',*,*,#54886,.F.);
#80008=ORIENTED_EDGE('',*,*,#56783,.T.);
#80009=ORIENTED_EDGE('',*,*,#54324,.F.);
#80010=ORIENTED_EDGE('',*,*,#54320,.T.);
#80011=ORIENTED_EDGE('',*,*,#56784,.F.);
#80012=ORIENTED_EDGE('',*,*,#54926,.F.);
#80013=ORIENTED_EDGE('',*,*,#56785,.F.);
#80014=ORIENTED_EDGE('',*,*,#54276,.F.);
#80015=ORIENTED_EDGE('',*,*,#56785,.T.);
#80016=ORIENTED_EDGE('',*,*,#54925,.F.);
#80017=ORIENTED_EDGE('',*,*,#56786,.F.);
#80018=ORIENTED_EDGE('',*,*,#54285,.F.);
#80019=ORIENTED_EDGE('',*,*,#54275,.T.);
#80020=ORIENTED_EDGE('',*,*,#54279,.F.);
#80021=ORIENTED_EDGE('',*,*,#56787,.F.);
#80022=ORIENTED_EDGE('',*,*,#54927,.F.);
#80023=ORIENTED_EDGE('',*,*,#56784,.T.);
#80024=ORIENTED_EDGE('',*,*,#56786,.T.);
#80025=ORIENTED_EDGE('',*,*,#54924,.F.);
#80026=ORIENTED_EDGE('',*,*,#56788,.F.);
#80027=ORIENTED_EDGE('',*,*,#54270,.F.);
#80028=ORIENTED_EDGE('',*,*,#56787,.T.);
#80029=ORIENTED_EDGE('',*,*,#54283,.F.);
#80030=ORIENTED_EDGE('',*,*,#56789,.F.);
#80031=ORIENTED_EDGE('',*,*,#54916,.F.);
#80032=ORIENTED_EDGE('',*,*,#56788,.T.);
#80033=ORIENTED_EDGE('',*,*,#54923,.F.);
#80034=ORIENTED_EDGE('',*,*,#56790,.F.);
#80035=ORIENTED_EDGE('',*,*,#54287,.F.);
#80036=ORIENTED_EDGE('',*,*,#56789,.T.);
#80037=ORIENTED_EDGE('',*,*,#52126,.F.);
#80038=ORIENTED_EDGE('',*,*,#56791,.F.);
#80039=ORIENTED_EDGE('',*,*,#54917,.F.);
#80040=ORIENTED_EDGE('',*,*,#56790,.T.);
#80041=ORIENTED_EDGE('',*,*,#54922,.F.);
#80042=ORIENTED_EDGE('',*,*,#56792,.F.);
#80043=ORIENTED_EDGE('',*,*,#54262,.T.);
#80044=ORIENTED_EDGE('',*,*,#54266,.F.);
#80045=ORIENTED_EDGE('',*,*,#56791,.T.);
#80046=ORIENTED_EDGE('',*,*,#52125,.F.);
#80047=ORIENTED_EDGE('',*,*,#56793,.F.);
#80048=ORIENTED_EDGE('',*,*,#56332,.F.);
#80049=ORIENTED_EDGE('',*,*,#56792,.T.);
#80050=ORIENTED_EDGE('',*,*,#54921,.F.);
#80051=ORIENTED_EDGE('',*,*,#56794,.F.);
#80052=ORIENTED_EDGE('',*,*,#54263,.F.);
#80053=ORIENTED_EDGE('',*,*,#56793,.T.);
#80054=ORIENTED_EDGE('',*,*,#52124,.F.);
#80055=ORIENTED_EDGE('',*,*,#56795,.F.);
#80056=ORIENTED_EDGE('',*,*,#54901,.F.);
#80057=ORIENTED_EDGE('',*,*,#56794,.T.);
#80058=ORIENTED_EDGE('',*,*,#54920,.F.);
#80059=ORIENTED_EDGE('',*,*,#56796,.F.);
#80060=ORIENTED_EDGE('',*,*,#54281,.F.);
#80061=ORIENTED_EDGE('',*,*,#56795,.T.);
#80062=ORIENTED_EDGE('',*,*,#52123,.F.);
#80063=ORIENTED_EDGE('',*,*,#56797,.F.);
#80064=ORIENTED_EDGE('',*,*,#56334,.F.);
#80065=ORIENTED_EDGE('',*,*,#56796,.T.);
#80066=ORIENTED_EDGE('',*,*,#54919,.F.);
#80067=ORIENTED_EDGE('',*,*,#56798,.F.);
#80068=ORIENTED_EDGE('',*,*,#52540,.F.);
#80069=ORIENTED_EDGE('',*,*,#56797,.T.);
#80070=ORIENTED_EDGE('',*,*,#52122,.F.);
#80071=ORIENTED_EDGE('',*,*,#56799,.F.);
#80072=ORIENTED_EDGE('',*,*,#54907,.F.);
#80073=ORIENTED_EDGE('',*,*,#56798,.T.);
#80074=ORIENTED_EDGE('',*,*,#56333,.F.);
#80075=ORIENTED_EDGE('',*,*,#56800,.F.);
#80076=ORIENTED_EDGE('',*,*,#52541,.F.);
#80077=ORIENTED_EDGE('',*,*,#56799,.T.);
#80078=ORIENTED_EDGE('',*,*,#54312,.F.);
#80079=ORIENTED_EDGE('',*,*,#56801,.F.);
#80080=ORIENTED_EDGE('',*,*,#54908,.F.);
#80081=ORIENTED_EDGE('',*,*,#56800,.T.);
#80082=ORIENTED_EDGE('',*,*,#54903,.F.);
#80083=ORIENTED_EDGE('',*,*,#56802,.F.);
#80084=ORIENTED_EDGE('',*,*,#52542,.F.);
#80085=ORIENTED_EDGE('',*,*,#54307,.F.);
#80086=ORIENTED_EDGE('',*,*,#54303,.T.);
#80087=ORIENTED_EDGE('',*,*,#56803,.F.);
#80088=ORIENTED_EDGE('',*,*,#54909,.F.);
#80089=ORIENTED_EDGE('',*,*,#56801,.T.);
#80090=ORIENTED_EDGE('',*,*,#56802,.T.);
#80091=ORIENTED_EDGE('',*,*,#56335,.F.);
#80092=ORIENTED_EDGE('',*,*,#56804,.F.);
#80093=ORIENTED_EDGE('',*,*,#52543,.F.);
#80094=ORIENTED_EDGE('',*,*,#56803,.T.);
#80095=ORIENTED_EDGE('',*,*,#54302,.F.);
#80096=ORIENTED_EDGE('',*,*,#56805,.F.);
#80097=ORIENTED_EDGE('',*,*,#54910,.F.);
#80098=ORIENTED_EDGE('',*,*,#56804,.T.);
#80099=ORIENTED_EDGE('',*,*,#54905,.F.);
#80100=ORIENTED_EDGE('',*,*,#56806,.F.);
#80101=ORIENTED_EDGE('',*,*,#52544,.F.);
#80102=ORIENTED_EDGE('',*,*,#56805,.T.);
#80103=ORIENTED_EDGE('',*,*,#54314,.F.);
#80104=ORIENTED_EDGE('',*,*,#56807,.F.);
#80105=ORIENTED_EDGE('',*,*,#54911,.F.);
#80106=ORIENTED_EDGE('',*,*,#56806,.T.);
#80107=ORIENTED_EDGE('',*,*,#54904,.F.);
#80108=ORIENTED_EDGE('',*,*,#56808,.F.);
#80109=ORIENTED_EDGE('',*,*,#54310,.F.);
#80110=ORIENTED_EDGE('',*,*,#56807,.T.);
#80111=ORIENTED_EDGE('',*,*,#54298,.F.);
#80112=ORIENTED_EDGE('',*,*,#56809,.F.);
#80113=ORIENTED_EDGE('',*,*,#54912,.F.);
#80114=ORIENTED_EDGE('',*,*,#56808,.T.);
#80115=ORIENTED_EDGE('',*,*,#54915,.F.);
#80116=ORIENTED_EDGE('',*,*,#56810,.F.);
#80117=ORIENTED_EDGE('',*,*,#54289,.F.);
#80118=ORIENTED_EDGE('',*,*,#56809,.T.);
#80119=ORIENTED_EDGE('',*,*,#54316,.F.);
#80120=ORIENTED_EDGE('',*,*,#56811,.F.);
#80121=ORIENTED_EDGE('',*,*,#54913,.F.);
#80122=ORIENTED_EDGE('',*,*,#56810,.T.);
#80123=ORIENTED_EDGE('',*,*,#54914,.F.);
#80124=ORIENTED_EDGE('',*,*,#56811,.T.);
#80125=ORIENTED_EDGE('',*,*,#54294,.F.);
#80126=ORIENTED_EDGE('',*,*,#54290,.T.);
#80127=ORIENTED_EDGE('',*,*,#56812,.F.);
#80128=ORIENTED_EDGE('',*,*,#54954,.F.);
#80129=ORIENTED_EDGE('',*,*,#56813,.F.);
#80130=ORIENTED_EDGE('',*,*,#54246,.F.);
#80131=ORIENTED_EDGE('',*,*,#56813,.T.);
#80132=ORIENTED_EDGE('',*,*,#54953,.F.);
#80133=ORIENTED_EDGE('',*,*,#56814,.F.);
#80134=ORIENTED_EDGE('',*,*,#54255,.F.);
#80135=ORIENTED_EDGE('',*,*,#54245,.T.);
#80136=ORIENTED_EDGE('',*,*,#54249,.F.);
#80137=ORIENTED_EDGE('',*,*,#56815,.F.);
#80138=ORIENTED_EDGE('',*,*,#54955,.F.);
#80139=ORIENTED_EDGE('',*,*,#56812,.T.);
#80140=ORIENTED_EDGE('',*,*,#56814,.T.);
#80141=ORIENTED_EDGE('',*,*,#54952,.F.);
#80142=ORIENTED_EDGE('',*,*,#56816,.F.);
#80143=ORIENTED_EDGE('',*,*,#54240,.F.);
#80144=ORIENTED_EDGE('',*,*,#56815,.T.);
#80145=ORIENTED_EDGE('',*,*,#54253,.F.);
#80146=ORIENTED_EDGE('',*,*,#56817,.F.);
#80147=ORIENTED_EDGE('',*,*,#54944,.F.);
#80148=ORIENTED_EDGE('',*,*,#56816,.T.);
#80149=ORIENTED_EDGE('',*,*,#54951,.F.);
#80150=ORIENTED_EDGE('',*,*,#56818,.F.);
#80151=ORIENTED_EDGE('',*,*,#54257,.F.);
#80152=ORIENTED_EDGE('',*,*,#56817,.T.);
#80153=ORIENTED_EDGE('',*,*,#52132,.F.);
#80154=ORIENTED_EDGE('',*,*,#56819,.F.);
#80155=ORIENTED_EDGE('',*,*,#54945,.F.);
#80156=ORIENTED_EDGE('',*,*,#56818,.T.);
#80157=ORIENTED_EDGE('',*,*,#54950,.F.);
#80158=ORIENTED_EDGE('',*,*,#56820,.F.);
#80159=ORIENTED_EDGE('',*,*,#54232,.T.);
#80160=ORIENTED_EDGE('',*,*,#54236,.F.);
#80161=ORIENTED_EDGE('',*,*,#56819,.T.);
#80162=ORIENTED_EDGE('',*,*,#52131,.F.);
#80163=ORIENTED_EDGE('',*,*,#56821,.F.);
#80164=ORIENTED_EDGE('',*,*,#56336,.F.);
#80165=ORIENTED_EDGE('',*,*,#56820,.T.);
#80166=ORIENTED_EDGE('',*,*,#54949,.F.);
#80167=ORIENTED_EDGE('',*,*,#56822,.F.);
#80168=ORIENTED_EDGE('',*,*,#54233,.F.);
#80169=ORIENTED_EDGE('',*,*,#56821,.T.);
#80170=ORIENTED_EDGE('',*,*,#52130,.F.);
#80171=ORIENTED_EDGE('',*,*,#56823,.F.);
#80172=ORIENTED_EDGE('',*,*,#54929,.F.);
#80173=ORIENTED_EDGE('',*,*,#56822,.T.);
#80174=ORIENTED_EDGE('',*,*,#54948,.F.);
#80175=ORIENTED_EDGE('',*,*,#56824,.F.);
#80176=ORIENTED_EDGE('',*,*,#54251,.F.);
#80177=ORIENTED_EDGE('',*,*,#56823,.T.);
#80178=ORIENTED_EDGE('',*,*,#52129,.F.);
#80179=ORIENTED_EDGE('',*,*,#56825,.F.);
#80180=ORIENTED_EDGE('',*,*,#56338,.F.);
#80181=ORIENTED_EDGE('',*,*,#56824,.T.);
#80182=ORIENTED_EDGE('',*,*,#54947,.F.);
#80183=ORIENTED_EDGE('',*,*,#56826,.F.);
#80184=ORIENTED_EDGE('',*,*,#52534,.F.);
#80185=ORIENTED_EDGE('',*,*,#56825,.T.);
#80186=ORIENTED_EDGE('',*,*,#52128,.F.);
#80187=ORIENTED_EDGE('',*,*,#56827,.F.);
#80188=ORIENTED_EDGE('',*,*,#54935,.F.);
#80189=ORIENTED_EDGE('',*,*,#56826,.T.);
#80190=ORIENTED_EDGE('',*,*,#56337,.F.);
#80191=ORIENTED_EDGE('',*,*,#56828,.F.);
#80192=ORIENTED_EDGE('',*,*,#52535,.F.);
#80193=ORIENTED_EDGE('',*,*,#56827,.T.);
#80194=ORIENTED_EDGE('',*,*,#54282,.F.);
#80195=ORIENTED_EDGE('',*,*,#56829,.F.);
#80196=ORIENTED_EDGE('',*,*,#54936,.F.);
#80197=ORIENTED_EDGE('',*,*,#56828,.T.);
#80198=ORIENTED_EDGE('',*,*,#54931,.F.);
#80199=ORIENTED_EDGE('',*,*,#56830,.F.);
#80200=ORIENTED_EDGE('',*,*,#52536,.F.);
#80201=ORIENTED_EDGE('',*,*,#54277,.F.);
#80202=ORIENTED_EDGE('',*,*,#54273,.T.);
#80203=ORIENTED_EDGE('',*,*,#56831,.F.);
#80204=ORIENTED_EDGE('',*,*,#54937,.F.);
#80205=ORIENTED_EDGE('',*,*,#56829,.T.);
#80206=ORIENTED_EDGE('',*,*,#56830,.T.);
#80207=ORIENTED_EDGE('',*,*,#56339,.F.);
#80208=ORIENTED_EDGE('',*,*,#56832,.F.);
#80209=ORIENTED_EDGE('',*,*,#52537,.F.);
#80210=ORIENTED_EDGE('',*,*,#56831,.T.);
#80211=ORIENTED_EDGE('',*,*,#54272,.F.);
#80212=ORIENTED_EDGE('',*,*,#56833,.F.);
#80213=ORIENTED_EDGE('',*,*,#54938,.F.);
#80214=ORIENTED_EDGE('',*,*,#56832,.T.);
#80215=ORIENTED_EDGE('',*,*,#54933,.F.);
#80216=ORIENTED_EDGE('',*,*,#56834,.F.);
#80217=ORIENTED_EDGE('',*,*,#52538,.F.);
#80218=ORIENTED_EDGE('',*,*,#56833,.T.);
#80219=ORIENTED_EDGE('',*,*,#54284,.F.);
#80220=ORIENTED_EDGE('',*,*,#56835,.F.);
#80221=ORIENTED_EDGE('',*,*,#54939,.F.);
#80222=ORIENTED_EDGE('',*,*,#56834,.T.);
#80223=ORIENTED_EDGE('',*,*,#54932,.F.);
#80224=ORIENTED_EDGE('',*,*,#56836,.F.);
#80225=ORIENTED_EDGE('',*,*,#54280,.F.);
#80226=ORIENTED_EDGE('',*,*,#56835,.T.);
#80227=ORIENTED_EDGE('',*,*,#54268,.F.);
#80228=ORIENTED_EDGE('',*,*,#56837,.F.);
#80229=ORIENTED_EDGE('',*,*,#54940,.F.);
#80230=ORIENTED_EDGE('',*,*,#56836,.T.);
#80231=ORIENTED_EDGE('',*,*,#54943,.F.);
#80232=ORIENTED_EDGE('',*,*,#56838,.F.);
#80233=ORIENTED_EDGE('',*,*,#54259,.F.);
#80234=ORIENTED_EDGE('',*,*,#56837,.T.);
#80235=ORIENTED_EDGE('',*,*,#54286,.F.);
#80236=ORIENTED_EDGE('',*,*,#56839,.F.);
#80237=ORIENTED_EDGE('',*,*,#54941,.F.);
#80238=ORIENTED_EDGE('',*,*,#56838,.T.);
#80239=ORIENTED_EDGE('',*,*,#54942,.F.);
#80240=ORIENTED_EDGE('',*,*,#56839,.T.);
#80241=ORIENTED_EDGE('',*,*,#54264,.F.);
#80242=ORIENTED_EDGE('',*,*,#54260,.T.);
#80243=ORIENTED_EDGE('',*,*,#56840,.F.);
#80244=ORIENTED_EDGE('',*,*,#54982,.F.);
#80245=ORIENTED_EDGE('',*,*,#56841,.F.);
#80246=ORIENTED_EDGE('',*,*,#54216,.F.);
#80247=ORIENTED_EDGE('',*,*,#56841,.T.);
#80248=ORIENTED_EDGE('',*,*,#54981,.F.);
#80249=ORIENTED_EDGE('',*,*,#56842,.F.);
#80250=ORIENTED_EDGE('',*,*,#54225,.F.);
#80251=ORIENTED_EDGE('',*,*,#54215,.T.);
#80252=ORIENTED_EDGE('',*,*,#54219,.F.);
#80253=ORIENTED_EDGE('',*,*,#56843,.F.);
#80254=ORIENTED_EDGE('',*,*,#54983,.F.);
#80255=ORIENTED_EDGE('',*,*,#56840,.T.);
#80256=ORIENTED_EDGE('',*,*,#56842,.T.);
#80257=ORIENTED_EDGE('',*,*,#54980,.F.);
#80258=ORIENTED_EDGE('',*,*,#56844,.F.);
#80259=ORIENTED_EDGE('',*,*,#54210,.F.);
#80260=ORIENTED_EDGE('',*,*,#56843,.T.);
#80261=ORIENTED_EDGE('',*,*,#54223,.F.);
#80262=ORIENTED_EDGE('',*,*,#56845,.F.);
#80263=ORIENTED_EDGE('',*,*,#54972,.F.);
#80264=ORIENTED_EDGE('',*,*,#56844,.T.);
#80265=ORIENTED_EDGE('',*,*,#54979,.F.);
#80266=ORIENTED_EDGE('',*,*,#56846,.F.);
#80267=ORIENTED_EDGE('',*,*,#54227,.F.);
#80268=ORIENTED_EDGE('',*,*,#56845,.T.);
#80269=ORIENTED_EDGE('',*,*,#52138,.F.);
#80270=ORIENTED_EDGE('',*,*,#56847,.F.);
#80271=ORIENTED_EDGE('',*,*,#54973,.F.);
#80272=ORIENTED_EDGE('',*,*,#56846,.T.);
#80273=ORIENTED_EDGE('',*,*,#54978,.F.);
#80274=ORIENTED_EDGE('',*,*,#56848,.F.);
#80275=ORIENTED_EDGE('',*,*,#54202,.T.);
#80276=ORIENTED_EDGE('',*,*,#54206,.F.);
#80277=ORIENTED_EDGE('',*,*,#56847,.T.);
#80278=ORIENTED_EDGE('',*,*,#52137,.F.);
#80279=ORIENTED_EDGE('',*,*,#56849,.F.);
#80280=ORIENTED_EDGE('',*,*,#56340,.F.);
#80281=ORIENTED_EDGE('',*,*,#56848,.T.);
#80282=ORIENTED_EDGE('',*,*,#54977,.F.);
#80283=ORIENTED_EDGE('',*,*,#56850,.F.);
#80284=ORIENTED_EDGE('',*,*,#54203,.F.);
#80285=ORIENTED_EDGE('',*,*,#56849,.T.);
#80286=ORIENTED_EDGE('',*,*,#52136,.F.);
#80287=ORIENTED_EDGE('',*,*,#56851,.F.);
#80288=ORIENTED_EDGE('',*,*,#54957,.F.);
#80289=ORIENTED_EDGE('',*,*,#56850,.T.);
#80290=ORIENTED_EDGE('',*,*,#54976,.F.);
#80291=ORIENTED_EDGE('',*,*,#56852,.F.);
#80292=ORIENTED_EDGE('',*,*,#54221,.F.);
#80293=ORIENTED_EDGE('',*,*,#56851,.T.);
#80294=ORIENTED_EDGE('',*,*,#52135,.F.);
#80295=ORIENTED_EDGE('',*,*,#56853,.F.);
#80296=ORIENTED_EDGE('',*,*,#56342,.F.);
#80297=ORIENTED_EDGE('',*,*,#56852,.T.);
#80298=ORIENTED_EDGE('',*,*,#54975,.F.);
#80299=ORIENTED_EDGE('',*,*,#56854,.F.);
#80300=ORIENTED_EDGE('',*,*,#52528,.F.);
#80301=ORIENTED_EDGE('',*,*,#56853,.T.);
#80302=ORIENTED_EDGE('',*,*,#52134,.F.);
#80303=ORIENTED_EDGE('',*,*,#56855,.F.);
#80304=ORIENTED_EDGE('',*,*,#54963,.F.);
#80305=ORIENTED_EDGE('',*,*,#56854,.T.);
#80306=ORIENTED_EDGE('',*,*,#56341,.F.);
#80307=ORIENTED_EDGE('',*,*,#56856,.F.);
#80308=ORIENTED_EDGE('',*,*,#52529,.F.);
#80309=ORIENTED_EDGE('',*,*,#56855,.T.);
#80310=ORIENTED_EDGE('',*,*,#54252,.F.);
#80311=ORIENTED_EDGE('',*,*,#56857,.F.);
#80312=ORIENTED_EDGE('',*,*,#54964,.F.);
#80313=ORIENTED_EDGE('',*,*,#56856,.T.);
#80314=ORIENTED_EDGE('',*,*,#54959,.F.);
#80315=ORIENTED_EDGE('',*,*,#56858,.F.);
#80316=ORIENTED_EDGE('',*,*,#52530,.F.);
#80317=ORIENTED_EDGE('',*,*,#54247,.F.);
#80318=ORIENTED_EDGE('',*,*,#54243,.T.);
#80319=ORIENTED_EDGE('',*,*,#56859,.F.);
#80320=ORIENTED_EDGE('',*,*,#54965,.F.);
#80321=ORIENTED_EDGE('',*,*,#56857,.T.);
#80322=ORIENTED_EDGE('',*,*,#56858,.T.);
#80323=ORIENTED_EDGE('',*,*,#56343,.F.);
#80324=ORIENTED_EDGE('',*,*,#56860,.F.);
#80325=ORIENTED_EDGE('',*,*,#52531,.F.);
#80326=ORIENTED_EDGE('',*,*,#56859,.T.);
#80327=ORIENTED_EDGE('',*,*,#54242,.F.);
#80328=ORIENTED_EDGE('',*,*,#56861,.F.);
#80329=ORIENTED_EDGE('',*,*,#54966,.F.);
#80330=ORIENTED_EDGE('',*,*,#56860,.T.);
#80331=ORIENTED_EDGE('',*,*,#54961,.F.);
#80332=ORIENTED_EDGE('',*,*,#56862,.F.);
#80333=ORIENTED_EDGE('',*,*,#52532,.F.);
#80334=ORIENTED_EDGE('',*,*,#56861,.T.);
#80335=ORIENTED_EDGE('',*,*,#54254,.F.);
#80336=ORIENTED_EDGE('',*,*,#56863,.F.);
#80337=ORIENTED_EDGE('',*,*,#54967,.F.);
#80338=ORIENTED_EDGE('',*,*,#56862,.T.);
#80339=ORIENTED_EDGE('',*,*,#54960,.F.);
#80340=ORIENTED_EDGE('',*,*,#56864,.F.);
#80341=ORIENTED_EDGE('',*,*,#54250,.F.);
#80342=ORIENTED_EDGE('',*,*,#56863,.T.);
#80343=ORIENTED_EDGE('',*,*,#54238,.F.);
#80344=ORIENTED_EDGE('',*,*,#56865,.F.);
#80345=ORIENTED_EDGE('',*,*,#54968,.F.);
#80346=ORIENTED_EDGE('',*,*,#56864,.T.);
#80347=ORIENTED_EDGE('',*,*,#54971,.F.);
#80348=ORIENTED_EDGE('',*,*,#56866,.F.);
#80349=ORIENTED_EDGE('',*,*,#54229,.F.);
#80350=ORIENTED_EDGE('',*,*,#56865,.T.);
#80351=ORIENTED_EDGE('',*,*,#54256,.F.);
#80352=ORIENTED_EDGE('',*,*,#56867,.F.);
#80353=ORIENTED_EDGE('',*,*,#54969,.F.);
#80354=ORIENTED_EDGE('',*,*,#56866,.T.);
#80355=ORIENTED_EDGE('',*,*,#54970,.F.);
#80356=ORIENTED_EDGE('',*,*,#56867,.T.);
#80357=ORIENTED_EDGE('',*,*,#54234,.F.);
#80358=ORIENTED_EDGE('',*,*,#54230,.T.);
#80359=ORIENTED_EDGE('',*,*,#56868,.F.);
#80360=ORIENTED_EDGE('',*,*,#55010,.F.);
#80361=ORIENTED_EDGE('',*,*,#56869,.F.);
#80362=ORIENTED_EDGE('',*,*,#54186,.F.);
#80363=ORIENTED_EDGE('',*,*,#56869,.T.);
#80364=ORIENTED_EDGE('',*,*,#55009,.F.);
#80365=ORIENTED_EDGE('',*,*,#56870,.F.);
#80366=ORIENTED_EDGE('',*,*,#54195,.F.);
#80367=ORIENTED_EDGE('',*,*,#54185,.T.);
#80368=ORIENTED_EDGE('',*,*,#54189,.F.);
#80369=ORIENTED_EDGE('',*,*,#56871,.F.);
#80370=ORIENTED_EDGE('',*,*,#55011,.F.);
#80371=ORIENTED_EDGE('',*,*,#56868,.T.);
#80372=ORIENTED_EDGE('',*,*,#56870,.T.);
#80373=ORIENTED_EDGE('',*,*,#55008,.F.);
#80374=ORIENTED_EDGE('',*,*,#56872,.F.);
#80375=ORIENTED_EDGE('',*,*,#54180,.F.);
#80376=ORIENTED_EDGE('',*,*,#56871,.T.);
#80377=ORIENTED_EDGE('',*,*,#54193,.F.);
#80378=ORIENTED_EDGE('',*,*,#56873,.F.);
#80379=ORIENTED_EDGE('',*,*,#55000,.F.);
#80380=ORIENTED_EDGE('',*,*,#56872,.T.);
#80381=ORIENTED_EDGE('',*,*,#55007,.F.);
#80382=ORIENTED_EDGE('',*,*,#56874,.F.);
#80383=ORIENTED_EDGE('',*,*,#54197,.F.);
#80384=ORIENTED_EDGE('',*,*,#56873,.T.);
#80385=ORIENTED_EDGE('',*,*,#52144,.F.);
#80386=ORIENTED_EDGE('',*,*,#56875,.F.);
#80387=ORIENTED_EDGE('',*,*,#55001,.F.);
#80388=ORIENTED_EDGE('',*,*,#56874,.T.);
#80389=ORIENTED_EDGE('',*,*,#55006,.F.);
#80390=ORIENTED_EDGE('',*,*,#56876,.F.);
#80391=ORIENTED_EDGE('',*,*,#54172,.T.);
#80392=ORIENTED_EDGE('',*,*,#54176,.F.);
#80393=ORIENTED_EDGE('',*,*,#56875,.T.);
#80394=ORIENTED_EDGE('',*,*,#52143,.F.);
#80395=ORIENTED_EDGE('',*,*,#56877,.F.);
#80396=ORIENTED_EDGE('',*,*,#56344,.F.);
#80397=ORIENTED_EDGE('',*,*,#56876,.T.);
#80398=ORIENTED_EDGE('',*,*,#55005,.F.);
#80399=ORIENTED_EDGE('',*,*,#56878,.F.);
#80400=ORIENTED_EDGE('',*,*,#54173,.F.);
#80401=ORIENTED_EDGE('',*,*,#56877,.T.);
#80402=ORIENTED_EDGE('',*,*,#52142,.F.);
#80403=ORIENTED_EDGE('',*,*,#56879,.F.);
#80404=ORIENTED_EDGE('',*,*,#54985,.F.);
#80405=ORIENTED_EDGE('',*,*,#56878,.T.);
#80406=ORIENTED_EDGE('',*,*,#55004,.F.);
#80407=ORIENTED_EDGE('',*,*,#56880,.F.);
#80408=ORIENTED_EDGE('',*,*,#54191,.F.);
#80409=ORIENTED_EDGE('',*,*,#56879,.T.);
#80410=ORIENTED_EDGE('',*,*,#52141,.F.);
#80411=ORIENTED_EDGE('',*,*,#56881,.F.);
#80412=ORIENTED_EDGE('',*,*,#56346,.F.);
#80413=ORIENTED_EDGE('',*,*,#56880,.T.);
#80414=ORIENTED_EDGE('',*,*,#55003,.F.);
#80415=ORIENTED_EDGE('',*,*,#56882,.F.);
#80416=ORIENTED_EDGE('',*,*,#52522,.F.);
#80417=ORIENTED_EDGE('',*,*,#56881,.T.);
#80418=ORIENTED_EDGE('',*,*,#52140,.F.);
#80419=ORIENTED_EDGE('',*,*,#56883,.F.);
#80420=ORIENTED_EDGE('',*,*,#54991,.F.);
#80421=ORIENTED_EDGE('',*,*,#56882,.T.);
#80422=ORIENTED_EDGE('',*,*,#56345,.F.);
#80423=ORIENTED_EDGE('',*,*,#56884,.F.);
#80424=ORIENTED_EDGE('',*,*,#52523,.F.);
#80425=ORIENTED_EDGE('',*,*,#56883,.T.);
#80426=ORIENTED_EDGE('',*,*,#54222,.F.);
#80427=ORIENTED_EDGE('',*,*,#56885,.F.);
#80428=ORIENTED_EDGE('',*,*,#54992,.F.);
#80429=ORIENTED_EDGE('',*,*,#56884,.T.);
#80430=ORIENTED_EDGE('',*,*,#54987,.F.);
#80431=ORIENTED_EDGE('',*,*,#56886,.F.);
#80432=ORIENTED_EDGE('',*,*,#52524,.F.);
#80433=ORIENTED_EDGE('',*,*,#54217,.F.);
#80434=ORIENTED_EDGE('',*,*,#54213,.T.);
#80435=ORIENTED_EDGE('',*,*,#56887,.F.);
#80436=ORIENTED_EDGE('',*,*,#54993,.F.);
#80437=ORIENTED_EDGE('',*,*,#56885,.T.);
#80438=ORIENTED_EDGE('',*,*,#56886,.T.);
#80439=ORIENTED_EDGE('',*,*,#56347,.F.);
#80440=ORIENTED_EDGE('',*,*,#56888,.F.);
#80441=ORIENTED_EDGE('',*,*,#52525,.F.);
#80442=ORIENTED_EDGE('',*,*,#56887,.T.);
#80443=ORIENTED_EDGE('',*,*,#54212,.F.);
#80444=ORIENTED_EDGE('',*,*,#56889,.F.);
#80445=ORIENTED_EDGE('',*,*,#54994,.F.);
#80446=ORIENTED_EDGE('',*,*,#56888,.T.);
#80447=ORIENTED_EDGE('',*,*,#54989,.F.);
#80448=ORIENTED_EDGE('',*,*,#56890,.F.);
#80449=ORIENTED_EDGE('',*,*,#52526,.F.);
#80450=ORIENTED_EDGE('',*,*,#56889,.T.);
#80451=ORIENTED_EDGE('',*,*,#54224,.F.);
#80452=ORIENTED_EDGE('',*,*,#56891,.F.);
#80453=ORIENTED_EDGE('',*,*,#54995,.F.);
#80454=ORIENTED_EDGE('',*,*,#56890,.T.);
#80455=ORIENTED_EDGE('',*,*,#54988,.F.);
#80456=ORIENTED_EDGE('',*,*,#56892,.F.);
#80457=ORIENTED_EDGE('',*,*,#54220,.F.);
#80458=ORIENTED_EDGE('',*,*,#56891,.T.);
#80459=ORIENTED_EDGE('',*,*,#54208,.F.);
#80460=ORIENTED_EDGE('',*,*,#56893,.F.);
#80461=ORIENTED_EDGE('',*,*,#54996,.F.);
#80462=ORIENTED_EDGE('',*,*,#56892,.T.);
#80463=ORIENTED_EDGE('',*,*,#54999,.F.);
#80464=ORIENTED_EDGE('',*,*,#56894,.F.);
#80465=ORIENTED_EDGE('',*,*,#54199,.F.);
#80466=ORIENTED_EDGE('',*,*,#56893,.T.);
#80467=ORIENTED_EDGE('',*,*,#54226,.F.);
#80468=ORIENTED_EDGE('',*,*,#56895,.F.);
#80469=ORIENTED_EDGE('',*,*,#54997,.F.);
#80470=ORIENTED_EDGE('',*,*,#56894,.T.);
#80471=ORIENTED_EDGE('',*,*,#54998,.F.);
#80472=ORIENTED_EDGE('',*,*,#56895,.T.);
#80473=ORIENTED_EDGE('',*,*,#54204,.F.);
#80474=ORIENTED_EDGE('',*,*,#54200,.T.);
#80475=ORIENTED_EDGE('',*,*,#56896,.F.);
#80476=ORIENTED_EDGE('',*,*,#55038,.F.);
#80477=ORIENTED_EDGE('',*,*,#56897,.F.);
#80478=ORIENTED_EDGE('',*,*,#54156,.F.);
#80479=ORIENTED_EDGE('',*,*,#56897,.T.);
#80480=ORIENTED_EDGE('',*,*,#55037,.F.);
#80481=ORIENTED_EDGE('',*,*,#56898,.F.);
#80482=ORIENTED_EDGE('',*,*,#54165,.F.);
#80483=ORIENTED_EDGE('',*,*,#54155,.T.);
#80484=ORIENTED_EDGE('',*,*,#54159,.F.);
#80485=ORIENTED_EDGE('',*,*,#56899,.F.);
#80486=ORIENTED_EDGE('',*,*,#55039,.F.);
#80487=ORIENTED_EDGE('',*,*,#56896,.T.);
#80488=ORIENTED_EDGE('',*,*,#56898,.T.);
#80489=ORIENTED_EDGE('',*,*,#55036,.F.);
#80490=ORIENTED_EDGE('',*,*,#56900,.F.);
#80491=ORIENTED_EDGE('',*,*,#54150,.F.);
#80492=ORIENTED_EDGE('',*,*,#56899,.T.);
#80493=ORIENTED_EDGE('',*,*,#54163,.F.);
#80494=ORIENTED_EDGE('',*,*,#56901,.F.);
#80495=ORIENTED_EDGE('',*,*,#55028,.F.);
#80496=ORIENTED_EDGE('',*,*,#56900,.T.);
#80497=ORIENTED_EDGE('',*,*,#55035,.F.);
#80498=ORIENTED_EDGE('',*,*,#56902,.F.);
#80499=ORIENTED_EDGE('',*,*,#54167,.F.);
#80500=ORIENTED_EDGE('',*,*,#56901,.T.);
#80501=ORIENTED_EDGE('',*,*,#52150,.F.);
#80502=ORIENTED_EDGE('',*,*,#56903,.F.);
#80503=ORIENTED_EDGE('',*,*,#55029,.F.);
#80504=ORIENTED_EDGE('',*,*,#56902,.T.);
#80505=ORIENTED_EDGE('',*,*,#55034,.F.);
#80506=ORIENTED_EDGE('',*,*,#56904,.F.);
#80507=ORIENTED_EDGE('',*,*,#54142,.T.);
#80508=ORIENTED_EDGE('',*,*,#54146,.F.);
#80509=ORIENTED_EDGE('',*,*,#56903,.T.);
#80510=ORIENTED_EDGE('',*,*,#52149,.F.);
#80511=ORIENTED_EDGE('',*,*,#56905,.F.);
#80512=ORIENTED_EDGE('',*,*,#56348,.F.);
#80513=ORIENTED_EDGE('',*,*,#56904,.T.);
#80514=ORIENTED_EDGE('',*,*,#55033,.F.);
#80515=ORIENTED_EDGE('',*,*,#56906,.F.);
#80516=ORIENTED_EDGE('',*,*,#54143,.F.);
#80517=ORIENTED_EDGE('',*,*,#56905,.T.);
#80518=ORIENTED_EDGE('',*,*,#52148,.F.);
#80519=ORIENTED_EDGE('',*,*,#56907,.F.);
#80520=ORIENTED_EDGE('',*,*,#55013,.F.);
#80521=ORIENTED_EDGE('',*,*,#56906,.T.);
#80522=ORIENTED_EDGE('',*,*,#55032,.F.);
#80523=ORIENTED_EDGE('',*,*,#56908,.F.);
#80524=ORIENTED_EDGE('',*,*,#54161,.F.);
#80525=ORIENTED_EDGE('',*,*,#56907,.T.);
#80526=ORIENTED_EDGE('',*,*,#52147,.F.);
#80527=ORIENTED_EDGE('',*,*,#56909,.F.);
#80528=ORIENTED_EDGE('',*,*,#56350,.F.);
#80529=ORIENTED_EDGE('',*,*,#56908,.T.);
#80530=ORIENTED_EDGE('',*,*,#55031,.F.);
#80531=ORIENTED_EDGE('',*,*,#56910,.F.);
#80532=ORIENTED_EDGE('',*,*,#52516,.F.);
#80533=ORIENTED_EDGE('',*,*,#56909,.T.);
#80534=ORIENTED_EDGE('',*,*,#52146,.F.);
#80535=ORIENTED_EDGE('',*,*,#56911,.F.);
#80536=ORIENTED_EDGE('',*,*,#55019,.F.);
#80537=ORIENTED_EDGE('',*,*,#56910,.T.);
#80538=ORIENTED_EDGE('',*,*,#56349,.F.);
#80539=ORIENTED_EDGE('',*,*,#56912,.F.);
#80540=ORIENTED_EDGE('',*,*,#52517,.F.);
#80541=ORIENTED_EDGE('',*,*,#56911,.T.);
#80542=ORIENTED_EDGE('',*,*,#54192,.F.);
#80543=ORIENTED_EDGE('',*,*,#56913,.F.);
#80544=ORIENTED_EDGE('',*,*,#55020,.F.);
#80545=ORIENTED_EDGE('',*,*,#56912,.T.);
#80546=ORIENTED_EDGE('',*,*,#55015,.F.);
#80547=ORIENTED_EDGE('',*,*,#56914,.F.);
#80548=ORIENTED_EDGE('',*,*,#52518,.F.);
#80549=ORIENTED_EDGE('',*,*,#54187,.F.);
#80550=ORIENTED_EDGE('',*,*,#54183,.T.);
#80551=ORIENTED_EDGE('',*,*,#56915,.F.);
#80552=ORIENTED_EDGE('',*,*,#55021,.F.);
#80553=ORIENTED_EDGE('',*,*,#56913,.T.);
#80554=ORIENTED_EDGE('',*,*,#56914,.T.);
#80555=ORIENTED_EDGE('',*,*,#56351,.F.);
#80556=ORIENTED_EDGE('',*,*,#56916,.F.);
#80557=ORIENTED_EDGE('',*,*,#52519,.F.);
#80558=ORIENTED_EDGE('',*,*,#56915,.T.);
#80559=ORIENTED_EDGE('',*,*,#54182,.F.);
#80560=ORIENTED_EDGE('',*,*,#56917,.F.);
#80561=ORIENTED_EDGE('',*,*,#55022,.F.);
#80562=ORIENTED_EDGE('',*,*,#56916,.T.);
#80563=ORIENTED_EDGE('',*,*,#55017,.F.);
#80564=ORIENTED_EDGE('',*,*,#56918,.F.);
#80565=ORIENTED_EDGE('',*,*,#52520,.F.);
#80566=ORIENTED_EDGE('',*,*,#56917,.T.);
#80567=ORIENTED_EDGE('',*,*,#54194,.F.);
#80568=ORIENTED_EDGE('',*,*,#56919,.F.);
#80569=ORIENTED_EDGE('',*,*,#55023,.F.);
#80570=ORIENTED_EDGE('',*,*,#56918,.T.);
#80571=ORIENTED_EDGE('',*,*,#55016,.F.);
#80572=ORIENTED_EDGE('',*,*,#56920,.F.);
#80573=ORIENTED_EDGE('',*,*,#54190,.F.);
#80574=ORIENTED_EDGE('',*,*,#56919,.T.);
#80575=ORIENTED_EDGE('',*,*,#54178,.F.);
#80576=ORIENTED_EDGE('',*,*,#56921,.F.);
#80577=ORIENTED_EDGE('',*,*,#55024,.F.);
#80578=ORIENTED_EDGE('',*,*,#56920,.T.);
#80579=ORIENTED_EDGE('',*,*,#55027,.F.);
#80580=ORIENTED_EDGE('',*,*,#56922,.F.);
#80581=ORIENTED_EDGE('',*,*,#54169,.F.);
#80582=ORIENTED_EDGE('',*,*,#56921,.T.);
#80583=ORIENTED_EDGE('',*,*,#54196,.F.);
#80584=ORIENTED_EDGE('',*,*,#56923,.F.);
#80585=ORIENTED_EDGE('',*,*,#55025,.F.);
#80586=ORIENTED_EDGE('',*,*,#56922,.T.);
#80587=ORIENTED_EDGE('',*,*,#55026,.F.);
#80588=ORIENTED_EDGE('',*,*,#56923,.T.);
#80589=ORIENTED_EDGE('',*,*,#54174,.F.);
#80590=ORIENTED_EDGE('',*,*,#54170,.T.);
#80591=ORIENTED_EDGE('',*,*,#56924,.F.);
#80592=ORIENTED_EDGE('',*,*,#55066,.F.);
#80593=ORIENTED_EDGE('',*,*,#56925,.F.);
#80594=ORIENTED_EDGE('',*,*,#54126,.F.);
#80595=ORIENTED_EDGE('',*,*,#56925,.T.);
#80596=ORIENTED_EDGE('',*,*,#55065,.F.);
#80597=ORIENTED_EDGE('',*,*,#56926,.F.);
#80598=ORIENTED_EDGE('',*,*,#54135,.F.);
#80599=ORIENTED_EDGE('',*,*,#54125,.T.);
#80600=ORIENTED_EDGE('',*,*,#54129,.F.);
#80601=ORIENTED_EDGE('',*,*,#56927,.F.);
#80602=ORIENTED_EDGE('',*,*,#55067,.F.);
#80603=ORIENTED_EDGE('',*,*,#56924,.T.);
#80604=ORIENTED_EDGE('',*,*,#56926,.T.);
#80605=ORIENTED_EDGE('',*,*,#55064,.F.);
#80606=ORIENTED_EDGE('',*,*,#56928,.F.);
#80607=ORIENTED_EDGE('',*,*,#54120,.F.);
#80608=ORIENTED_EDGE('',*,*,#56927,.T.);
#80609=ORIENTED_EDGE('',*,*,#54133,.F.);
#80610=ORIENTED_EDGE('',*,*,#56929,.F.);
#80611=ORIENTED_EDGE('',*,*,#55056,.F.);
#80612=ORIENTED_EDGE('',*,*,#56928,.T.);
#80613=ORIENTED_EDGE('',*,*,#55063,.F.);
#80614=ORIENTED_EDGE('',*,*,#56930,.F.);
#80615=ORIENTED_EDGE('',*,*,#54137,.F.);
#80616=ORIENTED_EDGE('',*,*,#56929,.T.);
#80617=ORIENTED_EDGE('',*,*,#52156,.F.);
#80618=ORIENTED_EDGE('',*,*,#56931,.F.);
#80619=ORIENTED_EDGE('',*,*,#55057,.F.);
#80620=ORIENTED_EDGE('',*,*,#56930,.T.);
#80621=ORIENTED_EDGE('',*,*,#55062,.F.);
#80622=ORIENTED_EDGE('',*,*,#56932,.F.);
#80623=ORIENTED_EDGE('',*,*,#54112,.T.);
#80624=ORIENTED_EDGE('',*,*,#54116,.F.);
#80625=ORIENTED_EDGE('',*,*,#56931,.T.);
#80626=ORIENTED_EDGE('',*,*,#52155,.F.);
#80627=ORIENTED_EDGE('',*,*,#56933,.F.);
#80628=ORIENTED_EDGE('',*,*,#56352,.F.);
#80629=ORIENTED_EDGE('',*,*,#56932,.T.);
#80630=ORIENTED_EDGE('',*,*,#55061,.F.);
#80631=ORIENTED_EDGE('',*,*,#56934,.F.);
#80632=ORIENTED_EDGE('',*,*,#54113,.F.);
#80633=ORIENTED_EDGE('',*,*,#56933,.T.);
#80634=ORIENTED_EDGE('',*,*,#52154,.F.);
#80635=ORIENTED_EDGE('',*,*,#56935,.F.);
#80636=ORIENTED_EDGE('',*,*,#55041,.F.);
#80637=ORIENTED_EDGE('',*,*,#56934,.T.);
#80638=ORIENTED_EDGE('',*,*,#55060,.F.);
#80639=ORIENTED_EDGE('',*,*,#56936,.F.);
#80640=ORIENTED_EDGE('',*,*,#54131,.F.);
#80641=ORIENTED_EDGE('',*,*,#56935,.T.);
#80642=ORIENTED_EDGE('',*,*,#52153,.F.);
#80643=ORIENTED_EDGE('',*,*,#56937,.F.);
#80644=ORIENTED_EDGE('',*,*,#56354,.F.);
#80645=ORIENTED_EDGE('',*,*,#56936,.T.);
#80646=ORIENTED_EDGE('',*,*,#55059,.F.);
#80647=ORIENTED_EDGE('',*,*,#56938,.F.);
#80648=ORIENTED_EDGE('',*,*,#52510,.F.);
#80649=ORIENTED_EDGE('',*,*,#56937,.T.);
#80650=ORIENTED_EDGE('',*,*,#52152,.F.);
#80651=ORIENTED_EDGE('',*,*,#56939,.F.);
#80652=ORIENTED_EDGE('',*,*,#55047,.F.);
#80653=ORIENTED_EDGE('',*,*,#56938,.T.);
#80654=ORIENTED_EDGE('',*,*,#56353,.F.);
#80655=ORIENTED_EDGE('',*,*,#56940,.F.);
#80656=ORIENTED_EDGE('',*,*,#52511,.F.);
#80657=ORIENTED_EDGE('',*,*,#56939,.T.);
#80658=ORIENTED_EDGE('',*,*,#54162,.F.);
#80659=ORIENTED_EDGE('',*,*,#56941,.F.);
#80660=ORIENTED_EDGE('',*,*,#55048,.F.);
#80661=ORIENTED_EDGE('',*,*,#56940,.T.);
#80662=ORIENTED_EDGE('',*,*,#55043,.F.);
#80663=ORIENTED_EDGE('',*,*,#56942,.F.);
#80664=ORIENTED_EDGE('',*,*,#52512,.F.);
#80665=ORIENTED_EDGE('',*,*,#54157,.F.);
#80666=ORIENTED_EDGE('',*,*,#54153,.T.);
#80667=ORIENTED_EDGE('',*,*,#56943,.F.);
#80668=ORIENTED_EDGE('',*,*,#55049,.F.);
#80669=ORIENTED_EDGE('',*,*,#56941,.T.);
#80670=ORIENTED_EDGE('',*,*,#56942,.T.);
#80671=ORIENTED_EDGE('',*,*,#56355,.F.);
#80672=ORIENTED_EDGE('',*,*,#56944,.F.);
#80673=ORIENTED_EDGE('',*,*,#52513,.F.);
#80674=ORIENTED_EDGE('',*,*,#56943,.T.);
#80675=ORIENTED_EDGE('',*,*,#54152,.F.);
#80676=ORIENTED_EDGE('',*,*,#56945,.F.);
#80677=ORIENTED_EDGE('',*,*,#55050,.F.);
#80678=ORIENTED_EDGE('',*,*,#56944,.T.);
#80679=ORIENTED_EDGE('',*,*,#55045,.F.);
#80680=ORIENTED_EDGE('',*,*,#56946,.F.);
#80681=ORIENTED_EDGE('',*,*,#52514,.F.);
#80682=ORIENTED_EDGE('',*,*,#56945,.T.);
#80683=ORIENTED_EDGE('',*,*,#54164,.F.);
#80684=ORIENTED_EDGE('',*,*,#56947,.F.);
#80685=ORIENTED_EDGE('',*,*,#55051,.F.);
#80686=ORIENTED_EDGE('',*,*,#56946,.T.);
#80687=ORIENTED_EDGE('',*,*,#55044,.F.);
#80688=ORIENTED_EDGE('',*,*,#56948,.F.);
#80689=ORIENTED_EDGE('',*,*,#54160,.F.);
#80690=ORIENTED_EDGE('',*,*,#56947,.T.);
#80691=ORIENTED_EDGE('',*,*,#54148,.F.);
#80692=ORIENTED_EDGE('',*,*,#56949,.F.);
#80693=ORIENTED_EDGE('',*,*,#55052,.F.);
#80694=ORIENTED_EDGE('',*,*,#56948,.T.);
#80695=ORIENTED_EDGE('',*,*,#55055,.F.);
#80696=ORIENTED_EDGE('',*,*,#56950,.F.);
#80697=ORIENTED_EDGE('',*,*,#54139,.F.);
#80698=ORIENTED_EDGE('',*,*,#56949,.T.);
#80699=ORIENTED_EDGE('',*,*,#54166,.F.);
#80700=ORIENTED_EDGE('',*,*,#56951,.F.);
#80701=ORIENTED_EDGE('',*,*,#55053,.F.);
#80702=ORIENTED_EDGE('',*,*,#56950,.T.);
#80703=ORIENTED_EDGE('',*,*,#55054,.F.);
#80704=ORIENTED_EDGE('',*,*,#56951,.T.);
#80705=ORIENTED_EDGE('',*,*,#54144,.F.);
#80706=ORIENTED_EDGE('',*,*,#54140,.T.);
#80707=ORIENTED_EDGE('',*,*,#56952,.F.);
#80708=ORIENTED_EDGE('',*,*,#55094,.F.);
#80709=ORIENTED_EDGE('',*,*,#56953,.F.);
#80710=ORIENTED_EDGE('',*,*,#54096,.F.);
#80711=ORIENTED_EDGE('',*,*,#56953,.T.);
#80712=ORIENTED_EDGE('',*,*,#55093,.F.);
#80713=ORIENTED_EDGE('',*,*,#56954,.F.);
#80714=ORIENTED_EDGE('',*,*,#54105,.F.);
#80715=ORIENTED_EDGE('',*,*,#54095,.T.);
#80716=ORIENTED_EDGE('',*,*,#54099,.F.);
#80717=ORIENTED_EDGE('',*,*,#56955,.F.);
#80718=ORIENTED_EDGE('',*,*,#55095,.F.);
#80719=ORIENTED_EDGE('',*,*,#56952,.T.);
#80720=ORIENTED_EDGE('',*,*,#56954,.T.);
#80721=ORIENTED_EDGE('',*,*,#55092,.F.);
#80722=ORIENTED_EDGE('',*,*,#56956,.F.);
#80723=ORIENTED_EDGE('',*,*,#54090,.F.);
#80724=ORIENTED_EDGE('',*,*,#56955,.T.);
#80725=ORIENTED_EDGE('',*,*,#54103,.F.);
#80726=ORIENTED_EDGE('',*,*,#56957,.F.);
#80727=ORIENTED_EDGE('',*,*,#55084,.F.);
#80728=ORIENTED_EDGE('',*,*,#56956,.T.);
#80729=ORIENTED_EDGE('',*,*,#55091,.F.);
#80730=ORIENTED_EDGE('',*,*,#56958,.F.);
#80731=ORIENTED_EDGE('',*,*,#54107,.F.);
#80732=ORIENTED_EDGE('',*,*,#56957,.T.);
#80733=ORIENTED_EDGE('',*,*,#52162,.F.);
#80734=ORIENTED_EDGE('',*,*,#56959,.F.);
#80735=ORIENTED_EDGE('',*,*,#55085,.F.);
#80736=ORIENTED_EDGE('',*,*,#56958,.T.);
#80737=ORIENTED_EDGE('',*,*,#55090,.F.);
#80738=ORIENTED_EDGE('',*,*,#56960,.F.);
#80739=ORIENTED_EDGE('',*,*,#54082,.T.);
#80740=ORIENTED_EDGE('',*,*,#54086,.F.);
#80741=ORIENTED_EDGE('',*,*,#56959,.T.);
#80742=ORIENTED_EDGE('',*,*,#52161,.F.);
#80743=ORIENTED_EDGE('',*,*,#56961,.F.);
#80744=ORIENTED_EDGE('',*,*,#56356,.F.);
#80745=ORIENTED_EDGE('',*,*,#56960,.T.);
#80746=ORIENTED_EDGE('',*,*,#55089,.F.);
#80747=ORIENTED_EDGE('',*,*,#56962,.F.);
#80748=ORIENTED_EDGE('',*,*,#54083,.F.);
#80749=ORIENTED_EDGE('',*,*,#56961,.T.);
#80750=ORIENTED_EDGE('',*,*,#52160,.F.);
#80751=ORIENTED_EDGE('',*,*,#56963,.F.);
#80752=ORIENTED_EDGE('',*,*,#55069,.F.);
#80753=ORIENTED_EDGE('',*,*,#56962,.T.);
#80754=ORIENTED_EDGE('',*,*,#55088,.F.);
#80755=ORIENTED_EDGE('',*,*,#56964,.F.);
#80756=ORIENTED_EDGE('',*,*,#54101,.F.);
#80757=ORIENTED_EDGE('',*,*,#56963,.T.);
#80758=ORIENTED_EDGE('',*,*,#52159,.F.);
#80759=ORIENTED_EDGE('',*,*,#56965,.F.);
#80760=ORIENTED_EDGE('',*,*,#56358,.F.);
#80761=ORIENTED_EDGE('',*,*,#56964,.T.);
#80762=ORIENTED_EDGE('',*,*,#55087,.F.);
#80763=ORIENTED_EDGE('',*,*,#56966,.F.);
#80764=ORIENTED_EDGE('',*,*,#52504,.F.);
#80765=ORIENTED_EDGE('',*,*,#56965,.T.);
#80766=ORIENTED_EDGE('',*,*,#52158,.F.);
#80767=ORIENTED_EDGE('',*,*,#56967,.F.);
#80768=ORIENTED_EDGE('',*,*,#55075,.F.);
#80769=ORIENTED_EDGE('',*,*,#56966,.T.);
#80770=ORIENTED_EDGE('',*,*,#56357,.F.);
#80771=ORIENTED_EDGE('',*,*,#56968,.F.);
#80772=ORIENTED_EDGE('',*,*,#52505,.F.);
#80773=ORIENTED_EDGE('',*,*,#56967,.T.);
#80774=ORIENTED_EDGE('',*,*,#54132,.F.);
#80775=ORIENTED_EDGE('',*,*,#56969,.F.);
#80776=ORIENTED_EDGE('',*,*,#55076,.F.);
#80777=ORIENTED_EDGE('',*,*,#56968,.T.);
#80778=ORIENTED_EDGE('',*,*,#55071,.F.);
#80779=ORIENTED_EDGE('',*,*,#56970,.F.);
#80780=ORIENTED_EDGE('',*,*,#52506,.F.);
#80781=ORIENTED_EDGE('',*,*,#54127,.F.);
#80782=ORIENTED_EDGE('',*,*,#54123,.T.);
#80783=ORIENTED_EDGE('',*,*,#56971,.F.);
#80784=ORIENTED_EDGE('',*,*,#55077,.F.);
#80785=ORIENTED_EDGE('',*,*,#56969,.T.);
#80786=ORIENTED_EDGE('',*,*,#56970,.T.);
#80787=ORIENTED_EDGE('',*,*,#56359,.F.);
#80788=ORIENTED_EDGE('',*,*,#56972,.F.);
#80789=ORIENTED_EDGE('',*,*,#52507,.F.);
#80790=ORIENTED_EDGE('',*,*,#56971,.T.);
#80791=ORIENTED_EDGE('',*,*,#54122,.F.);
#80792=ORIENTED_EDGE('',*,*,#56973,.F.);
#80793=ORIENTED_EDGE('',*,*,#55078,.F.);
#80794=ORIENTED_EDGE('',*,*,#56972,.T.);
#80795=ORIENTED_EDGE('',*,*,#55073,.F.);
#80796=ORIENTED_EDGE('',*,*,#56974,.F.);
#80797=ORIENTED_EDGE('',*,*,#52508,.F.);
#80798=ORIENTED_EDGE('',*,*,#56973,.T.);
#80799=ORIENTED_EDGE('',*,*,#54134,.F.);
#80800=ORIENTED_EDGE('',*,*,#56975,.F.);
#80801=ORIENTED_EDGE('',*,*,#55079,.F.);
#80802=ORIENTED_EDGE('',*,*,#56974,.T.);
#80803=ORIENTED_EDGE('',*,*,#55072,.F.);
#80804=ORIENTED_EDGE('',*,*,#56976,.F.);
#80805=ORIENTED_EDGE('',*,*,#54130,.F.);
#80806=ORIENTED_EDGE('',*,*,#56975,.T.);
#80807=ORIENTED_EDGE('',*,*,#54118,.F.);
#80808=ORIENTED_EDGE('',*,*,#56977,.F.);
#80809=ORIENTED_EDGE('',*,*,#55080,.F.);
#80810=ORIENTED_EDGE('',*,*,#56976,.T.);
#80811=ORIENTED_EDGE('',*,*,#55083,.F.);
#80812=ORIENTED_EDGE('',*,*,#56978,.F.);
#80813=ORIENTED_EDGE('',*,*,#54109,.F.);
#80814=ORIENTED_EDGE('',*,*,#56977,.T.);
#80815=ORIENTED_EDGE('',*,*,#54136,.F.);
#80816=ORIENTED_EDGE('',*,*,#56979,.F.);
#80817=ORIENTED_EDGE('',*,*,#55081,.F.);
#80818=ORIENTED_EDGE('',*,*,#56978,.T.);
#80819=ORIENTED_EDGE('',*,*,#55082,.F.);
#80820=ORIENTED_EDGE('',*,*,#56979,.T.);
#80821=ORIENTED_EDGE('',*,*,#54114,.F.);
#80822=ORIENTED_EDGE('',*,*,#54110,.T.);
#80823=ORIENTED_EDGE('',*,*,#56980,.F.);
#80824=ORIENTED_EDGE('',*,*,#55122,.F.);
#80825=ORIENTED_EDGE('',*,*,#56981,.F.);
#80826=ORIENTED_EDGE('',*,*,#54066,.F.);
#80827=ORIENTED_EDGE('',*,*,#56981,.T.);
#80828=ORIENTED_EDGE('',*,*,#55121,.F.);
#80829=ORIENTED_EDGE('',*,*,#56982,.F.);
#80830=ORIENTED_EDGE('',*,*,#54075,.F.);
#80831=ORIENTED_EDGE('',*,*,#54065,.T.);
#80832=ORIENTED_EDGE('',*,*,#54069,.F.);
#80833=ORIENTED_EDGE('',*,*,#56983,.F.);
#80834=ORIENTED_EDGE('',*,*,#55123,.F.);
#80835=ORIENTED_EDGE('',*,*,#56980,.T.);
#80836=ORIENTED_EDGE('',*,*,#56982,.T.);
#80837=ORIENTED_EDGE('',*,*,#55120,.F.);
#80838=ORIENTED_EDGE('',*,*,#56984,.F.);
#80839=ORIENTED_EDGE('',*,*,#54060,.F.);
#80840=ORIENTED_EDGE('',*,*,#56983,.T.);
#80841=ORIENTED_EDGE('',*,*,#54073,.F.);
#80842=ORIENTED_EDGE('',*,*,#56985,.F.);
#80843=ORIENTED_EDGE('',*,*,#55112,.F.);
#80844=ORIENTED_EDGE('',*,*,#56984,.T.);
#80845=ORIENTED_EDGE('',*,*,#55119,.F.);
#80846=ORIENTED_EDGE('',*,*,#56986,.F.);
#80847=ORIENTED_EDGE('',*,*,#54077,.F.);
#80848=ORIENTED_EDGE('',*,*,#56985,.T.);
#80849=ORIENTED_EDGE('',*,*,#52168,.F.);
#80850=ORIENTED_EDGE('',*,*,#56987,.F.);
#80851=ORIENTED_EDGE('',*,*,#55113,.F.);
#80852=ORIENTED_EDGE('',*,*,#56986,.T.);
#80853=ORIENTED_EDGE('',*,*,#55118,.F.);
#80854=ORIENTED_EDGE('',*,*,#56988,.F.);
#80855=ORIENTED_EDGE('',*,*,#54052,.T.);
#80856=ORIENTED_EDGE('',*,*,#54056,.F.);
#80857=ORIENTED_EDGE('',*,*,#56987,.T.);
#80858=ORIENTED_EDGE('',*,*,#52167,.F.);
#80859=ORIENTED_EDGE('',*,*,#56989,.F.);
#80860=ORIENTED_EDGE('',*,*,#56360,.F.);
#80861=ORIENTED_EDGE('',*,*,#56988,.T.);
#80862=ORIENTED_EDGE('',*,*,#55117,.F.);
#80863=ORIENTED_EDGE('',*,*,#56990,.F.);
#80864=ORIENTED_EDGE('',*,*,#54053,.F.);
#80865=ORIENTED_EDGE('',*,*,#56989,.T.);
#80866=ORIENTED_EDGE('',*,*,#52166,.F.);
#80867=ORIENTED_EDGE('',*,*,#56991,.F.);
#80868=ORIENTED_EDGE('',*,*,#55097,.F.);
#80869=ORIENTED_EDGE('',*,*,#56990,.T.);
#80870=ORIENTED_EDGE('',*,*,#55116,.F.);
#80871=ORIENTED_EDGE('',*,*,#56992,.F.);
#80872=ORIENTED_EDGE('',*,*,#54071,.F.);
#80873=ORIENTED_EDGE('',*,*,#56991,.T.);
#80874=ORIENTED_EDGE('',*,*,#52165,.F.);
#80875=ORIENTED_EDGE('',*,*,#56993,.F.);
#80876=ORIENTED_EDGE('',*,*,#56362,.F.);
#80877=ORIENTED_EDGE('',*,*,#56992,.T.);
#80878=ORIENTED_EDGE('',*,*,#55115,.F.);
#80879=ORIENTED_EDGE('',*,*,#56994,.F.);
#80880=ORIENTED_EDGE('',*,*,#52498,.F.);
#80881=ORIENTED_EDGE('',*,*,#56993,.T.);
#80882=ORIENTED_EDGE('',*,*,#52164,.F.);
#80883=ORIENTED_EDGE('',*,*,#56995,.F.);
#80884=ORIENTED_EDGE('',*,*,#55103,.F.);
#80885=ORIENTED_EDGE('',*,*,#56994,.T.);
#80886=ORIENTED_EDGE('',*,*,#56361,.F.);
#80887=ORIENTED_EDGE('',*,*,#56996,.F.);
#80888=ORIENTED_EDGE('',*,*,#52499,.F.);
#80889=ORIENTED_EDGE('',*,*,#56995,.T.);
#80890=ORIENTED_EDGE('',*,*,#54102,.F.);
#80891=ORIENTED_EDGE('',*,*,#56997,.F.);
#80892=ORIENTED_EDGE('',*,*,#55104,.F.);
#80893=ORIENTED_EDGE('',*,*,#56996,.T.);
#80894=ORIENTED_EDGE('',*,*,#55099,.F.);
#80895=ORIENTED_EDGE('',*,*,#56998,.F.);
#80896=ORIENTED_EDGE('',*,*,#52500,.F.);
#80897=ORIENTED_EDGE('',*,*,#54097,.F.);
#80898=ORIENTED_EDGE('',*,*,#54093,.T.);
#80899=ORIENTED_EDGE('',*,*,#56999,.F.);
#80900=ORIENTED_EDGE('',*,*,#55105,.F.);
#80901=ORIENTED_EDGE('',*,*,#56997,.T.);
#80902=ORIENTED_EDGE('',*,*,#56998,.T.);
#80903=ORIENTED_EDGE('',*,*,#56363,.F.);
#80904=ORIENTED_EDGE('',*,*,#57000,.F.);
#80905=ORIENTED_EDGE('',*,*,#52501,.F.);
#80906=ORIENTED_EDGE('',*,*,#56999,.T.);
#80907=ORIENTED_EDGE('',*,*,#54092,.F.);
#80908=ORIENTED_EDGE('',*,*,#57001,.F.);
#80909=ORIENTED_EDGE('',*,*,#55106,.F.);
#80910=ORIENTED_EDGE('',*,*,#57000,.T.);
#80911=ORIENTED_EDGE('',*,*,#55101,.F.);
#80912=ORIENTED_EDGE('',*,*,#57002,.F.);
#80913=ORIENTED_EDGE('',*,*,#52502,.F.);
#80914=ORIENTED_EDGE('',*,*,#57001,.T.);
#80915=ORIENTED_EDGE('',*,*,#54104,.F.);
#80916=ORIENTED_EDGE('',*,*,#57003,.F.);
#80917=ORIENTED_EDGE('',*,*,#55107,.F.);
#80918=ORIENTED_EDGE('',*,*,#57002,.T.);
#80919=ORIENTED_EDGE('',*,*,#55100,.F.);
#80920=ORIENTED_EDGE('',*,*,#57004,.F.);
#80921=ORIENTED_EDGE('',*,*,#54100,.F.);
#80922=ORIENTED_EDGE('',*,*,#57003,.T.);
#80923=ORIENTED_EDGE('',*,*,#54088,.F.);
#80924=ORIENTED_EDGE('',*,*,#57005,.F.);
#80925=ORIENTED_EDGE('',*,*,#55108,.F.);
#80926=ORIENTED_EDGE('',*,*,#57004,.T.);
#80927=ORIENTED_EDGE('',*,*,#55111,.F.);
#80928=ORIENTED_EDGE('',*,*,#57006,.F.);
#80929=ORIENTED_EDGE('',*,*,#54079,.F.);
#80930=ORIENTED_EDGE('',*,*,#57005,.T.);
#80931=ORIENTED_EDGE('',*,*,#54106,.F.);
#80932=ORIENTED_EDGE('',*,*,#57007,.F.);
#80933=ORIENTED_EDGE('',*,*,#55109,.F.);
#80934=ORIENTED_EDGE('',*,*,#57006,.T.);
#80935=ORIENTED_EDGE('',*,*,#55110,.F.);
#80936=ORIENTED_EDGE('',*,*,#57007,.T.);
#80937=ORIENTED_EDGE('',*,*,#54084,.F.);
#80938=ORIENTED_EDGE('',*,*,#54080,.T.);
#80939=ORIENTED_EDGE('',*,*,#57008,.F.);
#80940=ORIENTED_EDGE('',*,*,#55150,.F.);
#80941=ORIENTED_EDGE('',*,*,#57009,.F.);
#80942=ORIENTED_EDGE('',*,*,#54036,.F.);
#80943=ORIENTED_EDGE('',*,*,#57009,.T.);
#80944=ORIENTED_EDGE('',*,*,#55149,.F.);
#80945=ORIENTED_EDGE('',*,*,#57010,.F.);
#80946=ORIENTED_EDGE('',*,*,#54045,.F.);
#80947=ORIENTED_EDGE('',*,*,#54035,.T.);
#80948=ORIENTED_EDGE('',*,*,#54039,.F.);
#80949=ORIENTED_EDGE('',*,*,#57011,.F.);
#80950=ORIENTED_EDGE('',*,*,#55151,.F.);
#80951=ORIENTED_EDGE('',*,*,#57008,.T.);
#80952=ORIENTED_EDGE('',*,*,#57010,.T.);
#80953=ORIENTED_EDGE('',*,*,#55148,.F.);
#80954=ORIENTED_EDGE('',*,*,#57012,.F.);
#80955=ORIENTED_EDGE('',*,*,#54030,.F.);
#80956=ORIENTED_EDGE('',*,*,#57011,.T.);
#80957=ORIENTED_EDGE('',*,*,#54043,.F.);
#80958=ORIENTED_EDGE('',*,*,#57013,.F.);
#80959=ORIENTED_EDGE('',*,*,#55140,.F.);
#80960=ORIENTED_EDGE('',*,*,#57012,.T.);
#80961=ORIENTED_EDGE('',*,*,#55147,.F.);
#80962=ORIENTED_EDGE('',*,*,#57014,.F.);
#80963=ORIENTED_EDGE('',*,*,#54047,.F.);
#80964=ORIENTED_EDGE('',*,*,#57013,.T.);
#80965=ORIENTED_EDGE('',*,*,#52174,.F.);
#80966=ORIENTED_EDGE('',*,*,#57015,.F.);
#80967=ORIENTED_EDGE('',*,*,#55141,.F.);
#80968=ORIENTED_EDGE('',*,*,#57014,.T.);
#80969=ORIENTED_EDGE('',*,*,#55146,.F.);
#80970=ORIENTED_EDGE('',*,*,#57016,.F.);
#80971=ORIENTED_EDGE('',*,*,#54022,.T.);
#80972=ORIENTED_EDGE('',*,*,#54026,.F.);
#80973=ORIENTED_EDGE('',*,*,#57015,.T.);
#80974=ORIENTED_EDGE('',*,*,#52173,.F.);
#80975=ORIENTED_EDGE('',*,*,#57017,.F.);
#80976=ORIENTED_EDGE('',*,*,#56364,.F.);
#80977=ORIENTED_EDGE('',*,*,#57016,.T.);
#80978=ORIENTED_EDGE('',*,*,#55145,.F.);
#80979=ORIENTED_EDGE('',*,*,#57018,.F.);
#80980=ORIENTED_EDGE('',*,*,#54023,.F.);
#80981=ORIENTED_EDGE('',*,*,#57017,.T.);
#80982=ORIENTED_EDGE('',*,*,#52172,.F.);
#80983=ORIENTED_EDGE('',*,*,#57019,.F.);
#80984=ORIENTED_EDGE('',*,*,#55125,.F.);
#80985=ORIENTED_EDGE('',*,*,#57018,.T.);
#80986=ORIENTED_EDGE('',*,*,#55144,.F.);
#80987=ORIENTED_EDGE('',*,*,#57020,.F.);
#80988=ORIENTED_EDGE('',*,*,#54041,.F.);
#80989=ORIENTED_EDGE('',*,*,#57019,.T.);
#80990=ORIENTED_EDGE('',*,*,#52171,.F.);
#80991=ORIENTED_EDGE('',*,*,#57021,.F.);
#80992=ORIENTED_EDGE('',*,*,#56366,.F.);
#80993=ORIENTED_EDGE('',*,*,#57020,.T.);
#80994=ORIENTED_EDGE('',*,*,#55143,.F.);
#80995=ORIENTED_EDGE('',*,*,#57022,.F.);
#80996=ORIENTED_EDGE('',*,*,#52492,.F.);
#80997=ORIENTED_EDGE('',*,*,#57021,.T.);
#80998=ORIENTED_EDGE('',*,*,#52170,.F.);
#80999=ORIENTED_EDGE('',*,*,#57023,.F.);
#81000=ORIENTED_EDGE('',*,*,#55131,.F.);
#81001=ORIENTED_EDGE('',*,*,#57022,.T.);
#81002=ORIENTED_EDGE('',*,*,#56365,.F.);
#81003=ORIENTED_EDGE('',*,*,#57024,.F.);
#81004=ORIENTED_EDGE('',*,*,#52493,.F.);
#81005=ORIENTED_EDGE('',*,*,#57023,.T.);
#81006=ORIENTED_EDGE('',*,*,#54072,.F.);
#81007=ORIENTED_EDGE('',*,*,#57025,.F.);
#81008=ORIENTED_EDGE('',*,*,#55132,.F.);
#81009=ORIENTED_EDGE('',*,*,#57024,.T.);
#81010=ORIENTED_EDGE('',*,*,#55127,.F.);
#81011=ORIENTED_EDGE('',*,*,#57026,.F.);
#81012=ORIENTED_EDGE('',*,*,#52494,.F.);
#81013=ORIENTED_EDGE('',*,*,#54067,.F.);
#81014=ORIENTED_EDGE('',*,*,#54063,.T.);
#81015=ORIENTED_EDGE('',*,*,#57027,.F.);
#81016=ORIENTED_EDGE('',*,*,#55133,.F.);
#81017=ORIENTED_EDGE('',*,*,#57025,.T.);
#81018=ORIENTED_EDGE('',*,*,#57026,.T.);
#81019=ORIENTED_EDGE('',*,*,#56367,.F.);
#81020=ORIENTED_EDGE('',*,*,#57028,.F.);
#81021=ORIENTED_EDGE('',*,*,#52495,.F.);
#81022=ORIENTED_EDGE('',*,*,#57027,.T.);
#81023=ORIENTED_EDGE('',*,*,#54062,.F.);
#81024=ORIENTED_EDGE('',*,*,#57029,.F.);
#81025=ORIENTED_EDGE('',*,*,#55134,.F.);
#81026=ORIENTED_EDGE('',*,*,#57028,.T.);
#81027=ORIENTED_EDGE('',*,*,#55129,.F.);
#81028=ORIENTED_EDGE('',*,*,#57030,.F.);
#81029=ORIENTED_EDGE('',*,*,#52496,.F.);
#81030=ORIENTED_EDGE('',*,*,#57029,.T.);
#81031=ORIENTED_EDGE('',*,*,#54074,.F.);
#81032=ORIENTED_EDGE('',*,*,#57031,.F.);
#81033=ORIENTED_EDGE('',*,*,#55135,.F.);
#81034=ORIENTED_EDGE('',*,*,#57030,.T.);
#81035=ORIENTED_EDGE('',*,*,#55128,.F.);
#81036=ORIENTED_EDGE('',*,*,#57032,.F.);
#81037=ORIENTED_EDGE('',*,*,#54070,.F.);
#81038=ORIENTED_EDGE('',*,*,#57031,.T.);
#81039=ORIENTED_EDGE('',*,*,#54058,.F.);
#81040=ORIENTED_EDGE('',*,*,#57033,.F.);
#81041=ORIENTED_EDGE('',*,*,#55136,.F.);
#81042=ORIENTED_EDGE('',*,*,#57032,.T.);
#81043=ORIENTED_EDGE('',*,*,#55139,.F.);
#81044=ORIENTED_EDGE('',*,*,#57034,.F.);
#81045=ORIENTED_EDGE('',*,*,#54049,.F.);
#81046=ORIENTED_EDGE('',*,*,#57033,.T.);
#81047=ORIENTED_EDGE('',*,*,#54076,.F.);
#81048=ORIENTED_EDGE('',*,*,#57035,.F.);
#81049=ORIENTED_EDGE('',*,*,#55137,.F.);
#81050=ORIENTED_EDGE('',*,*,#57034,.T.);
#81051=ORIENTED_EDGE('',*,*,#55138,.F.);
#81052=ORIENTED_EDGE('',*,*,#57035,.T.);
#81053=ORIENTED_EDGE('',*,*,#54054,.F.);
#81054=ORIENTED_EDGE('',*,*,#54050,.T.);
#81055=ORIENTED_EDGE('',*,*,#57036,.F.);
#81056=ORIENTED_EDGE('',*,*,#55178,.F.);
#81057=ORIENTED_EDGE('',*,*,#57037,.F.);
#81058=ORIENTED_EDGE('',*,*,#54006,.F.);
#81059=ORIENTED_EDGE('',*,*,#57037,.T.);
#81060=ORIENTED_EDGE('',*,*,#55177,.F.);
#81061=ORIENTED_EDGE('',*,*,#57038,.F.);
#81062=ORIENTED_EDGE('',*,*,#54015,.F.);
#81063=ORIENTED_EDGE('',*,*,#54005,.T.);
#81064=ORIENTED_EDGE('',*,*,#54009,.F.);
#81065=ORIENTED_EDGE('',*,*,#57039,.F.);
#81066=ORIENTED_EDGE('',*,*,#55179,.F.);
#81067=ORIENTED_EDGE('',*,*,#57036,.T.);
#81068=ORIENTED_EDGE('',*,*,#57038,.T.);
#81069=ORIENTED_EDGE('',*,*,#55176,.F.);
#81070=ORIENTED_EDGE('',*,*,#57040,.F.);
#81071=ORIENTED_EDGE('',*,*,#54000,.F.);
#81072=ORIENTED_EDGE('',*,*,#57039,.T.);
#81073=ORIENTED_EDGE('',*,*,#54013,.F.);
#81074=ORIENTED_EDGE('',*,*,#57041,.F.);
#81075=ORIENTED_EDGE('',*,*,#55168,.F.);
#81076=ORIENTED_EDGE('',*,*,#57040,.T.);
#81077=ORIENTED_EDGE('',*,*,#55175,.F.);
#81078=ORIENTED_EDGE('',*,*,#57042,.F.);
#81079=ORIENTED_EDGE('',*,*,#54017,.F.);
#81080=ORIENTED_EDGE('',*,*,#57041,.T.);
#81081=ORIENTED_EDGE('',*,*,#52180,.F.);
#81082=ORIENTED_EDGE('',*,*,#57043,.F.);
#81083=ORIENTED_EDGE('',*,*,#55169,.F.);
#81084=ORIENTED_EDGE('',*,*,#57042,.T.);
#81085=ORIENTED_EDGE('',*,*,#55174,.F.);
#81086=ORIENTED_EDGE('',*,*,#57044,.F.);
#81087=ORIENTED_EDGE('',*,*,#53992,.T.);
#81088=ORIENTED_EDGE('',*,*,#53996,.F.);
#81089=ORIENTED_EDGE('',*,*,#57043,.T.);
#81090=ORIENTED_EDGE('',*,*,#52179,.F.);
#81091=ORIENTED_EDGE('',*,*,#57045,.F.);
#81092=ORIENTED_EDGE('',*,*,#56368,.F.);
#81093=ORIENTED_EDGE('',*,*,#57044,.T.);
#81094=ORIENTED_EDGE('',*,*,#55173,.F.);
#81095=ORIENTED_EDGE('',*,*,#57046,.F.);
#81096=ORIENTED_EDGE('',*,*,#53993,.F.);
#81097=ORIENTED_EDGE('',*,*,#57045,.T.);
#81098=ORIENTED_EDGE('',*,*,#52178,.F.);
#81099=ORIENTED_EDGE('',*,*,#57047,.F.);
#81100=ORIENTED_EDGE('',*,*,#55153,.F.);
#81101=ORIENTED_EDGE('',*,*,#57046,.T.);
#81102=ORIENTED_EDGE('',*,*,#55172,.F.);
#81103=ORIENTED_EDGE('',*,*,#57048,.F.);
#81104=ORIENTED_EDGE('',*,*,#54011,.F.);
#81105=ORIENTED_EDGE('',*,*,#57047,.T.);
#81106=ORIENTED_EDGE('',*,*,#52177,.F.);
#81107=ORIENTED_EDGE('',*,*,#57049,.F.);
#81108=ORIENTED_EDGE('',*,*,#56370,.F.);
#81109=ORIENTED_EDGE('',*,*,#57048,.T.);
#81110=ORIENTED_EDGE('',*,*,#55171,.F.);
#81111=ORIENTED_EDGE('',*,*,#57050,.F.);
#81112=ORIENTED_EDGE('',*,*,#52486,.F.);
#81113=ORIENTED_EDGE('',*,*,#57049,.T.);
#81114=ORIENTED_EDGE('',*,*,#52176,.F.);
#81115=ORIENTED_EDGE('',*,*,#57051,.F.);
#81116=ORIENTED_EDGE('',*,*,#55159,.F.);
#81117=ORIENTED_EDGE('',*,*,#57050,.T.);
#81118=ORIENTED_EDGE('',*,*,#56369,.F.);
#81119=ORIENTED_EDGE('',*,*,#57052,.F.);
#81120=ORIENTED_EDGE('',*,*,#52487,.F.);
#81121=ORIENTED_EDGE('',*,*,#57051,.T.);
#81122=ORIENTED_EDGE('',*,*,#54042,.F.);
#81123=ORIENTED_EDGE('',*,*,#57053,.F.);
#81124=ORIENTED_EDGE('',*,*,#55160,.F.);
#81125=ORIENTED_EDGE('',*,*,#57052,.T.);
#81126=ORIENTED_EDGE('',*,*,#55155,.F.);
#81127=ORIENTED_EDGE('',*,*,#57054,.F.);
#81128=ORIENTED_EDGE('',*,*,#52488,.F.);
#81129=ORIENTED_EDGE('',*,*,#54037,.F.);
#81130=ORIENTED_EDGE('',*,*,#54033,.T.);
#81131=ORIENTED_EDGE('',*,*,#57055,.F.);
#81132=ORIENTED_EDGE('',*,*,#55161,.F.);
#81133=ORIENTED_EDGE('',*,*,#57053,.T.);
#81134=ORIENTED_EDGE('',*,*,#57054,.T.);
#81135=ORIENTED_EDGE('',*,*,#56371,.F.);
#81136=ORIENTED_EDGE('',*,*,#57056,.F.);
#81137=ORIENTED_EDGE('',*,*,#52489,.F.);
#81138=ORIENTED_EDGE('',*,*,#57055,.T.);
#81139=ORIENTED_EDGE('',*,*,#54032,.F.);
#81140=ORIENTED_EDGE('',*,*,#57057,.F.);
#81141=ORIENTED_EDGE('',*,*,#55162,.F.);
#81142=ORIENTED_EDGE('',*,*,#57056,.T.);
#81143=ORIENTED_EDGE('',*,*,#55157,.F.);
#81144=ORIENTED_EDGE('',*,*,#57058,.F.);
#81145=ORIENTED_EDGE('',*,*,#52490,.F.);
#81146=ORIENTED_EDGE('',*,*,#57057,.T.);
#81147=ORIENTED_EDGE('',*,*,#54044,.F.);
#81148=ORIENTED_EDGE('',*,*,#57059,.F.);
#81149=ORIENTED_EDGE('',*,*,#55163,.F.);
#81150=ORIENTED_EDGE('',*,*,#57058,.T.);
#81151=ORIENTED_EDGE('',*,*,#55156,.F.);
#81152=ORIENTED_EDGE('',*,*,#57060,.F.);
#81153=ORIENTED_EDGE('',*,*,#54040,.F.);
#81154=ORIENTED_EDGE('',*,*,#57059,.T.);
#81155=ORIENTED_EDGE('',*,*,#54028,.F.);
#81156=ORIENTED_EDGE('',*,*,#57061,.F.);
#81157=ORIENTED_EDGE('',*,*,#55164,.F.);
#81158=ORIENTED_EDGE('',*,*,#57060,.T.);
#81159=ORIENTED_EDGE('',*,*,#55167,.F.);
#81160=ORIENTED_EDGE('',*,*,#57062,.F.);
#81161=ORIENTED_EDGE('',*,*,#54019,.F.);
#81162=ORIENTED_EDGE('',*,*,#57061,.T.);
#81163=ORIENTED_EDGE('',*,*,#54046,.F.);
#81164=ORIENTED_EDGE('',*,*,#57063,.F.);
#81165=ORIENTED_EDGE('',*,*,#55165,.F.);
#81166=ORIENTED_EDGE('',*,*,#57062,.T.);
#81167=ORIENTED_EDGE('',*,*,#55166,.F.);
#81168=ORIENTED_EDGE('',*,*,#57063,.T.);
#81169=ORIENTED_EDGE('',*,*,#54024,.F.);
#81170=ORIENTED_EDGE('',*,*,#54020,.T.);
#81171=ORIENTED_EDGE('',*,*,#57064,.F.);
#81172=ORIENTED_EDGE('',*,*,#55206,.F.);
#81173=ORIENTED_EDGE('',*,*,#57065,.F.);
#81174=ORIENTED_EDGE('',*,*,#53976,.F.);
#81175=ORIENTED_EDGE('',*,*,#57065,.T.);
#81176=ORIENTED_EDGE('',*,*,#55205,.F.);
#81177=ORIENTED_EDGE('',*,*,#57066,.F.);
#81178=ORIENTED_EDGE('',*,*,#53985,.F.);
#81179=ORIENTED_EDGE('',*,*,#53975,.T.);
#81180=ORIENTED_EDGE('',*,*,#53979,.F.);
#81181=ORIENTED_EDGE('',*,*,#57067,.F.);
#81182=ORIENTED_EDGE('',*,*,#55207,.F.);
#81183=ORIENTED_EDGE('',*,*,#57064,.T.);
#81184=ORIENTED_EDGE('',*,*,#57066,.T.);
#81185=ORIENTED_EDGE('',*,*,#55204,.F.);
#81186=ORIENTED_EDGE('',*,*,#57068,.F.);
#81187=ORIENTED_EDGE('',*,*,#53970,.F.);
#81188=ORIENTED_EDGE('',*,*,#57067,.T.);
#81189=ORIENTED_EDGE('',*,*,#53983,.F.);
#81190=ORIENTED_EDGE('',*,*,#57069,.F.);
#81191=ORIENTED_EDGE('',*,*,#55196,.F.);
#81192=ORIENTED_EDGE('',*,*,#57068,.T.);
#81193=ORIENTED_EDGE('',*,*,#55203,.F.);
#81194=ORIENTED_EDGE('',*,*,#57070,.F.);
#81195=ORIENTED_EDGE('',*,*,#53987,.F.);
#81196=ORIENTED_EDGE('',*,*,#57069,.T.);
#81197=ORIENTED_EDGE('',*,*,#52186,.F.);
#81198=ORIENTED_EDGE('',*,*,#57071,.F.);
#81199=ORIENTED_EDGE('',*,*,#55197,.F.);
#81200=ORIENTED_EDGE('',*,*,#57070,.T.);
#81201=ORIENTED_EDGE('',*,*,#55202,.F.);
#81202=ORIENTED_EDGE('',*,*,#57072,.F.);
#81203=ORIENTED_EDGE('',*,*,#53962,.T.);
#81204=ORIENTED_EDGE('',*,*,#53966,.F.);
#81205=ORIENTED_EDGE('',*,*,#57071,.T.);
#81206=ORIENTED_EDGE('',*,*,#52185,.F.);
#81207=ORIENTED_EDGE('',*,*,#57073,.F.);
#81208=ORIENTED_EDGE('',*,*,#56372,.F.);
#81209=ORIENTED_EDGE('',*,*,#57072,.T.);
#81210=ORIENTED_EDGE('',*,*,#55201,.F.);
#81211=ORIENTED_EDGE('',*,*,#57074,.F.);
#81212=ORIENTED_EDGE('',*,*,#53963,.F.);
#81213=ORIENTED_EDGE('',*,*,#57073,.T.);
#81214=ORIENTED_EDGE('',*,*,#52184,.F.);
#81215=ORIENTED_EDGE('',*,*,#57075,.F.);
#81216=ORIENTED_EDGE('',*,*,#55181,.F.);
#81217=ORIENTED_EDGE('',*,*,#57074,.T.);
#81218=ORIENTED_EDGE('',*,*,#55200,.F.);
#81219=ORIENTED_EDGE('',*,*,#57076,.F.);
#81220=ORIENTED_EDGE('',*,*,#53981,.F.);
#81221=ORIENTED_EDGE('',*,*,#57075,.T.);
#81222=ORIENTED_EDGE('',*,*,#52183,.F.);
#81223=ORIENTED_EDGE('',*,*,#57077,.F.);
#81224=ORIENTED_EDGE('',*,*,#56374,.F.);
#81225=ORIENTED_EDGE('',*,*,#57076,.T.);
#81226=ORIENTED_EDGE('',*,*,#55199,.F.);
#81227=ORIENTED_EDGE('',*,*,#57078,.F.);
#81228=ORIENTED_EDGE('',*,*,#52480,.F.);
#81229=ORIENTED_EDGE('',*,*,#57077,.T.);
#81230=ORIENTED_EDGE('',*,*,#52182,.F.);
#81231=ORIENTED_EDGE('',*,*,#57079,.F.);
#81232=ORIENTED_EDGE('',*,*,#55187,.F.);
#81233=ORIENTED_EDGE('',*,*,#57078,.T.);
#81234=ORIENTED_EDGE('',*,*,#56373,.F.);
#81235=ORIENTED_EDGE('',*,*,#57080,.F.);
#81236=ORIENTED_EDGE('',*,*,#52481,.F.);
#81237=ORIENTED_EDGE('',*,*,#57079,.T.);
#81238=ORIENTED_EDGE('',*,*,#54012,.F.);
#81239=ORIENTED_EDGE('',*,*,#57081,.F.);
#81240=ORIENTED_EDGE('',*,*,#55188,.F.);
#81241=ORIENTED_EDGE('',*,*,#57080,.T.);
#81242=ORIENTED_EDGE('',*,*,#55183,.F.);
#81243=ORIENTED_EDGE('',*,*,#57082,.F.);
#81244=ORIENTED_EDGE('',*,*,#52482,.F.);
#81245=ORIENTED_EDGE('',*,*,#54007,.F.);
#81246=ORIENTED_EDGE('',*,*,#54003,.T.);
#81247=ORIENTED_EDGE('',*,*,#57083,.F.);
#81248=ORIENTED_EDGE('',*,*,#55189,.F.);
#81249=ORIENTED_EDGE('',*,*,#57081,.T.);
#81250=ORIENTED_EDGE('',*,*,#57082,.T.);
#81251=ORIENTED_EDGE('',*,*,#56375,.F.);
#81252=ORIENTED_EDGE('',*,*,#57084,.F.);
#81253=ORIENTED_EDGE('',*,*,#52483,.F.);
#81254=ORIENTED_EDGE('',*,*,#57083,.T.);
#81255=ORIENTED_EDGE('',*,*,#54002,.F.);
#81256=ORIENTED_EDGE('',*,*,#57085,.F.);
#81257=ORIENTED_EDGE('',*,*,#55190,.F.);
#81258=ORIENTED_EDGE('',*,*,#57084,.T.);
#81259=ORIENTED_EDGE('',*,*,#55185,.F.);
#81260=ORIENTED_EDGE('',*,*,#57086,.F.);
#81261=ORIENTED_EDGE('',*,*,#52484,.F.);
#81262=ORIENTED_EDGE('',*,*,#57085,.T.);
#81263=ORIENTED_EDGE('',*,*,#54014,.F.);
#81264=ORIENTED_EDGE('',*,*,#57087,.F.);
#81265=ORIENTED_EDGE('',*,*,#55191,.F.);
#81266=ORIENTED_EDGE('',*,*,#57086,.T.);
#81267=ORIENTED_EDGE('',*,*,#55184,.F.);
#81268=ORIENTED_EDGE('',*,*,#57088,.F.);
#81269=ORIENTED_EDGE('',*,*,#54010,.F.);
#81270=ORIENTED_EDGE('',*,*,#57087,.T.);
#81271=ORIENTED_EDGE('',*,*,#53998,.F.);
#81272=ORIENTED_EDGE('',*,*,#57089,.F.);
#81273=ORIENTED_EDGE('',*,*,#55192,.F.);
#81274=ORIENTED_EDGE('',*,*,#57088,.T.);
#81275=ORIENTED_EDGE('',*,*,#55195,.F.);
#81276=ORIENTED_EDGE('',*,*,#57090,.F.);
#81277=ORIENTED_EDGE('',*,*,#53989,.F.);
#81278=ORIENTED_EDGE('',*,*,#57089,.T.);
#81279=ORIENTED_EDGE('',*,*,#54016,.F.);
#81280=ORIENTED_EDGE('',*,*,#57091,.F.);
#81281=ORIENTED_EDGE('',*,*,#55193,.F.);
#81282=ORIENTED_EDGE('',*,*,#57090,.T.);
#81283=ORIENTED_EDGE('',*,*,#55194,.F.);
#81284=ORIENTED_EDGE('',*,*,#57091,.T.);
#81285=ORIENTED_EDGE('',*,*,#53994,.F.);
#81286=ORIENTED_EDGE('',*,*,#53990,.T.);
#81287=ORIENTED_EDGE('',*,*,#57092,.F.);
#81288=ORIENTED_EDGE('',*,*,#55234,.F.);
#81289=ORIENTED_EDGE('',*,*,#57093,.F.);
#81290=ORIENTED_EDGE('',*,*,#53946,.F.);
#81291=ORIENTED_EDGE('',*,*,#57093,.T.);
#81292=ORIENTED_EDGE('',*,*,#55233,.F.);
#81293=ORIENTED_EDGE('',*,*,#57094,.F.);
#81294=ORIENTED_EDGE('',*,*,#53955,.F.);
#81295=ORIENTED_EDGE('',*,*,#53945,.T.);
#81296=ORIENTED_EDGE('',*,*,#53949,.F.);
#81297=ORIENTED_EDGE('',*,*,#57095,.F.);
#81298=ORIENTED_EDGE('',*,*,#55235,.F.);
#81299=ORIENTED_EDGE('',*,*,#57092,.T.);
#81300=ORIENTED_EDGE('',*,*,#57094,.T.);
#81301=ORIENTED_EDGE('',*,*,#55232,.F.);
#81302=ORIENTED_EDGE('',*,*,#57096,.F.);
#81303=ORIENTED_EDGE('',*,*,#53940,.F.);
#81304=ORIENTED_EDGE('',*,*,#57095,.T.);
#81305=ORIENTED_EDGE('',*,*,#53953,.F.);
#81306=ORIENTED_EDGE('',*,*,#57097,.F.);
#81307=ORIENTED_EDGE('',*,*,#55224,.F.);
#81308=ORIENTED_EDGE('',*,*,#57096,.T.);
#81309=ORIENTED_EDGE('',*,*,#55231,.F.);
#81310=ORIENTED_EDGE('',*,*,#57098,.F.);
#81311=ORIENTED_EDGE('',*,*,#53957,.F.);
#81312=ORIENTED_EDGE('',*,*,#57097,.T.);
#81313=ORIENTED_EDGE('',*,*,#52192,.F.);
#81314=ORIENTED_EDGE('',*,*,#57099,.F.);
#81315=ORIENTED_EDGE('',*,*,#55225,.F.);
#81316=ORIENTED_EDGE('',*,*,#57098,.T.);
#81317=ORIENTED_EDGE('',*,*,#55230,.F.);
#81318=ORIENTED_EDGE('',*,*,#57100,.F.);
#81319=ORIENTED_EDGE('',*,*,#53932,.T.);
#81320=ORIENTED_EDGE('',*,*,#53936,.F.);
#81321=ORIENTED_EDGE('',*,*,#57099,.T.);
#81322=ORIENTED_EDGE('',*,*,#52191,.F.);
#81323=ORIENTED_EDGE('',*,*,#57101,.F.);
#81324=ORIENTED_EDGE('',*,*,#56376,.F.);
#81325=ORIENTED_EDGE('',*,*,#57100,.T.);
#81326=ORIENTED_EDGE('',*,*,#55229,.F.);
#81327=ORIENTED_EDGE('',*,*,#57102,.F.);
#81328=ORIENTED_EDGE('',*,*,#53933,.F.);
#81329=ORIENTED_EDGE('',*,*,#57101,.T.);
#81330=ORIENTED_EDGE('',*,*,#52190,.F.);
#81331=ORIENTED_EDGE('',*,*,#57103,.F.);
#81332=ORIENTED_EDGE('',*,*,#55209,.F.);
#81333=ORIENTED_EDGE('',*,*,#57102,.T.);
#81334=ORIENTED_EDGE('',*,*,#55228,.F.);
#81335=ORIENTED_EDGE('',*,*,#57104,.F.);
#81336=ORIENTED_EDGE('',*,*,#53951,.F.);
#81337=ORIENTED_EDGE('',*,*,#57103,.T.);
#81338=ORIENTED_EDGE('',*,*,#52189,.F.);
#81339=ORIENTED_EDGE('',*,*,#57105,.F.);
#81340=ORIENTED_EDGE('',*,*,#56378,.F.);
#81341=ORIENTED_EDGE('',*,*,#57104,.T.);
#81342=ORIENTED_EDGE('',*,*,#55227,.F.);
#81343=ORIENTED_EDGE('',*,*,#57106,.F.);
#81344=ORIENTED_EDGE('',*,*,#52474,.F.);
#81345=ORIENTED_EDGE('',*,*,#57105,.T.);
#81346=ORIENTED_EDGE('',*,*,#52188,.F.);
#81347=ORIENTED_EDGE('',*,*,#57107,.F.);
#81348=ORIENTED_EDGE('',*,*,#55215,.F.);
#81349=ORIENTED_EDGE('',*,*,#57106,.T.);
#81350=ORIENTED_EDGE('',*,*,#56377,.F.);
#81351=ORIENTED_EDGE('',*,*,#57108,.F.);
#81352=ORIENTED_EDGE('',*,*,#52475,.F.);
#81353=ORIENTED_EDGE('',*,*,#57107,.T.);
#81354=ORIENTED_EDGE('',*,*,#53982,.F.);
#81355=ORIENTED_EDGE('',*,*,#57109,.F.);
#81356=ORIENTED_EDGE('',*,*,#55216,.F.);
#81357=ORIENTED_EDGE('',*,*,#57108,.T.);
#81358=ORIENTED_EDGE('',*,*,#55211,.F.);
#81359=ORIENTED_EDGE('',*,*,#57110,.F.);
#81360=ORIENTED_EDGE('',*,*,#52476,.F.);
#81361=ORIENTED_EDGE('',*,*,#53977,.F.);
#81362=ORIENTED_EDGE('',*,*,#53973,.T.);
#81363=ORIENTED_EDGE('',*,*,#57111,.F.);
#81364=ORIENTED_EDGE('',*,*,#55217,.F.);
#81365=ORIENTED_EDGE('',*,*,#57109,.T.);
#81366=ORIENTED_EDGE('',*,*,#57110,.T.);
#81367=ORIENTED_EDGE('',*,*,#56379,.F.);
#81368=ORIENTED_EDGE('',*,*,#57112,.F.);
#81369=ORIENTED_EDGE('',*,*,#52477,.F.);
#81370=ORIENTED_EDGE('',*,*,#57111,.T.);
#81371=ORIENTED_EDGE('',*,*,#53972,.F.);
#81372=ORIENTED_EDGE('',*,*,#57113,.F.);
#81373=ORIENTED_EDGE('',*,*,#55218,.F.);
#81374=ORIENTED_EDGE('',*,*,#57112,.T.);
#81375=ORIENTED_EDGE('',*,*,#55213,.F.);
#81376=ORIENTED_EDGE('',*,*,#57114,.F.);
#81377=ORIENTED_EDGE('',*,*,#52478,.F.);
#81378=ORIENTED_EDGE('',*,*,#57113,.T.);
#81379=ORIENTED_EDGE('',*,*,#53984,.F.);
#81380=ORIENTED_EDGE('',*,*,#57115,.F.);
#81381=ORIENTED_EDGE('',*,*,#55219,.F.);
#81382=ORIENTED_EDGE('',*,*,#57114,.T.);
#81383=ORIENTED_EDGE('',*,*,#55212,.F.);
#81384=ORIENTED_EDGE('',*,*,#57116,.F.);
#81385=ORIENTED_EDGE('',*,*,#53980,.F.);
#81386=ORIENTED_EDGE('',*,*,#57115,.T.);
#81387=ORIENTED_EDGE('',*,*,#53968,.F.);
#81388=ORIENTED_EDGE('',*,*,#57117,.F.);
#81389=ORIENTED_EDGE('',*,*,#55220,.F.);
#81390=ORIENTED_EDGE('',*,*,#57116,.T.);
#81391=ORIENTED_EDGE('',*,*,#55223,.F.);
#81392=ORIENTED_EDGE('',*,*,#57118,.F.);
#81393=ORIENTED_EDGE('',*,*,#53959,.F.);
#81394=ORIENTED_EDGE('',*,*,#57117,.T.);
#81395=ORIENTED_EDGE('',*,*,#53986,.F.);
#81396=ORIENTED_EDGE('',*,*,#57119,.F.);
#81397=ORIENTED_EDGE('',*,*,#55221,.F.);
#81398=ORIENTED_EDGE('',*,*,#57118,.T.);
#81399=ORIENTED_EDGE('',*,*,#55222,.F.);
#81400=ORIENTED_EDGE('',*,*,#57119,.T.);
#81401=ORIENTED_EDGE('',*,*,#53964,.F.);
#81402=ORIENTED_EDGE('',*,*,#53960,.T.);
#81403=ORIENTED_EDGE('',*,*,#57120,.F.);
#81404=ORIENTED_EDGE('',*,*,#55262,.F.);
#81405=ORIENTED_EDGE('',*,*,#57121,.F.);
#81406=ORIENTED_EDGE('',*,*,#53916,.F.);
#81407=ORIENTED_EDGE('',*,*,#57121,.T.);
#81408=ORIENTED_EDGE('',*,*,#55261,.F.);
#81409=ORIENTED_EDGE('',*,*,#57122,.F.);
#81410=ORIENTED_EDGE('',*,*,#53925,.F.);
#81411=ORIENTED_EDGE('',*,*,#53915,.T.);
#81412=ORIENTED_EDGE('',*,*,#53919,.F.);
#81413=ORIENTED_EDGE('',*,*,#57123,.F.);
#81414=ORIENTED_EDGE('',*,*,#55263,.F.);
#81415=ORIENTED_EDGE('',*,*,#57120,.T.);
#81416=ORIENTED_EDGE('',*,*,#57122,.T.);
#81417=ORIENTED_EDGE('',*,*,#55260,.F.);
#81418=ORIENTED_EDGE('',*,*,#57124,.F.);
#81419=ORIENTED_EDGE('',*,*,#53910,.F.);
#81420=ORIENTED_EDGE('',*,*,#57123,.T.);
#81421=ORIENTED_EDGE('',*,*,#53923,.F.);
#81422=ORIENTED_EDGE('',*,*,#57125,.F.);
#81423=ORIENTED_EDGE('',*,*,#55252,.F.);
#81424=ORIENTED_EDGE('',*,*,#57124,.T.);
#81425=ORIENTED_EDGE('',*,*,#55259,.F.);
#81426=ORIENTED_EDGE('',*,*,#57126,.F.);
#81427=ORIENTED_EDGE('',*,*,#53927,.F.);
#81428=ORIENTED_EDGE('',*,*,#57125,.T.);
#81429=ORIENTED_EDGE('',*,*,#52198,.F.);
#81430=ORIENTED_EDGE('',*,*,#57127,.F.);
#81431=ORIENTED_EDGE('',*,*,#55253,.F.);
#81432=ORIENTED_EDGE('',*,*,#57126,.T.);
#81433=ORIENTED_EDGE('',*,*,#55258,.F.);
#81434=ORIENTED_EDGE('',*,*,#57128,.F.);
#81435=ORIENTED_EDGE('',*,*,#53902,.T.);
#81436=ORIENTED_EDGE('',*,*,#53906,.F.);
#81437=ORIENTED_EDGE('',*,*,#57127,.T.);
#81438=ORIENTED_EDGE('',*,*,#52197,.F.);
#81439=ORIENTED_EDGE('',*,*,#57129,.F.);
#81440=ORIENTED_EDGE('',*,*,#56380,.F.);
#81441=ORIENTED_EDGE('',*,*,#57128,.T.);
#81442=ORIENTED_EDGE('',*,*,#55257,.F.);
#81443=ORIENTED_EDGE('',*,*,#57130,.F.);
#81444=ORIENTED_EDGE('',*,*,#53903,.F.);
#81445=ORIENTED_EDGE('',*,*,#57129,.T.);
#81446=ORIENTED_EDGE('',*,*,#52196,.F.);
#81447=ORIENTED_EDGE('',*,*,#57131,.F.);
#81448=ORIENTED_EDGE('',*,*,#55237,.F.);
#81449=ORIENTED_EDGE('',*,*,#57130,.T.);
#81450=ORIENTED_EDGE('',*,*,#55256,.F.);
#81451=ORIENTED_EDGE('',*,*,#57132,.F.);
#81452=ORIENTED_EDGE('',*,*,#53921,.F.);
#81453=ORIENTED_EDGE('',*,*,#57131,.T.);
#81454=ORIENTED_EDGE('',*,*,#52195,.F.);
#81455=ORIENTED_EDGE('',*,*,#57133,.F.);
#81456=ORIENTED_EDGE('',*,*,#56382,.F.);
#81457=ORIENTED_EDGE('',*,*,#57132,.T.);
#81458=ORIENTED_EDGE('',*,*,#55255,.F.);
#81459=ORIENTED_EDGE('',*,*,#57134,.F.);
#81460=ORIENTED_EDGE('',*,*,#52468,.F.);
#81461=ORIENTED_EDGE('',*,*,#57133,.T.);
#81462=ORIENTED_EDGE('',*,*,#52194,.F.);
#81463=ORIENTED_EDGE('',*,*,#57135,.F.);
#81464=ORIENTED_EDGE('',*,*,#55243,.F.);
#81465=ORIENTED_EDGE('',*,*,#57134,.T.);
#81466=ORIENTED_EDGE('',*,*,#56381,.F.);
#81467=ORIENTED_EDGE('',*,*,#57136,.F.);
#81468=ORIENTED_EDGE('',*,*,#52469,.F.);
#81469=ORIENTED_EDGE('',*,*,#57135,.T.);
#81470=ORIENTED_EDGE('',*,*,#53952,.F.);
#81471=ORIENTED_EDGE('',*,*,#57137,.F.);
#81472=ORIENTED_EDGE('',*,*,#55244,.F.);
#81473=ORIENTED_EDGE('',*,*,#57136,.T.);
#81474=ORIENTED_EDGE('',*,*,#55239,.F.);
#81475=ORIENTED_EDGE('',*,*,#57138,.F.);
#81476=ORIENTED_EDGE('',*,*,#52470,.F.);
#81477=ORIENTED_EDGE('',*,*,#53947,.F.);
#81478=ORIENTED_EDGE('',*,*,#53943,.T.);
#81479=ORIENTED_EDGE('',*,*,#57139,.F.);
#81480=ORIENTED_EDGE('',*,*,#55245,.F.);
#81481=ORIENTED_EDGE('',*,*,#57137,.T.);
#81482=ORIENTED_EDGE('',*,*,#57138,.T.);
#81483=ORIENTED_EDGE('',*,*,#56383,.F.);
#81484=ORIENTED_EDGE('',*,*,#57140,.F.);
#81485=ORIENTED_EDGE('',*,*,#52471,.F.);
#81486=ORIENTED_EDGE('',*,*,#57139,.T.);
#81487=ORIENTED_EDGE('',*,*,#53942,.F.);
#81488=ORIENTED_EDGE('',*,*,#57141,.F.);
#81489=ORIENTED_EDGE('',*,*,#55246,.F.);
#81490=ORIENTED_EDGE('',*,*,#57140,.T.);
#81491=ORIENTED_EDGE('',*,*,#55241,.F.);
#81492=ORIENTED_EDGE('',*,*,#57142,.F.);
#81493=ORIENTED_EDGE('',*,*,#52472,.F.);
#81494=ORIENTED_EDGE('',*,*,#57141,.T.);
#81495=ORIENTED_EDGE('',*,*,#53954,.F.);
#81496=ORIENTED_EDGE('',*,*,#57143,.F.);
#81497=ORIENTED_EDGE('',*,*,#55247,.F.);
#81498=ORIENTED_EDGE('',*,*,#57142,.T.);
#81499=ORIENTED_EDGE('',*,*,#55240,.F.);
#81500=ORIENTED_EDGE('',*,*,#57144,.F.);
#81501=ORIENTED_EDGE('',*,*,#53950,.F.);
#81502=ORIENTED_EDGE('',*,*,#57143,.T.);
#81503=ORIENTED_EDGE('',*,*,#53938,.F.);
#81504=ORIENTED_EDGE('',*,*,#57145,.F.);
#81505=ORIENTED_EDGE('',*,*,#55248,.F.);
#81506=ORIENTED_EDGE('',*,*,#57144,.T.);
#81507=ORIENTED_EDGE('',*,*,#55251,.F.);
#81508=ORIENTED_EDGE('',*,*,#57146,.F.);
#81509=ORIENTED_EDGE('',*,*,#53929,.F.);
#81510=ORIENTED_EDGE('',*,*,#57145,.T.);
#81511=ORIENTED_EDGE('',*,*,#53956,.F.);
#81512=ORIENTED_EDGE('',*,*,#57147,.F.);
#81513=ORIENTED_EDGE('',*,*,#55249,.F.);
#81514=ORIENTED_EDGE('',*,*,#57146,.T.);
#81515=ORIENTED_EDGE('',*,*,#55250,.F.);
#81516=ORIENTED_EDGE('',*,*,#57147,.T.);
#81517=ORIENTED_EDGE('',*,*,#53934,.F.);
#81518=ORIENTED_EDGE('',*,*,#53930,.T.);
#81519=ORIENTED_EDGE('',*,*,#57148,.F.);
#81520=ORIENTED_EDGE('',*,*,#55290,.F.);
#81521=ORIENTED_EDGE('',*,*,#57149,.F.);
#81522=ORIENTED_EDGE('',*,*,#53886,.F.);
#81523=ORIENTED_EDGE('',*,*,#57149,.T.);
#81524=ORIENTED_EDGE('',*,*,#55289,.F.);
#81525=ORIENTED_EDGE('',*,*,#57150,.F.);
#81526=ORIENTED_EDGE('',*,*,#53895,.F.);
#81527=ORIENTED_EDGE('',*,*,#53885,.T.);
#81528=ORIENTED_EDGE('',*,*,#53889,.F.);
#81529=ORIENTED_EDGE('',*,*,#57151,.F.);
#81530=ORIENTED_EDGE('',*,*,#55291,.F.);
#81531=ORIENTED_EDGE('',*,*,#57148,.T.);
#81532=ORIENTED_EDGE('',*,*,#57150,.T.);
#81533=ORIENTED_EDGE('',*,*,#55288,.F.);
#81534=ORIENTED_EDGE('',*,*,#57152,.F.);
#81535=ORIENTED_EDGE('',*,*,#53880,.F.);
#81536=ORIENTED_EDGE('',*,*,#57151,.T.);
#81537=ORIENTED_EDGE('',*,*,#53893,.F.);
#81538=ORIENTED_EDGE('',*,*,#57153,.F.);
#81539=ORIENTED_EDGE('',*,*,#55280,.F.);
#81540=ORIENTED_EDGE('',*,*,#57152,.T.);
#81541=ORIENTED_EDGE('',*,*,#55287,.F.);
#81542=ORIENTED_EDGE('',*,*,#57154,.F.);
#81543=ORIENTED_EDGE('',*,*,#53897,.F.);
#81544=ORIENTED_EDGE('',*,*,#57153,.T.);
#81545=ORIENTED_EDGE('',*,*,#52204,.F.);
#81546=ORIENTED_EDGE('',*,*,#57155,.F.);
#81547=ORIENTED_EDGE('',*,*,#55281,.F.);
#81548=ORIENTED_EDGE('',*,*,#57154,.T.);
#81549=ORIENTED_EDGE('',*,*,#55286,.F.);
#81550=ORIENTED_EDGE('',*,*,#57156,.F.);
#81551=ORIENTED_EDGE('',*,*,#53872,.T.);
#81552=ORIENTED_EDGE('',*,*,#53876,.F.);
#81553=ORIENTED_EDGE('',*,*,#57155,.T.);
#81554=ORIENTED_EDGE('',*,*,#52203,.F.);
#81555=ORIENTED_EDGE('',*,*,#57157,.F.);
#81556=ORIENTED_EDGE('',*,*,#56384,.F.);
#81557=ORIENTED_EDGE('',*,*,#57156,.T.);
#81558=ORIENTED_EDGE('',*,*,#55285,.F.);
#81559=ORIENTED_EDGE('',*,*,#57158,.F.);
#81560=ORIENTED_EDGE('',*,*,#53873,.F.);
#81561=ORIENTED_EDGE('',*,*,#57157,.T.);
#81562=ORIENTED_EDGE('',*,*,#52202,.F.);
#81563=ORIENTED_EDGE('',*,*,#57159,.F.);
#81564=ORIENTED_EDGE('',*,*,#55265,.F.);
#81565=ORIENTED_EDGE('',*,*,#57158,.T.);
#81566=ORIENTED_EDGE('',*,*,#55284,.F.);
#81567=ORIENTED_EDGE('',*,*,#57160,.F.);
#81568=ORIENTED_EDGE('',*,*,#53891,.F.);
#81569=ORIENTED_EDGE('',*,*,#57159,.T.);
#81570=ORIENTED_EDGE('',*,*,#52201,.F.);
#81571=ORIENTED_EDGE('',*,*,#57161,.F.);
#81572=ORIENTED_EDGE('',*,*,#56386,.F.);
#81573=ORIENTED_EDGE('',*,*,#57160,.T.);
#81574=ORIENTED_EDGE('',*,*,#55283,.F.);
#81575=ORIENTED_EDGE('',*,*,#57162,.F.);
#81576=ORIENTED_EDGE('',*,*,#52462,.F.);
#81577=ORIENTED_EDGE('',*,*,#57161,.T.);
#81578=ORIENTED_EDGE('',*,*,#52200,.F.);
#81579=ORIENTED_EDGE('',*,*,#57163,.F.);
#81580=ORIENTED_EDGE('',*,*,#55271,.F.);
#81581=ORIENTED_EDGE('',*,*,#57162,.T.);
#81582=ORIENTED_EDGE('',*,*,#56385,.F.);
#81583=ORIENTED_EDGE('',*,*,#57164,.F.);
#81584=ORIENTED_EDGE('',*,*,#52463,.F.);
#81585=ORIENTED_EDGE('',*,*,#57163,.T.);
#81586=ORIENTED_EDGE('',*,*,#53922,.F.);
#81587=ORIENTED_EDGE('',*,*,#57165,.F.);
#81588=ORIENTED_EDGE('',*,*,#55272,.F.);
#81589=ORIENTED_EDGE('',*,*,#57164,.T.);
#81590=ORIENTED_EDGE('',*,*,#55267,.F.);
#81591=ORIENTED_EDGE('',*,*,#57166,.F.);
#81592=ORIENTED_EDGE('',*,*,#52464,.F.);
#81593=ORIENTED_EDGE('',*,*,#53917,.F.);
#81594=ORIENTED_EDGE('',*,*,#53913,.T.);
#81595=ORIENTED_EDGE('',*,*,#57167,.F.);
#81596=ORIENTED_EDGE('',*,*,#55273,.F.);
#81597=ORIENTED_EDGE('',*,*,#57165,.T.);
#81598=ORIENTED_EDGE('',*,*,#57166,.T.);
#81599=ORIENTED_EDGE('',*,*,#56387,.F.);
#81600=ORIENTED_EDGE('',*,*,#57168,.F.);
#81601=ORIENTED_EDGE('',*,*,#52465,.F.);
#81602=ORIENTED_EDGE('',*,*,#57167,.T.);
#81603=ORIENTED_EDGE('',*,*,#53912,.F.);
#81604=ORIENTED_EDGE('',*,*,#57169,.F.);
#81605=ORIENTED_EDGE('',*,*,#55274,.F.);
#81606=ORIENTED_EDGE('',*,*,#57168,.T.);
#81607=ORIENTED_EDGE('',*,*,#55269,.F.);
#81608=ORIENTED_EDGE('',*,*,#57170,.F.);
#81609=ORIENTED_EDGE('',*,*,#52466,.F.);
#81610=ORIENTED_EDGE('',*,*,#57169,.T.);
#81611=ORIENTED_EDGE('',*,*,#53924,.F.);
#81612=ORIENTED_EDGE('',*,*,#57171,.F.);
#81613=ORIENTED_EDGE('',*,*,#55275,.F.);
#81614=ORIENTED_EDGE('',*,*,#57170,.T.);
#81615=ORIENTED_EDGE('',*,*,#55268,.F.);
#81616=ORIENTED_EDGE('',*,*,#57172,.F.);
#81617=ORIENTED_EDGE('',*,*,#53920,.F.);
#81618=ORIENTED_EDGE('',*,*,#57171,.T.);
#81619=ORIENTED_EDGE('',*,*,#53908,.F.);
#81620=ORIENTED_EDGE('',*,*,#57173,.F.);
#81621=ORIENTED_EDGE('',*,*,#55276,.F.);
#81622=ORIENTED_EDGE('',*,*,#57172,.T.);
#81623=ORIENTED_EDGE('',*,*,#55279,.F.);
#81624=ORIENTED_EDGE('',*,*,#57174,.F.);
#81625=ORIENTED_EDGE('',*,*,#53899,.F.);
#81626=ORIENTED_EDGE('',*,*,#57173,.T.);
#81627=ORIENTED_EDGE('',*,*,#53926,.F.);
#81628=ORIENTED_EDGE('',*,*,#57175,.F.);
#81629=ORIENTED_EDGE('',*,*,#55277,.F.);
#81630=ORIENTED_EDGE('',*,*,#57174,.T.);
#81631=ORIENTED_EDGE('',*,*,#55278,.F.);
#81632=ORIENTED_EDGE('',*,*,#57175,.T.);
#81633=ORIENTED_EDGE('',*,*,#53904,.F.);
#81634=ORIENTED_EDGE('',*,*,#53900,.T.);
#81635=ORIENTED_EDGE('',*,*,#57176,.F.);
#81636=ORIENTED_EDGE('',*,*,#55318,.F.);
#81637=ORIENTED_EDGE('',*,*,#57177,.F.);
#81638=ORIENTED_EDGE('',*,*,#53856,.F.);
#81639=ORIENTED_EDGE('',*,*,#57177,.T.);
#81640=ORIENTED_EDGE('',*,*,#55317,.F.);
#81641=ORIENTED_EDGE('',*,*,#57178,.F.);
#81642=ORIENTED_EDGE('',*,*,#53865,.F.);
#81643=ORIENTED_EDGE('',*,*,#53855,.T.);
#81644=ORIENTED_EDGE('',*,*,#53859,.F.);
#81645=ORIENTED_EDGE('',*,*,#57179,.F.);
#81646=ORIENTED_EDGE('',*,*,#55319,.F.);
#81647=ORIENTED_EDGE('',*,*,#57176,.T.);
#81648=ORIENTED_EDGE('',*,*,#57178,.T.);
#81649=ORIENTED_EDGE('',*,*,#55316,.F.);
#81650=ORIENTED_EDGE('',*,*,#57180,.F.);
#81651=ORIENTED_EDGE('',*,*,#53850,.F.);
#81652=ORIENTED_EDGE('',*,*,#57179,.T.);
#81653=ORIENTED_EDGE('',*,*,#53863,.F.);
#81654=ORIENTED_EDGE('',*,*,#57181,.F.);
#81655=ORIENTED_EDGE('',*,*,#55308,.F.);
#81656=ORIENTED_EDGE('',*,*,#57180,.T.);
#81657=ORIENTED_EDGE('',*,*,#55315,.F.);
#81658=ORIENTED_EDGE('',*,*,#57182,.F.);
#81659=ORIENTED_EDGE('',*,*,#53867,.F.);
#81660=ORIENTED_EDGE('',*,*,#57181,.T.);
#81661=ORIENTED_EDGE('',*,*,#52210,.F.);
#81662=ORIENTED_EDGE('',*,*,#57183,.F.);
#81663=ORIENTED_EDGE('',*,*,#55309,.F.);
#81664=ORIENTED_EDGE('',*,*,#57182,.T.);
#81665=ORIENTED_EDGE('',*,*,#55314,.F.);
#81666=ORIENTED_EDGE('',*,*,#57184,.F.);
#81667=ORIENTED_EDGE('',*,*,#53842,.T.);
#81668=ORIENTED_EDGE('',*,*,#53846,.F.);
#81669=ORIENTED_EDGE('',*,*,#57183,.T.);
#81670=ORIENTED_EDGE('',*,*,#52209,.F.);
#81671=ORIENTED_EDGE('',*,*,#57185,.F.);
#81672=ORIENTED_EDGE('',*,*,#56388,.F.);
#81673=ORIENTED_EDGE('',*,*,#57184,.T.);
#81674=ORIENTED_EDGE('',*,*,#55313,.F.);
#81675=ORIENTED_EDGE('',*,*,#57186,.F.);
#81676=ORIENTED_EDGE('',*,*,#53843,.F.);
#81677=ORIENTED_EDGE('',*,*,#57185,.T.);
#81678=ORIENTED_EDGE('',*,*,#52208,.F.);
#81679=ORIENTED_EDGE('',*,*,#57187,.F.);
#81680=ORIENTED_EDGE('',*,*,#55293,.F.);
#81681=ORIENTED_EDGE('',*,*,#57186,.T.);
#81682=ORIENTED_EDGE('',*,*,#55312,.F.);
#81683=ORIENTED_EDGE('',*,*,#57188,.F.);
#81684=ORIENTED_EDGE('',*,*,#53861,.F.);
#81685=ORIENTED_EDGE('',*,*,#57187,.T.);
#81686=ORIENTED_EDGE('',*,*,#52207,.F.);
#81687=ORIENTED_EDGE('',*,*,#57189,.F.);
#81688=ORIENTED_EDGE('',*,*,#56390,.F.);
#81689=ORIENTED_EDGE('',*,*,#57188,.T.);
#81690=ORIENTED_EDGE('',*,*,#55311,.F.);
#81691=ORIENTED_EDGE('',*,*,#57190,.F.);
#81692=ORIENTED_EDGE('',*,*,#52456,.F.);
#81693=ORIENTED_EDGE('',*,*,#57189,.T.);
#81694=ORIENTED_EDGE('',*,*,#52206,.F.);
#81695=ORIENTED_EDGE('',*,*,#57191,.F.);
#81696=ORIENTED_EDGE('',*,*,#55299,.F.);
#81697=ORIENTED_EDGE('',*,*,#57190,.T.);
#81698=ORIENTED_EDGE('',*,*,#56389,.F.);
#81699=ORIENTED_EDGE('',*,*,#57192,.F.);
#81700=ORIENTED_EDGE('',*,*,#52457,.F.);
#81701=ORIENTED_EDGE('',*,*,#57191,.T.);
#81702=ORIENTED_EDGE('',*,*,#53892,.F.);
#81703=ORIENTED_EDGE('',*,*,#57193,.F.);
#81704=ORIENTED_EDGE('',*,*,#55300,.F.);
#81705=ORIENTED_EDGE('',*,*,#57192,.T.);
#81706=ORIENTED_EDGE('',*,*,#55295,.F.);
#81707=ORIENTED_EDGE('',*,*,#57194,.F.);
#81708=ORIENTED_EDGE('',*,*,#52458,.F.);
#81709=ORIENTED_EDGE('',*,*,#53887,.F.);
#81710=ORIENTED_EDGE('',*,*,#53883,.T.);
#81711=ORIENTED_EDGE('',*,*,#57195,.F.);
#81712=ORIENTED_EDGE('',*,*,#55301,.F.);
#81713=ORIENTED_EDGE('',*,*,#57193,.T.);
#81714=ORIENTED_EDGE('',*,*,#57194,.T.);
#81715=ORIENTED_EDGE('',*,*,#56391,.F.);
#81716=ORIENTED_EDGE('',*,*,#57196,.F.);
#81717=ORIENTED_EDGE('',*,*,#52459,.F.);
#81718=ORIENTED_EDGE('',*,*,#57195,.T.);
#81719=ORIENTED_EDGE('',*,*,#53882,.F.);
#81720=ORIENTED_EDGE('',*,*,#57197,.F.);
#81721=ORIENTED_EDGE('',*,*,#55302,.F.);
#81722=ORIENTED_EDGE('',*,*,#57196,.T.);
#81723=ORIENTED_EDGE('',*,*,#55297,.F.);
#81724=ORIENTED_EDGE('',*,*,#57198,.F.);
#81725=ORIENTED_EDGE('',*,*,#52460,.F.);
#81726=ORIENTED_EDGE('',*,*,#57197,.T.);
#81727=ORIENTED_EDGE('',*,*,#53894,.F.);
#81728=ORIENTED_EDGE('',*,*,#57199,.F.);
#81729=ORIENTED_EDGE('',*,*,#55303,.F.);
#81730=ORIENTED_EDGE('',*,*,#57198,.T.);
#81731=ORIENTED_EDGE('',*,*,#55296,.F.);
#81732=ORIENTED_EDGE('',*,*,#57200,.F.);
#81733=ORIENTED_EDGE('',*,*,#53890,.F.);
#81734=ORIENTED_EDGE('',*,*,#57199,.T.);
#81735=ORIENTED_EDGE('',*,*,#53878,.F.);
#81736=ORIENTED_EDGE('',*,*,#57201,.F.);
#81737=ORIENTED_EDGE('',*,*,#55304,.F.);
#81738=ORIENTED_EDGE('',*,*,#57200,.T.);
#81739=ORIENTED_EDGE('',*,*,#55307,.F.);
#81740=ORIENTED_EDGE('',*,*,#57202,.F.);
#81741=ORIENTED_EDGE('',*,*,#53869,.F.);
#81742=ORIENTED_EDGE('',*,*,#57201,.T.);
#81743=ORIENTED_EDGE('',*,*,#53896,.F.);
#81744=ORIENTED_EDGE('',*,*,#57203,.F.);
#81745=ORIENTED_EDGE('',*,*,#55305,.F.);
#81746=ORIENTED_EDGE('',*,*,#57202,.T.);
#81747=ORIENTED_EDGE('',*,*,#55306,.F.);
#81748=ORIENTED_EDGE('',*,*,#57203,.T.);
#81749=ORIENTED_EDGE('',*,*,#53874,.F.);
#81750=ORIENTED_EDGE('',*,*,#53870,.T.);
#81751=ORIENTED_EDGE('',*,*,#57204,.F.);
#81752=ORIENTED_EDGE('',*,*,#55346,.F.);
#81753=ORIENTED_EDGE('',*,*,#57205,.F.);
#81754=ORIENTED_EDGE('',*,*,#53826,.F.);
#81755=ORIENTED_EDGE('',*,*,#57205,.T.);
#81756=ORIENTED_EDGE('',*,*,#55345,.F.);
#81757=ORIENTED_EDGE('',*,*,#57206,.F.);
#81758=ORIENTED_EDGE('',*,*,#53835,.F.);
#81759=ORIENTED_EDGE('',*,*,#53825,.T.);
#81760=ORIENTED_EDGE('',*,*,#53829,.F.);
#81761=ORIENTED_EDGE('',*,*,#57207,.F.);
#81762=ORIENTED_EDGE('',*,*,#55347,.F.);
#81763=ORIENTED_EDGE('',*,*,#57204,.T.);
#81764=ORIENTED_EDGE('',*,*,#57206,.T.);
#81765=ORIENTED_EDGE('',*,*,#55344,.F.);
#81766=ORIENTED_EDGE('',*,*,#57208,.F.);
#81767=ORIENTED_EDGE('',*,*,#53820,.F.);
#81768=ORIENTED_EDGE('',*,*,#57207,.T.);
#81769=ORIENTED_EDGE('',*,*,#53833,.F.);
#81770=ORIENTED_EDGE('',*,*,#57209,.F.);
#81771=ORIENTED_EDGE('',*,*,#55336,.F.);
#81772=ORIENTED_EDGE('',*,*,#57208,.T.);
#81773=ORIENTED_EDGE('',*,*,#55343,.F.);
#81774=ORIENTED_EDGE('',*,*,#57210,.F.);
#81775=ORIENTED_EDGE('',*,*,#53837,.F.);
#81776=ORIENTED_EDGE('',*,*,#57209,.T.);
#81777=ORIENTED_EDGE('',*,*,#52216,.F.);
#81778=ORIENTED_EDGE('',*,*,#57211,.F.);
#81779=ORIENTED_EDGE('',*,*,#55337,.F.);
#81780=ORIENTED_EDGE('',*,*,#57210,.T.);
#81781=ORIENTED_EDGE('',*,*,#55342,.F.);
#81782=ORIENTED_EDGE('',*,*,#57212,.F.);
#81783=ORIENTED_EDGE('',*,*,#53812,.T.);
#81784=ORIENTED_EDGE('',*,*,#53816,.F.);
#81785=ORIENTED_EDGE('',*,*,#57211,.T.);
#81786=ORIENTED_EDGE('',*,*,#52215,.F.);
#81787=ORIENTED_EDGE('',*,*,#57213,.F.);
#81788=ORIENTED_EDGE('',*,*,#56392,.F.);
#81789=ORIENTED_EDGE('',*,*,#57212,.T.);
#81790=ORIENTED_EDGE('',*,*,#55341,.F.);
#81791=ORIENTED_EDGE('',*,*,#57214,.F.);
#81792=ORIENTED_EDGE('',*,*,#53813,.F.);
#81793=ORIENTED_EDGE('',*,*,#57213,.T.);
#81794=ORIENTED_EDGE('',*,*,#52214,.F.);
#81795=ORIENTED_EDGE('',*,*,#57215,.F.);
#81796=ORIENTED_EDGE('',*,*,#55321,.F.);
#81797=ORIENTED_EDGE('',*,*,#57214,.T.);
#81798=ORIENTED_EDGE('',*,*,#55340,.F.);
#81799=ORIENTED_EDGE('',*,*,#57216,.F.);
#81800=ORIENTED_EDGE('',*,*,#53831,.F.);
#81801=ORIENTED_EDGE('',*,*,#57215,.T.);
#81802=ORIENTED_EDGE('',*,*,#52213,.F.);
#81803=ORIENTED_EDGE('',*,*,#57217,.F.);
#81804=ORIENTED_EDGE('',*,*,#56394,.F.);
#81805=ORIENTED_EDGE('',*,*,#57216,.T.);
#81806=ORIENTED_EDGE('',*,*,#55339,.F.);
#81807=ORIENTED_EDGE('',*,*,#57218,.F.);
#81808=ORIENTED_EDGE('',*,*,#52450,.F.);
#81809=ORIENTED_EDGE('',*,*,#57217,.T.);
#81810=ORIENTED_EDGE('',*,*,#52212,.F.);
#81811=ORIENTED_EDGE('',*,*,#57219,.F.);
#81812=ORIENTED_EDGE('',*,*,#55327,.F.);
#81813=ORIENTED_EDGE('',*,*,#57218,.T.);
#81814=ORIENTED_EDGE('',*,*,#56393,.F.);
#81815=ORIENTED_EDGE('',*,*,#57220,.F.);
#81816=ORIENTED_EDGE('',*,*,#52451,.F.);
#81817=ORIENTED_EDGE('',*,*,#57219,.T.);
#81818=ORIENTED_EDGE('',*,*,#53862,.F.);
#81819=ORIENTED_EDGE('',*,*,#57221,.F.);
#81820=ORIENTED_EDGE('',*,*,#55328,.F.);
#81821=ORIENTED_EDGE('',*,*,#57220,.T.);
#81822=ORIENTED_EDGE('',*,*,#55323,.F.);
#81823=ORIENTED_EDGE('',*,*,#57222,.F.);
#81824=ORIENTED_EDGE('',*,*,#52452,.F.);
#81825=ORIENTED_EDGE('',*,*,#53857,.F.);
#81826=ORIENTED_EDGE('',*,*,#53853,.T.);
#81827=ORIENTED_EDGE('',*,*,#57223,.F.);
#81828=ORIENTED_EDGE('',*,*,#55329,.F.);
#81829=ORIENTED_EDGE('',*,*,#57221,.T.);
#81830=ORIENTED_EDGE('',*,*,#57222,.T.);
#81831=ORIENTED_EDGE('',*,*,#56395,.F.);
#81832=ORIENTED_EDGE('',*,*,#57224,.F.);
#81833=ORIENTED_EDGE('',*,*,#52453,.F.);
#81834=ORIENTED_EDGE('',*,*,#57223,.T.);
#81835=ORIENTED_EDGE('',*,*,#53852,.F.);
#81836=ORIENTED_EDGE('',*,*,#57225,.F.);
#81837=ORIENTED_EDGE('',*,*,#55330,.F.);
#81838=ORIENTED_EDGE('',*,*,#57224,.T.);
#81839=ORIENTED_EDGE('',*,*,#55325,.F.);
#81840=ORIENTED_EDGE('',*,*,#57226,.F.);
#81841=ORIENTED_EDGE('',*,*,#52454,.F.);
#81842=ORIENTED_EDGE('',*,*,#57225,.T.);
#81843=ORIENTED_EDGE('',*,*,#53864,.F.);
#81844=ORIENTED_EDGE('',*,*,#57227,.F.);
#81845=ORIENTED_EDGE('',*,*,#55331,.F.);
#81846=ORIENTED_EDGE('',*,*,#57226,.T.);
#81847=ORIENTED_EDGE('',*,*,#55324,.F.);
#81848=ORIENTED_EDGE('',*,*,#57228,.F.);
#81849=ORIENTED_EDGE('',*,*,#53860,.F.);
#81850=ORIENTED_EDGE('',*,*,#57227,.T.);
#81851=ORIENTED_EDGE('',*,*,#53848,.F.);
#81852=ORIENTED_EDGE('',*,*,#57229,.F.);
#81853=ORIENTED_EDGE('',*,*,#55332,.F.);
#81854=ORIENTED_EDGE('',*,*,#57228,.T.);
#81855=ORIENTED_EDGE('',*,*,#55335,.F.);
#81856=ORIENTED_EDGE('',*,*,#57230,.F.);
#81857=ORIENTED_EDGE('',*,*,#53839,.F.);
#81858=ORIENTED_EDGE('',*,*,#57229,.T.);
#81859=ORIENTED_EDGE('',*,*,#53866,.F.);
#81860=ORIENTED_EDGE('',*,*,#57231,.F.);
#81861=ORIENTED_EDGE('',*,*,#55333,.F.);
#81862=ORIENTED_EDGE('',*,*,#57230,.T.);
#81863=ORIENTED_EDGE('',*,*,#55334,.F.);
#81864=ORIENTED_EDGE('',*,*,#57231,.T.);
#81865=ORIENTED_EDGE('',*,*,#53844,.F.);
#81866=ORIENTED_EDGE('',*,*,#53840,.T.);
#81867=ORIENTED_EDGE('',*,*,#57232,.F.);
#81868=ORIENTED_EDGE('',*,*,#55374,.F.);
#81869=ORIENTED_EDGE('',*,*,#57233,.F.);
#81870=ORIENTED_EDGE('',*,*,#53796,.F.);
#81871=ORIENTED_EDGE('',*,*,#57233,.T.);
#81872=ORIENTED_EDGE('',*,*,#55373,.F.);
#81873=ORIENTED_EDGE('',*,*,#57234,.F.);
#81874=ORIENTED_EDGE('',*,*,#53805,.F.);
#81875=ORIENTED_EDGE('',*,*,#53795,.T.);
#81876=ORIENTED_EDGE('',*,*,#53799,.F.);
#81877=ORIENTED_EDGE('',*,*,#57235,.F.);
#81878=ORIENTED_EDGE('',*,*,#55375,.F.);
#81879=ORIENTED_EDGE('',*,*,#57232,.T.);
#81880=ORIENTED_EDGE('',*,*,#57234,.T.);
#81881=ORIENTED_EDGE('',*,*,#55372,.F.);
#81882=ORIENTED_EDGE('',*,*,#57236,.F.);
#81883=ORIENTED_EDGE('',*,*,#53790,.F.);
#81884=ORIENTED_EDGE('',*,*,#57235,.T.);
#81885=ORIENTED_EDGE('',*,*,#53803,.F.);
#81886=ORIENTED_EDGE('',*,*,#57237,.F.);
#81887=ORIENTED_EDGE('',*,*,#55364,.F.);
#81888=ORIENTED_EDGE('',*,*,#57236,.T.);
#81889=ORIENTED_EDGE('',*,*,#55371,.F.);
#81890=ORIENTED_EDGE('',*,*,#57238,.F.);
#81891=ORIENTED_EDGE('',*,*,#53807,.F.);
#81892=ORIENTED_EDGE('',*,*,#57237,.T.);
#81893=ORIENTED_EDGE('',*,*,#52222,.F.);
#81894=ORIENTED_EDGE('',*,*,#57239,.F.);
#81895=ORIENTED_EDGE('',*,*,#55365,.F.);
#81896=ORIENTED_EDGE('',*,*,#57238,.T.);
#81897=ORIENTED_EDGE('',*,*,#55370,.F.);
#81898=ORIENTED_EDGE('',*,*,#57240,.F.);
#81899=ORIENTED_EDGE('',*,*,#53782,.T.);
#81900=ORIENTED_EDGE('',*,*,#53786,.F.);
#81901=ORIENTED_EDGE('',*,*,#57239,.T.);
#81902=ORIENTED_EDGE('',*,*,#52221,.F.);
#81903=ORIENTED_EDGE('',*,*,#57241,.F.);
#81904=ORIENTED_EDGE('',*,*,#56396,.F.);
#81905=ORIENTED_EDGE('',*,*,#57240,.T.);
#81906=ORIENTED_EDGE('',*,*,#55369,.F.);
#81907=ORIENTED_EDGE('',*,*,#57242,.F.);
#81908=ORIENTED_EDGE('',*,*,#53783,.F.);
#81909=ORIENTED_EDGE('',*,*,#57241,.T.);
#81910=ORIENTED_EDGE('',*,*,#52220,.F.);
#81911=ORIENTED_EDGE('',*,*,#57243,.F.);
#81912=ORIENTED_EDGE('',*,*,#55349,.F.);
#81913=ORIENTED_EDGE('',*,*,#57242,.T.);
#81914=ORIENTED_EDGE('',*,*,#55368,.F.);
#81915=ORIENTED_EDGE('',*,*,#57244,.F.);
#81916=ORIENTED_EDGE('',*,*,#53801,.F.);
#81917=ORIENTED_EDGE('',*,*,#57243,.T.);
#81918=ORIENTED_EDGE('',*,*,#52219,.F.);
#81919=ORIENTED_EDGE('',*,*,#57245,.F.);
#81920=ORIENTED_EDGE('',*,*,#56398,.F.);
#81921=ORIENTED_EDGE('',*,*,#57244,.T.);
#81922=ORIENTED_EDGE('',*,*,#55367,.F.);
#81923=ORIENTED_EDGE('',*,*,#57246,.F.);
#81924=ORIENTED_EDGE('',*,*,#52444,.F.);
#81925=ORIENTED_EDGE('',*,*,#57245,.T.);
#81926=ORIENTED_EDGE('',*,*,#52218,.F.);
#81927=ORIENTED_EDGE('',*,*,#57247,.F.);
#81928=ORIENTED_EDGE('',*,*,#55355,.F.);
#81929=ORIENTED_EDGE('',*,*,#57246,.T.);
#81930=ORIENTED_EDGE('',*,*,#56397,.F.);
#81931=ORIENTED_EDGE('',*,*,#57248,.F.);
#81932=ORIENTED_EDGE('',*,*,#52445,.F.);
#81933=ORIENTED_EDGE('',*,*,#57247,.T.);
#81934=ORIENTED_EDGE('',*,*,#53832,.F.);
#81935=ORIENTED_EDGE('',*,*,#57249,.F.);
#81936=ORIENTED_EDGE('',*,*,#55356,.F.);
#81937=ORIENTED_EDGE('',*,*,#57248,.T.);
#81938=ORIENTED_EDGE('',*,*,#55351,.F.);
#81939=ORIENTED_EDGE('',*,*,#57250,.F.);
#81940=ORIENTED_EDGE('',*,*,#52446,.F.);
#81941=ORIENTED_EDGE('',*,*,#53827,.F.);
#81942=ORIENTED_EDGE('',*,*,#53823,.T.);
#81943=ORIENTED_EDGE('',*,*,#57251,.F.);
#81944=ORIENTED_EDGE('',*,*,#55357,.F.);
#81945=ORIENTED_EDGE('',*,*,#57249,.T.);
#81946=ORIENTED_EDGE('',*,*,#57250,.T.);
#81947=ORIENTED_EDGE('',*,*,#56399,.F.);
#81948=ORIENTED_EDGE('',*,*,#57252,.F.);
#81949=ORIENTED_EDGE('',*,*,#52447,.F.);
#81950=ORIENTED_EDGE('',*,*,#57251,.T.);
#81951=ORIENTED_EDGE('',*,*,#53822,.F.);
#81952=ORIENTED_EDGE('',*,*,#57253,.F.);
#81953=ORIENTED_EDGE('',*,*,#55358,.F.);
#81954=ORIENTED_EDGE('',*,*,#57252,.T.);
#81955=ORIENTED_EDGE('',*,*,#55353,.F.);
#81956=ORIENTED_EDGE('',*,*,#57254,.F.);
#81957=ORIENTED_EDGE('',*,*,#52448,.F.);
#81958=ORIENTED_EDGE('',*,*,#57253,.T.);
#81959=ORIENTED_EDGE('',*,*,#53834,.F.);
#81960=ORIENTED_EDGE('',*,*,#57255,.F.);
#81961=ORIENTED_EDGE('',*,*,#55359,.F.);
#81962=ORIENTED_EDGE('',*,*,#57254,.T.);
#81963=ORIENTED_EDGE('',*,*,#55352,.F.);
#81964=ORIENTED_EDGE('',*,*,#57256,.F.);
#81965=ORIENTED_EDGE('',*,*,#53830,.F.);
#81966=ORIENTED_EDGE('',*,*,#57255,.T.);
#81967=ORIENTED_EDGE('',*,*,#53818,.F.);
#81968=ORIENTED_EDGE('',*,*,#57257,.F.);
#81969=ORIENTED_EDGE('',*,*,#55360,.F.);
#81970=ORIENTED_EDGE('',*,*,#57256,.T.);
#81971=ORIENTED_EDGE('',*,*,#55363,.F.);
#81972=ORIENTED_EDGE('',*,*,#57258,.F.);
#81973=ORIENTED_EDGE('',*,*,#53809,.F.);
#81974=ORIENTED_EDGE('',*,*,#57257,.T.);
#81975=ORIENTED_EDGE('',*,*,#53836,.F.);
#81976=ORIENTED_EDGE('',*,*,#57259,.F.);
#81977=ORIENTED_EDGE('',*,*,#55361,.F.);
#81978=ORIENTED_EDGE('',*,*,#57258,.T.);
#81979=ORIENTED_EDGE('',*,*,#55362,.F.);
#81980=ORIENTED_EDGE('',*,*,#57259,.T.);
#81981=ORIENTED_EDGE('',*,*,#53814,.F.);
#81982=ORIENTED_EDGE('',*,*,#53810,.T.);
#81983=ORIENTED_EDGE('',*,*,#57260,.F.);
#81984=ORIENTED_EDGE('',*,*,#55402,.F.);
#81985=ORIENTED_EDGE('',*,*,#57261,.F.);
#81986=ORIENTED_EDGE('',*,*,#53766,.F.);
#81987=ORIENTED_EDGE('',*,*,#57261,.T.);
#81988=ORIENTED_EDGE('',*,*,#55401,.F.);
#81989=ORIENTED_EDGE('',*,*,#57262,.F.);
#81990=ORIENTED_EDGE('',*,*,#53775,.F.);
#81991=ORIENTED_EDGE('',*,*,#53765,.T.);
#81992=ORIENTED_EDGE('',*,*,#53769,.F.);
#81993=ORIENTED_EDGE('',*,*,#57263,.F.);
#81994=ORIENTED_EDGE('',*,*,#55403,.F.);
#81995=ORIENTED_EDGE('',*,*,#57260,.T.);
#81996=ORIENTED_EDGE('',*,*,#57262,.T.);
#81997=ORIENTED_EDGE('',*,*,#55400,.F.);
#81998=ORIENTED_EDGE('',*,*,#57264,.F.);
#81999=ORIENTED_EDGE('',*,*,#53760,.F.);
#82000=ORIENTED_EDGE('',*,*,#57263,.T.);
#82001=ORIENTED_EDGE('',*,*,#53773,.F.);
#82002=ORIENTED_EDGE('',*,*,#57265,.F.);
#82003=ORIENTED_EDGE('',*,*,#55392,.F.);
#82004=ORIENTED_EDGE('',*,*,#57264,.T.);
#82005=ORIENTED_EDGE('',*,*,#55399,.F.);
#82006=ORIENTED_EDGE('',*,*,#57266,.F.);
#82007=ORIENTED_EDGE('',*,*,#53777,.F.);
#82008=ORIENTED_EDGE('',*,*,#57265,.T.);
#82009=ORIENTED_EDGE('',*,*,#52228,.F.);
#82010=ORIENTED_EDGE('',*,*,#57267,.F.);
#82011=ORIENTED_EDGE('',*,*,#55393,.F.);
#82012=ORIENTED_EDGE('',*,*,#57266,.T.);
#82013=ORIENTED_EDGE('',*,*,#55398,.F.);
#82014=ORIENTED_EDGE('',*,*,#57268,.F.);
#82015=ORIENTED_EDGE('',*,*,#53752,.T.);
#82016=ORIENTED_EDGE('',*,*,#53756,.F.);
#82017=ORIENTED_EDGE('',*,*,#57267,.T.);
#82018=ORIENTED_EDGE('',*,*,#52227,.F.);
#82019=ORIENTED_EDGE('',*,*,#57269,.F.);
#82020=ORIENTED_EDGE('',*,*,#56400,.F.);
#82021=ORIENTED_EDGE('',*,*,#57268,.T.);
#82022=ORIENTED_EDGE('',*,*,#55397,.F.);
#82023=ORIENTED_EDGE('',*,*,#57270,.F.);
#82024=ORIENTED_EDGE('',*,*,#53753,.F.);
#82025=ORIENTED_EDGE('',*,*,#57269,.T.);
#82026=ORIENTED_EDGE('',*,*,#52226,.F.);
#82027=ORIENTED_EDGE('',*,*,#57271,.F.);
#82028=ORIENTED_EDGE('',*,*,#55377,.F.);
#82029=ORIENTED_EDGE('',*,*,#57270,.T.);
#82030=ORIENTED_EDGE('',*,*,#55396,.F.);
#82031=ORIENTED_EDGE('',*,*,#57272,.F.);
#82032=ORIENTED_EDGE('',*,*,#53771,.F.);
#82033=ORIENTED_EDGE('',*,*,#57271,.T.);
#82034=ORIENTED_EDGE('',*,*,#52225,.F.);
#82035=ORIENTED_EDGE('',*,*,#57273,.F.);
#82036=ORIENTED_EDGE('',*,*,#56402,.F.);
#82037=ORIENTED_EDGE('',*,*,#57272,.T.);
#82038=ORIENTED_EDGE('',*,*,#55395,.F.);
#82039=ORIENTED_EDGE('',*,*,#57274,.F.);
#82040=ORIENTED_EDGE('',*,*,#52438,.F.);
#82041=ORIENTED_EDGE('',*,*,#57273,.T.);
#82042=ORIENTED_EDGE('',*,*,#52224,.F.);
#82043=ORIENTED_EDGE('',*,*,#57275,.F.);
#82044=ORIENTED_EDGE('',*,*,#55383,.F.);
#82045=ORIENTED_EDGE('',*,*,#57274,.T.);
#82046=ORIENTED_EDGE('',*,*,#56401,.F.);
#82047=ORIENTED_EDGE('',*,*,#57276,.F.);
#82048=ORIENTED_EDGE('',*,*,#52439,.F.);
#82049=ORIENTED_EDGE('',*,*,#57275,.T.);
#82050=ORIENTED_EDGE('',*,*,#53802,.F.);
#82051=ORIENTED_EDGE('',*,*,#57277,.F.);
#82052=ORIENTED_EDGE('',*,*,#55384,.F.);
#82053=ORIENTED_EDGE('',*,*,#57276,.T.);
#82054=ORIENTED_EDGE('',*,*,#55379,.F.);
#82055=ORIENTED_EDGE('',*,*,#57278,.F.);
#82056=ORIENTED_EDGE('',*,*,#52440,.F.);
#82057=ORIENTED_EDGE('',*,*,#53797,.F.);
#82058=ORIENTED_EDGE('',*,*,#53793,.T.);
#82059=ORIENTED_EDGE('',*,*,#57279,.F.);
#82060=ORIENTED_EDGE('',*,*,#55385,.F.);
#82061=ORIENTED_EDGE('',*,*,#57277,.T.);
#82062=ORIENTED_EDGE('',*,*,#57278,.T.);
#82063=ORIENTED_EDGE('',*,*,#56403,.F.);
#82064=ORIENTED_EDGE('',*,*,#57280,.F.);
#82065=ORIENTED_EDGE('',*,*,#52441,.F.);
#82066=ORIENTED_EDGE('',*,*,#57279,.T.);
#82067=ORIENTED_EDGE('',*,*,#53792,.F.);
#82068=ORIENTED_EDGE('',*,*,#57281,.F.);
#82069=ORIENTED_EDGE('',*,*,#55386,.F.);
#82070=ORIENTED_EDGE('',*,*,#57280,.T.);
#82071=ORIENTED_EDGE('',*,*,#55381,.F.);
#82072=ORIENTED_EDGE('',*,*,#57282,.F.);
#82073=ORIENTED_EDGE('',*,*,#52442,.F.);
#82074=ORIENTED_EDGE('',*,*,#57281,.T.);
#82075=ORIENTED_EDGE('',*,*,#53804,.F.);
#82076=ORIENTED_EDGE('',*,*,#57283,.F.);
#82077=ORIENTED_EDGE('',*,*,#55387,.F.);
#82078=ORIENTED_EDGE('',*,*,#57282,.T.);
#82079=ORIENTED_EDGE('',*,*,#55380,.F.);
#82080=ORIENTED_EDGE('',*,*,#57284,.F.);
#82081=ORIENTED_EDGE('',*,*,#53800,.F.);
#82082=ORIENTED_EDGE('',*,*,#57283,.T.);
#82083=ORIENTED_EDGE('',*,*,#53788,.F.);
#82084=ORIENTED_EDGE('',*,*,#57285,.F.);
#82085=ORIENTED_EDGE('',*,*,#55388,.F.);
#82086=ORIENTED_EDGE('',*,*,#57284,.T.);
#82087=ORIENTED_EDGE('',*,*,#55391,.F.);
#82088=ORIENTED_EDGE('',*,*,#57286,.F.);
#82089=ORIENTED_EDGE('',*,*,#53779,.F.);
#82090=ORIENTED_EDGE('',*,*,#57285,.T.);
#82091=ORIENTED_EDGE('',*,*,#53806,.F.);
#82092=ORIENTED_EDGE('',*,*,#57287,.F.);
#82093=ORIENTED_EDGE('',*,*,#55389,.F.);
#82094=ORIENTED_EDGE('',*,*,#57286,.T.);
#82095=ORIENTED_EDGE('',*,*,#55390,.F.);
#82096=ORIENTED_EDGE('',*,*,#57287,.T.);
#82097=ORIENTED_EDGE('',*,*,#53784,.F.);
#82098=ORIENTED_EDGE('',*,*,#53780,.T.);
#82099=ORIENTED_EDGE('',*,*,#57288,.F.);
#82100=ORIENTED_EDGE('',*,*,#55430,.F.);
#82101=ORIENTED_EDGE('',*,*,#57289,.F.);
#82102=ORIENTED_EDGE('',*,*,#53736,.F.);
#82103=ORIENTED_EDGE('',*,*,#57289,.T.);
#82104=ORIENTED_EDGE('',*,*,#55429,.F.);
#82105=ORIENTED_EDGE('',*,*,#57290,.F.);
#82106=ORIENTED_EDGE('',*,*,#53745,.F.);
#82107=ORIENTED_EDGE('',*,*,#53735,.T.);
#82108=ORIENTED_EDGE('',*,*,#53739,.F.);
#82109=ORIENTED_EDGE('',*,*,#57291,.F.);
#82110=ORIENTED_EDGE('',*,*,#55431,.F.);
#82111=ORIENTED_EDGE('',*,*,#57288,.T.);
#82112=ORIENTED_EDGE('',*,*,#57290,.T.);
#82113=ORIENTED_EDGE('',*,*,#55428,.F.);
#82114=ORIENTED_EDGE('',*,*,#57292,.F.);
#82115=ORIENTED_EDGE('',*,*,#53730,.F.);
#82116=ORIENTED_EDGE('',*,*,#57291,.T.);
#82117=ORIENTED_EDGE('',*,*,#53743,.F.);
#82118=ORIENTED_EDGE('',*,*,#57293,.F.);
#82119=ORIENTED_EDGE('',*,*,#55420,.F.);
#82120=ORIENTED_EDGE('',*,*,#57292,.T.);
#82121=ORIENTED_EDGE('',*,*,#55427,.F.);
#82122=ORIENTED_EDGE('',*,*,#57294,.F.);
#82123=ORIENTED_EDGE('',*,*,#53747,.F.);
#82124=ORIENTED_EDGE('',*,*,#57293,.T.);
#82125=ORIENTED_EDGE('',*,*,#52234,.F.);
#82126=ORIENTED_EDGE('',*,*,#57295,.F.);
#82127=ORIENTED_EDGE('',*,*,#55421,.F.);
#82128=ORIENTED_EDGE('',*,*,#57294,.T.);
#82129=ORIENTED_EDGE('',*,*,#55426,.F.);
#82130=ORIENTED_EDGE('',*,*,#57296,.F.);
#82131=ORIENTED_EDGE('',*,*,#53722,.T.);
#82132=ORIENTED_EDGE('',*,*,#53726,.F.);
#82133=ORIENTED_EDGE('',*,*,#57295,.T.);
#82134=ORIENTED_EDGE('',*,*,#52233,.F.);
#82135=ORIENTED_EDGE('',*,*,#57297,.F.);
#82136=ORIENTED_EDGE('',*,*,#56404,.F.);
#82137=ORIENTED_EDGE('',*,*,#57296,.T.);
#82138=ORIENTED_EDGE('',*,*,#55425,.F.);
#82139=ORIENTED_EDGE('',*,*,#57298,.F.);
#82140=ORIENTED_EDGE('',*,*,#53723,.F.);
#82141=ORIENTED_EDGE('',*,*,#57297,.T.);
#82142=ORIENTED_EDGE('',*,*,#52232,.F.);
#82143=ORIENTED_EDGE('',*,*,#57299,.F.);
#82144=ORIENTED_EDGE('',*,*,#55405,.F.);
#82145=ORIENTED_EDGE('',*,*,#57298,.T.);
#82146=ORIENTED_EDGE('',*,*,#55424,.F.);
#82147=ORIENTED_EDGE('',*,*,#57300,.F.);
#82148=ORIENTED_EDGE('',*,*,#53741,.F.);
#82149=ORIENTED_EDGE('',*,*,#57299,.T.);
#82150=ORIENTED_EDGE('',*,*,#52231,.F.);
#82151=ORIENTED_EDGE('',*,*,#57301,.F.);
#82152=ORIENTED_EDGE('',*,*,#56406,.F.);
#82153=ORIENTED_EDGE('',*,*,#57300,.T.);
#82154=ORIENTED_EDGE('',*,*,#55423,.F.);
#82155=ORIENTED_EDGE('',*,*,#57302,.F.);
#82156=ORIENTED_EDGE('',*,*,#52432,.F.);
#82157=ORIENTED_EDGE('',*,*,#57301,.T.);
#82158=ORIENTED_EDGE('',*,*,#52230,.F.);
#82159=ORIENTED_EDGE('',*,*,#57303,.F.);
#82160=ORIENTED_EDGE('',*,*,#55411,.F.);
#82161=ORIENTED_EDGE('',*,*,#57302,.T.);
#82162=ORIENTED_EDGE('',*,*,#56405,.F.);
#82163=ORIENTED_EDGE('',*,*,#57304,.F.);
#82164=ORIENTED_EDGE('',*,*,#52433,.F.);
#82165=ORIENTED_EDGE('',*,*,#57303,.T.);
#82166=ORIENTED_EDGE('',*,*,#53772,.F.);
#82167=ORIENTED_EDGE('',*,*,#57305,.F.);
#82168=ORIENTED_EDGE('',*,*,#55412,.F.);
#82169=ORIENTED_EDGE('',*,*,#57304,.T.);
#82170=ORIENTED_EDGE('',*,*,#55407,.F.);
#82171=ORIENTED_EDGE('',*,*,#57306,.F.);
#82172=ORIENTED_EDGE('',*,*,#52434,.F.);
#82173=ORIENTED_EDGE('',*,*,#53767,.F.);
#82174=ORIENTED_EDGE('',*,*,#53763,.T.);
#82175=ORIENTED_EDGE('',*,*,#57307,.F.);
#82176=ORIENTED_EDGE('',*,*,#55413,.F.);
#82177=ORIENTED_EDGE('',*,*,#57305,.T.);
#82178=ORIENTED_EDGE('',*,*,#57306,.T.);
#82179=ORIENTED_EDGE('',*,*,#56407,.F.);
#82180=ORIENTED_EDGE('',*,*,#57308,.F.);
#82181=ORIENTED_EDGE('',*,*,#52435,.F.);
#82182=ORIENTED_EDGE('',*,*,#57307,.T.);
#82183=ORIENTED_EDGE('',*,*,#53762,.F.);
#82184=ORIENTED_EDGE('',*,*,#57309,.F.);
#82185=ORIENTED_EDGE('',*,*,#55414,.F.);
#82186=ORIENTED_EDGE('',*,*,#57308,.T.);
#82187=ORIENTED_EDGE('',*,*,#55409,.F.);
#82188=ORIENTED_EDGE('',*,*,#57310,.F.);
#82189=ORIENTED_EDGE('',*,*,#52436,.F.);
#82190=ORIENTED_EDGE('',*,*,#57309,.T.);
#82191=ORIENTED_EDGE('',*,*,#53774,.F.);
#82192=ORIENTED_EDGE('',*,*,#57311,.F.);
#82193=ORIENTED_EDGE('',*,*,#55415,.F.);
#82194=ORIENTED_EDGE('',*,*,#57310,.T.);
#82195=ORIENTED_EDGE('',*,*,#55408,.F.);
#82196=ORIENTED_EDGE('',*,*,#57312,.F.);
#82197=ORIENTED_EDGE('',*,*,#53770,.F.);
#82198=ORIENTED_EDGE('',*,*,#57311,.T.);
#82199=ORIENTED_EDGE('',*,*,#53758,.F.);
#82200=ORIENTED_EDGE('',*,*,#57313,.F.);
#82201=ORIENTED_EDGE('',*,*,#55416,.F.);
#82202=ORIENTED_EDGE('',*,*,#57312,.T.);
#82203=ORIENTED_EDGE('',*,*,#55419,.F.);
#82204=ORIENTED_EDGE('',*,*,#57314,.F.);
#82205=ORIENTED_EDGE('',*,*,#53749,.F.);
#82206=ORIENTED_EDGE('',*,*,#57313,.T.);
#82207=ORIENTED_EDGE('',*,*,#53776,.F.);
#82208=ORIENTED_EDGE('',*,*,#57315,.F.);
#82209=ORIENTED_EDGE('',*,*,#55417,.F.);
#82210=ORIENTED_EDGE('',*,*,#57314,.T.);
#82211=ORIENTED_EDGE('',*,*,#55418,.F.);
#82212=ORIENTED_EDGE('',*,*,#57315,.T.);
#82213=ORIENTED_EDGE('',*,*,#53754,.F.);
#82214=ORIENTED_EDGE('',*,*,#53750,.T.);
#82215=ORIENTED_EDGE('',*,*,#57316,.F.);
#82216=ORIENTED_EDGE('',*,*,#55458,.F.);
#82217=ORIENTED_EDGE('',*,*,#57317,.F.);
#82218=ORIENTED_EDGE('',*,*,#53706,.F.);
#82219=ORIENTED_EDGE('',*,*,#57317,.T.);
#82220=ORIENTED_EDGE('',*,*,#55457,.F.);
#82221=ORIENTED_EDGE('',*,*,#57318,.F.);
#82222=ORIENTED_EDGE('',*,*,#53715,.F.);
#82223=ORIENTED_EDGE('',*,*,#53705,.T.);
#82224=ORIENTED_EDGE('',*,*,#53709,.F.);
#82225=ORIENTED_EDGE('',*,*,#57319,.F.);
#82226=ORIENTED_EDGE('',*,*,#55459,.F.);
#82227=ORIENTED_EDGE('',*,*,#57316,.T.);
#82228=ORIENTED_EDGE('',*,*,#57318,.T.);
#82229=ORIENTED_EDGE('',*,*,#55456,.F.);
#82230=ORIENTED_EDGE('',*,*,#57320,.F.);
#82231=ORIENTED_EDGE('',*,*,#53700,.F.);
#82232=ORIENTED_EDGE('',*,*,#57319,.T.);
#82233=ORIENTED_EDGE('',*,*,#53713,.F.);
#82234=ORIENTED_EDGE('',*,*,#57321,.F.);
#82235=ORIENTED_EDGE('',*,*,#55448,.F.);
#82236=ORIENTED_EDGE('',*,*,#57320,.T.);
#82237=ORIENTED_EDGE('',*,*,#55455,.F.);
#82238=ORIENTED_EDGE('',*,*,#57322,.F.);
#82239=ORIENTED_EDGE('',*,*,#53717,.F.);
#82240=ORIENTED_EDGE('',*,*,#57321,.T.);
#82241=ORIENTED_EDGE('',*,*,#52240,.F.);
#82242=ORIENTED_EDGE('',*,*,#57323,.F.);
#82243=ORIENTED_EDGE('',*,*,#55449,.F.);
#82244=ORIENTED_EDGE('',*,*,#57322,.T.);
#82245=ORIENTED_EDGE('',*,*,#55454,.F.);
#82246=ORIENTED_EDGE('',*,*,#57324,.F.);
#82247=ORIENTED_EDGE('',*,*,#53692,.T.);
#82248=ORIENTED_EDGE('',*,*,#53696,.F.);
#82249=ORIENTED_EDGE('',*,*,#57323,.T.);
#82250=ORIENTED_EDGE('',*,*,#52239,.F.);
#82251=ORIENTED_EDGE('',*,*,#57325,.F.);
#82252=ORIENTED_EDGE('',*,*,#56408,.F.);
#82253=ORIENTED_EDGE('',*,*,#57324,.T.);
#82254=ORIENTED_EDGE('',*,*,#55453,.F.);
#82255=ORIENTED_EDGE('',*,*,#57326,.F.);
#82256=ORIENTED_EDGE('',*,*,#53693,.F.);
#82257=ORIENTED_EDGE('',*,*,#57325,.T.);
#82258=ORIENTED_EDGE('',*,*,#52238,.F.);
#82259=ORIENTED_EDGE('',*,*,#57327,.F.);
#82260=ORIENTED_EDGE('',*,*,#55433,.F.);
#82261=ORIENTED_EDGE('',*,*,#57326,.T.);
#82262=ORIENTED_EDGE('',*,*,#55452,.F.);
#82263=ORIENTED_EDGE('',*,*,#57328,.F.);
#82264=ORIENTED_EDGE('',*,*,#53711,.F.);
#82265=ORIENTED_EDGE('',*,*,#57327,.T.);
#82266=ORIENTED_EDGE('',*,*,#52237,.F.);
#82267=ORIENTED_EDGE('',*,*,#57329,.F.);
#82268=ORIENTED_EDGE('',*,*,#56410,.F.);
#82269=ORIENTED_EDGE('',*,*,#57328,.T.);
#82270=ORIENTED_EDGE('',*,*,#55451,.F.);
#82271=ORIENTED_EDGE('',*,*,#57330,.F.);
#82272=ORIENTED_EDGE('',*,*,#52426,.F.);
#82273=ORIENTED_EDGE('',*,*,#57329,.T.);
#82274=ORIENTED_EDGE('',*,*,#52236,.F.);
#82275=ORIENTED_EDGE('',*,*,#57331,.F.);
#82276=ORIENTED_EDGE('',*,*,#55439,.F.);
#82277=ORIENTED_EDGE('',*,*,#57330,.T.);
#82278=ORIENTED_EDGE('',*,*,#56409,.F.);
#82279=ORIENTED_EDGE('',*,*,#57332,.F.);
#82280=ORIENTED_EDGE('',*,*,#52427,.F.);
#82281=ORIENTED_EDGE('',*,*,#57331,.T.);
#82282=ORIENTED_EDGE('',*,*,#53742,.F.);
#82283=ORIENTED_EDGE('',*,*,#57333,.F.);
#82284=ORIENTED_EDGE('',*,*,#55440,.F.);
#82285=ORIENTED_EDGE('',*,*,#57332,.T.);
#82286=ORIENTED_EDGE('',*,*,#55435,.F.);
#82287=ORIENTED_EDGE('',*,*,#57334,.F.);
#82288=ORIENTED_EDGE('',*,*,#52428,.F.);
#82289=ORIENTED_EDGE('',*,*,#53737,.F.);
#82290=ORIENTED_EDGE('',*,*,#53733,.T.);
#82291=ORIENTED_EDGE('',*,*,#57335,.F.);
#82292=ORIENTED_EDGE('',*,*,#55441,.F.);
#82293=ORIENTED_EDGE('',*,*,#57333,.T.);
#82294=ORIENTED_EDGE('',*,*,#57334,.T.);
#82295=ORIENTED_EDGE('',*,*,#56411,.F.);
#82296=ORIENTED_EDGE('',*,*,#57336,.F.);
#82297=ORIENTED_EDGE('',*,*,#52429,.F.);
#82298=ORIENTED_EDGE('',*,*,#57335,.T.);
#82299=ORIENTED_EDGE('',*,*,#53732,.F.);
#82300=ORIENTED_EDGE('',*,*,#57337,.F.);
#82301=ORIENTED_EDGE('',*,*,#55442,.F.);
#82302=ORIENTED_EDGE('',*,*,#57336,.T.);
#82303=ORIENTED_EDGE('',*,*,#55437,.F.);
#82304=ORIENTED_EDGE('',*,*,#57338,.F.);
#82305=ORIENTED_EDGE('',*,*,#52430,.F.);
#82306=ORIENTED_EDGE('',*,*,#57337,.T.);
#82307=ORIENTED_EDGE('',*,*,#53744,.F.);
#82308=ORIENTED_EDGE('',*,*,#57339,.F.);
#82309=ORIENTED_EDGE('',*,*,#55443,.F.);
#82310=ORIENTED_EDGE('',*,*,#57338,.T.);
#82311=ORIENTED_EDGE('',*,*,#55436,.F.);
#82312=ORIENTED_EDGE('',*,*,#57340,.F.);
#82313=ORIENTED_EDGE('',*,*,#53740,.F.);
#82314=ORIENTED_EDGE('',*,*,#57339,.T.);
#82315=ORIENTED_EDGE('',*,*,#53728,.F.);
#82316=ORIENTED_EDGE('',*,*,#57341,.F.);
#82317=ORIENTED_EDGE('',*,*,#55444,.F.);
#82318=ORIENTED_EDGE('',*,*,#57340,.T.);
#82319=ORIENTED_EDGE('',*,*,#55447,.F.);
#82320=ORIENTED_EDGE('',*,*,#57342,.F.);
#82321=ORIENTED_EDGE('',*,*,#53719,.F.);
#82322=ORIENTED_EDGE('',*,*,#57341,.T.);
#82323=ORIENTED_EDGE('',*,*,#53746,.F.);
#82324=ORIENTED_EDGE('',*,*,#57343,.F.);
#82325=ORIENTED_EDGE('',*,*,#55445,.F.);
#82326=ORIENTED_EDGE('',*,*,#57342,.T.);
#82327=ORIENTED_EDGE('',*,*,#55446,.F.);
#82328=ORIENTED_EDGE('',*,*,#57343,.T.);
#82329=ORIENTED_EDGE('',*,*,#53724,.F.);
#82330=ORIENTED_EDGE('',*,*,#53720,.T.);
#82331=ORIENTED_EDGE('',*,*,#57344,.F.);
#82332=ORIENTED_EDGE('',*,*,#55484,.F.);
#82333=ORIENTED_EDGE('',*,*,#57345,.F.);
#82334=ORIENTED_EDGE('',*,*,#53676,.F.);
#82335=ORIENTED_EDGE('',*,*,#57345,.T.);
#82336=ORIENTED_EDGE('',*,*,#55483,.F.);
#82337=ORIENTED_EDGE('',*,*,#57346,.F.);
#82338=ORIENTED_EDGE('',*,*,#53685,.F.);
#82339=ORIENTED_EDGE('',*,*,#53675,.T.);
#82340=ORIENTED_EDGE('',*,*,#53679,.F.);
#82341=ORIENTED_EDGE('',*,*,#57347,.F.);
#82342=ORIENTED_EDGE('',*,*,#55485,.F.);
#82343=ORIENTED_EDGE('',*,*,#57344,.T.);
#82344=ORIENTED_EDGE('',*,*,#57346,.T.);
#82345=ORIENTED_EDGE('',*,*,#55482,.F.);
#82346=ORIENTED_EDGE('',*,*,#57348,.F.);
#82347=ORIENTED_EDGE('',*,*,#53670,.F.);
#82348=ORIENTED_EDGE('',*,*,#57347,.T.);
#82349=ORIENTED_EDGE('',*,*,#53683,.F.);
#82350=ORIENTED_EDGE('',*,*,#57349,.F.);
#82351=ORIENTED_EDGE('',*,*,#55474,.F.);
#82352=ORIENTED_EDGE('',*,*,#57348,.T.);
#82353=ORIENTED_EDGE('',*,*,#55481,.F.);
#82354=ORIENTED_EDGE('',*,*,#57350,.F.);
#82355=ORIENTED_EDGE('',*,*,#53687,.F.);
#82356=ORIENTED_EDGE('',*,*,#57349,.T.);
#82357=ORIENTED_EDGE('',*,*,#52246,.F.);
#82358=ORIENTED_EDGE('',*,*,#57351,.F.);
#82359=ORIENTED_EDGE('',*,*,#55475,.F.);
#82360=ORIENTED_EDGE('',*,*,#57350,.T.);
#82361=ORIENTED_EDGE('',*,*,#55480,.F.);
#82362=ORIENTED_EDGE('',*,*,#57352,.F.);
#82363=ORIENTED_EDGE('',*,*,#53662,.T.);
#82364=ORIENTED_EDGE('',*,*,#53666,.F.);
#82365=ORIENTED_EDGE('',*,*,#57351,.T.);
#82366=ORIENTED_EDGE('',*,*,#52245,.F.);
#82367=ORIENTED_EDGE('',*,*,#52044,.F.);
#82368=ORIENTED_EDGE('',*,*,#56412,.F.);
#82369=ORIENTED_EDGE('',*,*,#57352,.T.);
#82370=ORIENTED_EDGE('',*,*,#55479,.F.);
#82371=ORIENTED_EDGE('',*,*,#57353,.F.);
#82372=ORIENTED_EDGE('',*,*,#53663,.F.);
#82373=ORIENTED_EDGE('',*,*,#57353,.T.);
#82374=ORIENTED_EDGE('',*,*,#55478,.F.);
#82375=ORIENTED_EDGE('',*,*,#57354,.F.);
#82376=ORIENTED_EDGE('',*,*,#53681,.F.);
#82377=ORIENTED_EDGE('',*,*,#52042,.T.);
#82378=ORIENTED_EDGE('',*,*,#52243,.F.);
#82379=ORIENTED_EDGE('',*,*,#57355,.F.);
#82380=ORIENTED_EDGE('',*,*,#56414,.F.);
#82381=ORIENTED_EDGE('',*,*,#57354,.T.);
#82382=ORIENTED_EDGE('',*,*,#55477,.F.);
#82383=ORIENTED_EDGE('',*,*,#57356,.F.);
#82384=ORIENTED_EDGE('',*,*,#52781,.F.);
#82385=ORIENTED_EDGE('',*,*,#57355,.T.);
#82386=ORIENTED_EDGE('',*,*,#52242,.F.);
#82387=ORIENTED_EDGE('',*,*,#57357,.F.);
#82388=ORIENTED_EDGE('',*,*,#55465,.F.);
#82389=ORIENTED_EDGE('',*,*,#57356,.T.);
#82390=ORIENTED_EDGE('',*,*,#56413,.F.);
#82391=ORIENTED_EDGE('',*,*,#52040,.F.);
#82392=ORIENTED_EDGE('',*,*,#52782,.F.);
#82393=ORIENTED_EDGE('',*,*,#57357,.T.);
#82394=ORIENTED_EDGE('',*,*,#53712,.F.);
#82395=ORIENTED_EDGE('',*,*,#57358,.F.);
#82396=ORIENTED_EDGE('',*,*,#55466,.F.);
#82397=ORIENTED_EDGE('',*,*,#53707,.F.);
#82398=ORIENTED_EDGE('',*,*,#53703,.T.);
#82399=ORIENTED_EDGE('',*,*,#57359,.F.);
#82400=ORIENTED_EDGE('',*,*,#55467,.F.);
#82401=ORIENTED_EDGE('',*,*,#57358,.T.);
#82402=ORIENTED_EDGE('',*,*,#52038,.T.);
#82403=ORIENTED_EDGE('',*,*,#56415,.F.);
#82404=ORIENTED_EDGE('',*,*,#57360,.F.);
#82405=ORIENTED_EDGE('',*,*,#52423,.F.);
#82406=ORIENTED_EDGE('',*,*,#57359,.T.);
#82407=ORIENTED_EDGE('',*,*,#53702,.F.);
#82408=ORIENTED_EDGE('',*,*,#57361,.F.);
#82409=ORIENTED_EDGE('',*,*,#55468,.F.);
#82410=ORIENTED_EDGE('',*,*,#57360,.T.);
#82411=ORIENTED_EDGE('',*,*,#55463,.F.);
#82412=ORIENTED_EDGE('',*,*,#57362,.F.);
#82413=ORIENTED_EDGE('',*,*,#52424,.F.);
#82414=ORIENTED_EDGE('',*,*,#57361,.T.);
#82415=ORIENTED_EDGE('',*,*,#53714,.F.);
#82416=ORIENTED_EDGE('',*,*,#57363,.F.);
#82417=ORIENTED_EDGE('',*,*,#55469,.F.);
#82418=ORIENTED_EDGE('',*,*,#57362,.T.);
#82419=ORIENTED_EDGE('',*,*,#55462,.F.);
#82420=ORIENTED_EDGE('',*,*,#57364,.F.);
#82421=ORIENTED_EDGE('',*,*,#53710,.F.);
#82422=ORIENTED_EDGE('',*,*,#57363,.T.);
#82423=ORIENTED_EDGE('',*,*,#53698,.F.);
#82424=ORIENTED_EDGE('',*,*,#57365,.F.);
#82425=ORIENTED_EDGE('',*,*,#55470,.F.);
#82426=ORIENTED_EDGE('',*,*,#57364,.T.);
#82427=ORIENTED_EDGE('',*,*,#55473,.F.);
#82428=ORIENTED_EDGE('',*,*,#57366,.F.);
#82429=ORIENTED_EDGE('',*,*,#53689,.F.);
#82430=ORIENTED_EDGE('',*,*,#57365,.T.);
#82431=ORIENTED_EDGE('',*,*,#53716,.F.);
#82432=ORIENTED_EDGE('',*,*,#57367,.F.);
#82433=ORIENTED_EDGE('',*,*,#55471,.F.);
#82434=ORIENTED_EDGE('',*,*,#57366,.T.);
#82435=ORIENTED_EDGE('',*,*,#55472,.F.);
#82436=ORIENTED_EDGE('',*,*,#57367,.T.);
#82437=ORIENTED_EDGE('',*,*,#53694,.F.);
#82438=ORIENTED_EDGE('',*,*,#53690,.T.);
#82439=ORIENTED_EDGE('',*,*,#57368,.F.);
#82440=ORIENTED_EDGE('',*,*,#55512,.F.);
#82441=ORIENTED_EDGE('',*,*,#57369,.F.);
#82442=ORIENTED_EDGE('',*,*,#53646,.F.);
#82443=ORIENTED_EDGE('',*,*,#57369,.T.);
#82444=ORIENTED_EDGE('',*,*,#55511,.F.);
#82445=ORIENTED_EDGE('',*,*,#57370,.F.);
#82446=ORIENTED_EDGE('',*,*,#53655,.F.);
#82447=ORIENTED_EDGE('',*,*,#53645,.T.);
#82448=ORIENTED_EDGE('',*,*,#53649,.F.);
#82449=ORIENTED_EDGE('',*,*,#57371,.F.);
#82450=ORIENTED_EDGE('',*,*,#55513,.F.);
#82451=ORIENTED_EDGE('',*,*,#57368,.T.);
#82452=ORIENTED_EDGE('',*,*,#57370,.T.);
#82453=ORIENTED_EDGE('',*,*,#55510,.F.);
#82454=ORIENTED_EDGE('',*,*,#57372,.F.);
#82455=ORIENTED_EDGE('',*,*,#53640,.F.);
#82456=ORIENTED_EDGE('',*,*,#57371,.T.);
#82457=ORIENTED_EDGE('',*,*,#53653,.F.);
#82458=ORIENTED_EDGE('',*,*,#57373,.F.);
#82459=ORIENTED_EDGE('',*,*,#55502,.F.);
#82460=ORIENTED_EDGE('',*,*,#57372,.T.);
#82461=ORIENTED_EDGE('',*,*,#55509,.F.);
#82462=ORIENTED_EDGE('',*,*,#57374,.F.);
#82463=ORIENTED_EDGE('',*,*,#53657,.F.);
#82464=ORIENTED_EDGE('',*,*,#57373,.T.);
#82465=ORIENTED_EDGE('',*,*,#52252,.F.);
#82466=ORIENTED_EDGE('',*,*,#57375,.F.);
#82467=ORIENTED_EDGE('',*,*,#55503,.F.);
#82468=ORIENTED_EDGE('',*,*,#57374,.T.);
#82469=ORIENTED_EDGE('',*,*,#55508,.F.);
#82470=ORIENTED_EDGE('',*,*,#57376,.F.);
#82471=ORIENTED_EDGE('',*,*,#53632,.T.);
#82472=ORIENTED_EDGE('',*,*,#53636,.F.);
#82473=ORIENTED_EDGE('',*,*,#57375,.T.);
#82474=ORIENTED_EDGE('',*,*,#52251,.F.);
#82475=ORIENTED_EDGE('',*,*,#57377,.F.);
#82476=ORIENTED_EDGE('',*,*,#56416,.F.);
#82477=ORIENTED_EDGE('',*,*,#57376,.T.);
#82478=ORIENTED_EDGE('',*,*,#55507,.F.);
#82479=ORIENTED_EDGE('',*,*,#57378,.F.);
#82480=ORIENTED_EDGE('',*,*,#53633,.F.);
#82481=ORIENTED_EDGE('',*,*,#57377,.T.);
#82482=ORIENTED_EDGE('',*,*,#52250,.F.);
#82483=ORIENTED_EDGE('',*,*,#57379,.F.);
#82484=ORIENTED_EDGE('',*,*,#55487,.F.);
#82485=ORIENTED_EDGE('',*,*,#57378,.T.);
#82486=ORIENTED_EDGE('',*,*,#55506,.F.);
#82487=ORIENTED_EDGE('',*,*,#57380,.F.);
#82488=ORIENTED_EDGE('',*,*,#53651,.F.);
#82489=ORIENTED_EDGE('',*,*,#57379,.T.);
#82490=ORIENTED_EDGE('',*,*,#52249,.F.);
#82491=ORIENTED_EDGE('',*,*,#57381,.F.);
#82492=ORIENTED_EDGE('',*,*,#56418,.F.);
#82493=ORIENTED_EDGE('',*,*,#57380,.T.);
#82494=ORIENTED_EDGE('',*,*,#55505,.F.);
#82495=ORIENTED_EDGE('',*,*,#57382,.F.);
#82496=ORIENTED_EDGE('',*,*,#52775,.F.);
#82497=ORIENTED_EDGE('',*,*,#57381,.T.);
#82498=ORIENTED_EDGE('',*,*,#52248,.F.);
#82499=ORIENTED_EDGE('',*,*,#57383,.F.);
#82500=ORIENTED_EDGE('',*,*,#55493,.F.);
#82501=ORIENTED_EDGE('',*,*,#57382,.T.);
#82502=ORIENTED_EDGE('',*,*,#56417,.F.);
#82503=ORIENTED_EDGE('',*,*,#57384,.F.);
#82504=ORIENTED_EDGE('',*,*,#52776,.F.);
#82505=ORIENTED_EDGE('',*,*,#57383,.T.);
#82506=ORIENTED_EDGE('',*,*,#53682,.F.);
#82507=ORIENTED_EDGE('',*,*,#57385,.F.);
#82508=ORIENTED_EDGE('',*,*,#55494,.F.);
#82509=ORIENTED_EDGE('',*,*,#57384,.T.);
#82510=ORIENTED_EDGE('',*,*,#55489,.F.);
#82511=ORIENTED_EDGE('',*,*,#57386,.F.);
#82512=ORIENTED_EDGE('',*,*,#52777,.F.);
#82513=ORIENTED_EDGE('',*,*,#53677,.F.);
#82514=ORIENTED_EDGE('',*,*,#53673,.T.);
#82515=ORIENTED_EDGE('',*,*,#57387,.F.);
#82516=ORIENTED_EDGE('',*,*,#55495,.F.);
#82517=ORIENTED_EDGE('',*,*,#57385,.T.);
#82518=ORIENTED_EDGE('',*,*,#57386,.T.);
#82519=ORIENTED_EDGE('',*,*,#56419,.F.);
#82520=ORIENTED_EDGE('',*,*,#57388,.F.);
#82521=ORIENTED_EDGE('',*,*,#52778,.F.);
#82522=ORIENTED_EDGE('',*,*,#57387,.T.);
#82523=ORIENTED_EDGE('',*,*,#53672,.F.);
#82524=ORIENTED_EDGE('',*,*,#57389,.F.);
#82525=ORIENTED_EDGE('',*,*,#55496,.F.);
#82526=ORIENTED_EDGE('',*,*,#57388,.T.);
#82527=ORIENTED_EDGE('',*,*,#55491,.F.);
#82528=ORIENTED_EDGE('',*,*,#57390,.F.);
#82529=ORIENTED_EDGE('',*,*,#52779,.F.);
#82530=ORIENTED_EDGE('',*,*,#57389,.T.);
#82531=ORIENTED_EDGE('',*,*,#53684,.F.);
#82532=ORIENTED_EDGE('',*,*,#57391,.F.);
#82533=ORIENTED_EDGE('',*,*,#55497,.F.);
#82534=ORIENTED_EDGE('',*,*,#57390,.T.);
#82535=ORIENTED_EDGE('',*,*,#55490,.F.);
#82536=ORIENTED_EDGE('',*,*,#57392,.F.);
#82537=ORIENTED_EDGE('',*,*,#53680,.F.);
#82538=ORIENTED_EDGE('',*,*,#57391,.T.);
#82539=ORIENTED_EDGE('',*,*,#53668,.F.);
#82540=ORIENTED_EDGE('',*,*,#57393,.F.);
#82541=ORIENTED_EDGE('',*,*,#55498,.F.);
#82542=ORIENTED_EDGE('',*,*,#57392,.T.);
#82543=ORIENTED_EDGE('',*,*,#55501,.F.);
#82544=ORIENTED_EDGE('',*,*,#57394,.F.);
#82545=ORIENTED_EDGE('',*,*,#53659,.F.);
#82546=ORIENTED_EDGE('',*,*,#57393,.T.);
#82547=ORIENTED_EDGE('',*,*,#53686,.F.);
#82548=ORIENTED_EDGE('',*,*,#57395,.F.);
#82549=ORIENTED_EDGE('',*,*,#55499,.F.);
#82550=ORIENTED_EDGE('',*,*,#57394,.T.);
#82551=ORIENTED_EDGE('',*,*,#55500,.F.);
#82552=ORIENTED_EDGE('',*,*,#57395,.T.);
#82553=ORIENTED_EDGE('',*,*,#53664,.F.);
#82554=ORIENTED_EDGE('',*,*,#53660,.T.);
#82555=ORIENTED_EDGE('',*,*,#57396,.F.);
#82556=ORIENTED_EDGE('',*,*,#55540,.F.);
#82557=ORIENTED_EDGE('',*,*,#57397,.F.);
#82558=ORIENTED_EDGE('',*,*,#53616,.F.);
#82559=ORIENTED_EDGE('',*,*,#57397,.T.);
#82560=ORIENTED_EDGE('',*,*,#55539,.F.);
#82561=ORIENTED_EDGE('',*,*,#57398,.F.);
#82562=ORIENTED_EDGE('',*,*,#53625,.F.);
#82563=ORIENTED_EDGE('',*,*,#53615,.T.);
#82564=ORIENTED_EDGE('',*,*,#53619,.F.);
#82565=ORIENTED_EDGE('',*,*,#57399,.F.);
#82566=ORIENTED_EDGE('',*,*,#55541,.F.);
#82567=ORIENTED_EDGE('',*,*,#57396,.T.);
#82568=ORIENTED_EDGE('',*,*,#57398,.T.);
#82569=ORIENTED_EDGE('',*,*,#55538,.F.);
#82570=ORIENTED_EDGE('',*,*,#57400,.F.);
#82571=ORIENTED_EDGE('',*,*,#53610,.F.);
#82572=ORIENTED_EDGE('',*,*,#57399,.T.);
#82573=ORIENTED_EDGE('',*,*,#53623,.F.);
#82574=ORIENTED_EDGE('',*,*,#57401,.F.);
#82575=ORIENTED_EDGE('',*,*,#55530,.F.);
#82576=ORIENTED_EDGE('',*,*,#57400,.T.);
#82577=ORIENTED_EDGE('',*,*,#55537,.F.);
#82578=ORIENTED_EDGE('',*,*,#57402,.F.);
#82579=ORIENTED_EDGE('',*,*,#53627,.F.);
#82580=ORIENTED_EDGE('',*,*,#57401,.T.);
#82581=ORIENTED_EDGE('',*,*,#52258,.F.);
#82582=ORIENTED_EDGE('',*,*,#57403,.F.);
#82583=ORIENTED_EDGE('',*,*,#55531,.F.);
#82584=ORIENTED_EDGE('',*,*,#57402,.T.);
#82585=ORIENTED_EDGE('',*,*,#55536,.F.);
#82586=ORIENTED_EDGE('',*,*,#57404,.F.);
#82587=ORIENTED_EDGE('',*,*,#53602,.T.);
#82588=ORIENTED_EDGE('',*,*,#53606,.F.);
#82589=ORIENTED_EDGE('',*,*,#57403,.T.);
#82590=ORIENTED_EDGE('',*,*,#52257,.F.);
#82591=ORIENTED_EDGE('',*,*,#57405,.F.);
#82592=ORIENTED_EDGE('',*,*,#56420,.F.);
#82593=ORIENTED_EDGE('',*,*,#57404,.T.);
#82594=ORIENTED_EDGE('',*,*,#55535,.F.);
#82595=ORIENTED_EDGE('',*,*,#57406,.F.);
#82596=ORIENTED_EDGE('',*,*,#53603,.F.);
#82597=ORIENTED_EDGE('',*,*,#57405,.T.);
#82598=ORIENTED_EDGE('',*,*,#52256,.F.);
#82599=ORIENTED_EDGE('',*,*,#57407,.F.);
#82600=ORIENTED_EDGE('',*,*,#55515,.F.);
#82601=ORIENTED_EDGE('',*,*,#57406,.T.);
#82602=ORIENTED_EDGE('',*,*,#55534,.F.);
#82603=ORIENTED_EDGE('',*,*,#57408,.F.);
#82604=ORIENTED_EDGE('',*,*,#53621,.F.);
#82605=ORIENTED_EDGE('',*,*,#57407,.T.);
#82606=ORIENTED_EDGE('',*,*,#52255,.F.);
#82607=ORIENTED_EDGE('',*,*,#57409,.F.);
#82608=ORIENTED_EDGE('',*,*,#56422,.F.);
#82609=ORIENTED_EDGE('',*,*,#57408,.T.);
#82610=ORIENTED_EDGE('',*,*,#55533,.F.);
#82611=ORIENTED_EDGE('',*,*,#57410,.F.);
#82612=ORIENTED_EDGE('',*,*,#52769,.F.);
#82613=ORIENTED_EDGE('',*,*,#57409,.T.);
#82614=ORIENTED_EDGE('',*,*,#52254,.F.);
#82615=ORIENTED_EDGE('',*,*,#57411,.F.);
#82616=ORIENTED_EDGE('',*,*,#55521,.F.);
#82617=ORIENTED_EDGE('',*,*,#57410,.T.);
#82618=ORIENTED_EDGE('',*,*,#56421,.F.);
#82619=ORIENTED_EDGE('',*,*,#57412,.F.);
#82620=ORIENTED_EDGE('',*,*,#52770,.F.);
#82621=ORIENTED_EDGE('',*,*,#57411,.T.);
#82622=ORIENTED_EDGE('',*,*,#53652,.F.);
#82623=ORIENTED_EDGE('',*,*,#57413,.F.);
#82624=ORIENTED_EDGE('',*,*,#55522,.F.);
#82625=ORIENTED_EDGE('',*,*,#57412,.T.);
#82626=ORIENTED_EDGE('',*,*,#55517,.F.);
#82627=ORIENTED_EDGE('',*,*,#57414,.F.);
#82628=ORIENTED_EDGE('',*,*,#52771,.F.);
#82629=ORIENTED_EDGE('',*,*,#53647,.F.);
#82630=ORIENTED_EDGE('',*,*,#53643,.T.);
#82631=ORIENTED_EDGE('',*,*,#57415,.F.);
#82632=ORIENTED_EDGE('',*,*,#55523,.F.);
#82633=ORIENTED_EDGE('',*,*,#57413,.T.);
#82634=ORIENTED_EDGE('',*,*,#57414,.T.);
#82635=ORIENTED_EDGE('',*,*,#56423,.F.);
#82636=ORIENTED_EDGE('',*,*,#57416,.F.);
#82637=ORIENTED_EDGE('',*,*,#52772,.F.);
#82638=ORIENTED_EDGE('',*,*,#57415,.T.);
#82639=ORIENTED_EDGE('',*,*,#53642,.F.);
#82640=ORIENTED_EDGE('',*,*,#57417,.F.);
#82641=ORIENTED_EDGE('',*,*,#55524,.F.);
#82642=ORIENTED_EDGE('',*,*,#57416,.T.);
#82643=ORIENTED_EDGE('',*,*,#55519,.F.);
#82644=ORIENTED_EDGE('',*,*,#57418,.F.);
#82645=ORIENTED_EDGE('',*,*,#52773,.F.);
#82646=ORIENTED_EDGE('',*,*,#57417,.T.);
#82647=ORIENTED_EDGE('',*,*,#53654,.F.);
#82648=ORIENTED_EDGE('',*,*,#57419,.F.);
#82649=ORIENTED_EDGE('',*,*,#55525,.F.);
#82650=ORIENTED_EDGE('',*,*,#57418,.T.);
#82651=ORIENTED_EDGE('',*,*,#55518,.F.);
#82652=ORIENTED_EDGE('',*,*,#57420,.F.);
#82653=ORIENTED_EDGE('',*,*,#53650,.F.);
#82654=ORIENTED_EDGE('',*,*,#57419,.T.);
#82655=ORIENTED_EDGE('',*,*,#53638,.F.);
#82656=ORIENTED_EDGE('',*,*,#57421,.F.);
#82657=ORIENTED_EDGE('',*,*,#55526,.F.);
#82658=ORIENTED_EDGE('',*,*,#57420,.T.);
#82659=ORIENTED_EDGE('',*,*,#55529,.F.);
#82660=ORIENTED_EDGE('',*,*,#57422,.F.);
#82661=ORIENTED_EDGE('',*,*,#53629,.F.);
#82662=ORIENTED_EDGE('',*,*,#57421,.T.);
#82663=ORIENTED_EDGE('',*,*,#53656,.F.);
#82664=ORIENTED_EDGE('',*,*,#57423,.F.);
#82665=ORIENTED_EDGE('',*,*,#55527,.F.);
#82666=ORIENTED_EDGE('',*,*,#57422,.T.);
#82667=ORIENTED_EDGE('',*,*,#55528,.F.);
#82668=ORIENTED_EDGE('',*,*,#57423,.T.);
#82669=ORIENTED_EDGE('',*,*,#53634,.F.);
#82670=ORIENTED_EDGE('',*,*,#53630,.T.);
#82671=ORIENTED_EDGE('',*,*,#57424,.F.);
#82672=ORIENTED_EDGE('',*,*,#55568,.F.);
#82673=ORIENTED_EDGE('',*,*,#57425,.F.);
#82674=ORIENTED_EDGE('',*,*,#53586,.F.);
#82675=ORIENTED_EDGE('',*,*,#57425,.T.);
#82676=ORIENTED_EDGE('',*,*,#55567,.F.);
#82677=ORIENTED_EDGE('',*,*,#57426,.F.);
#82678=ORIENTED_EDGE('',*,*,#53595,.F.);
#82679=ORIENTED_EDGE('',*,*,#53585,.T.);
#82680=ORIENTED_EDGE('',*,*,#53589,.F.);
#82681=ORIENTED_EDGE('',*,*,#57427,.F.);
#82682=ORIENTED_EDGE('',*,*,#55569,.F.);
#82683=ORIENTED_EDGE('',*,*,#57424,.T.);
#82684=ORIENTED_EDGE('',*,*,#57426,.T.);
#82685=ORIENTED_EDGE('',*,*,#55566,.F.);
#82686=ORIENTED_EDGE('',*,*,#57428,.F.);
#82687=ORIENTED_EDGE('',*,*,#53580,.F.);
#82688=ORIENTED_EDGE('',*,*,#57427,.T.);
#82689=ORIENTED_EDGE('',*,*,#53593,.F.);
#82690=ORIENTED_EDGE('',*,*,#57429,.F.);
#82691=ORIENTED_EDGE('',*,*,#55558,.F.);
#82692=ORIENTED_EDGE('',*,*,#57428,.T.);
#82693=ORIENTED_EDGE('',*,*,#55565,.F.);
#82694=ORIENTED_EDGE('',*,*,#57430,.F.);
#82695=ORIENTED_EDGE('',*,*,#53597,.F.);
#82696=ORIENTED_EDGE('',*,*,#57429,.T.);
#82697=ORIENTED_EDGE('',*,*,#52264,.F.);
#82698=ORIENTED_EDGE('',*,*,#57431,.F.);
#82699=ORIENTED_EDGE('',*,*,#55559,.F.);
#82700=ORIENTED_EDGE('',*,*,#57430,.T.);
#82701=ORIENTED_EDGE('',*,*,#55564,.F.);
#82702=ORIENTED_EDGE('',*,*,#57432,.F.);
#82703=ORIENTED_EDGE('',*,*,#53572,.T.);
#82704=ORIENTED_EDGE('',*,*,#53576,.F.);
#82705=ORIENTED_EDGE('',*,*,#57431,.T.);
#82706=ORIENTED_EDGE('',*,*,#52263,.F.);
#82707=ORIENTED_EDGE('',*,*,#57433,.F.);
#82708=ORIENTED_EDGE('',*,*,#56424,.F.);
#82709=ORIENTED_EDGE('',*,*,#57432,.T.);
#82710=ORIENTED_EDGE('',*,*,#55563,.F.);
#82711=ORIENTED_EDGE('',*,*,#57434,.F.);
#82712=ORIENTED_EDGE('',*,*,#53573,.F.);
#82713=ORIENTED_EDGE('',*,*,#57433,.T.);
#82714=ORIENTED_EDGE('',*,*,#52262,.F.);
#82715=ORIENTED_EDGE('',*,*,#57435,.F.);
#82716=ORIENTED_EDGE('',*,*,#55543,.F.);
#82717=ORIENTED_EDGE('',*,*,#57434,.T.);
#82718=ORIENTED_EDGE('',*,*,#55562,.F.);
#82719=ORIENTED_EDGE('',*,*,#57436,.F.);
#82720=ORIENTED_EDGE('',*,*,#53591,.F.);
#82721=ORIENTED_EDGE('',*,*,#57435,.T.);
#82722=ORIENTED_EDGE('',*,*,#52261,.F.);
#82723=ORIENTED_EDGE('',*,*,#57437,.F.);
#82724=ORIENTED_EDGE('',*,*,#56426,.F.);
#82725=ORIENTED_EDGE('',*,*,#57436,.T.);
#82726=ORIENTED_EDGE('',*,*,#55561,.F.);
#82727=ORIENTED_EDGE('',*,*,#57438,.F.);
#82728=ORIENTED_EDGE('',*,*,#52763,.F.);
#82729=ORIENTED_EDGE('',*,*,#57437,.T.);
#82730=ORIENTED_EDGE('',*,*,#52260,.F.);
#82731=ORIENTED_EDGE('',*,*,#57439,.F.);
#82732=ORIENTED_EDGE('',*,*,#55549,.F.);
#82733=ORIENTED_EDGE('',*,*,#57438,.T.);
#82734=ORIENTED_EDGE('',*,*,#56425,.F.);
#82735=ORIENTED_EDGE('',*,*,#57440,.F.);
#82736=ORIENTED_EDGE('',*,*,#52764,.F.);
#82737=ORIENTED_EDGE('',*,*,#57439,.T.);
#82738=ORIENTED_EDGE('',*,*,#53622,.F.);
#82739=ORIENTED_EDGE('',*,*,#57441,.F.);
#82740=ORIENTED_EDGE('',*,*,#55550,.F.);
#82741=ORIENTED_EDGE('',*,*,#57440,.T.);
#82742=ORIENTED_EDGE('',*,*,#55545,.F.);
#82743=ORIENTED_EDGE('',*,*,#57442,.F.);
#82744=ORIENTED_EDGE('',*,*,#52765,.F.);
#82745=ORIENTED_EDGE('',*,*,#53617,.F.);
#82746=ORIENTED_EDGE('',*,*,#53613,.T.);
#82747=ORIENTED_EDGE('',*,*,#57443,.F.);
#82748=ORIENTED_EDGE('',*,*,#55551,.F.);
#82749=ORIENTED_EDGE('',*,*,#57441,.T.);
#82750=ORIENTED_EDGE('',*,*,#57442,.T.);
#82751=ORIENTED_EDGE('',*,*,#56427,.F.);
#82752=ORIENTED_EDGE('',*,*,#57444,.F.);
#82753=ORIENTED_EDGE('',*,*,#52766,.F.);
#82754=ORIENTED_EDGE('',*,*,#57443,.T.);
#82755=ORIENTED_EDGE('',*,*,#53612,.F.);
#82756=ORIENTED_EDGE('',*,*,#57445,.F.);
#82757=ORIENTED_EDGE('',*,*,#55552,.F.);
#82758=ORIENTED_EDGE('',*,*,#57444,.T.);
#82759=ORIENTED_EDGE('',*,*,#55547,.F.);
#82760=ORIENTED_EDGE('',*,*,#57446,.F.);
#82761=ORIENTED_EDGE('',*,*,#52767,.F.);
#82762=ORIENTED_EDGE('',*,*,#57445,.T.);
#82763=ORIENTED_EDGE('',*,*,#53624,.F.);
#82764=ORIENTED_EDGE('',*,*,#57447,.F.);
#82765=ORIENTED_EDGE('',*,*,#55553,.F.);
#82766=ORIENTED_EDGE('',*,*,#57446,.T.);
#82767=ORIENTED_EDGE('',*,*,#55546,.F.);
#82768=ORIENTED_EDGE('',*,*,#57448,.F.);
#82769=ORIENTED_EDGE('',*,*,#53620,.F.);
#82770=ORIENTED_EDGE('',*,*,#57447,.T.);
#82771=ORIENTED_EDGE('',*,*,#53608,.F.);
#82772=ORIENTED_EDGE('',*,*,#57449,.F.);
#82773=ORIENTED_EDGE('',*,*,#55554,.F.);
#82774=ORIENTED_EDGE('',*,*,#57448,.T.);
#82775=ORIENTED_EDGE('',*,*,#55557,.F.);
#82776=ORIENTED_EDGE('',*,*,#57450,.F.);
#82777=ORIENTED_EDGE('',*,*,#53599,.F.);
#82778=ORIENTED_EDGE('',*,*,#57449,.T.);
#82779=ORIENTED_EDGE('',*,*,#53626,.F.);
#82780=ORIENTED_EDGE('',*,*,#57451,.F.);
#82781=ORIENTED_EDGE('',*,*,#55555,.F.);
#82782=ORIENTED_EDGE('',*,*,#57450,.T.);
#82783=ORIENTED_EDGE('',*,*,#55556,.F.);
#82784=ORIENTED_EDGE('',*,*,#57451,.T.);
#82785=ORIENTED_EDGE('',*,*,#53604,.F.);
#82786=ORIENTED_EDGE('',*,*,#53600,.T.);
#82787=ORIENTED_EDGE('',*,*,#57452,.F.);
#82788=ORIENTED_EDGE('',*,*,#55596,.F.);
#82789=ORIENTED_EDGE('',*,*,#57453,.F.);
#82790=ORIENTED_EDGE('',*,*,#53556,.F.);
#82791=ORIENTED_EDGE('',*,*,#57453,.T.);
#82792=ORIENTED_EDGE('',*,*,#55595,.F.);
#82793=ORIENTED_EDGE('',*,*,#57454,.F.);
#82794=ORIENTED_EDGE('',*,*,#53565,.F.);
#82795=ORIENTED_EDGE('',*,*,#53555,.T.);
#82796=ORIENTED_EDGE('',*,*,#53559,.F.);
#82797=ORIENTED_EDGE('',*,*,#57455,.F.);
#82798=ORIENTED_EDGE('',*,*,#55597,.F.);
#82799=ORIENTED_EDGE('',*,*,#57452,.T.);
#82800=ORIENTED_EDGE('',*,*,#57454,.T.);
#82801=ORIENTED_EDGE('',*,*,#55594,.F.);
#82802=ORIENTED_EDGE('',*,*,#57456,.F.);
#82803=ORIENTED_EDGE('',*,*,#53550,.F.);
#82804=ORIENTED_EDGE('',*,*,#57455,.T.);
#82805=ORIENTED_EDGE('',*,*,#53563,.F.);
#82806=ORIENTED_EDGE('',*,*,#57457,.F.);
#82807=ORIENTED_EDGE('',*,*,#55586,.F.);
#82808=ORIENTED_EDGE('',*,*,#57456,.T.);
#82809=ORIENTED_EDGE('',*,*,#55593,.F.);
#82810=ORIENTED_EDGE('',*,*,#57458,.F.);
#82811=ORIENTED_EDGE('',*,*,#53567,.F.);
#82812=ORIENTED_EDGE('',*,*,#57457,.T.);
#82813=ORIENTED_EDGE('',*,*,#52270,.F.);
#82814=ORIENTED_EDGE('',*,*,#57459,.F.);
#82815=ORIENTED_EDGE('',*,*,#55587,.F.);
#82816=ORIENTED_EDGE('',*,*,#57458,.T.);
#82817=ORIENTED_EDGE('',*,*,#55592,.F.);
#82818=ORIENTED_EDGE('',*,*,#57460,.F.);
#82819=ORIENTED_EDGE('',*,*,#53542,.T.);
#82820=ORIENTED_EDGE('',*,*,#53546,.F.);
#82821=ORIENTED_EDGE('',*,*,#57459,.T.);
#82822=ORIENTED_EDGE('',*,*,#52269,.F.);
#82823=ORIENTED_EDGE('',*,*,#57461,.F.);
#82824=ORIENTED_EDGE('',*,*,#56428,.F.);
#82825=ORIENTED_EDGE('',*,*,#57460,.T.);
#82826=ORIENTED_EDGE('',*,*,#55591,.F.);
#82827=ORIENTED_EDGE('',*,*,#57462,.F.);
#82828=ORIENTED_EDGE('',*,*,#53543,.F.);
#82829=ORIENTED_EDGE('',*,*,#57461,.T.);
#82830=ORIENTED_EDGE('',*,*,#52268,.F.);
#82831=ORIENTED_EDGE('',*,*,#57463,.F.);
#82832=ORIENTED_EDGE('',*,*,#55571,.F.);
#82833=ORIENTED_EDGE('',*,*,#57462,.T.);
#82834=ORIENTED_EDGE('',*,*,#55590,.F.);
#82835=ORIENTED_EDGE('',*,*,#57464,.F.);
#82836=ORIENTED_EDGE('',*,*,#53561,.F.);
#82837=ORIENTED_EDGE('',*,*,#57463,.T.);
#82838=ORIENTED_EDGE('',*,*,#52267,.F.);
#82839=ORIENTED_EDGE('',*,*,#57465,.F.);
#82840=ORIENTED_EDGE('',*,*,#56430,.F.);
#82841=ORIENTED_EDGE('',*,*,#57464,.T.);
#82842=ORIENTED_EDGE('',*,*,#55589,.F.);
#82843=ORIENTED_EDGE('',*,*,#57466,.F.);
#82844=ORIENTED_EDGE('',*,*,#52757,.F.);
#82845=ORIENTED_EDGE('',*,*,#57465,.T.);
#82846=ORIENTED_EDGE('',*,*,#52266,.F.);
#82847=ORIENTED_EDGE('',*,*,#57467,.F.);
#82848=ORIENTED_EDGE('',*,*,#55577,.F.);
#82849=ORIENTED_EDGE('',*,*,#57466,.T.);
#82850=ORIENTED_EDGE('',*,*,#56429,.F.);
#82851=ORIENTED_EDGE('',*,*,#57468,.F.);
#82852=ORIENTED_EDGE('',*,*,#52758,.F.);
#82853=ORIENTED_EDGE('',*,*,#57467,.T.);
#82854=ORIENTED_EDGE('',*,*,#53592,.F.);
#82855=ORIENTED_EDGE('',*,*,#57469,.F.);
#82856=ORIENTED_EDGE('',*,*,#55578,.F.);
#82857=ORIENTED_EDGE('',*,*,#57468,.T.);
#82858=ORIENTED_EDGE('',*,*,#55573,.F.);
#82859=ORIENTED_EDGE('',*,*,#57470,.F.);
#82860=ORIENTED_EDGE('',*,*,#52759,.F.);
#82861=ORIENTED_EDGE('',*,*,#53587,.F.);
#82862=ORIENTED_EDGE('',*,*,#53583,.T.);
#82863=ORIENTED_EDGE('',*,*,#57471,.F.);
#82864=ORIENTED_EDGE('',*,*,#55579,.F.);
#82865=ORIENTED_EDGE('',*,*,#57469,.T.);
#82866=ORIENTED_EDGE('',*,*,#57470,.T.);
#82867=ORIENTED_EDGE('',*,*,#56431,.F.);
#82868=ORIENTED_EDGE('',*,*,#57472,.F.);
#82869=ORIENTED_EDGE('',*,*,#52760,.F.);
#82870=ORIENTED_EDGE('',*,*,#57471,.T.);
#82871=ORIENTED_EDGE('',*,*,#53582,.F.);
#82872=ORIENTED_EDGE('',*,*,#57473,.F.);
#82873=ORIENTED_EDGE('',*,*,#55580,.F.);
#82874=ORIENTED_EDGE('',*,*,#57472,.T.);
#82875=ORIENTED_EDGE('',*,*,#55575,.F.);
#82876=ORIENTED_EDGE('',*,*,#57474,.F.);
#82877=ORIENTED_EDGE('',*,*,#52761,.F.);
#82878=ORIENTED_EDGE('',*,*,#57473,.T.);
#82879=ORIENTED_EDGE('',*,*,#53594,.F.);
#82880=ORIENTED_EDGE('',*,*,#57475,.F.);
#82881=ORIENTED_EDGE('',*,*,#55581,.F.);
#82882=ORIENTED_EDGE('',*,*,#57474,.T.);
#82883=ORIENTED_EDGE('',*,*,#55574,.F.);
#82884=ORIENTED_EDGE('',*,*,#57476,.F.);
#82885=ORIENTED_EDGE('',*,*,#53590,.F.);
#82886=ORIENTED_EDGE('',*,*,#57475,.T.);
#82887=ORIENTED_EDGE('',*,*,#53578,.F.);
#82888=ORIENTED_EDGE('',*,*,#57477,.F.);
#82889=ORIENTED_EDGE('',*,*,#55582,.F.);
#82890=ORIENTED_EDGE('',*,*,#57476,.T.);
#82891=ORIENTED_EDGE('',*,*,#55585,.F.);
#82892=ORIENTED_EDGE('',*,*,#57478,.F.);
#82893=ORIENTED_EDGE('',*,*,#53569,.F.);
#82894=ORIENTED_EDGE('',*,*,#57477,.T.);
#82895=ORIENTED_EDGE('',*,*,#53596,.F.);
#82896=ORIENTED_EDGE('',*,*,#57479,.F.);
#82897=ORIENTED_EDGE('',*,*,#55583,.F.);
#82898=ORIENTED_EDGE('',*,*,#57478,.T.);
#82899=ORIENTED_EDGE('',*,*,#55584,.F.);
#82900=ORIENTED_EDGE('',*,*,#57479,.T.);
#82901=ORIENTED_EDGE('',*,*,#53574,.F.);
#82902=ORIENTED_EDGE('',*,*,#53570,.T.);
#82903=ORIENTED_EDGE('',*,*,#57480,.F.);
#82904=ORIENTED_EDGE('',*,*,#55624,.F.);
#82905=ORIENTED_EDGE('',*,*,#57481,.F.);
#82906=ORIENTED_EDGE('',*,*,#53526,.F.);
#82907=ORIENTED_EDGE('',*,*,#57481,.T.);
#82908=ORIENTED_EDGE('',*,*,#55623,.F.);
#82909=ORIENTED_EDGE('',*,*,#57482,.F.);
#82910=ORIENTED_EDGE('',*,*,#53535,.F.);
#82911=ORIENTED_EDGE('',*,*,#53525,.T.);
#82912=ORIENTED_EDGE('',*,*,#53529,.F.);
#82913=ORIENTED_EDGE('',*,*,#57483,.F.);
#82914=ORIENTED_EDGE('',*,*,#55625,.F.);
#82915=ORIENTED_EDGE('',*,*,#57480,.T.);
#82916=ORIENTED_EDGE('',*,*,#57482,.T.);
#82917=ORIENTED_EDGE('',*,*,#55622,.F.);
#82918=ORIENTED_EDGE('',*,*,#57484,.F.);
#82919=ORIENTED_EDGE('',*,*,#53520,.F.);
#82920=ORIENTED_EDGE('',*,*,#57483,.T.);
#82921=ORIENTED_EDGE('',*,*,#53533,.F.);
#82922=ORIENTED_EDGE('',*,*,#57485,.F.);
#82923=ORIENTED_EDGE('',*,*,#55614,.F.);
#82924=ORIENTED_EDGE('',*,*,#57484,.T.);
#82925=ORIENTED_EDGE('',*,*,#55621,.F.);
#82926=ORIENTED_EDGE('',*,*,#57486,.F.);
#82927=ORIENTED_EDGE('',*,*,#53537,.F.);
#82928=ORIENTED_EDGE('',*,*,#57485,.T.);
#82929=ORIENTED_EDGE('',*,*,#52276,.F.);
#82930=ORIENTED_EDGE('',*,*,#57487,.F.);
#82931=ORIENTED_EDGE('',*,*,#55615,.F.);
#82932=ORIENTED_EDGE('',*,*,#57486,.T.);
#82933=ORIENTED_EDGE('',*,*,#55620,.F.);
#82934=ORIENTED_EDGE('',*,*,#57488,.F.);
#82935=ORIENTED_EDGE('',*,*,#53512,.T.);
#82936=ORIENTED_EDGE('',*,*,#53516,.F.);
#82937=ORIENTED_EDGE('',*,*,#57487,.T.);
#82938=ORIENTED_EDGE('',*,*,#52275,.F.);
#82939=ORIENTED_EDGE('',*,*,#57489,.F.);
#82940=ORIENTED_EDGE('',*,*,#56432,.F.);
#82941=ORIENTED_EDGE('',*,*,#57488,.T.);
#82942=ORIENTED_EDGE('',*,*,#55619,.F.);
#82943=ORIENTED_EDGE('',*,*,#57490,.F.);
#82944=ORIENTED_EDGE('',*,*,#53513,.F.);
#82945=ORIENTED_EDGE('',*,*,#57489,.T.);
#82946=ORIENTED_EDGE('',*,*,#52274,.F.);
#82947=ORIENTED_EDGE('',*,*,#57491,.F.);
#82948=ORIENTED_EDGE('',*,*,#55599,.F.);
#82949=ORIENTED_EDGE('',*,*,#57490,.T.);
#82950=ORIENTED_EDGE('',*,*,#55618,.F.);
#82951=ORIENTED_EDGE('',*,*,#57492,.F.);
#82952=ORIENTED_EDGE('',*,*,#53531,.F.);
#82953=ORIENTED_EDGE('',*,*,#57491,.T.);
#82954=ORIENTED_EDGE('',*,*,#52273,.F.);
#82955=ORIENTED_EDGE('',*,*,#57493,.F.);
#82956=ORIENTED_EDGE('',*,*,#56434,.F.);
#82957=ORIENTED_EDGE('',*,*,#57492,.T.);
#82958=ORIENTED_EDGE('',*,*,#55617,.F.);
#82959=ORIENTED_EDGE('',*,*,#57494,.F.);
#82960=ORIENTED_EDGE('',*,*,#52751,.F.);
#82961=ORIENTED_EDGE('',*,*,#57493,.T.);
#82962=ORIENTED_EDGE('',*,*,#52272,.F.);
#82963=ORIENTED_EDGE('',*,*,#57495,.F.);
#82964=ORIENTED_EDGE('',*,*,#55605,.F.);
#82965=ORIENTED_EDGE('',*,*,#57494,.T.);
#82966=ORIENTED_EDGE('',*,*,#56433,.F.);
#82967=ORIENTED_EDGE('',*,*,#57496,.F.);
#82968=ORIENTED_EDGE('',*,*,#52752,.F.);
#82969=ORIENTED_EDGE('',*,*,#57495,.T.);
#82970=ORIENTED_EDGE('',*,*,#53562,.F.);
#82971=ORIENTED_EDGE('',*,*,#57497,.F.);
#82972=ORIENTED_EDGE('',*,*,#55606,.F.);
#82973=ORIENTED_EDGE('',*,*,#57496,.T.);
#82974=ORIENTED_EDGE('',*,*,#55601,.F.);
#82975=ORIENTED_EDGE('',*,*,#57498,.F.);
#82976=ORIENTED_EDGE('',*,*,#52753,.F.);
#82977=ORIENTED_EDGE('',*,*,#53557,.F.);
#82978=ORIENTED_EDGE('',*,*,#53553,.T.);
#82979=ORIENTED_EDGE('',*,*,#57499,.F.);
#82980=ORIENTED_EDGE('',*,*,#55607,.F.);
#82981=ORIENTED_EDGE('',*,*,#57497,.T.);
#82982=ORIENTED_EDGE('',*,*,#57498,.T.);
#82983=ORIENTED_EDGE('',*,*,#56435,.F.);
#82984=ORIENTED_EDGE('',*,*,#57500,.F.);
#82985=ORIENTED_EDGE('',*,*,#52754,.F.);
#82986=ORIENTED_EDGE('',*,*,#57499,.T.);
#82987=ORIENTED_EDGE('',*,*,#53552,.F.);
#82988=ORIENTED_EDGE('',*,*,#57501,.F.);
#82989=ORIENTED_EDGE('',*,*,#55608,.F.);
#82990=ORIENTED_EDGE('',*,*,#57500,.T.);
#82991=ORIENTED_EDGE('',*,*,#55603,.F.);
#82992=ORIENTED_EDGE('',*,*,#57502,.F.);
#82993=ORIENTED_EDGE('',*,*,#52755,.F.);
#82994=ORIENTED_EDGE('',*,*,#57501,.T.);
#82995=ORIENTED_EDGE('',*,*,#53564,.F.);
#82996=ORIENTED_EDGE('',*,*,#57503,.F.);
#82997=ORIENTED_EDGE('',*,*,#55609,.F.);
#82998=ORIENTED_EDGE('',*,*,#57502,.T.);
#82999=ORIENTED_EDGE('',*,*,#55602,.F.);
#83000=ORIENTED_EDGE('',*,*,#57504,.F.);
#83001=ORIENTED_EDGE('',*,*,#53560,.F.);
#83002=ORIENTED_EDGE('',*,*,#57503,.T.);
#83003=ORIENTED_EDGE('',*,*,#53548,.F.);
#83004=ORIENTED_EDGE('',*,*,#57505,.F.);
#83005=ORIENTED_EDGE('',*,*,#55610,.F.);
#83006=ORIENTED_EDGE('',*,*,#57504,.T.);
#83007=ORIENTED_EDGE('',*,*,#55613,.F.);
#83008=ORIENTED_EDGE('',*,*,#57506,.F.);
#83009=ORIENTED_EDGE('',*,*,#53539,.F.);
#83010=ORIENTED_EDGE('',*,*,#57505,.T.);
#83011=ORIENTED_EDGE('',*,*,#53566,.F.);
#83012=ORIENTED_EDGE('',*,*,#57507,.F.);
#83013=ORIENTED_EDGE('',*,*,#55611,.F.);
#83014=ORIENTED_EDGE('',*,*,#57506,.T.);
#83015=ORIENTED_EDGE('',*,*,#55612,.F.);
#83016=ORIENTED_EDGE('',*,*,#57507,.T.);
#83017=ORIENTED_EDGE('',*,*,#53544,.F.);
#83018=ORIENTED_EDGE('',*,*,#53540,.T.);
#83019=ORIENTED_EDGE('',*,*,#57508,.F.);
#83020=ORIENTED_EDGE('',*,*,#55652,.F.);
#83021=ORIENTED_EDGE('',*,*,#57509,.F.);
#83022=ORIENTED_EDGE('',*,*,#53496,.F.);
#83023=ORIENTED_EDGE('',*,*,#57509,.T.);
#83024=ORIENTED_EDGE('',*,*,#55651,.F.);
#83025=ORIENTED_EDGE('',*,*,#57510,.F.);
#83026=ORIENTED_EDGE('',*,*,#53505,.F.);
#83027=ORIENTED_EDGE('',*,*,#53495,.T.);
#83028=ORIENTED_EDGE('',*,*,#53499,.F.);
#83029=ORIENTED_EDGE('',*,*,#57511,.F.);
#83030=ORIENTED_EDGE('',*,*,#55653,.F.);
#83031=ORIENTED_EDGE('',*,*,#57508,.T.);
#83032=ORIENTED_EDGE('',*,*,#57510,.T.);
#83033=ORIENTED_EDGE('',*,*,#55650,.F.);
#83034=ORIENTED_EDGE('',*,*,#57512,.F.);
#83035=ORIENTED_EDGE('',*,*,#53490,.F.);
#83036=ORIENTED_EDGE('',*,*,#57511,.T.);
#83037=ORIENTED_EDGE('',*,*,#53503,.F.);
#83038=ORIENTED_EDGE('',*,*,#57513,.F.);
#83039=ORIENTED_EDGE('',*,*,#55642,.F.);
#83040=ORIENTED_EDGE('',*,*,#57512,.T.);
#83041=ORIENTED_EDGE('',*,*,#55649,.F.);
#83042=ORIENTED_EDGE('',*,*,#57514,.F.);
#83043=ORIENTED_EDGE('',*,*,#53507,.F.);
#83044=ORIENTED_EDGE('',*,*,#57513,.T.);
#83045=ORIENTED_EDGE('',*,*,#52282,.F.);
#83046=ORIENTED_EDGE('',*,*,#57515,.F.);
#83047=ORIENTED_EDGE('',*,*,#55643,.F.);
#83048=ORIENTED_EDGE('',*,*,#57514,.T.);
#83049=ORIENTED_EDGE('',*,*,#55648,.F.);
#83050=ORIENTED_EDGE('',*,*,#57516,.F.);
#83051=ORIENTED_EDGE('',*,*,#53482,.T.);
#83052=ORIENTED_EDGE('',*,*,#53486,.F.);
#83053=ORIENTED_EDGE('',*,*,#57515,.T.);
#83054=ORIENTED_EDGE('',*,*,#52281,.F.);
#83055=ORIENTED_EDGE('',*,*,#57517,.F.);
#83056=ORIENTED_EDGE('',*,*,#56436,.F.);
#83057=ORIENTED_EDGE('',*,*,#57516,.T.);
#83058=ORIENTED_EDGE('',*,*,#55647,.F.);
#83059=ORIENTED_EDGE('',*,*,#57518,.F.);
#83060=ORIENTED_EDGE('',*,*,#53483,.F.);
#83061=ORIENTED_EDGE('',*,*,#57517,.T.);
#83062=ORIENTED_EDGE('',*,*,#52280,.F.);
#83063=ORIENTED_EDGE('',*,*,#57519,.F.);
#83064=ORIENTED_EDGE('',*,*,#55627,.F.);
#83065=ORIENTED_EDGE('',*,*,#57518,.T.);
#83066=ORIENTED_EDGE('',*,*,#55646,.F.);
#83067=ORIENTED_EDGE('',*,*,#57520,.F.);
#83068=ORIENTED_EDGE('',*,*,#53501,.F.);
#83069=ORIENTED_EDGE('',*,*,#57519,.T.);
#83070=ORIENTED_EDGE('',*,*,#52279,.F.);
#83071=ORIENTED_EDGE('',*,*,#57521,.F.);
#83072=ORIENTED_EDGE('',*,*,#56438,.F.);
#83073=ORIENTED_EDGE('',*,*,#57520,.T.);
#83074=ORIENTED_EDGE('',*,*,#55645,.F.);
#83075=ORIENTED_EDGE('',*,*,#57522,.F.);
#83076=ORIENTED_EDGE('',*,*,#52745,.F.);
#83077=ORIENTED_EDGE('',*,*,#57521,.T.);
#83078=ORIENTED_EDGE('',*,*,#52278,.F.);
#83079=ORIENTED_EDGE('',*,*,#57523,.F.);
#83080=ORIENTED_EDGE('',*,*,#55633,.F.);
#83081=ORIENTED_EDGE('',*,*,#57522,.T.);
#83082=ORIENTED_EDGE('',*,*,#56437,.F.);
#83083=ORIENTED_EDGE('',*,*,#57524,.F.);
#83084=ORIENTED_EDGE('',*,*,#52746,.F.);
#83085=ORIENTED_EDGE('',*,*,#57523,.T.);
#83086=ORIENTED_EDGE('',*,*,#53532,.F.);
#83087=ORIENTED_EDGE('',*,*,#57525,.F.);
#83088=ORIENTED_EDGE('',*,*,#55634,.F.);
#83089=ORIENTED_EDGE('',*,*,#57524,.T.);
#83090=ORIENTED_EDGE('',*,*,#55629,.F.);
#83091=ORIENTED_EDGE('',*,*,#57526,.F.);
#83092=ORIENTED_EDGE('',*,*,#52747,.F.);
#83093=ORIENTED_EDGE('',*,*,#53527,.F.);
#83094=ORIENTED_EDGE('',*,*,#53523,.T.);
#83095=ORIENTED_EDGE('',*,*,#57527,.F.);
#83096=ORIENTED_EDGE('',*,*,#55635,.F.);
#83097=ORIENTED_EDGE('',*,*,#57525,.T.);
#83098=ORIENTED_EDGE('',*,*,#57526,.T.);
#83099=ORIENTED_EDGE('',*,*,#56439,.F.);
#83100=ORIENTED_EDGE('',*,*,#57528,.F.);
#83101=ORIENTED_EDGE('',*,*,#52748,.F.);
#83102=ORIENTED_EDGE('',*,*,#57527,.T.);
#83103=ORIENTED_EDGE('',*,*,#53522,.F.);
#83104=ORIENTED_EDGE('',*,*,#57529,.F.);
#83105=ORIENTED_EDGE('',*,*,#55636,.F.);
#83106=ORIENTED_EDGE('',*,*,#57528,.T.);
#83107=ORIENTED_EDGE('',*,*,#55631,.F.);
#83108=ORIENTED_EDGE('',*,*,#57530,.F.);
#83109=ORIENTED_EDGE('',*,*,#52749,.F.);
#83110=ORIENTED_EDGE('',*,*,#57529,.T.);
#83111=ORIENTED_EDGE('',*,*,#53534,.F.);
#83112=ORIENTED_EDGE('',*,*,#57531,.F.);
#83113=ORIENTED_EDGE('',*,*,#55637,.F.);
#83114=ORIENTED_EDGE('',*,*,#57530,.T.);
#83115=ORIENTED_EDGE('',*,*,#55630,.F.);
#83116=ORIENTED_EDGE('',*,*,#57532,.F.);
#83117=ORIENTED_EDGE('',*,*,#53530,.F.);
#83118=ORIENTED_EDGE('',*,*,#57531,.T.);
#83119=ORIENTED_EDGE('',*,*,#53518,.F.);
#83120=ORIENTED_EDGE('',*,*,#57533,.F.);
#83121=ORIENTED_EDGE('',*,*,#55638,.F.);
#83122=ORIENTED_EDGE('',*,*,#57532,.T.);
#83123=ORIENTED_EDGE('',*,*,#55641,.F.);
#83124=ORIENTED_EDGE('',*,*,#57534,.F.);
#83125=ORIENTED_EDGE('',*,*,#53509,.F.);
#83126=ORIENTED_EDGE('',*,*,#57533,.T.);
#83127=ORIENTED_EDGE('',*,*,#53536,.F.);
#83128=ORIENTED_EDGE('',*,*,#57535,.F.);
#83129=ORIENTED_EDGE('',*,*,#55639,.F.);
#83130=ORIENTED_EDGE('',*,*,#57534,.T.);
#83131=ORIENTED_EDGE('',*,*,#55640,.F.);
#83132=ORIENTED_EDGE('',*,*,#57535,.T.);
#83133=ORIENTED_EDGE('',*,*,#53514,.F.);
#83134=ORIENTED_EDGE('',*,*,#53510,.T.);
#83135=ORIENTED_EDGE('',*,*,#57536,.F.);
#83136=ORIENTED_EDGE('',*,*,#55680,.F.);
#83137=ORIENTED_EDGE('',*,*,#57537,.F.);
#83138=ORIENTED_EDGE('',*,*,#53466,.F.);
#83139=ORIENTED_EDGE('',*,*,#57537,.T.);
#83140=ORIENTED_EDGE('',*,*,#55679,.F.);
#83141=ORIENTED_EDGE('',*,*,#57538,.F.);
#83142=ORIENTED_EDGE('',*,*,#53475,.F.);
#83143=ORIENTED_EDGE('',*,*,#53465,.T.);
#83144=ORIENTED_EDGE('',*,*,#53469,.F.);
#83145=ORIENTED_EDGE('',*,*,#57539,.F.);
#83146=ORIENTED_EDGE('',*,*,#55681,.F.);
#83147=ORIENTED_EDGE('',*,*,#57536,.T.);
#83148=ORIENTED_EDGE('',*,*,#57538,.T.);
#83149=ORIENTED_EDGE('',*,*,#55678,.F.);
#83150=ORIENTED_EDGE('',*,*,#57540,.F.);
#83151=ORIENTED_EDGE('',*,*,#53460,.F.);
#83152=ORIENTED_EDGE('',*,*,#57539,.T.);
#83153=ORIENTED_EDGE('',*,*,#53473,.F.);
#83154=ORIENTED_EDGE('',*,*,#57541,.F.);
#83155=ORIENTED_EDGE('',*,*,#55670,.F.);
#83156=ORIENTED_EDGE('',*,*,#57540,.T.);
#83157=ORIENTED_EDGE('',*,*,#55677,.F.);
#83158=ORIENTED_EDGE('',*,*,#57542,.F.);
#83159=ORIENTED_EDGE('',*,*,#53477,.F.);
#83160=ORIENTED_EDGE('',*,*,#57541,.T.);
#83161=ORIENTED_EDGE('',*,*,#52288,.F.);
#83162=ORIENTED_EDGE('',*,*,#57543,.F.);
#83163=ORIENTED_EDGE('',*,*,#55671,.F.);
#83164=ORIENTED_EDGE('',*,*,#57542,.T.);
#83165=ORIENTED_EDGE('',*,*,#55676,.F.);
#83166=ORIENTED_EDGE('',*,*,#57544,.F.);
#83167=ORIENTED_EDGE('',*,*,#53452,.T.);
#83168=ORIENTED_EDGE('',*,*,#53456,.F.);
#83169=ORIENTED_EDGE('',*,*,#57543,.T.);
#83170=ORIENTED_EDGE('',*,*,#52287,.F.);
#83171=ORIENTED_EDGE('',*,*,#57545,.F.);
#83172=ORIENTED_EDGE('',*,*,#56440,.F.);
#83173=ORIENTED_EDGE('',*,*,#57544,.T.);
#83174=ORIENTED_EDGE('',*,*,#55675,.F.);
#83175=ORIENTED_EDGE('',*,*,#57546,.F.);
#83176=ORIENTED_EDGE('',*,*,#53453,.F.);
#83177=ORIENTED_EDGE('',*,*,#57545,.T.);
#83178=ORIENTED_EDGE('',*,*,#52286,.F.);
#83179=ORIENTED_EDGE('',*,*,#57547,.F.);
#83180=ORIENTED_EDGE('',*,*,#55655,.F.);
#83181=ORIENTED_EDGE('',*,*,#57546,.T.);
#83182=ORIENTED_EDGE('',*,*,#55674,.F.);
#83183=ORIENTED_EDGE('',*,*,#57548,.F.);
#83184=ORIENTED_EDGE('',*,*,#53471,.F.);
#83185=ORIENTED_EDGE('',*,*,#57547,.T.);
#83186=ORIENTED_EDGE('',*,*,#52285,.F.);
#83187=ORIENTED_EDGE('',*,*,#57549,.F.);
#83188=ORIENTED_EDGE('',*,*,#56442,.F.);
#83189=ORIENTED_EDGE('',*,*,#57548,.T.);
#83190=ORIENTED_EDGE('',*,*,#55673,.F.);
#83191=ORIENTED_EDGE('',*,*,#57550,.F.);
#83192=ORIENTED_EDGE('',*,*,#52739,.F.);
#83193=ORIENTED_EDGE('',*,*,#57549,.T.);
#83194=ORIENTED_EDGE('',*,*,#52284,.F.);
#83195=ORIENTED_EDGE('',*,*,#57551,.F.);
#83196=ORIENTED_EDGE('',*,*,#55661,.F.);
#83197=ORIENTED_EDGE('',*,*,#57550,.T.);
#83198=ORIENTED_EDGE('',*,*,#56441,.F.);
#83199=ORIENTED_EDGE('',*,*,#57552,.F.);
#83200=ORIENTED_EDGE('',*,*,#52740,.F.);
#83201=ORIENTED_EDGE('',*,*,#57551,.T.);
#83202=ORIENTED_EDGE('',*,*,#53502,.F.);
#83203=ORIENTED_EDGE('',*,*,#57553,.F.);
#83204=ORIENTED_EDGE('',*,*,#55662,.F.);
#83205=ORIENTED_EDGE('',*,*,#57552,.T.);
#83206=ORIENTED_EDGE('',*,*,#55657,.F.);
#83207=ORIENTED_EDGE('',*,*,#57554,.F.);
#83208=ORIENTED_EDGE('',*,*,#52741,.F.);
#83209=ORIENTED_EDGE('',*,*,#53497,.F.);
#83210=ORIENTED_EDGE('',*,*,#53493,.T.);
#83211=ORIENTED_EDGE('',*,*,#57555,.F.);
#83212=ORIENTED_EDGE('',*,*,#55663,.F.);
#83213=ORIENTED_EDGE('',*,*,#57553,.T.);
#83214=ORIENTED_EDGE('',*,*,#57554,.T.);
#83215=ORIENTED_EDGE('',*,*,#56443,.F.);
#83216=ORIENTED_EDGE('',*,*,#57556,.F.);
#83217=ORIENTED_EDGE('',*,*,#52742,.F.);
#83218=ORIENTED_EDGE('',*,*,#57555,.T.);
#83219=ORIENTED_EDGE('',*,*,#53492,.F.);
#83220=ORIENTED_EDGE('',*,*,#57557,.F.);
#83221=ORIENTED_EDGE('',*,*,#55664,.F.);
#83222=ORIENTED_EDGE('',*,*,#57556,.T.);
#83223=ORIENTED_EDGE('',*,*,#55659,.F.);
#83224=ORIENTED_EDGE('',*,*,#57558,.F.);
#83225=ORIENTED_EDGE('',*,*,#52743,.F.);
#83226=ORIENTED_EDGE('',*,*,#57557,.T.);
#83227=ORIENTED_EDGE('',*,*,#53504,.F.);
#83228=ORIENTED_EDGE('',*,*,#57559,.F.);
#83229=ORIENTED_EDGE('',*,*,#55665,.F.);
#83230=ORIENTED_EDGE('',*,*,#57558,.T.);
#83231=ORIENTED_EDGE('',*,*,#55658,.F.);
#83232=ORIENTED_EDGE('',*,*,#57560,.F.);
#83233=ORIENTED_EDGE('',*,*,#53500,.F.);
#83234=ORIENTED_EDGE('',*,*,#57559,.T.);
#83235=ORIENTED_EDGE('',*,*,#53488,.F.);
#83236=ORIENTED_EDGE('',*,*,#57561,.F.);
#83237=ORIENTED_EDGE('',*,*,#55666,.F.);
#83238=ORIENTED_EDGE('',*,*,#57560,.T.);
#83239=ORIENTED_EDGE('',*,*,#55669,.F.);
#83240=ORIENTED_EDGE('',*,*,#57562,.F.);
#83241=ORIENTED_EDGE('',*,*,#53479,.F.);
#83242=ORIENTED_EDGE('',*,*,#57561,.T.);
#83243=ORIENTED_EDGE('',*,*,#53506,.F.);
#83244=ORIENTED_EDGE('',*,*,#57563,.F.);
#83245=ORIENTED_EDGE('',*,*,#55667,.F.);
#83246=ORIENTED_EDGE('',*,*,#57562,.T.);
#83247=ORIENTED_EDGE('',*,*,#55668,.F.);
#83248=ORIENTED_EDGE('',*,*,#57563,.T.);
#83249=ORIENTED_EDGE('',*,*,#53484,.F.);
#83250=ORIENTED_EDGE('',*,*,#53480,.T.);
#83251=ORIENTED_EDGE('',*,*,#57564,.F.);
#83252=ORIENTED_EDGE('',*,*,#55708,.F.);
#83253=ORIENTED_EDGE('',*,*,#57565,.F.);
#83254=ORIENTED_EDGE('',*,*,#53436,.F.);
#83255=ORIENTED_EDGE('',*,*,#57565,.T.);
#83256=ORIENTED_EDGE('',*,*,#55707,.F.);
#83257=ORIENTED_EDGE('',*,*,#57566,.F.);
#83258=ORIENTED_EDGE('',*,*,#53445,.F.);
#83259=ORIENTED_EDGE('',*,*,#53435,.T.);
#83260=ORIENTED_EDGE('',*,*,#53439,.F.);
#83261=ORIENTED_EDGE('',*,*,#57567,.F.);
#83262=ORIENTED_EDGE('',*,*,#55709,.F.);
#83263=ORIENTED_EDGE('',*,*,#57564,.T.);
#83264=ORIENTED_EDGE('',*,*,#57566,.T.);
#83265=ORIENTED_EDGE('',*,*,#55706,.F.);
#83266=ORIENTED_EDGE('',*,*,#57568,.F.);
#83267=ORIENTED_EDGE('',*,*,#53430,.F.);
#83268=ORIENTED_EDGE('',*,*,#57567,.T.);
#83269=ORIENTED_EDGE('',*,*,#53443,.F.);
#83270=ORIENTED_EDGE('',*,*,#57569,.F.);
#83271=ORIENTED_EDGE('',*,*,#55698,.F.);
#83272=ORIENTED_EDGE('',*,*,#57568,.T.);
#83273=ORIENTED_EDGE('',*,*,#55705,.F.);
#83274=ORIENTED_EDGE('',*,*,#57570,.F.);
#83275=ORIENTED_EDGE('',*,*,#53447,.F.);
#83276=ORIENTED_EDGE('',*,*,#57569,.T.);
#83277=ORIENTED_EDGE('',*,*,#52294,.F.);
#83278=ORIENTED_EDGE('',*,*,#57571,.F.);
#83279=ORIENTED_EDGE('',*,*,#55699,.F.);
#83280=ORIENTED_EDGE('',*,*,#57570,.T.);
#83281=ORIENTED_EDGE('',*,*,#55704,.F.);
#83282=ORIENTED_EDGE('',*,*,#57572,.F.);
#83283=ORIENTED_EDGE('',*,*,#53422,.T.);
#83284=ORIENTED_EDGE('',*,*,#53426,.F.);
#83285=ORIENTED_EDGE('',*,*,#57571,.T.);
#83286=ORIENTED_EDGE('',*,*,#52293,.F.);
#83287=ORIENTED_EDGE('',*,*,#57573,.F.);
#83288=ORIENTED_EDGE('',*,*,#56444,.F.);
#83289=ORIENTED_EDGE('',*,*,#57572,.T.);
#83290=ORIENTED_EDGE('',*,*,#55703,.F.);
#83291=ORIENTED_EDGE('',*,*,#57574,.F.);
#83292=ORIENTED_EDGE('',*,*,#53423,.F.);
#83293=ORIENTED_EDGE('',*,*,#57573,.T.);
#83294=ORIENTED_EDGE('',*,*,#52292,.F.);
#83295=ORIENTED_EDGE('',*,*,#57575,.F.);
#83296=ORIENTED_EDGE('',*,*,#55683,.F.);
#83297=ORIENTED_EDGE('',*,*,#57574,.T.);
#83298=ORIENTED_EDGE('',*,*,#55702,.F.);
#83299=ORIENTED_EDGE('',*,*,#57576,.F.);
#83300=ORIENTED_EDGE('',*,*,#53441,.F.);
#83301=ORIENTED_EDGE('',*,*,#57575,.T.);
#83302=ORIENTED_EDGE('',*,*,#52291,.F.);
#83303=ORIENTED_EDGE('',*,*,#57577,.F.);
#83304=ORIENTED_EDGE('',*,*,#56446,.F.);
#83305=ORIENTED_EDGE('',*,*,#57576,.T.);
#83306=ORIENTED_EDGE('',*,*,#55701,.F.);
#83307=ORIENTED_EDGE('',*,*,#57578,.F.);
#83308=ORIENTED_EDGE('',*,*,#52733,.F.);
#83309=ORIENTED_EDGE('',*,*,#57577,.T.);
#83310=ORIENTED_EDGE('',*,*,#52290,.F.);
#83311=ORIENTED_EDGE('',*,*,#57579,.F.);
#83312=ORIENTED_EDGE('',*,*,#55689,.F.);
#83313=ORIENTED_EDGE('',*,*,#57578,.T.);
#83314=ORIENTED_EDGE('',*,*,#56445,.F.);
#83315=ORIENTED_EDGE('',*,*,#57580,.F.);
#83316=ORIENTED_EDGE('',*,*,#52734,.F.);
#83317=ORIENTED_EDGE('',*,*,#57579,.T.);
#83318=ORIENTED_EDGE('',*,*,#53472,.F.);
#83319=ORIENTED_EDGE('',*,*,#57581,.F.);
#83320=ORIENTED_EDGE('',*,*,#55690,.F.);
#83321=ORIENTED_EDGE('',*,*,#57580,.T.);
#83322=ORIENTED_EDGE('',*,*,#55685,.F.);
#83323=ORIENTED_EDGE('',*,*,#57582,.F.);
#83324=ORIENTED_EDGE('',*,*,#52735,.F.);
#83325=ORIENTED_EDGE('',*,*,#53467,.F.);
#83326=ORIENTED_EDGE('',*,*,#53463,.T.);
#83327=ORIENTED_EDGE('',*,*,#57583,.F.);
#83328=ORIENTED_EDGE('',*,*,#55691,.F.);
#83329=ORIENTED_EDGE('',*,*,#57581,.T.);
#83330=ORIENTED_EDGE('',*,*,#57582,.T.);
#83331=ORIENTED_EDGE('',*,*,#56447,.F.);
#83332=ORIENTED_EDGE('',*,*,#57584,.F.);
#83333=ORIENTED_EDGE('',*,*,#52736,.F.);
#83334=ORIENTED_EDGE('',*,*,#57583,.T.);
#83335=ORIENTED_EDGE('',*,*,#53462,.F.);
#83336=ORIENTED_EDGE('',*,*,#57585,.F.);
#83337=ORIENTED_EDGE('',*,*,#55692,.F.);
#83338=ORIENTED_EDGE('',*,*,#57584,.T.);
#83339=ORIENTED_EDGE('',*,*,#55687,.F.);
#83340=ORIENTED_EDGE('',*,*,#57586,.F.);
#83341=ORIENTED_EDGE('',*,*,#52737,.F.);
#83342=ORIENTED_EDGE('',*,*,#57585,.T.);
#83343=ORIENTED_EDGE('',*,*,#53474,.F.);
#83344=ORIENTED_EDGE('',*,*,#57587,.F.);
#83345=ORIENTED_EDGE('',*,*,#55693,.F.);
#83346=ORIENTED_EDGE('',*,*,#57586,.T.);
#83347=ORIENTED_EDGE('',*,*,#55686,.F.);
#83348=ORIENTED_EDGE('',*,*,#57588,.F.);
#83349=ORIENTED_EDGE('',*,*,#53470,.F.);
#83350=ORIENTED_EDGE('',*,*,#57587,.T.);
#83351=ORIENTED_EDGE('',*,*,#53458,.F.);
#83352=ORIENTED_EDGE('',*,*,#57589,.F.);
#83353=ORIENTED_EDGE('',*,*,#55694,.F.);
#83354=ORIENTED_EDGE('',*,*,#57588,.T.);
#83355=ORIENTED_EDGE('',*,*,#55697,.F.);
#83356=ORIENTED_EDGE('',*,*,#57590,.F.);
#83357=ORIENTED_EDGE('',*,*,#53449,.F.);
#83358=ORIENTED_EDGE('',*,*,#57589,.T.);
#83359=ORIENTED_EDGE('',*,*,#53476,.F.);
#83360=ORIENTED_EDGE('',*,*,#57591,.F.);
#83361=ORIENTED_EDGE('',*,*,#55695,.F.);
#83362=ORIENTED_EDGE('',*,*,#57590,.T.);
#83363=ORIENTED_EDGE('',*,*,#55696,.F.);
#83364=ORIENTED_EDGE('',*,*,#57591,.T.);
#83365=ORIENTED_EDGE('',*,*,#53454,.F.);
#83366=ORIENTED_EDGE('',*,*,#53450,.T.);
#83367=ORIENTED_EDGE('',*,*,#57592,.F.);
#83368=ORIENTED_EDGE('',*,*,#55736,.F.);
#83369=ORIENTED_EDGE('',*,*,#57593,.F.);
#83370=ORIENTED_EDGE('',*,*,#53406,.F.);
#83371=ORIENTED_EDGE('',*,*,#57593,.T.);
#83372=ORIENTED_EDGE('',*,*,#55735,.F.);
#83373=ORIENTED_EDGE('',*,*,#57594,.F.);
#83374=ORIENTED_EDGE('',*,*,#53415,.F.);
#83375=ORIENTED_EDGE('',*,*,#53405,.T.);
#83376=ORIENTED_EDGE('',*,*,#53409,.F.);
#83377=ORIENTED_EDGE('',*,*,#57595,.F.);
#83378=ORIENTED_EDGE('',*,*,#55737,.F.);
#83379=ORIENTED_EDGE('',*,*,#57592,.T.);
#83380=ORIENTED_EDGE('',*,*,#57594,.T.);
#83381=ORIENTED_EDGE('',*,*,#55734,.F.);
#83382=ORIENTED_EDGE('',*,*,#57596,.F.);
#83383=ORIENTED_EDGE('',*,*,#53400,.F.);
#83384=ORIENTED_EDGE('',*,*,#57595,.T.);
#83385=ORIENTED_EDGE('',*,*,#53413,.F.);
#83386=ORIENTED_EDGE('',*,*,#57597,.F.);
#83387=ORIENTED_EDGE('',*,*,#55726,.F.);
#83388=ORIENTED_EDGE('',*,*,#57596,.T.);
#83389=ORIENTED_EDGE('',*,*,#55733,.F.);
#83390=ORIENTED_EDGE('',*,*,#57598,.F.);
#83391=ORIENTED_EDGE('',*,*,#53417,.F.);
#83392=ORIENTED_EDGE('',*,*,#57597,.T.);
#83393=ORIENTED_EDGE('',*,*,#52300,.F.);
#83394=ORIENTED_EDGE('',*,*,#57599,.F.);
#83395=ORIENTED_EDGE('',*,*,#55727,.F.);
#83396=ORIENTED_EDGE('',*,*,#57598,.T.);
#83397=ORIENTED_EDGE('',*,*,#55732,.F.);
#83398=ORIENTED_EDGE('',*,*,#57600,.F.);
#83399=ORIENTED_EDGE('',*,*,#53392,.T.);
#83400=ORIENTED_EDGE('',*,*,#53396,.F.);
#83401=ORIENTED_EDGE('',*,*,#57599,.T.);
#83402=ORIENTED_EDGE('',*,*,#52299,.F.);
#83403=ORIENTED_EDGE('',*,*,#57601,.F.);
#83404=ORIENTED_EDGE('',*,*,#56448,.F.);
#83405=ORIENTED_EDGE('',*,*,#57600,.T.);
#83406=ORIENTED_EDGE('',*,*,#55731,.F.);
#83407=ORIENTED_EDGE('',*,*,#57602,.F.);
#83408=ORIENTED_EDGE('',*,*,#53393,.F.);
#83409=ORIENTED_EDGE('',*,*,#57601,.T.);
#83410=ORIENTED_EDGE('',*,*,#52298,.F.);
#83411=ORIENTED_EDGE('',*,*,#57603,.F.);
#83412=ORIENTED_EDGE('',*,*,#55711,.F.);
#83413=ORIENTED_EDGE('',*,*,#57602,.T.);
#83414=ORIENTED_EDGE('',*,*,#55730,.F.);
#83415=ORIENTED_EDGE('',*,*,#57604,.F.);
#83416=ORIENTED_EDGE('',*,*,#53411,.F.);
#83417=ORIENTED_EDGE('',*,*,#57603,.T.);
#83418=ORIENTED_EDGE('',*,*,#52297,.F.);
#83419=ORIENTED_EDGE('',*,*,#57605,.F.);
#83420=ORIENTED_EDGE('',*,*,#56450,.F.);
#83421=ORIENTED_EDGE('',*,*,#57604,.T.);
#83422=ORIENTED_EDGE('',*,*,#55729,.F.);
#83423=ORIENTED_EDGE('',*,*,#57606,.F.);
#83424=ORIENTED_EDGE('',*,*,#52727,.F.);
#83425=ORIENTED_EDGE('',*,*,#57605,.T.);
#83426=ORIENTED_EDGE('',*,*,#52296,.F.);
#83427=ORIENTED_EDGE('',*,*,#57607,.F.);
#83428=ORIENTED_EDGE('',*,*,#55717,.F.);
#83429=ORIENTED_EDGE('',*,*,#57606,.T.);
#83430=ORIENTED_EDGE('',*,*,#56449,.F.);
#83431=ORIENTED_EDGE('',*,*,#57608,.F.);
#83432=ORIENTED_EDGE('',*,*,#52728,.F.);
#83433=ORIENTED_EDGE('',*,*,#57607,.T.);
#83434=ORIENTED_EDGE('',*,*,#53442,.F.);
#83435=ORIENTED_EDGE('',*,*,#57609,.F.);
#83436=ORIENTED_EDGE('',*,*,#55718,.F.);
#83437=ORIENTED_EDGE('',*,*,#57608,.T.);
#83438=ORIENTED_EDGE('',*,*,#55713,.F.);
#83439=ORIENTED_EDGE('',*,*,#57610,.F.);
#83440=ORIENTED_EDGE('',*,*,#52729,.F.);
#83441=ORIENTED_EDGE('',*,*,#53437,.F.);
#83442=ORIENTED_EDGE('',*,*,#53433,.T.);
#83443=ORIENTED_EDGE('',*,*,#57611,.F.);
#83444=ORIENTED_EDGE('',*,*,#55719,.F.);
#83445=ORIENTED_EDGE('',*,*,#57609,.T.);
#83446=ORIENTED_EDGE('',*,*,#57610,.T.);
#83447=ORIENTED_EDGE('',*,*,#56451,.F.);
#83448=ORIENTED_EDGE('',*,*,#57612,.F.);
#83449=ORIENTED_EDGE('',*,*,#52730,.F.);
#83450=ORIENTED_EDGE('',*,*,#57611,.T.);
#83451=ORIENTED_EDGE('',*,*,#53432,.F.);
#83452=ORIENTED_EDGE('',*,*,#57613,.F.);
#83453=ORIENTED_EDGE('',*,*,#55720,.F.);
#83454=ORIENTED_EDGE('',*,*,#57612,.T.);
#83455=ORIENTED_EDGE('',*,*,#55715,.F.);
#83456=ORIENTED_EDGE('',*,*,#57614,.F.);
#83457=ORIENTED_EDGE('',*,*,#52731,.F.);
#83458=ORIENTED_EDGE('',*,*,#57613,.T.);
#83459=ORIENTED_EDGE('',*,*,#53444,.F.);
#83460=ORIENTED_EDGE('',*,*,#57615,.F.);
#83461=ORIENTED_EDGE('',*,*,#55721,.F.);
#83462=ORIENTED_EDGE('',*,*,#57614,.T.);
#83463=ORIENTED_EDGE('',*,*,#55714,.F.);
#83464=ORIENTED_EDGE('',*,*,#57616,.F.);
#83465=ORIENTED_EDGE('',*,*,#53440,.F.);
#83466=ORIENTED_EDGE('',*,*,#57615,.T.);
#83467=ORIENTED_EDGE('',*,*,#53428,.F.);
#83468=ORIENTED_EDGE('',*,*,#57617,.F.);
#83469=ORIENTED_EDGE('',*,*,#55722,.F.);
#83470=ORIENTED_EDGE('',*,*,#57616,.T.);
#83471=ORIENTED_EDGE('',*,*,#55725,.F.);
#83472=ORIENTED_EDGE('',*,*,#57618,.F.);
#83473=ORIENTED_EDGE('',*,*,#53419,.F.);
#83474=ORIENTED_EDGE('',*,*,#57617,.T.);
#83475=ORIENTED_EDGE('',*,*,#53446,.F.);
#83476=ORIENTED_EDGE('',*,*,#57619,.F.);
#83477=ORIENTED_EDGE('',*,*,#55723,.F.);
#83478=ORIENTED_EDGE('',*,*,#57618,.T.);
#83479=ORIENTED_EDGE('',*,*,#55724,.F.);
#83480=ORIENTED_EDGE('',*,*,#57619,.T.);
#83481=ORIENTED_EDGE('',*,*,#53424,.F.);
#83482=ORIENTED_EDGE('',*,*,#53420,.T.);
#83483=ORIENTED_EDGE('',*,*,#57620,.F.);
#83484=ORIENTED_EDGE('',*,*,#55764,.F.);
#83485=ORIENTED_EDGE('',*,*,#57621,.F.);
#83486=ORIENTED_EDGE('',*,*,#53376,.F.);
#83487=ORIENTED_EDGE('',*,*,#57621,.T.);
#83488=ORIENTED_EDGE('',*,*,#55763,.F.);
#83489=ORIENTED_EDGE('',*,*,#57622,.F.);
#83490=ORIENTED_EDGE('',*,*,#53385,.F.);
#83491=ORIENTED_EDGE('',*,*,#53375,.T.);
#83492=ORIENTED_EDGE('',*,*,#53379,.F.);
#83493=ORIENTED_EDGE('',*,*,#57623,.F.);
#83494=ORIENTED_EDGE('',*,*,#55765,.F.);
#83495=ORIENTED_EDGE('',*,*,#57620,.T.);
#83496=ORIENTED_EDGE('',*,*,#57622,.T.);
#83497=ORIENTED_EDGE('',*,*,#55762,.F.);
#83498=ORIENTED_EDGE('',*,*,#57624,.F.);
#83499=ORIENTED_EDGE('',*,*,#53370,.F.);
#83500=ORIENTED_EDGE('',*,*,#57623,.T.);
#83501=ORIENTED_EDGE('',*,*,#53383,.F.);
#83502=ORIENTED_EDGE('',*,*,#57625,.F.);
#83503=ORIENTED_EDGE('',*,*,#55754,.F.);
#83504=ORIENTED_EDGE('',*,*,#57624,.T.);
#83505=ORIENTED_EDGE('',*,*,#55761,.F.);
#83506=ORIENTED_EDGE('',*,*,#57626,.F.);
#83507=ORIENTED_EDGE('',*,*,#53387,.F.);
#83508=ORIENTED_EDGE('',*,*,#57625,.T.);
#83509=ORIENTED_EDGE('',*,*,#52306,.F.);
#83510=ORIENTED_EDGE('',*,*,#57627,.F.);
#83511=ORIENTED_EDGE('',*,*,#55755,.F.);
#83512=ORIENTED_EDGE('',*,*,#57626,.T.);
#83513=ORIENTED_EDGE('',*,*,#55760,.F.);
#83514=ORIENTED_EDGE('',*,*,#57628,.F.);
#83515=ORIENTED_EDGE('',*,*,#53362,.T.);
#83516=ORIENTED_EDGE('',*,*,#53366,.F.);
#83517=ORIENTED_EDGE('',*,*,#57627,.T.);
#83518=ORIENTED_EDGE('',*,*,#52305,.F.);
#83519=ORIENTED_EDGE('',*,*,#57629,.F.);
#83520=ORIENTED_EDGE('',*,*,#56452,.F.);
#83521=ORIENTED_EDGE('',*,*,#57628,.T.);
#83522=ORIENTED_EDGE('',*,*,#55759,.F.);
#83523=ORIENTED_EDGE('',*,*,#57630,.F.);
#83524=ORIENTED_EDGE('',*,*,#53363,.F.);
#83525=ORIENTED_EDGE('',*,*,#57629,.T.);
#83526=ORIENTED_EDGE('',*,*,#52304,.F.);
#83527=ORIENTED_EDGE('',*,*,#57631,.F.);
#83528=ORIENTED_EDGE('',*,*,#55739,.F.);
#83529=ORIENTED_EDGE('',*,*,#57630,.T.);
#83530=ORIENTED_EDGE('',*,*,#55758,.F.);
#83531=ORIENTED_EDGE('',*,*,#57632,.F.);
#83532=ORIENTED_EDGE('',*,*,#53381,.F.);
#83533=ORIENTED_EDGE('',*,*,#57631,.T.);
#83534=ORIENTED_EDGE('',*,*,#52303,.F.);
#83535=ORIENTED_EDGE('',*,*,#57633,.F.);
#83536=ORIENTED_EDGE('',*,*,#56454,.F.);
#83537=ORIENTED_EDGE('',*,*,#57632,.T.);
#83538=ORIENTED_EDGE('',*,*,#55757,.F.);
#83539=ORIENTED_EDGE('',*,*,#57634,.F.);
#83540=ORIENTED_EDGE('',*,*,#52721,.F.);
#83541=ORIENTED_EDGE('',*,*,#57633,.T.);
#83542=ORIENTED_EDGE('',*,*,#52302,.F.);
#83543=ORIENTED_EDGE('',*,*,#57635,.F.);
#83544=ORIENTED_EDGE('',*,*,#55745,.F.);
#83545=ORIENTED_EDGE('',*,*,#57634,.T.);
#83546=ORIENTED_EDGE('',*,*,#56453,.F.);
#83547=ORIENTED_EDGE('',*,*,#57636,.F.);
#83548=ORIENTED_EDGE('',*,*,#52722,.F.);
#83549=ORIENTED_EDGE('',*,*,#57635,.T.);
#83550=ORIENTED_EDGE('',*,*,#53412,.F.);
#83551=ORIENTED_EDGE('',*,*,#57637,.F.);
#83552=ORIENTED_EDGE('',*,*,#55746,.F.);
#83553=ORIENTED_EDGE('',*,*,#57636,.T.);
#83554=ORIENTED_EDGE('',*,*,#55741,.F.);
#83555=ORIENTED_EDGE('',*,*,#57638,.F.);
#83556=ORIENTED_EDGE('',*,*,#52723,.F.);
#83557=ORIENTED_EDGE('',*,*,#53407,.F.);
#83558=ORIENTED_EDGE('',*,*,#53403,.T.);
#83559=ORIENTED_EDGE('',*,*,#57639,.F.);
#83560=ORIENTED_EDGE('',*,*,#55747,.F.);
#83561=ORIENTED_EDGE('',*,*,#57637,.T.);
#83562=ORIENTED_EDGE('',*,*,#57638,.T.);
#83563=ORIENTED_EDGE('',*,*,#56455,.F.);
#83564=ORIENTED_EDGE('',*,*,#57640,.F.);
#83565=ORIENTED_EDGE('',*,*,#52724,.F.);
#83566=ORIENTED_EDGE('',*,*,#57639,.T.);
#83567=ORIENTED_EDGE('',*,*,#53402,.F.);
#83568=ORIENTED_EDGE('',*,*,#57641,.F.);
#83569=ORIENTED_EDGE('',*,*,#55748,.F.);
#83570=ORIENTED_EDGE('',*,*,#57640,.T.);
#83571=ORIENTED_EDGE('',*,*,#55743,.F.);
#83572=ORIENTED_EDGE('',*,*,#57642,.F.);
#83573=ORIENTED_EDGE('',*,*,#52725,.F.);
#83574=ORIENTED_EDGE('',*,*,#57641,.T.);
#83575=ORIENTED_EDGE('',*,*,#53414,.F.);
#83576=ORIENTED_EDGE('',*,*,#57643,.F.);
#83577=ORIENTED_EDGE('',*,*,#55749,.F.);
#83578=ORIENTED_EDGE('',*,*,#57642,.T.);
#83579=ORIENTED_EDGE('',*,*,#55742,.F.);
#83580=ORIENTED_EDGE('',*,*,#57644,.F.);
#83581=ORIENTED_EDGE('',*,*,#53410,.F.);
#83582=ORIENTED_EDGE('',*,*,#57643,.T.);
#83583=ORIENTED_EDGE('',*,*,#53398,.F.);
#83584=ORIENTED_EDGE('',*,*,#57645,.F.);
#83585=ORIENTED_EDGE('',*,*,#55750,.F.);
#83586=ORIENTED_EDGE('',*,*,#57644,.T.);
#83587=ORIENTED_EDGE('',*,*,#55753,.F.);
#83588=ORIENTED_EDGE('',*,*,#57646,.F.);
#83589=ORIENTED_EDGE('',*,*,#53389,.F.);
#83590=ORIENTED_EDGE('',*,*,#57645,.T.);
#83591=ORIENTED_EDGE('',*,*,#53416,.F.);
#83592=ORIENTED_EDGE('',*,*,#57647,.F.);
#83593=ORIENTED_EDGE('',*,*,#55751,.F.);
#83594=ORIENTED_EDGE('',*,*,#57646,.T.);
#83595=ORIENTED_EDGE('',*,*,#55752,.F.);
#83596=ORIENTED_EDGE('',*,*,#57647,.T.);
#83597=ORIENTED_EDGE('',*,*,#53394,.F.);
#83598=ORIENTED_EDGE('',*,*,#53390,.T.);
#83599=ORIENTED_EDGE('',*,*,#57648,.F.);
#83600=ORIENTED_EDGE('',*,*,#55792,.F.);
#83601=ORIENTED_EDGE('',*,*,#57649,.F.);
#83602=ORIENTED_EDGE('',*,*,#53346,.F.);
#83603=ORIENTED_EDGE('',*,*,#57649,.T.);
#83604=ORIENTED_EDGE('',*,*,#55791,.F.);
#83605=ORIENTED_EDGE('',*,*,#57650,.F.);
#83606=ORIENTED_EDGE('',*,*,#53355,.F.);
#83607=ORIENTED_EDGE('',*,*,#53345,.T.);
#83608=ORIENTED_EDGE('',*,*,#53349,.F.);
#83609=ORIENTED_EDGE('',*,*,#57651,.F.);
#83610=ORIENTED_EDGE('',*,*,#55793,.F.);
#83611=ORIENTED_EDGE('',*,*,#57648,.T.);
#83612=ORIENTED_EDGE('',*,*,#57650,.T.);
#83613=ORIENTED_EDGE('',*,*,#55790,.F.);
#83614=ORIENTED_EDGE('',*,*,#57652,.F.);
#83615=ORIENTED_EDGE('',*,*,#53340,.F.);
#83616=ORIENTED_EDGE('',*,*,#57651,.T.);
#83617=ORIENTED_EDGE('',*,*,#53353,.F.);
#83618=ORIENTED_EDGE('',*,*,#57653,.F.);
#83619=ORIENTED_EDGE('',*,*,#55782,.F.);
#83620=ORIENTED_EDGE('',*,*,#57652,.T.);
#83621=ORIENTED_EDGE('',*,*,#55789,.F.);
#83622=ORIENTED_EDGE('',*,*,#57654,.F.);
#83623=ORIENTED_EDGE('',*,*,#53357,.F.);
#83624=ORIENTED_EDGE('',*,*,#57653,.T.);
#83625=ORIENTED_EDGE('',*,*,#52312,.F.);
#83626=ORIENTED_EDGE('',*,*,#57655,.F.);
#83627=ORIENTED_EDGE('',*,*,#55783,.F.);
#83628=ORIENTED_EDGE('',*,*,#57654,.T.);
#83629=ORIENTED_EDGE('',*,*,#55788,.F.);
#83630=ORIENTED_EDGE('',*,*,#57656,.F.);
#83631=ORIENTED_EDGE('',*,*,#53332,.T.);
#83632=ORIENTED_EDGE('',*,*,#53336,.F.);
#83633=ORIENTED_EDGE('',*,*,#57655,.T.);
#83634=ORIENTED_EDGE('',*,*,#52311,.F.);
#83635=ORIENTED_EDGE('',*,*,#57657,.F.);
#83636=ORIENTED_EDGE('',*,*,#56456,.F.);
#83637=ORIENTED_EDGE('',*,*,#57656,.T.);
#83638=ORIENTED_EDGE('',*,*,#55787,.F.);
#83639=ORIENTED_EDGE('',*,*,#57658,.F.);
#83640=ORIENTED_EDGE('',*,*,#53333,.F.);
#83641=ORIENTED_EDGE('',*,*,#57657,.T.);
#83642=ORIENTED_EDGE('',*,*,#52310,.F.);
#83643=ORIENTED_EDGE('',*,*,#57659,.F.);
#83644=ORIENTED_EDGE('',*,*,#55767,.F.);
#83645=ORIENTED_EDGE('',*,*,#57658,.T.);
#83646=ORIENTED_EDGE('',*,*,#55786,.F.);
#83647=ORIENTED_EDGE('',*,*,#57660,.F.);
#83648=ORIENTED_EDGE('',*,*,#53351,.F.);
#83649=ORIENTED_EDGE('',*,*,#57659,.T.);
#83650=ORIENTED_EDGE('',*,*,#52309,.F.);
#83651=ORIENTED_EDGE('',*,*,#57661,.F.);
#83652=ORIENTED_EDGE('',*,*,#56458,.F.);
#83653=ORIENTED_EDGE('',*,*,#57660,.T.);
#83654=ORIENTED_EDGE('',*,*,#55785,.F.);
#83655=ORIENTED_EDGE('',*,*,#57662,.F.);
#83656=ORIENTED_EDGE('',*,*,#52715,.F.);
#83657=ORIENTED_EDGE('',*,*,#57661,.T.);
#83658=ORIENTED_EDGE('',*,*,#52308,.F.);
#83659=ORIENTED_EDGE('',*,*,#57663,.F.);
#83660=ORIENTED_EDGE('',*,*,#55773,.F.);
#83661=ORIENTED_EDGE('',*,*,#57662,.T.);
#83662=ORIENTED_EDGE('',*,*,#56457,.F.);
#83663=ORIENTED_EDGE('',*,*,#57664,.F.);
#83664=ORIENTED_EDGE('',*,*,#52716,.F.);
#83665=ORIENTED_EDGE('',*,*,#57663,.T.);
#83666=ORIENTED_EDGE('',*,*,#53382,.F.);
#83667=ORIENTED_EDGE('',*,*,#57665,.F.);
#83668=ORIENTED_EDGE('',*,*,#55774,.F.);
#83669=ORIENTED_EDGE('',*,*,#57664,.T.);
#83670=ORIENTED_EDGE('',*,*,#55769,.F.);
#83671=ORIENTED_EDGE('',*,*,#57666,.F.);
#83672=ORIENTED_EDGE('',*,*,#52717,.F.);
#83673=ORIENTED_EDGE('',*,*,#53377,.F.);
#83674=ORIENTED_EDGE('',*,*,#53373,.T.);
#83675=ORIENTED_EDGE('',*,*,#57667,.F.);
#83676=ORIENTED_EDGE('',*,*,#55775,.F.);
#83677=ORIENTED_EDGE('',*,*,#57665,.T.);
#83678=ORIENTED_EDGE('',*,*,#57666,.T.);
#83679=ORIENTED_EDGE('',*,*,#56459,.F.);
#83680=ORIENTED_EDGE('',*,*,#57668,.F.);
#83681=ORIENTED_EDGE('',*,*,#52718,.F.);
#83682=ORIENTED_EDGE('',*,*,#57667,.T.);
#83683=ORIENTED_EDGE('',*,*,#53372,.F.);
#83684=ORIENTED_EDGE('',*,*,#57669,.F.);
#83685=ORIENTED_EDGE('',*,*,#55776,.F.);
#83686=ORIENTED_EDGE('',*,*,#57668,.T.);
#83687=ORIENTED_EDGE('',*,*,#55771,.F.);
#83688=ORIENTED_EDGE('',*,*,#57670,.F.);
#83689=ORIENTED_EDGE('',*,*,#52719,.F.);
#83690=ORIENTED_EDGE('',*,*,#57669,.T.);
#83691=ORIENTED_EDGE('',*,*,#53384,.F.);
#83692=ORIENTED_EDGE('',*,*,#57671,.F.);
#83693=ORIENTED_EDGE('',*,*,#55777,.F.);
#83694=ORIENTED_EDGE('',*,*,#57670,.T.);
#83695=ORIENTED_EDGE('',*,*,#55770,.F.);
#83696=ORIENTED_EDGE('',*,*,#57672,.F.);
#83697=ORIENTED_EDGE('',*,*,#53380,.F.);
#83698=ORIENTED_EDGE('',*,*,#57671,.T.);
#83699=ORIENTED_EDGE('',*,*,#53368,.F.);
#83700=ORIENTED_EDGE('',*,*,#57673,.F.);
#83701=ORIENTED_EDGE('',*,*,#55778,.F.);
#83702=ORIENTED_EDGE('',*,*,#57672,.T.);
#83703=ORIENTED_EDGE('',*,*,#55781,.F.);
#83704=ORIENTED_EDGE('',*,*,#57674,.F.);
#83705=ORIENTED_EDGE('',*,*,#53359,.F.);
#83706=ORIENTED_EDGE('',*,*,#57673,.T.);
#83707=ORIENTED_EDGE('',*,*,#53386,.F.);
#83708=ORIENTED_EDGE('',*,*,#57675,.F.);
#83709=ORIENTED_EDGE('',*,*,#55779,.F.);
#83710=ORIENTED_EDGE('',*,*,#57674,.T.);
#83711=ORIENTED_EDGE('',*,*,#55780,.F.);
#83712=ORIENTED_EDGE('',*,*,#57675,.T.);
#83713=ORIENTED_EDGE('',*,*,#53364,.F.);
#83714=ORIENTED_EDGE('',*,*,#53360,.T.);
#83715=ORIENTED_EDGE('',*,*,#57676,.F.);
#83716=ORIENTED_EDGE('',*,*,#55820,.F.);
#83717=ORIENTED_EDGE('',*,*,#57677,.F.);
#83718=ORIENTED_EDGE('',*,*,#53316,.F.);
#83719=ORIENTED_EDGE('',*,*,#57677,.T.);
#83720=ORIENTED_EDGE('',*,*,#55819,.F.);
#83721=ORIENTED_EDGE('',*,*,#57678,.F.);
#83722=ORIENTED_EDGE('',*,*,#53325,.F.);
#83723=ORIENTED_EDGE('',*,*,#53315,.T.);
#83724=ORIENTED_EDGE('',*,*,#53319,.F.);
#83725=ORIENTED_EDGE('',*,*,#57679,.F.);
#83726=ORIENTED_EDGE('',*,*,#55821,.F.);
#83727=ORIENTED_EDGE('',*,*,#57676,.T.);
#83728=ORIENTED_EDGE('',*,*,#57678,.T.);
#83729=ORIENTED_EDGE('',*,*,#55818,.F.);
#83730=ORIENTED_EDGE('',*,*,#57680,.F.);
#83731=ORIENTED_EDGE('',*,*,#53310,.F.);
#83732=ORIENTED_EDGE('',*,*,#57679,.T.);
#83733=ORIENTED_EDGE('',*,*,#53323,.F.);
#83734=ORIENTED_EDGE('',*,*,#57681,.F.);
#83735=ORIENTED_EDGE('',*,*,#55810,.F.);
#83736=ORIENTED_EDGE('',*,*,#57680,.T.);
#83737=ORIENTED_EDGE('',*,*,#55817,.F.);
#83738=ORIENTED_EDGE('',*,*,#57682,.F.);
#83739=ORIENTED_EDGE('',*,*,#53327,.F.);
#83740=ORIENTED_EDGE('',*,*,#57681,.T.);
#83741=ORIENTED_EDGE('',*,*,#52318,.F.);
#83742=ORIENTED_EDGE('',*,*,#57683,.F.);
#83743=ORIENTED_EDGE('',*,*,#55811,.F.);
#83744=ORIENTED_EDGE('',*,*,#57682,.T.);
#83745=ORIENTED_EDGE('',*,*,#55816,.F.);
#83746=ORIENTED_EDGE('',*,*,#57684,.F.);
#83747=ORIENTED_EDGE('',*,*,#53302,.T.);
#83748=ORIENTED_EDGE('',*,*,#53306,.F.);
#83749=ORIENTED_EDGE('',*,*,#57683,.T.);
#83750=ORIENTED_EDGE('',*,*,#52317,.F.);
#83751=ORIENTED_EDGE('',*,*,#57685,.F.);
#83752=ORIENTED_EDGE('',*,*,#56460,.F.);
#83753=ORIENTED_EDGE('',*,*,#57684,.T.);
#83754=ORIENTED_EDGE('',*,*,#55815,.F.);
#83755=ORIENTED_EDGE('',*,*,#57686,.F.);
#83756=ORIENTED_EDGE('',*,*,#53303,.F.);
#83757=ORIENTED_EDGE('',*,*,#57685,.T.);
#83758=ORIENTED_EDGE('',*,*,#52316,.F.);
#83759=ORIENTED_EDGE('',*,*,#57687,.F.);
#83760=ORIENTED_EDGE('',*,*,#55795,.F.);
#83761=ORIENTED_EDGE('',*,*,#57686,.T.);
#83762=ORIENTED_EDGE('',*,*,#55814,.F.);
#83763=ORIENTED_EDGE('',*,*,#57688,.F.);
#83764=ORIENTED_EDGE('',*,*,#53321,.F.);
#83765=ORIENTED_EDGE('',*,*,#57687,.T.);
#83766=ORIENTED_EDGE('',*,*,#52315,.F.);
#83767=ORIENTED_EDGE('',*,*,#57689,.F.);
#83768=ORIENTED_EDGE('',*,*,#56462,.F.);
#83769=ORIENTED_EDGE('',*,*,#57688,.T.);
#83770=ORIENTED_EDGE('',*,*,#55813,.F.);
#83771=ORIENTED_EDGE('',*,*,#57690,.F.);
#83772=ORIENTED_EDGE('',*,*,#52709,.F.);
#83773=ORIENTED_EDGE('',*,*,#57689,.T.);
#83774=ORIENTED_EDGE('',*,*,#52314,.F.);
#83775=ORIENTED_EDGE('',*,*,#57691,.F.);
#83776=ORIENTED_EDGE('',*,*,#55801,.F.);
#83777=ORIENTED_EDGE('',*,*,#57690,.T.);
#83778=ORIENTED_EDGE('',*,*,#56461,.F.);
#83779=ORIENTED_EDGE('',*,*,#57692,.F.);
#83780=ORIENTED_EDGE('',*,*,#52710,.F.);
#83781=ORIENTED_EDGE('',*,*,#57691,.T.);
#83782=ORIENTED_EDGE('',*,*,#53352,.F.);
#83783=ORIENTED_EDGE('',*,*,#57693,.F.);
#83784=ORIENTED_EDGE('',*,*,#55802,.F.);
#83785=ORIENTED_EDGE('',*,*,#57692,.T.);
#83786=ORIENTED_EDGE('',*,*,#55797,.F.);
#83787=ORIENTED_EDGE('',*,*,#57694,.F.);
#83788=ORIENTED_EDGE('',*,*,#52711,.F.);
#83789=ORIENTED_EDGE('',*,*,#53347,.F.);
#83790=ORIENTED_EDGE('',*,*,#53343,.T.);
#83791=ORIENTED_EDGE('',*,*,#57695,.F.);
#83792=ORIENTED_EDGE('',*,*,#55803,.F.);
#83793=ORIENTED_EDGE('',*,*,#57693,.T.);
#83794=ORIENTED_EDGE('',*,*,#57694,.T.);
#83795=ORIENTED_EDGE('',*,*,#56463,.F.);
#83796=ORIENTED_EDGE('',*,*,#57696,.F.);
#83797=ORIENTED_EDGE('',*,*,#52712,.F.);
#83798=ORIENTED_EDGE('',*,*,#57695,.T.);
#83799=ORIENTED_EDGE('',*,*,#53342,.F.);
#83800=ORIENTED_EDGE('',*,*,#57697,.F.);
#83801=ORIENTED_EDGE('',*,*,#55804,.F.);
#83802=ORIENTED_EDGE('',*,*,#57696,.T.);
#83803=ORIENTED_EDGE('',*,*,#55799,.F.);
#83804=ORIENTED_EDGE('',*,*,#57698,.F.);
#83805=ORIENTED_EDGE('',*,*,#52713,.F.);
#83806=ORIENTED_EDGE('',*,*,#57697,.T.);
#83807=ORIENTED_EDGE('',*,*,#53354,.F.);
#83808=ORIENTED_EDGE('',*,*,#57699,.F.);
#83809=ORIENTED_EDGE('',*,*,#55805,.F.);
#83810=ORIENTED_EDGE('',*,*,#57698,.T.);
#83811=ORIENTED_EDGE('',*,*,#55798,.F.);
#83812=ORIENTED_EDGE('',*,*,#57700,.F.);
#83813=ORIENTED_EDGE('',*,*,#53350,.F.);
#83814=ORIENTED_EDGE('',*,*,#57699,.T.);
#83815=ORIENTED_EDGE('',*,*,#53338,.F.);
#83816=ORIENTED_EDGE('',*,*,#57701,.F.);
#83817=ORIENTED_EDGE('',*,*,#55806,.F.);
#83818=ORIENTED_EDGE('',*,*,#57700,.T.);
#83819=ORIENTED_EDGE('',*,*,#55809,.F.);
#83820=ORIENTED_EDGE('',*,*,#57702,.F.);
#83821=ORIENTED_EDGE('',*,*,#53329,.F.);
#83822=ORIENTED_EDGE('',*,*,#57701,.T.);
#83823=ORIENTED_EDGE('',*,*,#53356,.F.);
#83824=ORIENTED_EDGE('',*,*,#57703,.F.);
#83825=ORIENTED_EDGE('',*,*,#55807,.F.);
#83826=ORIENTED_EDGE('',*,*,#57702,.T.);
#83827=ORIENTED_EDGE('',*,*,#55808,.F.);
#83828=ORIENTED_EDGE('',*,*,#57703,.T.);
#83829=ORIENTED_EDGE('',*,*,#53334,.F.);
#83830=ORIENTED_EDGE('',*,*,#53330,.T.);
#83831=ORIENTED_EDGE('',*,*,#57704,.F.);
#83832=ORIENTED_EDGE('',*,*,#55848,.F.);
#83833=ORIENTED_EDGE('',*,*,#57705,.F.);
#83834=ORIENTED_EDGE('',*,*,#53286,.F.);
#83835=ORIENTED_EDGE('',*,*,#57705,.T.);
#83836=ORIENTED_EDGE('',*,*,#55847,.F.);
#83837=ORIENTED_EDGE('',*,*,#57706,.F.);
#83838=ORIENTED_EDGE('',*,*,#53295,.F.);
#83839=ORIENTED_EDGE('',*,*,#53285,.T.);
#83840=ORIENTED_EDGE('',*,*,#53289,.F.);
#83841=ORIENTED_EDGE('',*,*,#57707,.F.);
#83842=ORIENTED_EDGE('',*,*,#55849,.F.);
#83843=ORIENTED_EDGE('',*,*,#57704,.T.);
#83844=ORIENTED_EDGE('',*,*,#57706,.T.);
#83845=ORIENTED_EDGE('',*,*,#55846,.F.);
#83846=ORIENTED_EDGE('',*,*,#57708,.F.);
#83847=ORIENTED_EDGE('',*,*,#53280,.F.);
#83848=ORIENTED_EDGE('',*,*,#57707,.T.);
#83849=ORIENTED_EDGE('',*,*,#53293,.F.);
#83850=ORIENTED_EDGE('',*,*,#57709,.F.);
#83851=ORIENTED_EDGE('',*,*,#55838,.F.);
#83852=ORIENTED_EDGE('',*,*,#57708,.T.);
#83853=ORIENTED_EDGE('',*,*,#55845,.F.);
#83854=ORIENTED_EDGE('',*,*,#57710,.F.);
#83855=ORIENTED_EDGE('',*,*,#53297,.F.);
#83856=ORIENTED_EDGE('',*,*,#57709,.T.);
#83857=ORIENTED_EDGE('',*,*,#52324,.F.);
#83858=ORIENTED_EDGE('',*,*,#57711,.F.);
#83859=ORIENTED_EDGE('',*,*,#55839,.F.);
#83860=ORIENTED_EDGE('',*,*,#57710,.T.);
#83861=ORIENTED_EDGE('',*,*,#55844,.F.);
#83862=ORIENTED_EDGE('',*,*,#57712,.F.);
#83863=ORIENTED_EDGE('',*,*,#53272,.T.);
#83864=ORIENTED_EDGE('',*,*,#53276,.F.);
#83865=ORIENTED_EDGE('',*,*,#57711,.T.);
#83866=ORIENTED_EDGE('',*,*,#52323,.F.);
#83867=ORIENTED_EDGE('',*,*,#57713,.F.);
#83868=ORIENTED_EDGE('',*,*,#56464,.F.);
#83869=ORIENTED_EDGE('',*,*,#57712,.T.);
#83870=ORIENTED_EDGE('',*,*,#55843,.F.);
#83871=ORIENTED_EDGE('',*,*,#57714,.F.);
#83872=ORIENTED_EDGE('',*,*,#53273,.F.);
#83873=ORIENTED_EDGE('',*,*,#57713,.T.);
#83874=ORIENTED_EDGE('',*,*,#52322,.F.);
#83875=ORIENTED_EDGE('',*,*,#57715,.F.);
#83876=ORIENTED_EDGE('',*,*,#55823,.F.);
#83877=ORIENTED_EDGE('',*,*,#57714,.T.);
#83878=ORIENTED_EDGE('',*,*,#55842,.F.);
#83879=ORIENTED_EDGE('',*,*,#57716,.F.);
#83880=ORIENTED_EDGE('',*,*,#53291,.F.);
#83881=ORIENTED_EDGE('',*,*,#57715,.T.);
#83882=ORIENTED_EDGE('',*,*,#52321,.F.);
#83883=ORIENTED_EDGE('',*,*,#57717,.F.);
#83884=ORIENTED_EDGE('',*,*,#56466,.F.);
#83885=ORIENTED_EDGE('',*,*,#57716,.T.);
#83886=ORIENTED_EDGE('',*,*,#55841,.F.);
#83887=ORIENTED_EDGE('',*,*,#57718,.F.);
#83888=ORIENTED_EDGE('',*,*,#52703,.F.);
#83889=ORIENTED_EDGE('',*,*,#57717,.T.);
#83890=ORIENTED_EDGE('',*,*,#52320,.F.);
#83891=ORIENTED_EDGE('',*,*,#57719,.F.);
#83892=ORIENTED_EDGE('',*,*,#55829,.F.);
#83893=ORIENTED_EDGE('',*,*,#57718,.T.);
#83894=ORIENTED_EDGE('',*,*,#56465,.F.);
#83895=ORIENTED_EDGE('',*,*,#57720,.F.);
#83896=ORIENTED_EDGE('',*,*,#52704,.F.);
#83897=ORIENTED_EDGE('',*,*,#57719,.T.);
#83898=ORIENTED_EDGE('',*,*,#53322,.F.);
#83899=ORIENTED_EDGE('',*,*,#57721,.F.);
#83900=ORIENTED_EDGE('',*,*,#55830,.F.);
#83901=ORIENTED_EDGE('',*,*,#57720,.T.);
#83902=ORIENTED_EDGE('',*,*,#55825,.F.);
#83903=ORIENTED_EDGE('',*,*,#57722,.F.);
#83904=ORIENTED_EDGE('',*,*,#52705,.F.);
#83905=ORIENTED_EDGE('',*,*,#53317,.F.);
#83906=ORIENTED_EDGE('',*,*,#53313,.T.);
#83907=ORIENTED_EDGE('',*,*,#57723,.F.);
#83908=ORIENTED_EDGE('',*,*,#55831,.F.);
#83909=ORIENTED_EDGE('',*,*,#57721,.T.);
#83910=ORIENTED_EDGE('',*,*,#57722,.T.);
#83911=ORIENTED_EDGE('',*,*,#56467,.F.);
#83912=ORIENTED_EDGE('',*,*,#57724,.F.);
#83913=ORIENTED_EDGE('',*,*,#52706,.F.);
#83914=ORIENTED_EDGE('',*,*,#57723,.T.);
#83915=ORIENTED_EDGE('',*,*,#53312,.F.);
#83916=ORIENTED_EDGE('',*,*,#57725,.F.);
#83917=ORIENTED_EDGE('',*,*,#55832,.F.);
#83918=ORIENTED_EDGE('',*,*,#57724,.T.);
#83919=ORIENTED_EDGE('',*,*,#55827,.F.);
#83920=ORIENTED_EDGE('',*,*,#57726,.F.);
#83921=ORIENTED_EDGE('',*,*,#52707,.F.);
#83922=ORIENTED_EDGE('',*,*,#57725,.T.);
#83923=ORIENTED_EDGE('',*,*,#53324,.F.);
#83924=ORIENTED_EDGE('',*,*,#57727,.F.);
#83925=ORIENTED_EDGE('',*,*,#55833,.F.);
#83926=ORIENTED_EDGE('',*,*,#57726,.T.);
#83927=ORIENTED_EDGE('',*,*,#55826,.F.);
#83928=ORIENTED_EDGE('',*,*,#57728,.F.);
#83929=ORIENTED_EDGE('',*,*,#53320,.F.);
#83930=ORIENTED_EDGE('',*,*,#57727,.T.);
#83931=ORIENTED_EDGE('',*,*,#53308,.F.);
#83932=ORIENTED_EDGE('',*,*,#57729,.F.);
#83933=ORIENTED_EDGE('',*,*,#55834,.F.);
#83934=ORIENTED_EDGE('',*,*,#57728,.T.);
#83935=ORIENTED_EDGE('',*,*,#55837,.F.);
#83936=ORIENTED_EDGE('',*,*,#57730,.F.);
#83937=ORIENTED_EDGE('',*,*,#53299,.F.);
#83938=ORIENTED_EDGE('',*,*,#57729,.T.);
#83939=ORIENTED_EDGE('',*,*,#53326,.F.);
#83940=ORIENTED_EDGE('',*,*,#57731,.F.);
#83941=ORIENTED_EDGE('',*,*,#55835,.F.);
#83942=ORIENTED_EDGE('',*,*,#57730,.T.);
#83943=ORIENTED_EDGE('',*,*,#55836,.F.);
#83944=ORIENTED_EDGE('',*,*,#57731,.T.);
#83945=ORIENTED_EDGE('',*,*,#53304,.F.);
#83946=ORIENTED_EDGE('',*,*,#53300,.T.);
#83947=ORIENTED_EDGE('',*,*,#57732,.F.);
#83948=ORIENTED_EDGE('',*,*,#55876,.F.);
#83949=ORIENTED_EDGE('',*,*,#57733,.F.);
#83950=ORIENTED_EDGE('',*,*,#53256,.F.);
#83951=ORIENTED_EDGE('',*,*,#57733,.T.);
#83952=ORIENTED_EDGE('',*,*,#55875,.F.);
#83953=ORIENTED_EDGE('',*,*,#57734,.F.);
#83954=ORIENTED_EDGE('',*,*,#53265,.F.);
#83955=ORIENTED_EDGE('',*,*,#53255,.T.);
#83956=ORIENTED_EDGE('',*,*,#53259,.F.);
#83957=ORIENTED_EDGE('',*,*,#57735,.F.);
#83958=ORIENTED_EDGE('',*,*,#55877,.F.);
#83959=ORIENTED_EDGE('',*,*,#57732,.T.);
#83960=ORIENTED_EDGE('',*,*,#57734,.T.);
#83961=ORIENTED_EDGE('',*,*,#55874,.F.);
#83962=ORIENTED_EDGE('',*,*,#57736,.F.);
#83963=ORIENTED_EDGE('',*,*,#53250,.F.);
#83964=ORIENTED_EDGE('',*,*,#57735,.T.);
#83965=ORIENTED_EDGE('',*,*,#53263,.F.);
#83966=ORIENTED_EDGE('',*,*,#57737,.F.);
#83967=ORIENTED_EDGE('',*,*,#55866,.F.);
#83968=ORIENTED_EDGE('',*,*,#57736,.T.);
#83969=ORIENTED_EDGE('',*,*,#55873,.F.);
#83970=ORIENTED_EDGE('',*,*,#57738,.F.);
#83971=ORIENTED_EDGE('',*,*,#53267,.F.);
#83972=ORIENTED_EDGE('',*,*,#57737,.T.);
#83973=ORIENTED_EDGE('',*,*,#52330,.F.);
#83974=ORIENTED_EDGE('',*,*,#57739,.F.);
#83975=ORIENTED_EDGE('',*,*,#55867,.F.);
#83976=ORIENTED_EDGE('',*,*,#57738,.T.);
#83977=ORIENTED_EDGE('',*,*,#55872,.F.);
#83978=ORIENTED_EDGE('',*,*,#57740,.F.);
#83979=ORIENTED_EDGE('',*,*,#53242,.T.);
#83980=ORIENTED_EDGE('',*,*,#53246,.F.);
#83981=ORIENTED_EDGE('',*,*,#57739,.T.);
#83982=ORIENTED_EDGE('',*,*,#52329,.F.);
#83983=ORIENTED_EDGE('',*,*,#57741,.F.);
#83984=ORIENTED_EDGE('',*,*,#56468,.F.);
#83985=ORIENTED_EDGE('',*,*,#57740,.T.);
#83986=ORIENTED_EDGE('',*,*,#55871,.F.);
#83987=ORIENTED_EDGE('',*,*,#57742,.F.);
#83988=ORIENTED_EDGE('',*,*,#53243,.F.);
#83989=ORIENTED_EDGE('',*,*,#57741,.T.);
#83990=ORIENTED_EDGE('',*,*,#52328,.F.);
#83991=ORIENTED_EDGE('',*,*,#57743,.F.);
#83992=ORIENTED_EDGE('',*,*,#55851,.F.);
#83993=ORIENTED_EDGE('',*,*,#57742,.T.);
#83994=ORIENTED_EDGE('',*,*,#55870,.F.);
#83995=ORIENTED_EDGE('',*,*,#57744,.F.);
#83996=ORIENTED_EDGE('',*,*,#53261,.F.);
#83997=ORIENTED_EDGE('',*,*,#57743,.T.);
#83998=ORIENTED_EDGE('',*,*,#52327,.F.);
#83999=ORIENTED_EDGE('',*,*,#57745,.F.);
#84000=ORIENTED_EDGE('',*,*,#56470,.F.);
#84001=ORIENTED_EDGE('',*,*,#57744,.T.);
#84002=ORIENTED_EDGE('',*,*,#55869,.F.);
#84003=ORIENTED_EDGE('',*,*,#57746,.F.);
#84004=ORIENTED_EDGE('',*,*,#52697,.F.);
#84005=ORIENTED_EDGE('',*,*,#57745,.T.);
#84006=ORIENTED_EDGE('',*,*,#52326,.F.);
#84007=ORIENTED_EDGE('',*,*,#57747,.F.);
#84008=ORIENTED_EDGE('',*,*,#55857,.F.);
#84009=ORIENTED_EDGE('',*,*,#57746,.T.);
#84010=ORIENTED_EDGE('',*,*,#56469,.F.);
#84011=ORIENTED_EDGE('',*,*,#57748,.F.);
#84012=ORIENTED_EDGE('',*,*,#52698,.F.);
#84013=ORIENTED_EDGE('',*,*,#57747,.T.);
#84014=ORIENTED_EDGE('',*,*,#53292,.F.);
#84015=ORIENTED_EDGE('',*,*,#57749,.F.);
#84016=ORIENTED_EDGE('',*,*,#55858,.F.);
#84017=ORIENTED_EDGE('',*,*,#57748,.T.);
#84018=ORIENTED_EDGE('',*,*,#55853,.F.);
#84019=ORIENTED_EDGE('',*,*,#57750,.F.);
#84020=ORIENTED_EDGE('',*,*,#52699,.F.);
#84021=ORIENTED_EDGE('',*,*,#53287,.F.);
#84022=ORIENTED_EDGE('',*,*,#53283,.T.);
#84023=ORIENTED_EDGE('',*,*,#57751,.F.);
#84024=ORIENTED_EDGE('',*,*,#55859,.F.);
#84025=ORIENTED_EDGE('',*,*,#57749,.T.);
#84026=ORIENTED_EDGE('',*,*,#57750,.T.);
#84027=ORIENTED_EDGE('',*,*,#56471,.F.);
#84028=ORIENTED_EDGE('',*,*,#57752,.F.);
#84029=ORIENTED_EDGE('',*,*,#52700,.F.);
#84030=ORIENTED_EDGE('',*,*,#57751,.T.);
#84031=ORIENTED_EDGE('',*,*,#53282,.F.);
#84032=ORIENTED_EDGE('',*,*,#57753,.F.);
#84033=ORIENTED_EDGE('',*,*,#55860,.F.);
#84034=ORIENTED_EDGE('',*,*,#57752,.T.);
#84035=ORIENTED_EDGE('',*,*,#55855,.F.);
#84036=ORIENTED_EDGE('',*,*,#57754,.F.);
#84037=ORIENTED_EDGE('',*,*,#52701,.F.);
#84038=ORIENTED_EDGE('',*,*,#57753,.T.);
#84039=ORIENTED_EDGE('',*,*,#53294,.F.);
#84040=ORIENTED_EDGE('',*,*,#57755,.F.);
#84041=ORIENTED_EDGE('',*,*,#55861,.F.);
#84042=ORIENTED_EDGE('',*,*,#57754,.T.);
#84043=ORIENTED_EDGE('',*,*,#55854,.F.);
#84044=ORIENTED_EDGE('',*,*,#57756,.F.);
#84045=ORIENTED_EDGE('',*,*,#53290,.F.);
#84046=ORIENTED_EDGE('',*,*,#57755,.T.);
#84047=ORIENTED_EDGE('',*,*,#53278,.F.);
#84048=ORIENTED_EDGE('',*,*,#57757,.F.);
#84049=ORIENTED_EDGE('',*,*,#55862,.F.);
#84050=ORIENTED_EDGE('',*,*,#57756,.T.);
#84051=ORIENTED_EDGE('',*,*,#55865,.F.);
#84052=ORIENTED_EDGE('',*,*,#57758,.F.);
#84053=ORIENTED_EDGE('',*,*,#53269,.F.);
#84054=ORIENTED_EDGE('',*,*,#57757,.T.);
#84055=ORIENTED_EDGE('',*,*,#53296,.F.);
#84056=ORIENTED_EDGE('',*,*,#57759,.F.);
#84057=ORIENTED_EDGE('',*,*,#55863,.F.);
#84058=ORIENTED_EDGE('',*,*,#57758,.T.);
#84059=ORIENTED_EDGE('',*,*,#55864,.F.);
#84060=ORIENTED_EDGE('',*,*,#57759,.T.);
#84061=ORIENTED_EDGE('',*,*,#53274,.F.);
#84062=ORIENTED_EDGE('',*,*,#53270,.T.);
#84063=ORIENTED_EDGE('',*,*,#57760,.F.);
#84064=ORIENTED_EDGE('',*,*,#55902,.F.);
#84065=ORIENTED_EDGE('',*,*,#57761,.F.);
#84066=ORIENTED_EDGE('',*,*,#53226,.F.);
#84067=ORIENTED_EDGE('',*,*,#57761,.T.);
#84068=ORIENTED_EDGE('',*,*,#55901,.F.);
#84069=ORIENTED_EDGE('',*,*,#57762,.F.);
#84070=ORIENTED_EDGE('',*,*,#53235,.F.);
#84071=ORIENTED_EDGE('',*,*,#53225,.T.);
#84072=ORIENTED_EDGE('',*,*,#53229,.F.);
#84073=ORIENTED_EDGE('',*,*,#57763,.F.);
#84074=ORIENTED_EDGE('',*,*,#55903,.F.);
#84075=ORIENTED_EDGE('',*,*,#57760,.T.);
#84076=ORIENTED_EDGE('',*,*,#57762,.T.);
#84077=ORIENTED_EDGE('',*,*,#55900,.F.);
#84078=ORIENTED_EDGE('',*,*,#57764,.F.);
#84079=ORIENTED_EDGE('',*,*,#53220,.F.);
#84080=ORIENTED_EDGE('',*,*,#57763,.T.);
#84081=ORIENTED_EDGE('',*,*,#53233,.F.);
#84082=ORIENTED_EDGE('',*,*,#57765,.F.);
#84083=ORIENTED_EDGE('',*,*,#55892,.F.);
#84084=ORIENTED_EDGE('',*,*,#57764,.T.);
#84085=ORIENTED_EDGE('',*,*,#55899,.F.);
#84086=ORIENTED_EDGE('',*,*,#57766,.F.);
#84087=ORIENTED_EDGE('',*,*,#53237,.F.);
#84088=ORIENTED_EDGE('',*,*,#57765,.T.);
#84089=ORIENTED_EDGE('',*,*,#52335,.F.);
#84090=ORIENTED_EDGE('',*,*,#57767,.F.);
#84091=ORIENTED_EDGE('',*,*,#55893,.F.);
#84092=ORIENTED_EDGE('',*,*,#57766,.T.);
#84093=ORIENTED_EDGE('',*,*,#55898,.F.);
#84094=ORIENTED_EDGE('',*,*,#57768,.F.);
#84095=ORIENTED_EDGE('',*,*,#53212,.T.);
#84096=ORIENTED_EDGE('',*,*,#53216,.F.);
#84097=ORIENTED_EDGE('',*,*,#57767,.T.);
#84098=ORIENTED_EDGE('',*,*,#52334,.F.);
#84099=ORIENTED_EDGE('',*,*,#52036,.F.);
#84100=ORIENTED_EDGE('',*,*,#56472,.F.);
#84101=ORIENTED_EDGE('',*,*,#57768,.T.);
#84102=ORIENTED_EDGE('',*,*,#55897,.F.);
#84103=ORIENTED_EDGE('',*,*,#57769,.F.);
#84104=ORIENTED_EDGE('',*,*,#53213,.F.);
#84105=ORIENTED_EDGE('',*,*,#57769,.T.);
#84106=ORIENTED_EDGE('',*,*,#55896,.F.);
#84107=ORIENTED_EDGE('',*,*,#57770,.F.);
#84108=ORIENTED_EDGE('',*,*,#53231,.F.);
#84109=ORIENTED_EDGE('',*,*,#52034,.T.);
#84110=ORIENTED_EDGE('',*,*,#52333,.F.);
#84111=ORIENTED_EDGE('',*,*,#57771,.F.);
#84112=ORIENTED_EDGE('',*,*,#56474,.F.);
#84113=ORIENTED_EDGE('',*,*,#57770,.T.);
#84114=ORIENTED_EDGE('',*,*,#55895,.F.);
#84115=ORIENTED_EDGE('',*,*,#57772,.F.);
#84116=ORIENTED_EDGE('',*,*,#52692,.F.);
#84117=ORIENTED_EDGE('',*,*,#57771,.T.);
#84118=ORIENTED_EDGE('',*,*,#52332,.F.);
#84119=ORIENTED_EDGE('',*,*,#57773,.F.);
#84120=ORIENTED_EDGE('',*,*,#55883,.F.);
#84121=ORIENTED_EDGE('',*,*,#57772,.T.);
#84122=ORIENTED_EDGE('',*,*,#56473,.F.);
#84123=ORIENTED_EDGE('',*,*,#52032,.F.);
#84124=ORIENTED_EDGE('',*,*,#52693,.F.);
#84125=ORIENTED_EDGE('',*,*,#57773,.T.);
#84126=ORIENTED_EDGE('',*,*,#53262,.F.);
#84127=ORIENTED_EDGE('',*,*,#57774,.F.);
#84128=ORIENTED_EDGE('',*,*,#55884,.F.);
#84129=ORIENTED_EDGE('',*,*,#53257,.F.);
#84130=ORIENTED_EDGE('',*,*,#53253,.T.);
#84131=ORIENTED_EDGE('',*,*,#57775,.F.);
#84132=ORIENTED_EDGE('',*,*,#55885,.F.);
#84133=ORIENTED_EDGE('',*,*,#57774,.T.);
#84134=ORIENTED_EDGE('',*,*,#52030,.T.);
#84135=ORIENTED_EDGE('',*,*,#56475,.F.);
#84136=ORIENTED_EDGE('',*,*,#57776,.F.);
#84137=ORIENTED_EDGE('',*,*,#52694,.F.);
#84138=ORIENTED_EDGE('',*,*,#57775,.T.);
#84139=ORIENTED_EDGE('',*,*,#53252,.F.);
#84140=ORIENTED_EDGE('',*,*,#57777,.F.);
#84141=ORIENTED_EDGE('',*,*,#55886,.F.);
#84142=ORIENTED_EDGE('',*,*,#57776,.T.);
#84143=ORIENTED_EDGE('',*,*,#55881,.F.);
#84144=ORIENTED_EDGE('',*,*,#57778,.F.);
#84145=ORIENTED_EDGE('',*,*,#52695,.F.);
#84146=ORIENTED_EDGE('',*,*,#57777,.T.);
#84147=ORIENTED_EDGE('',*,*,#53264,.F.);
#84148=ORIENTED_EDGE('',*,*,#57779,.F.);
#84149=ORIENTED_EDGE('',*,*,#55887,.F.);
#84150=ORIENTED_EDGE('',*,*,#57778,.T.);
#84151=ORIENTED_EDGE('',*,*,#55880,.F.);
#84152=ORIENTED_EDGE('',*,*,#57780,.F.);
#84153=ORIENTED_EDGE('',*,*,#53260,.F.);
#84154=ORIENTED_EDGE('',*,*,#57779,.T.);
#84155=ORIENTED_EDGE('',*,*,#53248,.F.);
#84156=ORIENTED_EDGE('',*,*,#57781,.F.);
#84157=ORIENTED_EDGE('',*,*,#55888,.F.);
#84158=ORIENTED_EDGE('',*,*,#57780,.T.);
#84159=ORIENTED_EDGE('',*,*,#55891,.F.);
#84160=ORIENTED_EDGE('',*,*,#57782,.F.);
#84161=ORIENTED_EDGE('',*,*,#53239,.F.);
#84162=ORIENTED_EDGE('',*,*,#57781,.T.);
#84163=ORIENTED_EDGE('',*,*,#53266,.F.);
#84164=ORIENTED_EDGE('',*,*,#57783,.F.);
#84165=ORIENTED_EDGE('',*,*,#55889,.F.);
#84166=ORIENTED_EDGE('',*,*,#57782,.T.);
#84167=ORIENTED_EDGE('',*,*,#55890,.F.);
#84168=ORIENTED_EDGE('',*,*,#57783,.T.);
#84169=ORIENTED_EDGE('',*,*,#53244,.F.);
#84170=ORIENTED_EDGE('',*,*,#53240,.T.);
#84171=ORIENTED_EDGE('',*,*,#57784,.F.);
#84172=ORIENTED_EDGE('',*,*,#55930,.F.);
#84173=ORIENTED_EDGE('',*,*,#57785,.F.);
#84174=ORIENTED_EDGE('',*,*,#53196,.F.);
#84175=ORIENTED_EDGE('',*,*,#57785,.T.);
#84176=ORIENTED_EDGE('',*,*,#55929,.F.);
#84177=ORIENTED_EDGE('',*,*,#57786,.F.);
#84178=ORIENTED_EDGE('',*,*,#53205,.F.);
#84179=ORIENTED_EDGE('',*,*,#53195,.T.);
#84180=ORIENTED_EDGE('',*,*,#53199,.F.);
#84181=ORIENTED_EDGE('',*,*,#57787,.F.);
#84182=ORIENTED_EDGE('',*,*,#55931,.F.);
#84183=ORIENTED_EDGE('',*,*,#57784,.T.);
#84184=ORIENTED_EDGE('',*,*,#57786,.T.);
#84185=ORIENTED_EDGE('',*,*,#55928,.F.);
#84186=ORIENTED_EDGE('',*,*,#57788,.F.);
#84187=ORIENTED_EDGE('',*,*,#53190,.F.);
#84188=ORIENTED_EDGE('',*,*,#57787,.T.);
#84189=ORIENTED_EDGE('',*,*,#53203,.F.);
#84190=ORIENTED_EDGE('',*,*,#57789,.F.);
#84191=ORIENTED_EDGE('',*,*,#55920,.F.);
#84192=ORIENTED_EDGE('',*,*,#57788,.T.);
#84193=ORIENTED_EDGE('',*,*,#55927,.F.);
#84194=ORIENTED_EDGE('',*,*,#57790,.F.);
#84195=ORIENTED_EDGE('',*,*,#53207,.F.);
#84196=ORIENTED_EDGE('',*,*,#57789,.T.);
#84197=ORIENTED_EDGE('',*,*,#52341,.F.);
#84198=ORIENTED_EDGE('',*,*,#57791,.F.);
#84199=ORIENTED_EDGE('',*,*,#55921,.F.);
#84200=ORIENTED_EDGE('',*,*,#57790,.T.);
#84201=ORIENTED_EDGE('',*,*,#55926,.F.);
#84202=ORIENTED_EDGE('',*,*,#57792,.F.);
#84203=ORIENTED_EDGE('',*,*,#53182,.T.);
#84204=ORIENTED_EDGE('',*,*,#53186,.F.);
#84205=ORIENTED_EDGE('',*,*,#57791,.T.);
#84206=ORIENTED_EDGE('',*,*,#52340,.F.);
#84207=ORIENTED_EDGE('',*,*,#57793,.F.);
#84208=ORIENTED_EDGE('',*,*,#56476,.F.);
#84209=ORIENTED_EDGE('',*,*,#57792,.T.);
#84210=ORIENTED_EDGE('',*,*,#55925,.F.);
#84211=ORIENTED_EDGE('',*,*,#57794,.F.);
#84212=ORIENTED_EDGE('',*,*,#53183,.F.);
#84213=ORIENTED_EDGE('',*,*,#57793,.T.);
#84214=ORIENTED_EDGE('',*,*,#52339,.F.);
#84215=ORIENTED_EDGE('',*,*,#57795,.F.);
#84216=ORIENTED_EDGE('',*,*,#55905,.F.);
#84217=ORIENTED_EDGE('',*,*,#57794,.T.);
#84218=ORIENTED_EDGE('',*,*,#55924,.F.);
#84219=ORIENTED_EDGE('',*,*,#57796,.F.);
#84220=ORIENTED_EDGE('',*,*,#53201,.F.);
#84221=ORIENTED_EDGE('',*,*,#57795,.T.);
#84222=ORIENTED_EDGE('',*,*,#52338,.F.);
#84223=ORIENTED_EDGE('',*,*,#57797,.F.);
#84224=ORIENTED_EDGE('',*,*,#56478,.F.);
#84225=ORIENTED_EDGE('',*,*,#57796,.T.);
#84226=ORIENTED_EDGE('',*,*,#55923,.F.);
#84227=ORIENTED_EDGE('',*,*,#57798,.F.);
#84228=ORIENTED_EDGE('',*,*,#52686,.F.);
#84229=ORIENTED_EDGE('',*,*,#57797,.T.);
#84230=ORIENTED_EDGE('',*,*,#52337,.F.);
#84231=ORIENTED_EDGE('',*,*,#57799,.F.);
#84232=ORIENTED_EDGE('',*,*,#55911,.F.);
#84233=ORIENTED_EDGE('',*,*,#57798,.T.);
#84234=ORIENTED_EDGE('',*,*,#56477,.F.);
#84235=ORIENTED_EDGE('',*,*,#57800,.F.);
#84236=ORIENTED_EDGE('',*,*,#52687,.F.);
#84237=ORIENTED_EDGE('',*,*,#57799,.T.);
#84238=ORIENTED_EDGE('',*,*,#53232,.F.);
#84239=ORIENTED_EDGE('',*,*,#57801,.F.);
#84240=ORIENTED_EDGE('',*,*,#55912,.F.);
#84241=ORIENTED_EDGE('',*,*,#57800,.T.);
#84242=ORIENTED_EDGE('',*,*,#55907,.F.);
#84243=ORIENTED_EDGE('',*,*,#57802,.F.);
#84244=ORIENTED_EDGE('',*,*,#52688,.F.);
#84245=ORIENTED_EDGE('',*,*,#53227,.F.);
#84246=ORIENTED_EDGE('',*,*,#53223,.T.);
#84247=ORIENTED_EDGE('',*,*,#57803,.F.);
#84248=ORIENTED_EDGE('',*,*,#55913,.F.);
#84249=ORIENTED_EDGE('',*,*,#57801,.T.);
#84250=ORIENTED_EDGE('',*,*,#57802,.T.);
#84251=ORIENTED_EDGE('',*,*,#56479,.F.);
#84252=ORIENTED_EDGE('',*,*,#57804,.F.);
#84253=ORIENTED_EDGE('',*,*,#52689,.F.);
#84254=ORIENTED_EDGE('',*,*,#57803,.T.);
#84255=ORIENTED_EDGE('',*,*,#53222,.F.);
#84256=ORIENTED_EDGE('',*,*,#57805,.F.);
#84257=ORIENTED_EDGE('',*,*,#55914,.F.);
#84258=ORIENTED_EDGE('',*,*,#57804,.T.);
#84259=ORIENTED_EDGE('',*,*,#55909,.F.);
#84260=ORIENTED_EDGE('',*,*,#57806,.F.);
#84261=ORIENTED_EDGE('',*,*,#52690,.F.);
#84262=ORIENTED_EDGE('',*,*,#57805,.T.);
#84263=ORIENTED_EDGE('',*,*,#53234,.F.);
#84264=ORIENTED_EDGE('',*,*,#57807,.F.);
#84265=ORIENTED_EDGE('',*,*,#55915,.F.);
#84266=ORIENTED_EDGE('',*,*,#57806,.T.);
#84267=ORIENTED_EDGE('',*,*,#55908,.F.);
#84268=ORIENTED_EDGE('',*,*,#57808,.F.);
#84269=ORIENTED_EDGE('',*,*,#53230,.F.);
#84270=ORIENTED_EDGE('',*,*,#57807,.T.);
#84271=ORIENTED_EDGE('',*,*,#53218,.F.);
#84272=ORIENTED_EDGE('',*,*,#57809,.F.);
#84273=ORIENTED_EDGE('',*,*,#55916,.F.);
#84274=ORIENTED_EDGE('',*,*,#57808,.T.);
#84275=ORIENTED_EDGE('',*,*,#55919,.F.);
#84276=ORIENTED_EDGE('',*,*,#57810,.F.);
#84277=ORIENTED_EDGE('',*,*,#53209,.F.);
#84278=ORIENTED_EDGE('',*,*,#57809,.T.);
#84279=ORIENTED_EDGE('',*,*,#53236,.F.);
#84280=ORIENTED_EDGE('',*,*,#57811,.F.);
#84281=ORIENTED_EDGE('',*,*,#55917,.F.);
#84282=ORIENTED_EDGE('',*,*,#57810,.T.);
#84283=ORIENTED_EDGE('',*,*,#55918,.F.);
#84284=ORIENTED_EDGE('',*,*,#57811,.T.);
#84285=ORIENTED_EDGE('',*,*,#53214,.F.);
#84286=ORIENTED_EDGE('',*,*,#53210,.T.);
#84287=ORIENTED_EDGE('',*,*,#57812,.F.);
#84288=ORIENTED_EDGE('',*,*,#55958,.F.);
#84289=ORIENTED_EDGE('',*,*,#57813,.F.);
#84290=ORIENTED_EDGE('',*,*,#53166,.F.);
#84291=ORIENTED_EDGE('',*,*,#57813,.T.);
#84292=ORIENTED_EDGE('',*,*,#55957,.F.);
#84293=ORIENTED_EDGE('',*,*,#57814,.F.);
#84294=ORIENTED_EDGE('',*,*,#53175,.F.);
#84295=ORIENTED_EDGE('',*,*,#53165,.T.);
#84296=ORIENTED_EDGE('',*,*,#53169,.F.);
#84297=ORIENTED_EDGE('',*,*,#57815,.F.);
#84298=ORIENTED_EDGE('',*,*,#55959,.F.);
#84299=ORIENTED_EDGE('',*,*,#57812,.T.);
#84300=ORIENTED_EDGE('',*,*,#57814,.T.);
#84301=ORIENTED_EDGE('',*,*,#55956,.F.);
#84302=ORIENTED_EDGE('',*,*,#57816,.F.);
#84303=ORIENTED_EDGE('',*,*,#53160,.F.);
#84304=ORIENTED_EDGE('',*,*,#57815,.T.);
#84305=ORIENTED_EDGE('',*,*,#53173,.F.);
#84306=ORIENTED_EDGE('',*,*,#57817,.F.);
#84307=ORIENTED_EDGE('',*,*,#55948,.F.);
#84308=ORIENTED_EDGE('',*,*,#57816,.T.);
#84309=ORIENTED_EDGE('',*,*,#55955,.F.);
#84310=ORIENTED_EDGE('',*,*,#57818,.F.);
#84311=ORIENTED_EDGE('',*,*,#53177,.F.);
#84312=ORIENTED_EDGE('',*,*,#57817,.T.);
#84313=ORIENTED_EDGE('',*,*,#52347,.F.);
#84314=ORIENTED_EDGE('',*,*,#57819,.F.);
#84315=ORIENTED_EDGE('',*,*,#55949,.F.);
#84316=ORIENTED_EDGE('',*,*,#57818,.T.);
#84317=ORIENTED_EDGE('',*,*,#55954,.F.);
#84318=ORIENTED_EDGE('',*,*,#57820,.F.);
#84319=ORIENTED_EDGE('',*,*,#53152,.T.);
#84320=ORIENTED_EDGE('',*,*,#53156,.F.);
#84321=ORIENTED_EDGE('',*,*,#57819,.T.);
#84322=ORIENTED_EDGE('',*,*,#52346,.F.);
#84323=ORIENTED_EDGE('',*,*,#57821,.F.);
#84324=ORIENTED_EDGE('',*,*,#56480,.F.);
#84325=ORIENTED_EDGE('',*,*,#57820,.T.);
#84326=ORIENTED_EDGE('',*,*,#55953,.F.);
#84327=ORIENTED_EDGE('',*,*,#57822,.F.);
#84328=ORIENTED_EDGE('',*,*,#53153,.F.);
#84329=ORIENTED_EDGE('',*,*,#57821,.T.);
#84330=ORIENTED_EDGE('',*,*,#52345,.F.);
#84331=ORIENTED_EDGE('',*,*,#57823,.F.);
#84332=ORIENTED_EDGE('',*,*,#55933,.F.);
#84333=ORIENTED_EDGE('',*,*,#57822,.T.);
#84334=ORIENTED_EDGE('',*,*,#55952,.F.);
#84335=ORIENTED_EDGE('',*,*,#57824,.F.);
#84336=ORIENTED_EDGE('',*,*,#53171,.F.);
#84337=ORIENTED_EDGE('',*,*,#57823,.T.);
#84338=ORIENTED_EDGE('',*,*,#52344,.F.);
#84339=ORIENTED_EDGE('',*,*,#57825,.F.);
#84340=ORIENTED_EDGE('',*,*,#56482,.F.);
#84341=ORIENTED_EDGE('',*,*,#57824,.T.);
#84342=ORIENTED_EDGE('',*,*,#55951,.F.);
#84343=ORIENTED_EDGE('',*,*,#57826,.F.);
#84344=ORIENTED_EDGE('',*,*,#52680,.F.);
#84345=ORIENTED_EDGE('',*,*,#57825,.T.);
#84346=ORIENTED_EDGE('',*,*,#52343,.F.);
#84347=ORIENTED_EDGE('',*,*,#57827,.F.);
#84348=ORIENTED_EDGE('',*,*,#55939,.F.);
#84349=ORIENTED_EDGE('',*,*,#57826,.T.);
#84350=ORIENTED_EDGE('',*,*,#56481,.F.);
#84351=ORIENTED_EDGE('',*,*,#57828,.F.);
#84352=ORIENTED_EDGE('',*,*,#52681,.F.);
#84353=ORIENTED_EDGE('',*,*,#57827,.T.);
#84354=ORIENTED_EDGE('',*,*,#53202,.F.);
#84355=ORIENTED_EDGE('',*,*,#57829,.F.);
#84356=ORIENTED_EDGE('',*,*,#55940,.F.);
#84357=ORIENTED_EDGE('',*,*,#57828,.T.);
#84358=ORIENTED_EDGE('',*,*,#55935,.F.);
#84359=ORIENTED_EDGE('',*,*,#57830,.F.);
#84360=ORIENTED_EDGE('',*,*,#52682,.F.);
#84361=ORIENTED_EDGE('',*,*,#53197,.F.);
#84362=ORIENTED_EDGE('',*,*,#53193,.T.);
#84363=ORIENTED_EDGE('',*,*,#57831,.F.);
#84364=ORIENTED_EDGE('',*,*,#55941,.F.);
#84365=ORIENTED_EDGE('',*,*,#57829,.T.);
#84366=ORIENTED_EDGE('',*,*,#57830,.T.);
#84367=ORIENTED_EDGE('',*,*,#56483,.F.);
#84368=ORIENTED_EDGE('',*,*,#57832,.F.);
#84369=ORIENTED_EDGE('',*,*,#52683,.F.);
#84370=ORIENTED_EDGE('',*,*,#57831,.T.);
#84371=ORIENTED_EDGE('',*,*,#53192,.F.);
#84372=ORIENTED_EDGE('',*,*,#57833,.F.);
#84373=ORIENTED_EDGE('',*,*,#55942,.F.);
#84374=ORIENTED_EDGE('',*,*,#57832,.T.);
#84375=ORIENTED_EDGE('',*,*,#55937,.F.);
#84376=ORIENTED_EDGE('',*,*,#57834,.F.);
#84377=ORIENTED_EDGE('',*,*,#52684,.F.);
#84378=ORIENTED_EDGE('',*,*,#57833,.T.);
#84379=ORIENTED_EDGE('',*,*,#53204,.F.);
#84380=ORIENTED_EDGE('',*,*,#57835,.F.);
#84381=ORIENTED_EDGE('',*,*,#55943,.F.);
#84382=ORIENTED_EDGE('',*,*,#57834,.T.);
#84383=ORIENTED_EDGE('',*,*,#55936,.F.);
#84384=ORIENTED_EDGE('',*,*,#57836,.F.);
#84385=ORIENTED_EDGE('',*,*,#53200,.F.);
#84386=ORIENTED_EDGE('',*,*,#57835,.T.);
#84387=ORIENTED_EDGE('',*,*,#53188,.F.);
#84388=ORIENTED_EDGE('',*,*,#57837,.F.);
#84389=ORIENTED_EDGE('',*,*,#55944,.F.);
#84390=ORIENTED_EDGE('',*,*,#57836,.T.);
#84391=ORIENTED_EDGE('',*,*,#55947,.F.);
#84392=ORIENTED_EDGE('',*,*,#57838,.F.);
#84393=ORIENTED_EDGE('',*,*,#53179,.F.);
#84394=ORIENTED_EDGE('',*,*,#57837,.T.);
#84395=ORIENTED_EDGE('',*,*,#53206,.F.);
#84396=ORIENTED_EDGE('',*,*,#57839,.F.);
#84397=ORIENTED_EDGE('',*,*,#55945,.F.);
#84398=ORIENTED_EDGE('',*,*,#57838,.T.);
#84399=ORIENTED_EDGE('',*,*,#55946,.F.);
#84400=ORIENTED_EDGE('',*,*,#57839,.T.);
#84401=ORIENTED_EDGE('',*,*,#53184,.F.);
#84402=ORIENTED_EDGE('',*,*,#53180,.T.);
#84403=ORIENTED_EDGE('',*,*,#57840,.F.);
#84404=ORIENTED_EDGE('',*,*,#55986,.F.);
#84405=ORIENTED_EDGE('',*,*,#57841,.F.);
#84406=ORIENTED_EDGE('',*,*,#53136,.F.);
#84407=ORIENTED_EDGE('',*,*,#57841,.T.);
#84408=ORIENTED_EDGE('',*,*,#55985,.F.);
#84409=ORIENTED_EDGE('',*,*,#57842,.F.);
#84410=ORIENTED_EDGE('',*,*,#53145,.F.);
#84411=ORIENTED_EDGE('',*,*,#53135,.T.);
#84412=ORIENTED_EDGE('',*,*,#53139,.F.);
#84413=ORIENTED_EDGE('',*,*,#57843,.F.);
#84414=ORIENTED_EDGE('',*,*,#55987,.F.);
#84415=ORIENTED_EDGE('',*,*,#57840,.T.);
#84416=ORIENTED_EDGE('',*,*,#57842,.T.);
#84417=ORIENTED_EDGE('',*,*,#55984,.F.);
#84418=ORIENTED_EDGE('',*,*,#57844,.F.);
#84419=ORIENTED_EDGE('',*,*,#53130,.F.);
#84420=ORIENTED_EDGE('',*,*,#57843,.T.);
#84421=ORIENTED_EDGE('',*,*,#53143,.F.);
#84422=ORIENTED_EDGE('',*,*,#57845,.F.);
#84423=ORIENTED_EDGE('',*,*,#55976,.F.);
#84424=ORIENTED_EDGE('',*,*,#57844,.T.);
#84425=ORIENTED_EDGE('',*,*,#55983,.F.);
#84426=ORIENTED_EDGE('',*,*,#57846,.F.);
#84427=ORIENTED_EDGE('',*,*,#53147,.F.);
#84428=ORIENTED_EDGE('',*,*,#57845,.T.);
#84429=ORIENTED_EDGE('',*,*,#52353,.F.);
#84430=ORIENTED_EDGE('',*,*,#57847,.F.);
#84431=ORIENTED_EDGE('',*,*,#55977,.F.);
#84432=ORIENTED_EDGE('',*,*,#57846,.T.);
#84433=ORIENTED_EDGE('',*,*,#55982,.F.);
#84434=ORIENTED_EDGE('',*,*,#57848,.F.);
#84435=ORIENTED_EDGE('',*,*,#53122,.T.);
#84436=ORIENTED_EDGE('',*,*,#53126,.F.);
#84437=ORIENTED_EDGE('',*,*,#57847,.T.);
#84438=ORIENTED_EDGE('',*,*,#52352,.F.);
#84439=ORIENTED_EDGE('',*,*,#57849,.F.);
#84440=ORIENTED_EDGE('',*,*,#56484,.F.);
#84441=ORIENTED_EDGE('',*,*,#57848,.T.);
#84442=ORIENTED_EDGE('',*,*,#55981,.F.);
#84443=ORIENTED_EDGE('',*,*,#57850,.F.);
#84444=ORIENTED_EDGE('',*,*,#53123,.F.);
#84445=ORIENTED_EDGE('',*,*,#57849,.T.);
#84446=ORIENTED_EDGE('',*,*,#52351,.F.);
#84447=ORIENTED_EDGE('',*,*,#57851,.F.);
#84448=ORIENTED_EDGE('',*,*,#55961,.F.);
#84449=ORIENTED_EDGE('',*,*,#57850,.T.);
#84450=ORIENTED_EDGE('',*,*,#55980,.F.);
#84451=ORIENTED_EDGE('',*,*,#57852,.F.);
#84452=ORIENTED_EDGE('',*,*,#53141,.F.);
#84453=ORIENTED_EDGE('',*,*,#57851,.T.);
#84454=ORIENTED_EDGE('',*,*,#52350,.F.);
#84455=ORIENTED_EDGE('',*,*,#57853,.F.);
#84456=ORIENTED_EDGE('',*,*,#56486,.F.);
#84457=ORIENTED_EDGE('',*,*,#57852,.T.);
#84458=ORIENTED_EDGE('',*,*,#55979,.F.);
#84459=ORIENTED_EDGE('',*,*,#57854,.F.);
#84460=ORIENTED_EDGE('',*,*,#52674,.F.);
#84461=ORIENTED_EDGE('',*,*,#57853,.T.);
#84462=ORIENTED_EDGE('',*,*,#52349,.F.);
#84463=ORIENTED_EDGE('',*,*,#57855,.F.);
#84464=ORIENTED_EDGE('',*,*,#55967,.F.);
#84465=ORIENTED_EDGE('',*,*,#57854,.T.);
#84466=ORIENTED_EDGE('',*,*,#56485,.F.);
#84467=ORIENTED_EDGE('',*,*,#57856,.F.);
#84468=ORIENTED_EDGE('',*,*,#52675,.F.);
#84469=ORIENTED_EDGE('',*,*,#57855,.T.);
#84470=ORIENTED_EDGE('',*,*,#53172,.F.);
#84471=ORIENTED_EDGE('',*,*,#57857,.F.);
#84472=ORIENTED_EDGE('',*,*,#55968,.F.);
#84473=ORIENTED_EDGE('',*,*,#57856,.T.);
#84474=ORIENTED_EDGE('',*,*,#55963,.F.);
#84475=ORIENTED_EDGE('',*,*,#57858,.F.);
#84476=ORIENTED_EDGE('',*,*,#52676,.F.);
#84477=ORIENTED_EDGE('',*,*,#53167,.F.);
#84478=ORIENTED_EDGE('',*,*,#53163,.T.);
#84479=ORIENTED_EDGE('',*,*,#57859,.F.);
#84480=ORIENTED_EDGE('',*,*,#55969,.F.);
#84481=ORIENTED_EDGE('',*,*,#57857,.T.);
#84482=ORIENTED_EDGE('',*,*,#57858,.T.);
#84483=ORIENTED_EDGE('',*,*,#56487,.F.);
#84484=ORIENTED_EDGE('',*,*,#57860,.F.);
#84485=ORIENTED_EDGE('',*,*,#52677,.F.);
#84486=ORIENTED_EDGE('',*,*,#57859,.T.);
#84487=ORIENTED_EDGE('',*,*,#53162,.F.);
#84488=ORIENTED_EDGE('',*,*,#57861,.F.);
#84489=ORIENTED_EDGE('',*,*,#55970,.F.);
#84490=ORIENTED_EDGE('',*,*,#57860,.T.);
#84491=ORIENTED_EDGE('',*,*,#55965,.F.);
#84492=ORIENTED_EDGE('',*,*,#57862,.F.);
#84493=ORIENTED_EDGE('',*,*,#52678,.F.);
#84494=ORIENTED_EDGE('',*,*,#57861,.T.);
#84495=ORIENTED_EDGE('',*,*,#53174,.F.);
#84496=ORIENTED_EDGE('',*,*,#57863,.F.);
#84497=ORIENTED_EDGE('',*,*,#55971,.F.);
#84498=ORIENTED_EDGE('',*,*,#57862,.T.);
#84499=ORIENTED_EDGE('',*,*,#55964,.F.);
#84500=ORIENTED_EDGE('',*,*,#57864,.F.);
#84501=ORIENTED_EDGE('',*,*,#53170,.F.);
#84502=ORIENTED_EDGE('',*,*,#57863,.T.);
#84503=ORIENTED_EDGE('',*,*,#53158,.F.);
#84504=ORIENTED_EDGE('',*,*,#57865,.F.);
#84505=ORIENTED_EDGE('',*,*,#55972,.F.);
#84506=ORIENTED_EDGE('',*,*,#57864,.T.);
#84507=ORIENTED_EDGE('',*,*,#55975,.F.);
#84508=ORIENTED_EDGE('',*,*,#57866,.F.);
#84509=ORIENTED_EDGE('',*,*,#53149,.F.);
#84510=ORIENTED_EDGE('',*,*,#57865,.T.);
#84511=ORIENTED_EDGE('',*,*,#53176,.F.);
#84512=ORIENTED_EDGE('',*,*,#57867,.F.);
#84513=ORIENTED_EDGE('',*,*,#55973,.F.);
#84514=ORIENTED_EDGE('',*,*,#57866,.T.);
#84515=ORIENTED_EDGE('',*,*,#55974,.F.);
#84516=ORIENTED_EDGE('',*,*,#57867,.T.);
#84517=ORIENTED_EDGE('',*,*,#53154,.F.);
#84518=ORIENTED_EDGE('',*,*,#53150,.T.);
#84519=ORIENTED_EDGE('',*,*,#57868,.F.);
#84520=ORIENTED_EDGE('',*,*,#56014,.F.);
#84521=ORIENTED_EDGE('',*,*,#57869,.F.);
#84522=ORIENTED_EDGE('',*,*,#53106,.F.);
#84523=ORIENTED_EDGE('',*,*,#57869,.T.);
#84524=ORIENTED_EDGE('',*,*,#56013,.F.);
#84525=ORIENTED_EDGE('',*,*,#57870,.F.);
#84526=ORIENTED_EDGE('',*,*,#53115,.F.);
#84527=ORIENTED_EDGE('',*,*,#53105,.T.);
#84528=ORIENTED_EDGE('',*,*,#53109,.F.);
#84529=ORIENTED_EDGE('',*,*,#57871,.F.);
#84530=ORIENTED_EDGE('',*,*,#56015,.F.);
#84531=ORIENTED_EDGE('',*,*,#57868,.T.);
#84532=ORIENTED_EDGE('',*,*,#57870,.T.);
#84533=ORIENTED_EDGE('',*,*,#56012,.F.);
#84534=ORIENTED_EDGE('',*,*,#57872,.F.);
#84535=ORIENTED_EDGE('',*,*,#53100,.F.);
#84536=ORIENTED_EDGE('',*,*,#57871,.T.);
#84537=ORIENTED_EDGE('',*,*,#53113,.F.);
#84538=ORIENTED_EDGE('',*,*,#57873,.F.);
#84539=ORIENTED_EDGE('',*,*,#56004,.F.);
#84540=ORIENTED_EDGE('',*,*,#57872,.T.);
#84541=ORIENTED_EDGE('',*,*,#56011,.F.);
#84542=ORIENTED_EDGE('',*,*,#57874,.F.);
#84543=ORIENTED_EDGE('',*,*,#53117,.F.);
#84544=ORIENTED_EDGE('',*,*,#57873,.T.);
#84545=ORIENTED_EDGE('',*,*,#52359,.F.);
#84546=ORIENTED_EDGE('',*,*,#57875,.F.);
#84547=ORIENTED_EDGE('',*,*,#56005,.F.);
#84548=ORIENTED_EDGE('',*,*,#57874,.T.);
#84549=ORIENTED_EDGE('',*,*,#56010,.F.);
#84550=ORIENTED_EDGE('',*,*,#57876,.F.);
#84551=ORIENTED_EDGE('',*,*,#53092,.T.);
#84552=ORIENTED_EDGE('',*,*,#53096,.F.);
#84553=ORIENTED_EDGE('',*,*,#57875,.T.);
#84554=ORIENTED_EDGE('',*,*,#52358,.F.);
#84555=ORIENTED_EDGE('',*,*,#57877,.F.);
#84556=ORIENTED_EDGE('',*,*,#56488,.F.);
#84557=ORIENTED_EDGE('',*,*,#57876,.T.);
#84558=ORIENTED_EDGE('',*,*,#56009,.F.);
#84559=ORIENTED_EDGE('',*,*,#57878,.F.);
#84560=ORIENTED_EDGE('',*,*,#53093,.F.);
#84561=ORIENTED_EDGE('',*,*,#57877,.T.);
#84562=ORIENTED_EDGE('',*,*,#52357,.F.);
#84563=ORIENTED_EDGE('',*,*,#57879,.F.);
#84564=ORIENTED_EDGE('',*,*,#55989,.F.);
#84565=ORIENTED_EDGE('',*,*,#57878,.T.);
#84566=ORIENTED_EDGE('',*,*,#56008,.F.);
#84567=ORIENTED_EDGE('',*,*,#57880,.F.);
#84568=ORIENTED_EDGE('',*,*,#53111,.F.);
#84569=ORIENTED_EDGE('',*,*,#57879,.T.);
#84570=ORIENTED_EDGE('',*,*,#52356,.F.);
#84571=ORIENTED_EDGE('',*,*,#57881,.F.);
#84572=ORIENTED_EDGE('',*,*,#56490,.F.);
#84573=ORIENTED_EDGE('',*,*,#57880,.T.);
#84574=ORIENTED_EDGE('',*,*,#56007,.F.);
#84575=ORIENTED_EDGE('',*,*,#57882,.F.);
#84576=ORIENTED_EDGE('',*,*,#52668,.F.);
#84577=ORIENTED_EDGE('',*,*,#57881,.T.);
#84578=ORIENTED_EDGE('',*,*,#52355,.F.);
#84579=ORIENTED_EDGE('',*,*,#57883,.F.);
#84580=ORIENTED_EDGE('',*,*,#55995,.F.);
#84581=ORIENTED_EDGE('',*,*,#57882,.T.);
#84582=ORIENTED_EDGE('',*,*,#56489,.F.);
#84583=ORIENTED_EDGE('',*,*,#57884,.F.);
#84584=ORIENTED_EDGE('',*,*,#52669,.F.);
#84585=ORIENTED_EDGE('',*,*,#57883,.T.);
#84586=ORIENTED_EDGE('',*,*,#53142,.F.);
#84587=ORIENTED_EDGE('',*,*,#57885,.F.);
#84588=ORIENTED_EDGE('',*,*,#55996,.F.);
#84589=ORIENTED_EDGE('',*,*,#57884,.T.);
#84590=ORIENTED_EDGE('',*,*,#55991,.F.);
#84591=ORIENTED_EDGE('',*,*,#57886,.F.);
#84592=ORIENTED_EDGE('',*,*,#52670,.F.);
#84593=ORIENTED_EDGE('',*,*,#53137,.F.);
#84594=ORIENTED_EDGE('',*,*,#53133,.T.);
#84595=ORIENTED_EDGE('',*,*,#57887,.F.);
#84596=ORIENTED_EDGE('',*,*,#55997,.F.);
#84597=ORIENTED_EDGE('',*,*,#57885,.T.);
#84598=ORIENTED_EDGE('',*,*,#57886,.T.);
#84599=ORIENTED_EDGE('',*,*,#56491,.F.);
#84600=ORIENTED_EDGE('',*,*,#57888,.F.);
#84601=ORIENTED_EDGE('',*,*,#52671,.F.);
#84602=ORIENTED_EDGE('',*,*,#57887,.T.);
#84603=ORIENTED_EDGE('',*,*,#53132,.F.);
#84604=ORIENTED_EDGE('',*,*,#57889,.F.);
#84605=ORIENTED_EDGE('',*,*,#55998,.F.);
#84606=ORIENTED_EDGE('',*,*,#57888,.T.);
#84607=ORIENTED_EDGE('',*,*,#55993,.F.);
#84608=ORIENTED_EDGE('',*,*,#57890,.F.);
#84609=ORIENTED_EDGE('',*,*,#52672,.F.);
#84610=ORIENTED_EDGE('',*,*,#57889,.T.);
#84611=ORIENTED_EDGE('',*,*,#53144,.F.);
#84612=ORIENTED_EDGE('',*,*,#57891,.F.);
#84613=ORIENTED_EDGE('',*,*,#55999,.F.);
#84614=ORIENTED_EDGE('',*,*,#57890,.T.);
#84615=ORIENTED_EDGE('',*,*,#55992,.F.);
#84616=ORIENTED_EDGE('',*,*,#57892,.F.);
#84617=ORIENTED_EDGE('',*,*,#53140,.F.);
#84618=ORIENTED_EDGE('',*,*,#57891,.T.);
#84619=ORIENTED_EDGE('',*,*,#53128,.F.);
#84620=ORIENTED_EDGE('',*,*,#57893,.F.);
#84621=ORIENTED_EDGE('',*,*,#56000,.F.);
#84622=ORIENTED_EDGE('',*,*,#57892,.T.);
#84623=ORIENTED_EDGE('',*,*,#56003,.F.);
#84624=ORIENTED_EDGE('',*,*,#57894,.F.);
#84625=ORIENTED_EDGE('',*,*,#53119,.F.);
#84626=ORIENTED_EDGE('',*,*,#57893,.T.);
#84627=ORIENTED_EDGE('',*,*,#53146,.F.);
#84628=ORIENTED_EDGE('',*,*,#57895,.F.);
#84629=ORIENTED_EDGE('',*,*,#56001,.F.);
#84630=ORIENTED_EDGE('',*,*,#57894,.T.);
#84631=ORIENTED_EDGE('',*,*,#56002,.F.);
#84632=ORIENTED_EDGE('',*,*,#57895,.T.);
#84633=ORIENTED_EDGE('',*,*,#53124,.F.);
#84634=ORIENTED_EDGE('',*,*,#53120,.T.);
#84635=ORIENTED_EDGE('',*,*,#57896,.F.);
#84636=ORIENTED_EDGE('',*,*,#56042,.F.);
#84637=ORIENTED_EDGE('',*,*,#57897,.F.);
#84638=ORIENTED_EDGE('',*,*,#53076,.F.);
#84639=ORIENTED_EDGE('',*,*,#57897,.T.);
#84640=ORIENTED_EDGE('',*,*,#56041,.F.);
#84641=ORIENTED_EDGE('',*,*,#57898,.F.);
#84642=ORIENTED_EDGE('',*,*,#53085,.F.);
#84643=ORIENTED_EDGE('',*,*,#53075,.T.);
#84644=ORIENTED_EDGE('',*,*,#53079,.F.);
#84645=ORIENTED_EDGE('',*,*,#57899,.F.);
#84646=ORIENTED_EDGE('',*,*,#56043,.F.);
#84647=ORIENTED_EDGE('',*,*,#57896,.T.);
#84648=ORIENTED_EDGE('',*,*,#57898,.T.);
#84649=ORIENTED_EDGE('',*,*,#56040,.F.);
#84650=ORIENTED_EDGE('',*,*,#57900,.F.);
#84651=ORIENTED_EDGE('',*,*,#53070,.F.);
#84652=ORIENTED_EDGE('',*,*,#57899,.T.);
#84653=ORIENTED_EDGE('',*,*,#53083,.F.);
#84654=ORIENTED_EDGE('',*,*,#57901,.F.);
#84655=ORIENTED_EDGE('',*,*,#56032,.F.);
#84656=ORIENTED_EDGE('',*,*,#57900,.T.);
#84657=ORIENTED_EDGE('',*,*,#56039,.F.);
#84658=ORIENTED_EDGE('',*,*,#57902,.F.);
#84659=ORIENTED_EDGE('',*,*,#53087,.F.);
#84660=ORIENTED_EDGE('',*,*,#57901,.T.);
#84661=ORIENTED_EDGE('',*,*,#52365,.F.);
#84662=ORIENTED_EDGE('',*,*,#57903,.F.);
#84663=ORIENTED_EDGE('',*,*,#56033,.F.);
#84664=ORIENTED_EDGE('',*,*,#57902,.T.);
#84665=ORIENTED_EDGE('',*,*,#56038,.F.);
#84666=ORIENTED_EDGE('',*,*,#57904,.F.);
#84667=ORIENTED_EDGE('',*,*,#53062,.T.);
#84668=ORIENTED_EDGE('',*,*,#53066,.F.);
#84669=ORIENTED_EDGE('',*,*,#57903,.T.);
#84670=ORIENTED_EDGE('',*,*,#52364,.F.);
#84671=ORIENTED_EDGE('',*,*,#57905,.F.);
#84672=ORIENTED_EDGE('',*,*,#56492,.F.);
#84673=ORIENTED_EDGE('',*,*,#57904,.T.);
#84674=ORIENTED_EDGE('',*,*,#56037,.F.);
#84675=ORIENTED_EDGE('',*,*,#57906,.F.);
#84676=ORIENTED_EDGE('',*,*,#53063,.F.);
#84677=ORIENTED_EDGE('',*,*,#57905,.T.);
#84678=ORIENTED_EDGE('',*,*,#52363,.F.);
#84679=ORIENTED_EDGE('',*,*,#57907,.F.);
#84680=ORIENTED_EDGE('',*,*,#56017,.F.);
#84681=ORIENTED_EDGE('',*,*,#57906,.T.);
#84682=ORIENTED_EDGE('',*,*,#56036,.F.);
#84683=ORIENTED_EDGE('',*,*,#57908,.F.);
#84684=ORIENTED_EDGE('',*,*,#53081,.F.);
#84685=ORIENTED_EDGE('',*,*,#57907,.T.);
#84686=ORIENTED_EDGE('',*,*,#52362,.F.);
#84687=ORIENTED_EDGE('',*,*,#57909,.F.);
#84688=ORIENTED_EDGE('',*,*,#56494,.F.);
#84689=ORIENTED_EDGE('',*,*,#57908,.T.);
#84690=ORIENTED_EDGE('',*,*,#56035,.F.);
#84691=ORIENTED_EDGE('',*,*,#57910,.F.);
#84692=ORIENTED_EDGE('',*,*,#52662,.F.);
#84693=ORIENTED_EDGE('',*,*,#57909,.T.);
#84694=ORIENTED_EDGE('',*,*,#52361,.F.);
#84695=ORIENTED_EDGE('',*,*,#57911,.F.);
#84696=ORIENTED_EDGE('',*,*,#56023,.F.);
#84697=ORIENTED_EDGE('',*,*,#57910,.T.);
#84698=ORIENTED_EDGE('',*,*,#56493,.F.);
#84699=ORIENTED_EDGE('',*,*,#57912,.F.);
#84700=ORIENTED_EDGE('',*,*,#52663,.F.);
#84701=ORIENTED_EDGE('',*,*,#57911,.T.);
#84702=ORIENTED_EDGE('',*,*,#53112,.F.);
#84703=ORIENTED_EDGE('',*,*,#57913,.F.);
#84704=ORIENTED_EDGE('',*,*,#56024,.F.);
#84705=ORIENTED_EDGE('',*,*,#57912,.T.);
#84706=ORIENTED_EDGE('',*,*,#56019,.F.);
#84707=ORIENTED_EDGE('',*,*,#57914,.F.);
#84708=ORIENTED_EDGE('',*,*,#52664,.F.);
#84709=ORIENTED_EDGE('',*,*,#53107,.F.);
#84710=ORIENTED_EDGE('',*,*,#53103,.T.);
#84711=ORIENTED_EDGE('',*,*,#57915,.F.);
#84712=ORIENTED_EDGE('',*,*,#56025,.F.);
#84713=ORIENTED_EDGE('',*,*,#57913,.T.);
#84714=ORIENTED_EDGE('',*,*,#57914,.T.);
#84715=ORIENTED_EDGE('',*,*,#56495,.F.);
#84716=ORIENTED_EDGE('',*,*,#57916,.F.);
#84717=ORIENTED_EDGE('',*,*,#52665,.F.);
#84718=ORIENTED_EDGE('',*,*,#57915,.T.);
#84719=ORIENTED_EDGE('',*,*,#53102,.F.);
#84720=ORIENTED_EDGE('',*,*,#57917,.F.);
#84721=ORIENTED_EDGE('',*,*,#56026,.F.);
#84722=ORIENTED_EDGE('',*,*,#57916,.T.);
#84723=ORIENTED_EDGE('',*,*,#56021,.F.);
#84724=ORIENTED_EDGE('',*,*,#57918,.F.);
#84725=ORIENTED_EDGE('',*,*,#52666,.F.);
#84726=ORIENTED_EDGE('',*,*,#57917,.T.);
#84727=ORIENTED_EDGE('',*,*,#53114,.F.);
#84728=ORIENTED_EDGE('',*,*,#57919,.F.);
#84729=ORIENTED_EDGE('',*,*,#56027,.F.);
#84730=ORIENTED_EDGE('',*,*,#57918,.T.);
#84731=ORIENTED_EDGE('',*,*,#56020,.F.);
#84732=ORIENTED_EDGE('',*,*,#57920,.F.);
#84733=ORIENTED_EDGE('',*,*,#53110,.F.);
#84734=ORIENTED_EDGE('',*,*,#57919,.T.);
#84735=ORIENTED_EDGE('',*,*,#53098,.F.);
#84736=ORIENTED_EDGE('',*,*,#57921,.F.);
#84737=ORIENTED_EDGE('',*,*,#56028,.F.);
#84738=ORIENTED_EDGE('',*,*,#57920,.T.);
#84739=ORIENTED_EDGE('',*,*,#56031,.F.);
#84740=ORIENTED_EDGE('',*,*,#57922,.F.);
#84741=ORIENTED_EDGE('',*,*,#53089,.F.);
#84742=ORIENTED_EDGE('',*,*,#57921,.T.);
#84743=ORIENTED_EDGE('',*,*,#53116,.F.);
#84744=ORIENTED_EDGE('',*,*,#57923,.F.);
#84745=ORIENTED_EDGE('',*,*,#56029,.F.);
#84746=ORIENTED_EDGE('',*,*,#57922,.T.);
#84747=ORIENTED_EDGE('',*,*,#56030,.F.);
#84748=ORIENTED_EDGE('',*,*,#57923,.T.);
#84749=ORIENTED_EDGE('',*,*,#53094,.F.);
#84750=ORIENTED_EDGE('',*,*,#53090,.T.);
#84751=ORIENTED_EDGE('',*,*,#57924,.F.);
#84752=ORIENTED_EDGE('',*,*,#56070,.F.);
#84753=ORIENTED_EDGE('',*,*,#57925,.F.);
#84754=ORIENTED_EDGE('',*,*,#53046,.F.);
#84755=ORIENTED_EDGE('',*,*,#57925,.T.);
#84756=ORIENTED_EDGE('',*,*,#56069,.F.);
#84757=ORIENTED_EDGE('',*,*,#57926,.F.);
#84758=ORIENTED_EDGE('',*,*,#53055,.F.);
#84759=ORIENTED_EDGE('',*,*,#53045,.T.);
#84760=ORIENTED_EDGE('',*,*,#53049,.F.);
#84761=ORIENTED_EDGE('',*,*,#57927,.F.);
#84762=ORIENTED_EDGE('',*,*,#56071,.F.);
#84763=ORIENTED_EDGE('',*,*,#57924,.T.);
#84764=ORIENTED_EDGE('',*,*,#57926,.T.);
#84765=ORIENTED_EDGE('',*,*,#56068,.F.);
#84766=ORIENTED_EDGE('',*,*,#57928,.F.);
#84767=ORIENTED_EDGE('',*,*,#53040,.F.);
#84768=ORIENTED_EDGE('',*,*,#57927,.T.);
#84769=ORIENTED_EDGE('',*,*,#53053,.F.);
#84770=ORIENTED_EDGE('',*,*,#57929,.F.);
#84771=ORIENTED_EDGE('',*,*,#56060,.F.);
#84772=ORIENTED_EDGE('',*,*,#57928,.T.);
#84773=ORIENTED_EDGE('',*,*,#56067,.F.);
#84774=ORIENTED_EDGE('',*,*,#57930,.F.);
#84775=ORIENTED_EDGE('',*,*,#53057,.F.);
#84776=ORIENTED_EDGE('',*,*,#57929,.T.);
#84777=ORIENTED_EDGE('',*,*,#52371,.F.);
#84778=ORIENTED_EDGE('',*,*,#57931,.F.);
#84779=ORIENTED_EDGE('',*,*,#56061,.F.);
#84780=ORIENTED_EDGE('',*,*,#57930,.T.);
#84781=ORIENTED_EDGE('',*,*,#56066,.F.);
#84782=ORIENTED_EDGE('',*,*,#57932,.F.);
#84783=ORIENTED_EDGE('',*,*,#53032,.T.);
#84784=ORIENTED_EDGE('',*,*,#53036,.F.);
#84785=ORIENTED_EDGE('',*,*,#57931,.T.);
#84786=ORIENTED_EDGE('',*,*,#52370,.F.);
#84787=ORIENTED_EDGE('',*,*,#57933,.F.);
#84788=ORIENTED_EDGE('',*,*,#56496,.F.);
#84789=ORIENTED_EDGE('',*,*,#57932,.T.);
#84790=ORIENTED_EDGE('',*,*,#56065,.F.);
#84791=ORIENTED_EDGE('',*,*,#57934,.F.);
#84792=ORIENTED_EDGE('',*,*,#53033,.F.);
#84793=ORIENTED_EDGE('',*,*,#57933,.T.);
#84794=ORIENTED_EDGE('',*,*,#52369,.F.);
#84795=ORIENTED_EDGE('',*,*,#57935,.F.);
#84796=ORIENTED_EDGE('',*,*,#56045,.F.);
#84797=ORIENTED_EDGE('',*,*,#57934,.T.);
#84798=ORIENTED_EDGE('',*,*,#56064,.F.);
#84799=ORIENTED_EDGE('',*,*,#57936,.F.);
#84800=ORIENTED_EDGE('',*,*,#53051,.F.);
#84801=ORIENTED_EDGE('',*,*,#57935,.T.);
#84802=ORIENTED_EDGE('',*,*,#52368,.F.);
#84803=ORIENTED_EDGE('',*,*,#57937,.F.);
#84804=ORIENTED_EDGE('',*,*,#56498,.F.);
#84805=ORIENTED_EDGE('',*,*,#57936,.T.);
#84806=ORIENTED_EDGE('',*,*,#56063,.F.);
#84807=ORIENTED_EDGE('',*,*,#57938,.F.);
#84808=ORIENTED_EDGE('',*,*,#52656,.F.);
#84809=ORIENTED_EDGE('',*,*,#57937,.T.);
#84810=ORIENTED_EDGE('',*,*,#52367,.F.);
#84811=ORIENTED_EDGE('',*,*,#57939,.F.);
#84812=ORIENTED_EDGE('',*,*,#56051,.F.);
#84813=ORIENTED_EDGE('',*,*,#57938,.T.);
#84814=ORIENTED_EDGE('',*,*,#56497,.F.);
#84815=ORIENTED_EDGE('',*,*,#57940,.F.);
#84816=ORIENTED_EDGE('',*,*,#52657,.F.);
#84817=ORIENTED_EDGE('',*,*,#57939,.T.);
#84818=ORIENTED_EDGE('',*,*,#53082,.F.);
#84819=ORIENTED_EDGE('',*,*,#57941,.F.);
#84820=ORIENTED_EDGE('',*,*,#56052,.F.);
#84821=ORIENTED_EDGE('',*,*,#57940,.T.);
#84822=ORIENTED_EDGE('',*,*,#56047,.F.);
#84823=ORIENTED_EDGE('',*,*,#57942,.F.);
#84824=ORIENTED_EDGE('',*,*,#52658,.F.);
#84825=ORIENTED_EDGE('',*,*,#53077,.F.);
#84826=ORIENTED_EDGE('',*,*,#53073,.T.);
#84827=ORIENTED_EDGE('',*,*,#57943,.F.);
#84828=ORIENTED_EDGE('',*,*,#56053,.F.);
#84829=ORIENTED_EDGE('',*,*,#57941,.T.);
#84830=ORIENTED_EDGE('',*,*,#57942,.T.);
#84831=ORIENTED_EDGE('',*,*,#56499,.F.);
#84832=ORIENTED_EDGE('',*,*,#57944,.F.);
#84833=ORIENTED_EDGE('',*,*,#52659,.F.);
#84834=ORIENTED_EDGE('',*,*,#57943,.T.);
#84835=ORIENTED_EDGE('',*,*,#53072,.F.);
#84836=ORIENTED_EDGE('',*,*,#57945,.F.);
#84837=ORIENTED_EDGE('',*,*,#56054,.F.);
#84838=ORIENTED_EDGE('',*,*,#57944,.T.);
#84839=ORIENTED_EDGE('',*,*,#56049,.F.);
#84840=ORIENTED_EDGE('',*,*,#57946,.F.);
#84841=ORIENTED_EDGE('',*,*,#52660,.F.);
#84842=ORIENTED_EDGE('',*,*,#57945,.T.);
#84843=ORIENTED_EDGE('',*,*,#53084,.F.);
#84844=ORIENTED_EDGE('',*,*,#57947,.F.);
#84845=ORIENTED_EDGE('',*,*,#56055,.F.);
#84846=ORIENTED_EDGE('',*,*,#57946,.T.);
#84847=ORIENTED_EDGE('',*,*,#56048,.F.);
#84848=ORIENTED_EDGE('',*,*,#57948,.F.);
#84849=ORIENTED_EDGE('',*,*,#53080,.F.);
#84850=ORIENTED_EDGE('',*,*,#57947,.T.);
#84851=ORIENTED_EDGE('',*,*,#53068,.F.);
#84852=ORIENTED_EDGE('',*,*,#57949,.F.);
#84853=ORIENTED_EDGE('',*,*,#56056,.F.);
#84854=ORIENTED_EDGE('',*,*,#57948,.T.);
#84855=ORIENTED_EDGE('',*,*,#56059,.F.);
#84856=ORIENTED_EDGE('',*,*,#57950,.F.);
#84857=ORIENTED_EDGE('',*,*,#53059,.F.);
#84858=ORIENTED_EDGE('',*,*,#57949,.T.);
#84859=ORIENTED_EDGE('',*,*,#53086,.F.);
#84860=ORIENTED_EDGE('',*,*,#57951,.F.);
#84861=ORIENTED_EDGE('',*,*,#56057,.F.);
#84862=ORIENTED_EDGE('',*,*,#57950,.T.);
#84863=ORIENTED_EDGE('',*,*,#56058,.F.);
#84864=ORIENTED_EDGE('',*,*,#57951,.T.);
#84865=ORIENTED_EDGE('',*,*,#53064,.F.);
#84866=ORIENTED_EDGE('',*,*,#53060,.T.);
#84867=ORIENTED_EDGE('',*,*,#57952,.F.);
#84868=ORIENTED_EDGE('',*,*,#56098,.F.);
#84869=ORIENTED_EDGE('',*,*,#57953,.F.);
#84870=ORIENTED_EDGE('',*,*,#53016,.F.);
#84871=ORIENTED_EDGE('',*,*,#57953,.T.);
#84872=ORIENTED_EDGE('',*,*,#56097,.F.);
#84873=ORIENTED_EDGE('',*,*,#57954,.F.);
#84874=ORIENTED_EDGE('',*,*,#53025,.F.);
#84875=ORIENTED_EDGE('',*,*,#53015,.T.);
#84876=ORIENTED_EDGE('',*,*,#53019,.F.);
#84877=ORIENTED_EDGE('',*,*,#57955,.F.);
#84878=ORIENTED_EDGE('',*,*,#56099,.F.);
#84879=ORIENTED_EDGE('',*,*,#57952,.T.);
#84880=ORIENTED_EDGE('',*,*,#57954,.T.);
#84881=ORIENTED_EDGE('',*,*,#56096,.F.);
#84882=ORIENTED_EDGE('',*,*,#57956,.F.);
#84883=ORIENTED_EDGE('',*,*,#53010,.F.);
#84884=ORIENTED_EDGE('',*,*,#57955,.T.);
#84885=ORIENTED_EDGE('',*,*,#53023,.F.);
#84886=ORIENTED_EDGE('',*,*,#57957,.F.);
#84887=ORIENTED_EDGE('',*,*,#56088,.F.);
#84888=ORIENTED_EDGE('',*,*,#57956,.T.);
#84889=ORIENTED_EDGE('',*,*,#56095,.F.);
#84890=ORIENTED_EDGE('',*,*,#57958,.F.);
#84891=ORIENTED_EDGE('',*,*,#53027,.F.);
#84892=ORIENTED_EDGE('',*,*,#57957,.T.);
#84893=ORIENTED_EDGE('',*,*,#52377,.F.);
#84894=ORIENTED_EDGE('',*,*,#57959,.F.);
#84895=ORIENTED_EDGE('',*,*,#56089,.F.);
#84896=ORIENTED_EDGE('',*,*,#57958,.T.);
#84897=ORIENTED_EDGE('',*,*,#56094,.F.);
#84898=ORIENTED_EDGE('',*,*,#57960,.F.);
#84899=ORIENTED_EDGE('',*,*,#53002,.T.);
#84900=ORIENTED_EDGE('',*,*,#53006,.F.);
#84901=ORIENTED_EDGE('',*,*,#57959,.T.);
#84902=ORIENTED_EDGE('',*,*,#52376,.F.);
#84903=ORIENTED_EDGE('',*,*,#57961,.F.);
#84904=ORIENTED_EDGE('',*,*,#56500,.F.);
#84905=ORIENTED_EDGE('',*,*,#57960,.T.);
#84906=ORIENTED_EDGE('',*,*,#56093,.F.);
#84907=ORIENTED_EDGE('',*,*,#57962,.F.);
#84908=ORIENTED_EDGE('',*,*,#53003,.F.);
#84909=ORIENTED_EDGE('',*,*,#57961,.T.);
#84910=ORIENTED_EDGE('',*,*,#52375,.F.);
#84911=ORIENTED_EDGE('',*,*,#57963,.F.);
#84912=ORIENTED_EDGE('',*,*,#56073,.F.);
#84913=ORIENTED_EDGE('',*,*,#57962,.T.);
#84914=ORIENTED_EDGE('',*,*,#56092,.F.);
#84915=ORIENTED_EDGE('',*,*,#57964,.F.);
#84916=ORIENTED_EDGE('',*,*,#53021,.F.);
#84917=ORIENTED_EDGE('',*,*,#57963,.T.);
#84918=ORIENTED_EDGE('',*,*,#52374,.F.);
#84919=ORIENTED_EDGE('',*,*,#57965,.F.);
#84920=ORIENTED_EDGE('',*,*,#56502,.F.);
#84921=ORIENTED_EDGE('',*,*,#57964,.T.);
#84922=ORIENTED_EDGE('',*,*,#56091,.F.);
#84923=ORIENTED_EDGE('',*,*,#57966,.F.);
#84924=ORIENTED_EDGE('',*,*,#52650,.F.);
#84925=ORIENTED_EDGE('',*,*,#57965,.T.);
#84926=ORIENTED_EDGE('',*,*,#52373,.F.);
#84927=ORIENTED_EDGE('',*,*,#57967,.F.);
#84928=ORIENTED_EDGE('',*,*,#56079,.F.);
#84929=ORIENTED_EDGE('',*,*,#57966,.T.);
#84930=ORIENTED_EDGE('',*,*,#56501,.F.);
#84931=ORIENTED_EDGE('',*,*,#57968,.F.);
#84932=ORIENTED_EDGE('',*,*,#52651,.F.);
#84933=ORIENTED_EDGE('',*,*,#57967,.T.);
#84934=ORIENTED_EDGE('',*,*,#53052,.F.);
#84935=ORIENTED_EDGE('',*,*,#57969,.F.);
#84936=ORIENTED_EDGE('',*,*,#56080,.F.);
#84937=ORIENTED_EDGE('',*,*,#57968,.T.);
#84938=ORIENTED_EDGE('',*,*,#56075,.F.);
#84939=ORIENTED_EDGE('',*,*,#57970,.F.);
#84940=ORIENTED_EDGE('',*,*,#52652,.F.);
#84941=ORIENTED_EDGE('',*,*,#53047,.F.);
#84942=ORIENTED_EDGE('',*,*,#53043,.T.);
#84943=ORIENTED_EDGE('',*,*,#57971,.F.);
#84944=ORIENTED_EDGE('',*,*,#56081,.F.);
#84945=ORIENTED_EDGE('',*,*,#57969,.T.);
#84946=ORIENTED_EDGE('',*,*,#57970,.T.);
#84947=ORIENTED_EDGE('',*,*,#56503,.F.);
#84948=ORIENTED_EDGE('',*,*,#57972,.F.);
#84949=ORIENTED_EDGE('',*,*,#52653,.F.);
#84950=ORIENTED_EDGE('',*,*,#57971,.T.);
#84951=ORIENTED_EDGE('',*,*,#53042,.F.);
#84952=ORIENTED_EDGE('',*,*,#57973,.F.);
#84953=ORIENTED_EDGE('',*,*,#56082,.F.);
#84954=ORIENTED_EDGE('',*,*,#57972,.T.);
#84955=ORIENTED_EDGE('',*,*,#56077,.F.);
#84956=ORIENTED_EDGE('',*,*,#57974,.F.);
#84957=ORIENTED_EDGE('',*,*,#52654,.F.);
#84958=ORIENTED_EDGE('',*,*,#57973,.T.);
#84959=ORIENTED_EDGE('',*,*,#53054,.F.);
#84960=ORIENTED_EDGE('',*,*,#57975,.F.);
#84961=ORIENTED_EDGE('',*,*,#56083,.F.);
#84962=ORIENTED_EDGE('',*,*,#57974,.T.);
#84963=ORIENTED_EDGE('',*,*,#56076,.F.);
#84964=ORIENTED_EDGE('',*,*,#57976,.F.);
#84965=ORIENTED_EDGE('',*,*,#53050,.F.);
#84966=ORIENTED_EDGE('',*,*,#57975,.T.);
#84967=ORIENTED_EDGE('',*,*,#53038,.F.);
#84968=ORIENTED_EDGE('',*,*,#57977,.F.);
#84969=ORIENTED_EDGE('',*,*,#56084,.F.);
#84970=ORIENTED_EDGE('',*,*,#57976,.T.);
#84971=ORIENTED_EDGE('',*,*,#56087,.F.);
#84972=ORIENTED_EDGE('',*,*,#57978,.F.);
#84973=ORIENTED_EDGE('',*,*,#53029,.F.);
#84974=ORIENTED_EDGE('',*,*,#57977,.T.);
#84975=ORIENTED_EDGE('',*,*,#53056,.F.);
#84976=ORIENTED_EDGE('',*,*,#57979,.F.);
#84977=ORIENTED_EDGE('',*,*,#56085,.F.);
#84978=ORIENTED_EDGE('',*,*,#57978,.T.);
#84979=ORIENTED_EDGE('',*,*,#56086,.F.);
#84980=ORIENTED_EDGE('',*,*,#57979,.T.);
#84981=ORIENTED_EDGE('',*,*,#53034,.F.);
#84982=ORIENTED_EDGE('',*,*,#53030,.T.);
#84983=ORIENTED_EDGE('',*,*,#57980,.F.);
#84984=ORIENTED_EDGE('',*,*,#56126,.F.);
#84985=ORIENTED_EDGE('',*,*,#57981,.F.);
#84986=ORIENTED_EDGE('',*,*,#52986,.F.);
#84987=ORIENTED_EDGE('',*,*,#57981,.T.);
#84988=ORIENTED_EDGE('',*,*,#56125,.F.);
#84989=ORIENTED_EDGE('',*,*,#57982,.F.);
#84990=ORIENTED_EDGE('',*,*,#52995,.F.);
#84991=ORIENTED_EDGE('',*,*,#52985,.T.);
#84992=ORIENTED_EDGE('',*,*,#52989,.F.);
#84993=ORIENTED_EDGE('',*,*,#57983,.F.);
#84994=ORIENTED_EDGE('',*,*,#56127,.F.);
#84995=ORIENTED_EDGE('',*,*,#57980,.T.);
#84996=ORIENTED_EDGE('',*,*,#57982,.T.);
#84997=ORIENTED_EDGE('',*,*,#56124,.F.);
#84998=ORIENTED_EDGE('',*,*,#57984,.F.);
#84999=ORIENTED_EDGE('',*,*,#52980,.F.);
#85000=ORIENTED_EDGE('',*,*,#57983,.T.);
#85001=ORIENTED_EDGE('',*,*,#52993,.F.);
#85002=ORIENTED_EDGE('',*,*,#57985,.F.);
#85003=ORIENTED_EDGE('',*,*,#56116,.F.);
#85004=ORIENTED_EDGE('',*,*,#57984,.T.);
#85005=ORIENTED_EDGE('',*,*,#56123,.F.);
#85006=ORIENTED_EDGE('',*,*,#57986,.F.);
#85007=ORIENTED_EDGE('',*,*,#52997,.F.);
#85008=ORIENTED_EDGE('',*,*,#57985,.T.);
#85009=ORIENTED_EDGE('',*,*,#52383,.F.);
#85010=ORIENTED_EDGE('',*,*,#57987,.F.);
#85011=ORIENTED_EDGE('',*,*,#56117,.F.);
#85012=ORIENTED_EDGE('',*,*,#57986,.T.);
#85013=ORIENTED_EDGE('',*,*,#56122,.F.);
#85014=ORIENTED_EDGE('',*,*,#57988,.F.);
#85015=ORIENTED_EDGE('',*,*,#52972,.T.);
#85016=ORIENTED_EDGE('',*,*,#52976,.F.);
#85017=ORIENTED_EDGE('',*,*,#57987,.T.);
#85018=ORIENTED_EDGE('',*,*,#52382,.F.);
#85019=ORIENTED_EDGE('',*,*,#57989,.F.);
#85020=ORIENTED_EDGE('',*,*,#56504,.F.);
#85021=ORIENTED_EDGE('',*,*,#57988,.T.);
#85022=ORIENTED_EDGE('',*,*,#56121,.F.);
#85023=ORIENTED_EDGE('',*,*,#57990,.F.);
#85024=ORIENTED_EDGE('',*,*,#52973,.F.);
#85025=ORIENTED_EDGE('',*,*,#57989,.T.);
#85026=ORIENTED_EDGE('',*,*,#52381,.F.);
#85027=ORIENTED_EDGE('',*,*,#57991,.F.);
#85028=ORIENTED_EDGE('',*,*,#56101,.F.);
#85029=ORIENTED_EDGE('',*,*,#57990,.T.);
#85030=ORIENTED_EDGE('',*,*,#56120,.F.);
#85031=ORIENTED_EDGE('',*,*,#57992,.F.);
#85032=ORIENTED_EDGE('',*,*,#52991,.F.);
#85033=ORIENTED_EDGE('',*,*,#57991,.T.);
#85034=ORIENTED_EDGE('',*,*,#52380,.F.);
#85035=ORIENTED_EDGE('',*,*,#57993,.F.);
#85036=ORIENTED_EDGE('',*,*,#56506,.F.);
#85037=ORIENTED_EDGE('',*,*,#57992,.T.);
#85038=ORIENTED_EDGE('',*,*,#56119,.F.);
#85039=ORIENTED_EDGE('',*,*,#57994,.F.);
#85040=ORIENTED_EDGE('',*,*,#52644,.F.);
#85041=ORIENTED_EDGE('',*,*,#57993,.T.);
#85042=ORIENTED_EDGE('',*,*,#52379,.F.);
#85043=ORIENTED_EDGE('',*,*,#57995,.F.);
#85044=ORIENTED_EDGE('',*,*,#56107,.F.);
#85045=ORIENTED_EDGE('',*,*,#57994,.T.);
#85046=ORIENTED_EDGE('',*,*,#56505,.F.);
#85047=ORIENTED_EDGE('',*,*,#57996,.F.);
#85048=ORIENTED_EDGE('',*,*,#52645,.F.);
#85049=ORIENTED_EDGE('',*,*,#57995,.T.);
#85050=ORIENTED_EDGE('',*,*,#53022,.F.);
#85051=ORIENTED_EDGE('',*,*,#57997,.F.);
#85052=ORIENTED_EDGE('',*,*,#56108,.F.);
#85053=ORIENTED_EDGE('',*,*,#57996,.T.);
#85054=ORIENTED_EDGE('',*,*,#56103,.F.);
#85055=ORIENTED_EDGE('',*,*,#57998,.F.);
#85056=ORIENTED_EDGE('',*,*,#52646,.F.);
#85057=ORIENTED_EDGE('',*,*,#53017,.F.);
#85058=ORIENTED_EDGE('',*,*,#53013,.T.);
#85059=ORIENTED_EDGE('',*,*,#57999,.F.);
#85060=ORIENTED_EDGE('',*,*,#56109,.F.);
#85061=ORIENTED_EDGE('',*,*,#57997,.T.);
#85062=ORIENTED_EDGE('',*,*,#57998,.T.);
#85063=ORIENTED_EDGE('',*,*,#56507,.F.);
#85064=ORIENTED_EDGE('',*,*,#58000,.F.);
#85065=ORIENTED_EDGE('',*,*,#52647,.F.);
#85066=ORIENTED_EDGE('',*,*,#57999,.T.);
#85067=ORIENTED_EDGE('',*,*,#53012,.F.);
#85068=ORIENTED_EDGE('',*,*,#58001,.F.);
#85069=ORIENTED_EDGE('',*,*,#56110,.F.);
#85070=ORIENTED_EDGE('',*,*,#58000,.T.);
#85071=ORIENTED_EDGE('',*,*,#56105,.F.);
#85072=ORIENTED_EDGE('',*,*,#58002,.F.);
#85073=ORIENTED_EDGE('',*,*,#52648,.F.);
#85074=ORIENTED_EDGE('',*,*,#58001,.T.);
#85075=ORIENTED_EDGE('',*,*,#53024,.F.);
#85076=ORIENTED_EDGE('',*,*,#58003,.F.);
#85077=ORIENTED_EDGE('',*,*,#56111,.F.);
#85078=ORIENTED_EDGE('',*,*,#58002,.T.);
#85079=ORIENTED_EDGE('',*,*,#56104,.F.);
#85080=ORIENTED_EDGE('',*,*,#58004,.F.);
#85081=ORIENTED_EDGE('',*,*,#53020,.F.);
#85082=ORIENTED_EDGE('',*,*,#58003,.T.);
#85083=ORIENTED_EDGE('',*,*,#53008,.F.);
#85084=ORIENTED_EDGE('',*,*,#58005,.F.);
#85085=ORIENTED_EDGE('',*,*,#56112,.F.);
#85086=ORIENTED_EDGE('',*,*,#58004,.T.);
#85087=ORIENTED_EDGE('',*,*,#56115,.F.);
#85088=ORIENTED_EDGE('',*,*,#58006,.F.);
#85089=ORIENTED_EDGE('',*,*,#52999,.F.);
#85090=ORIENTED_EDGE('',*,*,#58005,.T.);
#85091=ORIENTED_EDGE('',*,*,#53026,.F.);
#85092=ORIENTED_EDGE('',*,*,#58007,.F.);
#85093=ORIENTED_EDGE('',*,*,#56113,.F.);
#85094=ORIENTED_EDGE('',*,*,#58006,.T.);
#85095=ORIENTED_EDGE('',*,*,#56114,.F.);
#85096=ORIENTED_EDGE('',*,*,#58007,.T.);
#85097=ORIENTED_EDGE('',*,*,#53004,.F.);
#85098=ORIENTED_EDGE('',*,*,#53000,.T.);
#85099=ORIENTED_EDGE('',*,*,#58008,.F.);
#85100=ORIENTED_EDGE('',*,*,#56154,.F.);
#85101=ORIENTED_EDGE('',*,*,#58009,.F.);
#85102=ORIENTED_EDGE('',*,*,#52956,.F.);
#85103=ORIENTED_EDGE('',*,*,#58009,.T.);
#85104=ORIENTED_EDGE('',*,*,#56153,.F.);
#85105=ORIENTED_EDGE('',*,*,#58010,.F.);
#85106=ORIENTED_EDGE('',*,*,#52965,.F.);
#85107=ORIENTED_EDGE('',*,*,#52955,.T.);
#85108=ORIENTED_EDGE('',*,*,#52959,.F.);
#85109=ORIENTED_EDGE('',*,*,#58011,.F.);
#85110=ORIENTED_EDGE('',*,*,#56155,.F.);
#85111=ORIENTED_EDGE('',*,*,#58008,.T.);
#85112=ORIENTED_EDGE('',*,*,#58010,.T.);
#85113=ORIENTED_EDGE('',*,*,#56152,.F.);
#85114=ORIENTED_EDGE('',*,*,#58012,.F.);
#85115=ORIENTED_EDGE('',*,*,#52950,.F.);
#85116=ORIENTED_EDGE('',*,*,#58011,.T.);
#85117=ORIENTED_EDGE('',*,*,#52963,.F.);
#85118=ORIENTED_EDGE('',*,*,#58013,.F.);
#85119=ORIENTED_EDGE('',*,*,#56144,.F.);
#85120=ORIENTED_EDGE('',*,*,#58012,.T.);
#85121=ORIENTED_EDGE('',*,*,#56151,.F.);
#85122=ORIENTED_EDGE('',*,*,#58014,.F.);
#85123=ORIENTED_EDGE('',*,*,#52967,.F.);
#85124=ORIENTED_EDGE('',*,*,#58013,.T.);
#85125=ORIENTED_EDGE('',*,*,#52389,.F.);
#85126=ORIENTED_EDGE('',*,*,#58015,.F.);
#85127=ORIENTED_EDGE('',*,*,#56145,.F.);
#85128=ORIENTED_EDGE('',*,*,#58014,.T.);
#85129=ORIENTED_EDGE('',*,*,#56150,.F.);
#85130=ORIENTED_EDGE('',*,*,#58016,.F.);
#85131=ORIENTED_EDGE('',*,*,#52942,.T.);
#85132=ORIENTED_EDGE('',*,*,#52946,.F.);
#85133=ORIENTED_EDGE('',*,*,#58015,.T.);
#85134=ORIENTED_EDGE('',*,*,#52388,.F.);
#85135=ORIENTED_EDGE('',*,*,#58017,.F.);
#85136=ORIENTED_EDGE('',*,*,#56508,.F.);
#85137=ORIENTED_EDGE('',*,*,#58016,.T.);
#85138=ORIENTED_EDGE('',*,*,#56149,.F.);
#85139=ORIENTED_EDGE('',*,*,#58018,.F.);
#85140=ORIENTED_EDGE('',*,*,#52943,.F.);
#85141=ORIENTED_EDGE('',*,*,#58017,.T.);
#85142=ORIENTED_EDGE('',*,*,#52387,.F.);
#85143=ORIENTED_EDGE('',*,*,#58019,.F.);
#85144=ORIENTED_EDGE('',*,*,#56129,.F.);
#85145=ORIENTED_EDGE('',*,*,#58018,.T.);
#85146=ORIENTED_EDGE('',*,*,#56148,.F.);
#85147=ORIENTED_EDGE('',*,*,#58020,.F.);
#85148=ORIENTED_EDGE('',*,*,#52961,.F.);
#85149=ORIENTED_EDGE('',*,*,#58019,.T.);
#85150=ORIENTED_EDGE('',*,*,#52386,.F.);
#85151=ORIENTED_EDGE('',*,*,#58021,.F.);
#85152=ORIENTED_EDGE('',*,*,#56510,.F.);
#85153=ORIENTED_EDGE('',*,*,#58020,.T.);
#85154=ORIENTED_EDGE('',*,*,#56147,.F.);
#85155=ORIENTED_EDGE('',*,*,#58022,.F.);
#85156=ORIENTED_EDGE('',*,*,#52638,.F.);
#85157=ORIENTED_EDGE('',*,*,#58021,.T.);
#85158=ORIENTED_EDGE('',*,*,#52385,.F.);
#85159=ORIENTED_EDGE('',*,*,#58023,.F.);
#85160=ORIENTED_EDGE('',*,*,#56135,.F.);
#85161=ORIENTED_EDGE('',*,*,#58022,.T.);
#85162=ORIENTED_EDGE('',*,*,#56509,.F.);
#85163=ORIENTED_EDGE('',*,*,#58024,.F.);
#85164=ORIENTED_EDGE('',*,*,#52639,.F.);
#85165=ORIENTED_EDGE('',*,*,#58023,.T.);
#85166=ORIENTED_EDGE('',*,*,#52992,.F.);
#85167=ORIENTED_EDGE('',*,*,#58025,.F.);
#85168=ORIENTED_EDGE('',*,*,#56136,.F.);
#85169=ORIENTED_EDGE('',*,*,#58024,.T.);
#85170=ORIENTED_EDGE('',*,*,#56131,.F.);
#85171=ORIENTED_EDGE('',*,*,#58026,.F.);
#85172=ORIENTED_EDGE('',*,*,#52640,.F.);
#85173=ORIENTED_EDGE('',*,*,#52987,.F.);
#85174=ORIENTED_EDGE('',*,*,#52983,.T.);
#85175=ORIENTED_EDGE('',*,*,#58027,.F.);
#85176=ORIENTED_EDGE('',*,*,#56137,.F.);
#85177=ORIENTED_EDGE('',*,*,#58025,.T.);
#85178=ORIENTED_EDGE('',*,*,#58026,.T.);
#85179=ORIENTED_EDGE('',*,*,#56511,.F.);
#85180=ORIENTED_EDGE('',*,*,#58028,.F.);
#85181=ORIENTED_EDGE('',*,*,#52641,.F.);
#85182=ORIENTED_EDGE('',*,*,#58027,.T.);
#85183=ORIENTED_EDGE('',*,*,#52982,.F.);
#85184=ORIENTED_EDGE('',*,*,#58029,.F.);
#85185=ORIENTED_EDGE('',*,*,#56138,.F.);
#85186=ORIENTED_EDGE('',*,*,#58028,.T.);
#85187=ORIENTED_EDGE('',*,*,#56133,.F.);
#85188=ORIENTED_EDGE('',*,*,#58030,.F.);
#85189=ORIENTED_EDGE('',*,*,#52642,.F.);
#85190=ORIENTED_EDGE('',*,*,#58029,.T.);
#85191=ORIENTED_EDGE('',*,*,#52994,.F.);
#85192=ORIENTED_EDGE('',*,*,#58031,.F.);
#85193=ORIENTED_EDGE('',*,*,#56139,.F.);
#85194=ORIENTED_EDGE('',*,*,#58030,.T.);
#85195=ORIENTED_EDGE('',*,*,#56132,.F.);
#85196=ORIENTED_EDGE('',*,*,#58032,.F.);
#85197=ORIENTED_EDGE('',*,*,#52990,.F.);
#85198=ORIENTED_EDGE('',*,*,#58031,.T.);
#85199=ORIENTED_EDGE('',*,*,#52978,.F.);
#85200=ORIENTED_EDGE('',*,*,#58033,.F.);
#85201=ORIENTED_EDGE('',*,*,#56140,.F.);
#85202=ORIENTED_EDGE('',*,*,#58032,.T.);
#85203=ORIENTED_EDGE('',*,*,#56143,.F.);
#85204=ORIENTED_EDGE('',*,*,#58034,.F.);
#85205=ORIENTED_EDGE('',*,*,#52969,.F.);
#85206=ORIENTED_EDGE('',*,*,#58033,.T.);
#85207=ORIENTED_EDGE('',*,*,#52996,.F.);
#85208=ORIENTED_EDGE('',*,*,#58035,.F.);
#85209=ORIENTED_EDGE('',*,*,#56141,.F.);
#85210=ORIENTED_EDGE('',*,*,#58034,.T.);
#85211=ORIENTED_EDGE('',*,*,#56142,.F.);
#85212=ORIENTED_EDGE('',*,*,#58035,.T.);
#85213=ORIENTED_EDGE('',*,*,#52974,.F.);
#85214=ORIENTED_EDGE('',*,*,#52970,.T.);
#85215=ORIENTED_EDGE('',*,*,#58036,.F.);
#85216=ORIENTED_EDGE('',*,*,#56182,.F.);
#85217=ORIENTED_EDGE('',*,*,#58037,.F.);
#85218=ORIENTED_EDGE('',*,*,#52926,.F.);
#85219=ORIENTED_EDGE('',*,*,#58037,.T.);
#85220=ORIENTED_EDGE('',*,*,#56181,.F.);
#85221=ORIENTED_EDGE('',*,*,#58038,.F.);
#85222=ORIENTED_EDGE('',*,*,#52935,.F.);
#85223=ORIENTED_EDGE('',*,*,#52925,.T.);
#85224=ORIENTED_EDGE('',*,*,#52929,.F.);
#85225=ORIENTED_EDGE('',*,*,#58039,.F.);
#85226=ORIENTED_EDGE('',*,*,#56183,.F.);
#85227=ORIENTED_EDGE('',*,*,#58036,.T.);
#85228=ORIENTED_EDGE('',*,*,#58038,.T.);
#85229=ORIENTED_EDGE('',*,*,#56180,.F.);
#85230=ORIENTED_EDGE('',*,*,#58040,.F.);
#85231=ORIENTED_EDGE('',*,*,#52920,.F.);
#85232=ORIENTED_EDGE('',*,*,#58039,.T.);
#85233=ORIENTED_EDGE('',*,*,#52933,.F.);
#85234=ORIENTED_EDGE('',*,*,#58041,.F.);
#85235=ORIENTED_EDGE('',*,*,#56172,.F.);
#85236=ORIENTED_EDGE('',*,*,#58040,.T.);
#85237=ORIENTED_EDGE('',*,*,#56179,.F.);
#85238=ORIENTED_EDGE('',*,*,#58042,.F.);
#85239=ORIENTED_EDGE('',*,*,#52937,.F.);
#85240=ORIENTED_EDGE('',*,*,#58041,.T.);
#85241=ORIENTED_EDGE('',*,*,#52395,.F.);
#85242=ORIENTED_EDGE('',*,*,#58043,.F.);
#85243=ORIENTED_EDGE('',*,*,#56173,.F.);
#85244=ORIENTED_EDGE('',*,*,#58042,.T.);
#85245=ORIENTED_EDGE('',*,*,#56178,.F.);
#85246=ORIENTED_EDGE('',*,*,#58044,.F.);
#85247=ORIENTED_EDGE('',*,*,#52912,.T.);
#85248=ORIENTED_EDGE('',*,*,#52916,.F.);
#85249=ORIENTED_EDGE('',*,*,#58043,.T.);
#85250=ORIENTED_EDGE('',*,*,#52394,.F.);
#85251=ORIENTED_EDGE('',*,*,#58045,.F.);
#85252=ORIENTED_EDGE('',*,*,#56512,.F.);
#85253=ORIENTED_EDGE('',*,*,#58044,.T.);
#85254=ORIENTED_EDGE('',*,*,#56177,.F.);
#85255=ORIENTED_EDGE('',*,*,#58046,.F.);
#85256=ORIENTED_EDGE('',*,*,#52913,.F.);
#85257=ORIENTED_EDGE('',*,*,#58045,.T.);
#85258=ORIENTED_EDGE('',*,*,#52393,.F.);
#85259=ORIENTED_EDGE('',*,*,#58047,.F.);
#85260=ORIENTED_EDGE('',*,*,#56157,.F.);
#85261=ORIENTED_EDGE('',*,*,#58046,.T.);
#85262=ORIENTED_EDGE('',*,*,#56176,.F.);
#85263=ORIENTED_EDGE('',*,*,#58048,.F.);
#85264=ORIENTED_EDGE('',*,*,#52931,.F.);
#85265=ORIENTED_EDGE('',*,*,#58047,.T.);
#85266=ORIENTED_EDGE('',*,*,#52392,.F.);
#85267=ORIENTED_EDGE('',*,*,#58049,.F.);
#85268=ORIENTED_EDGE('',*,*,#56514,.F.);
#85269=ORIENTED_EDGE('',*,*,#58048,.T.);
#85270=ORIENTED_EDGE('',*,*,#56175,.F.);
#85271=ORIENTED_EDGE('',*,*,#58050,.F.);
#85272=ORIENTED_EDGE('',*,*,#52632,.F.);
#85273=ORIENTED_EDGE('',*,*,#58049,.T.);
#85274=ORIENTED_EDGE('',*,*,#52391,.F.);
#85275=ORIENTED_EDGE('',*,*,#58051,.F.);
#85276=ORIENTED_EDGE('',*,*,#56163,.F.);
#85277=ORIENTED_EDGE('',*,*,#58050,.T.);
#85278=ORIENTED_EDGE('',*,*,#56513,.F.);
#85279=ORIENTED_EDGE('',*,*,#58052,.F.);
#85280=ORIENTED_EDGE('',*,*,#52633,.F.);
#85281=ORIENTED_EDGE('',*,*,#58051,.T.);
#85282=ORIENTED_EDGE('',*,*,#52962,.F.);
#85283=ORIENTED_EDGE('',*,*,#58053,.F.);
#85284=ORIENTED_EDGE('',*,*,#56164,.F.);
#85285=ORIENTED_EDGE('',*,*,#58052,.T.);
#85286=ORIENTED_EDGE('',*,*,#56159,.F.);
#85287=ORIENTED_EDGE('',*,*,#58054,.F.);
#85288=ORIENTED_EDGE('',*,*,#52634,.F.);
#85289=ORIENTED_EDGE('',*,*,#52957,.F.);
#85290=ORIENTED_EDGE('',*,*,#52953,.T.);
#85291=ORIENTED_EDGE('',*,*,#58055,.F.);
#85292=ORIENTED_EDGE('',*,*,#56165,.F.);
#85293=ORIENTED_EDGE('',*,*,#58053,.T.);
#85294=ORIENTED_EDGE('',*,*,#58054,.T.);
#85295=ORIENTED_EDGE('',*,*,#56515,.F.);
#85296=ORIENTED_EDGE('',*,*,#58056,.F.);
#85297=ORIENTED_EDGE('',*,*,#52635,.F.);
#85298=ORIENTED_EDGE('',*,*,#58055,.T.);
#85299=ORIENTED_EDGE('',*,*,#52952,.F.);
#85300=ORIENTED_EDGE('',*,*,#58057,.F.);
#85301=ORIENTED_EDGE('',*,*,#56166,.F.);
#85302=ORIENTED_EDGE('',*,*,#58056,.T.);
#85303=ORIENTED_EDGE('',*,*,#56161,.F.);
#85304=ORIENTED_EDGE('',*,*,#58058,.F.);
#85305=ORIENTED_EDGE('',*,*,#52636,.F.);
#85306=ORIENTED_EDGE('',*,*,#58057,.T.);
#85307=ORIENTED_EDGE('',*,*,#52964,.F.);
#85308=ORIENTED_EDGE('',*,*,#58059,.F.);
#85309=ORIENTED_EDGE('',*,*,#56167,.F.);
#85310=ORIENTED_EDGE('',*,*,#58058,.T.);
#85311=ORIENTED_EDGE('',*,*,#56160,.F.);
#85312=ORIENTED_EDGE('',*,*,#58060,.F.);
#85313=ORIENTED_EDGE('',*,*,#52960,.F.);
#85314=ORIENTED_EDGE('',*,*,#58059,.T.);
#85315=ORIENTED_EDGE('',*,*,#52948,.F.);
#85316=ORIENTED_EDGE('',*,*,#58061,.F.);
#85317=ORIENTED_EDGE('',*,*,#56168,.F.);
#85318=ORIENTED_EDGE('',*,*,#58060,.T.);
#85319=ORIENTED_EDGE('',*,*,#56171,.F.);
#85320=ORIENTED_EDGE('',*,*,#58062,.F.);
#85321=ORIENTED_EDGE('',*,*,#52939,.F.);
#85322=ORIENTED_EDGE('',*,*,#58061,.T.);
#85323=ORIENTED_EDGE('',*,*,#52966,.F.);
#85324=ORIENTED_EDGE('',*,*,#58063,.F.);
#85325=ORIENTED_EDGE('',*,*,#56169,.F.);
#85326=ORIENTED_EDGE('',*,*,#58062,.T.);
#85327=ORIENTED_EDGE('',*,*,#56170,.F.);
#85328=ORIENTED_EDGE('',*,*,#58063,.T.);
#85329=ORIENTED_EDGE('',*,*,#52944,.F.);
#85330=ORIENTED_EDGE('',*,*,#52940,.T.);
#85331=ORIENTED_EDGE('',*,*,#58064,.F.);
#85332=ORIENTED_EDGE('',*,*,#56210,.F.);
#85333=ORIENTED_EDGE('',*,*,#58065,.F.);
#85334=ORIENTED_EDGE('',*,*,#52896,.F.);
#85335=ORIENTED_EDGE('',*,*,#58065,.T.);
#85336=ORIENTED_EDGE('',*,*,#56209,.F.);
#85337=ORIENTED_EDGE('',*,*,#58066,.F.);
#85338=ORIENTED_EDGE('',*,*,#52905,.F.);
#85339=ORIENTED_EDGE('',*,*,#52895,.T.);
#85340=ORIENTED_EDGE('',*,*,#52899,.F.);
#85341=ORIENTED_EDGE('',*,*,#58067,.F.);
#85342=ORIENTED_EDGE('',*,*,#56211,.F.);
#85343=ORIENTED_EDGE('',*,*,#58064,.T.);
#85344=ORIENTED_EDGE('',*,*,#58066,.T.);
#85345=ORIENTED_EDGE('',*,*,#56208,.F.);
#85346=ORIENTED_EDGE('',*,*,#58068,.F.);
#85347=ORIENTED_EDGE('',*,*,#52890,.F.);
#85348=ORIENTED_EDGE('',*,*,#58067,.T.);
#85349=ORIENTED_EDGE('',*,*,#52903,.F.);
#85350=ORIENTED_EDGE('',*,*,#58069,.F.);
#85351=ORIENTED_EDGE('',*,*,#56200,.F.);
#85352=ORIENTED_EDGE('',*,*,#58068,.T.);
#85353=ORIENTED_EDGE('',*,*,#56207,.F.);
#85354=ORIENTED_EDGE('',*,*,#58070,.F.);
#85355=ORIENTED_EDGE('',*,*,#52907,.F.);
#85356=ORIENTED_EDGE('',*,*,#58069,.T.);
#85357=ORIENTED_EDGE('',*,*,#52401,.F.);
#85358=ORIENTED_EDGE('',*,*,#58071,.F.);
#85359=ORIENTED_EDGE('',*,*,#56201,.F.);
#85360=ORIENTED_EDGE('',*,*,#58070,.T.);
#85361=ORIENTED_EDGE('',*,*,#56206,.F.);
#85362=ORIENTED_EDGE('',*,*,#58072,.F.);
#85363=ORIENTED_EDGE('',*,*,#52882,.T.);
#85364=ORIENTED_EDGE('',*,*,#52886,.F.);
#85365=ORIENTED_EDGE('',*,*,#58071,.T.);
#85366=ORIENTED_EDGE('',*,*,#52400,.F.);
#85367=ORIENTED_EDGE('',*,*,#58073,.F.);
#85368=ORIENTED_EDGE('',*,*,#56516,.F.);
#85369=ORIENTED_EDGE('',*,*,#58072,.T.);
#85370=ORIENTED_EDGE('',*,*,#56205,.F.);
#85371=ORIENTED_EDGE('',*,*,#58074,.F.);
#85372=ORIENTED_EDGE('',*,*,#52883,.F.);
#85373=ORIENTED_EDGE('',*,*,#58073,.T.);
#85374=ORIENTED_EDGE('',*,*,#52399,.F.);
#85375=ORIENTED_EDGE('',*,*,#58075,.F.);
#85376=ORIENTED_EDGE('',*,*,#56185,.F.);
#85377=ORIENTED_EDGE('',*,*,#58074,.T.);
#85378=ORIENTED_EDGE('',*,*,#56204,.F.);
#85379=ORIENTED_EDGE('',*,*,#58076,.F.);
#85380=ORIENTED_EDGE('',*,*,#52901,.F.);
#85381=ORIENTED_EDGE('',*,*,#58075,.T.);
#85382=ORIENTED_EDGE('',*,*,#52398,.F.);
#85383=ORIENTED_EDGE('',*,*,#58077,.F.);
#85384=ORIENTED_EDGE('',*,*,#56518,.F.);
#85385=ORIENTED_EDGE('',*,*,#58076,.T.);
#85386=ORIENTED_EDGE('',*,*,#56203,.F.);
#85387=ORIENTED_EDGE('',*,*,#58078,.F.);
#85388=ORIENTED_EDGE('',*,*,#52626,.F.);
#85389=ORIENTED_EDGE('',*,*,#58077,.T.);
#85390=ORIENTED_EDGE('',*,*,#52397,.F.);
#85391=ORIENTED_EDGE('',*,*,#58079,.F.);
#85392=ORIENTED_EDGE('',*,*,#56191,.F.);
#85393=ORIENTED_EDGE('',*,*,#58078,.T.);
#85394=ORIENTED_EDGE('',*,*,#56517,.F.);
#85395=ORIENTED_EDGE('',*,*,#58080,.F.);
#85396=ORIENTED_EDGE('',*,*,#52627,.F.);
#85397=ORIENTED_EDGE('',*,*,#58079,.T.);
#85398=ORIENTED_EDGE('',*,*,#52932,.F.);
#85399=ORIENTED_EDGE('',*,*,#58081,.F.);
#85400=ORIENTED_EDGE('',*,*,#56192,.F.);
#85401=ORIENTED_EDGE('',*,*,#58080,.T.);
#85402=ORIENTED_EDGE('',*,*,#56187,.F.);
#85403=ORIENTED_EDGE('',*,*,#58082,.F.);
#85404=ORIENTED_EDGE('',*,*,#52628,.F.);
#85405=ORIENTED_EDGE('',*,*,#52927,.F.);
#85406=ORIENTED_EDGE('',*,*,#52923,.T.);
#85407=ORIENTED_EDGE('',*,*,#58083,.F.);
#85408=ORIENTED_EDGE('',*,*,#56193,.F.);
#85409=ORIENTED_EDGE('',*,*,#58081,.T.);
#85410=ORIENTED_EDGE('',*,*,#58082,.T.);
#85411=ORIENTED_EDGE('',*,*,#56519,.F.);
#85412=ORIENTED_EDGE('',*,*,#58084,.F.);
#85413=ORIENTED_EDGE('',*,*,#52629,.F.);
#85414=ORIENTED_EDGE('',*,*,#58083,.T.);
#85415=ORIENTED_EDGE('',*,*,#52922,.F.);
#85416=ORIENTED_EDGE('',*,*,#58085,.F.);
#85417=ORIENTED_EDGE('',*,*,#56194,.F.);
#85418=ORIENTED_EDGE('',*,*,#58084,.T.);
#85419=ORIENTED_EDGE('',*,*,#56189,.F.);
#85420=ORIENTED_EDGE('',*,*,#58086,.F.);
#85421=ORIENTED_EDGE('',*,*,#52630,.F.);
#85422=ORIENTED_EDGE('',*,*,#58085,.T.);
#85423=ORIENTED_EDGE('',*,*,#52934,.F.);
#85424=ORIENTED_EDGE('',*,*,#58087,.F.);
#85425=ORIENTED_EDGE('',*,*,#56195,.F.);
#85426=ORIENTED_EDGE('',*,*,#58086,.T.);
#85427=ORIENTED_EDGE('',*,*,#56188,.F.);
#85428=ORIENTED_EDGE('',*,*,#58088,.F.);
#85429=ORIENTED_EDGE('',*,*,#52930,.F.);
#85430=ORIENTED_EDGE('',*,*,#58087,.T.);
#85431=ORIENTED_EDGE('',*,*,#52918,.F.);
#85432=ORIENTED_EDGE('',*,*,#58089,.F.);
#85433=ORIENTED_EDGE('',*,*,#56196,.F.);
#85434=ORIENTED_EDGE('',*,*,#58088,.T.);
#85435=ORIENTED_EDGE('',*,*,#56199,.F.);
#85436=ORIENTED_EDGE('',*,*,#58090,.F.);
#85437=ORIENTED_EDGE('',*,*,#52909,.F.);
#85438=ORIENTED_EDGE('',*,*,#58089,.T.);
#85439=ORIENTED_EDGE('',*,*,#52936,.F.);
#85440=ORIENTED_EDGE('',*,*,#58091,.F.);
#85441=ORIENTED_EDGE('',*,*,#56197,.F.);
#85442=ORIENTED_EDGE('',*,*,#58090,.T.);
#85443=ORIENTED_EDGE('',*,*,#56198,.F.);
#85444=ORIENTED_EDGE('',*,*,#58091,.T.);
#85445=ORIENTED_EDGE('',*,*,#52914,.F.);
#85446=ORIENTED_EDGE('',*,*,#52910,.T.);
#85447=ORIENTED_EDGE('',*,*,#58092,.F.);
#85448=ORIENTED_EDGE('',*,*,#56238,.F.);
#85449=ORIENTED_EDGE('',*,*,#58093,.F.);
#85450=ORIENTED_EDGE('',*,*,#52866,.F.);
#85451=ORIENTED_EDGE('',*,*,#58093,.T.);
#85452=ORIENTED_EDGE('',*,*,#56237,.F.);
#85453=ORIENTED_EDGE('',*,*,#58094,.F.);
#85454=ORIENTED_EDGE('',*,*,#52875,.F.);
#85455=ORIENTED_EDGE('',*,*,#52865,.T.);
#85456=ORIENTED_EDGE('',*,*,#52869,.F.);
#85457=ORIENTED_EDGE('',*,*,#58095,.F.);
#85458=ORIENTED_EDGE('',*,*,#56239,.F.);
#85459=ORIENTED_EDGE('',*,*,#58092,.T.);
#85460=ORIENTED_EDGE('',*,*,#58094,.T.);
#85461=ORIENTED_EDGE('',*,*,#56236,.F.);
#85462=ORIENTED_EDGE('',*,*,#58096,.F.);
#85463=ORIENTED_EDGE('',*,*,#52860,.F.);
#85464=ORIENTED_EDGE('',*,*,#58095,.T.);
#85465=ORIENTED_EDGE('',*,*,#52873,.F.);
#85466=ORIENTED_EDGE('',*,*,#58097,.F.);
#85467=ORIENTED_EDGE('',*,*,#56228,.F.);
#85468=ORIENTED_EDGE('',*,*,#58096,.T.);
#85469=ORIENTED_EDGE('',*,*,#56235,.F.);
#85470=ORIENTED_EDGE('',*,*,#58098,.F.);
#85471=ORIENTED_EDGE('',*,*,#52877,.F.);
#85472=ORIENTED_EDGE('',*,*,#58097,.T.);
#85473=ORIENTED_EDGE('',*,*,#52407,.F.);
#85474=ORIENTED_EDGE('',*,*,#58099,.F.);
#85475=ORIENTED_EDGE('',*,*,#56229,.F.);
#85476=ORIENTED_EDGE('',*,*,#58098,.T.);
#85477=ORIENTED_EDGE('',*,*,#56234,.F.);
#85478=ORIENTED_EDGE('',*,*,#58100,.F.);
#85479=ORIENTED_EDGE('',*,*,#52852,.T.);
#85480=ORIENTED_EDGE('',*,*,#52856,.F.);
#85481=ORIENTED_EDGE('',*,*,#58099,.T.);
#85482=ORIENTED_EDGE('',*,*,#52406,.F.);
#85483=ORIENTED_EDGE('',*,*,#58101,.F.);
#85484=ORIENTED_EDGE('',*,*,#56520,.F.);
#85485=ORIENTED_EDGE('',*,*,#58100,.T.);
#85486=ORIENTED_EDGE('',*,*,#56233,.F.);
#85487=ORIENTED_EDGE('',*,*,#58102,.F.);
#85488=ORIENTED_EDGE('',*,*,#52853,.F.);
#85489=ORIENTED_EDGE('',*,*,#58101,.T.);
#85490=ORIENTED_EDGE('',*,*,#52405,.F.);
#85491=ORIENTED_EDGE('',*,*,#58103,.F.);
#85492=ORIENTED_EDGE('',*,*,#56213,.F.);
#85493=ORIENTED_EDGE('',*,*,#58102,.T.);
#85494=ORIENTED_EDGE('',*,*,#56232,.F.);
#85495=ORIENTED_EDGE('',*,*,#58104,.F.);
#85496=ORIENTED_EDGE('',*,*,#52871,.F.);
#85497=ORIENTED_EDGE('',*,*,#58103,.T.);
#85498=ORIENTED_EDGE('',*,*,#52404,.F.);
#85499=ORIENTED_EDGE('',*,*,#58105,.F.);
#85500=ORIENTED_EDGE('',*,*,#56522,.F.);
#85501=ORIENTED_EDGE('',*,*,#58104,.T.);
#85502=ORIENTED_EDGE('',*,*,#56231,.F.);
#85503=ORIENTED_EDGE('',*,*,#58106,.F.);
#85504=ORIENTED_EDGE('',*,*,#52620,.F.);
#85505=ORIENTED_EDGE('',*,*,#58105,.T.);
#85506=ORIENTED_EDGE('',*,*,#52403,.F.);
#85507=ORIENTED_EDGE('',*,*,#58107,.F.);
#85508=ORIENTED_EDGE('',*,*,#56219,.F.);
#85509=ORIENTED_EDGE('',*,*,#58106,.T.);
#85510=ORIENTED_EDGE('',*,*,#56521,.F.);
#85511=ORIENTED_EDGE('',*,*,#58108,.F.);
#85512=ORIENTED_EDGE('',*,*,#52621,.F.);
#85513=ORIENTED_EDGE('',*,*,#58107,.T.);
#85514=ORIENTED_EDGE('',*,*,#52902,.F.);
#85515=ORIENTED_EDGE('',*,*,#58109,.F.);
#85516=ORIENTED_EDGE('',*,*,#56220,.F.);
#85517=ORIENTED_EDGE('',*,*,#58108,.T.);
#85518=ORIENTED_EDGE('',*,*,#56215,.F.);
#85519=ORIENTED_EDGE('',*,*,#58110,.F.);
#85520=ORIENTED_EDGE('',*,*,#52622,.F.);
#85521=ORIENTED_EDGE('',*,*,#52897,.F.);
#85522=ORIENTED_EDGE('',*,*,#52893,.T.);
#85523=ORIENTED_EDGE('',*,*,#58111,.F.);
#85524=ORIENTED_EDGE('',*,*,#56221,.F.);
#85525=ORIENTED_EDGE('',*,*,#58109,.T.);
#85526=ORIENTED_EDGE('',*,*,#58110,.T.);
#85527=ORIENTED_EDGE('',*,*,#56523,.F.);
#85528=ORIENTED_EDGE('',*,*,#58112,.F.);
#85529=ORIENTED_EDGE('',*,*,#52623,.F.);
#85530=ORIENTED_EDGE('',*,*,#58111,.T.);
#85531=ORIENTED_EDGE('',*,*,#52892,.F.);
#85532=ORIENTED_EDGE('',*,*,#58113,.F.);
#85533=ORIENTED_EDGE('',*,*,#56222,.F.);
#85534=ORIENTED_EDGE('',*,*,#58112,.T.);
#85535=ORIENTED_EDGE('',*,*,#56217,.F.);
#85536=ORIENTED_EDGE('',*,*,#58114,.F.);
#85537=ORIENTED_EDGE('',*,*,#52624,.F.);
#85538=ORIENTED_EDGE('',*,*,#58113,.T.);
#85539=ORIENTED_EDGE('',*,*,#52904,.F.);
#85540=ORIENTED_EDGE('',*,*,#58115,.F.);
#85541=ORIENTED_EDGE('',*,*,#56223,.F.);
#85542=ORIENTED_EDGE('',*,*,#58114,.T.);
#85543=ORIENTED_EDGE('',*,*,#56216,.F.);
#85544=ORIENTED_EDGE('',*,*,#58116,.F.);
#85545=ORIENTED_EDGE('',*,*,#52900,.F.);
#85546=ORIENTED_EDGE('',*,*,#58115,.T.);
#85547=ORIENTED_EDGE('',*,*,#52888,.F.);
#85548=ORIENTED_EDGE('',*,*,#58117,.F.);
#85549=ORIENTED_EDGE('',*,*,#56224,.F.);
#85550=ORIENTED_EDGE('',*,*,#58116,.T.);
#85551=ORIENTED_EDGE('',*,*,#56227,.F.);
#85552=ORIENTED_EDGE('',*,*,#58118,.F.);
#85553=ORIENTED_EDGE('',*,*,#52879,.F.);
#85554=ORIENTED_EDGE('',*,*,#58117,.T.);
#85555=ORIENTED_EDGE('',*,*,#52906,.F.);
#85556=ORIENTED_EDGE('',*,*,#58119,.F.);
#85557=ORIENTED_EDGE('',*,*,#56225,.F.);
#85558=ORIENTED_EDGE('',*,*,#58118,.T.);
#85559=ORIENTED_EDGE('',*,*,#56226,.F.);
#85560=ORIENTED_EDGE('',*,*,#58119,.T.);
#85561=ORIENTED_EDGE('',*,*,#52884,.F.);
#85562=ORIENTED_EDGE('',*,*,#52880,.T.);
#85563=ORIENTED_EDGE('',*,*,#58120,.F.);
#85564=ORIENTED_EDGE('',*,*,#56266,.F.);
#85565=ORIENTED_EDGE('',*,*,#58121,.F.);
#85566=ORIENTED_EDGE('',*,*,#52836,.F.);
#85567=ORIENTED_EDGE('',*,*,#58121,.T.);
#85568=ORIENTED_EDGE('',*,*,#56265,.F.);
#85569=ORIENTED_EDGE('',*,*,#58122,.F.);
#85570=ORIENTED_EDGE('',*,*,#52845,.F.);
#85571=ORIENTED_EDGE('',*,*,#52835,.T.);
#85572=ORIENTED_EDGE('',*,*,#52839,.F.);
#85573=ORIENTED_EDGE('',*,*,#58123,.F.);
#85574=ORIENTED_EDGE('',*,*,#56267,.F.);
#85575=ORIENTED_EDGE('',*,*,#58120,.T.);
#85576=ORIENTED_EDGE('',*,*,#58122,.T.);
#85577=ORIENTED_EDGE('',*,*,#56264,.F.);
#85578=ORIENTED_EDGE('',*,*,#58124,.F.);
#85579=ORIENTED_EDGE('',*,*,#52830,.F.);
#85580=ORIENTED_EDGE('',*,*,#58123,.T.);
#85581=ORIENTED_EDGE('',*,*,#52843,.F.);
#85582=ORIENTED_EDGE('',*,*,#58125,.F.);
#85583=ORIENTED_EDGE('',*,*,#56256,.F.);
#85584=ORIENTED_EDGE('',*,*,#58124,.T.);
#85585=ORIENTED_EDGE('',*,*,#56263,.F.);
#85586=ORIENTED_EDGE('',*,*,#58126,.F.);
#85587=ORIENTED_EDGE('',*,*,#52847,.F.);
#85588=ORIENTED_EDGE('',*,*,#58125,.T.);
#85589=ORIENTED_EDGE('',*,*,#52413,.F.);
#85590=ORIENTED_EDGE('',*,*,#58127,.F.);
#85591=ORIENTED_EDGE('',*,*,#56257,.F.);
#85592=ORIENTED_EDGE('',*,*,#58126,.T.);
#85593=ORIENTED_EDGE('',*,*,#56262,.F.);
#85594=ORIENTED_EDGE('',*,*,#58128,.F.);
#85595=ORIENTED_EDGE('',*,*,#52822,.T.);
#85596=ORIENTED_EDGE('',*,*,#52826,.F.);
#85597=ORIENTED_EDGE('',*,*,#58127,.T.);
#85598=ORIENTED_EDGE('',*,*,#52412,.F.);
#85599=ORIENTED_EDGE('',*,*,#58129,.F.);
#85600=ORIENTED_EDGE('',*,*,#56524,.F.);
#85601=ORIENTED_EDGE('',*,*,#58128,.T.);
#85602=ORIENTED_EDGE('',*,*,#56261,.F.);
#85603=ORIENTED_EDGE('',*,*,#58130,.F.);
#85604=ORIENTED_EDGE('',*,*,#52823,.F.);
#85605=ORIENTED_EDGE('',*,*,#58129,.T.);
#85606=ORIENTED_EDGE('',*,*,#52411,.F.);
#85607=ORIENTED_EDGE('',*,*,#58131,.F.);
#85608=ORIENTED_EDGE('',*,*,#56241,.F.);
#85609=ORIENTED_EDGE('',*,*,#58130,.T.);
#85610=ORIENTED_EDGE('',*,*,#56260,.F.);
#85611=ORIENTED_EDGE('',*,*,#58132,.F.);
#85612=ORIENTED_EDGE('',*,*,#52841,.F.);
#85613=ORIENTED_EDGE('',*,*,#58131,.T.);
#85614=ORIENTED_EDGE('',*,*,#52410,.F.);
#85615=ORIENTED_EDGE('',*,*,#58133,.F.);
#85616=ORIENTED_EDGE('',*,*,#56526,.F.);
#85617=ORIENTED_EDGE('',*,*,#58132,.T.);
#85618=ORIENTED_EDGE('',*,*,#56259,.F.);
#85619=ORIENTED_EDGE('',*,*,#58134,.F.);
#85620=ORIENTED_EDGE('',*,*,#52614,.F.);
#85621=ORIENTED_EDGE('',*,*,#58133,.T.);
#85622=ORIENTED_EDGE('',*,*,#52409,.F.);
#85623=ORIENTED_EDGE('',*,*,#58135,.F.);
#85624=ORIENTED_EDGE('',*,*,#56247,.F.);
#85625=ORIENTED_EDGE('',*,*,#58134,.T.);
#85626=ORIENTED_EDGE('',*,*,#56525,.F.);
#85627=ORIENTED_EDGE('',*,*,#58136,.F.);
#85628=ORIENTED_EDGE('',*,*,#52615,.F.);
#85629=ORIENTED_EDGE('',*,*,#58135,.T.);
#85630=ORIENTED_EDGE('',*,*,#52872,.F.);
#85631=ORIENTED_EDGE('',*,*,#58137,.F.);
#85632=ORIENTED_EDGE('',*,*,#56248,.F.);
#85633=ORIENTED_EDGE('',*,*,#58136,.T.);
#85634=ORIENTED_EDGE('',*,*,#56243,.F.);
#85635=ORIENTED_EDGE('',*,*,#58138,.F.);
#85636=ORIENTED_EDGE('',*,*,#52616,.F.);
#85637=ORIENTED_EDGE('',*,*,#52867,.F.);
#85638=ORIENTED_EDGE('',*,*,#52863,.T.);
#85639=ORIENTED_EDGE('',*,*,#58139,.F.);
#85640=ORIENTED_EDGE('',*,*,#56249,.F.);
#85641=ORIENTED_EDGE('',*,*,#58137,.T.);
#85642=ORIENTED_EDGE('',*,*,#58138,.T.);
#85643=ORIENTED_EDGE('',*,*,#56527,.F.);
#85644=ORIENTED_EDGE('',*,*,#58140,.F.);
#85645=ORIENTED_EDGE('',*,*,#52617,.F.);
#85646=ORIENTED_EDGE('',*,*,#58139,.T.);
#85647=ORIENTED_EDGE('',*,*,#52862,.F.);
#85648=ORIENTED_EDGE('',*,*,#58141,.F.);
#85649=ORIENTED_EDGE('',*,*,#56250,.F.);
#85650=ORIENTED_EDGE('',*,*,#58140,.T.);
#85651=ORIENTED_EDGE('',*,*,#56245,.F.);
#85652=ORIENTED_EDGE('',*,*,#58142,.F.);
#85653=ORIENTED_EDGE('',*,*,#52618,.F.);
#85654=ORIENTED_EDGE('',*,*,#58141,.T.);
#85655=ORIENTED_EDGE('',*,*,#52874,.F.);
#85656=ORIENTED_EDGE('',*,*,#58143,.F.);
#85657=ORIENTED_EDGE('',*,*,#56251,.F.);
#85658=ORIENTED_EDGE('',*,*,#58142,.T.);
#85659=ORIENTED_EDGE('',*,*,#56244,.F.);
#85660=ORIENTED_EDGE('',*,*,#58144,.F.);
#85661=ORIENTED_EDGE('',*,*,#52870,.F.);
#85662=ORIENTED_EDGE('',*,*,#58143,.T.);
#85663=ORIENTED_EDGE('',*,*,#52858,.F.);
#85664=ORIENTED_EDGE('',*,*,#58145,.F.);
#85665=ORIENTED_EDGE('',*,*,#56252,.F.);
#85666=ORIENTED_EDGE('',*,*,#58144,.T.);
#85667=ORIENTED_EDGE('',*,*,#56255,.F.);
#85668=ORIENTED_EDGE('',*,*,#58146,.F.);
#85669=ORIENTED_EDGE('',*,*,#52849,.F.);
#85670=ORIENTED_EDGE('',*,*,#58145,.T.);
#85671=ORIENTED_EDGE('',*,*,#52876,.F.);
#85672=ORIENTED_EDGE('',*,*,#58147,.F.);
#85673=ORIENTED_EDGE('',*,*,#56253,.F.);
#85674=ORIENTED_EDGE('',*,*,#58146,.T.);
#85675=ORIENTED_EDGE('',*,*,#56254,.F.);
#85676=ORIENTED_EDGE('',*,*,#58147,.T.);
#85677=ORIENTED_EDGE('',*,*,#52854,.F.);
#85678=ORIENTED_EDGE('',*,*,#52850,.T.);
#85679=ORIENTED_EDGE('',*,*,#58148,.F.);
#85680=ORIENTED_EDGE('',*,*,#56294,.F.);
#85681=ORIENTED_EDGE('',*,*,#58149,.F.);
#85682=ORIENTED_EDGE('',*,*,#52802,.F.);
#85683=ORIENTED_EDGE('',*,*,#58149,.T.);
#85684=ORIENTED_EDGE('',*,*,#56293,.F.);
#85685=ORIENTED_EDGE('',*,*,#58150,.F.);
#85686=ORIENTED_EDGE('',*,*,#52814,.F.);
#85687=ORIENTED_EDGE('',*,*,#52801,.T.);
#85688=ORIENTED_EDGE('',*,*,#52808,.F.);
#85689=ORIENTED_EDGE('',*,*,#58151,.F.);
#85690=ORIENTED_EDGE('',*,*,#56295,.F.);
#85691=ORIENTED_EDGE('',*,*,#58148,.T.);
#85692=ORIENTED_EDGE('',*,*,#58150,.T.);
#85693=ORIENTED_EDGE('',*,*,#56292,.F.);
#85694=ORIENTED_EDGE('',*,*,#58152,.F.);
#85695=ORIENTED_EDGE('',*,*,#52798,.F.);
#85696=ORIENTED_EDGE('',*,*,#58151,.T.);
#85697=ORIENTED_EDGE('',*,*,#52812,.F.);
#85698=ORIENTED_EDGE('',*,*,#58153,.F.);
#85699=ORIENTED_EDGE('',*,*,#56284,.F.);
#85700=ORIENTED_EDGE('',*,*,#58152,.T.);
#85701=ORIENTED_EDGE('',*,*,#56291,.F.);
#85702=ORIENTED_EDGE('',*,*,#58154,.F.);
#85703=ORIENTED_EDGE('',*,*,#52816,.F.);
#85704=ORIENTED_EDGE('',*,*,#58153,.T.);
#85705=ORIENTED_EDGE('',*,*,#52419,.F.);
#85706=ORIENTED_EDGE('',*,*,#58155,.F.);
#85707=ORIENTED_EDGE('',*,*,#56285,.F.);
#85708=ORIENTED_EDGE('',*,*,#58154,.T.);
#85709=ORIENTED_EDGE('',*,*,#56290,.F.);
#85710=ORIENTED_EDGE('',*,*,#58156,.F.);
#85711=ORIENTED_EDGE('',*,*,#52788,.T.);
#85712=ORIENTED_EDGE('',*,*,#52795,.F.);
#85713=ORIENTED_EDGE('',*,*,#58155,.T.);
#85714=ORIENTED_EDGE('',*,*,#52418,.F.);
#85715=ORIENTED_EDGE('',*,*,#58157,.F.);
#85716=ORIENTED_EDGE('',*,*,#56528,.F.);
#85717=ORIENTED_EDGE('',*,*,#58156,.T.);
#85718=ORIENTED_EDGE('',*,*,#56289,.F.);
#85719=ORIENTED_EDGE('',*,*,#58158,.F.);
#85720=ORIENTED_EDGE('',*,*,#52789,.F.);
#85721=ORIENTED_EDGE('',*,*,#58157,.T.);
#85722=ORIENTED_EDGE('',*,*,#52417,.F.);
#85723=ORIENTED_EDGE('',*,*,#58159,.F.);
#85724=ORIENTED_EDGE('',*,*,#56269,.F.);
#85725=ORIENTED_EDGE('',*,*,#58158,.T.);
#85726=ORIENTED_EDGE('',*,*,#56288,.F.);
#85727=ORIENTED_EDGE('',*,*,#58160,.F.);
#85728=ORIENTED_EDGE('',*,*,#52810,.F.);
#85729=ORIENTED_EDGE('',*,*,#58159,.T.);
#85730=ORIENTED_EDGE('',*,*,#52416,.F.);
#85731=ORIENTED_EDGE('',*,*,#58161,.F.);
#85732=ORIENTED_EDGE('',*,*,#56530,.F.);
#85733=ORIENTED_EDGE('',*,*,#58160,.T.);
#85734=ORIENTED_EDGE('',*,*,#56287,.F.);
#85735=ORIENTED_EDGE('',*,*,#58162,.F.);
#85736=ORIENTED_EDGE('',*,*,#52608,.F.);
#85737=ORIENTED_EDGE('',*,*,#58161,.T.);
#85738=ORIENTED_EDGE('',*,*,#52415,.F.);
#85739=ORIENTED_EDGE('',*,*,#58163,.F.);
#85740=ORIENTED_EDGE('',*,*,#56275,.F.);
#85741=ORIENTED_EDGE('',*,*,#58162,.T.);
#85742=ORIENTED_EDGE('',*,*,#56529,.F.);
#85743=ORIENTED_EDGE('',*,*,#58164,.F.);
#85744=ORIENTED_EDGE('',*,*,#52609,.F.);
#85745=ORIENTED_EDGE('',*,*,#58163,.T.);
#85746=ORIENTED_EDGE('',*,*,#52842,.F.);
#85747=ORIENTED_EDGE('',*,*,#58165,.F.);
#85748=ORIENTED_EDGE('',*,*,#56276,.F.);
#85749=ORIENTED_EDGE('',*,*,#58164,.T.);
#85750=ORIENTED_EDGE('',*,*,#56271,.F.);
#85751=ORIENTED_EDGE('',*,*,#58166,.F.);
#85752=ORIENTED_EDGE('',*,*,#52610,.F.);
#85753=ORIENTED_EDGE('',*,*,#52837,.F.);
#85754=ORIENTED_EDGE('',*,*,#52833,.T.);
#85755=ORIENTED_EDGE('',*,*,#58167,.F.);
#85756=ORIENTED_EDGE('',*,*,#56277,.F.);
#85757=ORIENTED_EDGE('',*,*,#58165,.T.);
#85758=ORIENTED_EDGE('',*,*,#58166,.T.);
#85759=ORIENTED_EDGE('',*,*,#56531,.F.);
#85760=ORIENTED_EDGE('',*,*,#58168,.F.);
#85761=ORIENTED_EDGE('',*,*,#52611,.F.);
#85762=ORIENTED_EDGE('',*,*,#58167,.T.);
#85763=ORIENTED_EDGE('',*,*,#52832,.F.);
#85764=ORIENTED_EDGE('',*,*,#58169,.F.);
#85765=ORIENTED_EDGE('',*,*,#56278,.F.);
#85766=ORIENTED_EDGE('',*,*,#58168,.T.);
#85767=ORIENTED_EDGE('',*,*,#56273,.F.);
#85768=ORIENTED_EDGE('',*,*,#58170,.F.);
#85769=ORIENTED_EDGE('',*,*,#52612,.F.);
#85770=ORIENTED_EDGE('',*,*,#58169,.T.);
#85771=ORIENTED_EDGE('',*,*,#52844,.F.);
#85772=ORIENTED_EDGE('',*,*,#58171,.F.);
#85773=ORIENTED_EDGE('',*,*,#56279,.F.);
#85774=ORIENTED_EDGE('',*,*,#58170,.T.);
#85775=ORIENTED_EDGE('',*,*,#56272,.F.);
#85776=ORIENTED_EDGE('',*,*,#58172,.F.);
#85777=ORIENTED_EDGE('',*,*,#52840,.F.);
#85778=ORIENTED_EDGE('',*,*,#58171,.T.);
#85779=ORIENTED_EDGE('',*,*,#52828,.F.);
#85780=ORIENTED_EDGE('',*,*,#58173,.F.);
#85781=ORIENTED_EDGE('',*,*,#56280,.F.);
#85782=ORIENTED_EDGE('',*,*,#58172,.T.);
#85783=ORIENTED_EDGE('',*,*,#56283,.F.);
#85784=ORIENTED_EDGE('',*,*,#58174,.F.);
#85785=ORIENTED_EDGE('',*,*,#52819,.F.);
#85786=ORIENTED_EDGE('',*,*,#58173,.T.);
#85787=ORIENTED_EDGE('',*,*,#52846,.F.);
#85788=ORIENTED_EDGE('',*,*,#58175,.F.);
#85789=ORIENTED_EDGE('',*,*,#56281,.F.);
#85790=ORIENTED_EDGE('',*,*,#58174,.T.);
#85791=ORIENTED_EDGE('',*,*,#56282,.F.);
#85792=ORIENTED_EDGE('',*,*,#58175,.T.);
#85793=ORIENTED_EDGE('',*,*,#52824,.F.);
#85794=ORIENTED_EDGE('',*,*,#52820,.T.);
#85795=ORIENTED_EDGE('',*,*,#58176,.F.);
#85796=ORIENTED_EDGE('',*,*,#58177,.T.);
#85797=ORIENTED_EDGE('',*,*,#58178,.F.);
#85798=ORIENTED_EDGE('',*,*,#58177,.F.);
#85799=ORIENTED_EDGE('',*,*,#58179,.F.);
#85800=ORIENTED_EDGE('',*,*,#58180,.T.);
#85801=ORIENTED_EDGE('',*,*,#58181,.F.);
#85802=ORIENTED_EDGE('',*,*,#58180,.F.);
#85803=ORIENTED_EDGE('',*,*,#58182,.F.);
#85804=ORIENTED_EDGE('',*,*,#58183,.T.);
#85805=ORIENTED_EDGE('',*,*,#58184,.F.);
#85806=ORIENTED_EDGE('',*,*,#58185,.F.);
#85807=ORIENTED_EDGE('',*,*,#58183,.F.);
#85808=ORIENTED_EDGE('',*,*,#58186,.F.);
#85809=ORIENTED_EDGE('',*,*,#58187,.T.);
#85810=ORIENTED_EDGE('',*,*,#58176,.T.);
#85811=ORIENTED_EDGE('',*,*,#58187,.F.);
#85812=ORIENTED_EDGE('',*,*,#58181,.T.);
#85813=ORIENTED_EDGE('',*,*,#58188,.T.);
#85814=ORIENTED_EDGE('',*,*,#58184,.T.);
#85815=ORIENTED_EDGE('',*,*,#58185,.T.);
#85816=ORIENTED_EDGE('',*,*,#58188,.F.);
#85817=ORIENTED_EDGE('',*,*,#58189,.T.);
#85818=ORIENTED_EDGE('',*,*,#58190,.T.);
#85819=ORIENTED_EDGE('',*,*,#58191,.F.);
#85820=ORIENTED_EDGE('',*,*,#58190,.F.);
#85821=ORIENTED_EDGE('',*,*,#58191,.T.);
#85822=ORIENTED_EDGE('',*,*,#58186,.T.);
#85823=ORIENTED_EDGE('',*,*,#58189,.F.);
#85824=ORIENTED_EDGE('',*,*,#58182,.T.);
#85825=ORIENTED_EDGE('',*,*,#58179,.T.);
#85826=ORIENTED_EDGE('',*,*,#58178,.T.);
#85827=ORIENTED_EDGE('',*,*,#58192,.F.);
#85828=ORIENTED_EDGE('',*,*,#58193,.T.);
#85829=ORIENTED_EDGE('',*,*,#58194,.F.);
#85830=ORIENTED_EDGE('',*,*,#58193,.F.);
#85831=ORIENTED_EDGE('',*,*,#58195,.F.);
#85832=ORIENTED_EDGE('',*,*,#58196,.T.);
#85833=ORIENTED_EDGE('',*,*,#58197,.F.);
#85834=ORIENTED_EDGE('',*,*,#58196,.F.);
#85835=ORIENTED_EDGE('',*,*,#58198,.F.);
#85836=ORIENTED_EDGE('',*,*,#58199,.T.);
#85837=ORIENTED_EDGE('',*,*,#58192,.T.);
#85838=ORIENTED_EDGE('',*,*,#58199,.F.);
#85839=ORIENTED_EDGE('',*,*,#58197,.T.);
#85840=ORIENTED_EDGE('',*,*,#58200,.T.);
#85841=ORIENTED_EDGE('',*,*,#58201,.T.);
#85842=ORIENTED_EDGE('',*,*,#58200,.F.);
#85843=ORIENTED_EDGE('',*,*,#58201,.F.);
#85844=ORIENTED_EDGE('',*,*,#58198,.T.);
#85845=ORIENTED_EDGE('',*,*,#58195,.T.);
#85846=ORIENTED_EDGE('',*,*,#58194,.T.);
#85847=ORIENTED_EDGE('',*,*,#58202,.T.);
#85848=ORIENTED_EDGE('',*,*,#58203,.T.);
#85849=ORIENTED_EDGE('',*,*,#58204,.F.);
#85850=ORIENTED_EDGE('',*,*,#58203,.F.);
#85851=ORIENTED_EDGE('',*,*,#58205,.F.);
#85852=ORIENTED_EDGE('',*,*,#58206,.F.);
#85853=ORIENTED_EDGE('',*,*,#58207,.F.);
#85854=ORIENTED_EDGE('',*,*,#58208,.T.);
#85855=ORIENTED_EDGE('',*,*,#58209,.F.);
#85856=ORIENTED_EDGE('',*,*,#58210,.T.);
#85857=ORIENTED_EDGE('',*,*,#58211,.F.);
#85858=ORIENTED_EDGE('',*,*,#58212,.F.);
#85859=ORIENTED_EDGE('',*,*,#58213,.F.);
#85860=ORIENTED_EDGE('',*,*,#58214,.T.);
#85861=ORIENTED_EDGE('',*,*,#58215,.F.);
#85862=ORIENTED_EDGE('',*,*,#58216,.F.);
#85863=ORIENTED_EDGE('',*,*,#58217,.F.);
#85864=ORIENTED_EDGE('',*,*,#58218,.T.);
#85865=ORIENTED_EDGE('',*,*,#58219,.F.);
#85866=ORIENTED_EDGE('',*,*,#58220,.F.);
#85867=ORIENTED_EDGE('',*,*,#58221,.F.);
#85868=ORIENTED_EDGE('',*,*,#58222,.F.);
#85869=ORIENTED_EDGE('',*,*,#58223,.F.);
#85870=ORIENTED_EDGE('',*,*,#58224,.F.);
#85871=ORIENTED_EDGE('',*,*,#58225,.F.);
#85872=ORIENTED_EDGE('',*,*,#58226,.T.);
#85873=ORIENTED_EDGE('',*,*,#58227,.F.);
#85874=ORIENTED_EDGE('',*,*,#58228,.F.);
#85875=ORIENTED_EDGE('',*,*,#58229,.F.);
#85876=ORIENTED_EDGE('',*,*,#58226,.F.);
#85877=ORIENTED_EDGE('',*,*,#58230,.F.);
#85878=ORIENTED_EDGE('',*,*,#58231,.T.);
#85879=ORIENTED_EDGE('',*,*,#58232,.F.);
#85880=ORIENTED_EDGE('',*,*,#58233,.F.);
#85881=ORIENTED_EDGE('',*,*,#58234,.F.);
#85882=ORIENTED_EDGE('',*,*,#58231,.F.);
#85883=ORIENTED_EDGE('',*,*,#58219,.T.);
#85884=ORIENTED_EDGE('',*,*,#58235,.F.);
#85885=ORIENTED_EDGE('',*,*,#58236,.F.);
#85886=ORIENTED_EDGE('',*,*,#58237,.T.);
#85887=ORIENTED_EDGE('',*,*,#58238,.T.);
#85888=ORIENTED_EDGE('',*,*,#58239,.F.);
#85889=ORIENTED_EDGE('',*,*,#58223,.T.);
#85890=ORIENTED_EDGE('',*,*,#58240,.F.);
#85891=ORIENTED_EDGE('',*,*,#58241,.T.);
#85892=ORIENTED_EDGE('',*,*,#58242,.T.);
#85893=ORIENTED_EDGE('',*,*,#58243,.F.);
#85894=ORIENTED_EDGE('',*,*,#58244,.F.);
#85895=ORIENTED_EDGE('',*,*,#58245,.F.);
#85896=ORIENTED_EDGE('',*,*,#58246,.T.);
#85897=ORIENTED_EDGE('',*,*,#58247,.F.);
#85898=ORIENTED_EDGE('',*,*,#58248,.T.);
#85899=ORIENTED_EDGE('',*,*,#58249,.F.);
#85900=ORIENTED_EDGE('',*,*,#58250,.T.);
#85901=ORIENTED_EDGE('',*,*,#58251,.T.);
#85902=ORIENTED_EDGE('',*,*,#58250,.F.);
#85903=ORIENTED_EDGE('',*,*,#58252,.T.);
#85904=ORIENTED_EDGE('',*,*,#58253,.T.);
#85905=ORIENTED_EDGE('',*,*,#58254,.T.);
#85906=ORIENTED_EDGE('',*,*,#58253,.F.);
#85907=ORIENTED_EDGE('',*,*,#58255,.T.);
#85908=ORIENTED_EDGE('',*,*,#58256,.T.);
#85909=ORIENTED_EDGE('',*,*,#58257,.T.);
#85910=ORIENTED_EDGE('',*,*,#58256,.F.);
#85911=ORIENTED_EDGE('',*,*,#58258,.T.);
#85912=ORIENTED_EDGE('',*,*,#58259,.T.);
#85913=ORIENTED_EDGE('',*,*,#58260,.T.);
#85914=ORIENTED_EDGE('',*,*,#58259,.F.);
#85915=ORIENTED_EDGE('',*,*,#58261,.T.);
#85916=ORIENTED_EDGE('',*,*,#58262,.T.);
#85917=ORIENTED_EDGE('',*,*,#58263,.T.);
#85918=ORIENTED_EDGE('',*,*,#58262,.F.);
#85919=ORIENTED_EDGE('',*,*,#58229,.T.);
#85920=ORIENTED_EDGE('',*,*,#58264,.T.);
#85921=ORIENTED_EDGE('',*,*,#58265,.T.);
#85922=ORIENTED_EDGE('',*,*,#58266,.T.);
#85923=ORIENTED_EDGE('',*,*,#58205,.T.);
#85924=ORIENTED_EDGE('',*,*,#58267,.T.);
#85925=ORIENTED_EDGE('',*,*,#58268,.T.);
#85926=ORIENTED_EDGE('',*,*,#58269,.T.);
#85927=ORIENTED_EDGE('',*,*,#58270,.T.);
#85928=ORIENTED_EDGE('',*,*,#58271,.T.);
#85929=ORIENTED_EDGE('',*,*,#58272,.T.);
#85930=ORIENTED_EDGE('',*,*,#58273,.T.);
#85931=ORIENTED_EDGE('',*,*,#58245,.T.);
#85932=ORIENTED_EDGE('',*,*,#58274,.T.);
#85933=ORIENTED_EDGE('',*,*,#58275,.T.);
#85934=ORIENTED_EDGE('',*,*,#58276,.T.);
#85935=ORIENTED_EDGE('',*,*,#58277,.T.);
#85936=ORIENTED_EDGE('',*,*,#58278,.T.);
#85937=ORIENTED_EDGE('',*,*,#58279,.T.);
#85938=ORIENTED_EDGE('',*,*,#58280,.T.);
#85939=ORIENTED_EDGE('',*,*,#58281,.T.);
#85940=ORIENTED_EDGE('',*,*,#58282,.T.);
#85941=ORIENTED_EDGE('',*,*,#58283,.T.);
#85942=ORIENTED_EDGE('',*,*,#58284,.T.);
#85943=ORIENTED_EDGE('',*,*,#58285,.T.);
#85944=ORIENTED_EDGE('',*,*,#58286,.T.);
#85945=ORIENTED_EDGE('',*,*,#58287,.T.);
#85946=ORIENTED_EDGE('',*,*,#58288,.T.);
#85947=ORIENTED_EDGE('',*,*,#58289,.T.);
#85948=ORIENTED_EDGE('',*,*,#58290,.T.);
#85949=ORIENTED_EDGE('',*,*,#58291,.T.);
#85950=ORIENTED_EDGE('',*,*,#58292,.T.);
#85951=ORIENTED_EDGE('',*,*,#58293,.T.);
#85952=ORIENTED_EDGE('',*,*,#58294,.F.);
#85953=ORIENTED_EDGE('',*,*,#58295,.T.);
#85954=ORIENTED_EDGE('',*,*,#58296,.T.);
#85955=ORIENTED_EDGE('',*,*,#58297,.T.);
#85956=ORIENTED_EDGE('',*,*,#58298,.F.);
#85957=ORIENTED_EDGE('',*,*,#58299,.F.);
#85958=ORIENTED_EDGE('',*,*,#58300,.T.);
#85959=ORIENTED_EDGE('',*,*,#58301,.T.);
#85960=ORIENTED_EDGE('',*,*,#58302,.T.);
#85961=ORIENTED_EDGE('',*,*,#58303,.T.);
#85962=ORIENTED_EDGE('',*,*,#58304,.F.);
#85963=ORIENTED_EDGE('',*,*,#58305,.T.);
#85964=ORIENTED_EDGE('',*,*,#58306,.T.);
#85965=ORIENTED_EDGE('',*,*,#58307,.T.);
#85966=ORIENTED_EDGE('',*,*,#58308,.F.);
#85967=ORIENTED_EDGE('',*,*,#58309,.F.);
#85968=ORIENTED_EDGE('',*,*,#58310,.T.);
#85969=ORIENTED_EDGE('',*,*,#58311,.T.);
#85970=ORIENTED_EDGE('',*,*,#58312,.T.);
#85971=ORIENTED_EDGE('',*,*,#58313,.F.);
#85972=ORIENTED_EDGE('',*,*,#58314,.T.);
#85973=ORIENTED_EDGE('',*,*,#58309,.T.);
#85974=ORIENTED_EDGE('',*,*,#58315,.F.);
#85975=ORIENTED_EDGE('',*,*,#58307,.F.);
#85976=ORIENTED_EDGE('',*,*,#58316,.T.);
#85977=ORIENTED_EDGE('',*,*,#58299,.T.);
#85978=ORIENTED_EDGE('',*,*,#58317,.F.);
#85979=ORIENTED_EDGE('',*,*,#58318,.F.);
#85980=ORIENTED_EDGE('',*,*,#58319,.T.);
#85981=ORIENTED_EDGE('',*,*,#58320,.T.);
#85982=ORIENTED_EDGE('',*,*,#58321,.F.);
#85983=ORIENTED_EDGE('',*,*,#58322,.T.);
#85984=ORIENTED_EDGE('',*,*,#58209,.T.);
#85985=ORIENTED_EDGE('',*,*,#58323,.F.);
#85986=ORIENTED_EDGE('',*,*,#58324,.T.);
#85987=ORIENTED_EDGE('',*,*,#58325,.T.);
#85988=ORIENTED_EDGE('',*,*,#58313,.T.);
#85989=ORIENTED_EDGE('',*,*,#58326,.F.);
#85990=ORIENTED_EDGE('',*,*,#58320,.F.);
#85991=ORIENTED_EDGE('',*,*,#58327,.T.);
#85992=ORIENTED_EDGE('',*,*,#58328,.T.);
#85993=ORIENTED_EDGE('',*,*,#58329,.T.);
#85994=ORIENTED_EDGE('',*,*,#58213,.T.);
#85995=ORIENTED_EDGE('',*,*,#58330,.F.);
#85996=ORIENTED_EDGE('',*,*,#58331,.T.);
#85997=ORIENTED_EDGE('',*,*,#58332,.T.);
#85998=ORIENTED_EDGE('',*,*,#58318,.T.);
#85999=ORIENTED_EDGE('',*,*,#58333,.F.);
#86000=ORIENTED_EDGE('',*,*,#58334,.F.);
#86001=ORIENTED_EDGE('',*,*,#58335,.T.);
#86002=ORIENTED_EDGE('',*,*,#58336,.T.);
#86003=ORIENTED_EDGE('',*,*,#58337,.T.);
#86004=ORIENTED_EDGE('',*,*,#58338,.T.);
#86005=ORIENTED_EDGE('',*,*,#58334,.T.);
#86006=ORIENTED_EDGE('',*,*,#58339,.F.);
#86007=ORIENTED_EDGE('',*,*,#58297,.F.);
#86008=ORIENTED_EDGE('',*,*,#58340,.T.);
#86009=ORIENTED_EDGE('',*,*,#58341,.F.);
#86010=ORIENTED_EDGE('',*,*,#58342,.T.);
#86011=ORIENTED_EDGE('',*,*,#58343,.T.);
#86012=ORIENTED_EDGE('',*,*,#58344,.F.);
#86013=ORIENTED_EDGE('',*,*,#58343,.F.);
#86014=ORIENTED_EDGE('',*,*,#58345,.T.);
#86015=ORIENTED_EDGE('',*,*,#58346,.T.);
#86016=ORIENTED_EDGE('',*,*,#58347,.F.);
#86017=ORIENTED_EDGE('',*,*,#58346,.F.);
#86018=ORIENTED_EDGE('',*,*,#58348,.T.);
#86019=ORIENTED_EDGE('',*,*,#58349,.T.);
#86020=ORIENTED_EDGE('',*,*,#58350,.F.);
#86021=ORIENTED_EDGE('',*,*,#58349,.F.);
#86022=ORIENTED_EDGE('',*,*,#58351,.T.);
#86023=ORIENTED_EDGE('',*,*,#58352,.T.);
#86024=ORIENTED_EDGE('',*,*,#58353,.F.);
#86025=ORIENTED_EDGE('',*,*,#58352,.F.);
#86026=ORIENTED_EDGE('',*,*,#58354,.T.);
#86027=ORIENTED_EDGE('',*,*,#58355,.T.);
#86028=ORIENTED_EDGE('',*,*,#58356,.F.);
#86029=ORIENTED_EDGE('',*,*,#58355,.F.);
#86030=ORIENTED_EDGE('',*,*,#58357,.T.);
#86031=ORIENTED_EDGE('',*,*,#58358,.T.);
#86032=ORIENTED_EDGE('',*,*,#58359,.F.);
#86033=ORIENTED_EDGE('',*,*,#58358,.F.);
#86034=ORIENTED_EDGE('',*,*,#58360,.T.);
#86035=ORIENTED_EDGE('',*,*,#58361,.T.);
#86036=ORIENTED_EDGE('',*,*,#58362,.F.);
#86037=ORIENTED_EDGE('',*,*,#58361,.F.);
#86038=ORIENTED_EDGE('',*,*,#58363,.T.);
#86039=ORIENTED_EDGE('',*,*,#58341,.T.);
#86040=ORIENTED_EDGE('',*,*,#58364,.F.);
#86041=ORIENTED_EDGE('',*,*,#58365,.T.);
#86042=ORIENTED_EDGE('',*,*,#58366,.T.);
#86043=ORIENTED_EDGE('',*,*,#58367,.T.);
#86044=ORIENTED_EDGE('',*,*,#58368,.T.);
#86045=ORIENTED_EDGE('',*,*,#58369,.T.);
#86046=ORIENTED_EDGE('',*,*,#58207,.T.);
#86047=ORIENTED_EDGE('',*,*,#58204,.T.);
#86048=ORIENTED_EDGE('',*,*,#58370,.T.);
#86049=ORIENTED_EDGE('',*,*,#58371,.T.);
#86050=ORIENTED_EDGE('',*,*,#58372,.F.);
#86051=ORIENTED_EDGE('',*,*,#58373,.T.);
#86052=ORIENTED_EDGE('',*,*,#58374,.T.);
#86053=ORIENTED_EDGE('',*,*,#58375,.T.);
#86054=ORIENTED_EDGE('',*,*,#58376,.T.);
#86055=ORIENTED_EDGE('',*,*,#58377,.T.);
#86056=ORIENTED_EDGE('',*,*,#58378,.T.);
#86057=ORIENTED_EDGE('',*,*,#58379,.T.);
#86058=ORIENTED_EDGE('',*,*,#58380,.T.);
#86059=ORIENTED_EDGE('',*,*,#58381,.T.);
#86060=ORIENTED_EDGE('',*,*,#58382,.T.);
#86061=ORIENTED_EDGE('',*,*,#58383,.T.);
#86062=ORIENTED_EDGE('',*,*,#58384,.T.);
#86063=ORIENTED_EDGE('',*,*,#58385,.T.);
#86064=ORIENTED_EDGE('',*,*,#58372,.T.);
#86065=ORIENTED_EDGE('',*,*,#58386,.T.);
#86066=ORIENTED_EDGE('',*,*,#58378,.F.);
#86067=ORIENTED_EDGE('',*,*,#58387,.T.);
#86068=ORIENTED_EDGE('',*,*,#58374,.F.);
#86069=ORIENTED_EDGE('',*,*,#58388,.T.);
#86070=ORIENTED_EDGE('',*,*,#58384,.F.);
#86071=ORIENTED_EDGE('',*,*,#58389,.T.);
#86072=ORIENTED_EDGE('',*,*,#58390,.T.);
#86073=ORIENTED_EDGE('',*,*,#58391,.T.);
#86074=ORIENTED_EDGE('',*,*,#58392,.T.);
#86075=ORIENTED_EDGE('',*,*,#58393,.T.);
#86076=ORIENTED_EDGE('',*,*,#58394,.T.);
#86077=ORIENTED_EDGE('',*,*,#58395,.T.);
#86078=ORIENTED_EDGE('',*,*,#58396,.T.);
#86079=ORIENTED_EDGE('',*,*,#58397,.T.);
#86080=ORIENTED_EDGE('',*,*,#58398,.T.);
#86081=ORIENTED_EDGE('',*,*,#58392,.F.);
#86082=ORIENTED_EDGE('',*,*,#58399,.T.);
#86083=ORIENTED_EDGE('',*,*,#58400,.F.);
#86084=ORIENTED_EDGE('',*,*,#58336,.F.);
#86085=ORIENTED_EDGE('',*,*,#58401,.T.);
#86086=ORIENTED_EDGE('',*,*,#58402,.T.);
#86087=ORIENTED_EDGE('',*,*,#58403,.T.);
#86088=ORIENTED_EDGE('',*,*,#58295,.F.);
#86089=ORIENTED_EDGE('',*,*,#58404,.F.);
#86090=ORIENTED_EDGE('',*,*,#58405,.T.);
#86091=ORIENTED_EDGE('',*,*,#58406,.F.);
#86092=ORIENTED_EDGE('',*,*,#58407,.T.);
#86093=ORIENTED_EDGE('',*,*,#58408,.T.);
#86094=ORIENTED_EDGE('',*,*,#58406,.T.);
#86095=ORIENTED_EDGE('',*,*,#58409,.T.);
#86096=ORIENTED_EDGE('',*,*,#58410,.T.);
#86097=ORIENTED_EDGE('',*,*,#58411,.T.);
#86098=ORIENTED_EDGE('',*,*,#58412,.T.);
#86099=ORIENTED_EDGE('',*,*,#58413,.T.);
#86100=ORIENTED_EDGE('',*,*,#58255,.F.);
#86101=ORIENTED_EDGE('',*,*,#58235,.T.);
#86102=ORIENTED_EDGE('',*,*,#58414,.T.);
#86103=ORIENTED_EDGE('',*,*,#58244,.T.);
#86104=ORIENTED_EDGE('',*,*,#58247,.T.);
#86105=ORIENTED_EDGE('',*,*,#58415,.T.);
#86106=ORIENTED_EDGE('',*,*,#58416,.T.);
#86107=ORIENTED_EDGE('',*,*,#58417,.T.);
#86108=ORIENTED_EDGE('',*,*,#58418,.T.);
#86109=ORIENTED_EDGE('',*,*,#58252,.F.);
#86110=ORIENTED_EDGE('',*,*,#58419,.T.);
#86111=ORIENTED_EDGE('',*,*,#58420,.T.);
#86112=ORIENTED_EDGE('',*,*,#58421,.T.);
#86113=ORIENTED_EDGE('',*,*,#58422,.T.);
#86114=ORIENTED_EDGE('',*,*,#58423,.T.);
#86115=ORIENTED_EDGE('',*,*,#58424,.T.);
#86116=ORIENTED_EDGE('',*,*,#58425,.T.);
#86117=ORIENTED_EDGE('',*,*,#58211,.T.);
#86118=ORIENTED_EDGE('',*,*,#58261,.F.);
#86119=ORIENTED_EDGE('',*,*,#58426,.T.);
#86120=ORIENTED_EDGE('',*,*,#58427,.T.);
#86121=ORIENTED_EDGE('',*,*,#58428,.T.);
#86122=ORIENTED_EDGE('',*,*,#58215,.T.);
#86123=ORIENTED_EDGE('',*,*,#58258,.F.);
#86124=ORIENTED_EDGE('',*,*,#58429,.T.);
#86125=ORIENTED_EDGE('',*,*,#58430,.T.);
#86126=ORIENTED_EDGE('',*,*,#58431,.T.);
#86127=ORIENTED_EDGE('',*,*,#58432,.T.);
#86128=ORIENTED_EDGE('',*,*,#58329,.F.);
#86129=ORIENTED_EDGE('',*,*,#58400,.T.);
#86130=ORIENTED_EDGE('',*,*,#58433,.T.);
#86131=ORIENTED_EDGE('',*,*,#58434,.T.);
#86132=ORIENTED_EDGE('',*,*,#58435,.T.);
#86133=ORIENTED_EDGE('',*,*,#58436,.T.);
#86134=ORIENTED_EDGE('',*,*,#58404,.T.);
#86135=ORIENTED_EDGE('',*,*,#58294,.T.);
#86136=ORIENTED_EDGE('',*,*,#58239,.T.);
#86137=ORIENTED_EDGE('',*,*,#58437,.T.);
#86138=ORIENTED_EDGE('',*,*,#58438,.T.);
#86139=ORIENTED_EDGE('',*,*,#58439,.T.);
#86140=ORIENTED_EDGE('',*,*,#58302,.F.);
#86141=ORIENTED_EDGE('',*,*,#58440,.T.);
#86142=ORIENTED_EDGE('',*,*,#58441,.T.);
#86143=ORIENTED_EDGE('',*,*,#58442,.T.);
#86144=ORIENTED_EDGE('',*,*,#58443,.T.);
#86145=ORIENTED_EDGE('',*,*,#58444,.T.);
#86146=ORIENTED_EDGE('',*,*,#58221,.T.);
#86147=ORIENTED_EDGE('',*,*,#58445,.T.);
#86148=ORIENTED_EDGE('',*,*,#58217,.T.);
#86149=ORIENTED_EDGE('',*,*,#58446,.T.);
#86150=ORIENTED_EDGE('',*,*,#58447,.T.);
#86151=ORIENTED_EDGE('',*,*,#58448,.T.);
#86152=ORIENTED_EDGE('',*,*,#58449,.T.);
#86153=ORIENTED_EDGE('',*,*,#58240,.T.);
#86154=ORIENTED_EDGE('',*,*,#58450,.T.);
#86155=ORIENTED_EDGE('',*,*,#58304,.T.);
#86156=ORIENTED_EDGE('',*,*,#58451,.T.);
#86157=ORIENTED_EDGE('',*,*,#58452,.T.);
#86158=ORIENTED_EDGE('',*,*,#58453,.T.);
#86159=ORIENTED_EDGE('',*,*,#58454,.T.);
#86160=ORIENTED_EDGE('',*,*,#58312,.F.);
#86161=ORIENTED_EDGE('',*,*,#58455,.T.);
#86162=ORIENTED_EDGE('',*,*,#58456,.T.);
#86163=ORIENTED_EDGE('',*,*,#58457,.T.);
#86164=ORIENTED_EDGE('',*,*,#58458,.T.);
#86165=ORIENTED_EDGE('',*,*,#58459,.T.);
#86166=ORIENTED_EDGE('',*,*,#58460,.T.);
#86167=ORIENTED_EDGE('',*,*,#58461,.T.);
#86168=ORIENTED_EDGE('',*,*,#58462,.T.);
#86169=ORIENTED_EDGE('',*,*,#58463,.T.);
#86170=ORIENTED_EDGE('',*,*,#58464,.T.);
#86171=ORIENTED_EDGE('',*,*,#58465,.T.);
#86172=ORIENTED_EDGE('',*,*,#58466,.T.);
#86173=ORIENTED_EDGE('',*,*,#58467,.T.);
#86174=ORIENTED_EDGE('',*,*,#58468,.T.);
#86175=ORIENTED_EDGE('',*,*,#58323,.T.);
#86176=ORIENTED_EDGE('',*,*,#58469,.T.);
#86177=ORIENTED_EDGE('',*,*,#58470,.T.);
#86178=ORIENTED_EDGE('',*,*,#58471,.T.);
#86179=ORIENTED_EDGE('',*,*,#58472,.T.);
#86180=ORIENTED_EDGE('',*,*,#58322,.F.);
#86181=ORIENTED_EDGE('',*,*,#58473,.T.);
#86182=ORIENTED_EDGE('',*,*,#58474,.T.);
#86183=ORIENTED_EDGE('',*,*,#58475,.T.);
#86184=ORIENTED_EDGE('',*,*,#58476,.T.);
#86185=ORIENTED_EDGE('',*,*,#58477,.T.);
#86186=ORIENTED_EDGE('',*,*,#58232,.T.);
#86187=ORIENTED_EDGE('',*,*,#58230,.T.);
#86188=ORIENTED_EDGE('',*,*,#58225,.T.);
#86189=ORIENTED_EDGE('',*,*,#58478,.T.);
#86190=ORIENTED_EDGE('',*,*,#58479,.T.);
#86191=ORIENTED_EDGE('',*,*,#58480,.T.);
#86192=ORIENTED_EDGE('',*,*,#58481,.T.);
#86193=ORIENTED_EDGE('',*,*,#58482,.T.);
#86194=ORIENTED_EDGE('',*,*,#58330,.T.);
#86195=ORIENTED_EDGE('',*,*,#58344,.T.);
#86196=ORIENTED_EDGE('',*,*,#58347,.T.);
#86197=ORIENTED_EDGE('',*,*,#58350,.T.);
#86198=ORIENTED_EDGE('',*,*,#58353,.T.);
#86199=ORIENTED_EDGE('',*,*,#58356,.T.);
#86200=ORIENTED_EDGE('',*,*,#58359,.T.);
#86201=ORIENTED_EDGE('',*,*,#58362,.T.);
#86202=ORIENTED_EDGE('',*,*,#58364,.T.);
#86203=ORIENTED_EDGE('',*,*,#58251,.F.);
#86204=ORIENTED_EDGE('',*,*,#58254,.F.);
#86205=ORIENTED_EDGE('',*,*,#58257,.F.);
#86206=ORIENTED_EDGE('',*,*,#58260,.F.);
#86207=ORIENTED_EDGE('',*,*,#58263,.F.);
#86208=ORIENTED_EDGE('',*,*,#58249,.T.);
#86209=ORIENTED_EDGE('',*,*,#58202,.F.);
#86210=ORIENTED_EDGE('',*,*,#58308,.T.);
#86211=ORIENTED_EDGE('',*,*,#58317,.T.);
#86212=ORIENTED_EDGE('',*,*,#58298,.T.);
#86213=ORIENTED_EDGE('',*,*,#58339,.T.);
#86214=ORIENTED_EDGE('',*,*,#58333,.T.);
#86215=ORIENTED_EDGE('',*,*,#58321,.T.);
#86216=ORIENTED_EDGE('',*,*,#58326,.T.);
#86217=ORIENTED_EDGE('',*,*,#58315,.T.);
#86218=ORIENTED_EDGE('',*,*,#58363,.F.);
#86219=ORIENTED_EDGE('',*,*,#58360,.F.);
#86220=ORIENTED_EDGE('',*,*,#58357,.F.);
#86221=ORIENTED_EDGE('',*,*,#58354,.F.);
#86222=ORIENTED_EDGE('',*,*,#58351,.F.);
#86223=ORIENTED_EDGE('',*,*,#58348,.F.);
#86224=ORIENTED_EDGE('',*,*,#58345,.F.);
#86225=ORIENTED_EDGE('',*,*,#58342,.F.);
#86226=ORIENTED_EDGE('',*,*,#58394,.F.);
#86227=ORIENTED_EDGE('',*,*,#58483,.T.);
#86228=ORIENTED_EDGE('',*,*,#58291,.F.);
#86229=ORIENTED_EDGE('',*,*,#58484,.T.);
#86230=ORIENTED_EDGE('',*,*,#58268,.F.);
#86231=ORIENTED_EDGE('',*,*,#58485,.T.);
#86232=ORIENTED_EDGE('',*,*,#58407,.F.);
#86233=ORIENTED_EDGE('',*,*,#58486,.T.);
#86234=ORIENTED_EDGE('',*,*,#58279,.F.);
#86235=ORIENTED_EDGE('',*,*,#58487,.T.);
#86236=ORIENTED_EDGE('',*,*,#58422,.F.);
#86237=ORIENTED_EDGE('',*,*,#58488,.T.);
#86238=ORIENTED_EDGE('',*,*,#58285,.F.);
#86239=ORIENTED_EDGE('',*,*,#58489,.T.);
#86240=ORIENTED_EDGE('',*,*,#58265,.F.);
#86241=ORIENTED_EDGE('',*,*,#58490,.T.);
#86242=ORIENTED_EDGE('',*,*,#58491,.F.);
#86243=ORIENTED_EDGE('',*,*,#58492,.T.);
#86244=ORIENTED_EDGE('',*,*,#58451,.F.);
#86245=ORIENTED_EDGE('',*,*,#58493,.T.);
#86246=ORIENTED_EDGE('',*,*,#58419,.F.);
#86247=ORIENTED_EDGE('',*,*,#58487,.F.);
#86248=ORIENTED_EDGE('',*,*,#58494,.T.);
#86249=ORIENTED_EDGE('',*,*,#58495,.T.);
#86250=ORIENTED_EDGE('',*,*,#58491,.T.);
#86251=ORIENTED_EDGE('',*,*,#58467,.F.);
#86252=ORIENTED_EDGE('',*,*,#58496,.T.);
#86253=ORIENTED_EDGE('',*,*,#58497,.F.);
#86254=ORIENTED_EDGE('',*,*,#58421,.F.);
#86255=ORIENTED_EDGE('',*,*,#58498,.T.);
#86256=ORIENTED_EDGE('',*,*,#58499,.T.);
#86257=ORIENTED_EDGE('',*,*,#58500,.T.);
#86258=ORIENTED_EDGE('',*,*,#58488,.F.);
#86259=ORIENTED_EDGE('',*,*,#58497,.T.);
#86260=ORIENTED_EDGE('',*,*,#58501,.F.);
#86261=ORIENTED_EDGE('',*,*,#58502,.T.);
#86262=ORIENTED_EDGE('',*,*,#58469,.F.);
#86263=ORIENTED_EDGE('',*,*,#58227,.T.);
#86264=ORIENTED_EDGE('',*,*,#58266,.F.);
#86265=ORIENTED_EDGE('',*,*,#58489,.F.);
#86266=ORIENTED_EDGE('',*,*,#58503,.T.);
#86267=ORIENTED_EDGE('',*,*,#58504,.T.);
#86268=ORIENTED_EDGE('',*,*,#58501,.T.);
#86269=ORIENTED_EDGE('',*,*,#58481,.F.);
#86270=ORIENTED_EDGE('',*,*,#58505,.T.);
#86271=ORIENTED_EDGE('',*,*,#58506,.T.);
#86272=ORIENTED_EDGE('',*,*,#58507,.F.);
#86273=ORIENTED_EDGE('',*,*,#58264,.F.);
#86274=ORIENTED_EDGE('',*,*,#58234,.T.);
#86275=ORIENTED_EDGE('',*,*,#58508,.T.);
#86276=ORIENTED_EDGE('',*,*,#58509,.T.);
#86277=ORIENTED_EDGE('',*,*,#58490,.F.);
#86278=ORIENTED_EDGE('',*,*,#58507,.T.);
#86279=ORIENTED_EDGE('',*,*,#58510,.F.);
#86280=ORIENTED_EDGE('',*,*,#58511,.T.);
#86281=ORIENTED_EDGE('',*,*,#58429,.F.);
#86282=ORIENTED_EDGE('',*,*,#58399,.F.);
#86283=ORIENTED_EDGE('',*,*,#58395,.F.);
#86284=ORIENTED_EDGE('',*,*,#58484,.F.);
#86285=ORIENTED_EDGE('',*,*,#58512,.T.);
#86286=ORIENTED_EDGE('',*,*,#58513,.T.);
#86287=ORIENTED_EDGE('',*,*,#58510,.T.);
#86288=ORIENTED_EDGE('',*,*,#58436,.F.);
#86289=ORIENTED_EDGE('',*,*,#58514,.T.);
#86290=ORIENTED_EDGE('',*,*,#58515,.F.);
#86291=ORIENTED_EDGE('',*,*,#58409,.F.);
#86292=ORIENTED_EDGE('',*,*,#58405,.F.);
#86293=ORIENTED_EDGE('',*,*,#58516,.T.);
#86294=ORIENTED_EDGE('',*,*,#58517,.T.);
#86295=ORIENTED_EDGE('',*,*,#58486,.F.);
#86296=ORIENTED_EDGE('',*,*,#58515,.T.);
#86297=ORIENTED_EDGE('',*,*,#58518,.T.);
#86298=ORIENTED_EDGE('',*,*,#58519,.T.);
#86299=ORIENTED_EDGE('',*,*,#58248,.F.);
#86300=ORIENTED_EDGE('',*,*,#58243,.T.);
#86301=ORIENTED_EDGE('',*,*,#58246,.F.);
#86302=ORIENTED_EDGE('',*,*,#58520,.T.);
#86303=ORIENTED_EDGE('',*,*,#58521,.T.);
#86304=ORIENTED_EDGE('',*,*,#58236,.T.);
#86305=ORIENTED_EDGE('',*,*,#58522,.F.);
#86306=ORIENTED_EDGE('',*,*,#58460,.F.);
#86307=ORIENTED_EDGE('',*,*,#58523,.F.);
#86308=ORIENTED_EDGE('',*,*,#58498,.F.);
#86309=ORIENTED_EDGE('',*,*,#58523,.T.);
#86310=ORIENTED_EDGE('',*,*,#58459,.F.);
#86311=ORIENTED_EDGE('',*,*,#58524,.F.);
#86312=ORIENTED_EDGE('',*,*,#58468,.F.);
#86313=ORIENTED_EDGE('',*,*,#58522,.T.);
#86314=ORIENTED_EDGE('',*,*,#58420,.F.);
#86315=ORIENTED_EDGE('',*,*,#58525,.F.);
#86316=ORIENTED_EDGE('',*,*,#58461,.F.);
#86317=ORIENTED_EDGE('',*,*,#58524,.T.);
#86318=ORIENTED_EDGE('',*,*,#58458,.F.);
#86319=ORIENTED_EDGE('',*,*,#58526,.F.);
#86320=ORIENTED_EDGE('',*,*,#58324,.F.);
#86321=ORIENTED_EDGE('',*,*,#58525,.T.);
#86322=ORIENTED_EDGE('',*,*,#58493,.F.);
#86323=ORIENTED_EDGE('',*,*,#58527,.F.);
#86324=ORIENTED_EDGE('',*,*,#58462,.F.);
#86325=ORIENTED_EDGE('',*,*,#58325,.F.);
#86326=ORIENTED_EDGE('',*,*,#58526,.T.);
#86327=ORIENTED_EDGE('',*,*,#58528,.F.);
#86328=ORIENTED_EDGE('',*,*,#58527,.T.);
#86329=ORIENTED_EDGE('',*,*,#58455,.F.);
#86330=ORIENTED_EDGE('',*,*,#58529,.F.);
#86331=ORIENTED_EDGE('',*,*,#58463,.F.);
#86332=ORIENTED_EDGE('',*,*,#58528,.T.);
#86333=ORIENTED_EDGE('',*,*,#58457,.F.);
#86334=ORIENTED_EDGE('',*,*,#58530,.F.);
#86335=ORIENTED_EDGE('',*,*,#58314,.F.);
#86336=ORIENTED_EDGE('',*,*,#58529,.T.);
#86337=ORIENTED_EDGE('',*,*,#58311,.F.);
#86338=ORIENTED_EDGE('',*,*,#58531,.F.);
#86339=ORIENTED_EDGE('',*,*,#58456,.F.);
#86340=ORIENTED_EDGE('',*,*,#58310,.F.);
#86341=ORIENTED_EDGE('',*,*,#58530,.T.);
#86342=ORIENTED_EDGE('',*,*,#58531,.T.);
#86343=ORIENTED_EDGE('',*,*,#58233,.T.);
#86344=ORIENTED_EDGE('',*,*,#58477,.F.);
#86345=ORIENTED_EDGE('',*,*,#58532,.F.);
#86346=ORIENTED_EDGE('',*,*,#58482,.F.);
#86347=ORIENTED_EDGE('',*,*,#58532,.T.);
#86348=ORIENTED_EDGE('',*,*,#58476,.F.);
#86349=ORIENTED_EDGE('',*,*,#58533,.F.);
#86350=ORIENTED_EDGE('',*,*,#58331,.F.);
#86351=ORIENTED_EDGE('',*,*,#58332,.F.);
#86352=ORIENTED_EDGE('',*,*,#58533,.T.);
#86353=ORIENTED_EDGE('',*,*,#58534,.F.);
#86354=ORIENTED_EDGE('',*,*,#58228,.T.);
#86355=ORIENTED_EDGE('',*,*,#58473,.F.);
#86356=ORIENTED_EDGE('',*,*,#58535,.F.);
#86357=ORIENTED_EDGE('',*,*,#58478,.F.);
#86358=ORIENTED_EDGE('',*,*,#58534,.T.);
#86359=ORIENTED_EDGE('',*,*,#58475,.F.);
#86360=ORIENTED_EDGE('',*,*,#58536,.F.);
#86361=ORIENTED_EDGE('',*,*,#58319,.F.);
#86362=ORIENTED_EDGE('',*,*,#58535,.T.);
#86363=ORIENTED_EDGE('',*,*,#58328,.F.);
#86364=ORIENTED_EDGE('',*,*,#58537,.F.);
#86365=ORIENTED_EDGE('',*,*,#58474,.F.);
#86366=ORIENTED_EDGE('',*,*,#58327,.F.);
#86367=ORIENTED_EDGE('',*,*,#58536,.T.);
#86368=ORIENTED_EDGE('',*,*,#58537,.T.);
#86369=ORIENTED_EDGE('',*,*,#58222,.T.);
#86370=ORIENTED_EDGE('',*,*,#58444,.F.);
#86371=ORIENTED_EDGE('',*,*,#58538,.F.);
#86372=ORIENTED_EDGE('',*,*,#58450,.F.);
#86373=ORIENTED_EDGE('',*,*,#58224,.T.);
#86374=ORIENTED_EDGE('',*,*,#58414,.F.);
#86375=ORIENTED_EDGE('',*,*,#58218,.F.);
#86376=ORIENTED_EDGE('',*,*,#58445,.F.);
#86377=ORIENTED_EDGE('',*,*,#58538,.T.);
#86378=ORIENTED_EDGE('',*,*,#58443,.F.);
#86379=ORIENTED_EDGE('',*,*,#58539,.F.);
#86380=ORIENTED_EDGE('',*,*,#58305,.F.);
#86381=ORIENTED_EDGE('',*,*,#58306,.F.);
#86382=ORIENTED_EDGE('',*,*,#58539,.T.);
#86383=ORIENTED_EDGE('',*,*,#58540,.F.);
#86384=ORIENTED_EDGE('',*,*,#58220,.T.);
#86385=ORIENTED_EDGE('',*,*,#58440,.F.);
#86386=ORIENTED_EDGE('',*,*,#58541,.F.);
#86387=ORIENTED_EDGE('',*,*,#58446,.F.);
#86388=ORIENTED_EDGE('',*,*,#58540,.T.);
#86389=ORIENTED_EDGE('',*,*,#58442,.F.);
#86390=ORIENTED_EDGE('',*,*,#58542,.F.);
#86391=ORIENTED_EDGE('',*,*,#58316,.F.);
#86392=ORIENTED_EDGE('',*,*,#58541,.T.);
#86393=ORIENTED_EDGE('',*,*,#58301,.F.);
#86394=ORIENTED_EDGE('',*,*,#58543,.F.);
#86395=ORIENTED_EDGE('',*,*,#58441,.F.);
#86396=ORIENTED_EDGE('',*,*,#58300,.F.);
#86397=ORIENTED_EDGE('',*,*,#58542,.T.);
#86398=ORIENTED_EDGE('',*,*,#58543,.T.);
#86399=ORIENTED_EDGE('',*,*,#58403,.F.);
#86400=ORIENTED_EDGE('',*,*,#58544,.T.);
#86401=ORIENTED_EDGE('',*,*,#58340,.F.);
#86402=ORIENTED_EDGE('',*,*,#58296,.F.);
#86403=ORIENTED_EDGE('',*,*,#58390,.F.);
#86404=ORIENTED_EDGE('',*,*,#58545,.T.);
#86405=ORIENTED_EDGE('',*,*,#58337,.F.);
#86406=ORIENTED_EDGE('',*,*,#58546,.T.);
#86407=ORIENTED_EDGE('',*,*,#58338,.F.);
#86408=ORIENTED_EDGE('',*,*,#58547,.T.);
#86409=ORIENTED_EDGE('',*,*,#58396,.F.);
#86410=ORIENTED_EDGE('',*,*,#58335,.F.);
#86411=ORIENTED_EDGE('',*,*,#58439,.F.);
#86412=ORIENTED_EDGE('',*,*,#58548,.T.);
#86413=ORIENTED_EDGE('',*,*,#58410,.F.);
#86414=ORIENTED_EDGE('',*,*,#58549,.F.);
#86415=ORIENTED_EDGE('',*,*,#58549,.T.);
#86416=ORIENTED_EDGE('',*,*,#58413,.F.);
#86417=ORIENTED_EDGE('',*,*,#58550,.F.);
#86418=ORIENTED_EDGE('',*,*,#58293,.F.);
#86419=ORIENTED_EDGE('',*,*,#58412,.F.);
#86420=ORIENTED_EDGE('',*,*,#58551,.T.);
#86421=ORIENTED_EDGE('',*,*,#58433,.F.);
#86422=ORIENTED_EDGE('',*,*,#58550,.T.);
#86423=ORIENTED_EDGE('',*,*,#58432,.F.);
#86424=ORIENTED_EDGE('',*,*,#58552,.T.);
#86425=ORIENTED_EDGE('',*,*,#58426,.F.);
#86426=ORIENTED_EDGE('',*,*,#58214,.F.);
#86427=ORIENTED_EDGE('',*,*,#58428,.F.);
#86428=ORIENTED_EDGE('',*,*,#58553,.T.);
#86429=ORIENTED_EDGE('',*,*,#58479,.F.);
#86430=ORIENTED_EDGE('',*,*,#58216,.T.);
#86431=ORIENTED_EDGE('',*,*,#58472,.F.);
#86432=ORIENTED_EDGE('',*,*,#58554,.T.);
#86433=ORIENTED_EDGE('',*,*,#58423,.F.);
#86434=ORIENTED_EDGE('',*,*,#58210,.F.);
#86435=ORIENTED_EDGE('',*,*,#58425,.F.);
#86436=ORIENTED_EDGE('',*,*,#58555,.T.);
#86437=ORIENTED_EDGE('',*,*,#58464,.F.);
#86438=ORIENTED_EDGE('',*,*,#58212,.T.);
#86439=ORIENTED_EDGE('',*,*,#58454,.F.);
#86440=ORIENTED_EDGE('',*,*,#58556,.T.);
#86441=ORIENTED_EDGE('',*,*,#58415,.F.);
#86442=ORIENTED_EDGE('',*,*,#58557,.F.);
#86443=ORIENTED_EDGE('',*,*,#58557,.T.);
#86444=ORIENTED_EDGE('',*,*,#58418,.F.);
#86445=ORIENTED_EDGE('',*,*,#58558,.F.);
#86446=ORIENTED_EDGE('',*,*,#58303,.F.);
#86447=ORIENTED_EDGE('',*,*,#58417,.F.);
#86448=ORIENTED_EDGE('',*,*,#58559,.T.);
#86449=ORIENTED_EDGE('',*,*,#58447,.F.);
#86450=ORIENTED_EDGE('',*,*,#58558,.T.);
#86451=ORIENTED_EDGE('',*,*,#58560,.T.);
#86452=ORIENTED_EDGE('',*,*,#58561,.T.);
#86453=ORIENTED_EDGE('',*,*,#58277,.F.);
#86454=ORIENTED_EDGE('',*,*,#58562,.F.);
#86455=ORIENTED_EDGE('',*,*,#58556,.F.);
#86456=ORIENTED_EDGE('',*,*,#58453,.F.);
#86457=ORIENTED_EDGE('',*,*,#58562,.T.);
#86458=ORIENTED_EDGE('',*,*,#58276,.F.);
#86459=ORIENTED_EDGE('',*,*,#58563,.F.);
#86460=ORIENTED_EDGE('',*,*,#58416,.F.);
#86461=ORIENTED_EDGE('',*,*,#58275,.F.);
#86462=ORIENTED_EDGE('',*,*,#58564,.T.);
#86463=ORIENTED_EDGE('',*,*,#58565,.T.);
#86464=ORIENTED_EDGE('',*,*,#58448,.F.);
#86465=ORIENTED_EDGE('',*,*,#58559,.F.);
#86466=ORIENTED_EDGE('',*,*,#58563,.T.);
#86467=ORIENTED_EDGE('',*,*,#58566,.T.);
#86468=ORIENTED_EDGE('',*,*,#58567,.T.);
#86469=ORIENTED_EDGE('',*,*,#58283,.F.);
#86470=ORIENTED_EDGE('',*,*,#58568,.F.);
#86471=ORIENTED_EDGE('',*,*,#58554,.F.);
#86472=ORIENTED_EDGE('',*,*,#58471,.F.);
#86473=ORIENTED_EDGE('',*,*,#58568,.T.);
#86474=ORIENTED_EDGE('',*,*,#58282,.F.);
#86475=ORIENTED_EDGE('',*,*,#58569,.F.);
#86476=ORIENTED_EDGE('',*,*,#58424,.F.);
#86477=ORIENTED_EDGE('',*,*,#58570,.T.);
#86478=ORIENTED_EDGE('',*,*,#58571,.T.);
#86479=ORIENTED_EDGE('',*,*,#58465,.F.);
#86480=ORIENTED_EDGE('',*,*,#58555,.F.);
#86481=ORIENTED_EDGE('',*,*,#58569,.T.);
#86482=ORIENTED_EDGE('',*,*,#58281,.F.);
#86483=ORIENTED_EDGE('',*,*,#58572,.T.);
#86484=ORIENTED_EDGE('',*,*,#58573,.T.);
#86485=ORIENTED_EDGE('',*,*,#58289,.F.);
#86486=ORIENTED_EDGE('',*,*,#58574,.F.);
#86487=ORIENTED_EDGE('',*,*,#58552,.F.);
#86488=ORIENTED_EDGE('',*,*,#58431,.F.);
#86489=ORIENTED_EDGE('',*,*,#58574,.T.);
#86490=ORIENTED_EDGE('',*,*,#58288,.F.);
#86491=ORIENTED_EDGE('',*,*,#58575,.F.);
#86492=ORIENTED_EDGE('',*,*,#58427,.F.);
#86493=ORIENTED_EDGE('',*,*,#58287,.F.);
#86494=ORIENTED_EDGE('',*,*,#58576,.T.);
#86495=ORIENTED_EDGE('',*,*,#58577,.T.);
#86496=ORIENTED_EDGE('',*,*,#58578,.T.);
#86497=ORIENTED_EDGE('',*,*,#58553,.F.);
#86498=ORIENTED_EDGE('',*,*,#58575,.T.);
#86499=ORIENTED_EDGE('',*,*,#58270,.F.);
#86500=ORIENTED_EDGE('',*,*,#58579,.T.);
#86501=ORIENTED_EDGE('',*,*,#58580,.T.);
#86502=ORIENTED_EDGE('',*,*,#58434,.F.);
#86503=ORIENTED_EDGE('',*,*,#58551,.F.);
#86504=ORIENTED_EDGE('',*,*,#58581,.F.);
#86505=ORIENTED_EDGE('',*,*,#58581,.T.);
#86506=ORIENTED_EDGE('',*,*,#58411,.F.);
#86507=ORIENTED_EDGE('',*,*,#58582,.F.);
#86508=ORIENTED_EDGE('',*,*,#58271,.F.);
#86509=ORIENTED_EDGE('',*,*,#58583,.T.);
#86510=ORIENTED_EDGE('',*,*,#58584,.T.);
#86511=ORIENTED_EDGE('',*,*,#58272,.F.);
#86512=ORIENTED_EDGE('',*,*,#58582,.T.);
#86513=ORIENTED_EDGE('',*,*,#58548,.F.);
#86514=ORIENTED_EDGE('',*,*,#58438,.F.);
#86515=ORIENTED_EDGE('',*,*,#58380,.F.);
#86516=ORIENTED_EDGE('',*,*,#58585,.T.);
#86517=ORIENTED_EDGE('',*,*,#58292,.F.);
#86518=ORIENTED_EDGE('',*,*,#58586,.F.);
#86519=ORIENTED_EDGE('',*,*,#58586,.T.);
#86520=ORIENTED_EDGE('',*,*,#58483,.F.);
#86521=ORIENTED_EDGE('',*,*,#58587,.F.);
#86522=ORIENTED_EDGE('',*,*,#58381,.F.);
#86523=ORIENTED_EDGE('',*,*,#58587,.T.);
#86524=ORIENTED_EDGE('',*,*,#58393,.F.);
#86525=ORIENTED_EDGE('',*,*,#58398,.F.);
#86526=ORIENTED_EDGE('',*,*,#58588,.T.);
#86527=ORIENTED_EDGE('',*,*,#58382,.F.);
#86528=ORIENTED_EDGE('',*,*,#58267,.F.);
#86529=ORIENTED_EDGE('',*,*,#58589,.T.);
#86530=ORIENTED_EDGE('',*,*,#58370,.F.);
#86531=ORIENTED_EDGE('',*,*,#58590,.F.);
#86532=ORIENTED_EDGE('',*,*,#58590,.T.);
#86533=ORIENTED_EDGE('',*,*,#58377,.F.);
#86534=ORIENTED_EDGE('',*,*,#58591,.F.);
#86535=ORIENTED_EDGE('',*,*,#58485,.F.);
#86536=ORIENTED_EDGE('',*,*,#58591,.T.);
#86537=ORIENTED_EDGE('',*,*,#58376,.F.);
#86538=ORIENTED_EDGE('',*,*,#58592,.T.);
#86539=ORIENTED_EDGE('',*,*,#58401,.F.);
#86540=ORIENTED_EDGE('',*,*,#58408,.F.);
#86541=ORIENTED_EDGE('',*,*,#58593,.F.);
#86542=ORIENTED_EDGE('',*,*,#58389,.F.);
#86543=ORIENTED_EDGE('',*,*,#58383,.F.);
#86544=ORIENTED_EDGE('',*,*,#58588,.F.);
#86545=ORIENTED_EDGE('',*,*,#58397,.F.);
#86546=ORIENTED_EDGE('',*,*,#58547,.F.);
#86547=ORIENTED_EDGE('',*,*,#58545,.F.);
#86548=ORIENTED_EDGE('',*,*,#58593,.T.);
#86549=ORIENTED_EDGE('',*,*,#58594,.F.);
#86550=ORIENTED_EDGE('',*,*,#58402,.F.);
#86551=ORIENTED_EDGE('',*,*,#58592,.F.);
#86552=ORIENTED_EDGE('',*,*,#58375,.F.);
#86553=ORIENTED_EDGE('',*,*,#58391,.F.);
#86554=ORIENTED_EDGE('',*,*,#58546,.F.);
#86555=ORIENTED_EDGE('',*,*,#58544,.F.);
#86556=ORIENTED_EDGE('',*,*,#58594,.T.);
#86557=ORIENTED_EDGE('',*,*,#58385,.F.);
#86558=ORIENTED_EDGE('',*,*,#58388,.F.);
#86559=ORIENTED_EDGE('',*,*,#58373,.F.);
#86560=ORIENTED_EDGE('',*,*,#58387,.F.);
#86561=ORIENTED_EDGE('',*,*,#58595,.F.);
#86562=ORIENTED_EDGE('',*,*,#58480,.F.);
#86563=ORIENTED_EDGE('',*,*,#58578,.F.);
#86564=ORIENTED_EDGE('',*,*,#58505,.F.);
#86565=ORIENTED_EDGE('',*,*,#58595,.T.);
#86566=ORIENTED_EDGE('',*,*,#58596,.F.);
#86567=ORIENTED_EDGE('',*,*,#58596,.T.);
#86568=ORIENTED_EDGE('',*,*,#58577,.F.);
#86569=ORIENTED_EDGE('',*,*,#58597,.F.);
#86570=ORIENTED_EDGE('',*,*,#58506,.F.);
#86571=ORIENTED_EDGE('',*,*,#58597,.T.);
#86572=ORIENTED_EDGE('',*,*,#58576,.F.);
#86573=ORIENTED_EDGE('',*,*,#58598,.F.);
#86574=ORIENTED_EDGE('',*,*,#58508,.F.);
#86575=ORIENTED_EDGE('',*,*,#58286,.F.);
#86576=ORIENTED_EDGE('',*,*,#58509,.F.);
#86577=ORIENTED_EDGE('',*,*,#58598,.T.);
#86578=ORIENTED_EDGE('',*,*,#58430,.F.);
#86579=ORIENTED_EDGE('',*,*,#58511,.F.);
#86580=ORIENTED_EDGE('',*,*,#58599,.F.);
#86581=ORIENTED_EDGE('',*,*,#58572,.F.);
#86582=ORIENTED_EDGE('',*,*,#58599,.T.);
#86583=ORIENTED_EDGE('',*,*,#58513,.F.);
#86584=ORIENTED_EDGE('',*,*,#58600,.F.);
#86585=ORIENTED_EDGE('',*,*,#58573,.F.);
#86586=ORIENTED_EDGE('',*,*,#58600,.T.);
#86587=ORIENTED_EDGE('',*,*,#58512,.F.);
#86588=ORIENTED_EDGE('',*,*,#58290,.F.);
#86589=ORIENTED_EDGE('',*,*,#58435,.F.);
#86590=ORIENTED_EDGE('',*,*,#58580,.F.);
#86591=ORIENTED_EDGE('',*,*,#58601,.F.);
#86592=ORIENTED_EDGE('',*,*,#58514,.F.);
#86593=ORIENTED_EDGE('',*,*,#58601,.T.);
#86594=ORIENTED_EDGE('',*,*,#58579,.F.);
#86595=ORIENTED_EDGE('',*,*,#58602,.F.);
#86596=ORIENTED_EDGE('',*,*,#58516,.F.);
#86597=ORIENTED_EDGE('',*,*,#58269,.F.);
#86598=ORIENTED_EDGE('',*,*,#58517,.F.);
#86599=ORIENTED_EDGE('',*,*,#58602,.T.);
#86600=ORIENTED_EDGE('',*,*,#58437,.F.);
#86601=ORIENTED_EDGE('',*,*,#58238,.F.);
#86602=ORIENTED_EDGE('',*,*,#58237,.F.);
#86603=ORIENTED_EDGE('',*,*,#58603,.F.);
#86604=ORIENTED_EDGE('',*,*,#58583,.F.);
#86605=ORIENTED_EDGE('',*,*,#58603,.T.);
#86606=ORIENTED_EDGE('',*,*,#58521,.F.);
#86607=ORIENTED_EDGE('',*,*,#58604,.F.);
#86608=ORIENTED_EDGE('',*,*,#58584,.F.);
#86609=ORIENTED_EDGE('',*,*,#58604,.T.);
#86610=ORIENTED_EDGE('',*,*,#58520,.F.);
#86611=ORIENTED_EDGE('',*,*,#58273,.F.);
#86612=ORIENTED_EDGE('',*,*,#58449,.F.);
#86613=ORIENTED_EDGE('',*,*,#58565,.F.);
#86614=ORIENTED_EDGE('',*,*,#58605,.F.);
#86615=ORIENTED_EDGE('',*,*,#58242,.F.);
#86616=ORIENTED_EDGE('',*,*,#58241,.F.);
#86617=ORIENTED_EDGE('',*,*,#58605,.T.);
#86618=ORIENTED_EDGE('',*,*,#58564,.F.);
#86619=ORIENTED_EDGE('',*,*,#58606,.F.);
#86620=ORIENTED_EDGE('',*,*,#58518,.F.);
#86621=ORIENTED_EDGE('',*,*,#58274,.F.);
#86622=ORIENTED_EDGE('',*,*,#58519,.F.);
#86623=ORIENTED_EDGE('',*,*,#58606,.T.);
#86624=ORIENTED_EDGE('',*,*,#58452,.F.);
#86625=ORIENTED_EDGE('',*,*,#58492,.F.);
#86626=ORIENTED_EDGE('',*,*,#58607,.F.);
#86627=ORIENTED_EDGE('',*,*,#58560,.F.);
#86628=ORIENTED_EDGE('',*,*,#58607,.T.);
#86629=ORIENTED_EDGE('',*,*,#58495,.F.);
#86630=ORIENTED_EDGE('',*,*,#58608,.F.);
#86631=ORIENTED_EDGE('',*,*,#58561,.F.);
#86632=ORIENTED_EDGE('',*,*,#58608,.T.);
#86633=ORIENTED_EDGE('',*,*,#58494,.F.);
#86634=ORIENTED_EDGE('',*,*,#58278,.F.);
#86635=ORIENTED_EDGE('',*,*,#58280,.F.);
#86636=ORIENTED_EDGE('',*,*,#58500,.F.);
#86637=ORIENTED_EDGE('',*,*,#58609,.F.);
#86638=ORIENTED_EDGE('',*,*,#58609,.T.);
#86639=ORIENTED_EDGE('',*,*,#58499,.F.);
#86640=ORIENTED_EDGE('',*,*,#58610,.F.);
#86641=ORIENTED_EDGE('',*,*,#58570,.F.);
#86642=ORIENTED_EDGE('',*,*,#58466,.F.);
#86643=ORIENTED_EDGE('',*,*,#58571,.F.);
#86644=ORIENTED_EDGE('',*,*,#58610,.T.);
#86645=ORIENTED_EDGE('',*,*,#58496,.F.);
#86646=ORIENTED_EDGE('',*,*,#58470,.F.);
#86647=ORIENTED_EDGE('',*,*,#58502,.F.);
#86648=ORIENTED_EDGE('',*,*,#58611,.F.);
#86649=ORIENTED_EDGE('',*,*,#58566,.F.);
#86650=ORIENTED_EDGE('',*,*,#58611,.T.);
#86651=ORIENTED_EDGE('',*,*,#58504,.F.);
#86652=ORIENTED_EDGE('',*,*,#58612,.F.);
#86653=ORIENTED_EDGE('',*,*,#58567,.F.);
#86654=ORIENTED_EDGE('',*,*,#58612,.T.);
#86655=ORIENTED_EDGE('',*,*,#58503,.F.);
#86656=ORIENTED_EDGE('',*,*,#58284,.F.);
#86657=ORIENTED_EDGE('',*,*,#58613,.F.);
#86658=ORIENTED_EDGE('',*,*,#58589,.F.);
#86659=ORIENTED_EDGE('',*,*,#58208,.F.);
#86660=ORIENTED_EDGE('',*,*,#58369,.F.);
#86661=ORIENTED_EDGE('',*,*,#58613,.T.);
#86662=ORIENTED_EDGE('',*,*,#58368,.F.);
#86663=ORIENTED_EDGE('',*,*,#58614,.F.);
#86664=ORIENTED_EDGE('',*,*,#58371,.F.);
#86665=ORIENTED_EDGE('',*,*,#58206,.T.);
#86666=ORIENTED_EDGE('',*,*,#58585,.F.);
#86667=ORIENTED_EDGE('',*,*,#58615,.F.);
#86668=ORIENTED_EDGE('',*,*,#58365,.F.);
#86669=ORIENTED_EDGE('',*,*,#58614,.T.);
#86670=ORIENTED_EDGE('',*,*,#58367,.F.);
#86671=ORIENTED_EDGE('',*,*,#58616,.F.);
#86672=ORIENTED_EDGE('',*,*,#58386,.F.);
#86673=ORIENTED_EDGE('',*,*,#58615,.T.);
#86674=ORIENTED_EDGE('',*,*,#58379,.F.);
#86675=ORIENTED_EDGE('',*,*,#58616,.T.);
#86676=ORIENTED_EDGE('',*,*,#58366,.F.);
#86677=ORIENTED_EDGE('',*,*,#58617,.T.);
#86678=ORIENTED_EDGE('',*,*,#58617,.F.);
#86679=ORIENTED_EDGE('',*,*,#58618,.F.);
#86680=ORIENTED_EDGE('',*,*,#58619,.T.);
#86681=ORIENTED_EDGE('',*,*,#58620,.F.);
#86682=ORIENTED_EDGE('',*,*,#58619,.F.);
#86683=ORIENTED_EDGE('',*,*,#58621,.F.);
#86684=ORIENTED_EDGE('',*,*,#58622,.F.);
#86685=ORIENTED_EDGE('',*,*,#58623,.T.);
#86686=ORIENTED_EDGE('',*,*,#58624,.F.);
#86687=ORIENTED_EDGE('',*,*,#58623,.F.);
#86688=ORIENTED_EDGE('',*,*,#58625,.F.);
#86689=ORIENTED_EDGE('',*,*,#58626,.F.);
#86690=ORIENTED_EDGE('',*,*,#58627,.T.);
#86691=ORIENTED_EDGE('',*,*,#58628,.F.);
#86692=ORIENTED_EDGE('',*,*,#58629,.F.);
#86693=ORIENTED_EDGE('',*,*,#58630,.F.);
#86694=ORIENTED_EDGE('',*,*,#58631,.F.);
#86695=ORIENTED_EDGE('',*,*,#58632,.T.);
#86696=ORIENTED_EDGE('',*,*,#58629,.T.);
#86697=ORIENTED_EDGE('',*,*,#58628,.T.);
#86698=ORIENTED_EDGE('',*,*,#58633,.T.);
#86699=ORIENTED_EDGE('',*,*,#58634,.T.);
#86700=ORIENTED_EDGE('',*,*,#58635,.T.);
#86701=ORIENTED_EDGE('',*,*,#58636,.T.);
#86702=ORIENTED_EDGE('',*,*,#58626,.T.);
#86703=ORIENTED_EDGE('',*,*,#58631,.T.);
#86704=ORIENTED_EDGE('',*,*,#58637,.T.);
#86705=ORIENTED_EDGE('',*,*,#58635,.F.);
#86706=ORIENTED_EDGE('',*,*,#58622,.T.);
#86707=ORIENTED_EDGE('',*,*,#58638,.T.);
#86708=ORIENTED_EDGE('',*,*,#58621,.T.);
#86709=ORIENTED_EDGE('',*,*,#58618,.T.);
#86710=ORIENTED_EDGE('',*,*,#58638,.F.);
#86711=ORIENTED_EDGE('',*,*,#58625,.T.);
#86712=ORIENTED_EDGE('',*,*,#58620,.T.);
#86713=ORIENTED_EDGE('',*,*,#58639,.F.);
#86714=ORIENTED_EDGE('',*,*,#58639,.T.);
#86715=ORIENTED_EDGE('',*,*,#58624,.T.);
#86716=ORIENTED_EDGE('',*,*,#58634,.F.);
#86717=ORIENTED_EDGE('',*,*,#58627,.F.);
#86718=ORIENTED_EDGE('',*,*,#58636,.F.);
#86719=ORIENTED_EDGE('',*,*,#58637,.F.);
#86720=ORIENTED_EDGE('',*,*,#58630,.T.);
#86721=ORIENTED_EDGE('',*,*,#58632,.F.);
#86722=ORIENTED_EDGE('',*,*,#58633,.F.);
#86723=ORIENTED_EDGE('',*,*,#58640,.F.);
#86724=ORIENTED_EDGE('',*,*,#58641,.T.);
#86725=ORIENTED_EDGE('',*,*,#58642,.F.);
#86726=ORIENTED_EDGE('',*,*,#58641,.F.);
#86727=ORIENTED_EDGE('',*,*,#58643,.F.);
#86728=ORIENTED_EDGE('',*,*,#58644,.F.);
#86729=ORIENTED_EDGE('',*,*,#58645,.T.);
#86730=ORIENTED_EDGE('',*,*,#58646,.F.);
#86731=ORIENTED_EDGE('',*,*,#58647,.F.);
#86732=ORIENTED_EDGE('',*,*,#58645,.F.);
#86733=ORIENTED_EDGE('',*,*,#58648,.F.);
#86734=ORIENTED_EDGE('',*,*,#58649,.T.);
#86735=ORIENTED_EDGE('',*,*,#58650,.T.);
#86736=ORIENTED_EDGE('',*,*,#58651,.T.);
#86737=ORIENTED_EDGE('',*,*,#58649,.F.);
#86738=ORIENTED_EDGE('',*,*,#58652,.F.);
#86739=ORIENTED_EDGE('',*,*,#58653,.T.);
#86740=ORIENTED_EDGE('',*,*,#58643,.T.);
#86741=ORIENTED_EDGE('',*,*,#58640,.T.);
#86742=ORIENTED_EDGE('',*,*,#58653,.F.);
#86743=ORIENTED_EDGE('',*,*,#58648,.T.);
#86744=ORIENTED_EDGE('',*,*,#58646,.T.);
#86745=ORIENTED_EDGE('',*,*,#58647,.T.);
#86746=ORIENTED_EDGE('',*,*,#58654,.T.);
#86747=ORIENTED_EDGE('',*,*,#58655,.T.);
#86748=ORIENTED_EDGE('',*,*,#58654,.F.);
#86749=ORIENTED_EDGE('',*,*,#58651,.F.);
#86750=ORIENTED_EDGE('',*,*,#58650,.F.);
#86751=ORIENTED_EDGE('',*,*,#58655,.F.);
#86752=ORIENTED_EDGE('',*,*,#58652,.T.);
#86753=ORIENTED_EDGE('',*,*,#58644,.T.);
#86754=ORIENTED_EDGE('',*,*,#58642,.T.);
#86755=ORIENTED_EDGE('',*,*,#58656,.F.);
#86756=ORIENTED_EDGE('',*,*,#58657,.T.);
#86757=ORIENTED_EDGE('',*,*,#58658,.F.);
#86758=ORIENTED_EDGE('',*,*,#58657,.F.);
#86759=ORIENTED_EDGE('',*,*,#58659,.F.);
#86760=ORIENTED_EDGE('',*,*,#58660,.T.);
#86761=ORIENTED_EDGE('',*,*,#58661,.F.);
#86762=ORIENTED_EDGE('',*,*,#58662,.F.);
#86763=ORIENTED_EDGE('',*,*,#58660,.F.);
#86764=ORIENTED_EDGE('',*,*,#58663,.F.);
#86765=ORIENTED_EDGE('',*,*,#58664,.F.);
#86766=ORIENTED_EDGE('',*,*,#58665,.T.);
#86767=ORIENTED_EDGE('',*,*,#58666,.F.);
#86768=ORIENTED_EDGE('',*,*,#58665,.F.);
#86769=ORIENTED_EDGE('',*,*,#58667,.F.);
#86770=ORIENTED_EDGE('',*,*,#58668,.T.);
#86771=ORIENTED_EDGE('',*,*,#58669,.F.);
#86772=ORIENTED_EDGE('',*,*,#58668,.F.);
#86773=ORIENTED_EDGE('',*,*,#58670,.F.);
#86774=ORIENTED_EDGE('',*,*,#58671,.T.);
#86775=ORIENTED_EDGE('',*,*,#58672,.F.);
#86776=ORIENTED_EDGE('',*,*,#58671,.F.);
#86777=ORIENTED_EDGE('',*,*,#58673,.F.);
#86778=ORIENTED_EDGE('',*,*,#58674,.T.);
#86779=ORIENTED_EDGE('',*,*,#58675,.T.);
#86780=ORIENTED_EDGE('',*,*,#58674,.F.);
#86781=ORIENTED_EDGE('',*,*,#58658,.T.);
#86782=ORIENTED_EDGE('',*,*,#58676,.T.);
#86783=ORIENTED_EDGE('',*,*,#58667,.T.);
#86784=ORIENTED_EDGE('',*,*,#58676,.F.);
#86785=ORIENTED_EDGE('',*,*,#58672,.T.);
#86786=ORIENTED_EDGE('',*,*,#58677,.T.);
#86787=ORIENTED_EDGE('',*,*,#58673,.T.);
#86788=ORIENTED_EDGE('',*,*,#58677,.F.);
#86789=ORIENTED_EDGE('',*,*,#58678,.T.);
#86790=ORIENTED_EDGE('',*,*,#58679,.T.);
#86791=ORIENTED_EDGE('',*,*,#58661,.T.);
#86792=ORIENTED_EDGE('',*,*,#58662,.T.);
#86793=ORIENTED_EDGE('',*,*,#58679,.F.);
#86794=ORIENTED_EDGE('',*,*,#58663,.T.);
#86795=ORIENTED_EDGE('',*,*,#58664,.T.);
#86796=ORIENTED_EDGE('',*,*,#58680,.T.);
#86797=ORIENTED_EDGE('',*,*,#58681,.T.);
#86798=ORIENTED_EDGE('',*,*,#58680,.F.);
#86799=ORIENTED_EDGE('',*,*,#58682,.F.);
#86800=ORIENTED_EDGE('',*,*,#58683,.T.);
#86801=ORIENTED_EDGE('',*,*,#58684,.T.);
#86802=ORIENTED_EDGE('',*,*,#58683,.F.);
#86803=ORIENTED_EDGE('',*,*,#58684,.F.);
#86804=ORIENTED_EDGE('',*,*,#58675,.F.);
#86805=ORIENTED_EDGE('',*,*,#58682,.T.);
#86806=ORIENTED_EDGE('',*,*,#58681,.F.);
#86807=ORIENTED_EDGE('',*,*,#58659,.T.);
#86808=ORIENTED_EDGE('',*,*,#58666,.T.);
#86809=ORIENTED_EDGE('',*,*,#58670,.T.);
#86810=ORIENTED_EDGE('',*,*,#58669,.T.);
#86811=ORIENTED_EDGE('',*,*,#58656,.T.);
#86812=ORIENTED_EDGE('',*,*,#58678,.F.);
#86813=ORIENTED_EDGE('',*,*,#58685,.F.);
#86814=ORIENTED_EDGE('',*,*,#58686,.T.);
#86815=ORIENTED_EDGE('',*,*,#58687,.T.);
#86816=ORIENTED_EDGE('',*,*,#58688,.F.);
#86817=ORIENTED_EDGE('',*,*,#58689,.F.);
#86818=ORIENTED_EDGE('',*,*,#58690,.T.);
#86819=ORIENTED_EDGE('',*,*,#58685,.T.);
#86820=ORIENTED_EDGE('',*,*,#58691,.F.);
#86821=ORIENTED_EDGE('',*,*,#58692,.F.);
#86822=ORIENTED_EDGE('',*,*,#58693,.T.);
#86823=ORIENTED_EDGE('',*,*,#58689,.T.);
#86824=ORIENTED_EDGE('',*,*,#58694,.F.);
#86825=ORIENTED_EDGE('',*,*,#58695,.F.);
#86826=ORIENTED_EDGE('',*,*,#58696,.T.);
#86827=ORIENTED_EDGE('',*,*,#58692,.T.);
#86828=ORIENTED_EDGE('',*,*,#58697,.F.);
#86829=ORIENTED_EDGE('',*,*,#58698,.F.);
#86830=ORIENTED_EDGE('',*,*,#58699,.T.);
#86831=ORIENTED_EDGE('',*,*,#58695,.T.);
#86832=ORIENTED_EDGE('',*,*,#58700,.F.);
#86833=ORIENTED_EDGE('',*,*,#58701,.F.);
#86834=ORIENTED_EDGE('',*,*,#58702,.T.);
#86835=ORIENTED_EDGE('',*,*,#58698,.T.);
#86836=ORIENTED_EDGE('',*,*,#58703,.F.);
#86837=ORIENTED_EDGE('',*,*,#58704,.F.);
#86838=ORIENTED_EDGE('',*,*,#58705,.F.);
#86839=ORIENTED_EDGE('',*,*,#58706,.T.);
#86840=ORIENTED_EDGE('',*,*,#58707,.F.);
#86841=ORIENTED_EDGE('',*,*,#58708,.F.);
#86842=ORIENTED_EDGE('',*,*,#58704,.T.);
#86843=ORIENTED_EDGE('',*,*,#58709,.T.);
#86844=ORIENTED_EDGE('',*,*,#58710,.F.);
#86845=ORIENTED_EDGE('',*,*,#58711,.F.);
#86846=ORIENTED_EDGE('',*,*,#58712,.F.);
#86847=ORIENTED_EDGE('',*,*,#58707,.T.);
#86848=ORIENTED_EDGE('',*,*,#58713,.F.);
#86849=ORIENTED_EDGE('',*,*,#58714,.F.);
#86850=ORIENTED_EDGE('',*,*,#58715,.F.);
#86851=ORIENTED_EDGE('',*,*,#58711,.T.);
#86852=ORIENTED_EDGE('',*,*,#58716,.F.);
#86853=ORIENTED_EDGE('',*,*,#58717,.F.);
#86854=ORIENTED_EDGE('',*,*,#58718,.F.);
#86855=ORIENTED_EDGE('',*,*,#58714,.T.);
#86856=ORIENTED_EDGE('',*,*,#58719,.F.);
#86857=ORIENTED_EDGE('',*,*,#58720,.F.);
#86858=ORIENTED_EDGE('',*,*,#58721,.F.);
#86859=ORIENTED_EDGE('',*,*,#58717,.T.);
#86860=ORIENTED_EDGE('',*,*,#58722,.F.);
#86861=ORIENTED_EDGE('',*,*,#58723,.F.);
#86862=ORIENTED_EDGE('',*,*,#58724,.F.);
#86863=ORIENTED_EDGE('',*,*,#58720,.T.);
#86864=ORIENTED_EDGE('',*,*,#58725,.F.);
#86865=ORIENTED_EDGE('',*,*,#58726,.F.);
#86866=ORIENTED_EDGE('',*,*,#58727,.T.);
#86867=ORIENTED_EDGE('',*,*,#58728,.F.);
#86868=ORIENTED_EDGE('',*,*,#58723,.T.);
#86869=ORIENTED_EDGE('',*,*,#58729,.F.);
#86870=ORIENTED_EDGE('',*,*,#58706,.F.);
#86871=ORIENTED_EDGE('',*,*,#58730,.F.);
#86872=ORIENTED_EDGE('',*,*,#58731,.F.);
#86873=ORIENTED_EDGE('',*,*,#58732,.F.);
#86874=ORIENTED_EDGE('',*,*,#58709,.F.);
#86875=ORIENTED_EDGE('',*,*,#58733,.T.);
#86876=ORIENTED_EDGE('',*,*,#58734,.F.);
#86877=ORIENTED_EDGE('',*,*,#58733,.F.);
#86878=ORIENTED_EDGE('',*,*,#58735,.F.);
#86879=ORIENTED_EDGE('',*,*,#58736,.F.);
#86880=ORIENTED_EDGE('',*,*,#58687,.F.);
#86881=ORIENTED_EDGE('',*,*,#58737,.F.);
#86882=ORIENTED_EDGE('',*,*,#58727,.F.);
#86883=ORIENTED_EDGE('',*,*,#58738,.F.);
#86884=ORIENTED_EDGE('',*,*,#58739,.T.);
#86885=ORIENTED_EDGE('',*,*,#58740,.F.);
#86886=ORIENTED_EDGE('',*,*,#58739,.F.);
#86887=ORIENTED_EDGE('',*,*,#58726,.T.);
#86888=ORIENTED_EDGE('',*,*,#58741,.F.);
#86889=ORIENTED_EDGE('',*,*,#58735,.T.);
#86890=ORIENTED_EDGE('',*,*,#58738,.T.);
#86891=ORIENTED_EDGE('',*,*,#58734,.T.);
#86892=ORIENTED_EDGE('',*,*,#58740,.T.);
#86893=ORIENTED_EDGE('',*,*,#58742,.F.);
#86894=ORIENTED_EDGE('',*,*,#58743,.F.);
#86895=ORIENTED_EDGE('',*,*,#58744,.F.);
#86896=ORIENTED_EDGE('',*,*,#58745,.F.);
#86897=ORIENTED_EDGE('',*,*,#58746,.F.);
#86898=ORIENTED_EDGE('',*,*,#58747,.F.);
#86899=ORIENTED_EDGE('',*,*,#58742,.T.);
#86900=ORIENTED_EDGE('',*,*,#58748,.F.);
#86901=ORIENTED_EDGE('',*,*,#58747,.T.);
#86902=ORIENTED_EDGE('',*,*,#58749,.F.);
#86903=ORIENTED_EDGE('',*,*,#58746,.T.);
#86904=ORIENTED_EDGE('',*,*,#58750,.F.);
#86905=ORIENTED_EDGE('',*,*,#58745,.T.);
#86906=ORIENTED_EDGE('',*,*,#58751,.F.);
#86907=ORIENTED_EDGE('',*,*,#58744,.T.);
#86908=ORIENTED_EDGE('',*,*,#58752,.F.);
#86909=ORIENTED_EDGE('',*,*,#58743,.T.);
#86910=ORIENTED_EDGE('',*,*,#58753,.F.);
#86911=ORIENTED_EDGE('',*,*,#58754,.T.);
#86912=ORIENTED_EDGE('',*,*,#58755,.T.);
#86913=ORIENTED_EDGE('',*,*,#58756,.T.);
#86914=ORIENTED_EDGE('',*,*,#58757,.T.);
#86915=ORIENTED_EDGE('',*,*,#58758,.T.);
#86916=ORIENTED_EDGE('',*,*,#58759,.T.);
#86917=ORIENTED_EDGE('',*,*,#58760,.T.);
#86918=ORIENTED_EDGE('',*,*,#58748,.T.);
#86919=ORIENTED_EDGE('',*,*,#58761,.F.);
#86920=ORIENTED_EDGE('',*,*,#58755,.F.);
#86921=ORIENTED_EDGE('',*,*,#58761,.T.);
#86922=ORIENTED_EDGE('',*,*,#58749,.T.);
#86923=ORIENTED_EDGE('',*,*,#58762,.F.);
#86924=ORIENTED_EDGE('',*,*,#58756,.F.);
#86925=ORIENTED_EDGE('',*,*,#58762,.T.);
#86926=ORIENTED_EDGE('',*,*,#58750,.T.);
#86927=ORIENTED_EDGE('',*,*,#58763,.F.);
#86928=ORIENTED_EDGE('',*,*,#58757,.F.);
#86929=ORIENTED_EDGE('',*,*,#58763,.T.);
#86930=ORIENTED_EDGE('',*,*,#58751,.T.);
#86931=ORIENTED_EDGE('',*,*,#58764,.F.);
#86932=ORIENTED_EDGE('',*,*,#58758,.F.);
#86933=ORIENTED_EDGE('',*,*,#58764,.T.);
#86934=ORIENTED_EDGE('',*,*,#58752,.T.);
#86935=ORIENTED_EDGE('',*,*,#58765,.F.);
#86936=ORIENTED_EDGE('',*,*,#58759,.F.);
#86937=ORIENTED_EDGE('',*,*,#58765,.T.);
#86938=ORIENTED_EDGE('',*,*,#58753,.T.);
#86939=ORIENTED_EDGE('',*,*,#58760,.F.);
#86940=ORIENTED_EDGE('',*,*,#58754,.F.);
#86941=ORIENTED_EDGE('',*,*,#58736,.T.);
#86942=ORIENTED_EDGE('',*,*,#58741,.T.);
#86943=ORIENTED_EDGE('',*,*,#58729,.T.);
#86944=ORIENTED_EDGE('',*,*,#58725,.T.);
#86945=ORIENTED_EDGE('',*,*,#58722,.T.);
#86946=ORIENTED_EDGE('',*,*,#58719,.T.);
#86947=ORIENTED_EDGE('',*,*,#58716,.T.);
#86948=ORIENTED_EDGE('',*,*,#58713,.T.);
#86949=ORIENTED_EDGE('',*,*,#58710,.T.);
#86950=ORIENTED_EDGE('',*,*,#58732,.T.);
#86951=ORIENTED_EDGE('',*,*,#58766,.T.);
#86952=ORIENTED_EDGE('',*,*,#58703,.T.);
#86953=ORIENTED_EDGE('',*,*,#58700,.T.);
#86954=ORIENTED_EDGE('',*,*,#58697,.T.);
#86955=ORIENTED_EDGE('',*,*,#58694,.T.);
#86956=ORIENTED_EDGE('',*,*,#58691,.T.);
#86957=ORIENTED_EDGE('',*,*,#58688,.T.);
#86958=ORIENTED_EDGE('',*,*,#58701,.T.);
#86959=ORIENTED_EDGE('',*,*,#58766,.F.);
#86960=ORIENTED_EDGE('',*,*,#58731,.T.);
#86961=ORIENTED_EDGE('',*,*,#58767,.T.);
#86962=ORIENTED_EDGE('',*,*,#58737,.T.);
#86963=ORIENTED_EDGE('',*,*,#58686,.F.);
#86964=ORIENTED_EDGE('',*,*,#58690,.F.);
#86965=ORIENTED_EDGE('',*,*,#58693,.F.);
#86966=ORIENTED_EDGE('',*,*,#58696,.F.);
#86967=ORIENTED_EDGE('',*,*,#58699,.F.);
#86968=ORIENTED_EDGE('',*,*,#58702,.F.);
#86969=ORIENTED_EDGE('',*,*,#58767,.F.);
#86970=ORIENTED_EDGE('',*,*,#58730,.T.);
#86971=ORIENTED_EDGE('',*,*,#58705,.T.);
#86972=ORIENTED_EDGE('',*,*,#58708,.T.);
#86973=ORIENTED_EDGE('',*,*,#58712,.T.);
#86974=ORIENTED_EDGE('',*,*,#58715,.T.);
#86975=ORIENTED_EDGE('',*,*,#58718,.T.);
#86976=ORIENTED_EDGE('',*,*,#58721,.T.);
#86977=ORIENTED_EDGE('',*,*,#58724,.T.);
#86978=ORIENTED_EDGE('',*,*,#58728,.T.);
#86979=ORIENTED_EDGE('',*,*,#58768,.F.);
#86980=ORIENTED_EDGE('',*,*,#58769,.T.);
#86981=ORIENTED_EDGE('',*,*,#58770,.T.);
#86982=ORIENTED_EDGE('',*,*,#58771,.F.);
#86983=ORIENTED_EDGE('',*,*,#58772,.F.);
#86984=ORIENTED_EDGE('',*,*,#58773,.T.);
#86985=ORIENTED_EDGE('',*,*,#58768,.T.);
#86986=ORIENTED_EDGE('',*,*,#58774,.F.);
#86987=ORIENTED_EDGE('',*,*,#58775,.F.);
#86988=ORIENTED_EDGE('',*,*,#58776,.T.);
#86989=ORIENTED_EDGE('',*,*,#58772,.T.);
#86990=ORIENTED_EDGE('',*,*,#58777,.F.);
#86991=ORIENTED_EDGE('',*,*,#58778,.F.);
#86992=ORIENTED_EDGE('',*,*,#58779,.T.);
#86993=ORIENTED_EDGE('',*,*,#58775,.T.);
#86994=ORIENTED_EDGE('',*,*,#58780,.F.);
#86995=ORIENTED_EDGE('',*,*,#58781,.F.);
#86996=ORIENTED_EDGE('',*,*,#58782,.T.);
#86997=ORIENTED_EDGE('',*,*,#58778,.T.);
#86998=ORIENTED_EDGE('',*,*,#58783,.F.);
#86999=ORIENTED_EDGE('',*,*,#58784,.F.);
#87000=ORIENTED_EDGE('',*,*,#58785,.T.);
#87001=ORIENTED_EDGE('',*,*,#58781,.T.);
#87002=ORIENTED_EDGE('',*,*,#58786,.F.);
#87003=ORIENTED_EDGE('',*,*,#58787,.F.);
#87004=ORIENTED_EDGE('',*,*,#58788,.F.);
#87005=ORIENTED_EDGE('',*,*,#58789,.T.);
#87006=ORIENTED_EDGE('',*,*,#58790,.F.);
#87007=ORIENTED_EDGE('',*,*,#58791,.F.);
#87008=ORIENTED_EDGE('',*,*,#58787,.T.);
#87009=ORIENTED_EDGE('',*,*,#58792,.T.);
#87010=ORIENTED_EDGE('',*,*,#58793,.F.);
#87011=ORIENTED_EDGE('',*,*,#58794,.F.);
#87012=ORIENTED_EDGE('',*,*,#58795,.F.);
#87013=ORIENTED_EDGE('',*,*,#58790,.T.);
#87014=ORIENTED_EDGE('',*,*,#58796,.F.);
#87015=ORIENTED_EDGE('',*,*,#58797,.F.);
#87016=ORIENTED_EDGE('',*,*,#58798,.F.);
#87017=ORIENTED_EDGE('',*,*,#58794,.T.);
#87018=ORIENTED_EDGE('',*,*,#58799,.F.);
#87019=ORIENTED_EDGE('',*,*,#58800,.F.);
#87020=ORIENTED_EDGE('',*,*,#58801,.F.);
#87021=ORIENTED_EDGE('',*,*,#58797,.T.);
#87022=ORIENTED_EDGE('',*,*,#58802,.F.);
#87023=ORIENTED_EDGE('',*,*,#58803,.F.);
#87024=ORIENTED_EDGE('',*,*,#58804,.F.);
#87025=ORIENTED_EDGE('',*,*,#58800,.T.);
#87026=ORIENTED_EDGE('',*,*,#58805,.F.);
#87027=ORIENTED_EDGE('',*,*,#58806,.F.);
#87028=ORIENTED_EDGE('',*,*,#58807,.F.);
#87029=ORIENTED_EDGE('',*,*,#58803,.T.);
#87030=ORIENTED_EDGE('',*,*,#58808,.F.);
#87031=ORIENTED_EDGE('',*,*,#58809,.F.);
#87032=ORIENTED_EDGE('',*,*,#58810,.T.);
#87033=ORIENTED_EDGE('',*,*,#58811,.F.);
#87034=ORIENTED_EDGE('',*,*,#58806,.T.);
#87035=ORIENTED_EDGE('',*,*,#58812,.F.);
#87036=ORIENTED_EDGE('',*,*,#58789,.F.);
#87037=ORIENTED_EDGE('',*,*,#58813,.F.);
#87038=ORIENTED_EDGE('',*,*,#58814,.F.);
#87039=ORIENTED_EDGE('',*,*,#58815,.F.);
#87040=ORIENTED_EDGE('',*,*,#58792,.F.);
#87041=ORIENTED_EDGE('',*,*,#58816,.T.);
#87042=ORIENTED_EDGE('',*,*,#58817,.F.);
#87043=ORIENTED_EDGE('',*,*,#58816,.F.);
#87044=ORIENTED_EDGE('',*,*,#58818,.F.);
#87045=ORIENTED_EDGE('',*,*,#58819,.F.);
#87046=ORIENTED_EDGE('',*,*,#58770,.F.);
#87047=ORIENTED_EDGE('',*,*,#58820,.F.);
#87048=ORIENTED_EDGE('',*,*,#58810,.F.);
#87049=ORIENTED_EDGE('',*,*,#58821,.F.);
#87050=ORIENTED_EDGE('',*,*,#58822,.T.);
#87051=ORIENTED_EDGE('',*,*,#58823,.F.);
#87052=ORIENTED_EDGE('',*,*,#58822,.F.);
#87053=ORIENTED_EDGE('',*,*,#58809,.T.);
#87054=ORIENTED_EDGE('',*,*,#58824,.F.);
#87055=ORIENTED_EDGE('',*,*,#58818,.T.);
#87056=ORIENTED_EDGE('',*,*,#58821,.T.);
#87057=ORIENTED_EDGE('',*,*,#58817,.T.);
#87058=ORIENTED_EDGE('',*,*,#58823,.T.);
#87059=ORIENTED_EDGE('',*,*,#58825,.F.);
#87060=ORIENTED_EDGE('',*,*,#58826,.F.);
#87061=ORIENTED_EDGE('',*,*,#58827,.F.);
#87062=ORIENTED_EDGE('',*,*,#58828,.F.);
#87063=ORIENTED_EDGE('',*,*,#58829,.F.);
#87064=ORIENTED_EDGE('',*,*,#58830,.F.);
#87065=ORIENTED_EDGE('',*,*,#58825,.T.);
#87066=ORIENTED_EDGE('',*,*,#58831,.F.);
#87067=ORIENTED_EDGE('',*,*,#58830,.T.);
#87068=ORIENTED_EDGE('',*,*,#58832,.F.);
#87069=ORIENTED_EDGE('',*,*,#58829,.T.);
#87070=ORIENTED_EDGE('',*,*,#58833,.F.);
#87071=ORIENTED_EDGE('',*,*,#58828,.T.);
#87072=ORIENTED_EDGE('',*,*,#58834,.F.);
#87073=ORIENTED_EDGE('',*,*,#58827,.T.);
#87074=ORIENTED_EDGE('',*,*,#58835,.F.);
#87075=ORIENTED_EDGE('',*,*,#58826,.T.);
#87076=ORIENTED_EDGE('',*,*,#58836,.F.);
#87077=ORIENTED_EDGE('',*,*,#58837,.T.);
#87078=ORIENTED_EDGE('',*,*,#58838,.T.);
#87079=ORIENTED_EDGE('',*,*,#58839,.T.);
#87080=ORIENTED_EDGE('',*,*,#58840,.T.);
#87081=ORIENTED_EDGE('',*,*,#58841,.T.);
#87082=ORIENTED_EDGE('',*,*,#58842,.T.);
#87083=ORIENTED_EDGE('',*,*,#58843,.T.);
#87084=ORIENTED_EDGE('',*,*,#58831,.T.);
#87085=ORIENTED_EDGE('',*,*,#58844,.F.);
#87086=ORIENTED_EDGE('',*,*,#58838,.F.);
#87087=ORIENTED_EDGE('',*,*,#58844,.T.);
#87088=ORIENTED_EDGE('',*,*,#58832,.T.);
#87089=ORIENTED_EDGE('',*,*,#58845,.F.);
#87090=ORIENTED_EDGE('',*,*,#58839,.F.);
#87091=ORIENTED_EDGE('',*,*,#58845,.T.);
#87092=ORIENTED_EDGE('',*,*,#58833,.T.);
#87093=ORIENTED_EDGE('',*,*,#58846,.F.);
#87094=ORIENTED_EDGE('',*,*,#58840,.F.);
#87095=ORIENTED_EDGE('',*,*,#58846,.T.);
#87096=ORIENTED_EDGE('',*,*,#58834,.T.);
#87097=ORIENTED_EDGE('',*,*,#58847,.F.);
#87098=ORIENTED_EDGE('',*,*,#58841,.F.);
#87099=ORIENTED_EDGE('',*,*,#58847,.T.);
#87100=ORIENTED_EDGE('',*,*,#58835,.T.);
#87101=ORIENTED_EDGE('',*,*,#58848,.F.);
#87102=ORIENTED_EDGE('',*,*,#58842,.F.);
#87103=ORIENTED_EDGE('',*,*,#58848,.T.);
#87104=ORIENTED_EDGE('',*,*,#58836,.T.);
#87105=ORIENTED_EDGE('',*,*,#58843,.F.);
#87106=ORIENTED_EDGE('',*,*,#58837,.F.);
#87107=ORIENTED_EDGE('',*,*,#58819,.T.);
#87108=ORIENTED_EDGE('',*,*,#58824,.T.);
#87109=ORIENTED_EDGE('',*,*,#58812,.T.);
#87110=ORIENTED_EDGE('',*,*,#58808,.T.);
#87111=ORIENTED_EDGE('',*,*,#58805,.T.);
#87112=ORIENTED_EDGE('',*,*,#58802,.T.);
#87113=ORIENTED_EDGE('',*,*,#58799,.T.);
#87114=ORIENTED_EDGE('',*,*,#58796,.T.);
#87115=ORIENTED_EDGE('',*,*,#58793,.T.);
#87116=ORIENTED_EDGE('',*,*,#58815,.T.);
#87117=ORIENTED_EDGE('',*,*,#58849,.T.);
#87118=ORIENTED_EDGE('',*,*,#58786,.T.);
#87119=ORIENTED_EDGE('',*,*,#58783,.T.);
#87120=ORIENTED_EDGE('',*,*,#58780,.T.);
#87121=ORIENTED_EDGE('',*,*,#58777,.T.);
#87122=ORIENTED_EDGE('',*,*,#58774,.T.);
#87123=ORIENTED_EDGE('',*,*,#58771,.T.);
#87124=ORIENTED_EDGE('',*,*,#58784,.T.);
#87125=ORIENTED_EDGE('',*,*,#58849,.F.);
#87126=ORIENTED_EDGE('',*,*,#58814,.T.);
#87127=ORIENTED_EDGE('',*,*,#58850,.T.);
#87128=ORIENTED_EDGE('',*,*,#58820,.T.);
#87129=ORIENTED_EDGE('',*,*,#58769,.F.);
#87130=ORIENTED_EDGE('',*,*,#58773,.F.);
#87131=ORIENTED_EDGE('',*,*,#58776,.F.);
#87132=ORIENTED_EDGE('',*,*,#58779,.F.);
#87133=ORIENTED_EDGE('',*,*,#58782,.F.);
#87134=ORIENTED_EDGE('',*,*,#58785,.F.);
#87135=ORIENTED_EDGE('',*,*,#58850,.F.);
#87136=ORIENTED_EDGE('',*,*,#58813,.T.);
#87137=ORIENTED_EDGE('',*,*,#58788,.T.);
#87138=ORIENTED_EDGE('',*,*,#58791,.T.);
#87139=ORIENTED_EDGE('',*,*,#58795,.T.);
#87140=ORIENTED_EDGE('',*,*,#58798,.T.);
#87141=ORIENTED_EDGE('',*,*,#58801,.T.);
#87142=ORIENTED_EDGE('',*,*,#58804,.T.);
#87143=ORIENTED_EDGE('',*,*,#58807,.T.);
#87144=ORIENTED_EDGE('',*,*,#58811,.T.);
#87145=ORIENTED_EDGE('',*,*,#58851,.F.);
#87146=ORIENTED_EDGE('',*,*,#58852,.T.);
#87147=ORIENTED_EDGE('',*,*,#58853,.F.);
#87148=ORIENTED_EDGE('',*,*,#58852,.F.);
#87149=ORIENTED_EDGE('',*,*,#58854,.F.);
#87150=ORIENTED_EDGE('',*,*,#58855,.F.);
#87151=ORIENTED_EDGE('',*,*,#58856,.T.);
#87152=ORIENTED_EDGE('',*,*,#58857,.F.);
#87153=ORIENTED_EDGE('',*,*,#58856,.F.);
#87154=ORIENTED_EDGE('',*,*,#58858,.F.);
#87155=ORIENTED_EDGE('',*,*,#58859,.T.);
#87156=ORIENTED_EDGE('',*,*,#58860,.F.);
#87157=ORIENTED_EDGE('',*,*,#58859,.F.);
#87158=ORIENTED_EDGE('',*,*,#58861,.F.);
#87159=ORIENTED_EDGE('',*,*,#58862,.F.);
#87160=ORIENTED_EDGE('',*,*,#58863,.T.);
#87161=ORIENTED_EDGE('',*,*,#58864,.F.);
#87162=ORIENTED_EDGE('',*,*,#58863,.F.);
#87163=ORIENTED_EDGE('',*,*,#58861,.T.);
#87164=ORIENTED_EDGE('',*,*,#58862,.T.);
#87165=ORIENTED_EDGE('',*,*,#58865,.T.);
#87166=ORIENTED_EDGE('',*,*,#58866,.F.);
#87167=ORIENTED_EDGE('',*,*,#58867,.T.);
#87168=ORIENTED_EDGE('',*,*,#58858,.T.);
#87169=ORIENTED_EDGE('',*,*,#58867,.F.);
#87170=ORIENTED_EDGE('',*,*,#58868,.F.);
#87171=ORIENTED_EDGE('',*,*,#58865,.F.);
#87172=ORIENTED_EDGE('',*,*,#58869,.F.);
#87173=ORIENTED_EDGE('',*,*,#58870,.F.);
#87174=ORIENTED_EDGE('',*,*,#58869,.T.);
#87175=ORIENTED_EDGE('',*,*,#58871,.T.);
#87176=ORIENTED_EDGE('',*,*,#58872,.F.);
#87177=ORIENTED_EDGE('',*,*,#58871,.F.);
#87178=ORIENTED_EDGE('',*,*,#58870,.T.);
#87179=ORIENTED_EDGE('',*,*,#58866,.T.);
#87180=ORIENTED_EDGE('',*,*,#58868,.T.);
#87181=ORIENTED_EDGE('',*,*,#58873,.T.);
#87182=ORIENTED_EDGE('',*,*,#58874,.F.);
#87183=ORIENTED_EDGE('',*,*,#58875,.F.);
#87184=ORIENTED_EDGE('',*,*,#58873,.F.);
#87185=ORIENTED_EDGE('',*,*,#58854,.T.);
#87186=ORIENTED_EDGE('',*,*,#58855,.T.);
#87187=ORIENTED_EDGE('',*,*,#58876,.T.);
#87188=ORIENTED_EDGE('',*,*,#58875,.T.);
#87189=ORIENTED_EDGE('',*,*,#58877,.T.);
#87190=ORIENTED_EDGE('',*,*,#58851,.T.);
#87191=ORIENTED_EDGE('',*,*,#58877,.F.);
#87192=ORIENTED_EDGE('',*,*,#58874,.T.);
#87193=ORIENTED_EDGE('',*,*,#58876,.F.);
#87194=ORIENTED_EDGE('',*,*,#58872,.T.);
#87195=ORIENTED_EDGE('',*,*,#58860,.T.);
#87196=ORIENTED_EDGE('',*,*,#58857,.T.);
#87197=ORIENTED_EDGE('',*,*,#58864,.T.);
#87198=ORIENTED_EDGE('',*,*,#58853,.T.);
#87199=ORIENTED_EDGE('',*,*,#58878,.F.);
#87200=ORIENTED_EDGE('',*,*,#58879,.T.);
#87201=ORIENTED_EDGE('',*,*,#58880,.T.);
#87202=ORIENTED_EDGE('',*,*,#58879,.F.);
#87203=ORIENTED_EDGE('',*,*,#58881,.T.);
#87204=ORIENTED_EDGE('',*,*,#58882,.T.);
#87205=ORIENTED_EDGE('',*,*,#58883,.F.);
#87206=ORIENTED_EDGE('',*,*,#58882,.F.);
#87207=ORIENTED_EDGE('',*,*,#58884,.F.);
#87208=ORIENTED_EDGE('',*,*,#58885,.T.);
#87209=ORIENTED_EDGE('',*,*,#58886,.F.);
#87210=ORIENTED_EDGE('',*,*,#58887,.F.);
#87211=ORIENTED_EDGE('',*,*,#58885,.F.);
#87212=ORIENTED_EDGE('',*,*,#58888,.T.);
#87213=ORIENTED_EDGE('',*,*,#58889,.T.);
#87214=ORIENTED_EDGE('',*,*,#58886,.T.);
#87215=ORIENTED_EDGE('',*,*,#58887,.T.);
#87216=ORIENTED_EDGE('',*,*,#58889,.F.);
#87217=ORIENTED_EDGE('',*,*,#58890,.T.);
#87218=ORIENTED_EDGE('',*,*,#58891,.F.);
#87219=ORIENTED_EDGE('',*,*,#58892,.T.);
#87220=ORIENTED_EDGE('',*,*,#58893,.T.);
#87221=ORIENTED_EDGE('',*,*,#58894,.T.);
#87222=ORIENTED_EDGE('',*,*,#58895,.T.);
#87223=ORIENTED_EDGE('',*,*,#58896,.F.);
#87224=ORIENTED_EDGE('',*,*,#58895,.F.);
#87225=ORIENTED_EDGE('',*,*,#58897,.F.);
#87226=ORIENTED_EDGE('',*,*,#58898,.T.);
#87227=ORIENTED_EDGE('',*,*,#58899,.T.);
#87228=ORIENTED_EDGE('',*,*,#58898,.F.);
#87229=ORIENTED_EDGE('',*,*,#58900,.F.);
#87230=ORIENTED_EDGE('',*,*,#58901,.T.);
#87231=ORIENTED_EDGE('',*,*,#58902,.T.);
#87232=ORIENTED_EDGE('',*,*,#58901,.F.);
#87233=ORIENTED_EDGE('',*,*,#58903,.F.);
#87234=ORIENTED_EDGE('',*,*,#58904,.T.);
#87235=ORIENTED_EDGE('',*,*,#58905,.T.);
#87236=ORIENTED_EDGE('',*,*,#58904,.F.);
#87237=ORIENTED_EDGE('',*,*,#58906,.F.);
#87238=ORIENTED_EDGE('',*,*,#58907,.T.);
#87239=ORIENTED_EDGE('',*,*,#58908,.T.);
#87240=ORIENTED_EDGE('',*,*,#58907,.F.);
#87241=ORIENTED_EDGE('',*,*,#58909,.F.);
#87242=ORIENTED_EDGE('',*,*,#58910,.T.);
#87243=ORIENTED_EDGE('',*,*,#58911,.T.);
#87244=ORIENTED_EDGE('',*,*,#58910,.F.);
#87245=ORIENTED_EDGE('',*,*,#58912,.T.);
#87246=ORIENTED_EDGE('',*,*,#58913,.T.);
#87247=ORIENTED_EDGE('',*,*,#58914,.F.);
#87248=ORIENTED_EDGE('',*,*,#58913,.F.);
#87249=ORIENTED_EDGE('',*,*,#58915,.T.);
#87250=ORIENTED_EDGE('',*,*,#58916,.T.);
#87251=ORIENTED_EDGE('',*,*,#58917,.F.);
#87252=ORIENTED_EDGE('',*,*,#58916,.F.);
#87253=ORIENTED_EDGE('',*,*,#58918,.T.);
#87254=ORIENTED_EDGE('',*,*,#58919,.T.);
#87255=ORIENTED_EDGE('',*,*,#58920,.F.);
#87256=ORIENTED_EDGE('',*,*,#58919,.F.);
#87257=ORIENTED_EDGE('',*,*,#58921,.T.);
#87258=ORIENTED_EDGE('',*,*,#58922,.T.);
#87259=ORIENTED_EDGE('',*,*,#58923,.F.);
#87260=ORIENTED_EDGE('',*,*,#58922,.F.);
#87261=ORIENTED_EDGE('',*,*,#58924,.T.);
#87262=ORIENTED_EDGE('',*,*,#58925,.T.);
#87263=ORIENTED_EDGE('',*,*,#58926,.F.);
#87264=ORIENTED_EDGE('',*,*,#58927,.F.);
#87265=ORIENTED_EDGE('',*,*,#58926,.T.);
#87266=ORIENTED_EDGE('',*,*,#58928,.T.);
#87267=ORIENTED_EDGE('',*,*,#58929,.F.);
#87268=ORIENTED_EDGE('',*,*,#58930,.F.);
#87269=ORIENTED_EDGE('',*,*,#58929,.T.);
#87270=ORIENTED_EDGE('',*,*,#58931,.T.);
#87271=ORIENTED_EDGE('',*,*,#58932,.F.);
#87272=ORIENTED_EDGE('',*,*,#58933,.F.);
#87273=ORIENTED_EDGE('',*,*,#58932,.T.);
#87274=ORIENTED_EDGE('',*,*,#58934,.T.);
#87275=ORIENTED_EDGE('',*,*,#58935,.F.);
#87276=ORIENTED_EDGE('',*,*,#58936,.F.);
#87277=ORIENTED_EDGE('',*,*,#58935,.T.);
#87278=ORIENTED_EDGE('',*,*,#58937,.T.);
#87279=ORIENTED_EDGE('',*,*,#58938,.F.);
#87280=ORIENTED_EDGE('',*,*,#58939,.F.);
#87281=ORIENTED_EDGE('',*,*,#58938,.T.);
#87282=ORIENTED_EDGE('',*,*,#58940,.T.);
#87283=ORIENTED_EDGE('',*,*,#58941,.F.);
#87284=ORIENTED_EDGE('',*,*,#58942,.F.);
#87285=ORIENTED_EDGE('',*,*,#58941,.T.);
#87286=ORIENTED_EDGE('',*,*,#58943,.T.);
#87287=ORIENTED_EDGE('',*,*,#58944,.F.);
#87288=ORIENTED_EDGE('',*,*,#58945,.F.);
#87289=ORIENTED_EDGE('',*,*,#58944,.T.);
#87290=ORIENTED_EDGE('',*,*,#58946,.T.);
#87291=ORIENTED_EDGE('',*,*,#58924,.F.);
#87292=ORIENTED_EDGE('',*,*,#58947,.F.);
#87293=ORIENTED_EDGE('',*,*,#58948,.T.);
#87294=ORIENTED_EDGE('',*,*,#58949,.T.);
#87295=ORIENTED_EDGE('',*,*,#58950,.T.);
#87296=ORIENTED_EDGE('',*,*,#58951,.T.);
#87297=ORIENTED_EDGE('',*,*,#58952,.T.);
#87298=ORIENTED_EDGE('',*,*,#58953,.T.);
#87299=ORIENTED_EDGE('',*,*,#58954,.T.);
#87300=ORIENTED_EDGE('',*,*,#58955,.T.);
#87301=ORIENTED_EDGE('',*,*,#58900,.T.);
#87302=ORIENTED_EDGE('',*,*,#58903,.T.);
#87303=ORIENTED_EDGE('',*,*,#58906,.T.);
#87304=ORIENTED_EDGE('',*,*,#58909,.T.);
#87305=ORIENTED_EDGE('',*,*,#58896,.T.);
#87306=ORIENTED_EDGE('',*,*,#58911,.F.);
#87307=ORIENTED_EDGE('',*,*,#58914,.T.);
#87308=ORIENTED_EDGE('',*,*,#58908,.F.);
#87309=ORIENTED_EDGE('',*,*,#58917,.T.);
#87310=ORIENTED_EDGE('',*,*,#58905,.F.);
#87311=ORIENTED_EDGE('',*,*,#58920,.T.);
#87312=ORIENTED_EDGE('',*,*,#58902,.F.);
#87313=ORIENTED_EDGE('',*,*,#58923,.T.);
#87314=ORIENTED_EDGE('',*,*,#58956,.F.);
#87315=ORIENTED_EDGE('',*,*,#58957,.F.);
#87316=ORIENTED_EDGE('',*,*,#58958,.F.);
#87317=ORIENTED_EDGE('',*,*,#58959,.F.);
#87318=ORIENTED_EDGE('',*,*,#58960,.F.);
#87319=ORIENTED_EDGE('',*,*,#58961,.F.);
#87320=ORIENTED_EDGE('',*,*,#58962,.F.);
#87321=ORIENTED_EDGE('',*,*,#58963,.F.);
#87322=ORIENTED_EDGE('',*,*,#58947,.T.);
#87323=ORIENTED_EDGE('',*,*,#58927,.T.);
#87324=ORIENTED_EDGE('',*,*,#58930,.T.);
#87325=ORIENTED_EDGE('',*,*,#58933,.T.);
#87326=ORIENTED_EDGE('',*,*,#58936,.T.);
#87327=ORIENTED_EDGE('',*,*,#58939,.T.);
#87328=ORIENTED_EDGE('',*,*,#58942,.T.);
#87329=ORIENTED_EDGE('',*,*,#58945,.T.);
#87330=ORIENTED_EDGE('',*,*,#58956,.T.);
#87331=ORIENTED_EDGE('',*,*,#58964,.F.);
#87332=ORIENTED_EDGE('',*,*,#58965,.F.);
#87333=ORIENTED_EDGE('',*,*,#58966,.T.);
#87334=ORIENTED_EDGE('',*,*,#58963,.T.);
#87335=ORIENTED_EDGE('',*,*,#58967,.F.);
#87336=ORIENTED_EDGE('',*,*,#58968,.F.);
#87337=ORIENTED_EDGE('',*,*,#58964,.T.);
#87338=ORIENTED_EDGE('',*,*,#58962,.T.);
#87339=ORIENTED_EDGE('',*,*,#58969,.F.);
#87340=ORIENTED_EDGE('',*,*,#58970,.F.);
#87341=ORIENTED_EDGE('',*,*,#58967,.T.);
#87342=ORIENTED_EDGE('',*,*,#58961,.T.);
#87343=ORIENTED_EDGE('',*,*,#58971,.F.);
#87344=ORIENTED_EDGE('',*,*,#58972,.F.);
#87345=ORIENTED_EDGE('',*,*,#58969,.T.);
#87346=ORIENTED_EDGE('',*,*,#58960,.T.);
#87347=ORIENTED_EDGE('',*,*,#58973,.F.);
#87348=ORIENTED_EDGE('',*,*,#58974,.F.);
#87349=ORIENTED_EDGE('',*,*,#58971,.T.);
#87350=ORIENTED_EDGE('',*,*,#58959,.T.);
#87351=ORIENTED_EDGE('',*,*,#58975,.F.);
#87352=ORIENTED_EDGE('',*,*,#58976,.F.);
#87353=ORIENTED_EDGE('',*,*,#58973,.T.);
#87354=ORIENTED_EDGE('',*,*,#58958,.T.);
#87355=ORIENTED_EDGE('',*,*,#58977,.F.);
#87356=ORIENTED_EDGE('',*,*,#58978,.F.);
#87357=ORIENTED_EDGE('',*,*,#58975,.T.);
#87358=ORIENTED_EDGE('',*,*,#58957,.T.);
#87359=ORIENTED_EDGE('',*,*,#58966,.F.);
#87360=ORIENTED_EDGE('',*,*,#58979,.F.);
#87361=ORIENTED_EDGE('',*,*,#58977,.T.);
#87362=ORIENTED_EDGE('',*,*,#58980,.F.);
#87363=ORIENTED_EDGE('',*,*,#58953,.F.);
#87364=ORIENTED_EDGE('',*,*,#58981,.F.);
#87365=ORIENTED_EDGE('',*,*,#58937,.F.);
#87366=ORIENTED_EDGE('',*,*,#58981,.T.);
#87367=ORIENTED_EDGE('',*,*,#58952,.F.);
#87368=ORIENTED_EDGE('',*,*,#58982,.F.);
#87369=ORIENTED_EDGE('',*,*,#58940,.F.);
#87370=ORIENTED_EDGE('',*,*,#58980,.T.);
#87371=ORIENTED_EDGE('',*,*,#58934,.F.);
#87372=ORIENTED_EDGE('',*,*,#58983,.F.);
#87373=ORIENTED_EDGE('',*,*,#58954,.F.);
#87374=ORIENTED_EDGE('',*,*,#58982,.T.);
#87375=ORIENTED_EDGE('',*,*,#58951,.F.);
#87376=ORIENTED_EDGE('',*,*,#58984,.F.);
#87377=ORIENTED_EDGE('',*,*,#58943,.F.);
#87378=ORIENTED_EDGE('',*,*,#58983,.T.);
#87379=ORIENTED_EDGE('',*,*,#58931,.F.);
#87380=ORIENTED_EDGE('',*,*,#58985,.F.);
#87381=ORIENTED_EDGE('',*,*,#58955,.F.);
#87382=ORIENTED_EDGE('',*,*,#58984,.T.);
#87383=ORIENTED_EDGE('',*,*,#58950,.F.);
#87384=ORIENTED_EDGE('',*,*,#58986,.F.);
#87385=ORIENTED_EDGE('',*,*,#58946,.F.);
#87386=ORIENTED_EDGE('',*,*,#58985,.T.);
#87387=ORIENTED_EDGE('',*,*,#58928,.F.);
#87388=ORIENTED_EDGE('',*,*,#58987,.F.);
#87389=ORIENTED_EDGE('',*,*,#58948,.F.);
#87390=ORIENTED_EDGE('',*,*,#58986,.T.);
#87391=ORIENTED_EDGE('',*,*,#58949,.F.);
#87392=ORIENTED_EDGE('',*,*,#58987,.T.);
#87393=ORIENTED_EDGE('',*,*,#58925,.F.);
#87394=ORIENTED_EDGE('',*,*,#58965,.T.);
#87395=ORIENTED_EDGE('',*,*,#58968,.T.);
#87396=ORIENTED_EDGE('',*,*,#58970,.T.);
#87397=ORIENTED_EDGE('',*,*,#58972,.T.);
#87398=ORIENTED_EDGE('',*,*,#58974,.T.);
#87399=ORIENTED_EDGE('',*,*,#58976,.T.);
#87400=ORIENTED_EDGE('',*,*,#58978,.T.);
#87401=ORIENTED_EDGE('',*,*,#58979,.T.);
#87402=ORIENTED_EDGE('',*,*,#58912,.F.);
#87403=ORIENTED_EDGE('',*,*,#58918,.F.);
#87404=ORIENTED_EDGE('',*,*,#58899,.F.);
#87405=ORIENTED_EDGE('',*,*,#58915,.F.);
#87406=ORIENTED_EDGE('',*,*,#58921,.F.);
#87407=ORIENTED_EDGE('',*,*,#58988,.T.);
#87408=ORIENTED_EDGE('',*,*,#58989,.T.);
#87409=ORIENTED_EDGE('',*,*,#58990,.F.);
#87410=ORIENTED_EDGE('',*,*,#58991,.T.);
#87411=ORIENTED_EDGE('',*,*,#58884,.T.);
#87412=ORIENTED_EDGE('',*,*,#58992,.T.);
#87413=ORIENTED_EDGE('',*,*,#58993,.T.);
#87414=ORIENTED_EDGE('',*,*,#58994,.T.);
#87415=ORIENTED_EDGE('',*,*,#58890,.F.);
#87416=ORIENTED_EDGE('',*,*,#58995,.F.);
#87417=ORIENTED_EDGE('',*,*,#58996,.F.);
#87418=ORIENTED_EDGE('',*,*,#58997,.F.);
#87419=ORIENTED_EDGE('',*,*,#58989,.F.);
#87420=ORIENTED_EDGE('',*,*,#58894,.F.);
#87421=ORIENTED_EDGE('',*,*,#58883,.T.);
#87422=ORIENTED_EDGE('',*,*,#58897,.T.);
#87423=ORIENTED_EDGE('',*,*,#58888,.F.);
#87424=ORIENTED_EDGE('',*,*,#58878,.T.);
#87425=ORIENTED_EDGE('',*,*,#58881,.F.);
#87426=ORIENTED_EDGE('',*,*,#58996,.T.);
#87427=ORIENTED_EDGE('',*,*,#58998,.F.);
#87428=ORIENTED_EDGE('',*,*,#58999,.F.);
#87429=ORIENTED_EDGE('',*,*,#59000,.T.);
#87430=ORIENTED_EDGE('',*,*,#58997,.T.);
#87431=ORIENTED_EDGE('',*,*,#59000,.F.);
#87432=ORIENTED_EDGE('',*,*,#59001,.F.);
#87433=ORIENTED_EDGE('',*,*,#58990,.T.);
#87434=ORIENTED_EDGE('',*,*,#58995,.T.);
#87435=ORIENTED_EDGE('',*,*,#58893,.F.);
#87436=ORIENTED_EDGE('',*,*,#59002,.F.);
#87437=ORIENTED_EDGE('',*,*,#58998,.T.);
#87438=ORIENTED_EDGE('',*,*,#58999,.T.);
#87439=ORIENTED_EDGE('',*,*,#59002,.T.);
#87440=ORIENTED_EDGE('',*,*,#58892,.F.);
#87441=ORIENTED_EDGE('',*,*,#59003,.F.);
#87442=ORIENTED_EDGE('',*,*,#59004,.F.);
#87443=ORIENTED_EDGE('',*,*,#59005,.F.);
#87444=ORIENTED_EDGE('',*,*,#58991,.F.);
#87445=ORIENTED_EDGE('',*,*,#59001,.T.);
#87446=ORIENTED_EDGE('',*,*,#58880,.F.);
#87447=ORIENTED_EDGE('',*,*,#58993,.F.);
#87448=ORIENTED_EDGE('',*,*,#59006,.F.);
#87449=ORIENTED_EDGE('',*,*,#59004,.T.);
#87450=ORIENTED_EDGE('',*,*,#59007,.T.);
#87451=ORIENTED_EDGE('',*,*,#58992,.F.);
#87452=ORIENTED_EDGE('',*,*,#58988,.F.);
#87453=ORIENTED_EDGE('',*,*,#59005,.T.);
#87454=ORIENTED_EDGE('',*,*,#59006,.T.);
#87455=ORIENTED_EDGE('',*,*,#58994,.F.);
#87456=ORIENTED_EDGE('',*,*,#59007,.F.);
#87457=ORIENTED_EDGE('',*,*,#59003,.T.);
#87458=ORIENTED_EDGE('',*,*,#58891,.T.);
#87459=ORIENTED_EDGE('',*,*,#59008,.F.);
#87460=ORIENTED_EDGE('',*,*,#59009,.F.);
#87461=ORIENTED_EDGE('',*,*,#59010,.T.);
#87462=ORIENTED_EDGE('',*,*,#59011,.T.);
#87463=ORIENTED_EDGE('',*,*,#59012,.F.);
#87464=ORIENTED_EDGE('',*,*,#59013,.F.);
#87465=ORIENTED_EDGE('',*,*,#59014,.T.);
#87466=ORIENTED_EDGE('',*,*,#59009,.T.);
#87467=ORIENTED_EDGE('',*,*,#59015,.F.);
#87468=ORIENTED_EDGE('',*,*,#59016,.F.);
#87469=ORIENTED_EDGE('',*,*,#59017,.T.);
#87470=ORIENTED_EDGE('',*,*,#59013,.T.);
#87471=ORIENTED_EDGE('',*,*,#59018,.F.);
#87472=ORIENTED_EDGE('',*,*,#59011,.F.);
#87473=ORIENTED_EDGE('',*,*,#59019,.T.);
#87474=ORIENTED_EDGE('',*,*,#59016,.T.);
#87475=ORIENTED_EDGE('',*,*,#59010,.F.);
#87476=ORIENTED_EDGE('',*,*,#59014,.F.);
#87477=ORIENTED_EDGE('',*,*,#59017,.F.);
#87478=ORIENTED_EDGE('',*,*,#59019,.F.);
#87479=ORIENTED_EDGE('',*,*,#59008,.T.);
#87480=ORIENTED_EDGE('',*,*,#59018,.T.);
#87481=ORIENTED_EDGE('',*,*,#59015,.T.);
#87482=ORIENTED_EDGE('',*,*,#59012,.T.);
#87483=ORIENTED_EDGE('',*,*,#59020,.F.);
#87484=ORIENTED_EDGE('',*,*,#59021,.F.);
#87485=ORIENTED_EDGE('',*,*,#59022,.T.);
#87486=ORIENTED_EDGE('',*,*,#59023,.T.);
#87487=ORIENTED_EDGE('',*,*,#59024,.F.);
#87488=ORIENTED_EDGE('',*,*,#59025,.F.);
#87489=ORIENTED_EDGE('',*,*,#59026,.T.);
#87490=ORIENTED_EDGE('',*,*,#59021,.T.);
#87491=ORIENTED_EDGE('',*,*,#59027,.F.);
#87492=ORIENTED_EDGE('',*,*,#59028,.F.);
#87493=ORIENTED_EDGE('',*,*,#59029,.T.);
#87494=ORIENTED_EDGE('',*,*,#59025,.T.);
#87495=ORIENTED_EDGE('',*,*,#59030,.F.);
#87496=ORIENTED_EDGE('',*,*,#59023,.F.);
#87497=ORIENTED_EDGE('',*,*,#59031,.T.);
#87498=ORIENTED_EDGE('',*,*,#59028,.T.);
#87499=ORIENTED_EDGE('',*,*,#59022,.F.);
#87500=ORIENTED_EDGE('',*,*,#59026,.F.);
#87501=ORIENTED_EDGE('',*,*,#59029,.F.);
#87502=ORIENTED_EDGE('',*,*,#59031,.F.);
#87503=ORIENTED_EDGE('',*,*,#59020,.T.);
#87504=ORIENTED_EDGE('',*,*,#59030,.T.);
#87505=ORIENTED_EDGE('',*,*,#59027,.T.);
#87506=ORIENTED_EDGE('',*,*,#59024,.T.);
#87507=ORIENTED_EDGE('',*,*,#59032,.F.);
#87508=ORIENTED_EDGE('',*,*,#59033,.T.);
#87509=ORIENTED_EDGE('',*,*,#59034,.T.);
#87510=ORIENTED_EDGE('',*,*,#59033,.F.);
#87511=ORIENTED_EDGE('',*,*,#59035,.T.);
#87512=ORIENTED_EDGE('',*,*,#59032,.T.);
#87513=ORIENTED_EDGE('',*,*,#59035,.F.);
#87514=ORIENTED_EDGE('',*,*,#59036,.F.);
#87515=ORIENTED_EDGE('',*,*,#59037,.T.);
#87516=ORIENTED_EDGE('',*,*,#59038,.T.);
#87517=ORIENTED_EDGE('',*,*,#59037,.F.);
#87518=ORIENTED_EDGE('',*,*,#59039,.T.);
#87519=ORIENTED_EDGE('',*,*,#59040,.T.);
#87520=ORIENTED_EDGE('',*,*,#59041,.T.);
#87521=ORIENTED_EDGE('',*,*,#59042,.T.);
#87522=ORIENTED_EDGE('',*,*,#59043,.F.);
#87523=ORIENTED_EDGE('',*,*,#59044,.T.);
#87524=ORIENTED_EDGE('',*,*,#59045,.T.);
#87525=ORIENTED_EDGE('',*,*,#59044,.F.);
#87526=ORIENTED_EDGE('',*,*,#59046,.F.);
#87527=ORIENTED_EDGE('',*,*,#59047,.T.);
#87528=ORIENTED_EDGE('',*,*,#59048,.T.);
#87529=ORIENTED_EDGE('',*,*,#59049,.T.);
#87530=ORIENTED_EDGE('',*,*,#59050,.T.);
#87531=ORIENTED_EDGE('',*,*,#59051,.T.);
#87532=ORIENTED_EDGE('',*,*,#59052,.T.);
#87533=ORIENTED_EDGE('',*,*,#59053,.F.);
#87534=ORIENTED_EDGE('',*,*,#59052,.F.);
#87535=ORIENTED_EDGE('',*,*,#59054,.T.);
#87536=ORIENTED_EDGE('',*,*,#59055,.F.);
#87537=ORIENTED_EDGE('',*,*,#59056,.F.);
#87538=ORIENTED_EDGE('',*,*,#59057,.F.);
#87539=ORIENTED_EDGE('',*,*,#59058,.F.);
#87540=ORIENTED_EDGE('',*,*,#59059,.T.);
#87541=ORIENTED_EDGE('',*,*,#59060,.T.);
#87542=ORIENTED_EDGE('',*,*,#59061,.F.);
#87543=ORIENTED_EDGE('',*,*,#59060,.F.);
#87544=ORIENTED_EDGE('',*,*,#59062,.T.);
#87545=ORIENTED_EDGE('',*,*,#59063,.F.);
#87546=ORIENTED_EDGE('',*,*,#59064,.F.);
#87547=ORIENTED_EDGE('',*,*,#59065,.F.);
#87548=ORIENTED_EDGE('',*,*,#59066,.F.);
#87549=ORIENTED_EDGE('',*,*,#59067,.F.);
#87550=ORIENTED_EDGE('',*,*,#59068,.T.);
#87551=ORIENTED_EDGE('',*,*,#59069,.F.);
#87552=ORIENTED_EDGE('',*,*,#59068,.F.);
#87553=ORIENTED_EDGE('',*,*,#59070,.F.);
#87554=ORIENTED_EDGE('',*,*,#59071,.T.);
#87555=ORIENTED_EDGE('',*,*,#59072,.T.);
#87556=ORIENTED_EDGE('',*,*,#59073,.T.);
#87557=ORIENTED_EDGE('',*,*,#59074,.T.);
#87558=ORIENTED_EDGE('',*,*,#59075,.F.);
#87559=ORIENTED_EDGE('',*,*,#59076,.F.);
#87560=ORIENTED_EDGE('',*,*,#59077,.F.);
#87561=ORIENTED_EDGE('',*,*,#59078,.F.);
#87562=ORIENTED_EDGE('',*,*,#59079,.T.);
#87563=ORIENTED_EDGE('',*,*,#59080,.T.);
#87564=ORIENTED_EDGE('',*,*,#59081,.T.);
#87565=ORIENTED_EDGE('',*,*,#59080,.F.);
#87566=ORIENTED_EDGE('',*,*,#59082,.T.);
#87567=ORIENTED_EDGE('',*,*,#59083,.T.);
#87568=ORIENTED_EDGE('',*,*,#59084,.T.);
#87569=ORIENTED_EDGE('',*,*,#59085,.T.);
#87570=ORIENTED_EDGE('',*,*,#59086,.T.);
#87571=ORIENTED_EDGE('',*,*,#59087,.F.);
#87572=ORIENTED_EDGE('',*,*,#59088,.F.);
#87573=ORIENTED_EDGE('',*,*,#59089,.F.);
#87574=ORIENTED_EDGE('',*,*,#59090,.F.);
#87575=ORIENTED_EDGE('',*,*,#59043,.T.);
#87576=ORIENTED_EDGE('',*,*,#59091,.T.);
#87577=ORIENTED_EDGE('',*,*,#59059,.F.);
#87578=ORIENTED_EDGE('',*,*,#59092,.T.);
#87579=ORIENTED_EDGE('',*,*,#59067,.T.);
#87580=ORIENTED_EDGE('',*,*,#59093,.T.);
#87581=ORIENTED_EDGE('',*,*,#59051,.F.);
#87582=ORIENTED_EDGE('',*,*,#59094,.T.);
#87583=ORIENTED_EDGE('',*,*,#59095,.T.);
#87584=ORIENTED_EDGE('',*,*,#59094,.F.);
#87585=ORIENTED_EDGE('',*,*,#59054,.F.);
#87586=ORIENTED_EDGE('',*,*,#59093,.F.);
#87587=ORIENTED_EDGE('',*,*,#59070,.T.);
#87588=ORIENTED_EDGE('',*,*,#59092,.F.);
#87589=ORIENTED_EDGE('',*,*,#59062,.F.);
#87590=ORIENTED_EDGE('',*,*,#59096,.T.);
#87591=ORIENTED_EDGE('',*,*,#59046,.T.);
#87592=ORIENTED_EDGE('',*,*,#59036,.T.);
#87593=ORIENTED_EDGE('',*,*,#59079,.F.);
#87594=ORIENTED_EDGE('',*,*,#59082,.F.);
#87595=ORIENTED_EDGE('',*,*,#59040,.F.);
#87596=ORIENTED_EDGE('',*,*,#59097,.T.);
#87597=ORIENTED_EDGE('',*,*,#59084,.F.);
#87598=ORIENTED_EDGE('',*,*,#59098,.F.);
#87599=ORIENTED_EDGE('',*,*,#59041,.F.);
#87600=ORIENTED_EDGE('',*,*,#59098,.T.);
#87601=ORIENTED_EDGE('',*,*,#59083,.F.);
#87602=ORIENTED_EDGE('',*,*,#59099,.F.);
#87603=ORIENTED_EDGE('',*,*,#59042,.F.);
#87604=ORIENTED_EDGE('',*,*,#59099,.T.);
#87605=ORIENTED_EDGE('',*,*,#59086,.F.);
#87606=ORIENTED_EDGE('',*,*,#59100,.F.);
#87607=ORIENTED_EDGE('',*,*,#59039,.F.);
#87608=ORIENTED_EDGE('',*,*,#59100,.T.);
#87609=ORIENTED_EDGE('',*,*,#59085,.F.);
#87610=ORIENTED_EDGE('',*,*,#59097,.F.);
#87611=ORIENTED_EDGE('',*,*,#59081,.F.);
#87612=ORIENTED_EDGE('',*,*,#59101,.F.);
#87613=ORIENTED_EDGE('',*,*,#59102,.F.);
#87614=ORIENTED_EDGE('',*,*,#59103,.T.);
#87615=ORIENTED_EDGE('',*,*,#59104,.T.);
#87616=ORIENTED_EDGE('',*,*,#59105,.F.);
#87617=ORIENTED_EDGE('',*,*,#59106,.F.);
#87618=ORIENTED_EDGE('',*,*,#59105,.T.);
#87619=ORIENTED_EDGE('',*,*,#59101,.T.);
#87620=ORIENTED_EDGE('',*,*,#59107,.T.);
#87621=ORIENTED_EDGE('',*,*,#59107,.F.);
#87622=ORIENTED_EDGE('',*,*,#59106,.T.);
#87623=ORIENTED_EDGE('',*,*,#59103,.F.);
#87624=ORIENTED_EDGE('',*,*,#59108,.T.);
#87625=ORIENTED_EDGE('',*,*,#59104,.F.);
#87626=ORIENTED_EDGE('',*,*,#59108,.F.);
#87627=ORIENTED_EDGE('',*,*,#59102,.T.);
#87628=ORIENTED_EDGE('',*,*,#59048,.F.);
#87629=ORIENTED_EDGE('',*,*,#59109,.F.);
#87630=ORIENTED_EDGE('',*,*,#59087,.T.);
#87631=ORIENTED_EDGE('',*,*,#59110,.T.);
#87632=ORIENTED_EDGE('',*,*,#59047,.F.);
#87633=ORIENTED_EDGE('',*,*,#59111,.F.);
#87634=ORIENTED_EDGE('',*,*,#59088,.T.);
#87635=ORIENTED_EDGE('',*,*,#59109,.T.);
#87636=ORIENTED_EDGE('',*,*,#59050,.F.);
#87637=ORIENTED_EDGE('',*,*,#59112,.F.);
#87638=ORIENTED_EDGE('',*,*,#59089,.T.);
#87639=ORIENTED_EDGE('',*,*,#59111,.T.);
#87640=ORIENTED_EDGE('',*,*,#59049,.F.);
#87641=ORIENTED_EDGE('',*,*,#59110,.F.);
#87642=ORIENTED_EDGE('',*,*,#59090,.T.);
#87643=ORIENTED_EDGE('',*,*,#59112,.T.);
#87644=ORIENTED_EDGE('',*,*,#59113,.F.);
#87645=ORIENTED_EDGE('',*,*,#59055,.T.);
#87646=ORIENTED_EDGE('',*,*,#59114,.T.);
#87647=ORIENTED_EDGE('',*,*,#59075,.T.);
#87648=ORIENTED_EDGE('',*,*,#59115,.F.);
#87649=ORIENTED_EDGE('',*,*,#59056,.T.);
#87650=ORIENTED_EDGE('',*,*,#59113,.T.);
#87651=ORIENTED_EDGE('',*,*,#59078,.T.);
#87652=ORIENTED_EDGE('',*,*,#59116,.F.);
#87653=ORIENTED_EDGE('',*,*,#59057,.T.);
#87654=ORIENTED_EDGE('',*,*,#59115,.T.);
#87655=ORIENTED_EDGE('',*,*,#59077,.T.);
#87656=ORIENTED_EDGE('',*,*,#59114,.F.);
#87657=ORIENTED_EDGE('',*,*,#59058,.T.);
#87658=ORIENTED_EDGE('',*,*,#59116,.T.);
#87659=ORIENTED_EDGE('',*,*,#59076,.T.);
#87660=ORIENTED_EDGE('',*,*,#59117,.T.);
#87661=ORIENTED_EDGE('',*,*,#59063,.T.);
#87662=ORIENTED_EDGE('',*,*,#59118,.F.);
#87663=ORIENTED_EDGE('',*,*,#59074,.F.);
#87664=ORIENTED_EDGE('',*,*,#59119,.T.);
#87665=ORIENTED_EDGE('',*,*,#59064,.T.);
#87666=ORIENTED_EDGE('',*,*,#59117,.F.);
#87667=ORIENTED_EDGE('',*,*,#59073,.F.);
#87668=ORIENTED_EDGE('',*,*,#59118,.T.);
#87669=ORIENTED_EDGE('',*,*,#59066,.T.);
#87670=ORIENTED_EDGE('',*,*,#59120,.F.);
#87671=ORIENTED_EDGE('',*,*,#59071,.F.);
#87672=ORIENTED_EDGE('',*,*,#59120,.T.);
#87673=ORIENTED_EDGE('',*,*,#59065,.T.);
#87674=ORIENTED_EDGE('',*,*,#59119,.F.);
#87675=ORIENTED_EDGE('',*,*,#59072,.F.);
#87676=ORIENTED_EDGE('',*,*,#59069,.T.);
#87677=ORIENTED_EDGE('',*,*,#59121,.F.);
#87678=ORIENTED_EDGE('',*,*,#59122,.F.);
#87679=ORIENTED_EDGE('',*,*,#59123,.F.);
#87680=ORIENTED_EDGE('',*,*,#59124,.F.);
#87681=ORIENTED_EDGE('',*,*,#59125,.T.);
#87682=ORIENTED_EDGE('',*,*,#59126,.T.);
#87683=ORIENTED_EDGE('',*,*,#59125,.F.);
#87684=ORIENTED_EDGE('',*,*,#59127,.F.);
#87685=ORIENTED_EDGE('',*,*,#59126,.F.);
#87686=ORIENTED_EDGE('',*,*,#59127,.T.);
#87687=ORIENTED_EDGE('',*,*,#59124,.T.);
#87688=ORIENTED_EDGE('',*,*,#59128,.T.);
#87689=ORIENTED_EDGE('',*,*,#59122,.T.);
#87690=ORIENTED_EDGE('',*,*,#59121,.T.);
#87691=ORIENTED_EDGE('',*,*,#59123,.T.);
#87692=ORIENTED_EDGE('',*,*,#59128,.F.);
#87693=ORIENTED_EDGE('',*,*,#59061,.T.);
#87694=ORIENTED_EDGE('',*,*,#59129,.F.);
#87695=ORIENTED_EDGE('',*,*,#59130,.T.);
#87696=ORIENTED_EDGE('',*,*,#59131,.T.);
#87697=ORIENTED_EDGE('',*,*,#59131,.F.);
#87698=ORIENTED_EDGE('',*,*,#59132,.T.);
#87699=ORIENTED_EDGE('',*,*,#59129,.T.);
#87700=ORIENTED_EDGE('',*,*,#59130,.F.);
#87701=ORIENTED_EDGE('',*,*,#59132,.F.);
#87702=ORIENTED_EDGE('',*,*,#59053,.T.);
#87703=ORIENTED_EDGE('',*,*,#59133,.T.);
#87704=ORIENTED_EDGE('',*,*,#59134,.T.);
#87705=ORIENTED_EDGE('',*,*,#59135,.F.);
#87706=ORIENTED_EDGE('',*,*,#59134,.F.);
#87707=ORIENTED_EDGE('',*,*,#59136,.F.);
#87708=ORIENTED_EDGE('',*,*,#59135,.T.);
#87709=ORIENTED_EDGE('',*,*,#59133,.F.);
#87710=ORIENTED_EDGE('',*,*,#59136,.T.);
#87711=ORIENTED_EDGE('',*,*,#59045,.F.);
#87712=ORIENTED_EDGE('',*,*,#59137,.F.);
#87713=ORIENTED_EDGE('',*,*,#59138,.F.);
#87714=ORIENTED_EDGE('',*,*,#59139,.F.);
#87715=ORIENTED_EDGE('',*,*,#59138,.T.);
#87716=ORIENTED_EDGE('',*,*,#59137,.T.);
#87717=ORIENTED_EDGE('',*,*,#59140,.T.);
#87718=ORIENTED_EDGE('',*,*,#59140,.F.);
#87719=ORIENTED_EDGE('',*,*,#59139,.T.);
#87720=ORIENTED_EDGE('',*,*,#59038,.F.);
#87721=ORIENTED_EDGE('',*,*,#59141,.F.);
#87722=ORIENTED_EDGE('',*,*,#59142,.F.);
#87723=ORIENTED_EDGE('',*,*,#59143,.F.);
#87724=ORIENTED_EDGE('',*,*,#59144,.T.);
#87725=ORIENTED_EDGE('',*,*,#59143,.T.);
#87726=ORIENTED_EDGE('',*,*,#59142,.T.);
#87727=ORIENTED_EDGE('',*,*,#59141,.T.);
#87728=ORIENTED_EDGE('',*,*,#59144,.F.);
#87729=ORIENTED_EDGE('',*,*,#59095,.F.);
#87730=ORIENTED_EDGE('',*,*,#59034,.F.);
#87731=ORIENTED_EDGE('',*,*,#59091,.F.);
#87732=ORIENTED_EDGE('',*,*,#59096,.F.);
#87733=ORIENTED_EDGE('',*,*,#59145,.F.);
#87734=ORIENTED_EDGE('',*,*,#59146,.F.);
#87735=ORIENTED_EDGE('',*,*,#59147,.F.);
#87736=ORIENTED_EDGE('',*,*,#59148,.F.);
#87737=ORIENTED_EDGE('',*,*,#59149,.T.);
#87738=ORIENTED_EDGE('',*,*,#59150,.T.);
#87739=ORIENTED_EDGE('',*,*,#59151,.F.);
#87740=ORIENTED_EDGE('',*,*,#59152,.F.);
#87741=ORIENTED_EDGE('',*,*,#59153,.F.);
#87742=ORIENTED_EDGE('',*,*,#59154,.T.);
#87743=ORIENTED_EDGE('',*,*,#59155,.T.);
#87744=ORIENTED_EDGE('',*,*,#59156,.T.);
#87745=ORIENTED_EDGE('',*,*,#59157,.T.);
#87746=ORIENTED_EDGE('',*,*,#59158,.F.);
#87747=ORIENTED_EDGE('',*,*,#59159,.T.);
#87748=ORIENTED_EDGE('',*,*,#59146,.T.);
#87749=ORIENTED_EDGE('',*,*,#59160,.F.);
#87750=ORIENTED_EDGE('',*,*,#59161,.F.);
#87751=ORIENTED_EDGE('',*,*,#59162,.T.);
#87752=ORIENTED_EDGE('',*,*,#59163,.T.);
#87753=ORIENTED_EDGE('',*,*,#59164,.T.);
#87754=ORIENTED_EDGE('',*,*,#59165,.F.);
#87755=ORIENTED_EDGE('',*,*,#59166,.T.);
#87756=ORIENTED_EDGE('',*,*,#59167,.T.);
#87757=ORIENTED_EDGE('',*,*,#59168,.T.);
#87758=ORIENTED_EDGE('',*,*,#59169,.F.);
#87759=ORIENTED_EDGE('',*,*,#59170,.T.);
#87760=ORIENTED_EDGE('',*,*,#59148,.T.);
#87761=ORIENTED_EDGE('',*,*,#59171,.F.);
#87762=ORIENTED_EDGE('',*,*,#59172,.F.);
#87763=ORIENTED_EDGE('',*,*,#59173,.T.);
#87764=ORIENTED_EDGE('',*,*,#59174,.T.);
#87765=ORIENTED_EDGE('',*,*,#59175,.T.);
#87766=ORIENTED_EDGE('',*,*,#59176,.F.);
#87767=ORIENTED_EDGE('',*,*,#59177,.T.);
#87768=ORIENTED_EDGE('',*,*,#59178,.T.);
#87769=ORIENTED_EDGE('',*,*,#59179,.T.);
#87770=ORIENTED_EDGE('',*,*,#59180,.T.);
#87771=ORIENTED_EDGE('',*,*,#59181,.T.);
#87772=ORIENTED_EDGE('',*,*,#59182,.T.);
#87773=ORIENTED_EDGE('',*,*,#59183,.T.);
#87774=ORIENTED_EDGE('',*,*,#59184,.T.);
#87775=ORIENTED_EDGE('',*,*,#59185,.T.);
#87776=ORIENTED_EDGE('',*,*,#59186,.T.);
#87777=ORIENTED_EDGE('',*,*,#59187,.T.);
#87778=ORIENTED_EDGE('',*,*,#59188,.T.);
#87779=ORIENTED_EDGE('',*,*,#59189,.T.);
#87780=ORIENTED_EDGE('',*,*,#59190,.T.);
#87781=ORIENTED_EDGE('',*,*,#59191,.T.);
#87782=ORIENTED_EDGE('',*,*,#59192,.T.);
#87783=ORIENTED_EDGE('',*,*,#59193,.T.);
#87784=ORIENTED_EDGE('',*,*,#59194,.T.);
#87785=ORIENTED_EDGE('',*,*,#59195,.T.);
#87786=ORIENTED_EDGE('',*,*,#59196,.T.);
#87787=ORIENTED_EDGE('',*,*,#59197,.T.);
#87788=ORIENTED_EDGE('',*,*,#59198,.T.);
#87789=ORIENTED_EDGE('',*,*,#59199,.T.);
#87790=ORIENTED_EDGE('',*,*,#59200,.T.);
#87791=ORIENTED_EDGE('',*,*,#59201,.T.);
#87792=ORIENTED_EDGE('',*,*,#59202,.T.);
#87793=ORIENTED_EDGE('',*,*,#59203,.T.);
#87794=ORIENTED_EDGE('',*,*,#59204,.T.);
#87795=ORIENTED_EDGE('',*,*,#59205,.T.);
#87796=ORIENTED_EDGE('',*,*,#59206,.T.);
#87797=ORIENTED_EDGE('',*,*,#59207,.T.);
#87798=ORIENTED_EDGE('',*,*,#59208,.T.);
#87799=ORIENTED_EDGE('',*,*,#59157,.F.);
#87800=ORIENTED_EDGE('',*,*,#59209,.T.);
#87801=ORIENTED_EDGE('',*,*,#59173,.F.);
#87802=ORIENTED_EDGE('',*,*,#59210,.F.);
#87803=ORIENTED_EDGE('',*,*,#59168,.F.);
#87804=ORIENTED_EDGE('',*,*,#59211,.T.);
#87805=ORIENTED_EDGE('',*,*,#59162,.F.);
#87806=ORIENTED_EDGE('',*,*,#59212,.F.);
#87807=ORIENTED_EDGE('',*,*,#59164,.F.);
#87808=ORIENTED_EDGE('',*,*,#59213,.T.);
#87809=ORIENTED_EDGE('',*,*,#59155,.F.);
#87810=ORIENTED_EDGE('',*,*,#59214,.F.);
#87811=ORIENTED_EDGE('',*,*,#59175,.F.);
#87812=ORIENTED_EDGE('',*,*,#59215,.T.);
#87813=ORIENTED_EDGE('',*,*,#59166,.F.);
#87814=ORIENTED_EDGE('',*,*,#59216,.F.);
#87815=ORIENTED_EDGE('',*,*,#59217,.F.);
#87816=ORIENTED_EDGE('',*,*,#59213,.F.);
#87817=ORIENTED_EDGE('',*,*,#59218,.F.);
#87818=ORIENTED_EDGE('',*,*,#59182,.F.);
#87819=ORIENTED_EDGE('',*,*,#59218,.T.);
#87820=ORIENTED_EDGE('',*,*,#59163,.F.);
#87821=ORIENTED_EDGE('',*,*,#59219,.F.);
#87822=ORIENTED_EDGE('',*,*,#59183,.F.);
#87823=ORIENTED_EDGE('',*,*,#59217,.T.);
#87824=ORIENTED_EDGE('',*,*,#59181,.F.);
#87825=ORIENTED_EDGE('',*,*,#59220,.F.);
#87826=ORIENTED_EDGE('',*,*,#59156,.F.);
#87827=ORIENTED_EDGE('',*,*,#59219,.T.);
#87828=ORIENTED_EDGE('',*,*,#59211,.F.);
#87829=ORIENTED_EDGE('',*,*,#59221,.F.);
#87830=ORIENTED_EDGE('',*,*,#59184,.F.);
#87831=ORIENTED_EDGE('',*,*,#59220,.T.);
#87832=ORIENTED_EDGE('',*,*,#59180,.F.);
#87833=ORIENTED_EDGE('',*,*,#59222,.F.);
#87834=ORIENTED_EDGE('',*,*,#59209,.F.);
#87835=ORIENTED_EDGE('',*,*,#59221,.T.);
#87836=ORIENTED_EDGE('',*,*,#59167,.F.);
#87837=ORIENTED_EDGE('',*,*,#59223,.F.);
#87838=ORIENTED_EDGE('',*,*,#59177,.F.);
#87839=ORIENTED_EDGE('',*,*,#59222,.T.);
#87840=ORIENTED_EDGE('',*,*,#59179,.F.);
#87841=ORIENTED_EDGE('',*,*,#59224,.F.);
#87842=ORIENTED_EDGE('',*,*,#59174,.F.);
#87843=ORIENTED_EDGE('',*,*,#59223,.T.);
#87844=ORIENTED_EDGE('',*,*,#59215,.F.);
#87845=ORIENTED_EDGE('',*,*,#59224,.T.);
#87846=ORIENTED_EDGE('',*,*,#59178,.F.);
#87847=ORIENTED_EDGE('',*,*,#59207,.F.);
#87848=ORIENTED_EDGE('',*,*,#59225,.T.);
#87849=ORIENTED_EDGE('',*,*,#59193,.F.);
#87850=ORIENTED_EDGE('',*,*,#59226,.T.);
#87851=ORIENTED_EDGE('',*,*,#59227,.T.);
#87852=ORIENTED_EDGE('',*,*,#59203,.F.);
#87853=ORIENTED_EDGE('',*,*,#59228,.T.);
#87854=ORIENTED_EDGE('',*,*,#59205,.F.);
#87855=ORIENTED_EDGE('',*,*,#59229,.T.);
#87856=ORIENTED_EDGE('',*,*,#59230,.T.);
#87857=ORIENTED_EDGE('',*,*,#59195,.F.);
#87858=ORIENTED_EDGE('',*,*,#59231,.T.);
#87859=ORIENTED_EDGE('',*,*,#59199,.F.);
#87860=ORIENTED_EDGE('',*,*,#59232,.T.);
#87861=ORIENTED_EDGE('',*,*,#59233,.T.);
#87862=ORIENTED_EDGE('',*,*,#59197,.F.);
#87863=ORIENTED_EDGE('',*,*,#59234,.T.);
#87864=ORIENTED_EDGE('',*,*,#59201,.F.);
#87865=ORIENTED_EDGE('',*,*,#59235,.T.);
#87866=ORIENTED_EDGE('',*,*,#59236,.T.);
#87867=ORIENTED_EDGE('',*,*,#59152,.T.);
#87868=ORIENTED_EDGE('',*,*,#59237,.F.);
#87869=ORIENTED_EDGE('',*,*,#59238,.F.);
#87870=ORIENTED_EDGE('',*,*,#59239,.T.);
#87871=ORIENTED_EDGE('',*,*,#59151,.T.);
#87872=ORIENTED_EDGE('',*,*,#59240,.T.);
#87873=ORIENTED_EDGE('',*,*,#59241,.T.);
#87874=ORIENTED_EDGE('',*,*,#59242,.T.);
#87875=ORIENTED_EDGE('',*,*,#59243,.T.);
#87876=ORIENTED_EDGE('',*,*,#59244,.F.);
#87877=ORIENTED_EDGE('',*,*,#59245,.F.);
#87878=ORIENTED_EDGE('',*,*,#59237,.T.);
#87879=ORIENTED_EDGE('',*,*,#59246,.T.);
#87880=ORIENTED_EDGE('',*,*,#59247,.F.);
#87881=ORIENTED_EDGE('',*,*,#59248,.F.);
#87882=ORIENTED_EDGE('',*,*,#59244,.T.);
#87883=ORIENTED_EDGE('',*,*,#59249,.T.);
#87884=ORIENTED_EDGE('',*,*,#59250,.T.);
#87885=ORIENTED_EDGE('',*,*,#59251,.T.);
#87886=ORIENTED_EDGE('',*,*,#59252,.T.);
#87887=ORIENTED_EDGE('',*,*,#59153,.T.);
#87888=ORIENTED_EDGE('',*,*,#59239,.F.);
#87889=ORIENTED_EDGE('',*,*,#59253,.F.);
#87890=ORIENTED_EDGE('',*,*,#59247,.T.);
#87891=ORIENTED_EDGE('',*,*,#59254,.T.);
#87892=ORIENTED_EDGE('',*,*,#59255,.T.);
#87893=ORIENTED_EDGE('',*,*,#59249,.F.);
#87894=ORIENTED_EDGE('',*,*,#59246,.F.);
#87895=ORIENTED_EDGE('',*,*,#59243,.F.);
#87896=ORIENTED_EDGE('',*,*,#59256,.T.);
#87897=ORIENTED_EDGE('',*,*,#59257,.F.);
#87898=ORIENTED_EDGE('',*,*,#59228,.F.);
#87899=ORIENTED_EDGE('',*,*,#59258,.F.);
#87900=ORIENTED_EDGE('',*,*,#59190,.F.);
#87901=ORIENTED_EDGE('',*,*,#59258,.T.);
#87902=ORIENTED_EDGE('',*,*,#59202,.F.);
#87903=ORIENTED_EDGE('',*,*,#59259,.F.);
#87904=ORIENTED_EDGE('',*,*,#59191,.F.);
#87905=ORIENTED_EDGE('',*,*,#59257,.T.);
#87906=ORIENTED_EDGE('',*,*,#59189,.F.);
#87907=ORIENTED_EDGE('',*,*,#59260,.F.);
#87908=ORIENTED_EDGE('',*,*,#59206,.F.);
#87909=ORIENTED_EDGE('',*,*,#59259,.T.);
#87910=ORIENTED_EDGE('',*,*,#59234,.F.);
#87911=ORIENTED_EDGE('',*,*,#59261,.F.);
#87912=ORIENTED_EDGE('',*,*,#59192,.F.);
#87913=ORIENTED_EDGE('',*,*,#59260,.T.);
#87914=ORIENTED_EDGE('',*,*,#59188,.F.);
#87915=ORIENTED_EDGE('',*,*,#59262,.F.);
#87916=ORIENTED_EDGE('',*,*,#59225,.F.);
#87917=ORIENTED_EDGE('',*,*,#59261,.T.);
#87918=ORIENTED_EDGE('',*,*,#59200,.F.);
#87919=ORIENTED_EDGE('',*,*,#59263,.F.);
#87920=ORIENTED_EDGE('',*,*,#59185,.F.);
#87921=ORIENTED_EDGE('',*,*,#59262,.T.);
#87922=ORIENTED_EDGE('',*,*,#59187,.F.);
#87923=ORIENTED_EDGE('',*,*,#59264,.F.);
#87924=ORIENTED_EDGE('',*,*,#59194,.F.);
#87925=ORIENTED_EDGE('',*,*,#59263,.T.);
#87926=ORIENTED_EDGE('',*,*,#59231,.F.);
#87927=ORIENTED_EDGE('',*,*,#59264,.T.);
#87928=ORIENTED_EDGE('',*,*,#59186,.F.);
#87929=ORIENTED_EDGE('',*,*,#59265,.F.);
#87930=ORIENTED_EDGE('',*,*,#59230,.F.);
#87931=ORIENTED_EDGE('',*,*,#59266,.F.);
#87932=ORIENTED_EDGE('',*,*,#59255,.F.);
#87933=ORIENTED_EDGE('',*,*,#59266,.T.);
#87934=ORIENTED_EDGE('',*,*,#59229,.F.);
#87935=ORIENTED_EDGE('',*,*,#59267,.F.);
#87936=ORIENTED_EDGE('',*,*,#59250,.F.);
#87937=ORIENTED_EDGE('',*,*,#59265,.T.);
#87938=ORIENTED_EDGE('',*,*,#59254,.F.);
#87939=ORIENTED_EDGE('',*,*,#59268,.F.);
#87940=ORIENTED_EDGE('',*,*,#59204,.F.);
#87941=ORIENTED_EDGE('',*,*,#59267,.T.);
#87942=ORIENTED_EDGE('',*,*,#59208,.F.);
#87943=ORIENTED_EDGE('',*,*,#59269,.F.);
#87944=ORIENTED_EDGE('',*,*,#59251,.F.);
#87945=ORIENTED_EDGE('',*,*,#59268,.T.);
#87946=ORIENTED_EDGE('',*,*,#59256,.F.);
#87947=ORIENTED_EDGE('',*,*,#59270,.F.);
#87948=ORIENTED_EDGE('',*,*,#59235,.F.);
#87949=ORIENTED_EDGE('',*,*,#59269,.T.);
#87950=ORIENTED_EDGE('',*,*,#59227,.F.);
#87951=ORIENTED_EDGE('',*,*,#59271,.F.);
#87952=ORIENTED_EDGE('',*,*,#59252,.F.);
#87953=ORIENTED_EDGE('',*,*,#59270,.T.);
#87954=ORIENTED_EDGE('',*,*,#59242,.F.);
#87955=ORIENTED_EDGE('',*,*,#59272,.F.);
#87956=ORIENTED_EDGE('',*,*,#59236,.F.);
#87957=ORIENTED_EDGE('',*,*,#59271,.T.);
#87958=ORIENTED_EDGE('',*,*,#59226,.F.);
#87959=ORIENTED_EDGE('',*,*,#59273,.F.);
#87960=ORIENTED_EDGE('',*,*,#59154,.F.);
#87961=ORIENTED_EDGE('',*,*,#59272,.T.);
#87962=ORIENTED_EDGE('',*,*,#59241,.F.);
#87963=ORIENTED_EDGE('',*,*,#59274,.F.);
#87964=ORIENTED_EDGE('',*,*,#59198,.F.);
#87965=ORIENTED_EDGE('',*,*,#59273,.T.);
#87966=ORIENTED_EDGE('',*,*,#59196,.F.);
#87967=ORIENTED_EDGE('',*,*,#59275,.F.);
#87968=ORIENTED_EDGE('',*,*,#59149,.F.);
#87969=ORIENTED_EDGE('',*,*,#59274,.T.);
#87970=ORIENTED_EDGE('',*,*,#59240,.F.);
#87971=ORIENTED_EDGE('',*,*,#59276,.F.);
#87972=ORIENTED_EDGE('',*,*,#59232,.F.);
#87973=ORIENTED_EDGE('',*,*,#59275,.T.);
#87974=ORIENTED_EDGE('',*,*,#59233,.F.);
#87975=ORIENTED_EDGE('',*,*,#59276,.T.);
#87976=ORIENTED_EDGE('',*,*,#59150,.F.);
#87977=ORIENTED_EDGE('',*,*,#59277,.F.);
#87978=ORIENTED_EDGE('',*,*,#59278,.F.);
#87979=ORIENTED_EDGE('',*,*,#59279,.F.);
#87980=ORIENTED_EDGE('',*,*,#59280,.F.);
#87981=ORIENTED_EDGE('',*,*,#59253,.T.);
#87982=ORIENTED_EDGE('',*,*,#59238,.T.);
#87983=ORIENTED_EDGE('',*,*,#59245,.T.);
#87984=ORIENTED_EDGE('',*,*,#59248,.T.);
#87985=ORIENTED_EDGE('',*,*,#59277,.T.);
#87986=ORIENTED_EDGE('',*,*,#59281,.F.);
#87987=ORIENTED_EDGE('',*,*,#59282,.F.);
#87988=ORIENTED_EDGE('',*,*,#59283,.T.);
#87989=ORIENTED_EDGE('',*,*,#59280,.T.);
#87990=ORIENTED_EDGE('',*,*,#59284,.F.);
#87991=ORIENTED_EDGE('',*,*,#59285,.F.);
#87992=ORIENTED_EDGE('',*,*,#59281,.T.);
#87993=ORIENTED_EDGE('',*,*,#59279,.T.);
#87994=ORIENTED_EDGE('',*,*,#59286,.F.);
#87995=ORIENTED_EDGE('',*,*,#59287,.F.);
#87996=ORIENTED_EDGE('',*,*,#59284,.T.);
#87997=ORIENTED_EDGE('',*,*,#59278,.T.);
#87998=ORIENTED_EDGE('',*,*,#59283,.F.);
#87999=ORIENTED_EDGE('',*,*,#59288,.F.);
#88000=ORIENTED_EDGE('',*,*,#59286,.T.);
#88001=ORIENTED_EDGE('',*,*,#59282,.T.);
#88002=ORIENTED_EDGE('',*,*,#59285,.T.);
#88003=ORIENTED_EDGE('',*,*,#59287,.T.);
#88004=ORIENTED_EDGE('',*,*,#59288,.T.);
#88005=ORIENTED_EDGE('',*,*,#59147,.T.);
#88006=ORIENTED_EDGE('',*,*,#59159,.F.);
#88007=ORIENTED_EDGE('',*,*,#59289,.F.);
#88008=ORIENTED_EDGE('',*,*,#59171,.T.);
#88009=ORIENTED_EDGE('',*,*,#59210,.T.);
#88010=ORIENTED_EDGE('',*,*,#59176,.T.);
#88011=ORIENTED_EDGE('',*,*,#59216,.T.);
#88012=ORIENTED_EDGE('',*,*,#59172,.T.);
#88013=ORIENTED_EDGE('',*,*,#59289,.T.);
#88014=ORIENTED_EDGE('',*,*,#59158,.T.);
#88015=ORIENTED_EDGE('',*,*,#59145,.T.);
#88016=ORIENTED_EDGE('',*,*,#59170,.F.);
#88017=ORIENTED_EDGE('',*,*,#59290,.F.);
#88018=ORIENTED_EDGE('',*,*,#59160,.T.);
#88019=ORIENTED_EDGE('',*,*,#59214,.T.);
#88020=ORIENTED_EDGE('',*,*,#59161,.T.);
#88021=ORIENTED_EDGE('',*,*,#59290,.T.);
#88022=ORIENTED_EDGE('',*,*,#59169,.T.);
#88023=ORIENTED_EDGE('',*,*,#59212,.T.);
#88024=ORIENTED_EDGE('',*,*,#59165,.T.);
#88025=ORIENTED_EDGE('',*,*,#59291,.T.);
#88026=ORIENTED_EDGE('',*,*,#59292,.T.);
#88027=ORIENTED_EDGE('',*,*,#59293,.F.);
#88028=ORIENTED_EDGE('',*,*,#59294,.F.);
#88029=ORIENTED_EDGE('',*,*,#59295,.T.);
#88030=ORIENTED_EDGE('',*,*,#59296,.T.);
#88031=ORIENTED_EDGE('',*,*,#59297,.T.);
#88032=ORIENTED_EDGE('',*,*,#59298,.T.);
#88033=ORIENTED_EDGE('',*,*,#59299,.T.);
#88034=ORIENTED_EDGE('',*,*,#59300,.T.);
#88035=ORIENTED_EDGE('',*,*,#59301,.T.);
#88036=ORIENTED_EDGE('',*,*,#59302,.T.);
#88037=ORIENTED_EDGE('',*,*,#59303,.T.);
#88038=ORIENTED_EDGE('',*,*,#59304,.T.);
#88039=ORIENTED_EDGE('',*,*,#59305,.T.);
#88040=ORIENTED_EDGE('',*,*,#59306,.T.);
#88041=ORIENTED_EDGE('',*,*,#59307,.T.);
#88042=ORIENTED_EDGE('',*,*,#59308,.T.);
#88043=ORIENTED_EDGE('',*,*,#59293,.T.);
#88044=ORIENTED_EDGE('',*,*,#59309,.T.);
#88045=ORIENTED_EDGE('',*,*,#59292,.F.);
#88046=ORIENTED_EDGE('',*,*,#59310,.T.);
#88047=ORIENTED_EDGE('',*,*,#59311,.T.);
#88048=ORIENTED_EDGE('',*,*,#59309,.F.);
#88049=ORIENTED_EDGE('',*,*,#59312,.F.);
#88050=ORIENTED_EDGE('',*,*,#59313,.T.);
#88051=ORIENTED_EDGE('',*,*,#59294,.T.);
#88052=ORIENTED_EDGE('',*,*,#59308,.F.);
#88053=ORIENTED_EDGE('',*,*,#59314,.F.);
#88054=ORIENTED_EDGE('',*,*,#59315,.T.);
#88055=ORIENTED_EDGE('',*,*,#59312,.T.);
#88056=ORIENTED_EDGE('',*,*,#59307,.F.);
#88057=ORIENTED_EDGE('',*,*,#59316,.F.);
#88058=ORIENTED_EDGE('',*,*,#59317,.T.);
#88059=ORIENTED_EDGE('',*,*,#59314,.T.);
#88060=ORIENTED_EDGE('',*,*,#59306,.F.);
#88061=ORIENTED_EDGE('',*,*,#59318,.F.);
#88062=ORIENTED_EDGE('',*,*,#59319,.T.);
#88063=ORIENTED_EDGE('',*,*,#59316,.T.);
#88064=ORIENTED_EDGE('',*,*,#59305,.F.);
#88065=ORIENTED_EDGE('',*,*,#59320,.F.);
#88066=ORIENTED_EDGE('',*,*,#59321,.T.);
#88067=ORIENTED_EDGE('',*,*,#59318,.T.);
#88068=ORIENTED_EDGE('',*,*,#59304,.F.);
#88069=ORIENTED_EDGE('',*,*,#59322,.F.);
#88070=ORIENTED_EDGE('',*,*,#59323,.T.);
#88071=ORIENTED_EDGE('',*,*,#59320,.T.);
#88072=ORIENTED_EDGE('',*,*,#59303,.F.);
#88073=ORIENTED_EDGE('',*,*,#59324,.F.);
#88074=ORIENTED_EDGE('',*,*,#59325,.T.);
#88075=ORIENTED_EDGE('',*,*,#59322,.T.);
#88076=ORIENTED_EDGE('',*,*,#59302,.F.);
#88077=ORIENTED_EDGE('',*,*,#59326,.F.);
#88078=ORIENTED_EDGE('',*,*,#59327,.T.);
#88079=ORIENTED_EDGE('',*,*,#59324,.T.);
#88080=ORIENTED_EDGE('',*,*,#59301,.F.);
#88081=ORIENTED_EDGE('',*,*,#59328,.F.);
#88082=ORIENTED_EDGE('',*,*,#59329,.T.);
#88083=ORIENTED_EDGE('',*,*,#59326,.T.);
#88084=ORIENTED_EDGE('',*,*,#59300,.F.);
#88085=ORIENTED_EDGE('',*,*,#59330,.F.);
#88086=ORIENTED_EDGE('',*,*,#59331,.T.);
#88087=ORIENTED_EDGE('',*,*,#59328,.T.);
#88088=ORIENTED_EDGE('',*,*,#59299,.F.);
#88089=ORIENTED_EDGE('',*,*,#59332,.F.);
#88090=ORIENTED_EDGE('',*,*,#59333,.T.);
#88091=ORIENTED_EDGE('',*,*,#59330,.T.);
#88092=ORIENTED_EDGE('',*,*,#59298,.F.);
#88093=ORIENTED_EDGE('',*,*,#59334,.F.);
#88094=ORIENTED_EDGE('',*,*,#59335,.T.);
#88095=ORIENTED_EDGE('',*,*,#59332,.T.);
#88096=ORIENTED_EDGE('',*,*,#59297,.F.);
#88097=ORIENTED_EDGE('',*,*,#59336,.F.);
#88098=ORIENTED_EDGE('',*,*,#59337,.T.);
#88099=ORIENTED_EDGE('',*,*,#59334,.T.);
#88100=ORIENTED_EDGE('',*,*,#59296,.F.);
#88101=ORIENTED_EDGE('',*,*,#59311,.F.);
#88102=ORIENTED_EDGE('',*,*,#59338,.T.);
#88103=ORIENTED_EDGE('',*,*,#59336,.T.);
#88104=ORIENTED_EDGE('',*,*,#59295,.F.);
#88105=ORIENTED_EDGE('',*,*,#59338,.F.);
#88106=ORIENTED_EDGE('',*,*,#59310,.F.);
#88107=ORIENTED_EDGE('',*,*,#59291,.F.);
#88108=ORIENTED_EDGE('',*,*,#59313,.F.);
#88109=ORIENTED_EDGE('',*,*,#59315,.F.);
#88110=ORIENTED_EDGE('',*,*,#59317,.F.);
#88111=ORIENTED_EDGE('',*,*,#59319,.F.);
#88112=ORIENTED_EDGE('',*,*,#59321,.F.);
#88113=ORIENTED_EDGE('',*,*,#59323,.F.);
#88114=ORIENTED_EDGE('',*,*,#59325,.F.);
#88115=ORIENTED_EDGE('',*,*,#59327,.F.);
#88116=ORIENTED_EDGE('',*,*,#59329,.F.);
#88117=ORIENTED_EDGE('',*,*,#59331,.F.);
#88118=ORIENTED_EDGE('',*,*,#59333,.F.);
#88119=ORIENTED_EDGE('',*,*,#59335,.F.);
#88120=ORIENTED_EDGE('',*,*,#59337,.F.);
#88121=ORIENTED_EDGE('',*,*,#59339,.T.);
#88122=ORIENTED_EDGE('',*,*,#59340,.T.);
#88123=ORIENTED_EDGE('',*,*,#59341,.T.);
#88124=ORIENTED_EDGE('',*,*,#59342,.T.);
#88125=ORIENTED_EDGE('',*,*,#59343,.T.);
#88126=ORIENTED_EDGE('',*,*,#59344,.T.);
#88127=ORIENTED_EDGE('',*,*,#59345,.T.);
#88128=ORIENTED_EDGE('',*,*,#59346,.T.);
#88129=ORIENTED_EDGE('',*,*,#59347,.F.);
#88130=ORIENTED_EDGE('',*,*,#59348,.T.);
#88131=ORIENTED_EDGE('',*,*,#59349,.T.);
#88132=ORIENTED_EDGE('',*,*,#59346,.F.);
#88133=ORIENTED_EDGE('',*,*,#59350,.F.);
#88134=ORIENTED_EDGE('',*,*,#59351,.T.);
#88135=ORIENTED_EDGE('',*,*,#59347,.T.);
#88136=ORIENTED_EDGE('',*,*,#59345,.F.);
#88137=ORIENTED_EDGE('',*,*,#59352,.F.);
#88138=ORIENTED_EDGE('',*,*,#59353,.T.);
#88139=ORIENTED_EDGE('',*,*,#59350,.T.);
#88140=ORIENTED_EDGE('',*,*,#59344,.F.);
#88141=ORIENTED_EDGE('',*,*,#59354,.F.);
#88142=ORIENTED_EDGE('',*,*,#59355,.T.);
#88143=ORIENTED_EDGE('',*,*,#59352,.T.);
#88144=ORIENTED_EDGE('',*,*,#59343,.F.);
#88145=ORIENTED_EDGE('',*,*,#59356,.F.);
#88146=ORIENTED_EDGE('',*,*,#59357,.T.);
#88147=ORIENTED_EDGE('',*,*,#59354,.T.);
#88148=ORIENTED_EDGE('',*,*,#59342,.F.);
#88149=ORIENTED_EDGE('',*,*,#59358,.F.);
#88150=ORIENTED_EDGE('',*,*,#59359,.T.);
#88151=ORIENTED_EDGE('',*,*,#59356,.T.);
#88152=ORIENTED_EDGE('',*,*,#59341,.F.);
#88153=ORIENTED_EDGE('',*,*,#59360,.F.);
#88154=ORIENTED_EDGE('',*,*,#59361,.T.);
#88155=ORIENTED_EDGE('',*,*,#59358,.T.);
#88156=ORIENTED_EDGE('',*,*,#59340,.F.);
#88157=ORIENTED_EDGE('',*,*,#59349,.F.);
#88158=ORIENTED_EDGE('',*,*,#59362,.T.);
#88159=ORIENTED_EDGE('',*,*,#59360,.T.);
#88160=ORIENTED_EDGE('',*,*,#59339,.F.);
#88161=ORIENTED_EDGE('',*,*,#59362,.F.);
#88162=ORIENTED_EDGE('',*,*,#59348,.F.);
#88163=ORIENTED_EDGE('',*,*,#59351,.F.);
#88164=ORIENTED_EDGE('',*,*,#59353,.F.);
#88165=ORIENTED_EDGE('',*,*,#59355,.F.);
#88166=ORIENTED_EDGE('',*,*,#59357,.F.);
#88167=ORIENTED_EDGE('',*,*,#59359,.F.);
#88168=ORIENTED_EDGE('',*,*,#59361,.F.);
#88169=ORIENTED_EDGE('',*,*,#59363,.T.);
#88170=ORIENTED_EDGE('',*,*,#59364,.T.);
#88171=ORIENTED_EDGE('',*,*,#59365,.T.);
#88172=ORIENTED_EDGE('',*,*,#59366,.T.);
#88173=ORIENTED_EDGE('',*,*,#59367,.T.);
#88174=ORIENTED_EDGE('',*,*,#59368,.T.);
#88175=ORIENTED_EDGE('',*,*,#59369,.T.);
#88176=ORIENTED_EDGE('',*,*,#59370,.T.);
#88177=ORIENTED_EDGE('',*,*,#59371,.T.);
#88178=ORIENTED_EDGE('',*,*,#59372,.T.);
#88179=ORIENTED_EDGE('',*,*,#59373,.T.);
#88180=ORIENTED_EDGE('',*,*,#59374,.T.);
#88181=ORIENTED_EDGE('',*,*,#59375,.T.);
#88182=ORIENTED_EDGE('',*,*,#59376,.T.);
#88183=ORIENTED_EDGE('',*,*,#59377,.T.);
#88184=ORIENTED_EDGE('',*,*,#59378,.T.);
#88185=ORIENTED_EDGE('',*,*,#59379,.T.);
#88186=ORIENTED_EDGE('',*,*,#59380,.T.);
#88187=ORIENTED_EDGE('',*,*,#59381,.T.);
#88188=ORIENTED_EDGE('',*,*,#59382,.T.);
#88189=ORIENTED_EDGE('',*,*,#59383,.T.);
#88190=ORIENTED_EDGE('',*,*,#59384,.T.);
#88191=ORIENTED_EDGE('',*,*,#59385,.T.);
#88192=ORIENTED_EDGE('',*,*,#59386,.T.);
#88193=ORIENTED_EDGE('',*,*,#59387,.T.);
#88194=ORIENTED_EDGE('',*,*,#59388,.T.);
#88195=ORIENTED_EDGE('',*,*,#59389,.T.);
#88196=ORIENTED_EDGE('',*,*,#59390,.T.);
#88197=ORIENTED_EDGE('',*,*,#59391,.T.);
#88198=ORIENTED_EDGE('',*,*,#59392,.T.);
#88199=ORIENTED_EDGE('',*,*,#59393,.T.);
#88200=ORIENTED_EDGE('',*,*,#59394,.T.);
#88201=ORIENTED_EDGE('',*,*,#59395,.T.);
#88202=ORIENTED_EDGE('',*,*,#59396,.T.);
#88203=ORIENTED_EDGE('',*,*,#59397,.T.);
#88204=ORIENTED_EDGE('',*,*,#59398,.T.);
#88205=ORIENTED_EDGE('',*,*,#59399,.T.);
#88206=ORIENTED_EDGE('',*,*,#59400,.T.);
#88207=ORIENTED_EDGE('',*,*,#59401,.T.);
#88208=ORIENTED_EDGE('',*,*,#59402,.T.);
#88209=ORIENTED_EDGE('',*,*,#59403,.T.);
#88210=ORIENTED_EDGE('',*,*,#59404,.T.);
#88211=ORIENTED_EDGE('',*,*,#59405,.T.);
#88212=ORIENTED_EDGE('',*,*,#59406,.T.);
#88213=ORIENTED_EDGE('',*,*,#59407,.T.);
#88214=ORIENTED_EDGE('',*,*,#59408,.T.);
#88215=ORIENTED_EDGE('',*,*,#59409,.T.);
#88216=ORIENTED_EDGE('',*,*,#59410,.T.);
#88217=ORIENTED_EDGE('',*,*,#59411,.T.);
#88218=ORIENTED_EDGE('',*,*,#59412,.T.);
#88219=ORIENTED_EDGE('',*,*,#59413,.T.);
#88220=ORIENTED_EDGE('',*,*,#59414,.T.);
#88221=ORIENTED_EDGE('',*,*,#59415,.T.);
#88222=ORIENTED_EDGE('',*,*,#59416,.T.);
#88223=ORIENTED_EDGE('',*,*,#59417,.T.);
#88224=ORIENTED_EDGE('',*,*,#59418,.T.);
#88225=ORIENTED_EDGE('',*,*,#59419,.F.);
#88226=ORIENTED_EDGE('',*,*,#59420,.F.);
#88227=ORIENTED_EDGE('',*,*,#59421,.F.);
#88228=ORIENTED_EDGE('',*,*,#59422,.F.);
#88229=ORIENTED_EDGE('',*,*,#59423,.F.);
#88230=ORIENTED_EDGE('',*,*,#59424,.F.);
#88231=ORIENTED_EDGE('',*,*,#59425,.F.);
#88232=ORIENTED_EDGE('',*,*,#59426,.F.);
#88233=ORIENTED_EDGE('',*,*,#59427,.F.);
#88234=ORIENTED_EDGE('',*,*,#59428,.F.);
#88235=ORIENTED_EDGE('',*,*,#59429,.F.);
#88236=ORIENTED_EDGE('',*,*,#59430,.F.);
#88237=ORIENTED_EDGE('',*,*,#59431,.F.);
#88238=ORIENTED_EDGE('',*,*,#59432,.F.);
#88239=ORIENTED_EDGE('',*,*,#59433,.F.);
#88240=ORIENTED_EDGE('',*,*,#59434,.F.);
#88241=ORIENTED_EDGE('',*,*,#59435,.F.);
#88242=ORIENTED_EDGE('',*,*,#59436,.F.);
#88243=ORIENTED_EDGE('',*,*,#59437,.F.);
#88244=ORIENTED_EDGE('',*,*,#59438,.F.);
#88245=ORIENTED_EDGE('',*,*,#59439,.F.);
#88246=ORIENTED_EDGE('',*,*,#59440,.F.);
#88247=ORIENTED_EDGE('',*,*,#59441,.F.);
#88248=ORIENTED_EDGE('',*,*,#59442,.F.);
#88249=ORIENTED_EDGE('',*,*,#59443,.F.);
#88250=ORIENTED_EDGE('',*,*,#59444,.F.);
#88251=ORIENTED_EDGE('',*,*,#59445,.F.);
#88252=ORIENTED_EDGE('',*,*,#59446,.F.);
#88253=ORIENTED_EDGE('',*,*,#59447,.F.);
#88254=ORIENTED_EDGE('',*,*,#59448,.F.);
#88255=ORIENTED_EDGE('',*,*,#59449,.F.);
#88256=ORIENTED_EDGE('',*,*,#59450,.F.);
#88257=ORIENTED_EDGE('',*,*,#59451,.F.);
#88258=ORIENTED_EDGE('',*,*,#59452,.F.);
#88259=ORIENTED_EDGE('',*,*,#59453,.F.);
#88260=ORIENTED_EDGE('',*,*,#59454,.F.);
#88261=ORIENTED_EDGE('',*,*,#59455,.F.);
#88262=ORIENTED_EDGE('',*,*,#59456,.F.);
#88263=ORIENTED_EDGE('',*,*,#59457,.F.);
#88264=ORIENTED_EDGE('',*,*,#59458,.F.);
#88265=ORIENTED_EDGE('',*,*,#59459,.F.);
#88266=ORIENTED_EDGE('',*,*,#59460,.F.);
#88267=ORIENTED_EDGE('',*,*,#59461,.F.);
#88268=ORIENTED_EDGE('',*,*,#59462,.F.);
#88269=ORIENTED_EDGE('',*,*,#59463,.F.);
#88270=ORIENTED_EDGE('',*,*,#59464,.F.);
#88271=ORIENTED_EDGE('',*,*,#59465,.F.);
#88272=ORIENTED_EDGE('',*,*,#59466,.F.);
#88273=ORIENTED_EDGE('',*,*,#59467,.F.);
#88274=ORIENTED_EDGE('',*,*,#59468,.F.);
#88275=ORIENTED_EDGE('',*,*,#59469,.F.);
#88276=ORIENTED_EDGE('',*,*,#59470,.F.);
#88277=ORIENTED_EDGE('',*,*,#59471,.F.);
#88278=ORIENTED_EDGE('',*,*,#59472,.F.);
#88279=ORIENTED_EDGE('',*,*,#59473,.F.);
#88280=ORIENTED_EDGE('',*,*,#59474,.F.);
#88281=ORIENTED_EDGE('',*,*,#59363,.F.);
#88282=ORIENTED_EDGE('',*,*,#59475,.T.);
#88283=ORIENTED_EDGE('',*,*,#59421,.T.);
#88284=ORIENTED_EDGE('',*,*,#59476,.F.);
#88285=ORIENTED_EDGE('',*,*,#59418,.F.);
#88286=ORIENTED_EDGE('',*,*,#59477,.T.);
#88287=ORIENTED_EDGE('',*,*,#59422,.T.);
#88288=ORIENTED_EDGE('',*,*,#59475,.F.);
#88289=ORIENTED_EDGE('',*,*,#59417,.F.);
#88290=ORIENTED_EDGE('',*,*,#59478,.T.);
#88291=ORIENTED_EDGE('',*,*,#59423,.T.);
#88292=ORIENTED_EDGE('',*,*,#59477,.F.);
#88293=ORIENTED_EDGE('',*,*,#59416,.F.);
#88294=ORIENTED_EDGE('',*,*,#59479,.T.);
#88295=ORIENTED_EDGE('',*,*,#59424,.T.);
#88296=ORIENTED_EDGE('',*,*,#59478,.F.);
#88297=ORIENTED_EDGE('',*,*,#59415,.F.);
#88298=ORIENTED_EDGE('',*,*,#59480,.T.);
#88299=ORIENTED_EDGE('',*,*,#59425,.T.);
#88300=ORIENTED_EDGE('',*,*,#59479,.F.);
#88301=ORIENTED_EDGE('',*,*,#59414,.F.);
#88302=ORIENTED_EDGE('',*,*,#59481,.T.);
#88303=ORIENTED_EDGE('',*,*,#59426,.T.);
#88304=ORIENTED_EDGE('',*,*,#59480,.F.);
#88305=ORIENTED_EDGE('',*,*,#59413,.F.);
#88306=ORIENTED_EDGE('',*,*,#59482,.T.);
#88307=ORIENTED_EDGE('',*,*,#59427,.T.);
#88308=ORIENTED_EDGE('',*,*,#59481,.F.);
#88309=ORIENTED_EDGE('',*,*,#59412,.F.);
#88310=ORIENTED_EDGE('',*,*,#59483,.T.);
#88311=ORIENTED_EDGE('',*,*,#59428,.T.);
#88312=ORIENTED_EDGE('',*,*,#59482,.F.);
#88313=ORIENTED_EDGE('',*,*,#59411,.F.);
#88314=ORIENTED_EDGE('',*,*,#59484,.T.);
#88315=ORIENTED_EDGE('',*,*,#59429,.T.);
#88316=ORIENTED_EDGE('',*,*,#59483,.F.);
#88317=ORIENTED_EDGE('',*,*,#59410,.F.);
#88318=ORIENTED_EDGE('',*,*,#59485,.T.);
#88319=ORIENTED_EDGE('',*,*,#59430,.T.);
#88320=ORIENTED_EDGE('',*,*,#59484,.F.);
#88321=ORIENTED_EDGE('',*,*,#59409,.F.);
#88322=ORIENTED_EDGE('',*,*,#59486,.T.);
#88323=ORIENTED_EDGE('',*,*,#59431,.T.);
#88324=ORIENTED_EDGE('',*,*,#59485,.F.);
#88325=ORIENTED_EDGE('',*,*,#59408,.F.);
#88326=ORIENTED_EDGE('',*,*,#59487,.T.);
#88327=ORIENTED_EDGE('',*,*,#59432,.T.);
#88328=ORIENTED_EDGE('',*,*,#59486,.F.);
#88329=ORIENTED_EDGE('',*,*,#59407,.F.);
#88330=ORIENTED_EDGE('',*,*,#59488,.T.);
#88331=ORIENTED_EDGE('',*,*,#59433,.T.);
#88332=ORIENTED_EDGE('',*,*,#59487,.F.);
#88333=ORIENTED_EDGE('',*,*,#59406,.F.);
#88334=ORIENTED_EDGE('',*,*,#59489,.T.);
#88335=ORIENTED_EDGE('',*,*,#59434,.T.);
#88336=ORIENTED_EDGE('',*,*,#59488,.F.);
#88337=ORIENTED_EDGE('',*,*,#59405,.F.);
#88338=ORIENTED_EDGE('',*,*,#59490,.T.);
#88339=ORIENTED_EDGE('',*,*,#59435,.T.);
#88340=ORIENTED_EDGE('',*,*,#59489,.F.);
#88341=ORIENTED_EDGE('',*,*,#59404,.F.);
#88342=ORIENTED_EDGE('',*,*,#59491,.T.);
#88343=ORIENTED_EDGE('',*,*,#59436,.T.);
#88344=ORIENTED_EDGE('',*,*,#59490,.F.);
#88345=ORIENTED_EDGE('',*,*,#59403,.F.);
#88346=ORIENTED_EDGE('',*,*,#59492,.T.);
#88347=ORIENTED_EDGE('',*,*,#59437,.T.);
#88348=ORIENTED_EDGE('',*,*,#59491,.F.);
#88349=ORIENTED_EDGE('',*,*,#59402,.F.);
#88350=ORIENTED_EDGE('',*,*,#59493,.T.);
#88351=ORIENTED_EDGE('',*,*,#59438,.T.);
#88352=ORIENTED_EDGE('',*,*,#59492,.F.);
#88353=ORIENTED_EDGE('',*,*,#59401,.F.);
#88354=ORIENTED_EDGE('',*,*,#59494,.T.);
#88355=ORIENTED_EDGE('',*,*,#59439,.T.);
#88356=ORIENTED_EDGE('',*,*,#59493,.F.);
#88357=ORIENTED_EDGE('',*,*,#59400,.F.);
#88358=ORIENTED_EDGE('',*,*,#59495,.T.);
#88359=ORIENTED_EDGE('',*,*,#59440,.T.);
#88360=ORIENTED_EDGE('',*,*,#59494,.F.);
#88361=ORIENTED_EDGE('',*,*,#59399,.F.);
#88362=ORIENTED_EDGE('',*,*,#59496,.T.);
#88363=ORIENTED_EDGE('',*,*,#59441,.T.);
#88364=ORIENTED_EDGE('',*,*,#59495,.F.);
#88365=ORIENTED_EDGE('',*,*,#59398,.F.);
#88366=ORIENTED_EDGE('',*,*,#59497,.T.);
#88367=ORIENTED_EDGE('',*,*,#59442,.T.);
#88368=ORIENTED_EDGE('',*,*,#59496,.F.);
#88369=ORIENTED_EDGE('',*,*,#59397,.F.);
#88370=ORIENTED_EDGE('',*,*,#59498,.T.);
#88371=ORIENTED_EDGE('',*,*,#59443,.T.);
#88372=ORIENTED_EDGE('',*,*,#59497,.F.);
#88373=ORIENTED_EDGE('',*,*,#59396,.F.);
#88374=ORIENTED_EDGE('',*,*,#59499,.T.);
#88375=ORIENTED_EDGE('',*,*,#59444,.T.);
#88376=ORIENTED_EDGE('',*,*,#59498,.F.);
#88377=ORIENTED_EDGE('',*,*,#59395,.F.);
#88378=ORIENTED_EDGE('',*,*,#59500,.T.);
#88379=ORIENTED_EDGE('',*,*,#59445,.T.);
#88380=ORIENTED_EDGE('',*,*,#59499,.F.);
#88381=ORIENTED_EDGE('',*,*,#59394,.F.);
#88382=ORIENTED_EDGE('',*,*,#59501,.T.);
#88383=ORIENTED_EDGE('',*,*,#59446,.T.);
#88384=ORIENTED_EDGE('',*,*,#59500,.F.);
#88385=ORIENTED_EDGE('',*,*,#59393,.F.);
#88386=ORIENTED_EDGE('',*,*,#59502,.T.);
#88387=ORIENTED_EDGE('',*,*,#59447,.T.);
#88388=ORIENTED_EDGE('',*,*,#59501,.F.);
#88389=ORIENTED_EDGE('',*,*,#59392,.F.);
#88390=ORIENTED_EDGE('',*,*,#59503,.T.);
#88391=ORIENTED_EDGE('',*,*,#59448,.T.);
#88392=ORIENTED_EDGE('',*,*,#59502,.F.);
#88393=ORIENTED_EDGE('',*,*,#59391,.F.);
#88394=ORIENTED_EDGE('',*,*,#59504,.T.);
#88395=ORIENTED_EDGE('',*,*,#59449,.T.);
#88396=ORIENTED_EDGE('',*,*,#59503,.F.);
#88397=ORIENTED_EDGE('',*,*,#59390,.F.);
#88398=ORIENTED_EDGE('',*,*,#59505,.T.);
#88399=ORIENTED_EDGE('',*,*,#59450,.T.);
#88400=ORIENTED_EDGE('',*,*,#59504,.F.);
#88401=ORIENTED_EDGE('',*,*,#59389,.F.);
#88402=ORIENTED_EDGE('',*,*,#59506,.T.);
#88403=ORIENTED_EDGE('',*,*,#59451,.T.);
#88404=ORIENTED_EDGE('',*,*,#59505,.F.);
#88405=ORIENTED_EDGE('',*,*,#59388,.F.);
#88406=ORIENTED_EDGE('',*,*,#59507,.T.);
#88407=ORIENTED_EDGE('',*,*,#59452,.T.);
#88408=ORIENTED_EDGE('',*,*,#59506,.F.);
#88409=ORIENTED_EDGE('',*,*,#59387,.F.);
#88410=ORIENTED_EDGE('',*,*,#59508,.T.);
#88411=ORIENTED_EDGE('',*,*,#59453,.T.);
#88412=ORIENTED_EDGE('',*,*,#59507,.F.);
#88413=ORIENTED_EDGE('',*,*,#59386,.F.);
#88414=ORIENTED_EDGE('',*,*,#59509,.T.);
#88415=ORIENTED_EDGE('',*,*,#59454,.T.);
#88416=ORIENTED_EDGE('',*,*,#59508,.F.);
#88417=ORIENTED_EDGE('',*,*,#59385,.F.);
#88418=ORIENTED_EDGE('',*,*,#59510,.T.);
#88419=ORIENTED_EDGE('',*,*,#59455,.T.);
#88420=ORIENTED_EDGE('',*,*,#59509,.F.);
#88421=ORIENTED_EDGE('',*,*,#59384,.F.);
#88422=ORIENTED_EDGE('',*,*,#59511,.T.);
#88423=ORIENTED_EDGE('',*,*,#59456,.T.);
#88424=ORIENTED_EDGE('',*,*,#59510,.F.);
#88425=ORIENTED_EDGE('',*,*,#59383,.F.);
#88426=ORIENTED_EDGE('',*,*,#59512,.T.);
#88427=ORIENTED_EDGE('',*,*,#59457,.T.);
#88428=ORIENTED_EDGE('',*,*,#59511,.F.);
#88429=ORIENTED_EDGE('',*,*,#59382,.F.);
#88430=ORIENTED_EDGE('',*,*,#59513,.T.);
#88431=ORIENTED_EDGE('',*,*,#59458,.T.);
#88432=ORIENTED_EDGE('',*,*,#59512,.F.);
#88433=ORIENTED_EDGE('',*,*,#59381,.F.);
#88434=ORIENTED_EDGE('',*,*,#59514,.T.);
#88435=ORIENTED_EDGE('',*,*,#59459,.T.);
#88436=ORIENTED_EDGE('',*,*,#59513,.F.);
#88437=ORIENTED_EDGE('',*,*,#59380,.F.);
#88438=ORIENTED_EDGE('',*,*,#59515,.T.);
#88439=ORIENTED_EDGE('',*,*,#59460,.T.);
#88440=ORIENTED_EDGE('',*,*,#59514,.F.);
#88441=ORIENTED_EDGE('',*,*,#59379,.F.);
#88442=ORIENTED_EDGE('',*,*,#59516,.T.);
#88443=ORIENTED_EDGE('',*,*,#59461,.T.);
#88444=ORIENTED_EDGE('',*,*,#59515,.F.);
#88445=ORIENTED_EDGE('',*,*,#59378,.F.);
#88446=ORIENTED_EDGE('',*,*,#59517,.T.);
#88447=ORIENTED_EDGE('',*,*,#59462,.T.);
#88448=ORIENTED_EDGE('',*,*,#59516,.F.);
#88449=ORIENTED_EDGE('',*,*,#59377,.F.);
#88450=ORIENTED_EDGE('',*,*,#59518,.T.);
#88451=ORIENTED_EDGE('',*,*,#59463,.T.);
#88452=ORIENTED_EDGE('',*,*,#59517,.F.);
#88453=ORIENTED_EDGE('',*,*,#59376,.F.);
#88454=ORIENTED_EDGE('',*,*,#59519,.T.);
#88455=ORIENTED_EDGE('',*,*,#59464,.T.);
#88456=ORIENTED_EDGE('',*,*,#59518,.F.);
#88457=ORIENTED_EDGE('',*,*,#59375,.F.);
#88458=ORIENTED_EDGE('',*,*,#59520,.T.);
#88459=ORIENTED_EDGE('',*,*,#59465,.T.);
#88460=ORIENTED_EDGE('',*,*,#59519,.F.);
#88461=ORIENTED_EDGE('',*,*,#59374,.F.);
#88462=ORIENTED_EDGE('',*,*,#59521,.T.);
#88463=ORIENTED_EDGE('',*,*,#59466,.T.);
#88464=ORIENTED_EDGE('',*,*,#59520,.F.);
#88465=ORIENTED_EDGE('',*,*,#59373,.F.);
#88466=ORIENTED_EDGE('',*,*,#59522,.T.);
#88467=ORIENTED_EDGE('',*,*,#59467,.T.);
#88468=ORIENTED_EDGE('',*,*,#59521,.F.);
#88469=ORIENTED_EDGE('',*,*,#59372,.F.);
#88470=ORIENTED_EDGE('',*,*,#59523,.T.);
#88471=ORIENTED_EDGE('',*,*,#59468,.T.);
#88472=ORIENTED_EDGE('',*,*,#59522,.F.);
#88473=ORIENTED_EDGE('',*,*,#59371,.F.);
#88474=ORIENTED_EDGE('',*,*,#59524,.T.);
#88475=ORIENTED_EDGE('',*,*,#59469,.T.);
#88476=ORIENTED_EDGE('',*,*,#59523,.F.);
#88477=ORIENTED_EDGE('',*,*,#59370,.F.);
#88478=ORIENTED_EDGE('',*,*,#59525,.T.);
#88479=ORIENTED_EDGE('',*,*,#59470,.T.);
#88480=ORIENTED_EDGE('',*,*,#59524,.F.);
#88481=ORIENTED_EDGE('',*,*,#59369,.F.);
#88482=ORIENTED_EDGE('',*,*,#59526,.T.);
#88483=ORIENTED_EDGE('',*,*,#59471,.T.);
#88484=ORIENTED_EDGE('',*,*,#59525,.F.);
#88485=ORIENTED_EDGE('',*,*,#59368,.F.);
#88486=ORIENTED_EDGE('',*,*,#59527,.T.);
#88487=ORIENTED_EDGE('',*,*,#59472,.T.);
#88488=ORIENTED_EDGE('',*,*,#59526,.F.);
#88489=ORIENTED_EDGE('',*,*,#59367,.F.);
#88490=ORIENTED_EDGE('',*,*,#59528,.T.);
#88491=ORIENTED_EDGE('',*,*,#59473,.T.);
#88492=ORIENTED_EDGE('',*,*,#59527,.F.);
#88493=ORIENTED_EDGE('',*,*,#59366,.F.);
#88494=ORIENTED_EDGE('',*,*,#59529,.T.);
#88495=ORIENTED_EDGE('',*,*,#59474,.T.);
#88496=ORIENTED_EDGE('',*,*,#59528,.F.);
#88497=ORIENTED_EDGE('',*,*,#59365,.F.);
#88498=ORIENTED_EDGE('',*,*,#59530,.T.);
#88499=ORIENTED_EDGE('',*,*,#59419,.T.);
#88500=ORIENTED_EDGE('',*,*,#59529,.F.);
#88501=ORIENTED_EDGE('',*,*,#59364,.F.);
#88502=ORIENTED_EDGE('',*,*,#59476,.T.);
#88503=ORIENTED_EDGE('',*,*,#59420,.T.);
#88504=ORIENTED_EDGE('',*,*,#59530,.F.);
#88505=ORIENTED_EDGE('',*,*,#59531,.T.);
#88506=ORIENTED_EDGE('',*,*,#59532,.T.);
#88507=ORIENTED_EDGE('',*,*,#59533,.F.);
#88508=ORIENTED_EDGE('',*,*,#59534,.F.);
#88509=ORIENTED_EDGE('',*,*,#59535,.T.);
#88510=ORIENTED_EDGE('',*,*,#59536,.T.);
#88511=ORIENTED_EDGE('',*,*,#59537,.T.);
#88512=ORIENTED_EDGE('',*,*,#59538,.T.);
#88513=ORIENTED_EDGE('',*,*,#59539,.T.);
#88514=ORIENTED_EDGE('',*,*,#59540,.T.);
#88515=ORIENTED_EDGE('',*,*,#59533,.T.);
#88516=ORIENTED_EDGE('',*,*,#59541,.T.);
#88517=ORIENTED_EDGE('',*,*,#59542,.T.);
#88518=ORIENTED_EDGE('',*,*,#59543,.T.);
#88519=ORIENTED_EDGE('',*,*,#59544,.T.);
#88520=ORIENTED_EDGE('',*,*,#59545,.T.);
#88521=ORIENTED_EDGE('',*,*,#59546,.T.);
#88522=ORIENTED_EDGE('',*,*,#59547,.T.);
#88523=ORIENTED_EDGE('',*,*,#59548,.T.);
#88524=ORIENTED_EDGE('',*,*,#59549,.T.);
#88525=ORIENTED_EDGE('',*,*,#59550,.F.);
#88526=ORIENTED_EDGE('',*,*,#59551,.T.);
#88527=ORIENTED_EDGE('',*,*,#59552,.T.);
#88528=ORIENTED_EDGE('',*,*,#59549,.F.);
#88529=ORIENTED_EDGE('',*,*,#59553,.F.);
#88530=ORIENTED_EDGE('',*,*,#59554,.T.);
#88531=ORIENTED_EDGE('',*,*,#59550,.T.);
#88532=ORIENTED_EDGE('',*,*,#59548,.F.);
#88533=ORIENTED_EDGE('',*,*,#59555,.F.);
#88534=ORIENTED_EDGE('',*,*,#59556,.T.);
#88535=ORIENTED_EDGE('',*,*,#59553,.T.);
#88536=ORIENTED_EDGE('',*,*,#59547,.F.);
#88537=ORIENTED_EDGE('',*,*,#59557,.F.);
#88538=ORIENTED_EDGE('',*,*,#59558,.T.);
#88539=ORIENTED_EDGE('',*,*,#59555,.T.);
#88540=ORIENTED_EDGE('',*,*,#59546,.F.);
#88541=ORIENTED_EDGE('',*,*,#59559,.F.);
#88542=ORIENTED_EDGE('',*,*,#59560,.T.);
#88543=ORIENTED_EDGE('',*,*,#59557,.T.);
#88544=ORIENTED_EDGE('',*,*,#59545,.F.);
#88545=ORIENTED_EDGE('',*,*,#59561,.F.);
#88546=ORIENTED_EDGE('',*,*,#59562,.T.);
#88547=ORIENTED_EDGE('',*,*,#59559,.T.);
#88548=ORIENTED_EDGE('',*,*,#59544,.F.);
#88549=ORIENTED_EDGE('',*,*,#59563,.F.);
#88550=ORIENTED_EDGE('',*,*,#59564,.T.);
#88551=ORIENTED_EDGE('',*,*,#59561,.T.);
#88552=ORIENTED_EDGE('',*,*,#59543,.F.);
#88553=ORIENTED_EDGE('',*,*,#59565,.F.);
#88554=ORIENTED_EDGE('',*,*,#59566,.T.);
#88555=ORIENTED_EDGE('',*,*,#59563,.T.);
#88556=ORIENTED_EDGE('',*,*,#59542,.F.);
#88557=ORIENTED_EDGE('',*,*,#59532,.F.);
#88558=ORIENTED_EDGE('',*,*,#59567,.T.);
#88559=ORIENTED_EDGE('',*,*,#59565,.T.);
#88560=ORIENTED_EDGE('',*,*,#59541,.F.);
#88561=ORIENTED_EDGE('',*,*,#59568,.F.);
#88562=ORIENTED_EDGE('',*,*,#59569,.T.);
#88563=ORIENTED_EDGE('',*,*,#59534,.T.);
#88564=ORIENTED_EDGE('',*,*,#59540,.F.);
#88565=ORIENTED_EDGE('',*,*,#59570,.F.);
#88566=ORIENTED_EDGE('',*,*,#59571,.T.);
#88567=ORIENTED_EDGE('',*,*,#59568,.T.);
#88568=ORIENTED_EDGE('',*,*,#59539,.F.);
#88569=ORIENTED_EDGE('',*,*,#59572,.F.);
#88570=ORIENTED_EDGE('',*,*,#59573,.T.);
#88571=ORIENTED_EDGE('',*,*,#59570,.T.);
#88572=ORIENTED_EDGE('',*,*,#59538,.F.);
#88573=ORIENTED_EDGE('',*,*,#59574,.F.);
#88574=ORIENTED_EDGE('',*,*,#59575,.T.);
#88575=ORIENTED_EDGE('',*,*,#59572,.T.);
#88576=ORIENTED_EDGE('',*,*,#59537,.F.);
#88577=ORIENTED_EDGE('',*,*,#59576,.F.);
#88578=ORIENTED_EDGE('',*,*,#59577,.T.);
#88579=ORIENTED_EDGE('',*,*,#59574,.T.);
#88580=ORIENTED_EDGE('',*,*,#59536,.F.);
#88581=ORIENTED_EDGE('',*,*,#59552,.F.);
#88582=ORIENTED_EDGE('',*,*,#59578,.T.);
#88583=ORIENTED_EDGE('',*,*,#59576,.T.);
#88584=ORIENTED_EDGE('',*,*,#59535,.F.);
#88585=ORIENTED_EDGE('',*,*,#59578,.F.);
#88586=ORIENTED_EDGE('',*,*,#59551,.F.);
#88587=ORIENTED_EDGE('',*,*,#59554,.F.);
#88588=ORIENTED_EDGE('',*,*,#59556,.F.);
#88589=ORIENTED_EDGE('',*,*,#59558,.F.);
#88590=ORIENTED_EDGE('',*,*,#59560,.F.);
#88591=ORIENTED_EDGE('',*,*,#59562,.F.);
#88592=ORIENTED_EDGE('',*,*,#59564,.F.);
#88593=ORIENTED_EDGE('',*,*,#59566,.F.);
#88594=ORIENTED_EDGE('',*,*,#59567,.F.);
#88595=ORIENTED_EDGE('',*,*,#59531,.F.);
#88596=ORIENTED_EDGE('',*,*,#59569,.F.);
#88597=ORIENTED_EDGE('',*,*,#59571,.F.);
#88598=ORIENTED_EDGE('',*,*,#59573,.F.);
#88599=ORIENTED_EDGE('',*,*,#59575,.F.);
#88600=ORIENTED_EDGE('',*,*,#59577,.F.);
#88601=ORIENTED_EDGE('',*,*,#59579,.T.);
#88602=ORIENTED_EDGE('',*,*,#59580,.T.);
#88603=ORIENTED_EDGE('',*,*,#59581,.T.);
#88604=ORIENTED_EDGE('',*,*,#59582,.T.);
#88605=ORIENTED_EDGE('',*,*,#59583,.T.);
#88606=ORIENTED_EDGE('',*,*,#59584,.T.);
#88607=ORIENTED_EDGE('',*,*,#59585,.T.);
#88608=ORIENTED_EDGE('',*,*,#59586,.T.);
#88609=ORIENTED_EDGE('',*,*,#59587,.F.);
#88610=ORIENTED_EDGE('',*,*,#59588,.T.);
#88611=ORIENTED_EDGE('',*,*,#59589,.T.);
#88612=ORIENTED_EDGE('',*,*,#59586,.F.);
#88613=ORIENTED_EDGE('',*,*,#59590,.F.);
#88614=ORIENTED_EDGE('',*,*,#59591,.T.);
#88615=ORIENTED_EDGE('',*,*,#59587,.T.);
#88616=ORIENTED_EDGE('',*,*,#59585,.F.);
#88617=ORIENTED_EDGE('',*,*,#59592,.F.);
#88618=ORIENTED_EDGE('',*,*,#59593,.T.);
#88619=ORIENTED_EDGE('',*,*,#59590,.T.);
#88620=ORIENTED_EDGE('',*,*,#59584,.F.);
#88621=ORIENTED_EDGE('',*,*,#59594,.F.);
#88622=ORIENTED_EDGE('',*,*,#59595,.T.);
#88623=ORIENTED_EDGE('',*,*,#59592,.T.);
#88624=ORIENTED_EDGE('',*,*,#59583,.F.);
#88625=ORIENTED_EDGE('',*,*,#59596,.F.);
#88626=ORIENTED_EDGE('',*,*,#59597,.T.);
#88627=ORIENTED_EDGE('',*,*,#59594,.T.);
#88628=ORIENTED_EDGE('',*,*,#59582,.F.);
#88629=ORIENTED_EDGE('',*,*,#59598,.F.);
#88630=ORIENTED_EDGE('',*,*,#59599,.T.);
#88631=ORIENTED_EDGE('',*,*,#59596,.T.);
#88632=ORIENTED_EDGE('',*,*,#59581,.F.);
#88633=ORIENTED_EDGE('',*,*,#59600,.F.);
#88634=ORIENTED_EDGE('',*,*,#59601,.T.);
#88635=ORIENTED_EDGE('',*,*,#59598,.T.);
#88636=ORIENTED_EDGE('',*,*,#59580,.F.);
#88637=ORIENTED_EDGE('',*,*,#59589,.F.);
#88638=ORIENTED_EDGE('',*,*,#59602,.T.);
#88639=ORIENTED_EDGE('',*,*,#59600,.T.);
#88640=ORIENTED_EDGE('',*,*,#59579,.F.);
#88641=ORIENTED_EDGE('',*,*,#59602,.F.);
#88642=ORIENTED_EDGE('',*,*,#59588,.F.);
#88643=ORIENTED_EDGE('',*,*,#59591,.F.);
#88644=ORIENTED_EDGE('',*,*,#59593,.F.);
#88645=ORIENTED_EDGE('',*,*,#59595,.F.);
#88646=ORIENTED_EDGE('',*,*,#59597,.F.);
#88647=ORIENTED_EDGE('',*,*,#59599,.F.);
#88648=ORIENTED_EDGE('',*,*,#59601,.F.);
#88649=ORIENTED_EDGE('',*,*,#59603,.T.);
#88650=ORIENTED_EDGE('',*,*,#59604,.T.);
#88651=ORIENTED_EDGE('',*,*,#59605,.F.);
#88652=ORIENTED_EDGE('',*,*,#59606,.F.);
#88653=ORIENTED_EDGE('',*,*,#59607,.T.);
#88654=ORIENTED_EDGE('',*,*,#59608,.T.);
#88655=ORIENTED_EDGE('',*,*,#59605,.T.);
#88656=ORIENTED_EDGE('',*,*,#59609,.T.);
#88657=ORIENTED_EDGE('',*,*,#59610,.T.);
#88658=ORIENTED_EDGE('',*,*,#59611,.T.);
#88659=ORIENTED_EDGE('',*,*,#59612,.T.);
#88660=ORIENTED_EDGE('',*,*,#59613,.T.);
#88661=ORIENTED_EDGE('',*,*,#59614,.T.);
#88662=ORIENTED_EDGE('',*,*,#59615,.T.);
#88663=ORIENTED_EDGE('',*,*,#59616,.T.);
#88664=ORIENTED_EDGE('',*,*,#59617,.T.);
#88665=ORIENTED_EDGE('',*,*,#59618,.T.);
#88666=ORIENTED_EDGE('',*,*,#59619,.T.);
#88667=ORIENTED_EDGE('',*,*,#59620,.T.);
#88668=ORIENTED_EDGE('',*,*,#59621,.T.);
#88669=ORIENTED_EDGE('',*,*,#59622,.F.);
#88670=ORIENTED_EDGE('',*,*,#59623,.T.);
#88671=ORIENTED_EDGE('',*,*,#59624,.T.);
#88672=ORIENTED_EDGE('',*,*,#59621,.F.);
#88673=ORIENTED_EDGE('',*,*,#59625,.F.);
#88674=ORIENTED_EDGE('',*,*,#59626,.T.);
#88675=ORIENTED_EDGE('',*,*,#59622,.T.);
#88676=ORIENTED_EDGE('',*,*,#59620,.F.);
#88677=ORIENTED_EDGE('',*,*,#59627,.F.);
#88678=ORIENTED_EDGE('',*,*,#59628,.T.);
#88679=ORIENTED_EDGE('',*,*,#59625,.T.);
#88680=ORIENTED_EDGE('',*,*,#59619,.F.);
#88681=ORIENTED_EDGE('',*,*,#59629,.F.);
#88682=ORIENTED_EDGE('',*,*,#59630,.T.);
#88683=ORIENTED_EDGE('',*,*,#59627,.T.);
#88684=ORIENTED_EDGE('',*,*,#59618,.F.);
#88685=ORIENTED_EDGE('',*,*,#59631,.F.);
#88686=ORIENTED_EDGE('',*,*,#59632,.T.);
#88687=ORIENTED_EDGE('',*,*,#59629,.T.);
#88688=ORIENTED_EDGE('',*,*,#59617,.F.);
#88689=ORIENTED_EDGE('',*,*,#59633,.F.);
#88690=ORIENTED_EDGE('',*,*,#59634,.T.);
#88691=ORIENTED_EDGE('',*,*,#59631,.T.);
#88692=ORIENTED_EDGE('',*,*,#59616,.F.);
#88693=ORIENTED_EDGE('',*,*,#59635,.F.);
#88694=ORIENTED_EDGE('',*,*,#59636,.T.);
#88695=ORIENTED_EDGE('',*,*,#59633,.T.);
#88696=ORIENTED_EDGE('',*,*,#59615,.F.);
#88697=ORIENTED_EDGE('',*,*,#59637,.F.);
#88698=ORIENTED_EDGE('',*,*,#59638,.T.);
#88699=ORIENTED_EDGE('',*,*,#59635,.T.);
#88700=ORIENTED_EDGE('',*,*,#59614,.F.);
#88701=ORIENTED_EDGE('',*,*,#59639,.F.);
#88702=ORIENTED_EDGE('',*,*,#59640,.T.);
#88703=ORIENTED_EDGE('',*,*,#59637,.T.);
#88704=ORIENTED_EDGE('',*,*,#59613,.F.);
#88705=ORIENTED_EDGE('',*,*,#59641,.F.);
#88706=ORIENTED_EDGE('',*,*,#59642,.T.);
#88707=ORIENTED_EDGE('',*,*,#59639,.T.);
#88708=ORIENTED_EDGE('',*,*,#59612,.F.);
#88709=ORIENTED_EDGE('',*,*,#59643,.F.);
#88710=ORIENTED_EDGE('',*,*,#59644,.T.);
#88711=ORIENTED_EDGE('',*,*,#59641,.T.);
#88712=ORIENTED_EDGE('',*,*,#59611,.F.);
#88713=ORIENTED_EDGE('',*,*,#59645,.F.);
#88714=ORIENTED_EDGE('',*,*,#59646,.T.);
#88715=ORIENTED_EDGE('',*,*,#59643,.T.);
#88716=ORIENTED_EDGE('',*,*,#59610,.F.);
#88717=ORIENTED_EDGE('',*,*,#59604,.F.);
#88718=ORIENTED_EDGE('',*,*,#59647,.T.);
#88719=ORIENTED_EDGE('',*,*,#59645,.T.);
#88720=ORIENTED_EDGE('',*,*,#59609,.F.);
#88721=ORIENTED_EDGE('',*,*,#59648,.F.);
#88722=ORIENTED_EDGE('',*,*,#59649,.T.);
#88723=ORIENTED_EDGE('',*,*,#59606,.T.);
#88724=ORIENTED_EDGE('',*,*,#59608,.F.);
#88725=ORIENTED_EDGE('',*,*,#59624,.F.);
#88726=ORIENTED_EDGE('',*,*,#59650,.T.);
#88727=ORIENTED_EDGE('',*,*,#59648,.T.);
#88728=ORIENTED_EDGE('',*,*,#59607,.F.);
#88729=ORIENTED_EDGE('',*,*,#59650,.F.);
#88730=ORIENTED_EDGE('',*,*,#59623,.F.);
#88731=ORIENTED_EDGE('',*,*,#59626,.F.);
#88732=ORIENTED_EDGE('',*,*,#59628,.F.);
#88733=ORIENTED_EDGE('',*,*,#59630,.F.);
#88734=ORIENTED_EDGE('',*,*,#59632,.F.);
#88735=ORIENTED_EDGE('',*,*,#59634,.F.);
#88736=ORIENTED_EDGE('',*,*,#59636,.F.);
#88737=ORIENTED_EDGE('',*,*,#59638,.F.);
#88738=ORIENTED_EDGE('',*,*,#59640,.F.);
#88739=ORIENTED_EDGE('',*,*,#59642,.F.);
#88740=ORIENTED_EDGE('',*,*,#59644,.F.);
#88741=ORIENTED_EDGE('',*,*,#59646,.F.);
#88742=ORIENTED_EDGE('',*,*,#59647,.F.);
#88743=ORIENTED_EDGE('',*,*,#59603,.F.);
#88744=ORIENTED_EDGE('',*,*,#59649,.F.);
#88745=ORIENTED_EDGE('',*,*,#59651,.T.);
#88746=ORIENTED_EDGE('',*,*,#59652,.T.);
#88747=ORIENTED_EDGE('',*,*,#59653,.T.);
#88748=ORIENTED_EDGE('',*,*,#59654,.T.);
#88749=ORIENTED_EDGE('',*,*,#59655,.T.);
#88750=ORIENTED_EDGE('',*,*,#59656,.T.);
#88751=ORIENTED_EDGE('',*,*,#59657,.T.);
#88752=ORIENTED_EDGE('',*,*,#59658,.T.);
#88753=ORIENTED_EDGE('',*,*,#59659,.F.);
#88754=ORIENTED_EDGE('',*,*,#59660,.T.);
#88755=ORIENTED_EDGE('',*,*,#59661,.T.);
#88756=ORIENTED_EDGE('',*,*,#59658,.F.);
#88757=ORIENTED_EDGE('',*,*,#59662,.F.);
#88758=ORIENTED_EDGE('',*,*,#59663,.T.);
#88759=ORIENTED_EDGE('',*,*,#59659,.T.);
#88760=ORIENTED_EDGE('',*,*,#59657,.F.);
#88761=ORIENTED_EDGE('',*,*,#59664,.F.);
#88762=ORIENTED_EDGE('',*,*,#59665,.T.);
#88763=ORIENTED_EDGE('',*,*,#59662,.T.);
#88764=ORIENTED_EDGE('',*,*,#59656,.F.);
#88765=ORIENTED_EDGE('',*,*,#59666,.F.);
#88766=ORIENTED_EDGE('',*,*,#59667,.T.);
#88767=ORIENTED_EDGE('',*,*,#59664,.T.);
#88768=ORIENTED_EDGE('',*,*,#59655,.F.);
#88769=ORIENTED_EDGE('',*,*,#59668,.F.);
#88770=ORIENTED_EDGE('',*,*,#59669,.T.);
#88771=ORIENTED_EDGE('',*,*,#59666,.T.);
#88772=ORIENTED_EDGE('',*,*,#59654,.F.);
#88773=ORIENTED_EDGE('',*,*,#59670,.F.);
#88774=ORIENTED_EDGE('',*,*,#59671,.T.);
#88775=ORIENTED_EDGE('',*,*,#59668,.T.);
#88776=ORIENTED_EDGE('',*,*,#59653,.F.);
#88777=ORIENTED_EDGE('',*,*,#59672,.F.);
#88778=ORIENTED_EDGE('',*,*,#59673,.T.);
#88779=ORIENTED_EDGE('',*,*,#59670,.T.);
#88780=ORIENTED_EDGE('',*,*,#59652,.F.);
#88781=ORIENTED_EDGE('',*,*,#59661,.F.);
#88782=ORIENTED_EDGE('',*,*,#59674,.T.);
#88783=ORIENTED_EDGE('',*,*,#59672,.T.);
#88784=ORIENTED_EDGE('',*,*,#59651,.F.);
#88785=ORIENTED_EDGE('',*,*,#59674,.F.);
#88786=ORIENTED_EDGE('',*,*,#59660,.F.);
#88787=ORIENTED_EDGE('',*,*,#59663,.F.);
#88788=ORIENTED_EDGE('',*,*,#59665,.F.);
#88789=ORIENTED_EDGE('',*,*,#59667,.F.);
#88790=ORIENTED_EDGE('',*,*,#59669,.F.);
#88791=ORIENTED_EDGE('',*,*,#59671,.F.);
#88792=ORIENTED_EDGE('',*,*,#59673,.F.);
#88793=ORIENTED_EDGE('',*,*,#59675,.T.);
#88794=ORIENTED_EDGE('',*,*,#59676,.T.);
#88795=ORIENTED_EDGE('',*,*,#59677,.F.);
#88796=ORIENTED_EDGE('',*,*,#59678,.F.);
#88797=ORIENTED_EDGE('',*,*,#59679,.T.);
#88798=ORIENTED_EDGE('',*,*,#59680,.T.);
#88799=ORIENTED_EDGE('',*,*,#59677,.T.);
#88800=ORIENTED_EDGE('',*,*,#59681,.T.);
#88801=ORIENTED_EDGE('',*,*,#59682,.T.);
#88802=ORIENTED_EDGE('',*,*,#59683,.T.);
#88803=ORIENTED_EDGE('',*,*,#59684,.T.);
#88804=ORIENTED_EDGE('',*,*,#59685,.T.);
#88805=ORIENTED_EDGE('',*,*,#59686,.T.);
#88806=ORIENTED_EDGE('',*,*,#59687,.T.);
#88807=ORIENTED_EDGE('',*,*,#59688,.T.);
#88808=ORIENTED_EDGE('',*,*,#59689,.T.);
#88809=ORIENTED_EDGE('',*,*,#59690,.T.);
#88810=ORIENTED_EDGE('',*,*,#59691,.T.);
#88811=ORIENTED_EDGE('',*,*,#59692,.T.);
#88812=ORIENTED_EDGE('',*,*,#59693,.T.);
#88813=ORIENTED_EDGE('',*,*,#59694,.F.);
#88814=ORIENTED_EDGE('',*,*,#59695,.T.);
#88815=ORIENTED_EDGE('',*,*,#59696,.T.);
#88816=ORIENTED_EDGE('',*,*,#59693,.F.);
#88817=ORIENTED_EDGE('',*,*,#59697,.F.);
#88818=ORIENTED_EDGE('',*,*,#59698,.T.);
#88819=ORIENTED_EDGE('',*,*,#59694,.T.);
#88820=ORIENTED_EDGE('',*,*,#59692,.F.);
#88821=ORIENTED_EDGE('',*,*,#59699,.F.);
#88822=ORIENTED_EDGE('',*,*,#59700,.T.);
#88823=ORIENTED_EDGE('',*,*,#59697,.T.);
#88824=ORIENTED_EDGE('',*,*,#59691,.F.);
#88825=ORIENTED_EDGE('',*,*,#59701,.F.);
#88826=ORIENTED_EDGE('',*,*,#59702,.T.);
#88827=ORIENTED_EDGE('',*,*,#59699,.T.);
#88828=ORIENTED_EDGE('',*,*,#59690,.F.);
#88829=ORIENTED_EDGE('',*,*,#59703,.F.);
#88830=ORIENTED_EDGE('',*,*,#59704,.T.);
#88831=ORIENTED_EDGE('',*,*,#59701,.T.);
#88832=ORIENTED_EDGE('',*,*,#59689,.F.);
#88833=ORIENTED_EDGE('',*,*,#59705,.F.);
#88834=ORIENTED_EDGE('',*,*,#59706,.T.);
#88835=ORIENTED_EDGE('',*,*,#59703,.T.);
#88836=ORIENTED_EDGE('',*,*,#59688,.F.);
#88837=ORIENTED_EDGE('',*,*,#59707,.F.);
#88838=ORIENTED_EDGE('',*,*,#59708,.T.);
#88839=ORIENTED_EDGE('',*,*,#59705,.T.);
#88840=ORIENTED_EDGE('',*,*,#59687,.F.);
#88841=ORIENTED_EDGE('',*,*,#59709,.F.);
#88842=ORIENTED_EDGE('',*,*,#59710,.T.);
#88843=ORIENTED_EDGE('',*,*,#59707,.T.);
#88844=ORIENTED_EDGE('',*,*,#59686,.F.);
#88845=ORIENTED_EDGE('',*,*,#59711,.F.);
#88846=ORIENTED_EDGE('',*,*,#59712,.T.);
#88847=ORIENTED_EDGE('',*,*,#59709,.T.);
#88848=ORIENTED_EDGE('',*,*,#59685,.F.);
#88849=ORIENTED_EDGE('',*,*,#59713,.F.);
#88850=ORIENTED_EDGE('',*,*,#59714,.T.);
#88851=ORIENTED_EDGE('',*,*,#59711,.T.);
#88852=ORIENTED_EDGE('',*,*,#59684,.F.);
#88853=ORIENTED_EDGE('',*,*,#59715,.F.);
#88854=ORIENTED_EDGE('',*,*,#59716,.T.);
#88855=ORIENTED_EDGE('',*,*,#59713,.T.);
#88856=ORIENTED_EDGE('',*,*,#59683,.F.);
#88857=ORIENTED_EDGE('',*,*,#59717,.F.);
#88858=ORIENTED_EDGE('',*,*,#59718,.T.);
#88859=ORIENTED_EDGE('',*,*,#59715,.T.);
#88860=ORIENTED_EDGE('',*,*,#59682,.F.);
#88861=ORIENTED_EDGE('',*,*,#59676,.F.);
#88862=ORIENTED_EDGE('',*,*,#59719,.T.);
#88863=ORIENTED_EDGE('',*,*,#59717,.T.);
#88864=ORIENTED_EDGE('',*,*,#59681,.F.);
#88865=ORIENTED_EDGE('',*,*,#59720,.F.);
#88866=ORIENTED_EDGE('',*,*,#59721,.T.);
#88867=ORIENTED_EDGE('',*,*,#59678,.T.);
#88868=ORIENTED_EDGE('',*,*,#59680,.F.);
#88869=ORIENTED_EDGE('',*,*,#59696,.F.);
#88870=ORIENTED_EDGE('',*,*,#59722,.T.);
#88871=ORIENTED_EDGE('',*,*,#59720,.T.);
#88872=ORIENTED_EDGE('',*,*,#59679,.F.);
#88873=ORIENTED_EDGE('',*,*,#59722,.F.);
#88874=ORIENTED_EDGE('',*,*,#59695,.F.);
#88875=ORIENTED_EDGE('',*,*,#59698,.F.);
#88876=ORIENTED_EDGE('',*,*,#59700,.F.);
#88877=ORIENTED_EDGE('',*,*,#59702,.F.);
#88878=ORIENTED_EDGE('',*,*,#59704,.F.);
#88879=ORIENTED_EDGE('',*,*,#59706,.F.);
#88880=ORIENTED_EDGE('',*,*,#59708,.F.);
#88881=ORIENTED_EDGE('',*,*,#59710,.F.);
#88882=ORIENTED_EDGE('',*,*,#59712,.F.);
#88883=ORIENTED_EDGE('',*,*,#59714,.F.);
#88884=ORIENTED_EDGE('',*,*,#59716,.F.);
#88885=ORIENTED_EDGE('',*,*,#59718,.F.);
#88886=ORIENTED_EDGE('',*,*,#59719,.F.);
#88887=ORIENTED_EDGE('',*,*,#59675,.F.);
#88888=ORIENTED_EDGE('',*,*,#59721,.F.);
#88889=ORIENTED_EDGE('',*,*,#59723,.T.);
#88890=ORIENTED_EDGE('',*,*,#59724,.T.);
#88891=ORIENTED_EDGE('',*,*,#59725,.T.);
#88892=ORIENTED_EDGE('',*,*,#59726,.T.);
#88893=ORIENTED_EDGE('',*,*,#59727,.T.);
#88894=ORIENTED_EDGE('',*,*,#59728,.T.);
#88895=ORIENTED_EDGE('',*,*,#59729,.T.);
#88896=ORIENTED_EDGE('',*,*,#59730,.T.);
#88897=ORIENTED_EDGE('',*,*,#59731,.F.);
#88898=ORIENTED_EDGE('',*,*,#59732,.T.);
#88899=ORIENTED_EDGE('',*,*,#59733,.T.);
#88900=ORIENTED_EDGE('',*,*,#59730,.F.);
#88901=ORIENTED_EDGE('',*,*,#59734,.F.);
#88902=ORIENTED_EDGE('',*,*,#59735,.T.);
#88903=ORIENTED_EDGE('',*,*,#59731,.T.);
#88904=ORIENTED_EDGE('',*,*,#59729,.F.);
#88905=ORIENTED_EDGE('',*,*,#59736,.F.);
#88906=ORIENTED_EDGE('',*,*,#59737,.T.);
#88907=ORIENTED_EDGE('',*,*,#59734,.T.);
#88908=ORIENTED_EDGE('',*,*,#59728,.F.);
#88909=ORIENTED_EDGE('',*,*,#59738,.F.);
#88910=ORIENTED_EDGE('',*,*,#59739,.T.);
#88911=ORIENTED_EDGE('',*,*,#59736,.T.);
#88912=ORIENTED_EDGE('',*,*,#59727,.F.);
#88913=ORIENTED_EDGE('',*,*,#59740,.F.);
#88914=ORIENTED_EDGE('',*,*,#59741,.T.);
#88915=ORIENTED_EDGE('',*,*,#59738,.T.);
#88916=ORIENTED_EDGE('',*,*,#59726,.F.);
#88917=ORIENTED_EDGE('',*,*,#59742,.F.);
#88918=ORIENTED_EDGE('',*,*,#59743,.T.);
#88919=ORIENTED_EDGE('',*,*,#59740,.T.);
#88920=ORIENTED_EDGE('',*,*,#59725,.F.);
#88921=ORIENTED_EDGE('',*,*,#59744,.F.);
#88922=ORIENTED_EDGE('',*,*,#59745,.T.);
#88923=ORIENTED_EDGE('',*,*,#59742,.T.);
#88924=ORIENTED_EDGE('',*,*,#59724,.F.);
#88925=ORIENTED_EDGE('',*,*,#59733,.F.);
#88926=ORIENTED_EDGE('',*,*,#59746,.T.);
#88927=ORIENTED_EDGE('',*,*,#59744,.T.);
#88928=ORIENTED_EDGE('',*,*,#59723,.F.);
#88929=ORIENTED_EDGE('',*,*,#59746,.F.);
#88930=ORIENTED_EDGE('',*,*,#59732,.F.);
#88931=ORIENTED_EDGE('',*,*,#59735,.F.);
#88932=ORIENTED_EDGE('',*,*,#59737,.F.);
#88933=ORIENTED_EDGE('',*,*,#59739,.F.);
#88934=ORIENTED_EDGE('',*,*,#59741,.F.);
#88935=ORIENTED_EDGE('',*,*,#59743,.F.);
#88936=ORIENTED_EDGE('',*,*,#59745,.F.);
#88937=ORIENTED_EDGE('',*,*,#59747,.F.);
#88938=ORIENTED_EDGE('',*,*,#59748,.T.);
#88939=ORIENTED_EDGE('',*,*,#59749,.T.);
#88940=ORIENTED_EDGE('',*,*,#59750,.T.);
#88941=ORIENTED_EDGE('',*,*,#59751,.F.);
#88942=ORIENTED_EDGE('',*,*,#59752,.T.);
#88943=ORIENTED_EDGE('',*,*,#59753,.T.);
#88944=ORIENTED_EDGE('',*,*,#59754,.F.);
#88945=ORIENTED_EDGE('',*,*,#59755,.F.);
#88946=ORIENTED_EDGE('',*,*,#59756,.T.);
#88947=ORIENTED_EDGE('',*,*,#59757,.T.);
#88948=ORIENTED_EDGE('',*,*,#59758,.F.);
#88949=ORIENTED_EDGE('',*,*,#59759,.F.);
#88950=ORIENTED_EDGE('',*,*,#59758,.T.);
#88951=ORIENTED_EDGE('',*,*,#59760,.T.);
#88952=ORIENTED_EDGE('',*,*,#59761,.F.);
#88953=ORIENTED_EDGE('',*,*,#59762,.F.);
#88954=ORIENTED_EDGE('',*,*,#59761,.T.);
#88955=ORIENTED_EDGE('',*,*,#59763,.T.);
#88956=ORIENTED_EDGE('',*,*,#59764,.F.);
#88957=ORIENTED_EDGE('',*,*,#59765,.F.);
#88958=ORIENTED_EDGE('',*,*,#59764,.T.);
#88959=ORIENTED_EDGE('',*,*,#59766,.T.);
#88960=ORIENTED_EDGE('',*,*,#59767,.F.);
#88961=ORIENTED_EDGE('',*,*,#59768,.F.);
#88962=ORIENTED_EDGE('',*,*,#59767,.T.);
#88963=ORIENTED_EDGE('',*,*,#59769,.T.);
#88964=ORIENTED_EDGE('',*,*,#59770,.F.);
#88965=ORIENTED_EDGE('',*,*,#59771,.F.);
#88966=ORIENTED_EDGE('',*,*,#59770,.T.);
#88967=ORIENTED_EDGE('',*,*,#59772,.T.);
#88968=ORIENTED_EDGE('',*,*,#59773,.F.);
#88969=ORIENTED_EDGE('',*,*,#59774,.F.);
#88970=ORIENTED_EDGE('',*,*,#59773,.T.);
#88971=ORIENTED_EDGE('',*,*,#59775,.T.);
#88972=ORIENTED_EDGE('',*,*,#59776,.F.);
#88973=ORIENTED_EDGE('',*,*,#59777,.F.);
#88974=ORIENTED_EDGE('',*,*,#59776,.T.);
#88975=ORIENTED_EDGE('',*,*,#59778,.T.);
#88976=ORIENTED_EDGE('',*,*,#59779,.F.);
#88977=ORIENTED_EDGE('',*,*,#59780,.F.);
#88978=ORIENTED_EDGE('',*,*,#59779,.T.);
#88979=ORIENTED_EDGE('',*,*,#59781,.T.);
#88980=ORIENTED_EDGE('',*,*,#59782,.F.);
#88981=ORIENTED_EDGE('',*,*,#59783,.F.);
#88982=ORIENTED_EDGE('',*,*,#59782,.T.);
#88983=ORIENTED_EDGE('',*,*,#59784,.T.);
#88984=ORIENTED_EDGE('',*,*,#59785,.F.);
#88985=ORIENTED_EDGE('',*,*,#59786,.F.);
#88986=ORIENTED_EDGE('',*,*,#59785,.T.);
#88987=ORIENTED_EDGE('',*,*,#59787,.T.);
#88988=ORIENTED_EDGE('',*,*,#59788,.F.);
#88989=ORIENTED_EDGE('',*,*,#59789,.F.);
#88990=ORIENTED_EDGE('',*,*,#59788,.T.);
#88991=ORIENTED_EDGE('',*,*,#59790,.T.);
#88992=ORIENTED_EDGE('',*,*,#59791,.F.);
#88993=ORIENTED_EDGE('',*,*,#59792,.F.);
#88994=ORIENTED_EDGE('',*,*,#59791,.T.);
#88995=ORIENTED_EDGE('',*,*,#59793,.T.);
#88996=ORIENTED_EDGE('',*,*,#59794,.F.);
#88997=ORIENTED_EDGE('',*,*,#59795,.F.);
#88998=ORIENTED_EDGE('',*,*,#59794,.T.);
#88999=ORIENTED_EDGE('',*,*,#59796,.T.);
#89000=ORIENTED_EDGE('',*,*,#59797,.F.);
#89001=ORIENTED_EDGE('',*,*,#59798,.F.);
#89002=ORIENTED_EDGE('',*,*,#59799,.T.);
#89003=ORIENTED_EDGE('',*,*,#59800,.T.);
#89004=ORIENTED_EDGE('',*,*,#59801,.F.);
#89005=ORIENTED_EDGE('',*,*,#59802,.F.);
#89006=ORIENTED_EDGE('',*,*,#59801,.T.);
#89007=ORIENTED_EDGE('',*,*,#59803,.T.);
#89008=ORIENTED_EDGE('',*,*,#59804,.F.);
#89009=ORIENTED_EDGE('',*,*,#59805,.F.);
#89010=ORIENTED_EDGE('',*,*,#59804,.T.);
#89011=ORIENTED_EDGE('',*,*,#59806,.T.);
#89012=ORIENTED_EDGE('',*,*,#59807,.F.);
#89013=ORIENTED_EDGE('',*,*,#59808,.F.);
#89014=ORIENTED_EDGE('',*,*,#59807,.T.);
#89015=ORIENTED_EDGE('',*,*,#59809,.T.);
#89016=ORIENTED_EDGE('',*,*,#59810,.F.);
#89017=ORIENTED_EDGE('',*,*,#59811,.F.);
#89018=ORIENTED_EDGE('',*,*,#59810,.T.);
#89019=ORIENTED_EDGE('',*,*,#59812,.T.);
#89020=ORIENTED_EDGE('',*,*,#59813,.F.);
#89021=ORIENTED_EDGE('',*,*,#59814,.F.);
#89022=ORIENTED_EDGE('',*,*,#59813,.T.);
#89023=ORIENTED_EDGE('',*,*,#59815,.T.);
#89024=ORIENTED_EDGE('',*,*,#59816,.F.);
#89025=ORIENTED_EDGE('',*,*,#59817,.F.);
#89026=ORIENTED_EDGE('',*,*,#59816,.T.);
#89027=ORIENTED_EDGE('',*,*,#59818,.T.);
#89028=ORIENTED_EDGE('',*,*,#59819,.F.);
#89029=ORIENTED_EDGE('',*,*,#59820,.F.);
#89030=ORIENTED_EDGE('',*,*,#59819,.T.);
#89031=ORIENTED_EDGE('',*,*,#59821,.T.);
#89032=ORIENTED_EDGE('',*,*,#59822,.F.);
#89033=ORIENTED_EDGE('',*,*,#59823,.F.);
#89034=ORIENTED_EDGE('',*,*,#59822,.T.);
#89035=ORIENTED_EDGE('',*,*,#59824,.T.);
#89036=ORIENTED_EDGE('',*,*,#59825,.F.);
#89037=ORIENTED_EDGE('',*,*,#59826,.F.);
#89038=ORIENTED_EDGE('',*,*,#59825,.T.);
#89039=ORIENTED_EDGE('',*,*,#59827,.T.);
#89040=ORIENTED_EDGE('',*,*,#59828,.F.);
#89041=ORIENTED_EDGE('',*,*,#59829,.F.);
#89042=ORIENTED_EDGE('',*,*,#59828,.T.);
#89043=ORIENTED_EDGE('',*,*,#59830,.T.);
#89044=ORIENTED_EDGE('',*,*,#59831,.F.);
#89045=ORIENTED_EDGE('',*,*,#59832,.F.);
#89046=ORIENTED_EDGE('',*,*,#59831,.T.);
#89047=ORIENTED_EDGE('',*,*,#59833,.T.);
#89048=ORIENTED_EDGE('',*,*,#59834,.F.);
#89049=ORIENTED_EDGE('',*,*,#59835,.F.);
#89050=ORIENTED_EDGE('',*,*,#59834,.T.);
#89051=ORIENTED_EDGE('',*,*,#59836,.T.);
#89052=ORIENTED_EDGE('',*,*,#59837,.F.);
#89053=ORIENTED_EDGE('',*,*,#59838,.F.);
#89054=ORIENTED_EDGE('',*,*,#59837,.T.);
#89055=ORIENTED_EDGE('',*,*,#59839,.T.);
#89056=ORIENTED_EDGE('',*,*,#59840,.F.);
#89057=ORIENTED_EDGE('',*,*,#59841,.F.);
#89058=ORIENTED_EDGE('',*,*,#59840,.T.);
#89059=ORIENTED_EDGE('',*,*,#59842,.T.);
#89060=ORIENTED_EDGE('',*,*,#59843,.F.);
#89061=ORIENTED_EDGE('',*,*,#59844,.F.);
#89062=ORIENTED_EDGE('',*,*,#59843,.T.);
#89063=ORIENTED_EDGE('',*,*,#59845,.T.);
#89064=ORIENTED_EDGE('',*,*,#59846,.F.);
#89065=ORIENTED_EDGE('',*,*,#59847,.F.);
#89066=ORIENTED_EDGE('',*,*,#59846,.T.);
#89067=ORIENTED_EDGE('',*,*,#59848,.T.);
#89068=ORIENTED_EDGE('',*,*,#59849,.F.);
#89069=ORIENTED_EDGE('',*,*,#59850,.F.);
#89070=ORIENTED_EDGE('',*,*,#59849,.T.);
#89071=ORIENTED_EDGE('',*,*,#59851,.T.);
#89072=ORIENTED_EDGE('',*,*,#59852,.F.);
#89073=ORIENTED_EDGE('',*,*,#59853,.F.);
#89074=ORIENTED_EDGE('',*,*,#59852,.T.);
#89075=ORIENTED_EDGE('',*,*,#59854,.T.);
#89076=ORIENTED_EDGE('',*,*,#59855,.F.);
#89077=ORIENTED_EDGE('',*,*,#59856,.F.);
#89078=ORIENTED_EDGE('',*,*,#59855,.T.);
#89079=ORIENTED_EDGE('',*,*,#59857,.T.);
#89080=ORIENTED_EDGE('',*,*,#59748,.F.);
#89081=ORIENTED_EDGE('',*,*,#59858,.F.);
#89082=ORIENTED_EDGE('',*,*,#59859,.T.);
#89083=ORIENTED_EDGE('',*,*,#59860,.T.);
#89084=ORIENTED_EDGE('',*,*,#59861,.F.);
#89085=ORIENTED_EDGE('',*,*,#59862,.F.);
#89086=ORIENTED_EDGE('',*,*,#59861,.T.);
#89087=ORIENTED_EDGE('',*,*,#59863,.T.);
#89088=ORIENTED_EDGE('',*,*,#59864,.F.);
#89089=ORIENTED_EDGE('',*,*,#59865,.F.);
#89090=ORIENTED_EDGE('',*,*,#59864,.T.);
#89091=ORIENTED_EDGE('',*,*,#59866,.T.);
#89092=ORIENTED_EDGE('',*,*,#59867,.F.);
#89093=ORIENTED_EDGE('',*,*,#59868,.F.);
#89094=ORIENTED_EDGE('',*,*,#59867,.T.);
#89095=ORIENTED_EDGE('',*,*,#59869,.T.);
#89096=ORIENTED_EDGE('',*,*,#59870,.F.);
#89097=ORIENTED_EDGE('',*,*,#59871,.F.);
#89098=ORIENTED_EDGE('',*,*,#59870,.T.);
#89099=ORIENTED_EDGE('',*,*,#59872,.T.);
#89100=ORIENTED_EDGE('',*,*,#59873,.F.);
#89101=ORIENTED_EDGE('',*,*,#59874,.F.);
#89102=ORIENTED_EDGE('',*,*,#59873,.T.);
#89103=ORIENTED_EDGE('',*,*,#59875,.T.);
#89104=ORIENTED_EDGE('',*,*,#59876,.F.);
#89105=ORIENTED_EDGE('',*,*,#59877,.F.);
#89106=ORIENTED_EDGE('',*,*,#59876,.T.);
#89107=ORIENTED_EDGE('',*,*,#59878,.T.);
#89108=ORIENTED_EDGE('',*,*,#59879,.F.);
#89109=ORIENTED_EDGE('',*,*,#59880,.F.);
#89110=ORIENTED_EDGE('',*,*,#59879,.T.);
#89111=ORIENTED_EDGE('',*,*,#59881,.T.);
#89112=ORIENTED_EDGE('',*,*,#59882,.F.);
#89113=ORIENTED_EDGE('',*,*,#59883,.F.);
#89114=ORIENTED_EDGE('',*,*,#59882,.T.);
#89115=ORIENTED_EDGE('',*,*,#59884,.T.);
#89116=ORIENTED_EDGE('',*,*,#59885,.F.);
#89117=ORIENTED_EDGE('',*,*,#59886,.F.);
#89118=ORIENTED_EDGE('',*,*,#59885,.T.);
#89119=ORIENTED_EDGE('',*,*,#59887,.T.);
#89120=ORIENTED_EDGE('',*,*,#59888,.F.);
#89121=ORIENTED_EDGE('',*,*,#59889,.F.);
#89122=ORIENTED_EDGE('',*,*,#59888,.T.);
#89123=ORIENTED_EDGE('',*,*,#59890,.T.);
#89124=ORIENTED_EDGE('',*,*,#59891,.F.);
#89125=ORIENTED_EDGE('',*,*,#59892,.F.);
#89126=ORIENTED_EDGE('',*,*,#59891,.T.);
#89127=ORIENTED_EDGE('',*,*,#59893,.T.);
#89128=ORIENTED_EDGE('',*,*,#59894,.F.);
#89129=ORIENTED_EDGE('',*,*,#59895,.F.);
#89130=ORIENTED_EDGE('',*,*,#59894,.T.);
#89131=ORIENTED_EDGE('',*,*,#59896,.T.);
#89132=ORIENTED_EDGE('',*,*,#59897,.T.);
#89133=ORIENTED_EDGE('',*,*,#59898,.F.);
#89134=ORIENTED_EDGE('',*,*,#59754,.T.);
#89135=ORIENTED_EDGE('',*,*,#59899,.T.);
#89136=ORIENTED_EDGE('',*,*,#59900,.F.);
#89137=ORIENTED_EDGE('',*,*,#59901,.F.);
#89138=ORIENTED_EDGE('',*,*,#59900,.T.);
#89139=ORIENTED_EDGE('',*,*,#59902,.T.);
#89140=ORIENTED_EDGE('',*,*,#59903,.F.);
#89141=ORIENTED_EDGE('',*,*,#59904,.F.);
#89142=ORIENTED_EDGE('',*,*,#59903,.T.);
#89143=ORIENTED_EDGE('',*,*,#59905,.T.);
#89144=ORIENTED_EDGE('',*,*,#59906,.F.);
#89145=ORIENTED_EDGE('',*,*,#59907,.F.);
#89146=ORIENTED_EDGE('',*,*,#59906,.T.);
#89147=ORIENTED_EDGE('',*,*,#59908,.T.);
#89148=ORIENTED_EDGE('',*,*,#59909,.F.);
#89149=ORIENTED_EDGE('',*,*,#59910,.F.);
#89150=ORIENTED_EDGE('',*,*,#59909,.T.);
#89151=ORIENTED_EDGE('',*,*,#59911,.T.);
#89152=ORIENTED_EDGE('',*,*,#59912,.F.);
#89153=ORIENTED_EDGE('',*,*,#59913,.F.);
#89154=ORIENTED_EDGE('',*,*,#59912,.T.);
#89155=ORIENTED_EDGE('',*,*,#59914,.T.);
#89156=ORIENTED_EDGE('',*,*,#59756,.F.);
#89157=ORIENTED_EDGE('',*,*,#59915,.F.);
#89158=ORIENTED_EDGE('',*,*,#59916,.T.);
#89159=ORIENTED_EDGE('',*,*,#59917,.T.);
#89160=ORIENTED_EDGE('',*,*,#59918,.F.);
#89161=ORIENTED_EDGE('',*,*,#59919,.F.);
#89162=ORIENTED_EDGE('',*,*,#59918,.T.);
#89163=ORIENTED_EDGE('',*,*,#59920,.T.);
#89164=ORIENTED_EDGE('',*,*,#59921,.F.);
#89165=ORIENTED_EDGE('',*,*,#59922,.F.);
#89166=ORIENTED_EDGE('',*,*,#59921,.T.);
#89167=ORIENTED_EDGE('',*,*,#59923,.T.);
#89168=ORIENTED_EDGE('',*,*,#59924,.F.);
#89169=ORIENTED_EDGE('',*,*,#59925,.F.);
#89170=ORIENTED_EDGE('',*,*,#59924,.T.);
#89171=ORIENTED_EDGE('',*,*,#59926,.T.);
#89172=ORIENTED_EDGE('',*,*,#59927,.F.);
#89173=ORIENTED_EDGE('',*,*,#59928,.F.);
#89174=ORIENTED_EDGE('',*,*,#59927,.T.);
#89175=ORIENTED_EDGE('',*,*,#59929,.T.);
#89176=ORIENTED_EDGE('',*,*,#59930,.F.);
#89177=ORIENTED_EDGE('',*,*,#59931,.F.);
#89178=ORIENTED_EDGE('',*,*,#59930,.T.);
#89179=ORIENTED_EDGE('',*,*,#59932,.T.);
#89180=ORIENTED_EDGE('',*,*,#59933,.F.);
#89181=ORIENTED_EDGE('',*,*,#59934,.F.);
#89182=ORIENTED_EDGE('',*,*,#59933,.T.);
#89183=ORIENTED_EDGE('',*,*,#59935,.T.);
#89184=ORIENTED_EDGE('',*,*,#59936,.F.);
#89185=ORIENTED_EDGE('',*,*,#59937,.F.);
#89186=ORIENTED_EDGE('',*,*,#59936,.T.);
#89187=ORIENTED_EDGE('',*,*,#59938,.T.);
#89188=ORIENTED_EDGE('',*,*,#59939,.F.);
#89189=ORIENTED_EDGE('',*,*,#59940,.F.);
#89190=ORIENTED_EDGE('',*,*,#59939,.T.);
#89191=ORIENTED_EDGE('',*,*,#59941,.T.);
#89192=ORIENTED_EDGE('',*,*,#59942,.F.);
#89193=ORIENTED_EDGE('',*,*,#59943,.F.);
#89194=ORIENTED_EDGE('',*,*,#59942,.T.);
#89195=ORIENTED_EDGE('',*,*,#59944,.T.);
#89196=ORIENTED_EDGE('',*,*,#59945,.F.);
#89197=ORIENTED_EDGE('',*,*,#59946,.F.);
#89198=ORIENTED_EDGE('',*,*,#59945,.T.);
#89199=ORIENTED_EDGE('',*,*,#59947,.T.);
#89200=ORIENTED_EDGE('',*,*,#59948,.F.);
#89201=ORIENTED_EDGE('',*,*,#59949,.F.);
#89202=ORIENTED_EDGE('',*,*,#59948,.T.);
#89203=ORIENTED_EDGE('',*,*,#59950,.T.);
#89204=ORIENTED_EDGE('',*,*,#59951,.F.);
#89205=ORIENTED_EDGE('',*,*,#59952,.F.);
#89206=ORIENTED_EDGE('',*,*,#59951,.T.);
#89207=ORIENTED_EDGE('',*,*,#59953,.T.);
#89208=ORIENTED_EDGE('',*,*,#59799,.F.);
#89209=ORIENTED_EDGE('',*,*,#59954,.F.);
#89210=ORIENTED_EDGE('',*,*,#59955,.T.);
#89211=ORIENTED_EDGE('',*,*,#59956,.T.);
#89212=ORIENTED_EDGE('',*,*,#59957,.F.);
#89213=ORIENTED_EDGE('',*,*,#59958,.F.);
#89214=ORIENTED_EDGE('',*,*,#59957,.T.);
#89215=ORIENTED_EDGE('',*,*,#59959,.T.);
#89216=ORIENTED_EDGE('',*,*,#59960,.F.);
#89217=ORIENTED_EDGE('',*,*,#59961,.F.);
#89218=ORIENTED_EDGE('',*,*,#59960,.T.);
#89219=ORIENTED_EDGE('',*,*,#59962,.T.);
#89220=ORIENTED_EDGE('',*,*,#59963,.F.);
#89221=ORIENTED_EDGE('',*,*,#59964,.F.);
#89222=ORIENTED_EDGE('',*,*,#59963,.T.);
#89223=ORIENTED_EDGE('',*,*,#59965,.T.);
#89224=ORIENTED_EDGE('',*,*,#59966,.F.);
#89225=ORIENTED_EDGE('',*,*,#59967,.F.);
#89226=ORIENTED_EDGE('',*,*,#59966,.T.);
#89227=ORIENTED_EDGE('',*,*,#59968,.T.);
#89228=ORIENTED_EDGE('',*,*,#59969,.F.);
#89229=ORIENTED_EDGE('',*,*,#59970,.F.);
#89230=ORIENTED_EDGE('',*,*,#59969,.T.);
#89231=ORIENTED_EDGE('',*,*,#59971,.T.);
#89232=ORIENTED_EDGE('',*,*,#59972,.F.);
#89233=ORIENTED_EDGE('',*,*,#59973,.F.);
#89234=ORIENTED_EDGE('',*,*,#59972,.T.);
#89235=ORIENTED_EDGE('',*,*,#59974,.T.);
#89236=ORIENTED_EDGE('',*,*,#59975,.F.);
#89237=ORIENTED_EDGE('',*,*,#59976,.F.);
#89238=ORIENTED_EDGE('',*,*,#59975,.T.);
#89239=ORIENTED_EDGE('',*,*,#59977,.T.);
#89240=ORIENTED_EDGE('',*,*,#59978,.F.);
#89241=ORIENTED_EDGE('',*,*,#59979,.F.);
#89242=ORIENTED_EDGE('',*,*,#59978,.T.);
#89243=ORIENTED_EDGE('',*,*,#59980,.T.);
#89244=ORIENTED_EDGE('',*,*,#59981,.F.);
#89245=ORIENTED_EDGE('',*,*,#59982,.F.);
#89246=ORIENTED_EDGE('',*,*,#59981,.T.);
#89247=ORIENTED_EDGE('',*,*,#59983,.T.);
#89248=ORIENTED_EDGE('',*,*,#59984,.F.);
#89249=ORIENTED_EDGE('',*,*,#59985,.F.);
#89250=ORIENTED_EDGE('',*,*,#59984,.T.);
#89251=ORIENTED_EDGE('',*,*,#59986,.T.);
#89252=ORIENTED_EDGE('',*,*,#59987,.F.);
#89253=ORIENTED_EDGE('',*,*,#59988,.F.);
#89254=ORIENTED_EDGE('',*,*,#59987,.T.);
#89255=ORIENTED_EDGE('',*,*,#59989,.T.);
#89256=ORIENTED_EDGE('',*,*,#59990,.F.);
#89257=ORIENTED_EDGE('',*,*,#59991,.F.);
#89258=ORIENTED_EDGE('',*,*,#59990,.T.);
#89259=ORIENTED_EDGE('',*,*,#59992,.T.);
#89260=ORIENTED_EDGE('',*,*,#59993,.F.);
#89261=ORIENTED_EDGE('',*,*,#59994,.F.);
#89262=ORIENTED_EDGE('',*,*,#59993,.T.);
#89263=ORIENTED_EDGE('',*,*,#59995,.T.);
#89264=ORIENTED_EDGE('',*,*,#59996,.F.);
#89265=ORIENTED_EDGE('',*,*,#59997,.F.);
#89266=ORIENTED_EDGE('',*,*,#59996,.T.);
#89267=ORIENTED_EDGE('',*,*,#59998,.T.);
#89268=ORIENTED_EDGE('',*,*,#59999,.F.);
#89269=ORIENTED_EDGE('',*,*,#60000,.F.);
#89270=ORIENTED_EDGE('',*,*,#59999,.T.);
#89271=ORIENTED_EDGE('',*,*,#60001,.T.);
#89272=ORIENTED_EDGE('',*,*,#60002,.F.);
#89273=ORIENTED_EDGE('',*,*,#60003,.F.);
#89274=ORIENTED_EDGE('',*,*,#60002,.T.);
#89275=ORIENTED_EDGE('',*,*,#60004,.T.);
#89276=ORIENTED_EDGE('',*,*,#60005,.F.);
#89277=ORIENTED_EDGE('',*,*,#60006,.F.);
#89278=ORIENTED_EDGE('',*,*,#60005,.T.);
#89279=ORIENTED_EDGE('',*,*,#60007,.T.);
#89280=ORIENTED_EDGE('',*,*,#60008,.F.);
#89281=ORIENTED_EDGE('',*,*,#60009,.F.);
#89282=ORIENTED_EDGE('',*,*,#60008,.T.);
#89283=ORIENTED_EDGE('',*,*,#60010,.T.);
#89284=ORIENTED_EDGE('',*,*,#60011,.F.);
#89285=ORIENTED_EDGE('',*,*,#60012,.F.);
#89286=ORIENTED_EDGE('',*,*,#60011,.T.);
#89287=ORIENTED_EDGE('',*,*,#60013,.T.);
#89288=ORIENTED_EDGE('',*,*,#60014,.F.);
#89289=ORIENTED_EDGE('',*,*,#60015,.F.);
#89290=ORIENTED_EDGE('',*,*,#60014,.T.);
#89291=ORIENTED_EDGE('',*,*,#60016,.T.);
#89292=ORIENTED_EDGE('',*,*,#60017,.F.);
#89293=ORIENTED_EDGE('',*,*,#60018,.F.);
#89294=ORIENTED_EDGE('',*,*,#60017,.T.);
#89295=ORIENTED_EDGE('',*,*,#60019,.T.);
#89296=ORIENTED_EDGE('',*,*,#60020,.F.);
#89297=ORIENTED_EDGE('',*,*,#60021,.F.);
#89298=ORIENTED_EDGE('',*,*,#60020,.T.);
#89299=ORIENTED_EDGE('',*,*,#60022,.T.);
#89300=ORIENTED_EDGE('',*,*,#60023,.F.);
#89301=ORIENTED_EDGE('',*,*,#60024,.F.);
#89302=ORIENTED_EDGE('',*,*,#60023,.T.);
#89303=ORIENTED_EDGE('',*,*,#60025,.T.);
#89304=ORIENTED_EDGE('',*,*,#60026,.F.);
#89305=ORIENTED_EDGE('',*,*,#60027,.F.);
#89306=ORIENTED_EDGE('',*,*,#60026,.T.);
#89307=ORIENTED_EDGE('',*,*,#60028,.T.);
#89308=ORIENTED_EDGE('',*,*,#60029,.F.);
#89309=ORIENTED_EDGE('',*,*,#60030,.F.);
#89310=ORIENTED_EDGE('',*,*,#60029,.T.);
#89311=ORIENTED_EDGE('',*,*,#60031,.T.);
#89312=ORIENTED_EDGE('',*,*,#60032,.F.);
#89313=ORIENTED_EDGE('',*,*,#60033,.F.);
#89314=ORIENTED_EDGE('',*,*,#60032,.T.);
#89315=ORIENTED_EDGE('',*,*,#60034,.T.);
#89316=ORIENTED_EDGE('',*,*,#60035,.F.);
#89317=ORIENTED_EDGE('',*,*,#60036,.F.);
#89318=ORIENTED_EDGE('',*,*,#60035,.T.);
#89319=ORIENTED_EDGE('',*,*,#60037,.T.);
#89320=ORIENTED_EDGE('',*,*,#60038,.F.);
#89321=ORIENTED_EDGE('',*,*,#60039,.F.);
#89322=ORIENTED_EDGE('',*,*,#60038,.T.);
#89323=ORIENTED_EDGE('',*,*,#60040,.T.);
#89324=ORIENTED_EDGE('',*,*,#60041,.F.);
#89325=ORIENTED_EDGE('',*,*,#60042,.F.);
#89326=ORIENTED_EDGE('',*,*,#60041,.T.);
#89327=ORIENTED_EDGE('',*,*,#60043,.T.);
#89328=ORIENTED_EDGE('',*,*,#60044,.F.);
#89329=ORIENTED_EDGE('',*,*,#60045,.F.);
#89330=ORIENTED_EDGE('',*,*,#60044,.T.);
#89331=ORIENTED_EDGE('',*,*,#60046,.T.);
#89332=ORIENTED_EDGE('',*,*,#60047,.F.);
#89333=ORIENTED_EDGE('',*,*,#60048,.F.);
#89334=ORIENTED_EDGE('',*,*,#60047,.T.);
#89335=ORIENTED_EDGE('',*,*,#60049,.T.);
#89336=ORIENTED_EDGE('',*,*,#60050,.F.);
#89337=ORIENTED_EDGE('',*,*,#60051,.F.);
#89338=ORIENTED_EDGE('',*,*,#60050,.T.);
#89339=ORIENTED_EDGE('',*,*,#60052,.T.);
#89340=ORIENTED_EDGE('',*,*,#60053,.F.);
#89341=ORIENTED_EDGE('',*,*,#60054,.F.);
#89342=ORIENTED_EDGE('',*,*,#60053,.T.);
#89343=ORIENTED_EDGE('',*,*,#60055,.T.);
#89344=ORIENTED_EDGE('',*,*,#60056,.F.);
#89345=ORIENTED_EDGE('',*,*,#60057,.F.);
#89346=ORIENTED_EDGE('',*,*,#60056,.T.);
#89347=ORIENTED_EDGE('',*,*,#60058,.T.);
#89348=ORIENTED_EDGE('',*,*,#60059,.F.);
#89349=ORIENTED_EDGE('',*,*,#60060,.F.);
#89350=ORIENTED_EDGE('',*,*,#60059,.T.);
#89351=ORIENTED_EDGE('',*,*,#60061,.T.);
#89352=ORIENTED_EDGE('',*,*,#60062,.F.);
#89353=ORIENTED_EDGE('',*,*,#60063,.F.);
#89354=ORIENTED_EDGE('',*,*,#60062,.T.);
#89355=ORIENTED_EDGE('',*,*,#60064,.T.);
#89356=ORIENTED_EDGE('',*,*,#60065,.F.);
#89357=ORIENTED_EDGE('',*,*,#60066,.F.);
#89358=ORIENTED_EDGE('',*,*,#60065,.T.);
#89359=ORIENTED_EDGE('',*,*,#60067,.T.);
#89360=ORIENTED_EDGE('',*,*,#60068,.F.);
#89361=ORIENTED_EDGE('',*,*,#60069,.F.);
#89362=ORIENTED_EDGE('',*,*,#60068,.T.);
#89363=ORIENTED_EDGE('',*,*,#60070,.T.);
#89364=ORIENTED_EDGE('',*,*,#59916,.F.);
#89365=ORIENTED_EDGE('',*,*,#60071,.F.);
#89366=ORIENTED_EDGE('',*,*,#60072,.T.);
#89367=ORIENTED_EDGE('',*,*,#60073,.T.);
#89368=ORIENTED_EDGE('',*,*,#60074,.F.);
#89369=ORIENTED_EDGE('',*,*,#60075,.F.);
#89370=ORIENTED_EDGE('',*,*,#60074,.T.);
#89371=ORIENTED_EDGE('',*,*,#60076,.T.);
#89372=ORIENTED_EDGE('',*,*,#60077,.F.);
#89373=ORIENTED_EDGE('',*,*,#60078,.F.);
#89374=ORIENTED_EDGE('',*,*,#60077,.T.);
#89375=ORIENTED_EDGE('',*,*,#60079,.T.);
#89376=ORIENTED_EDGE('',*,*,#60080,.F.);
#89377=ORIENTED_EDGE('',*,*,#60081,.F.);
#89378=ORIENTED_EDGE('',*,*,#60080,.T.);
#89379=ORIENTED_EDGE('',*,*,#60082,.T.);
#89380=ORIENTED_EDGE('',*,*,#60083,.F.);
#89381=ORIENTED_EDGE('',*,*,#60084,.F.);
#89382=ORIENTED_EDGE('',*,*,#60083,.T.);
#89383=ORIENTED_EDGE('',*,*,#60085,.T.);
#89384=ORIENTED_EDGE('',*,*,#60086,.F.);
#89385=ORIENTED_EDGE('',*,*,#60087,.F.);
#89386=ORIENTED_EDGE('',*,*,#60086,.T.);
#89387=ORIENTED_EDGE('',*,*,#60088,.T.);
#89388=ORIENTED_EDGE('',*,*,#60089,.F.);
#89389=ORIENTED_EDGE('',*,*,#60090,.F.);
#89390=ORIENTED_EDGE('',*,*,#60089,.T.);
#89391=ORIENTED_EDGE('',*,*,#60091,.T.);
#89392=ORIENTED_EDGE('',*,*,#60092,.F.);
#89393=ORIENTED_EDGE('',*,*,#60093,.F.);
#89394=ORIENTED_EDGE('',*,*,#60092,.T.);
#89395=ORIENTED_EDGE('',*,*,#60094,.T.);
#89396=ORIENTED_EDGE('',*,*,#60095,.F.);
#89397=ORIENTED_EDGE('',*,*,#60096,.F.);
#89398=ORIENTED_EDGE('',*,*,#60095,.T.);
#89399=ORIENTED_EDGE('',*,*,#60097,.T.);
#89400=ORIENTED_EDGE('',*,*,#60098,.F.);
#89401=ORIENTED_EDGE('',*,*,#60099,.F.);
#89402=ORIENTED_EDGE('',*,*,#60098,.T.);
#89403=ORIENTED_EDGE('',*,*,#60100,.T.);
#89404=ORIENTED_EDGE('',*,*,#60101,.F.);
#89405=ORIENTED_EDGE('',*,*,#60102,.F.);
#89406=ORIENTED_EDGE('',*,*,#60101,.T.);
#89407=ORIENTED_EDGE('',*,*,#60103,.T.);
#89408=ORIENTED_EDGE('',*,*,#60104,.F.);
#89409=ORIENTED_EDGE('',*,*,#60105,.F.);
#89410=ORIENTED_EDGE('',*,*,#60104,.T.);
#89411=ORIENTED_EDGE('',*,*,#60106,.T.);
#89412=ORIENTED_EDGE('',*,*,#60107,.F.);
#89413=ORIENTED_EDGE('',*,*,#60108,.F.);
#89414=ORIENTED_EDGE('',*,*,#60107,.T.);
#89415=ORIENTED_EDGE('',*,*,#60109,.T.);
#89416=ORIENTED_EDGE('',*,*,#59955,.F.);
#89417=ORIENTED_EDGE('',*,*,#60110,.F.);
#89418=ORIENTED_EDGE('',*,*,#60111,.T.);
#89419=ORIENTED_EDGE('',*,*,#60112,.T.);
#89420=ORIENTED_EDGE('',*,*,#60113,.F.);
#89421=ORIENTED_EDGE('',*,*,#60114,.F.);
#89422=ORIENTED_EDGE('',*,*,#60113,.T.);
#89423=ORIENTED_EDGE('',*,*,#60115,.T.);
#89424=ORIENTED_EDGE('',*,*,#60116,.F.);
#89425=ORIENTED_EDGE('',*,*,#60117,.F.);
#89426=ORIENTED_EDGE('',*,*,#60116,.T.);
#89427=ORIENTED_EDGE('',*,*,#60118,.T.);
#89428=ORIENTED_EDGE('',*,*,#60119,.F.);
#89429=ORIENTED_EDGE('',*,*,#60120,.F.);
#89430=ORIENTED_EDGE('',*,*,#60119,.T.);
#89431=ORIENTED_EDGE('',*,*,#60121,.T.);
#89432=ORIENTED_EDGE('',*,*,#60122,.F.);
#89433=ORIENTED_EDGE('',*,*,#60123,.F.);
#89434=ORIENTED_EDGE('',*,*,#60122,.T.);
#89435=ORIENTED_EDGE('',*,*,#60124,.T.);
#89436=ORIENTED_EDGE('',*,*,#60125,.F.);
#89437=ORIENTED_EDGE('',*,*,#60126,.F.);
#89438=ORIENTED_EDGE('',*,*,#60125,.T.);
#89439=ORIENTED_EDGE('',*,*,#60127,.T.);
#89440=ORIENTED_EDGE('',*,*,#60128,.F.);
#89441=ORIENTED_EDGE('',*,*,#60129,.F.);
#89442=ORIENTED_EDGE('',*,*,#60128,.T.);
#89443=ORIENTED_EDGE('',*,*,#60130,.T.);
#89444=ORIENTED_EDGE('',*,*,#60131,.F.);
#89445=ORIENTED_EDGE('',*,*,#60132,.F.);
#89446=ORIENTED_EDGE('',*,*,#60131,.T.);
#89447=ORIENTED_EDGE('',*,*,#60133,.T.);
#89448=ORIENTED_EDGE('',*,*,#60134,.F.);
#89449=ORIENTED_EDGE('',*,*,#60135,.F.);
#89450=ORIENTED_EDGE('',*,*,#60134,.T.);
#89451=ORIENTED_EDGE('',*,*,#60136,.T.);
#89452=ORIENTED_EDGE('',*,*,#60137,.F.);
#89453=ORIENTED_EDGE('',*,*,#60138,.F.);
#89454=ORIENTED_EDGE('',*,*,#60137,.T.);
#89455=ORIENTED_EDGE('',*,*,#60139,.T.);
#89456=ORIENTED_EDGE('',*,*,#60140,.F.);
#89457=ORIENTED_EDGE('',*,*,#60141,.F.);
#89458=ORIENTED_EDGE('',*,*,#60140,.T.);
#89459=ORIENTED_EDGE('',*,*,#60142,.T.);
#89460=ORIENTED_EDGE('',*,*,#60143,.F.);
#89461=ORIENTED_EDGE('',*,*,#60144,.F.);
#89462=ORIENTED_EDGE('',*,*,#60143,.T.);
#89463=ORIENTED_EDGE('',*,*,#60145,.T.);
#89464=ORIENTED_EDGE('',*,*,#60146,.F.);
#89465=ORIENTED_EDGE('',*,*,#60147,.F.);
#89466=ORIENTED_EDGE('',*,*,#60146,.T.);
#89467=ORIENTED_EDGE('',*,*,#60148,.T.);
#89468=ORIENTED_EDGE('',*,*,#60149,.F.);
#89469=ORIENTED_EDGE('',*,*,#60150,.F.);
#89470=ORIENTED_EDGE('',*,*,#60149,.T.);
#89471=ORIENTED_EDGE('',*,*,#60151,.T.);
#89472=ORIENTED_EDGE('',*,*,#60152,.F.);
#89473=ORIENTED_EDGE('',*,*,#60153,.F.);
#89474=ORIENTED_EDGE('',*,*,#60152,.T.);
#89475=ORIENTED_EDGE('',*,*,#60154,.T.);
#89476=ORIENTED_EDGE('',*,*,#60155,.F.);
#89477=ORIENTED_EDGE('',*,*,#60156,.F.);
#89478=ORIENTED_EDGE('',*,*,#60155,.T.);
#89479=ORIENTED_EDGE('',*,*,#60157,.T.);
#89480=ORIENTED_EDGE('',*,*,#60158,.F.);
#89481=ORIENTED_EDGE('',*,*,#60159,.F.);
#89482=ORIENTED_EDGE('',*,*,#60158,.T.);
#89483=ORIENTED_EDGE('',*,*,#60160,.T.);
#89484=ORIENTED_EDGE('',*,*,#60161,.F.);
#89485=ORIENTED_EDGE('',*,*,#60162,.F.);
#89486=ORIENTED_EDGE('',*,*,#60161,.T.);
#89487=ORIENTED_EDGE('',*,*,#60163,.T.);
#89488=ORIENTED_EDGE('',*,*,#60164,.F.);
#89489=ORIENTED_EDGE('',*,*,#60165,.F.);
#89490=ORIENTED_EDGE('',*,*,#60164,.T.);
#89491=ORIENTED_EDGE('',*,*,#60166,.T.);
#89492=ORIENTED_EDGE('',*,*,#60167,.F.);
#89493=ORIENTED_EDGE('',*,*,#60168,.F.);
#89494=ORIENTED_EDGE('',*,*,#60167,.T.);
#89495=ORIENTED_EDGE('',*,*,#60169,.T.);
#89496=ORIENTED_EDGE('',*,*,#60170,.F.);
#89497=ORIENTED_EDGE('',*,*,#60171,.F.);
#89498=ORIENTED_EDGE('',*,*,#60170,.T.);
#89499=ORIENTED_EDGE('',*,*,#60172,.T.);
#89500=ORIENTED_EDGE('',*,*,#60173,.F.);
#89501=ORIENTED_EDGE('',*,*,#60174,.F.);
#89502=ORIENTED_EDGE('',*,*,#60173,.T.);
#89503=ORIENTED_EDGE('',*,*,#60175,.T.);
#89504=ORIENTED_EDGE('',*,*,#60176,.F.);
#89505=ORIENTED_EDGE('',*,*,#60177,.F.);
#89506=ORIENTED_EDGE('',*,*,#60176,.T.);
#89507=ORIENTED_EDGE('',*,*,#60178,.T.);
#89508=ORIENTED_EDGE('',*,*,#60179,.F.);
#89509=ORIENTED_EDGE('',*,*,#60180,.F.);
#89510=ORIENTED_EDGE('',*,*,#60179,.T.);
#89511=ORIENTED_EDGE('',*,*,#60181,.T.);
#89512=ORIENTED_EDGE('',*,*,#60182,.F.);
#89513=ORIENTED_EDGE('',*,*,#60183,.F.);
#89514=ORIENTED_EDGE('',*,*,#60182,.T.);
#89515=ORIENTED_EDGE('',*,*,#60184,.T.);
#89516=ORIENTED_EDGE('',*,*,#60185,.F.);
#89517=ORIENTED_EDGE('',*,*,#60186,.F.);
#89518=ORIENTED_EDGE('',*,*,#60185,.T.);
#89519=ORIENTED_EDGE('',*,*,#60187,.T.);
#89520=ORIENTED_EDGE('',*,*,#60188,.F.);
#89521=ORIENTED_EDGE('',*,*,#60189,.F.);
#89522=ORIENTED_EDGE('',*,*,#60188,.T.);
#89523=ORIENTED_EDGE('',*,*,#60190,.T.);
#89524=ORIENTED_EDGE('',*,*,#60191,.F.);
#89525=ORIENTED_EDGE('',*,*,#60192,.F.);
#89526=ORIENTED_EDGE('',*,*,#60191,.T.);
#89527=ORIENTED_EDGE('',*,*,#60193,.T.);
#89528=ORIENTED_EDGE('',*,*,#60194,.F.);
#89529=ORIENTED_EDGE('',*,*,#60195,.F.);
#89530=ORIENTED_EDGE('',*,*,#60194,.T.);
#89531=ORIENTED_EDGE('',*,*,#60196,.T.);
#89532=ORIENTED_EDGE('',*,*,#60197,.F.);
#89533=ORIENTED_EDGE('',*,*,#60198,.F.);
#89534=ORIENTED_EDGE('',*,*,#60197,.T.);
#89535=ORIENTED_EDGE('',*,*,#60199,.T.);
#89536=ORIENTED_EDGE('',*,*,#60200,.F.);
#89537=ORIENTED_EDGE('',*,*,#60201,.F.);
#89538=ORIENTED_EDGE('',*,*,#60200,.T.);
#89539=ORIENTED_EDGE('',*,*,#60202,.T.);
#89540=ORIENTED_EDGE('',*,*,#60203,.F.);
#89541=ORIENTED_EDGE('',*,*,#60204,.F.);
#89542=ORIENTED_EDGE('',*,*,#60203,.T.);
#89543=ORIENTED_EDGE('',*,*,#60205,.T.);
#89544=ORIENTED_EDGE('',*,*,#60206,.F.);
#89545=ORIENTED_EDGE('',*,*,#60207,.F.);
#89546=ORIENTED_EDGE('',*,*,#60206,.T.);
#89547=ORIENTED_EDGE('',*,*,#60208,.T.);
#89548=ORIENTED_EDGE('',*,*,#60209,.F.);
#89549=ORIENTED_EDGE('',*,*,#60210,.F.);
#89550=ORIENTED_EDGE('',*,*,#60209,.T.);
#89551=ORIENTED_EDGE('',*,*,#60211,.T.);
#89552=ORIENTED_EDGE('',*,*,#60212,.F.);
#89553=ORIENTED_EDGE('',*,*,#60213,.F.);
#89554=ORIENTED_EDGE('',*,*,#60212,.T.);
#89555=ORIENTED_EDGE('',*,*,#60214,.T.);
#89556=ORIENTED_EDGE('',*,*,#60215,.F.);
#89557=ORIENTED_EDGE('',*,*,#60216,.F.);
#89558=ORIENTED_EDGE('',*,*,#60215,.T.);
#89559=ORIENTED_EDGE('',*,*,#60217,.T.);
#89560=ORIENTED_EDGE('',*,*,#60218,.F.);
#89561=ORIENTED_EDGE('',*,*,#60219,.F.);
#89562=ORIENTED_EDGE('',*,*,#60218,.T.);
#89563=ORIENTED_EDGE('',*,*,#60220,.T.);
#89564=ORIENTED_EDGE('',*,*,#60221,.F.);
#89565=ORIENTED_EDGE('',*,*,#60222,.F.);
#89566=ORIENTED_EDGE('',*,*,#60221,.T.);
#89567=ORIENTED_EDGE('',*,*,#60223,.T.);
#89568=ORIENTED_EDGE('',*,*,#60224,.F.);
#89569=ORIENTED_EDGE('',*,*,#60225,.F.);
#89570=ORIENTED_EDGE('',*,*,#60224,.T.);
#89571=ORIENTED_EDGE('',*,*,#60226,.T.);
#89572=ORIENTED_EDGE('',*,*,#60072,.F.);
#89573=ORIENTED_EDGE('',*,*,#60227,.F.);
#89574=ORIENTED_EDGE('',*,*,#60228,.T.);
#89575=ORIENTED_EDGE('',*,*,#60229,.T.);
#89576=ORIENTED_EDGE('',*,*,#60230,.F.);
#89577=ORIENTED_EDGE('',*,*,#60231,.F.);
#89578=ORIENTED_EDGE('',*,*,#60230,.T.);
#89579=ORIENTED_EDGE('',*,*,#60232,.T.);
#89580=ORIENTED_EDGE('',*,*,#60233,.F.);
#89581=ORIENTED_EDGE('',*,*,#60234,.F.);
#89582=ORIENTED_EDGE('',*,*,#60233,.T.);
#89583=ORIENTED_EDGE('',*,*,#60235,.T.);
#89584=ORIENTED_EDGE('',*,*,#60236,.F.);
#89585=ORIENTED_EDGE('',*,*,#60237,.F.);
#89586=ORIENTED_EDGE('',*,*,#60236,.T.);
#89587=ORIENTED_EDGE('',*,*,#60238,.T.);
#89588=ORIENTED_EDGE('',*,*,#60239,.F.);
#89589=ORIENTED_EDGE('',*,*,#60240,.F.);
#89590=ORIENTED_EDGE('',*,*,#60239,.T.);
#89591=ORIENTED_EDGE('',*,*,#60241,.T.);
#89592=ORIENTED_EDGE('',*,*,#60242,.F.);
#89593=ORIENTED_EDGE('',*,*,#60243,.F.);
#89594=ORIENTED_EDGE('',*,*,#60242,.T.);
#89595=ORIENTED_EDGE('',*,*,#60244,.T.);
#89596=ORIENTED_EDGE('',*,*,#60245,.F.);
#89597=ORIENTED_EDGE('',*,*,#60246,.F.);
#89598=ORIENTED_EDGE('',*,*,#60245,.T.);
#89599=ORIENTED_EDGE('',*,*,#60247,.T.);
#89600=ORIENTED_EDGE('',*,*,#60248,.F.);
#89601=ORIENTED_EDGE('',*,*,#60249,.F.);
#89602=ORIENTED_EDGE('',*,*,#60248,.T.);
#89603=ORIENTED_EDGE('',*,*,#60250,.T.);
#89604=ORIENTED_EDGE('',*,*,#60251,.F.);
#89605=ORIENTED_EDGE('',*,*,#60252,.F.);
#89606=ORIENTED_EDGE('',*,*,#60251,.T.);
#89607=ORIENTED_EDGE('',*,*,#60253,.T.);
#89608=ORIENTED_EDGE('',*,*,#60254,.F.);
#89609=ORIENTED_EDGE('',*,*,#60255,.F.);
#89610=ORIENTED_EDGE('',*,*,#60254,.T.);
#89611=ORIENTED_EDGE('',*,*,#60256,.T.);
#89612=ORIENTED_EDGE('',*,*,#60257,.F.);
#89613=ORIENTED_EDGE('',*,*,#60258,.F.);
#89614=ORIENTED_EDGE('',*,*,#60257,.T.);
#89615=ORIENTED_EDGE('',*,*,#60259,.T.);
#89616=ORIENTED_EDGE('',*,*,#60260,.F.);
#89617=ORIENTED_EDGE('',*,*,#60261,.F.);
#89618=ORIENTED_EDGE('',*,*,#60260,.T.);
#89619=ORIENTED_EDGE('',*,*,#60262,.T.);
#89620=ORIENTED_EDGE('',*,*,#60263,.F.);
#89621=ORIENTED_EDGE('',*,*,#60264,.F.);
#89622=ORIENTED_EDGE('',*,*,#60263,.T.);
#89623=ORIENTED_EDGE('',*,*,#60265,.T.);
#89624=ORIENTED_EDGE('',*,*,#60111,.F.);
#89625=ORIENTED_EDGE('',*,*,#60266,.F.);
#89626=ORIENTED_EDGE('',*,*,#59797,.T.);
#89627=ORIENTED_EDGE('',*,*,#60267,.T.);
#89628=ORIENTED_EDGE('',*,*,#60268,.F.);
#89629=ORIENTED_EDGE('',*,*,#60269,.F.);
#89630=ORIENTED_EDGE('',*,*,#60268,.T.);
#89631=ORIENTED_EDGE('',*,*,#60270,.T.);
#89632=ORIENTED_EDGE('',*,*,#60271,.F.);
#89633=ORIENTED_EDGE('',*,*,#60272,.F.);
#89634=ORIENTED_EDGE('',*,*,#60271,.T.);
#89635=ORIENTED_EDGE('',*,*,#60273,.T.);
#89636=ORIENTED_EDGE('',*,*,#60274,.F.);
#89637=ORIENTED_EDGE('',*,*,#60275,.F.);
#89638=ORIENTED_EDGE('',*,*,#60274,.T.);
#89639=ORIENTED_EDGE('',*,*,#60276,.T.);
#89640=ORIENTED_EDGE('',*,*,#60277,.F.);
#89641=ORIENTED_EDGE('',*,*,#60278,.F.);
#89642=ORIENTED_EDGE('',*,*,#60277,.T.);
#89643=ORIENTED_EDGE('',*,*,#60279,.T.);
#89644=ORIENTED_EDGE('',*,*,#60280,.F.);
#89645=ORIENTED_EDGE('',*,*,#60281,.F.);
#89646=ORIENTED_EDGE('',*,*,#60280,.T.);
#89647=ORIENTED_EDGE('',*,*,#60282,.T.);
#89648=ORIENTED_EDGE('',*,*,#60283,.F.);
#89649=ORIENTED_EDGE('',*,*,#60284,.F.);
#89650=ORIENTED_EDGE('',*,*,#60283,.T.);
#89651=ORIENTED_EDGE('',*,*,#60285,.T.);
#89652=ORIENTED_EDGE('',*,*,#60286,.F.);
#89653=ORIENTED_EDGE('',*,*,#60287,.F.);
#89654=ORIENTED_EDGE('',*,*,#60286,.T.);
#89655=ORIENTED_EDGE('',*,*,#60288,.T.);
#89656=ORIENTED_EDGE('',*,*,#60289,.F.);
#89657=ORIENTED_EDGE('',*,*,#60290,.F.);
#89658=ORIENTED_EDGE('',*,*,#60289,.T.);
#89659=ORIENTED_EDGE('',*,*,#60291,.T.);
#89660=ORIENTED_EDGE('',*,*,#60292,.F.);
#89661=ORIENTED_EDGE('',*,*,#60293,.F.);
#89662=ORIENTED_EDGE('',*,*,#60292,.T.);
#89663=ORIENTED_EDGE('',*,*,#60294,.T.);
#89664=ORIENTED_EDGE('',*,*,#60295,.F.);
#89665=ORIENTED_EDGE('',*,*,#60296,.F.);
#89666=ORIENTED_EDGE('',*,*,#60295,.T.);
#89667=ORIENTED_EDGE('',*,*,#60297,.T.);
#89668=ORIENTED_EDGE('',*,*,#60298,.F.);
#89669=ORIENTED_EDGE('',*,*,#60299,.F.);
#89670=ORIENTED_EDGE('',*,*,#60298,.T.);
#89671=ORIENTED_EDGE('',*,*,#60300,.T.);
#89672=ORIENTED_EDGE('',*,*,#60301,.F.);
#89673=ORIENTED_EDGE('',*,*,#60302,.F.);
#89674=ORIENTED_EDGE('',*,*,#60301,.T.);
#89675=ORIENTED_EDGE('',*,*,#60303,.T.);
#89676=ORIENTED_EDGE('',*,*,#60304,.F.);
#89677=ORIENTED_EDGE('',*,*,#60305,.F.);
#89678=ORIENTED_EDGE('',*,*,#60304,.T.);
#89679=ORIENTED_EDGE('',*,*,#60306,.T.);
#89680=ORIENTED_EDGE('',*,*,#60307,.F.);
#89681=ORIENTED_EDGE('',*,*,#60308,.F.);
#89682=ORIENTED_EDGE('',*,*,#60307,.T.);
#89683=ORIENTED_EDGE('',*,*,#60309,.T.);
#89684=ORIENTED_EDGE('',*,*,#60310,.F.);
#89685=ORIENTED_EDGE('',*,*,#60311,.F.);
#89686=ORIENTED_EDGE('',*,*,#60310,.T.);
#89687=ORIENTED_EDGE('',*,*,#60312,.T.);
#89688=ORIENTED_EDGE('',*,*,#60313,.F.);
#89689=ORIENTED_EDGE('',*,*,#60314,.F.);
#89690=ORIENTED_EDGE('',*,*,#60313,.T.);
#89691=ORIENTED_EDGE('',*,*,#60315,.T.);
#89692=ORIENTED_EDGE('',*,*,#60316,.F.);
#89693=ORIENTED_EDGE('',*,*,#60317,.F.);
#89694=ORIENTED_EDGE('',*,*,#60316,.T.);
#89695=ORIENTED_EDGE('',*,*,#60318,.T.);
#89696=ORIENTED_EDGE('',*,*,#60319,.F.);
#89697=ORIENTED_EDGE('',*,*,#60320,.F.);
#89698=ORIENTED_EDGE('',*,*,#60319,.T.);
#89699=ORIENTED_EDGE('',*,*,#60321,.T.);
#89700=ORIENTED_EDGE('',*,*,#60322,.F.);
#89701=ORIENTED_EDGE('',*,*,#60323,.F.);
#89702=ORIENTED_EDGE('',*,*,#60322,.T.);
#89703=ORIENTED_EDGE('',*,*,#60324,.T.);
#89704=ORIENTED_EDGE('',*,*,#60325,.F.);
#89705=ORIENTED_EDGE('',*,*,#60326,.F.);
#89706=ORIENTED_EDGE('',*,*,#60325,.T.);
#89707=ORIENTED_EDGE('',*,*,#60327,.T.);
#89708=ORIENTED_EDGE('',*,*,#60328,.F.);
#89709=ORIENTED_EDGE('',*,*,#60329,.F.);
#89710=ORIENTED_EDGE('',*,*,#60328,.T.);
#89711=ORIENTED_EDGE('',*,*,#60330,.T.);
#89712=ORIENTED_EDGE('',*,*,#60331,.F.);
#89713=ORIENTED_EDGE('',*,*,#60332,.F.);
#89714=ORIENTED_EDGE('',*,*,#60331,.T.);
#89715=ORIENTED_EDGE('',*,*,#60333,.T.);
#89716=ORIENTED_EDGE('',*,*,#60334,.F.);
#89717=ORIENTED_EDGE('',*,*,#60335,.F.);
#89718=ORIENTED_EDGE('',*,*,#60334,.T.);
#89719=ORIENTED_EDGE('',*,*,#60336,.T.);
#89720=ORIENTED_EDGE('',*,*,#60337,.F.);
#89721=ORIENTED_EDGE('',*,*,#60338,.F.);
#89722=ORIENTED_EDGE('',*,*,#60337,.T.);
#89723=ORIENTED_EDGE('',*,*,#60339,.T.);
#89724=ORIENTED_EDGE('',*,*,#60340,.F.);
#89725=ORIENTED_EDGE('',*,*,#60341,.F.);
#89726=ORIENTED_EDGE('',*,*,#60340,.T.);
#89727=ORIENTED_EDGE('',*,*,#60342,.T.);
#89728=ORIENTED_EDGE('',*,*,#60343,.F.);
#89729=ORIENTED_EDGE('',*,*,#60344,.F.);
#89730=ORIENTED_EDGE('',*,*,#60343,.T.);
#89731=ORIENTED_EDGE('',*,*,#60345,.T.);
#89732=ORIENTED_EDGE('',*,*,#60346,.F.);
#89733=ORIENTED_EDGE('',*,*,#60347,.F.);
#89734=ORIENTED_EDGE('',*,*,#60346,.T.);
#89735=ORIENTED_EDGE('',*,*,#60348,.T.);
#89736=ORIENTED_EDGE('',*,*,#60349,.F.);
#89737=ORIENTED_EDGE('',*,*,#60350,.F.);
#89738=ORIENTED_EDGE('',*,*,#60349,.T.);
#89739=ORIENTED_EDGE('',*,*,#60351,.T.);
#89740=ORIENTED_EDGE('',*,*,#60352,.F.);
#89741=ORIENTED_EDGE('',*,*,#60353,.F.);
#89742=ORIENTED_EDGE('',*,*,#60352,.T.);
#89743=ORIENTED_EDGE('',*,*,#60354,.T.);
#89744=ORIENTED_EDGE('',*,*,#60355,.F.);
#89745=ORIENTED_EDGE('',*,*,#60356,.F.);
#89746=ORIENTED_EDGE('',*,*,#60355,.T.);
#89747=ORIENTED_EDGE('',*,*,#60357,.T.);
#89748=ORIENTED_EDGE('',*,*,#60358,.F.);
#89749=ORIENTED_EDGE('',*,*,#60359,.F.);
#89750=ORIENTED_EDGE('',*,*,#60358,.T.);
#89751=ORIENTED_EDGE('',*,*,#60360,.T.);
#89752=ORIENTED_EDGE('',*,*,#60361,.F.);
#89753=ORIENTED_EDGE('',*,*,#60362,.F.);
#89754=ORIENTED_EDGE('',*,*,#60361,.T.);
#89755=ORIENTED_EDGE('',*,*,#60363,.T.);
#89756=ORIENTED_EDGE('',*,*,#60364,.F.);
#89757=ORIENTED_EDGE('',*,*,#60365,.F.);
#89758=ORIENTED_EDGE('',*,*,#60364,.T.);
#89759=ORIENTED_EDGE('',*,*,#60366,.T.);
#89760=ORIENTED_EDGE('',*,*,#60367,.F.);
#89761=ORIENTED_EDGE('',*,*,#60368,.F.);
#89762=ORIENTED_EDGE('',*,*,#60367,.T.);
#89763=ORIENTED_EDGE('',*,*,#60369,.T.);
#89764=ORIENTED_EDGE('',*,*,#60370,.F.);
#89765=ORIENTED_EDGE('',*,*,#60371,.F.);
#89766=ORIENTED_EDGE('',*,*,#60370,.T.);
#89767=ORIENTED_EDGE('',*,*,#60372,.T.);
#89768=ORIENTED_EDGE('',*,*,#60373,.F.);
#89769=ORIENTED_EDGE('',*,*,#60374,.F.);
#89770=ORIENTED_EDGE('',*,*,#60373,.T.);
#89771=ORIENTED_EDGE('',*,*,#60375,.T.);
#89772=ORIENTED_EDGE('',*,*,#60376,.F.);
#89773=ORIENTED_EDGE('',*,*,#60377,.F.);
#89774=ORIENTED_EDGE('',*,*,#60376,.T.);
#89775=ORIENTED_EDGE('',*,*,#60378,.T.);
#89776=ORIENTED_EDGE('',*,*,#60228,.F.);
#89777=ORIENTED_EDGE('',*,*,#60379,.F.);
#89778=ORIENTED_EDGE('',*,*,#60380,.F.);
#89779=ORIENTED_EDGE('',*,*,#60381,.T.);
#89780=ORIENTED_EDGE('',*,*,#59752,.F.);
#89781=ORIENTED_EDGE('',*,*,#60382,.F.);
#89782=ORIENTED_EDGE('',*,*,#59897,.F.);
#89783=ORIENTED_EDGE('',*,*,#60383,.T.);
#89784=ORIENTED_EDGE('',*,*,#60380,.T.);
#89785=ORIENTED_EDGE('',*,*,#60384,.F.);
#89786=ORIENTED_EDGE('',*,*,#59750,.F.);
#89787=ORIENTED_EDGE('',*,*,#60385,.T.);
#89788=ORIENTED_EDGE('',*,*,#60386,.T.);
#89789=ORIENTED_EDGE('',*,*,#60387,.F.);
#89790=ORIENTED_EDGE('',*,*,#60386,.F.);
#89791=ORIENTED_EDGE('',*,*,#60388,.T.);
#89792=ORIENTED_EDGE('',*,*,#59859,.F.);
#89793=ORIENTED_EDGE('',*,*,#60389,.F.);
#89794=ORIENTED_EDGE('',*,*,#60390,.F.);
#89795=ORIENTED_EDGE('',*,*,#60391,.F.);
#89796=ORIENTED_EDGE('',*,*,#60392,.T.);
#89797=ORIENTED_EDGE('',*,*,#60393,.F.);
#89798=ORIENTED_EDGE('',*,*,#60394,.T.);
#89799=ORIENTED_EDGE('',*,*,#60395,.T.);
#89800=ORIENTED_EDGE('',*,*,#60396,.F.);
#89801=ORIENTED_EDGE('',*,*,#60397,.F.);
#89802=ORIENTED_EDGE('',*,*,#60398,.F.);
#89803=ORIENTED_EDGE('',*,*,#60396,.T.);
#89804=ORIENTED_EDGE('',*,*,#60399,.T.);
#89805=ORIENTED_EDGE('',*,*,#60400,.T.);
#89806=ORIENTED_EDGE('',*,*,#60399,.F.);
#89807=ORIENTED_EDGE('',*,*,#60395,.F.);
#89808=ORIENTED_EDGE('',*,*,#60401,.T.);
#89809=ORIENTED_EDGE('',*,*,#60402,.T.);
#89810=ORIENTED_EDGE('',*,*,#60401,.F.);
#89811=ORIENTED_EDGE('',*,*,#60394,.F.);
#89812=ORIENTED_EDGE('',*,*,#60403,.T.);
#89813=ORIENTED_EDGE('',*,*,#60404,.F.);
#89814=ORIENTED_EDGE('',*,*,#60403,.F.);
#89815=ORIENTED_EDGE('',*,*,#60393,.T.);
#89816=ORIENTED_EDGE('',*,*,#60405,.T.);
#89817=ORIENTED_EDGE('',*,*,#60406,.T.);
#89818=ORIENTED_EDGE('',*,*,#60405,.F.);
#89819=ORIENTED_EDGE('',*,*,#60392,.F.);
#89820=ORIENTED_EDGE('',*,*,#60407,.T.);
#89821=ORIENTED_EDGE('',*,*,#60408,.F.);
#89822=ORIENTED_EDGE('',*,*,#60407,.F.);
#89823=ORIENTED_EDGE('',*,*,#60391,.T.);
#89824=ORIENTED_EDGE('',*,*,#60409,.T.);
#89825=ORIENTED_EDGE('',*,*,#60410,.F.);
#89826=ORIENTED_EDGE('',*,*,#60409,.F.);
#89827=ORIENTED_EDGE('',*,*,#60390,.T.);
#89828=ORIENTED_EDGE('',*,*,#60411,.T.);
#89829=ORIENTED_EDGE('',*,*,#60412,.F.);
#89830=ORIENTED_EDGE('',*,*,#60411,.F.);
#89831=ORIENTED_EDGE('',*,*,#60389,.T.);
#89832=ORIENTED_EDGE('',*,*,#60398,.T.);
#89833=ORIENTED_EDGE('',*,*,#60412,.T.);
#89834=ORIENTED_EDGE('',*,*,#60397,.T.);
#89835=ORIENTED_EDGE('',*,*,#60400,.F.);
#89836=ORIENTED_EDGE('',*,*,#60402,.F.);
#89837=ORIENTED_EDGE('',*,*,#60404,.T.);
#89838=ORIENTED_EDGE('',*,*,#60406,.F.);
#89839=ORIENTED_EDGE('',*,*,#60408,.T.);
#89840=ORIENTED_EDGE('',*,*,#60410,.T.);
#89841=ORIENTED_EDGE('',*,*,#59893,.F.);
#89842=ORIENTED_EDGE('',*,*,#59890,.F.);
#89843=ORIENTED_EDGE('',*,*,#59887,.F.);
#89844=ORIENTED_EDGE('',*,*,#59884,.F.);
#89845=ORIENTED_EDGE('',*,*,#59881,.F.);
#89846=ORIENTED_EDGE('',*,*,#59878,.F.);
#89847=ORIENTED_EDGE('',*,*,#59875,.F.);
#89848=ORIENTED_EDGE('',*,*,#59872,.F.);
#89849=ORIENTED_EDGE('',*,*,#59869,.F.);
#89850=ORIENTED_EDGE('',*,*,#59866,.F.);
#89851=ORIENTED_EDGE('',*,*,#59863,.F.);
#89852=ORIENTED_EDGE('',*,*,#59860,.F.);
#89853=ORIENTED_EDGE('',*,*,#60388,.F.);
#89854=ORIENTED_EDGE('',*,*,#60385,.F.);
#89855=ORIENTED_EDGE('',*,*,#59749,.F.);
#89856=ORIENTED_EDGE('',*,*,#59857,.F.);
#89857=ORIENTED_EDGE('',*,*,#59854,.F.);
#89858=ORIENTED_EDGE('',*,*,#59851,.F.);
#89859=ORIENTED_EDGE('',*,*,#59848,.F.);
#89860=ORIENTED_EDGE('',*,*,#59845,.F.);
#89861=ORIENTED_EDGE('',*,*,#59842,.F.);
#89862=ORIENTED_EDGE('',*,*,#59839,.F.);
#89863=ORIENTED_EDGE('',*,*,#59836,.F.);
#89864=ORIENTED_EDGE('',*,*,#59833,.F.);
#89865=ORIENTED_EDGE('',*,*,#59830,.F.);
#89866=ORIENTED_EDGE('',*,*,#59827,.F.);
#89867=ORIENTED_EDGE('',*,*,#59824,.F.);
#89868=ORIENTED_EDGE('',*,*,#59821,.F.);
#89869=ORIENTED_EDGE('',*,*,#59818,.F.);
#89870=ORIENTED_EDGE('',*,*,#59815,.F.);
#89871=ORIENTED_EDGE('',*,*,#59812,.F.);
#89872=ORIENTED_EDGE('',*,*,#59809,.F.);
#89873=ORIENTED_EDGE('',*,*,#59806,.F.);
#89874=ORIENTED_EDGE('',*,*,#59803,.F.);
#89875=ORIENTED_EDGE('',*,*,#59800,.F.);
#89876=ORIENTED_EDGE('',*,*,#59953,.F.);
#89877=ORIENTED_EDGE('',*,*,#59950,.F.);
#89878=ORIENTED_EDGE('',*,*,#59947,.F.);
#89879=ORIENTED_EDGE('',*,*,#59944,.F.);
#89880=ORIENTED_EDGE('',*,*,#59941,.F.);
#89881=ORIENTED_EDGE('',*,*,#59938,.F.);
#89882=ORIENTED_EDGE('',*,*,#59935,.F.);
#89883=ORIENTED_EDGE('',*,*,#59932,.F.);
#89884=ORIENTED_EDGE('',*,*,#59929,.F.);
#89885=ORIENTED_EDGE('',*,*,#59926,.F.);
#89886=ORIENTED_EDGE('',*,*,#59923,.F.);
#89887=ORIENTED_EDGE('',*,*,#59920,.F.);
#89888=ORIENTED_EDGE('',*,*,#59917,.F.);
#89889=ORIENTED_EDGE('',*,*,#60070,.F.);
#89890=ORIENTED_EDGE('',*,*,#60067,.F.);
#89891=ORIENTED_EDGE('',*,*,#60064,.F.);
#89892=ORIENTED_EDGE('',*,*,#60061,.F.);
#89893=ORIENTED_EDGE('',*,*,#60058,.F.);
#89894=ORIENTED_EDGE('',*,*,#60055,.F.);
#89895=ORIENTED_EDGE('',*,*,#60052,.F.);
#89896=ORIENTED_EDGE('',*,*,#60049,.F.);
#89897=ORIENTED_EDGE('',*,*,#60046,.F.);
#89898=ORIENTED_EDGE('',*,*,#60043,.F.);
#89899=ORIENTED_EDGE('',*,*,#60040,.F.);
#89900=ORIENTED_EDGE('',*,*,#60037,.F.);
#89901=ORIENTED_EDGE('',*,*,#60034,.F.);
#89902=ORIENTED_EDGE('',*,*,#60031,.F.);
#89903=ORIENTED_EDGE('',*,*,#60028,.F.);
#89904=ORIENTED_EDGE('',*,*,#60025,.F.);
#89905=ORIENTED_EDGE('',*,*,#60022,.F.);
#89906=ORIENTED_EDGE('',*,*,#60019,.F.);
#89907=ORIENTED_EDGE('',*,*,#60016,.F.);
#89908=ORIENTED_EDGE('',*,*,#60013,.F.);
#89909=ORIENTED_EDGE('',*,*,#60010,.F.);
#89910=ORIENTED_EDGE('',*,*,#60007,.F.);
#89911=ORIENTED_EDGE('',*,*,#60004,.F.);
#89912=ORIENTED_EDGE('',*,*,#60001,.F.);
#89913=ORIENTED_EDGE('',*,*,#59998,.F.);
#89914=ORIENTED_EDGE('',*,*,#59995,.F.);
#89915=ORIENTED_EDGE('',*,*,#59992,.F.);
#89916=ORIENTED_EDGE('',*,*,#59989,.F.);
#89917=ORIENTED_EDGE('',*,*,#59986,.F.);
#89918=ORIENTED_EDGE('',*,*,#59983,.F.);
#89919=ORIENTED_EDGE('',*,*,#59980,.F.);
#89920=ORIENTED_EDGE('',*,*,#59977,.F.);
#89921=ORIENTED_EDGE('',*,*,#59974,.F.);
#89922=ORIENTED_EDGE('',*,*,#59971,.F.);
#89923=ORIENTED_EDGE('',*,*,#59968,.F.);
#89924=ORIENTED_EDGE('',*,*,#59965,.F.);
#89925=ORIENTED_EDGE('',*,*,#59962,.F.);
#89926=ORIENTED_EDGE('',*,*,#59959,.F.);
#89927=ORIENTED_EDGE('',*,*,#59956,.F.);
#89928=ORIENTED_EDGE('',*,*,#60109,.F.);
#89929=ORIENTED_EDGE('',*,*,#60106,.F.);
#89930=ORIENTED_EDGE('',*,*,#60103,.F.);
#89931=ORIENTED_EDGE('',*,*,#60100,.F.);
#89932=ORIENTED_EDGE('',*,*,#60097,.F.);
#89933=ORIENTED_EDGE('',*,*,#60094,.F.);
#89934=ORIENTED_EDGE('',*,*,#60091,.F.);
#89935=ORIENTED_EDGE('',*,*,#60088,.F.);
#89936=ORIENTED_EDGE('',*,*,#60085,.F.);
#89937=ORIENTED_EDGE('',*,*,#60082,.F.);
#89938=ORIENTED_EDGE('',*,*,#60079,.F.);
#89939=ORIENTED_EDGE('',*,*,#60076,.F.);
#89940=ORIENTED_EDGE('',*,*,#60073,.F.);
#89941=ORIENTED_EDGE('',*,*,#60226,.F.);
#89942=ORIENTED_EDGE('',*,*,#60223,.F.);
#89943=ORIENTED_EDGE('',*,*,#60220,.F.);
#89944=ORIENTED_EDGE('',*,*,#60217,.F.);
#89945=ORIENTED_EDGE('',*,*,#60214,.F.);
#89946=ORIENTED_EDGE('',*,*,#60211,.F.);
#89947=ORIENTED_EDGE('',*,*,#60208,.F.);
#89948=ORIENTED_EDGE('',*,*,#60205,.F.);
#89949=ORIENTED_EDGE('',*,*,#60202,.F.);
#89950=ORIENTED_EDGE('',*,*,#60199,.F.);
#89951=ORIENTED_EDGE('',*,*,#60196,.F.);
#89952=ORIENTED_EDGE('',*,*,#60193,.F.);
#89953=ORIENTED_EDGE('',*,*,#60190,.F.);
#89954=ORIENTED_EDGE('',*,*,#60187,.F.);
#89955=ORIENTED_EDGE('',*,*,#60184,.F.);
#89956=ORIENTED_EDGE('',*,*,#60181,.F.);
#89957=ORIENTED_EDGE('',*,*,#60178,.F.);
#89958=ORIENTED_EDGE('',*,*,#60175,.F.);
#89959=ORIENTED_EDGE('',*,*,#60172,.F.);
#89960=ORIENTED_EDGE('',*,*,#60169,.F.);
#89961=ORIENTED_EDGE('',*,*,#60166,.F.);
#89962=ORIENTED_EDGE('',*,*,#60163,.F.);
#89963=ORIENTED_EDGE('',*,*,#60160,.F.);
#89964=ORIENTED_EDGE('',*,*,#60157,.F.);
#89965=ORIENTED_EDGE('',*,*,#60154,.F.);
#89966=ORIENTED_EDGE('',*,*,#60151,.F.);
#89967=ORIENTED_EDGE('',*,*,#60148,.F.);
#89968=ORIENTED_EDGE('',*,*,#60145,.F.);
#89969=ORIENTED_EDGE('',*,*,#60142,.F.);
#89970=ORIENTED_EDGE('',*,*,#60139,.F.);
#89971=ORIENTED_EDGE('',*,*,#60136,.F.);
#89972=ORIENTED_EDGE('',*,*,#60133,.F.);
#89973=ORIENTED_EDGE('',*,*,#60130,.F.);
#89974=ORIENTED_EDGE('',*,*,#60127,.F.);
#89975=ORIENTED_EDGE('',*,*,#60124,.F.);
#89976=ORIENTED_EDGE('',*,*,#60121,.F.);
#89977=ORIENTED_EDGE('',*,*,#60118,.F.);
#89978=ORIENTED_EDGE('',*,*,#60115,.F.);
#89979=ORIENTED_EDGE('',*,*,#60112,.F.);
#89980=ORIENTED_EDGE('',*,*,#60265,.F.);
#89981=ORIENTED_EDGE('',*,*,#60262,.F.);
#89982=ORIENTED_EDGE('',*,*,#60259,.F.);
#89983=ORIENTED_EDGE('',*,*,#60256,.F.);
#89984=ORIENTED_EDGE('',*,*,#60253,.F.);
#89985=ORIENTED_EDGE('',*,*,#60250,.F.);
#89986=ORIENTED_EDGE('',*,*,#60247,.F.);
#89987=ORIENTED_EDGE('',*,*,#60244,.F.);
#89988=ORIENTED_EDGE('',*,*,#60241,.F.);
#89989=ORIENTED_EDGE('',*,*,#60238,.F.);
#89990=ORIENTED_EDGE('',*,*,#60235,.F.);
#89991=ORIENTED_EDGE('',*,*,#60232,.F.);
#89992=ORIENTED_EDGE('',*,*,#60229,.F.);
#89993=ORIENTED_EDGE('',*,*,#60378,.F.);
#89994=ORIENTED_EDGE('',*,*,#60375,.F.);
#89995=ORIENTED_EDGE('',*,*,#60372,.F.);
#89996=ORIENTED_EDGE('',*,*,#60369,.F.);
#89997=ORIENTED_EDGE('',*,*,#60366,.F.);
#89998=ORIENTED_EDGE('',*,*,#60363,.F.);
#89999=ORIENTED_EDGE('',*,*,#60360,.F.);
#90000=ORIENTED_EDGE('',*,*,#60357,.F.);
#90001=ORIENTED_EDGE('',*,*,#60354,.F.);
#90002=ORIENTED_EDGE('',*,*,#60351,.F.);
#90003=ORIENTED_EDGE('',*,*,#60348,.F.);
#90004=ORIENTED_EDGE('',*,*,#60345,.F.);
#90005=ORIENTED_EDGE('',*,*,#60342,.F.);
#90006=ORIENTED_EDGE('',*,*,#60339,.F.);
#90007=ORIENTED_EDGE('',*,*,#60336,.F.);
#90008=ORIENTED_EDGE('',*,*,#60333,.F.);
#90009=ORIENTED_EDGE('',*,*,#60330,.F.);
#90010=ORIENTED_EDGE('',*,*,#60327,.F.);
#90011=ORIENTED_EDGE('',*,*,#60324,.F.);
#90012=ORIENTED_EDGE('',*,*,#60321,.F.);
#90013=ORIENTED_EDGE('',*,*,#60318,.F.);
#90014=ORIENTED_EDGE('',*,*,#60315,.F.);
#90015=ORIENTED_EDGE('',*,*,#60312,.F.);
#90016=ORIENTED_EDGE('',*,*,#60309,.F.);
#90017=ORIENTED_EDGE('',*,*,#60306,.F.);
#90018=ORIENTED_EDGE('',*,*,#60303,.F.);
#90019=ORIENTED_EDGE('',*,*,#60300,.F.);
#90020=ORIENTED_EDGE('',*,*,#60297,.F.);
#90021=ORIENTED_EDGE('',*,*,#60294,.F.);
#90022=ORIENTED_EDGE('',*,*,#60291,.F.);
#90023=ORIENTED_EDGE('',*,*,#60288,.F.);
#90024=ORIENTED_EDGE('',*,*,#60285,.F.);
#90025=ORIENTED_EDGE('',*,*,#60282,.F.);
#90026=ORIENTED_EDGE('',*,*,#60279,.F.);
#90027=ORIENTED_EDGE('',*,*,#60276,.F.);
#90028=ORIENTED_EDGE('',*,*,#60273,.F.);
#90029=ORIENTED_EDGE('',*,*,#60270,.F.);
#90030=ORIENTED_EDGE('',*,*,#60267,.F.);
#90031=ORIENTED_EDGE('',*,*,#59796,.F.);
#90032=ORIENTED_EDGE('',*,*,#59793,.F.);
#90033=ORIENTED_EDGE('',*,*,#59790,.F.);
#90034=ORIENTED_EDGE('',*,*,#59787,.F.);
#90035=ORIENTED_EDGE('',*,*,#59784,.F.);
#90036=ORIENTED_EDGE('',*,*,#59781,.F.);
#90037=ORIENTED_EDGE('',*,*,#59778,.F.);
#90038=ORIENTED_EDGE('',*,*,#59775,.F.);
#90039=ORIENTED_EDGE('',*,*,#59772,.F.);
#90040=ORIENTED_EDGE('',*,*,#59769,.F.);
#90041=ORIENTED_EDGE('',*,*,#59766,.F.);
#90042=ORIENTED_EDGE('',*,*,#59763,.F.);
#90043=ORIENTED_EDGE('',*,*,#59760,.F.);
#90044=ORIENTED_EDGE('',*,*,#59757,.F.);
#90045=ORIENTED_EDGE('',*,*,#59914,.F.);
#90046=ORIENTED_EDGE('',*,*,#59911,.F.);
#90047=ORIENTED_EDGE('',*,*,#59908,.F.);
#90048=ORIENTED_EDGE('',*,*,#59905,.F.);
#90049=ORIENTED_EDGE('',*,*,#59902,.F.);
#90050=ORIENTED_EDGE('',*,*,#59899,.F.);
#90051=ORIENTED_EDGE('',*,*,#59753,.F.);
#90052=ORIENTED_EDGE('',*,*,#60381,.F.);
#90053=ORIENTED_EDGE('',*,*,#60383,.F.);
#90054=ORIENTED_EDGE('',*,*,#59896,.F.);
#90055=ORIENTED_EDGE('',*,*,#60413,.F.);
#90056=ORIENTED_EDGE('',*,*,#60414,.F.);
#90057=ORIENTED_EDGE('',*,*,#60415,.T.);
#90058=ORIENTED_EDGE('',*,*,#60416,.T.);
#90059=ORIENTED_EDGE('',*,*,#60417,.F.);
#90060=ORIENTED_EDGE('',*,*,#60416,.F.);
#90061=ORIENTED_EDGE('',*,*,#60418,.T.);
#90062=ORIENTED_EDGE('',*,*,#60419,.T.);
#90063=ORIENTED_EDGE('',*,*,#60420,.F.);
#90064=ORIENTED_EDGE('',*,*,#60419,.F.);
#90065=ORIENTED_EDGE('',*,*,#60421,.T.);
#90066=ORIENTED_EDGE('',*,*,#60422,.T.);
#90067=ORIENTED_EDGE('',*,*,#60423,.F.);
#90068=ORIENTED_EDGE('',*,*,#60422,.F.);
#90069=ORIENTED_EDGE('',*,*,#60424,.T.);
#90070=ORIENTED_EDGE('',*,*,#60414,.T.);
#90071=ORIENTED_EDGE('',*,*,#60424,.F.);
#90072=ORIENTED_EDGE('',*,*,#60421,.F.);
#90073=ORIENTED_EDGE('',*,*,#60418,.F.);
#90074=ORIENTED_EDGE('',*,*,#60415,.F.);
#90075=ORIENTED_EDGE('',*,*,#59886,.T.);
#90076=ORIENTED_EDGE('',*,*,#59889,.T.);
#90077=ORIENTED_EDGE('',*,*,#59892,.T.);
#90078=ORIENTED_EDGE('',*,*,#59895,.T.);
#90079=ORIENTED_EDGE('',*,*,#60382,.T.);
#90080=ORIENTED_EDGE('',*,*,#60379,.T.);
#90081=ORIENTED_EDGE('',*,*,#59751,.T.);
#90082=ORIENTED_EDGE('',*,*,#59898,.T.);
#90083=ORIENTED_EDGE('',*,*,#59901,.T.);
#90084=ORIENTED_EDGE('',*,*,#59904,.T.);
#90085=ORIENTED_EDGE('',*,*,#59907,.T.);
#90086=ORIENTED_EDGE('',*,*,#59910,.T.);
#90087=ORIENTED_EDGE('',*,*,#59913,.T.);
#90088=ORIENTED_EDGE('',*,*,#59755,.T.);
#90089=ORIENTED_EDGE('',*,*,#59759,.T.);
#90090=ORIENTED_EDGE('',*,*,#59762,.T.);
#90091=ORIENTED_EDGE('',*,*,#59765,.T.);
#90092=ORIENTED_EDGE('',*,*,#59768,.T.);
#90093=ORIENTED_EDGE('',*,*,#59771,.T.);
#90094=ORIENTED_EDGE('',*,*,#59774,.T.);
#90095=ORIENTED_EDGE('',*,*,#59777,.T.);
#90096=ORIENTED_EDGE('',*,*,#59780,.T.);
#90097=ORIENTED_EDGE('',*,*,#59783,.T.);
#90098=ORIENTED_EDGE('',*,*,#59786,.T.);
#90099=ORIENTED_EDGE('',*,*,#59789,.T.);
#90100=ORIENTED_EDGE('',*,*,#59792,.T.);
#90101=ORIENTED_EDGE('',*,*,#59795,.T.);
#90102=ORIENTED_EDGE('',*,*,#60266,.T.);
#90103=ORIENTED_EDGE('',*,*,#60269,.T.);
#90104=ORIENTED_EDGE('',*,*,#60272,.T.);
#90105=ORIENTED_EDGE('',*,*,#60275,.T.);
#90106=ORIENTED_EDGE('',*,*,#60278,.T.);
#90107=ORIENTED_EDGE('',*,*,#60281,.T.);
#90108=ORIENTED_EDGE('',*,*,#60284,.T.);
#90109=ORIENTED_EDGE('',*,*,#60287,.T.);
#90110=ORIENTED_EDGE('',*,*,#60290,.T.);
#90111=ORIENTED_EDGE('',*,*,#60293,.T.);
#90112=ORIENTED_EDGE('',*,*,#60296,.T.);
#90113=ORIENTED_EDGE('',*,*,#60299,.T.);
#90114=ORIENTED_EDGE('',*,*,#60302,.T.);
#90115=ORIENTED_EDGE('',*,*,#60305,.T.);
#90116=ORIENTED_EDGE('',*,*,#60308,.T.);
#90117=ORIENTED_EDGE('',*,*,#60311,.T.);
#90118=ORIENTED_EDGE('',*,*,#60314,.T.);
#90119=ORIENTED_EDGE('',*,*,#60317,.T.);
#90120=ORIENTED_EDGE('',*,*,#60320,.T.);
#90121=ORIENTED_EDGE('',*,*,#60323,.T.);
#90122=ORIENTED_EDGE('',*,*,#60326,.T.);
#90123=ORIENTED_EDGE('',*,*,#60329,.T.);
#90124=ORIENTED_EDGE('',*,*,#60332,.T.);
#90125=ORIENTED_EDGE('',*,*,#60335,.T.);
#90126=ORIENTED_EDGE('',*,*,#60338,.T.);
#90127=ORIENTED_EDGE('',*,*,#60341,.T.);
#90128=ORIENTED_EDGE('',*,*,#60344,.T.);
#90129=ORIENTED_EDGE('',*,*,#60347,.T.);
#90130=ORIENTED_EDGE('',*,*,#60350,.T.);
#90131=ORIENTED_EDGE('',*,*,#60353,.T.);
#90132=ORIENTED_EDGE('',*,*,#60356,.T.);
#90133=ORIENTED_EDGE('',*,*,#60359,.T.);
#90134=ORIENTED_EDGE('',*,*,#60362,.T.);
#90135=ORIENTED_EDGE('',*,*,#60365,.T.);
#90136=ORIENTED_EDGE('',*,*,#60368,.T.);
#90137=ORIENTED_EDGE('',*,*,#60371,.T.);
#90138=ORIENTED_EDGE('',*,*,#60374,.T.);
#90139=ORIENTED_EDGE('',*,*,#60377,.T.);
#90140=ORIENTED_EDGE('',*,*,#60227,.T.);
#90141=ORIENTED_EDGE('',*,*,#60231,.T.);
#90142=ORIENTED_EDGE('',*,*,#60234,.T.);
#90143=ORIENTED_EDGE('',*,*,#60237,.T.);
#90144=ORIENTED_EDGE('',*,*,#60240,.T.);
#90145=ORIENTED_EDGE('',*,*,#60243,.T.);
#90146=ORIENTED_EDGE('',*,*,#60246,.T.);
#90147=ORIENTED_EDGE('',*,*,#60249,.T.);
#90148=ORIENTED_EDGE('',*,*,#60252,.T.);
#90149=ORIENTED_EDGE('',*,*,#60255,.T.);
#90150=ORIENTED_EDGE('',*,*,#60258,.T.);
#90151=ORIENTED_EDGE('',*,*,#60261,.T.);
#90152=ORIENTED_EDGE('',*,*,#60264,.T.);
#90153=ORIENTED_EDGE('',*,*,#60110,.T.);
#90154=ORIENTED_EDGE('',*,*,#60114,.T.);
#90155=ORIENTED_EDGE('',*,*,#60117,.T.);
#90156=ORIENTED_EDGE('',*,*,#60120,.T.);
#90157=ORIENTED_EDGE('',*,*,#60123,.T.);
#90158=ORIENTED_EDGE('',*,*,#60126,.T.);
#90159=ORIENTED_EDGE('',*,*,#60129,.T.);
#90160=ORIENTED_EDGE('',*,*,#60132,.T.);
#90161=ORIENTED_EDGE('',*,*,#60135,.T.);
#90162=ORIENTED_EDGE('',*,*,#60138,.T.);
#90163=ORIENTED_EDGE('',*,*,#60141,.T.);
#90164=ORIENTED_EDGE('',*,*,#60144,.T.);
#90165=ORIENTED_EDGE('',*,*,#60147,.T.);
#90166=ORIENTED_EDGE('',*,*,#60150,.T.);
#90167=ORIENTED_EDGE('',*,*,#60153,.T.);
#90168=ORIENTED_EDGE('',*,*,#60156,.T.);
#90169=ORIENTED_EDGE('',*,*,#60159,.T.);
#90170=ORIENTED_EDGE('',*,*,#60162,.T.);
#90171=ORIENTED_EDGE('',*,*,#60165,.T.);
#90172=ORIENTED_EDGE('',*,*,#60168,.T.);
#90173=ORIENTED_EDGE('',*,*,#60171,.T.);
#90174=ORIENTED_EDGE('',*,*,#60174,.T.);
#90175=ORIENTED_EDGE('',*,*,#60177,.T.);
#90176=ORIENTED_EDGE('',*,*,#60180,.T.);
#90177=ORIENTED_EDGE('',*,*,#60183,.T.);
#90178=ORIENTED_EDGE('',*,*,#60186,.T.);
#90179=ORIENTED_EDGE('',*,*,#60189,.T.);
#90180=ORIENTED_EDGE('',*,*,#60192,.T.);
#90181=ORIENTED_EDGE('',*,*,#60195,.T.);
#90182=ORIENTED_EDGE('',*,*,#60198,.T.);
#90183=ORIENTED_EDGE('',*,*,#60201,.T.);
#90184=ORIENTED_EDGE('',*,*,#60204,.T.);
#90185=ORIENTED_EDGE('',*,*,#60207,.T.);
#90186=ORIENTED_EDGE('',*,*,#60210,.T.);
#90187=ORIENTED_EDGE('',*,*,#60213,.T.);
#90188=ORIENTED_EDGE('',*,*,#60216,.T.);
#90189=ORIENTED_EDGE('',*,*,#60219,.T.);
#90190=ORIENTED_EDGE('',*,*,#60222,.T.);
#90191=ORIENTED_EDGE('',*,*,#60225,.T.);
#90192=ORIENTED_EDGE('',*,*,#60071,.T.);
#90193=ORIENTED_EDGE('',*,*,#60075,.T.);
#90194=ORIENTED_EDGE('',*,*,#60078,.T.);
#90195=ORIENTED_EDGE('',*,*,#60081,.T.);
#90196=ORIENTED_EDGE('',*,*,#60084,.T.);
#90197=ORIENTED_EDGE('',*,*,#60087,.T.);
#90198=ORIENTED_EDGE('',*,*,#60090,.T.);
#90199=ORIENTED_EDGE('',*,*,#60093,.T.);
#90200=ORIENTED_EDGE('',*,*,#60096,.T.);
#90201=ORIENTED_EDGE('',*,*,#60099,.T.);
#90202=ORIENTED_EDGE('',*,*,#60102,.T.);
#90203=ORIENTED_EDGE('',*,*,#60105,.T.);
#90204=ORIENTED_EDGE('',*,*,#60108,.T.);
#90205=ORIENTED_EDGE('',*,*,#59954,.T.);
#90206=ORIENTED_EDGE('',*,*,#59958,.T.);
#90207=ORIENTED_EDGE('',*,*,#59961,.T.);
#90208=ORIENTED_EDGE('',*,*,#59964,.T.);
#90209=ORIENTED_EDGE('',*,*,#59967,.T.);
#90210=ORIENTED_EDGE('',*,*,#59970,.T.);
#90211=ORIENTED_EDGE('',*,*,#59973,.T.);
#90212=ORIENTED_EDGE('',*,*,#59976,.T.);
#90213=ORIENTED_EDGE('',*,*,#59979,.T.);
#90214=ORIENTED_EDGE('',*,*,#59982,.T.);
#90215=ORIENTED_EDGE('',*,*,#59985,.T.);
#90216=ORIENTED_EDGE('',*,*,#59988,.T.);
#90217=ORIENTED_EDGE('',*,*,#59991,.T.);
#90218=ORIENTED_EDGE('',*,*,#59994,.T.);
#90219=ORIENTED_EDGE('',*,*,#59997,.T.);
#90220=ORIENTED_EDGE('',*,*,#60000,.T.);
#90221=ORIENTED_EDGE('',*,*,#60003,.T.);
#90222=ORIENTED_EDGE('',*,*,#60006,.T.);
#90223=ORIENTED_EDGE('',*,*,#60009,.T.);
#90224=ORIENTED_EDGE('',*,*,#60012,.T.);
#90225=ORIENTED_EDGE('',*,*,#60015,.T.);
#90226=ORIENTED_EDGE('',*,*,#60018,.T.);
#90227=ORIENTED_EDGE('',*,*,#60021,.T.);
#90228=ORIENTED_EDGE('',*,*,#60024,.T.);
#90229=ORIENTED_EDGE('',*,*,#60027,.T.);
#90230=ORIENTED_EDGE('',*,*,#60030,.T.);
#90231=ORIENTED_EDGE('',*,*,#60033,.T.);
#90232=ORIENTED_EDGE('',*,*,#60036,.T.);
#90233=ORIENTED_EDGE('',*,*,#60039,.T.);
#90234=ORIENTED_EDGE('',*,*,#60042,.T.);
#90235=ORIENTED_EDGE('',*,*,#60045,.T.);
#90236=ORIENTED_EDGE('',*,*,#60048,.T.);
#90237=ORIENTED_EDGE('',*,*,#60051,.T.);
#90238=ORIENTED_EDGE('',*,*,#60054,.T.);
#90239=ORIENTED_EDGE('',*,*,#60057,.T.);
#90240=ORIENTED_EDGE('',*,*,#60060,.T.);
#90241=ORIENTED_EDGE('',*,*,#60063,.T.);
#90242=ORIENTED_EDGE('',*,*,#60066,.T.);
#90243=ORIENTED_EDGE('',*,*,#60069,.T.);
#90244=ORIENTED_EDGE('',*,*,#59915,.T.);
#90245=ORIENTED_EDGE('',*,*,#59919,.T.);
#90246=ORIENTED_EDGE('',*,*,#59922,.T.);
#90247=ORIENTED_EDGE('',*,*,#59925,.T.);
#90248=ORIENTED_EDGE('',*,*,#59928,.T.);
#90249=ORIENTED_EDGE('',*,*,#59931,.T.);
#90250=ORIENTED_EDGE('',*,*,#59934,.T.);
#90251=ORIENTED_EDGE('',*,*,#59937,.T.);
#90252=ORIENTED_EDGE('',*,*,#59940,.T.);
#90253=ORIENTED_EDGE('',*,*,#59943,.T.);
#90254=ORIENTED_EDGE('',*,*,#59946,.T.);
#90255=ORIENTED_EDGE('',*,*,#59949,.T.);
#90256=ORIENTED_EDGE('',*,*,#59952,.T.);
#90257=ORIENTED_EDGE('',*,*,#59798,.T.);
#90258=ORIENTED_EDGE('',*,*,#59802,.T.);
#90259=ORIENTED_EDGE('',*,*,#59805,.T.);
#90260=ORIENTED_EDGE('',*,*,#59808,.T.);
#90261=ORIENTED_EDGE('',*,*,#59811,.T.);
#90262=ORIENTED_EDGE('',*,*,#59814,.T.);
#90263=ORIENTED_EDGE('',*,*,#59817,.T.);
#90264=ORIENTED_EDGE('',*,*,#59820,.T.);
#90265=ORIENTED_EDGE('',*,*,#59823,.T.);
#90266=ORIENTED_EDGE('',*,*,#59826,.T.);
#90267=ORIENTED_EDGE('',*,*,#59829,.T.);
#90268=ORIENTED_EDGE('',*,*,#59832,.T.);
#90269=ORIENTED_EDGE('',*,*,#59835,.T.);
#90270=ORIENTED_EDGE('',*,*,#59838,.T.);
#90271=ORIENTED_EDGE('',*,*,#59841,.T.);
#90272=ORIENTED_EDGE('',*,*,#59844,.T.);
#90273=ORIENTED_EDGE('',*,*,#59847,.T.);
#90274=ORIENTED_EDGE('',*,*,#59850,.T.);
#90275=ORIENTED_EDGE('',*,*,#59853,.T.);
#90276=ORIENTED_EDGE('',*,*,#59856,.T.);
#90277=ORIENTED_EDGE('',*,*,#59747,.T.);
#90278=ORIENTED_EDGE('',*,*,#60384,.T.);
#90279=ORIENTED_EDGE('',*,*,#60387,.T.);
#90280=ORIENTED_EDGE('',*,*,#59858,.T.);
#90281=ORIENTED_EDGE('',*,*,#59862,.T.);
#90282=ORIENTED_EDGE('',*,*,#59865,.T.);
#90283=ORIENTED_EDGE('',*,*,#59868,.T.);
#90284=ORIENTED_EDGE('',*,*,#59871,.T.);
#90285=ORIENTED_EDGE('',*,*,#59874,.T.);
#90286=ORIENTED_EDGE('',*,*,#59877,.T.);
#90287=ORIENTED_EDGE('',*,*,#59880,.T.);
#90288=ORIENTED_EDGE('',*,*,#59883,.T.);
#90289=ORIENTED_EDGE('',*,*,#60423,.T.);
#90290=ORIENTED_EDGE('',*,*,#60413,.T.);
#90291=ORIENTED_EDGE('',*,*,#60417,.T.);
#90292=ORIENTED_EDGE('',*,*,#60420,.T.);
#90293=CYLINDRICAL_SURFACE('',#98804,8.4455);
#90294=CYLINDRICAL_SURFACE('',#98807,8.4455);
#90295=CYLINDRICAL_SURFACE('',#98810,8.4455);
#90296=CYLINDRICAL_SURFACE('',#98813,8.4455);
#90297=CYLINDRICAL_SURFACE('',#98851,25.);
#90298=CYLINDRICAL_SURFACE('',#98853,25.);
#90299=CYLINDRICAL_SURFACE('',#98855,25.);
#90300=CYLINDRICAL_SURFACE('',#98857,25.);
#90301=CYLINDRICAL_SURFACE('',#98862,2.);
#90302=CYLINDRICAL_SURFACE('',#98864,2.);
#90303=CYLINDRICAL_SURFACE('',#98870,2.);
#90304=CYLINDRICAL_SURFACE('',#98872,2.);
#90305=CYLINDRICAL_SURFACE('',#98886,5.15937500000002);
#90306=CYLINDRICAL_SURFACE('',#98887,5.15937500000002);
#90307=CYLINDRICAL_SURFACE('',#98888,5.15937500000008);
#90308=CYLINDRICAL_SURFACE('',#98889,5.15937500000008);
#90309=CYLINDRICAL_SURFACE('',#98890,11.3170000000002);
#90310=CYLINDRICAL_SURFACE('',#98892,9.00000000000018);
#90311=CYLINDRICAL_SURFACE('',#98896,18.0480000000001);
#90312=CYLINDRICAL_SURFACE('',#98897,18.0480000000001);
#90313=CYLINDRICAL_SURFACE('',#98898,18.0480000000001);
#90314=CYLINDRICAL_SURFACE('',#98899,18.0480000000001);
#90315=CYLINDRICAL_SURFACE('',#98900,18.0480000000001);
#90316=CYLINDRICAL_SURFACE('',#98901,18.0480000000001);
#90317=CYLINDRICAL_SURFACE('',#98902,18.0480000000001);
#90318=CYLINDRICAL_SURFACE('',#98903,18.0480000000001);
#90319=CYLINDRICAL_SURFACE('',#98904,15.);
#90320=CYLINDRICAL_SURFACE('',#98906,15.);
#90321=CYLINDRICAL_SURFACE('',#98907,15.);
#90322=CYLINDRICAL_SURFACE('',#98908,15.);
#90323=CYLINDRICAL_SURFACE('',#98909,15.);
#90324=CYLINDRICAL_SURFACE('',#98910,15.);
#90325=CYLINDRICAL_SURFACE('',#98911,15.);
#90326=CYLINDRICAL_SURFACE('',#98912,15.);
#90327=CYLINDRICAL_SURFACE('',#98913,39.);
#90328=CYLINDRICAL_SURFACE('',#98915,39.);
#90329=CYLINDRICAL_SURFACE('',#98916,39.);
#90330=CYLINDRICAL_SURFACE('',#98917,39.);
#90331=CYLINDRICAL_SURFACE('',#98918,39.);
#90332=CYLINDRICAL_SURFACE('',#98919,39.);
#90333=CYLINDRICAL_SURFACE('',#98920,39.);
#90334=CYLINDRICAL_SURFACE('',#98921,39.);
#90335=CYLINDRICAL_SURFACE('',#98922,5.15937500000002);
#90336=CYLINDRICAL_SURFACE('',#98923,5.15937500000002);
#90337=CYLINDRICAL_SURFACE('',#98924,5.15937500000008);
#90338=CYLINDRICAL_SURFACE('',#98925,5.15937500000008);
#90339=CYLINDRICAL_SURFACE('',#98926,39.);
#90340=CYLINDRICAL_SURFACE('',#98927,15.);
#90341=CYLINDRICAL_SURFACE('',#98929,11.444);
#90342=CYLINDRICAL_SURFACE('',#98934,18.0480000000001);
#90343=CYLINDRICAL_SURFACE('',#98945,0.508000000000002);
#90344=CYLINDRICAL_SURFACE('',#98948,5.1435);
#90345=CYLINDRICAL_SURFACE('',#98972,0.952499999999998);
#90346=CYLINDRICAL_SURFACE('',#99000,0.508000000000002);
#90347=CYLINDRICAL_SURFACE('',#99001,0.508000000000002);
#90348=CYLINDRICAL_SURFACE('',#99002,0.508000000000002);
#90349=CYLINDRICAL_SURFACE('',#99003,0.508000000000002);
#90350=CYLINDRICAL_SURFACE('',#99004,0.508000000000002);
#90351=CYLINDRICAL_SURFACE('',#99005,7.9375);
#90352=CYLINDRICAL_SURFACE('',#99008,8.4455);
#90353=CYLINDRICAL_SURFACE('',#99013,7.9375);
#90354=CYLINDRICAL_SURFACE('',#99016,8.4455);
#90355=CYLINDRICAL_SURFACE('',#99021,7.9375);
#90356=CYLINDRICAL_SURFACE('',#99024,8.4455);
#90357=CYLINDRICAL_SURFACE('',#99029,7.9375);
#90358=CYLINDRICAL_SURFACE('',#99032,8.4455);
#90359=CYLINDRICAL_SURFACE('',#99047,51.27);
#90360=CYLINDRICAL_SURFACE('',#99049,50.);
#90361=CYLINDRICAL_SURFACE('',#99063,56.875);
#90362=CYLINDRICAL_SURFACE('',#99065,55.605);
#90363=CYLINDRICAL_SURFACE('',#99069,51.27);
#90364=CYLINDRICAL_SURFACE('',#99072,55.605);
#90365=CYLINDRICAL_SURFACE('',#99116,65.);
#90366=CYLINDRICAL_SURFACE('',#99362,56.875);
#90367=CYLINDRICAL_SURFACE('',#101120,0.175259999999997);
#90368=CYLINDRICAL_SURFACE('',#101121,0.175259999999997);
#90369=CYLINDRICAL_SURFACE('',#101122,0.126999999706107);
#90370=CYLINDRICAL_SURFACE('',#101126,0.127000000000002);
#90371=CYLINDRICAL_SURFACE('',#101128,0.127000000000002);
#90372=CYLINDRICAL_SURFACE('',#101132,0.127000005437004);
#90373=CYLINDRICAL_SURFACE('',#101134,0.12700000128033);
#90374=CYLINDRICAL_SURFACE('',#101137,0.127000000000002);
#90375=CYLINDRICAL_SURFACE('',#101143,0.126999993615305);
#90376=CYLINDRICAL_SURFACE('',#101145,0.127000005453425);
#90377=CYLINDRICAL_SURFACE('',#101151,0.127000000000002);
#90378=CYLINDRICAL_SURFACE('',#101154,0.126999998754292);
#90379=CYLINDRICAL_SURFACE('',#101156,0.126999993594532);
#90380=CYLINDRICAL_SURFACE('',#101160,0.127000000000002);
#90381=CYLINDRICAL_SURFACE('',#101162,0.127000000000002);
#90382=CYLINDRICAL_SURFACE('',#101165,0.127000000300332);
#90383=CYLINDRICAL_SURFACE('',#101929,0.175259999999999);
#90384=CYLINDRICAL_SURFACE('',#101930,0.17526);
#90385=CYLINDRICAL_SURFACE('',#101931,0.175259999999999);
#90386=CYLINDRICAL_SURFACE('',#101932,0.17526);
#90387=CYLINDRICAL_SURFACE('',#101933,0.175259999999999);
#90388=CYLINDRICAL_SURFACE('',#101934,0.17526);
#90389=CYLINDRICAL_SURFACE('',#101935,0.17526);
#90390=CYLINDRICAL_SURFACE('',#101936,0.17526);
#90391=CYLINDRICAL_SURFACE('',#101937,0.175259999999998);
#90392=CYLINDRICAL_SURFACE('',#101938,0.17526);
#90393=CYLINDRICAL_SURFACE('',#101939,0.17526);
#90394=CYLINDRICAL_SURFACE('',#101940,0.17526);
#90395=CYLINDRICAL_SURFACE('',#101941,0.175260000000001);
#90396=CYLINDRICAL_SURFACE('',#101942,0.17526);
#90397=CYLINDRICAL_SURFACE('',#101943,0.175260000000001);
#90398=CYLINDRICAL_SURFACE('',#101944,0.17526);
#90399=CYLINDRICAL_SURFACE('',#101945,0.17526);
#90400=CYLINDRICAL_SURFACE('',#101946,0.17526);
#90401=CYLINDRICAL_SURFACE('',#101947,0.175260000000001);
#90402=CYLINDRICAL_SURFACE('',#101948,0.17526);
#90403=CYLINDRICAL_SURFACE('',#101949,0.17526);
#90404=CYLINDRICAL_SURFACE('',#101950,0.17526);
#90405=CYLINDRICAL_SURFACE('',#101951,0.175259999999999);
#90406=CYLINDRICAL_SURFACE('',#101952,0.17526);
#90407=CYLINDRICAL_SURFACE('',#101953,0.175259999999999);
#90408=CYLINDRICAL_SURFACE('',#101954,0.17526);
#90409=CYLINDRICAL_SURFACE('',#101955,0.175259999999999);
#90410=CYLINDRICAL_SURFACE('',#101956,0.17526);
#90411=CYLINDRICAL_SURFACE('',#101957,0.17526);
#90412=CYLINDRICAL_SURFACE('',#101958,0.17526);
#90413=CYLINDRICAL_SURFACE('',#101959,0.175259999999999);
#90414=CYLINDRICAL_SURFACE('',#101960,0.17526);
#90415=CYLINDRICAL_SURFACE('',#101961,0.17526);
#90416=CYLINDRICAL_SURFACE('',#101962,0.17526);
#90417=CYLINDRICAL_SURFACE('',#101963,0.175259999999999);
#90418=CYLINDRICAL_SURFACE('',#101964,0.17526);
#90419=CYLINDRICAL_SURFACE('',#101965,0.17526);
#90420=CYLINDRICAL_SURFACE('',#101966,0.17526);
#90421=CYLINDRICAL_SURFACE('',#101967,0.175259999999998);
#90422=CYLINDRICAL_SURFACE('',#101968,0.17526);
#90423=CYLINDRICAL_SURFACE('',#101969,0.17526);
#90424=CYLINDRICAL_SURFACE('',#101970,0.17526);
#90425=CYLINDRICAL_SURFACE('',#101971,0.175260000000001);
#90426=CYLINDRICAL_SURFACE('',#101972,0.17526);
#90427=CYLINDRICAL_SURFACE('',#101973,0.175260000000001);
#90428=CYLINDRICAL_SURFACE('',#101974,0.17526);
#90429=CYLINDRICAL_SURFACE('',#101975,0.17526);
#90430=CYLINDRICAL_SURFACE('',#101976,0.17526);
#90431=CYLINDRICAL_SURFACE('',#101977,0.175260000000001);
#90432=CYLINDRICAL_SURFACE('',#101978,0.17526);
#90433=CYLINDRICAL_SURFACE('',#101979,0.175260000000003);
#90434=CYLINDRICAL_SURFACE('',#101980,0.17526);
#90435=CYLINDRICAL_SURFACE('',#101981,0.175259999999999);
#90436=CYLINDRICAL_SURFACE('',#101982,0.17526);
#90437=CYLINDRICAL_SURFACE('',#101983,0.175259999999999);
#90438=CYLINDRICAL_SURFACE('',#101984,0.17526);
#90439=CYLINDRICAL_SURFACE('',#101985,0.17526);
#90440=CYLINDRICAL_SURFACE('',#101986,0.17526);
#90441=CYLINDRICAL_SURFACE('',#101987,0.175259999999997);
#90442=CYLINDRICAL_SURFACE('',#101988,0.175259999999997);
#90443=CYLINDRICAL_SURFACE('',#101989,0.17526);
#90444=CYLINDRICAL_SURFACE('',#101990,0.17526);
#90445=CYLINDRICAL_SURFACE('',#101991,0.17526);
#90446=CYLINDRICAL_SURFACE('',#101992,0.17526);
#90447=CYLINDRICAL_SURFACE('',#101993,0.175259999999999);
#90448=CYLINDRICAL_SURFACE('',#101994,0.17526);
#90449=CYLINDRICAL_SURFACE('',#101995,0.17526);
#90450=CYLINDRICAL_SURFACE('',#101996,0.17526);
#90451=CYLINDRICAL_SURFACE('',#101997,0.175259999999998);
#90452=CYLINDRICAL_SURFACE('',#101998,0.17526);
#90453=CYLINDRICAL_SURFACE('',#101999,0.17526);
#90454=CYLINDRICAL_SURFACE('',#102000,0.17526);
#90455=CYLINDRICAL_SURFACE('',#102001,0.175259999999996);
#90456=CYLINDRICAL_SURFACE('',#102002,0.17526);
#90457=CYLINDRICAL_SURFACE('',#102003,0.175260000000001);
#90458=CYLINDRICAL_SURFACE('',#102004,0.17526);
#90459=CYLINDRICAL_SURFACE('',#102005,0.175259999999995);
#90460=CYLINDRICAL_SURFACE('',#102006,0.17526);
#90461=CYLINDRICAL_SURFACE('',#102007,0.175260000000001);
#90462=CYLINDRICAL_SURFACE('',#102008,0.17526);
#90463=CYLINDRICAL_SURFACE('',#102009,0.17526);
#90464=CYLINDRICAL_SURFACE('',#102010,0.17526);
#90465=CYLINDRICAL_SURFACE('',#102011,0.175259999999999);
#90466=CYLINDRICAL_SURFACE('',#102012,0.17526);
#90467=CYLINDRICAL_SURFACE('',#102013,0.175259999999999);
#90468=CYLINDRICAL_SURFACE('',#102014,0.17526);
#90469=CYLINDRICAL_SURFACE('',#102015,0.17526);
#90470=CYLINDRICAL_SURFACE('',#102016,0.17526);
#90471=CYLINDRICAL_SURFACE('',#102017,0.17526);
#90472=CYLINDRICAL_SURFACE('',#102018,0.17526);
#90473=CYLINDRICAL_SURFACE('',#102019,0.17526);
#90474=CYLINDRICAL_SURFACE('',#102020,0.17526);
#90475=CYLINDRICAL_SURFACE('',#102021,0.17526);
#90476=CYLINDRICAL_SURFACE('',#102022,0.17526);
#90477=CYLINDRICAL_SURFACE('',#102023,0.175259999999999);
#90478=CYLINDRICAL_SURFACE('',#102024,0.17526);
#90479=CYLINDRICAL_SURFACE('',#102025,0.17526);
#90480=CYLINDRICAL_SURFACE('',#102026,0.17526);
#90481=CYLINDRICAL_SURFACE('',#102027,0.175260000000001);
#90482=CYLINDRICAL_SURFACE('',#102028,0.17526);
#90483=CYLINDRICAL_SURFACE('',#102029,0.17526);
#90484=CYLINDRICAL_SURFACE('',#102030,0.17526);
#90485=CYLINDRICAL_SURFACE('',#102031,0.175259999999996);
#90486=CYLINDRICAL_SURFACE('',#102032,0.17526);
#90487=CYLINDRICAL_SURFACE('',#102033,0.175260000000001);
#90488=CYLINDRICAL_SURFACE('',#102034,0.17526);
#90489=CYLINDRICAL_SURFACE('',#102035,0.175260000000001);
#90490=CYLINDRICAL_SURFACE('',#102036,0.17526);
#90491=CYLINDRICAL_SURFACE('',#102037,0.175260000000001);
#90492=CYLINDRICAL_SURFACE('',#102038,0.17526);
#90493=CYLINDRICAL_SURFACE('',#102039,0.17526);
#90494=CYLINDRICAL_SURFACE('',#102040,0.17526);
#90495=CYLINDRICAL_SURFACE('',#102041,0.175259999999999);
#90496=CYLINDRICAL_SURFACE('',#102042,0.17526);
#90497=CYLINDRICAL_SURFACE('',#102043,0.175260000000001);
#90498=CYLINDRICAL_SURFACE('',#102044,0.17526);
#90499=CYLINDRICAL_SURFACE('',#102045,0.17526);
#90500=CYLINDRICAL_SURFACE('',#102046,0.17526);
#90501=CYLINDRICAL_SURFACE('',#102047,0.12699999970626);
#90502=CYLINDRICAL_SURFACE('',#102051,0.127);
#90503=CYLINDRICAL_SURFACE('',#102053,0.127);
#90504=CYLINDRICAL_SURFACE('',#102057,0.12700000543866);
#90505=CYLINDRICAL_SURFACE('',#102059,0.127000001278441);
#90506=CYLINDRICAL_SURFACE('',#102062,0.127);
#90507=CYLINDRICAL_SURFACE('',#102068,0.126999993613266);
#90508=CYLINDRICAL_SURFACE('',#102070,0.12700000545647);
#90509=CYLINDRICAL_SURFACE('',#102076,0.126999999999999);
#90510=CYLINDRICAL_SURFACE('',#102079,0.126999998753988);
#90511=CYLINDRICAL_SURFACE('',#102081,0.126999993594684);
#90512=CYLINDRICAL_SURFACE('',#102085,0.126999999999999);
#90513=CYLINDRICAL_SURFACE('',#102087,0.126999999999999);
#90514=CYLINDRICAL_SURFACE('',#102090,0.127000000302185);
#90515=CYLINDRICAL_SURFACE('',#102091,0.126999999706651);
#90516=CYLINDRICAL_SURFACE('',#102095,0.127);
#90517=CYLINDRICAL_SURFACE('',#102097,0.127);
#90518=CYLINDRICAL_SURFACE('',#102101,0.127000005437342);
#90519=CYLINDRICAL_SURFACE('',#102103,0.127000001278921);
#90520=CYLINDRICAL_SURFACE('',#102106,0.127);
#90521=CYLINDRICAL_SURFACE('',#102112,0.126999993613615);
#90522=CYLINDRICAL_SURFACE('',#102114,0.127000005453428);
#90523=CYLINDRICAL_SURFACE('',#102120,0.126999999999999);
#90524=CYLINDRICAL_SURFACE('',#102123,0.126999998753426);
#90525=CYLINDRICAL_SURFACE('',#102125,0.126999993596104);
#90526=CYLINDRICAL_SURFACE('',#102129,0.126999999999999);
#90527=CYLINDRICAL_SURFACE('',#102131,0.126999999999999);
#90528=CYLINDRICAL_SURFACE('',#102134,0.127000000302599);
#90529=CYLINDRICAL_SURFACE('',#102135,0.126999999706856);
#90530=CYLINDRICAL_SURFACE('',#102139,0.127);
#90531=CYLINDRICAL_SURFACE('',#102141,0.127);
#90532=CYLINDRICAL_SURFACE('',#102145,0.127000005440703);
#90533=CYLINDRICAL_SURFACE('',#102147,0.127000001279188);
#90534=CYLINDRICAL_SURFACE('',#102150,0.127);
#90535=CYLINDRICAL_SURFACE('',#102156,0.126999993614716);
#90536=CYLINDRICAL_SURFACE('',#102158,0.127000005454496);
#90537=CYLINDRICAL_SURFACE('',#102164,0.127000000000002);
#90538=CYLINDRICAL_SURFACE('',#102167,0.126999998752722);
#90539=CYLINDRICAL_SURFACE('',#102169,0.126999993594443);
#90540=CYLINDRICAL_SURFACE('',#102173,0.127000000000002);
#90541=CYLINDRICAL_SURFACE('',#102175,0.127000000000002);
#90542=CYLINDRICAL_SURFACE('',#102178,0.127000000302178);
#90543=CYLINDRICAL_SURFACE('',#102179,0.126999999705935);
#90544=CYLINDRICAL_SURFACE('',#102183,0.127);
#90545=CYLINDRICAL_SURFACE('',#102185,0.127);
#90546=CYLINDRICAL_SURFACE('',#102189,0.127000005438044);
#90547=CYLINDRICAL_SURFACE('',#102191,0.127000001278499);
#90548=CYLINDRICAL_SURFACE('',#102194,0.127);
#90549=CYLINDRICAL_SURFACE('',#102200,0.12699999361266);
#90550=CYLINDRICAL_SURFACE('',#102202,0.12700000545514);
#90551=CYLINDRICAL_SURFACE('',#102208,0.127000000000001);
#90552=CYLINDRICAL_SURFACE('',#102211,0.12699999875473);
#90553=CYLINDRICAL_SURFACE('',#102213,0.126999993593948);
#90554=CYLINDRICAL_SURFACE('',#102217,0.127000000000001);
#90555=CYLINDRICAL_SURFACE('',#102219,0.127000000000001);
#90556=CYLINDRICAL_SURFACE('',#102222,0.127000000303238);
#90557=CYLINDRICAL_SURFACE('',#102223,0.126999999706812);
#90558=CYLINDRICAL_SURFACE('',#102227,0.127);
#90559=CYLINDRICAL_SURFACE('',#102229,0.127);
#90560=CYLINDRICAL_SURFACE('',#102233,0.127000005438477);
#90561=CYLINDRICAL_SURFACE('',#102235,0.127000001279166);
#90562=CYLINDRICAL_SURFACE('',#102238,0.127);
#90563=CYLINDRICAL_SURFACE('',#102244,0.126999993615516);
#90564=CYLINDRICAL_SURFACE('',#102246,0.127000005451529);
#90565=CYLINDRICAL_SURFACE('',#102252,0.127);
#90566=CYLINDRICAL_SURFACE('',#102255,0.126999998753742);
#90567=CYLINDRICAL_SURFACE('',#102257,0.126999993594221);
#90568=CYLINDRICAL_SURFACE('',#102261,0.127);
#90569=CYLINDRICAL_SURFACE('',#102263,0.127);
#90570=CYLINDRICAL_SURFACE('',#102266,0.127000000301966);
#90571=CYLINDRICAL_SURFACE('',#102267,0.126999999706062);
#90572=CYLINDRICAL_SURFACE('',#102271,0.127);
#90573=CYLINDRICAL_SURFACE('',#102273,0.127);
#90574=CYLINDRICAL_SURFACE('',#102277,0.127000005437502);
#90575=CYLINDRICAL_SURFACE('',#102279,0.127000001278692);
#90576=CYLINDRICAL_SURFACE('',#102282,0.127);
#90577=CYLINDRICAL_SURFACE('',#102288,0.126999993615408);
#90578=CYLINDRICAL_SURFACE('',#102290,0.127000005455299);
#90579=CYLINDRICAL_SURFACE('',#102296,0.127000000000001);
#90580=CYLINDRICAL_SURFACE('',#102299,0.126999998754172);
#90581=CYLINDRICAL_SURFACE('',#102301,0.126999993593136);
#90582=CYLINDRICAL_SURFACE('',#102305,0.127000000000001);
#90583=CYLINDRICAL_SURFACE('',#102307,0.127000000000001);
#90584=CYLINDRICAL_SURFACE('',#102310,0.127000000300007);
#90585=CYLINDRICAL_SURFACE('',#102311,0.126999999707742);
#90586=CYLINDRICAL_SURFACE('',#102315,0.127);
#90587=CYLINDRICAL_SURFACE('',#102317,0.127);
#90588=CYLINDRICAL_SURFACE('',#102321,0.127000005438627);
#90589=CYLINDRICAL_SURFACE('',#102323,0.127000001278838);
#90590=CYLINDRICAL_SURFACE('',#102326,0.127);
#90591=CYLINDRICAL_SURFACE('',#102332,0.126999993616684);
#90592=CYLINDRICAL_SURFACE('',#102334,0.127000005454564);
#90593=CYLINDRICAL_SURFACE('',#102340,0.126999999999998);
#90594=CYLINDRICAL_SURFACE('',#102343,0.126999998752247);
#90595=CYLINDRICAL_SURFACE('',#102345,0.126999993594708);
#90596=CYLINDRICAL_SURFACE('',#102349,0.126999999999998);
#90597=CYLINDRICAL_SURFACE('',#102351,0.126999999999998);
#90598=CYLINDRICAL_SURFACE('',#102354,0.127000000303882);
#90599=CYLINDRICAL_SURFACE('',#102355,0.126999999707639);
#90600=CYLINDRICAL_SURFACE('',#102359,0.127);
#90601=CYLINDRICAL_SURFACE('',#102361,0.127);
#90602=CYLINDRICAL_SURFACE('',#102365,0.127000005438079);
#90603=CYLINDRICAL_SURFACE('',#102367,0.127000001278142);
#90604=CYLINDRICAL_SURFACE('',#102370,0.127);
#90605=CYLINDRICAL_SURFACE('',#102376,0.126999993613654);
#90606=CYLINDRICAL_SURFACE('',#102378,0.127000005454222);
#90607=CYLINDRICAL_SURFACE('',#102384,0.127);
#90608=CYLINDRICAL_SURFACE('',#102387,0.126999998752798);
#90609=CYLINDRICAL_SURFACE('',#102389,0.126999993596256);
#90610=CYLINDRICAL_SURFACE('',#102393,0.127);
#90611=CYLINDRICAL_SURFACE('',#102395,0.127);
#90612=CYLINDRICAL_SURFACE('',#102398,0.127000000302042);
#90613=CYLINDRICAL_SURFACE('',#102399,0.126999999706423);
#90614=CYLINDRICAL_SURFACE('',#102403,0.127);
#90615=CYLINDRICAL_SURFACE('',#102405,0.127);
#90616=CYLINDRICAL_SURFACE('',#102409,0.127000005437262);
#90617=CYLINDRICAL_SURFACE('',#102411,0.127000001279889);
#90618=CYLINDRICAL_SURFACE('',#102414,0.127);
#90619=CYLINDRICAL_SURFACE('',#102420,0.126999993614019);
#90620=CYLINDRICAL_SURFACE('',#102422,0.127000005452903);
#90621=CYLINDRICAL_SURFACE('',#102428,0.126999999999999);
#90622=CYLINDRICAL_SURFACE('',#102431,0.126999998754081);
#90623=CYLINDRICAL_SURFACE('',#102433,0.126999993593342);
#90624=CYLINDRICAL_SURFACE('',#102437,0.126999999999999);
#90625=CYLINDRICAL_SURFACE('',#102439,0.126999999999999);
#90626=CYLINDRICAL_SURFACE('',#102442,0.127000000301453);
#90627=CYLINDRICAL_SURFACE('',#102443,0.12699999970728);
#90628=CYLINDRICAL_SURFACE('',#102447,0.127);
#90629=CYLINDRICAL_SURFACE('',#102449,0.127);
#90630=CYLINDRICAL_SURFACE('',#102453,0.12700000543635);
#90631=CYLINDRICAL_SURFACE('',#102455,0.127000001280708);
#90632=CYLINDRICAL_SURFACE('',#102458,0.127);
#90633=CYLINDRICAL_SURFACE('',#102464,0.126999993613472);
#90634=CYLINDRICAL_SURFACE('',#102466,0.127000005453988);
#90635=CYLINDRICAL_SURFACE('',#102472,0.127);
#90636=CYLINDRICAL_SURFACE('',#102475,0.12699999875345);
#90637=CYLINDRICAL_SURFACE('',#102477,0.126999993596425);
#90638=CYLINDRICAL_SURFACE('',#102481,0.127000000000001);
#90639=CYLINDRICAL_SURFACE('',#102483,0.127000000000001);
#90640=CYLINDRICAL_SURFACE('',#102486,0.127000000302115);
#90641=CYLINDRICAL_SURFACE('',#102487,0.126999999706815);
#90642=CYLINDRICAL_SURFACE('',#102491,0.127);
#90643=CYLINDRICAL_SURFACE('',#102493,0.127);
#90644=CYLINDRICAL_SURFACE('',#102497,0.127000005436472);
#90645=CYLINDRICAL_SURFACE('',#102499,0.127000001280011);
#90646=CYLINDRICAL_SURFACE('',#102502,0.127);
#90647=CYLINDRICAL_SURFACE('',#102508,0.126999993613169);
#90648=CYLINDRICAL_SURFACE('',#102510,0.127000005455449);
#90649=CYLINDRICAL_SURFACE('',#102516,0.127000000000001);
#90650=CYLINDRICAL_SURFACE('',#102519,0.126999998752879);
#90651=CYLINDRICAL_SURFACE('',#102521,0.126999993596861);
#90652=CYLINDRICAL_SURFACE('',#102525,0.127000000000001);
#90653=CYLINDRICAL_SURFACE('',#102527,0.127000000000001);
#90654=CYLINDRICAL_SURFACE('',#102530,0.127000000301642);
#90655=CYLINDRICAL_SURFACE('',#102531,0.126999999706798);
#90656=CYLINDRICAL_SURFACE('',#102535,0.127);
#90657=CYLINDRICAL_SURFACE('',#102537,0.127);
#90658=CYLINDRICAL_SURFACE('',#102541,0.127000005438588);
#90659=CYLINDRICAL_SURFACE('',#102543,0.127000001278904);
#90660=CYLINDRICAL_SURFACE('',#102546,0.127);
#90661=CYLINDRICAL_SURFACE('',#102552,0.126999993613602);
#90662=CYLINDRICAL_SURFACE('',#102554,0.127000005455578);
#90663=CYLINDRICAL_SURFACE('',#102560,0.127);
#90664=CYLINDRICAL_SURFACE('',#102563,0.126999998752696);
#90665=CYLINDRICAL_SURFACE('',#102565,0.126999993594751);
#90666=CYLINDRICAL_SURFACE('',#102569,0.127);
#90667=CYLINDRICAL_SURFACE('',#102571,0.127);
#90668=CYLINDRICAL_SURFACE('',#102574,0.127000000302741);
#90669=CYLINDRICAL_SURFACE('',#102575,0.126999999706774);
#90670=CYLINDRICAL_SURFACE('',#102579,0.127);
#90671=CYLINDRICAL_SURFACE('',#102581,0.127);
#90672=CYLINDRICAL_SURFACE('',#102585,0.127000005439607);
#90673=CYLINDRICAL_SURFACE('',#102587,0.127000001278421);
#90674=CYLINDRICAL_SURFACE('',#102590,0.127);
#90675=CYLINDRICAL_SURFACE('',#102596,0.126999993617745);
#90676=CYLINDRICAL_SURFACE('',#102598,0.127000005455381);
#90677=CYLINDRICAL_SURFACE('',#102604,0.127);
#90678=CYLINDRICAL_SURFACE('',#102607,0.126999998754997);
#90679=CYLINDRICAL_SURFACE('',#102609,0.126999993595255);
#90680=CYLINDRICAL_SURFACE('',#102613,0.127);
#90681=CYLINDRICAL_SURFACE('',#102615,0.127);
#90682=CYLINDRICAL_SURFACE('',#102618,0.127000000301444);
#90683=CYLINDRICAL_SURFACE('',#102619,0.126999999706383);
#90684=CYLINDRICAL_SURFACE('',#102623,0.127);
#90685=CYLINDRICAL_SURFACE('',#102625,0.127);
#90686=CYLINDRICAL_SURFACE('',#102629,0.127000005439654);
#90687=CYLINDRICAL_SURFACE('',#102631,0.12700000127798);
#90688=CYLINDRICAL_SURFACE('',#102634,0.127);
#90689=CYLINDRICAL_SURFACE('',#102640,0.126999993615447);
#90690=CYLINDRICAL_SURFACE('',#102642,0.127000005453466);
#90691=CYLINDRICAL_SURFACE('',#102648,0.127);
#90692=CYLINDRICAL_SURFACE('',#102651,0.126999998751995);
#90693=CYLINDRICAL_SURFACE('',#102653,0.12699999359383);
#90694=CYLINDRICAL_SURFACE('',#102657,0.127);
#90695=CYLINDRICAL_SURFACE('',#102659,0.127);
#90696=CYLINDRICAL_SURFACE('',#102662,0.127000000301414);
#90697=CYLINDRICAL_SURFACE('',#102663,0.12699999970812);
#90698=CYLINDRICAL_SURFACE('',#102667,0.127);
#90699=CYLINDRICAL_SURFACE('',#102669,0.127);
#90700=CYLINDRICAL_SURFACE('',#102673,0.127000005437224);
#90701=CYLINDRICAL_SURFACE('',#102675,0.127000001279242);
#90702=CYLINDRICAL_SURFACE('',#102678,0.127);
#90703=CYLINDRICAL_SURFACE('',#102684,0.126999993612789);
#90704=CYLINDRICAL_SURFACE('',#102686,0.127000005453465);
#90705=CYLINDRICAL_SURFACE('',#102692,0.127);
#90706=CYLINDRICAL_SURFACE('',#102695,0.126999998752582);
#90707=CYLINDRICAL_SURFACE('',#102697,0.126999993593896);
#90708=CYLINDRICAL_SURFACE('',#102701,0.127);
#90709=CYLINDRICAL_SURFACE('',#102703,0.127);
#90710=CYLINDRICAL_SURFACE('',#102706,0.127000000300403);
#90711=CYLINDRICAL_SURFACE('',#102707,0.126999999707339);
#90712=CYLINDRICAL_SURFACE('',#102711,0.127);
#90713=CYLINDRICAL_SURFACE('',#102713,0.127);
#90714=CYLINDRICAL_SURFACE('',#102717,0.12700000543759);
#90715=CYLINDRICAL_SURFACE('',#102719,0.127000001278668);
#90716=CYLINDRICAL_SURFACE('',#102722,0.127);
#90717=CYLINDRICAL_SURFACE('',#102728,0.126999993616971);
#90718=CYLINDRICAL_SURFACE('',#102730,0.127000005453324);
#90719=CYLINDRICAL_SURFACE('',#102736,0.127);
#90720=CYLINDRICAL_SURFACE('',#102739,0.126999998753525);
#90721=CYLINDRICAL_SURFACE('',#102741,0.12699999359536);
#90722=CYLINDRICAL_SURFACE('',#102745,0.127);
#90723=CYLINDRICAL_SURFACE('',#102747,0.127);
#90724=CYLINDRICAL_SURFACE('',#102750,0.127000000300871);
#90725=CYLINDRICAL_SURFACE('',#102751,0.126999999706726);
#90726=CYLINDRICAL_SURFACE('',#102755,0.127);
#90727=CYLINDRICAL_SURFACE('',#102757,0.127);
#90728=CYLINDRICAL_SURFACE('',#102761,0.127000005436566);
#90729=CYLINDRICAL_SURFACE('',#102763,0.127000001279669);
#90730=CYLINDRICAL_SURFACE('',#102766,0.127);
#90731=CYLINDRICAL_SURFACE('',#102772,0.126999993612996);
#90732=CYLINDRICAL_SURFACE('',#102774,0.127000005451943);
#90733=CYLINDRICAL_SURFACE('',#102780,0.127);
#90734=CYLINDRICAL_SURFACE('',#102783,0.126999998753668);
#90735=CYLINDRICAL_SURFACE('',#102785,0.126999993597716);
#90736=CYLINDRICAL_SURFACE('',#102789,0.127);
#90737=CYLINDRICAL_SURFACE('',#102791,0.127);
#90738=CYLINDRICAL_SURFACE('',#102794,0.12700000030196);
#90739=CYLINDRICAL_SURFACE('',#102795,0.126999999706616);
#90740=CYLINDRICAL_SURFACE('',#102799,0.127);
#90741=CYLINDRICAL_SURFACE('',#102801,0.127);
#90742=CYLINDRICAL_SURFACE('',#102805,0.127000005440328);
#90743=CYLINDRICAL_SURFACE('',#102807,0.127000001279997);
#90744=CYLINDRICAL_SURFACE('',#102810,0.127);
#90745=CYLINDRICAL_SURFACE('',#102816,0.126999993614862);
#90746=CYLINDRICAL_SURFACE('',#102818,0.127000005453936);
#90747=CYLINDRICAL_SURFACE('',#102824,0.126999999999999);
#90748=CYLINDRICAL_SURFACE('',#102827,0.126999998752473);
#90749=CYLINDRICAL_SURFACE('',#102829,0.126999993593647);
#90750=CYLINDRICAL_SURFACE('',#102833,0.126999999999999);
#90751=CYLINDRICAL_SURFACE('',#102835,0.126999999999999);
#90752=CYLINDRICAL_SURFACE('',#102838,0.127000000302768);
#90753=CYLINDRICAL_SURFACE('',#102839,0.126999999706514);
#90754=CYLINDRICAL_SURFACE('',#102843,0.127);
#90755=CYLINDRICAL_SURFACE('',#102845,0.127);
#90756=CYLINDRICAL_SURFACE('',#102849,0.127000005434962);
#90757=CYLINDRICAL_SURFACE('',#102851,0.127000001278088);
#90758=CYLINDRICAL_SURFACE('',#102854,0.127);
#90759=CYLINDRICAL_SURFACE('',#102860,0.126999993617541);
#90760=CYLINDRICAL_SURFACE('',#102862,0.127000005452558);
#90761=CYLINDRICAL_SURFACE('',#102868,0.127000000000001);
#90762=CYLINDRICAL_SURFACE('',#102871,0.12699999875113);
#90763=CYLINDRICAL_SURFACE('',#102873,0.126999993594463);
#90764=CYLINDRICAL_SURFACE('',#102877,0.127000000000001);
#90765=CYLINDRICAL_SURFACE('',#102879,0.127000000000001);
#90766=CYLINDRICAL_SURFACE('',#102882,0.127000000300141);
#90767=CYLINDRICAL_SURFACE('',#102883,0.12699999970714);
#90768=CYLINDRICAL_SURFACE('',#102887,0.127);
#90769=CYLINDRICAL_SURFACE('',#102889,0.127);
#90770=CYLINDRICAL_SURFACE('',#102893,0.127000005439957);
#90771=CYLINDRICAL_SURFACE('',#102895,0.12700000127911);
#90772=CYLINDRICAL_SURFACE('',#102898,0.127);
#90773=CYLINDRICAL_SURFACE('',#102904,0.126999993615602);
#90774=CYLINDRICAL_SURFACE('',#102906,0.127000005454291);
#90775=CYLINDRICAL_SURFACE('',#102912,0.127);
#90776=CYLINDRICAL_SURFACE('',#102915,0.126999998753839);
#90777=CYLINDRICAL_SURFACE('',#102917,0.126999993595304);
#90778=CYLINDRICAL_SURFACE('',#102921,0.127);
#90779=CYLINDRICAL_SURFACE('',#102923,0.127);
#90780=CYLINDRICAL_SURFACE('',#102926,0.127000000301699);
#90781=CYLINDRICAL_SURFACE('',#102927,0.126999999705295);
#90782=CYLINDRICAL_SURFACE('',#102931,0.127);
#90783=CYLINDRICAL_SURFACE('',#102933,0.127);
#90784=CYLINDRICAL_SURFACE('',#102937,0.127000005439621);
#90785=CYLINDRICAL_SURFACE('',#102939,0.127000001279142);
#90786=CYLINDRICAL_SURFACE('',#102942,0.127);
#90787=CYLINDRICAL_SURFACE('',#102948,0.126999993614056);
#90788=CYLINDRICAL_SURFACE('',#102950,0.127000005452498);
#90789=CYLINDRICAL_SURFACE('',#102956,0.127000000000001);
#90790=CYLINDRICAL_SURFACE('',#102959,0.126999998753414);
#90791=CYLINDRICAL_SURFACE('',#102961,0.1269999935946);
#90792=CYLINDRICAL_SURFACE('',#102965,0.127000000000001);
#90793=CYLINDRICAL_SURFACE('',#102967,0.127000000000001);
#90794=CYLINDRICAL_SURFACE('',#102970,0.127000000300451);
#90795=CYLINDRICAL_SURFACE('',#102971,0.126999999707799);
#90796=CYLINDRICAL_SURFACE('',#102975,0.127);
#90797=CYLINDRICAL_SURFACE('',#102977,0.127);
#90798=CYLINDRICAL_SURFACE('',#102981,0.127000005436198);
#90799=CYLINDRICAL_SURFACE('',#102983,0.127000001278508);
#90800=CYLINDRICAL_SURFACE('',#102986,0.127);
#90801=CYLINDRICAL_SURFACE('',#102992,0.126999993613461);
#90802=CYLINDRICAL_SURFACE('',#102994,0.127000005454311);
#90803=CYLINDRICAL_SURFACE('',#103000,0.127);
#90804=CYLINDRICAL_SURFACE('',#103003,0.126999998752435);
#90805=CYLINDRICAL_SURFACE('',#103005,0.126999993594948);
#90806=CYLINDRICAL_SURFACE('',#103009,0.127);
#90807=CYLINDRICAL_SURFACE('',#103011,0.127);
#90808=CYLINDRICAL_SURFACE('',#103014,0.127000000300104);
#90809=CYLINDRICAL_SURFACE('',#103015,0.1269999997076);
#90810=CYLINDRICAL_SURFACE('',#103019,0.127);
#90811=CYLINDRICAL_SURFACE('',#103021,0.127);
#90812=CYLINDRICAL_SURFACE('',#103025,0.127000005437536);
#90813=CYLINDRICAL_SURFACE('',#103027,0.127000001280254);
#90814=CYLINDRICAL_SURFACE('',#103030,0.127);
#90815=CYLINDRICAL_SURFACE('',#103036,0.126999993616732);
#90816=CYLINDRICAL_SURFACE('',#103038,0.127000005453867);
#90817=CYLINDRICAL_SURFACE('',#103044,0.127);
#90818=CYLINDRICAL_SURFACE('',#103047,0.12699999875391);
#90819=CYLINDRICAL_SURFACE('',#103049,0.126999993592352);
#90820=CYLINDRICAL_SURFACE('',#103053,0.127);
#90821=CYLINDRICAL_SURFACE('',#103055,0.127);
#90822=CYLINDRICAL_SURFACE('',#103058,0.127000000301673);
#90823=CYLINDRICAL_SURFACE('',#103059,0.12699999970761);
#90824=CYLINDRICAL_SURFACE('',#103063,0.127);
#90825=CYLINDRICAL_SURFACE('',#103065,0.127);
#90826=CYLINDRICAL_SURFACE('',#103069,0.127000005437743);
#90827=CYLINDRICAL_SURFACE('',#103071,0.127000001277194);
#90828=CYLINDRICAL_SURFACE('',#103074,0.127);
#90829=CYLINDRICAL_SURFACE('',#103080,0.126999993615799);
#90830=CYLINDRICAL_SURFACE('',#103082,0.127000005454222);
#90831=CYLINDRICAL_SURFACE('',#103088,0.127000000000001);
#90832=CYLINDRICAL_SURFACE('',#103091,0.126999998753413);
#90833=CYLINDRICAL_SURFACE('',#103093,0.126999993594634);
#90834=CYLINDRICAL_SURFACE('',#103097,0.127000000000001);
#90835=CYLINDRICAL_SURFACE('',#103099,0.127000000000001);
#90836=CYLINDRICAL_SURFACE('',#103102,0.127000000300308);
#90837=CYLINDRICAL_SURFACE('',#103103,0.126999999707545);
#90838=CYLINDRICAL_SURFACE('',#103107,0.127);
#90839=CYLINDRICAL_SURFACE('',#103109,0.127);
#90840=CYLINDRICAL_SURFACE('',#103113,0.127000005434043);
#90841=CYLINDRICAL_SURFACE('',#103115,0.127000001279328);
#90842=CYLINDRICAL_SURFACE('',#103118,0.127);
#90843=CYLINDRICAL_SURFACE('',#103124,0.126999993613876);
#90844=CYLINDRICAL_SURFACE('',#103126,0.127000005452976);
#90845=CYLINDRICAL_SURFACE('',#103132,0.127);
#90846=CYLINDRICAL_SURFACE('',#103135,0.126999998753321);
#90847=CYLINDRICAL_SURFACE('',#103137,0.126999993597018);
#90848=CYLINDRICAL_SURFACE('',#103141,0.127);
#90849=CYLINDRICAL_SURFACE('',#103143,0.127);
#90850=CYLINDRICAL_SURFACE('',#103146,0.127000000301608);
#90851=CYLINDRICAL_SURFACE('',#103147,0.126999999705367);
#90852=CYLINDRICAL_SURFACE('',#103151,0.127);
#90853=CYLINDRICAL_SURFACE('',#103153,0.127);
#90854=CYLINDRICAL_SURFACE('',#103157,0.127000005439731);
#90855=CYLINDRICAL_SURFACE('',#103159,0.127000001277541);
#90856=CYLINDRICAL_SURFACE('',#103162,0.127);
#90857=CYLINDRICAL_SURFACE('',#103168,0.126999993617131);
#90858=CYLINDRICAL_SURFACE('',#103170,0.127000005454814);
#90859=CYLINDRICAL_SURFACE('',#103176,0.127000000000001);
#90860=CYLINDRICAL_SURFACE('',#103179,0.126999998753577);
#90861=CYLINDRICAL_SURFACE('',#103181,0.126999993598197);
#90862=CYLINDRICAL_SURFACE('',#103185,0.127000000000001);
#90863=CYLINDRICAL_SURFACE('',#103187,0.127000000000001);
#90864=CYLINDRICAL_SURFACE('',#103190,0.127000000301002);
#90865=CYLINDRICAL_SURFACE('',#103191,0.12699999970699);
#90866=CYLINDRICAL_SURFACE('',#103195,0.127);
#90867=CYLINDRICAL_SURFACE('',#103197,0.127);
#90868=CYLINDRICAL_SURFACE('',#103201,0.127000005438292);
#90869=CYLINDRICAL_SURFACE('',#103203,0.127000001278948);
#90870=CYLINDRICAL_SURFACE('',#103206,0.127);
#90871=CYLINDRICAL_SURFACE('',#103212,0.126999993613223);
#90872=CYLINDRICAL_SURFACE('',#103214,0.127000005454579);
#90873=CYLINDRICAL_SURFACE('',#103220,0.127000000000002);
#90874=CYLINDRICAL_SURFACE('',#103223,0.126999998753176);
#90875=CYLINDRICAL_SURFACE('',#103225,0.126999993594714);
#90876=CYLINDRICAL_SURFACE('',#103229,0.127000000000002);
#90877=CYLINDRICAL_SURFACE('',#103231,0.127000000000002);
#90878=CYLINDRICAL_SURFACE('',#103234,0.127000000302915);
#90879=CYLINDRICAL_SURFACE('',#103235,0.126999999706383);
#90880=CYLINDRICAL_SURFACE('',#103239,0.127);
#90881=CYLINDRICAL_SURFACE('',#103241,0.127);
#90882=CYLINDRICAL_SURFACE('',#103245,0.127000005440828);
#90883=CYLINDRICAL_SURFACE('',#103247,0.12700000127864);
#90884=CYLINDRICAL_SURFACE('',#103250,0.127);
#90885=CYLINDRICAL_SURFACE('',#103256,0.126999993616967);
#90886=CYLINDRICAL_SURFACE('',#103258,0.127000005453503);
#90887=CYLINDRICAL_SURFACE('',#103264,0.126999999999999);
#90888=CYLINDRICAL_SURFACE('',#103267,0.126999998754026);
#90889=CYLINDRICAL_SURFACE('',#103269,0.126999993593209);
#90890=CYLINDRICAL_SURFACE('',#103273,0.126999999999999);
#90891=CYLINDRICAL_SURFACE('',#103275,0.126999999999999);
#90892=CYLINDRICAL_SURFACE('',#103278,0.127000000300874);
#90893=CYLINDRICAL_SURFACE('',#103279,0.126999999706456);
#90894=CYLINDRICAL_SURFACE('',#103283,0.127);
#90895=CYLINDRICAL_SURFACE('',#103285,0.127);
#90896=CYLINDRICAL_SURFACE('',#103289,0.127000005438321);
#90897=CYLINDRICAL_SURFACE('',#103291,0.127000001279013);
#90898=CYLINDRICAL_SURFACE('',#103294,0.127);
#90899=CYLINDRICAL_SURFACE('',#103300,0.126999993615933);
#90900=CYLINDRICAL_SURFACE('',#103302,0.127000005453603);
#90901=CYLINDRICAL_SURFACE('',#103308,0.126999999999999);
#90902=CYLINDRICAL_SURFACE('',#103311,0.126999998752138);
#90903=CYLINDRICAL_SURFACE('',#103313,0.126999993597807);
#90904=CYLINDRICAL_SURFACE('',#103317,0.126999999999999);
#90905=CYLINDRICAL_SURFACE('',#103319,0.126999999999999);
#90906=CYLINDRICAL_SURFACE('',#103322,0.127000000301534);
#90907=CYLINDRICAL_SURFACE('',#103323,0.126999999705897);
#90908=CYLINDRICAL_SURFACE('',#103327,0.127000000000002);
#90909=CYLINDRICAL_SURFACE('',#103329,0.127000000000002);
#90910=CYLINDRICAL_SURFACE('',#103333,0.127000005437536);
#90911=CYLINDRICAL_SURFACE('',#103335,0.127000001278742);
#90912=CYLINDRICAL_SURFACE('',#103337,0.127000000000002);
#90913=CYLINDRICAL_SURFACE('',#103341,0.126999993615157);
#90914=CYLINDRICAL_SURFACE('',#103343,0.127000005454198);
#90915=CYLINDRICAL_SURFACE('',#103346,0.127000000000002);
#90916=CYLINDRICAL_SURFACE('',#103349,0.126999998753399);
#90917=CYLINDRICAL_SURFACE('',#103351,0.126999993594869);
#90918=CYLINDRICAL_SURFACE('',#103355,0.127000000000002);
#90919=CYLINDRICAL_SURFACE('',#103357,0.127000000000002);
#90920=CYLINDRICAL_SURFACE('',#103360,0.12700000030155);
#90921=CYLINDRICAL_SURFACE('',#103361,0.126999999707605);
#90922=CYLINDRICAL_SURFACE('',#103365,0.127);
#90923=CYLINDRICAL_SURFACE('',#103367,0.127);
#90924=CYLINDRICAL_SURFACE('',#103371,0.127000005437624);
#90925=CYLINDRICAL_SURFACE('',#103373,0.127000001279377);
#90926=CYLINDRICAL_SURFACE('',#103376,0.127);
#90927=CYLINDRICAL_SURFACE('',#103382,0.12699999361462);
#90928=CYLINDRICAL_SURFACE('',#103384,0.127000005452932);
#90929=CYLINDRICAL_SURFACE('',#103390,0.127);
#90930=CYLINDRICAL_SURFACE('',#103393,0.12699999875397);
#90931=CYLINDRICAL_SURFACE('',#103395,0.1269999935932);
#90932=CYLINDRICAL_SURFACE('',#103399,0.127);
#90933=CYLINDRICAL_SURFACE('',#103401,0.127);
#90934=CYLINDRICAL_SURFACE('',#103404,0.127000000302331);
#90935=CYLINDRICAL_SURFACE('',#103405,0.126999999708275);
#90936=CYLINDRICAL_SURFACE('',#103409,0.127);
#90937=CYLINDRICAL_SURFACE('',#103411,0.127);
#90938=CYLINDRICAL_SURFACE('',#103415,0.127000005437317);
#90939=CYLINDRICAL_SURFACE('',#103417,0.127000001278536);
#90940=CYLINDRICAL_SURFACE('',#103420,0.127);
#90941=CYLINDRICAL_SURFACE('',#103426,0.12699999361381);
#90942=CYLINDRICAL_SURFACE('',#103428,0.127000005454359);
#90943=CYLINDRICAL_SURFACE('',#103434,0.126999999999999);
#90944=CYLINDRICAL_SURFACE('',#103437,0.126999998753825);
#90945=CYLINDRICAL_SURFACE('',#103439,0.126999993596437);
#90946=CYLINDRICAL_SURFACE('',#103443,0.126999999999999);
#90947=CYLINDRICAL_SURFACE('',#103445,0.126999999999999);
#90948=CYLINDRICAL_SURFACE('',#103448,0.12700000030131);
#90949=CYLINDRICAL_SURFACE('',#103449,0.126999999705017);
#90950=CYLINDRICAL_SURFACE('',#103453,0.127);
#90951=CYLINDRICAL_SURFACE('',#103455,0.127);
#90952=CYLINDRICAL_SURFACE('',#103459,0.127000005437735);
#90953=CYLINDRICAL_SURFACE('',#103461,0.127000001278806);
#90954=CYLINDRICAL_SURFACE('',#103464,0.127);
#90955=CYLINDRICAL_SURFACE('',#103470,0.126999993614013);
#90956=CYLINDRICAL_SURFACE('',#103472,0.127000005453686);
#90957=CYLINDRICAL_SURFACE('',#103478,0.127000000000002);
#90958=CYLINDRICAL_SURFACE('',#103481,0.126999998752789);
#90959=CYLINDRICAL_SURFACE('',#103483,0.126999993596079);
#90960=CYLINDRICAL_SURFACE('',#103487,0.127000000000002);
#90961=CYLINDRICAL_SURFACE('',#103489,0.127000000000002);
#90962=CYLINDRICAL_SURFACE('',#103492,0.127000000301439);
#90963=CYLINDRICAL_SURFACE('',#103493,0.126999999704935);
#90964=CYLINDRICAL_SURFACE('',#103497,0.127);
#90965=CYLINDRICAL_SURFACE('',#103499,0.127);
#90966=CYLINDRICAL_SURFACE('',#103503,0.127000005439358);
#90967=CYLINDRICAL_SURFACE('',#103505,0.127000001277789);
#90968=CYLINDRICAL_SURFACE('',#103508,0.127);
#90969=CYLINDRICAL_SURFACE('',#103514,0.126999993617532);
#90970=CYLINDRICAL_SURFACE('',#103516,0.127000005455948);
#90971=CYLINDRICAL_SURFACE('',#103522,0.127000000000001);
#90972=CYLINDRICAL_SURFACE('',#103525,0.126999998752883);
#90973=CYLINDRICAL_SURFACE('',#103527,0.126999993593983);
#90974=CYLINDRICAL_SURFACE('',#103531,0.127000000000001);
#90975=CYLINDRICAL_SURFACE('',#103533,0.127000000000001);
#90976=CYLINDRICAL_SURFACE('',#103536,0.127000000304323);
#90977=CYLINDRICAL_SURFACE('',#103537,0.12699999970756);
#90978=CYLINDRICAL_SURFACE('',#103541,0.127);
#90979=CYLINDRICAL_SURFACE('',#103543,0.127);
#90980=CYLINDRICAL_SURFACE('',#103547,0.127000005440239);
#90981=CYLINDRICAL_SURFACE('',#103549,0.127000001279599);
#90982=CYLINDRICAL_SURFACE('',#103552,0.127);
#90983=CYLINDRICAL_SURFACE('',#103558,0.126999993612611);
#90984=CYLINDRICAL_SURFACE('',#103560,0.127000005457026);
#90985=CYLINDRICAL_SURFACE('',#103566,0.127);
#90986=CYLINDRICAL_SURFACE('',#103569,0.12699999875316);
#90987=CYLINDRICAL_SURFACE('',#103571,0.126999993596404);
#90988=CYLINDRICAL_SURFACE('',#103575,0.127);
#90989=CYLINDRICAL_SURFACE('',#103577,0.127);
#90990=CYLINDRICAL_SURFACE('',#103580,0.127000000301405);
#90991=CYLINDRICAL_SURFACE('',#103581,0.126999999707666);
#90992=CYLINDRICAL_SURFACE('',#103585,0.127);
#90993=CYLINDRICAL_SURFACE('',#103587,0.127);
#90994=CYLINDRICAL_SURFACE('',#103591,0.127000005438194);
#90995=CYLINDRICAL_SURFACE('',#103593,0.127000001279677);
#90996=CYLINDRICAL_SURFACE('',#103596,0.127);
#90997=CYLINDRICAL_SURFACE('',#103602,0.12699999361647);
#90998=CYLINDRICAL_SURFACE('',#103604,0.127000005453912);
#90999=CYLINDRICAL_SURFACE('',#103610,0.127000000000001);
#91000=CYLINDRICAL_SURFACE('',#103613,0.126999998753327);
#91001=CYLINDRICAL_SURFACE('',#103615,0.12699999359527);
#91002=CYLINDRICAL_SURFACE('',#103619,0.127000000000001);
#91003=CYLINDRICAL_SURFACE('',#103621,0.127000000000001);
#91004=CYLINDRICAL_SURFACE('',#103624,0.127000000299871);
#91005=CYLINDRICAL_SURFACE('',#103625,0.126999999705577);
#91006=CYLINDRICAL_SURFACE('',#103629,0.127);
#91007=CYLINDRICAL_SURFACE('',#103631,0.127);
#91008=CYLINDRICAL_SURFACE('',#103635,0.127000005435759);
#91009=CYLINDRICAL_SURFACE('',#103637,0.12700000127797);
#91010=CYLINDRICAL_SURFACE('',#103640,0.127);
#91011=CYLINDRICAL_SURFACE('',#103646,0.126999993612283);
#91012=CYLINDRICAL_SURFACE('',#103648,0.127000005450208);
#91013=CYLINDRICAL_SURFACE('',#103654,0.126999999999998);
#91014=CYLINDRICAL_SURFACE('',#103657,0.126999998752389);
#91015=CYLINDRICAL_SURFACE('',#103659,0.126999993595374);
#91016=CYLINDRICAL_SURFACE('',#103663,0.126999999999998);
#91017=CYLINDRICAL_SURFACE('',#103665,0.126999999999998);
#91018=CYLINDRICAL_SURFACE('',#103668,0.127000000300949);
#91019=CYLINDRICAL_SURFACE('',#103669,0.126999999707429);
#91020=CYLINDRICAL_SURFACE('',#103673,0.127);
#91021=CYLINDRICAL_SURFACE('',#103675,0.127);
#91022=CYLINDRICAL_SURFACE('',#103679,0.127000005435469);
#91023=CYLINDRICAL_SURFACE('',#103681,0.127000001280724);
#91024=CYLINDRICAL_SURFACE('',#103684,0.127);
#91025=CYLINDRICAL_SURFACE('',#103690,0.126999993616767);
#91026=CYLINDRICAL_SURFACE('',#103692,0.127000005452434);
#91027=CYLINDRICAL_SURFACE('',#103698,0.127);
#91028=CYLINDRICAL_SURFACE('',#103701,0.12699999875229);
#91029=CYLINDRICAL_SURFACE('',#103703,0.126999993596947);
#91030=CYLINDRICAL_SURFACE('',#103707,0.127);
#91031=CYLINDRICAL_SURFACE('',#103709,0.127);
#91032=CYLINDRICAL_SURFACE('',#103712,0.127000000301637);
#91033=CYLINDRICAL_SURFACE('',#103713,0.126999999707563);
#91034=CYLINDRICAL_SURFACE('',#103717,0.127);
#91035=CYLINDRICAL_SURFACE('',#103719,0.127);
#91036=CYLINDRICAL_SURFACE('',#103723,0.12700000543493);
#91037=CYLINDRICAL_SURFACE('',#103725,0.12700000127735);
#91038=CYLINDRICAL_SURFACE('',#103728,0.127);
#91039=CYLINDRICAL_SURFACE('',#103734,0.126999993615612);
#91040=CYLINDRICAL_SURFACE('',#103736,0.127000005453414);
#91041=CYLINDRICAL_SURFACE('',#103742,0.126999999999999);
#91042=CYLINDRICAL_SURFACE('',#103745,0.126999998752984);
#91043=CYLINDRICAL_SURFACE('',#103747,0.126999993593435);
#91044=CYLINDRICAL_SURFACE('',#103751,0.126999999999999);
#91045=CYLINDRICAL_SURFACE('',#103753,0.126999999999999);
#91046=CYLINDRICAL_SURFACE('',#103756,0.127000000301768);
#91047=CYLINDRICAL_SURFACE('',#103757,0.126999999706787);
#91048=CYLINDRICAL_SURFACE('',#103761,0.127);
#91049=CYLINDRICAL_SURFACE('',#103763,0.127);
#91050=CYLINDRICAL_SURFACE('',#103767,0.127000005433587);
#91051=CYLINDRICAL_SURFACE('',#103769,0.127000001278825);
#91052=CYLINDRICAL_SURFACE('',#103772,0.127);
#91053=CYLINDRICAL_SURFACE('',#103778,0.126999993613855);
#91054=CYLINDRICAL_SURFACE('',#103780,0.127000005455278);
#91055=CYLINDRICAL_SURFACE('',#103786,0.126999999999999);
#91056=CYLINDRICAL_SURFACE('',#103789,0.126999998754249);
#91057=CYLINDRICAL_SURFACE('',#103791,0.12699999359443);
#91058=CYLINDRICAL_SURFACE('',#103795,0.126999999999999);
#91059=CYLINDRICAL_SURFACE('',#103797,0.126999999999999);
#91060=CYLINDRICAL_SURFACE('',#103800,0.127000000301345);
#91061=CYLINDRICAL_SURFACE('',#103801,0.126999999707803);
#91062=CYLINDRICAL_SURFACE('',#103805,0.127);
#91063=CYLINDRICAL_SURFACE('',#103807,0.127);
#91064=CYLINDRICAL_SURFACE('',#103811,0.12700000543712);
#91065=CYLINDRICAL_SURFACE('',#103813,0.127000001279907);
#91066=CYLINDRICAL_SURFACE('',#103816,0.127);
#91067=CYLINDRICAL_SURFACE('',#103822,0.126999993614048);
#91068=CYLINDRICAL_SURFACE('',#103824,0.127000005454575);
#91069=CYLINDRICAL_SURFACE('',#103830,0.127);
#91070=CYLINDRICAL_SURFACE('',#103833,0.126999998752347);
#91071=CYLINDRICAL_SURFACE('',#103835,0.126999993597714);
#91072=CYLINDRICAL_SURFACE('',#103839,0.127);
#91073=CYLINDRICAL_SURFACE('',#103841,0.127);
#91074=CYLINDRICAL_SURFACE('',#103844,0.127000000301343);
#91075=CYLINDRICAL_SURFACE('',#103845,0.126999999707272);
#91076=CYLINDRICAL_SURFACE('',#103849,0.127);
#91077=CYLINDRICAL_SURFACE('',#103851,0.127);
#91078=CYLINDRICAL_SURFACE('',#103855,0.127000005433796);
#91079=CYLINDRICAL_SURFACE('',#103857,0.127000001278195);
#91080=CYLINDRICAL_SURFACE('',#103860,0.127);
#91081=CYLINDRICAL_SURFACE('',#103866,0.126999993613666);
#91082=CYLINDRICAL_SURFACE('',#103868,0.127000005453606);
#91083=CYLINDRICAL_SURFACE('',#103874,0.127);
#91084=CYLINDRICAL_SURFACE('',#103877,0.126999998755233);
#91085=CYLINDRICAL_SURFACE('',#103879,0.126999993596122);
#91086=CYLINDRICAL_SURFACE('',#103883,0.127);
#91087=CYLINDRICAL_SURFACE('',#103885,0.127);
#91088=CYLINDRICAL_SURFACE('',#103888,0.127000000301413);
#91089=CYLINDRICAL_SURFACE('',#103889,0.126999999707218);
#91090=CYLINDRICAL_SURFACE('',#103893,0.127);
#91091=CYLINDRICAL_SURFACE('',#103895,0.127);
#91092=CYLINDRICAL_SURFACE('',#103899,0.127000005439452);
#91093=CYLINDRICAL_SURFACE('',#103901,0.12700000127914);
#91094=CYLINDRICAL_SURFACE('',#103904,0.127);
#91095=CYLINDRICAL_SURFACE('',#103910,0.126999993615814);
#91096=CYLINDRICAL_SURFACE('',#103912,0.127000005453094);
#91097=CYLINDRICAL_SURFACE('',#103918,0.127);
#91098=CYLINDRICAL_SURFACE('',#103921,0.126999998753958);
#91099=CYLINDRICAL_SURFACE('',#103923,0.12699999359588);
#91100=CYLINDRICAL_SURFACE('',#103927,0.127);
#91101=CYLINDRICAL_SURFACE('',#103929,0.127);
#91102=CYLINDRICAL_SURFACE('',#103932,0.127000000300461);
#91103=CYLINDRICAL_SURFACE('',#103933,0.126999999706217);
#91104=CYLINDRICAL_SURFACE('',#103937,0.127);
#91105=CYLINDRICAL_SURFACE('',#103939,0.127);
#91106=CYLINDRICAL_SURFACE('',#103943,0.127000005437066);
#91107=CYLINDRICAL_SURFACE('',#103945,0.127000001279617);
#91108=CYLINDRICAL_SURFACE('',#103948,0.127);
#91109=CYLINDRICAL_SURFACE('',#103954,0.126999993615203);
#91110=CYLINDRICAL_SURFACE('',#103956,0.127000005454548);
#91111=CYLINDRICAL_SURFACE('',#103962,0.127);
#91112=CYLINDRICAL_SURFACE('',#103965,0.126999998753434);
#91113=CYLINDRICAL_SURFACE('',#103967,0.126999993595871);
#91114=CYLINDRICAL_SURFACE('',#103971,0.127);
#91115=CYLINDRICAL_SURFACE('',#103973,0.127);
#91116=CYLINDRICAL_SURFACE('',#103976,0.127000000301136);
#91117=CYLINDRICAL_SURFACE('',#103977,0.126999999708071);
#91118=CYLINDRICAL_SURFACE('',#103981,0.127);
#91119=CYLINDRICAL_SURFACE('',#103983,0.127);
#91120=CYLINDRICAL_SURFACE('',#103987,0.1270000054394);
#91121=CYLINDRICAL_SURFACE('',#103989,0.127000001278787);
#91122=CYLINDRICAL_SURFACE('',#103991,0.127);
#91123=CYLINDRICAL_SURFACE('',#103995,0.126999993612156);
#91124=CYLINDRICAL_SURFACE('',#103997,0.12700000545294);
#91125=CYLINDRICAL_SURFACE('',#104000,0.127);
#91126=CYLINDRICAL_SURFACE('',#104003,0.126999998752275);
#91127=CYLINDRICAL_SURFACE('',#104005,0.126999993594249);
#91128=CYLINDRICAL_SURFACE('',#104009,0.127);
#91129=CYLINDRICAL_SURFACE('',#104011,0.127);
#91130=CYLINDRICAL_SURFACE('',#104014,0.127000000300402);
#91131=CYLINDRICAL_SURFACE('',#104015,0.126999999707371);
#91132=CYLINDRICAL_SURFACE('',#104019,0.127);
#91133=CYLINDRICAL_SURFACE('',#104021,0.127);
#91134=CYLINDRICAL_SURFACE('',#104025,0.127000005437447);
#91135=CYLINDRICAL_SURFACE('',#104027,0.127000001277987);
#91136=CYLINDRICAL_SURFACE('',#104030,0.127);
#91137=CYLINDRICAL_SURFACE('',#104036,0.12699999361552);
#91138=CYLINDRICAL_SURFACE('',#104038,0.127000005453145);
#91139=CYLINDRICAL_SURFACE('',#104044,0.127);
#91140=CYLINDRICAL_SURFACE('',#104047,0.12699999875448);
#91141=CYLINDRICAL_SURFACE('',#104049,0.126999993595573);
#91142=CYLINDRICAL_SURFACE('',#104053,0.127);
#91143=CYLINDRICAL_SURFACE('',#104055,0.127);
#91144=CYLINDRICAL_SURFACE('',#104058,0.127000000300409);
#91145=CYLINDRICAL_SURFACE('',#104059,0.126999999706503);
#91146=CYLINDRICAL_SURFACE('',#104063,0.127);
#91147=CYLINDRICAL_SURFACE('',#104065,0.127);
#91148=CYLINDRICAL_SURFACE('',#104069,0.127000005438401);
#91149=CYLINDRICAL_SURFACE('',#104071,0.127000001278597);
#91150=CYLINDRICAL_SURFACE('',#104074,0.127);
#91151=CYLINDRICAL_SURFACE('',#104080,0.126999993616107);
#91152=CYLINDRICAL_SURFACE('',#104082,0.127000005453882);
#91153=CYLINDRICAL_SURFACE('',#104088,0.127);
#91154=CYLINDRICAL_SURFACE('',#104091,0.126999998753241);
#91155=CYLINDRICAL_SURFACE('',#104093,0.126999993597234);
#91156=CYLINDRICAL_SURFACE('',#104097,0.127);
#91157=CYLINDRICAL_SURFACE('',#104099,0.127);
#91158=CYLINDRICAL_SURFACE('',#104102,0.127000000301718);
#91159=CYLINDRICAL_SURFACE('',#104103,0.12699999970547);
#91160=CYLINDRICAL_SURFACE('',#104107,0.127);
#91161=CYLINDRICAL_SURFACE('',#104109,0.127);
#91162=CYLINDRICAL_SURFACE('',#104113,0.127000005436057);
#91163=CYLINDRICAL_SURFACE('',#104115,0.127000001278805);
#91164=CYLINDRICAL_SURFACE('',#104118,0.127);
#91165=CYLINDRICAL_SURFACE('',#104124,0.126999993612556);
#91166=CYLINDRICAL_SURFACE('',#104126,0.127000005453779);
#91167=CYLINDRICAL_SURFACE('',#104132,0.127);
#91168=CYLINDRICAL_SURFACE('',#104135,0.126999998751993);
#91169=CYLINDRICAL_SURFACE('',#104137,0.126999993594818);
#91170=CYLINDRICAL_SURFACE('',#104141,0.127);
#91171=CYLINDRICAL_SURFACE('',#104143,0.127);
#91172=CYLINDRICAL_SURFACE('',#104146,0.127000000301938);
#91173=CYLINDRICAL_SURFACE('',#104147,0.126999999706208);
#91174=CYLINDRICAL_SURFACE('',#104151,0.127);
#91175=CYLINDRICAL_SURFACE('',#104153,0.127);
#91176=CYLINDRICAL_SURFACE('',#104157,0.127000005437245);
#91177=CYLINDRICAL_SURFACE('',#104159,0.127000001279644);
#91178=CYLINDRICAL_SURFACE('',#104162,0.127);
#91179=CYLINDRICAL_SURFACE('',#104168,0.126999993611974);
#91180=CYLINDRICAL_SURFACE('',#104170,0.127000005449949);
#91181=CYLINDRICAL_SURFACE('',#104176,0.126999999999999);
#91182=CYLINDRICAL_SURFACE('',#104179,0.126999998751559);
#91183=CYLINDRICAL_SURFACE('',#104181,0.126999993594054);
#91184=CYLINDRICAL_SURFACE('',#104185,0.126999999999999);
#91185=CYLINDRICAL_SURFACE('',#104187,0.126999999999999);
#91186=CYLINDRICAL_SURFACE('',#104190,0.127000000300251);
#91187=CYLINDRICAL_SURFACE('',#104191,0.126999999705737);
#91188=CYLINDRICAL_SURFACE('',#104195,0.127);
#91189=CYLINDRICAL_SURFACE('',#104197,0.127);
#91190=CYLINDRICAL_SURFACE('',#104201,0.127000005438409);
#91191=CYLINDRICAL_SURFACE('',#104203,0.127000001278734);
#91192=CYLINDRICAL_SURFACE('',#104206,0.127);
#91193=CYLINDRICAL_SURFACE('',#104212,0.126999993613275);
#91194=CYLINDRICAL_SURFACE('',#104214,0.127000005453712);
#91195=CYLINDRICAL_SURFACE('',#104220,0.127);
#91196=CYLINDRICAL_SURFACE('',#104223,0.126999998753237);
#91197=CYLINDRICAL_SURFACE('',#104225,0.126999993593396);
#91198=CYLINDRICAL_SURFACE('',#104229,0.127);
#91199=CYLINDRICAL_SURFACE('',#104231,0.127);
#91200=CYLINDRICAL_SURFACE('',#104234,0.127000000301442);
#91201=CYLINDRICAL_SURFACE('',#104235,0.126999999706943);
#91202=CYLINDRICAL_SURFACE('',#104239,0.127);
#91203=CYLINDRICAL_SURFACE('',#104241,0.127);
#91204=CYLINDRICAL_SURFACE('',#104245,0.127000005438704);
#91205=CYLINDRICAL_SURFACE('',#104247,0.1270000012792);
#91206=CYLINDRICAL_SURFACE('',#104250,0.127);
#91207=CYLINDRICAL_SURFACE('',#104256,0.126999993618011);
#91208=CYLINDRICAL_SURFACE('',#104258,0.12700000545145);
#91209=CYLINDRICAL_SURFACE('',#104264,0.127000000000001);
#91210=CYLINDRICAL_SURFACE('',#104267,0.126999998753892);
#91211=CYLINDRICAL_SURFACE('',#104269,0.126999993593854);
#91212=CYLINDRICAL_SURFACE('',#104273,0.127000000000001);
#91213=CYLINDRICAL_SURFACE('',#104275,0.127000000000001);
#91214=CYLINDRICAL_SURFACE('',#104278,0.127000000300314);
#91215=CYLINDRICAL_SURFACE('',#104279,0.126999999707915);
#91216=CYLINDRICAL_SURFACE('',#104283,0.127);
#91217=CYLINDRICAL_SURFACE('',#104285,0.127);
#91218=CYLINDRICAL_SURFACE('',#104289,0.127000005436347);
#91219=CYLINDRICAL_SURFACE('',#104291,0.127000001279015);
#91220=CYLINDRICAL_SURFACE('',#104294,0.127);
#91221=CYLINDRICAL_SURFACE('',#104300,0.126999993613876);
#91222=CYLINDRICAL_SURFACE('',#104302,0.127000005455893);
#91223=CYLINDRICAL_SURFACE('',#104308,0.127);
#91224=CYLINDRICAL_SURFACE('',#104311,0.126999998752179);
#91225=CYLINDRICAL_SURFACE('',#104313,0.126999993595854);
#91226=CYLINDRICAL_SURFACE('',#104317,0.127);
#91227=CYLINDRICAL_SURFACE('',#104319,0.127);
#91228=CYLINDRICAL_SURFACE('',#104322,0.127000000300653);
#91229=CYLINDRICAL_SURFACE('',#104323,0.126999999706938);
#91230=CYLINDRICAL_SURFACE('',#104327,0.127);
#91231=CYLINDRICAL_SURFACE('',#104329,0.127);
#91232=CYLINDRICAL_SURFACE('',#104333,0.127000005436586);
#91233=CYLINDRICAL_SURFACE('',#104335,0.127000001280382);
#91234=CYLINDRICAL_SURFACE('',#104338,0.127);
#91235=CYLINDRICAL_SURFACE('',#104344,0.126999993617505);
#91236=CYLINDRICAL_SURFACE('',#104346,0.127000005453856);
#91237=CYLINDRICAL_SURFACE('',#104352,0.126999999999998);
#91238=CYLINDRICAL_SURFACE('',#104355,0.126999998753061);
#91239=CYLINDRICAL_SURFACE('',#104357,0.126999993592484);
#91240=CYLINDRICAL_SURFACE('',#104361,0.127);
#91241=CYLINDRICAL_SURFACE('',#104363,0.127);
#91242=CYLINDRICAL_SURFACE('',#104366,0.127000000301914);
#91243=CYLINDRICAL_SURFACE('',#104367,0.126999999708164);
#91244=CYLINDRICAL_SURFACE('',#104371,0.127);
#91245=CYLINDRICAL_SURFACE('',#104373,0.127);
#91246=CYLINDRICAL_SURFACE('',#104377,0.127000005436732);
#91247=CYLINDRICAL_SURFACE('',#104379,0.127000001278542);
#91248=CYLINDRICAL_SURFACE('',#104382,0.127);
#91249=CYLINDRICAL_SURFACE('',#104388,0.126999993613755);
#91250=CYLINDRICAL_SURFACE('',#104390,0.1270000054525);
#91251=CYLINDRICAL_SURFACE('',#104396,0.127000000000001);
#91252=CYLINDRICAL_SURFACE('',#104399,0.126999998753982);
#91253=CYLINDRICAL_SURFACE('',#104401,0.12699999359441);
#91254=CYLINDRICAL_SURFACE('',#104405,0.127000000000001);
#91255=CYLINDRICAL_SURFACE('',#104407,0.127000000000001);
#91256=CYLINDRICAL_SURFACE('',#104410,0.127000000300815);
#91257=CYLINDRICAL_SURFACE('',#104411,0.126999999707749);
#91258=CYLINDRICAL_SURFACE('',#104415,0.127);
#91259=CYLINDRICAL_SURFACE('',#104417,0.127);
#91260=CYLINDRICAL_SURFACE('',#104421,0.127000005437114);
#91261=CYLINDRICAL_SURFACE('',#104423,0.127000001278914);
#91262=CYLINDRICAL_SURFACE('',#104426,0.127);
#91263=CYLINDRICAL_SURFACE('',#104432,0.126999993615937);
#91264=CYLINDRICAL_SURFACE('',#104434,0.127000005456152);
#91265=CYLINDRICAL_SURFACE('',#104440,0.127000000000003);
#91266=CYLINDRICAL_SURFACE('',#104443,0.126999998752603);
#91267=CYLINDRICAL_SURFACE('',#104445,0.126999993596602);
#91268=CYLINDRICAL_SURFACE('',#104449,0.127000000000003);
#91269=CYLINDRICAL_SURFACE('',#104451,0.127000000000003);
#91270=CYLINDRICAL_SURFACE('',#104454,0.127000000301358);
#91271=CYLINDRICAL_SURFACE('',#104455,0.126999999706635);
#91272=CYLINDRICAL_SURFACE('',#104459,0.127);
#91273=CYLINDRICAL_SURFACE('',#104461,0.127);
#91274=CYLINDRICAL_SURFACE('',#104465,0.127000005440303);
#91275=CYLINDRICAL_SURFACE('',#104467,0.127000001277462);
#91276=CYLINDRICAL_SURFACE('',#104470,0.127);
#91277=CYLINDRICAL_SURFACE('',#104476,0.126999993614758);
#91278=CYLINDRICAL_SURFACE('',#104478,0.127000005453311);
#91279=CYLINDRICAL_SURFACE('',#104484,0.127000000000001);
#91280=CYLINDRICAL_SURFACE('',#104487,0.126999998753895);
#91281=CYLINDRICAL_SURFACE('',#104489,0.126999993594221);
#91282=CYLINDRICAL_SURFACE('',#104493,0.127000000000001);
#91283=CYLINDRICAL_SURFACE('',#104495,0.127000000000001);
#91284=CYLINDRICAL_SURFACE('',#104498,0.127000000302199);
#91285=CYLINDRICAL_SURFACE('',#104499,0.12699999970607);
#91286=CYLINDRICAL_SURFACE('',#104503,0.127);
#91287=CYLINDRICAL_SURFACE('',#104505,0.127);
#91288=CYLINDRICAL_SURFACE('',#104509,0.12700000543857);
#91289=CYLINDRICAL_SURFACE('',#104511,0.127000001278887);
#91290=CYLINDRICAL_SURFACE('',#104514,0.127);
#91291=CYLINDRICAL_SURFACE('',#104520,0.126999993614607);
#91292=CYLINDRICAL_SURFACE('',#104522,0.127000005454939);
#91293=CYLINDRICAL_SURFACE('',#104528,0.127);
#91294=CYLINDRICAL_SURFACE('',#104531,0.126999998753384);
#91295=CYLINDRICAL_SURFACE('',#104533,0.12699999359301);
#91296=CYLINDRICAL_SURFACE('',#104537,0.127);
#91297=CYLINDRICAL_SURFACE('',#104539,0.127);
#91298=CYLINDRICAL_SURFACE('',#104542,0.12700000030178);
#91299=CYLINDRICAL_SURFACE('',#104543,0.126999999706677);
#91300=CYLINDRICAL_SURFACE('',#104547,0.127);
#91301=CYLINDRICAL_SURFACE('',#104549,0.127);
#91302=CYLINDRICAL_SURFACE('',#104553,0.127000005438697);
#91303=CYLINDRICAL_SURFACE('',#104555,0.127000001277866);
#91304=CYLINDRICAL_SURFACE('',#104558,0.127);
#91305=CYLINDRICAL_SURFACE('',#104564,0.126999993613173);
#91306=CYLINDRICAL_SURFACE('',#104566,0.127000005452212);
#91307=CYLINDRICAL_SURFACE('',#104572,0.127000000000001);
#91308=CYLINDRICAL_SURFACE('',#104575,0.126999998752685);
#91309=CYLINDRICAL_SURFACE('',#104577,0.126999993595208);
#91310=CYLINDRICAL_SURFACE('',#104581,0.127000000000001);
#91311=CYLINDRICAL_SURFACE('',#104583,0.127000000000001);
#91312=CYLINDRICAL_SURFACE('',#104586,0.127000000300787);
#91313=CYLINDRICAL_SURFACE('',#104587,0.126999999705652);
#91314=CYLINDRICAL_SURFACE('',#104591,0.127);
#91315=CYLINDRICAL_SURFACE('',#104593,0.127);
#91316=CYLINDRICAL_SURFACE('',#104597,0.127000005437709);
#91317=CYLINDRICAL_SURFACE('',#104599,0.127000001279523);
#91318=CYLINDRICAL_SURFACE('',#104602,0.127);
#91319=CYLINDRICAL_SURFACE('',#104608,0.126999993615976);
#91320=CYLINDRICAL_SURFACE('',#104610,0.127000005453785);
#91321=CYLINDRICAL_SURFACE('',#104616,0.126999999999999);
#91322=CYLINDRICAL_SURFACE('',#104619,0.126999998753079);
#91323=CYLINDRICAL_SURFACE('',#104621,0.126999993596377);
#91324=CYLINDRICAL_SURFACE('',#104625,0.126999999999999);
#91325=CYLINDRICAL_SURFACE('',#104627,0.126999999999999);
#91326=CYLINDRICAL_SURFACE('',#104630,0.12700000030257);
#91327=CYLINDRICAL_SURFACE('',#104670,65.);
#91328=CYLINDRICAL_SURFACE('',#104916,56.875);
#91329=CYLINDRICAL_SURFACE('',#106674,0.17526);
#91330=CYLINDRICAL_SURFACE('',#106675,0.17526);
#91331=CYLINDRICAL_SURFACE('',#106676,0.126999999705986);
#91332=CYLINDRICAL_SURFACE('',#106680,0.127);
#91333=CYLINDRICAL_SURFACE('',#106682,0.127);
#91334=CYLINDRICAL_SURFACE('',#106686,0.127000005436524);
#91335=CYLINDRICAL_SURFACE('',#106688,0.127000001280155);
#91336=CYLINDRICAL_SURFACE('',#106691,0.127);
#91337=CYLINDRICAL_SURFACE('',#106697,0.126999993615336);
#91338=CYLINDRICAL_SURFACE('',#106699,0.127000005452344);
#91339=CYLINDRICAL_SURFACE('',#106705,0.127);
#91340=CYLINDRICAL_SURFACE('',#106708,0.126999998752966);
#91341=CYLINDRICAL_SURFACE('',#106710,0.126999993594016);
#91342=CYLINDRICAL_SURFACE('',#106714,0.127);
#91343=CYLINDRICAL_SURFACE('',#106716,0.127);
#91344=CYLINDRICAL_SURFACE('',#106719,0.127000000300436);
#91345=CYLINDRICAL_SURFACE('',#107483,0.175259999999999);
#91346=CYLINDRICAL_SURFACE('',#107484,0.17526);
#91347=CYLINDRICAL_SURFACE('',#107485,0.175259999999999);
#91348=CYLINDRICAL_SURFACE('',#107486,0.17526);
#91349=CYLINDRICAL_SURFACE('',#107487,0.175259999999999);
#91350=CYLINDRICAL_SURFACE('',#107488,0.17526);
#91351=CYLINDRICAL_SURFACE('',#107489,0.17526);
#91352=CYLINDRICAL_SURFACE('',#107490,0.17526);
#91353=CYLINDRICAL_SURFACE('',#107491,0.175259999999998);
#91354=CYLINDRICAL_SURFACE('',#107492,0.17526);
#91355=CYLINDRICAL_SURFACE('',#107493,0.17526);
#91356=CYLINDRICAL_SURFACE('',#107494,0.17526);
#91357=CYLINDRICAL_SURFACE('',#107495,0.175260000000001);
#91358=CYLINDRICAL_SURFACE('',#107496,0.17526);
#91359=CYLINDRICAL_SURFACE('',#107497,0.175260000000001);
#91360=CYLINDRICAL_SURFACE('',#107498,0.17526);
#91361=CYLINDRICAL_SURFACE('',#107499,0.17526);
#91362=CYLINDRICAL_SURFACE('',#107500,0.17526);
#91363=CYLINDRICAL_SURFACE('',#107501,0.175260000000001);
#91364=CYLINDRICAL_SURFACE('',#107502,0.17526);
#91365=CYLINDRICAL_SURFACE('',#107503,0.17526);
#91366=CYLINDRICAL_SURFACE('',#107504,0.17526);
#91367=CYLINDRICAL_SURFACE('',#107505,0.175259999999999);
#91368=CYLINDRICAL_SURFACE('',#107506,0.17526);
#91369=CYLINDRICAL_SURFACE('',#107507,0.175259999999999);
#91370=CYLINDRICAL_SURFACE('',#107508,0.17526);
#91371=CYLINDRICAL_SURFACE('',#107509,0.175259999999999);
#91372=CYLINDRICAL_SURFACE('',#107510,0.17526);
#91373=CYLINDRICAL_SURFACE('',#107511,0.17526);
#91374=CYLINDRICAL_SURFACE('',#107512,0.17526);
#91375=CYLINDRICAL_SURFACE('',#107513,0.175259999999999);
#91376=CYLINDRICAL_SURFACE('',#107514,0.17526);
#91377=CYLINDRICAL_SURFACE('',#107515,0.17526);
#91378=CYLINDRICAL_SURFACE('',#107516,0.17526);
#91379=CYLINDRICAL_SURFACE('',#107517,0.175259999999999);
#91380=CYLINDRICAL_SURFACE('',#107518,0.17526);
#91381=CYLINDRICAL_SURFACE('',#107519,0.17526);
#91382=CYLINDRICAL_SURFACE('',#107520,0.17526);
#91383=CYLINDRICAL_SURFACE('',#107521,0.175259999999998);
#91384=CYLINDRICAL_SURFACE('',#107522,0.17526);
#91385=CYLINDRICAL_SURFACE('',#107523,0.17526);
#91386=CYLINDRICAL_SURFACE('',#107524,0.17526);
#91387=CYLINDRICAL_SURFACE('',#107525,0.175260000000001);
#91388=CYLINDRICAL_SURFACE('',#107526,0.17526);
#91389=CYLINDRICAL_SURFACE('',#107527,0.175260000000001);
#91390=CYLINDRICAL_SURFACE('',#107528,0.17526);
#91391=CYLINDRICAL_SURFACE('',#107529,0.17526);
#91392=CYLINDRICAL_SURFACE('',#107530,0.17526);
#91393=CYLINDRICAL_SURFACE('',#107531,0.175260000000001);
#91394=CYLINDRICAL_SURFACE('',#107532,0.17526);
#91395=CYLINDRICAL_SURFACE('',#107533,0.175260000000003);
#91396=CYLINDRICAL_SURFACE('',#107534,0.17526);
#91397=CYLINDRICAL_SURFACE('',#107535,0.175259999999999);
#91398=CYLINDRICAL_SURFACE('',#107536,0.17526);
#91399=CYLINDRICAL_SURFACE('',#107537,0.175259999999999);
#91400=CYLINDRICAL_SURFACE('',#107538,0.17526);
#91401=CYLINDRICAL_SURFACE('',#107539,0.17526);
#91402=CYLINDRICAL_SURFACE('',#107540,0.17526);
#91403=CYLINDRICAL_SURFACE('',#107541,0.17526);
#91404=CYLINDRICAL_SURFACE('',#107542,0.17526);
#91405=CYLINDRICAL_SURFACE('',#107543,0.17526);
#91406=CYLINDRICAL_SURFACE('',#107544,0.17526);
#91407=CYLINDRICAL_SURFACE('',#107545,0.17526);
#91408=CYLINDRICAL_SURFACE('',#107546,0.17526);
#91409=CYLINDRICAL_SURFACE('',#107547,0.175259999999999);
#91410=CYLINDRICAL_SURFACE('',#107548,0.17526);
#91411=CYLINDRICAL_SURFACE('',#107549,0.17526);
#91412=CYLINDRICAL_SURFACE('',#107550,0.17526);
#91413=CYLINDRICAL_SURFACE('',#107551,0.175259999999998);
#91414=CYLINDRICAL_SURFACE('',#107552,0.17526);
#91415=CYLINDRICAL_SURFACE('',#107553,0.17526);
#91416=CYLINDRICAL_SURFACE('',#107554,0.17526);
#91417=CYLINDRICAL_SURFACE('',#107555,0.175259999999996);
#91418=CYLINDRICAL_SURFACE('',#107556,0.17526);
#91419=CYLINDRICAL_SURFACE('',#107557,0.175260000000001);
#91420=CYLINDRICAL_SURFACE('',#107558,0.17526);
#91421=CYLINDRICAL_SURFACE('',#107559,0.175259999999995);
#91422=CYLINDRICAL_SURFACE('',#107560,0.17526);
#91423=CYLINDRICAL_SURFACE('',#107561,0.175260000000001);
#91424=CYLINDRICAL_SURFACE('',#107562,0.17526);
#91425=CYLINDRICAL_SURFACE('',#107563,0.17526);
#91426=CYLINDRICAL_SURFACE('',#107564,0.17526);
#91427=CYLINDRICAL_SURFACE('',#107565,0.175259999999999);
#91428=CYLINDRICAL_SURFACE('',#107566,0.17526);
#91429=CYLINDRICAL_SURFACE('',#107567,0.175259999999999);
#91430=CYLINDRICAL_SURFACE('',#107568,0.17526);
#91431=CYLINDRICAL_SURFACE('',#107569,0.17526);
#91432=CYLINDRICAL_SURFACE('',#107570,0.17526);
#91433=CYLINDRICAL_SURFACE('',#107571,0.17526);
#91434=CYLINDRICAL_SURFACE('',#107572,0.17526);
#91435=CYLINDRICAL_SURFACE('',#107573,0.17526);
#91436=CYLINDRICAL_SURFACE('',#107574,0.17526);
#91437=CYLINDRICAL_SURFACE('',#107575,0.17526);
#91438=CYLINDRICAL_SURFACE('',#107576,0.17526);
#91439=CYLINDRICAL_SURFACE('',#107577,0.175259999999999);
#91440=CYLINDRICAL_SURFACE('',#107578,0.17526);
#91441=CYLINDRICAL_SURFACE('',#107579,0.17526);
#91442=CYLINDRICAL_SURFACE('',#107580,0.17526);
#91443=CYLINDRICAL_SURFACE('',#107581,0.175260000000001);
#91444=CYLINDRICAL_SURFACE('',#107582,0.17526);
#91445=CYLINDRICAL_SURFACE('',#107583,0.17526);
#91446=CYLINDRICAL_SURFACE('',#107584,0.17526);
#91447=CYLINDRICAL_SURFACE('',#107585,0.175259999999996);
#91448=CYLINDRICAL_SURFACE('',#107586,0.17526);
#91449=CYLINDRICAL_SURFACE('',#107587,0.175260000000001);
#91450=CYLINDRICAL_SURFACE('',#107588,0.17526);
#91451=CYLINDRICAL_SURFACE('',#107589,0.175260000000001);
#91452=CYLINDRICAL_SURFACE('',#107590,0.17526);
#91453=CYLINDRICAL_SURFACE('',#107591,0.175260000000001);
#91454=CYLINDRICAL_SURFACE('',#107592,0.17526);
#91455=CYLINDRICAL_SURFACE('',#107593,0.17526);
#91456=CYLINDRICAL_SURFACE('',#107594,0.17526);
#91457=CYLINDRICAL_SURFACE('',#107595,0.175259999999999);
#91458=CYLINDRICAL_SURFACE('',#107596,0.17526);
#91459=CYLINDRICAL_SURFACE('',#107597,0.175259999999999);
#91460=CYLINDRICAL_SURFACE('',#107598,0.17526);
#91461=CYLINDRICAL_SURFACE('',#107599,0.17526);
#91462=CYLINDRICAL_SURFACE('',#107600,0.17526);
#91463=CYLINDRICAL_SURFACE('',#107601,0.126999999705659);
#91464=CYLINDRICAL_SURFACE('',#107605,0.127);
#91465=CYLINDRICAL_SURFACE('',#107607,0.127);
#91466=CYLINDRICAL_SURFACE('',#107611,0.127000005438804);
#91467=CYLINDRICAL_SURFACE('',#107613,0.127000001278595);
#91468=CYLINDRICAL_SURFACE('',#107616,0.127);
#91469=CYLINDRICAL_SURFACE('',#107622,0.126999993613258);
#91470=CYLINDRICAL_SURFACE('',#107624,0.127000005456531);
#91471=CYLINDRICAL_SURFACE('',#107630,0.126999999999999);
#91472=CYLINDRICAL_SURFACE('',#107633,0.126999998754334);
#91473=CYLINDRICAL_SURFACE('',#107635,0.126999993594558);
#91474=CYLINDRICAL_SURFACE('',#107639,0.126999999999999);
#91475=CYLINDRICAL_SURFACE('',#107641,0.126999999999999);
#91476=CYLINDRICAL_SURFACE('',#107644,0.127000000302017);
#91477=CYLINDRICAL_SURFACE('',#107645,0.126999999706877);
#91478=CYLINDRICAL_SURFACE('',#107649,0.127);
#91479=CYLINDRICAL_SURFACE('',#107651,0.127);
#91480=CYLINDRICAL_SURFACE('',#107655,0.127000005438286);
#91481=CYLINDRICAL_SURFACE('',#107657,0.127000001280016);
#91482=CYLINDRICAL_SURFACE('',#107660,0.127);
#91483=CYLINDRICAL_SURFACE('',#107666,0.126999993612901);
#91484=CYLINDRICAL_SURFACE('',#107668,0.127000005452847);
#91485=CYLINDRICAL_SURFACE('',#107674,0.126999999999999);
#91486=CYLINDRICAL_SURFACE('',#107677,0.12699999875172);
#91487=CYLINDRICAL_SURFACE('',#107679,0.126999993595217);
#91488=CYLINDRICAL_SURFACE('',#107683,0.126999999999999);
#91489=CYLINDRICAL_SURFACE('',#107685,0.126999999999999);
#91490=CYLINDRICAL_SURFACE('',#107688,0.127000000302727);
#91491=CYLINDRICAL_SURFACE('',#107689,0.126999999707438);
#91492=CYLINDRICAL_SURFACE('',#107693,0.127);
#91493=CYLINDRICAL_SURFACE('',#107695,0.127);
#91494=CYLINDRICAL_SURFACE('',#107699,0.127000005439645);
#91495=CYLINDRICAL_SURFACE('',#107701,0.127000001279045);
#91496=CYLINDRICAL_SURFACE('',#107704,0.127);
#91497=CYLINDRICAL_SURFACE('',#107710,0.126999993613143);
#91498=CYLINDRICAL_SURFACE('',#107712,0.127000005454004);
#91499=CYLINDRICAL_SURFACE('',#107718,0.127000000000002);
#91500=CYLINDRICAL_SURFACE('',#107721,0.126999998753197);
#91501=CYLINDRICAL_SURFACE('',#107723,0.126999993594632);
#91502=CYLINDRICAL_SURFACE('',#107727,0.127000000000002);
#91503=CYLINDRICAL_SURFACE('',#107729,0.127000000000002);
#91504=CYLINDRICAL_SURFACE('',#107732,0.127000000302894);
#91505=CYLINDRICAL_SURFACE('',#107733,0.126999999705007);
#91506=CYLINDRICAL_SURFACE('',#107737,0.127);
#91507=CYLINDRICAL_SURFACE('',#107739,0.127);
#91508=CYLINDRICAL_SURFACE('',#107743,0.127000005436761);
#91509=CYLINDRICAL_SURFACE('',#107745,0.127000001278623);
#91510=CYLINDRICAL_SURFACE('',#107748,0.127);
#91511=CYLINDRICAL_SURFACE('',#107754,0.126999993614452);
#91512=CYLINDRICAL_SURFACE('',#107756,0.127000005456074);
#91513=CYLINDRICAL_SURFACE('',#107762,0.127000000000001);
#91514=CYLINDRICAL_SURFACE('',#107765,0.126999998753102);
#91515=CYLINDRICAL_SURFACE('',#107767,0.126999993593139);
#91516=CYLINDRICAL_SURFACE('',#107771,0.127000000000001);
#91517=CYLINDRICAL_SURFACE('',#107773,0.127000000000001);
#91518=CYLINDRICAL_SURFACE('',#107776,0.127000000302033);
#91519=CYLINDRICAL_SURFACE('',#107777,0.126999999705891);
#91520=CYLINDRICAL_SURFACE('',#107781,0.127);
#91521=CYLINDRICAL_SURFACE('',#107783,0.127);
#91522=CYLINDRICAL_SURFACE('',#107787,0.127000005438578);
#91523=CYLINDRICAL_SURFACE('',#107789,0.127000001278986);
#91524=CYLINDRICAL_SURFACE('',#107792,0.127);
#91525=CYLINDRICAL_SURFACE('',#107798,0.126999993613499);
#91526=CYLINDRICAL_SURFACE('',#107800,0.127000005452666);
#91527=CYLINDRICAL_SURFACE('',#107806,0.127);
#91528=CYLINDRICAL_SURFACE('',#107809,0.1269999987535);
#91529=CYLINDRICAL_SURFACE('',#107811,0.126999993594111);
#91530=CYLINDRICAL_SURFACE('',#107815,0.127);
#91531=CYLINDRICAL_SURFACE('',#107817,0.127);
#91532=CYLINDRICAL_SURFACE('',#107820,0.127000000301114);
#91533=CYLINDRICAL_SURFACE('',#107821,0.126999999706381);
#91534=CYLINDRICAL_SURFACE('',#107825,0.127);
#91535=CYLINDRICAL_SURFACE('',#107827,0.127);
#91536=CYLINDRICAL_SURFACE('',#107831,0.127000005437376);
#91537=CYLINDRICAL_SURFACE('',#107833,0.12700000127869);
#91538=CYLINDRICAL_SURFACE('',#107836,0.127);
#91539=CYLINDRICAL_SURFACE('',#107842,0.126999993614952);
#91540=CYLINDRICAL_SURFACE('',#107844,0.127000005452941);
#91541=CYLINDRICAL_SURFACE('',#107850,0.127000000000001);
#91542=CYLINDRICAL_SURFACE('',#107853,0.126999998752931);
#91543=CYLINDRICAL_SURFACE('',#107855,0.126999993591758);
#91544=CYLINDRICAL_SURFACE('',#107859,0.127000000000001);
#91545=CYLINDRICAL_SURFACE('',#107861,0.127000000000001);
#91546=CYLINDRICAL_SURFACE('',#107864,0.127000000300221);
#91547=CYLINDRICAL_SURFACE('',#107865,0.126999999706944);
#91548=CYLINDRICAL_SURFACE('',#107869,0.127);
#91549=CYLINDRICAL_SURFACE('',#107871,0.127);
#91550=CYLINDRICAL_SURFACE('',#107875,0.127000005438498);
#91551=CYLINDRICAL_SURFACE('',#107877,0.127000001278942);
#91552=CYLINDRICAL_SURFACE('',#107880,0.127);
#91553=CYLINDRICAL_SURFACE('',#107886,0.126999993619589);
#91554=CYLINDRICAL_SURFACE('',#107888,0.12700000545362);
#91555=CYLINDRICAL_SURFACE('',#107894,0.126999999999998);
#91556=CYLINDRICAL_SURFACE('',#107897,0.12699999875288);
#91557=CYLINDRICAL_SURFACE('',#107899,0.126999993594423);
#91558=CYLINDRICAL_SURFACE('',#107903,0.126999999999998);
#91559=CYLINDRICAL_SURFACE('',#107905,0.126999999999998);
#91560=CYLINDRICAL_SURFACE('',#107908,0.127000000302494);
#91561=CYLINDRICAL_SURFACE('',#107909,0.126999999707788);
#91562=CYLINDRICAL_SURFACE('',#107913,0.127);
#91563=CYLINDRICAL_SURFACE('',#107915,0.127);
#91564=CYLINDRICAL_SURFACE('',#107919,0.127000005437275);
#91565=CYLINDRICAL_SURFACE('',#107921,0.127000001280034);
#91566=CYLINDRICAL_SURFACE('',#107924,0.127);
#91567=CYLINDRICAL_SURFACE('',#107930,0.126999993614549);
#91568=CYLINDRICAL_SURFACE('',#107932,0.127000005453645);
#91569=CYLINDRICAL_SURFACE('',#107938,0.127);
#91570=CYLINDRICAL_SURFACE('',#107941,0.126999998753375);
#91571=CYLINDRICAL_SURFACE('',#107943,0.126999993593803);
#91572=CYLINDRICAL_SURFACE('',#107947,0.127);
#91573=CYLINDRICAL_SURFACE('',#107949,0.127);
#91574=CYLINDRICAL_SURFACE('',#107952,0.127000000302309);
#91575=CYLINDRICAL_SURFACE('',#107953,0.126999999706647);
#91576=CYLINDRICAL_SURFACE('',#107957,0.127);
#91577=CYLINDRICAL_SURFACE('',#107959,0.127);
#91578=CYLINDRICAL_SURFACE('',#107963,0.127000005438832);
#91579=CYLINDRICAL_SURFACE('',#107965,0.127000001280675);
#91580=CYLINDRICAL_SURFACE('',#107968,0.127);
#91581=CYLINDRICAL_SURFACE('',#107974,0.126999993615939);
#91582=CYLINDRICAL_SURFACE('',#107976,0.12700000545297);
#91583=CYLINDRICAL_SURFACE('',#107982,0.126999999999999);
#91584=CYLINDRICAL_SURFACE('',#107985,0.126999998754127);
#91585=CYLINDRICAL_SURFACE('',#107987,0.126999993593799);
#91586=CYLINDRICAL_SURFACE('',#107991,0.126999999999999);
#91587=CYLINDRICAL_SURFACE('',#107993,0.126999999999999);
#91588=CYLINDRICAL_SURFACE('',#107996,0.12700000030121);
#91589=CYLINDRICAL_SURFACE('',#107997,0.126999999706712);
#91590=CYLINDRICAL_SURFACE('',#108001,0.127);
#91591=CYLINDRICAL_SURFACE('',#108003,0.127);
#91592=CYLINDRICAL_SURFACE('',#108007,0.127000005438327);
#91593=CYLINDRICAL_SURFACE('',#108009,0.127000001279818);
#91594=CYLINDRICAL_SURFACE('',#108012,0.127);
#91595=CYLINDRICAL_SURFACE('',#108018,0.126999993613333);
#91596=CYLINDRICAL_SURFACE('',#108020,0.127000005454714);
#91597=CYLINDRICAL_SURFACE('',#108026,0.127);
#91598=CYLINDRICAL_SURFACE('',#108029,0.126999998752385);
#91599=CYLINDRICAL_SURFACE('',#108031,0.126999993595799);
#91600=CYLINDRICAL_SURFACE('',#108035,0.127000000000001);
#91601=CYLINDRICAL_SURFACE('',#108037,0.127000000000001);
#91602=CYLINDRICAL_SURFACE('',#108040,0.12700000030205);
#91603=CYLINDRICAL_SURFACE('',#108041,0.126999999707271);
#91604=CYLINDRICAL_SURFACE('',#108045,0.127);
#91605=CYLINDRICAL_SURFACE('',#108047,0.127);
#91606=CYLINDRICAL_SURFACE('',#108051,0.127000005437262);
#91607=CYLINDRICAL_SURFACE('',#108053,0.127000001277901);
#91608=CYLINDRICAL_SURFACE('',#108056,0.127);
#91609=CYLINDRICAL_SURFACE('',#108062,0.126999993615953);
#91610=CYLINDRICAL_SURFACE('',#108064,0.127000005455153);
#91611=CYLINDRICAL_SURFACE('',#108070,0.127000000000001);
#91612=CYLINDRICAL_SURFACE('',#108073,0.126999998754757);
#91613=CYLINDRICAL_SURFACE('',#108075,0.12699999359852);
#91614=CYLINDRICAL_SURFACE('',#108079,0.127000000000001);
#91615=CYLINDRICAL_SURFACE('',#108081,0.127000000000001);
#91616=CYLINDRICAL_SURFACE('',#108084,0.127000000302116);
#91617=CYLINDRICAL_SURFACE('',#108085,0.126999999707366);
#91618=CYLINDRICAL_SURFACE('',#108089,0.127);
#91619=CYLINDRICAL_SURFACE('',#108091,0.127);
#91620=CYLINDRICAL_SURFACE('',#108095,0.127000005434585);
#91621=CYLINDRICAL_SURFACE('',#108097,0.127000001280038);
#91622=CYLINDRICAL_SURFACE('',#108100,0.127);
#91623=CYLINDRICAL_SURFACE('',#108106,0.126999993613355);
#91624=CYLINDRICAL_SURFACE('',#108108,0.127000005454191);
#91625=CYLINDRICAL_SURFACE('',#108114,0.127);
#91626=CYLINDRICAL_SURFACE('',#108117,0.126999998752333);
#91627=CYLINDRICAL_SURFACE('',#108119,0.126999993594576);
#91628=CYLINDRICAL_SURFACE('',#108123,0.127);
#91629=CYLINDRICAL_SURFACE('',#108125,0.127);
#91630=CYLINDRICAL_SURFACE('',#108128,0.127000000300596);
#91631=CYLINDRICAL_SURFACE('',#108129,0.126999999707311);
#91632=CYLINDRICAL_SURFACE('',#108133,0.127);
#91633=CYLINDRICAL_SURFACE('',#108135,0.127);
#91634=CYLINDRICAL_SURFACE('',#108139,0.127000005439773);
#91635=CYLINDRICAL_SURFACE('',#108141,0.127000001277871);
#91636=CYLINDRICAL_SURFACE('',#108144,0.127);
#91637=CYLINDRICAL_SURFACE('',#108150,0.126999993616715);
#91638=CYLINDRICAL_SURFACE('',#108152,0.127000005452816);
#91639=CYLINDRICAL_SURFACE('',#108158,0.127);
#91640=CYLINDRICAL_SURFACE('',#108161,0.126999998753913);
#91641=CYLINDRICAL_SURFACE('',#108163,0.126999993595481);
#91642=CYLINDRICAL_SURFACE('',#108167,0.127);
#91643=CYLINDRICAL_SURFACE('',#108169,0.127);
#91644=CYLINDRICAL_SURFACE('',#108172,0.127000000300196);
#91645=CYLINDRICAL_SURFACE('',#108173,0.126999999705456);
#91646=CYLINDRICAL_SURFACE('',#108177,0.127);
#91647=CYLINDRICAL_SURFACE('',#108179,0.127);
#91648=CYLINDRICAL_SURFACE('',#108183,0.127000005436537);
#91649=CYLINDRICAL_SURFACE('',#108185,0.12700000127896);
#91650=CYLINDRICAL_SURFACE('',#108188,0.127);
#91651=CYLINDRICAL_SURFACE('',#108194,0.126999993615659);
#91652=CYLINDRICAL_SURFACE('',#108196,0.127000005453786);
#91653=CYLINDRICAL_SURFACE('',#108202,0.127);
#91654=CYLINDRICAL_SURFACE('',#108205,0.12699999875271);
#91655=CYLINDRICAL_SURFACE('',#108207,0.126999993596784);
#91656=CYLINDRICAL_SURFACE('',#108211,0.127);
#91657=CYLINDRICAL_SURFACE('',#108213,0.127);
#91658=CYLINDRICAL_SURFACE('',#108216,0.127000000301125);
#91659=CYLINDRICAL_SURFACE('',#108217,0.126999999707381);
#91660=CYLINDRICAL_SURFACE('',#108221,0.127);
#91661=CYLINDRICAL_SURFACE('',#108223,0.127);
#91662=CYLINDRICAL_SURFACE('',#108227,0.127000005436994);
#91663=CYLINDRICAL_SURFACE('',#108229,0.127000001279189);
#91664=CYLINDRICAL_SURFACE('',#108232,0.127);
#91665=CYLINDRICAL_SURFACE('',#108238,0.126999993613671);
#91666=CYLINDRICAL_SURFACE('',#108240,0.127000005453692);
#91667=CYLINDRICAL_SURFACE('',#108246,0.127);
#91668=CYLINDRICAL_SURFACE('',#108249,0.126999998754202);
#91669=CYLINDRICAL_SURFACE('',#108251,0.126999993593398);
#91670=CYLINDRICAL_SURFACE('',#108255,0.127);
#91671=CYLINDRICAL_SURFACE('',#108257,0.127);
#91672=CYLINDRICAL_SURFACE('',#108260,0.127000000301612);
#91673=CYLINDRICAL_SURFACE('',#108261,0.126999999706848);
#91674=CYLINDRICAL_SURFACE('',#108265,0.127);
#91675=CYLINDRICAL_SURFACE('',#108267,0.127);
#91676=CYLINDRICAL_SURFACE('',#108271,0.127000005437153);
#91677=CYLINDRICAL_SURFACE('',#108273,0.127000001278536);
#91678=CYLINDRICAL_SURFACE('',#108276,0.127);
#91679=CYLINDRICAL_SURFACE('',#108282,0.126999993614016);
#91680=CYLINDRICAL_SURFACE('',#108284,0.127000005452352);
#91681=CYLINDRICAL_SURFACE('',#108290,0.127);
#91682=CYLINDRICAL_SURFACE('',#108293,0.126999998753935);
#91683=CYLINDRICAL_SURFACE('',#108295,0.126999993594902);
#91684=CYLINDRICAL_SURFACE('',#108299,0.127);
#91685=CYLINDRICAL_SURFACE('',#108301,0.127);
#91686=CYLINDRICAL_SURFACE('',#108304,0.127000000300736);
#91687=CYLINDRICAL_SURFACE('',#108305,0.126999999706529);
#91688=CYLINDRICAL_SURFACE('',#108309,0.127);
#91689=CYLINDRICAL_SURFACE('',#108311,0.127);
#91690=CYLINDRICAL_SURFACE('',#108315,0.127000005438594);
#91691=CYLINDRICAL_SURFACE('',#108317,0.127000001279977);
#91692=CYLINDRICAL_SURFACE('',#108320,0.127);
#91693=CYLINDRICAL_SURFACE('',#108326,0.126999993615537);
#91694=CYLINDRICAL_SURFACE('',#108328,0.127000005452522);
#91695=CYLINDRICAL_SURFACE('',#108334,0.127);
#91696=CYLINDRICAL_SURFACE('',#108337,0.126999998752468);
#91697=CYLINDRICAL_SURFACE('',#108339,0.126999993596773);
#91698=CYLINDRICAL_SURFACE('',#108343,0.127);
#91699=CYLINDRICAL_SURFACE('',#108345,0.127);
#91700=CYLINDRICAL_SURFACE('',#108348,0.127000000301443);
#91701=CYLINDRICAL_SURFACE('',#108349,0.126999999704752);
#91702=CYLINDRICAL_SURFACE('',#108353,0.127);
#91703=CYLINDRICAL_SURFACE('',#108355,0.127);
#91704=CYLINDRICAL_SURFACE('',#108359,0.127000005440182);
#91705=CYLINDRICAL_SURFACE('',#108361,0.127000001279415);
#91706=CYLINDRICAL_SURFACE('',#108364,0.127);
#91707=CYLINDRICAL_SURFACE('',#108370,0.12699999361407);
#91708=CYLINDRICAL_SURFACE('',#108372,0.127000005453498);
#91709=CYLINDRICAL_SURFACE('',#108378,0.126999999999999);
#91710=CYLINDRICAL_SURFACE('',#108381,0.126999998753558);
#91711=CYLINDRICAL_SURFACE('',#108383,0.126999993595186);
#91712=CYLINDRICAL_SURFACE('',#108387,0.126999999999999);
#91713=CYLINDRICAL_SURFACE('',#108389,0.126999999999999);
#91714=CYLINDRICAL_SURFACE('',#108392,0.127000000302269);
#91715=CYLINDRICAL_SURFACE('',#108393,0.126999999706853);
#91716=CYLINDRICAL_SURFACE('',#108397,0.127);
#91717=CYLINDRICAL_SURFACE('',#108399,0.127);
#91718=CYLINDRICAL_SURFACE('',#108403,0.127000005436064);
#91719=CYLINDRICAL_SURFACE('',#108405,0.127000001278517);
#91720=CYLINDRICAL_SURFACE('',#108408,0.127);
#91721=CYLINDRICAL_SURFACE('',#108414,0.126999993620423);
#91722=CYLINDRICAL_SURFACE('',#108416,0.127000005452903);
#91723=CYLINDRICAL_SURFACE('',#108422,0.127000000000001);
#91724=CYLINDRICAL_SURFACE('',#108425,0.126999998753051);
#91725=CYLINDRICAL_SURFACE('',#108427,0.126999993597228);
#91726=CYLINDRICAL_SURFACE('',#108431,0.127000000000001);
#91727=CYLINDRICAL_SURFACE('',#108433,0.127000000000001);
#91728=CYLINDRICAL_SURFACE('',#108436,0.127000000301954);
#91729=CYLINDRICAL_SURFACE('',#108437,0.126999999706396);
#91730=CYLINDRICAL_SURFACE('',#108441,0.127);
#91731=CYLINDRICAL_SURFACE('',#108443,0.127);
#91732=CYLINDRICAL_SURFACE('',#108447,0.127000005437226);
#91733=CYLINDRICAL_SURFACE('',#108449,0.127000001279001);
#91734=CYLINDRICAL_SURFACE('',#108452,0.127);
#91735=CYLINDRICAL_SURFACE('',#108458,0.12699999361601);
#91736=CYLINDRICAL_SURFACE('',#108460,0.127000005455446);
#91737=CYLINDRICAL_SURFACE('',#108466,0.127);
#91738=CYLINDRICAL_SURFACE('',#108469,0.126999998753164);
#91739=CYLINDRICAL_SURFACE('',#108471,0.126999993595105);
#91740=CYLINDRICAL_SURFACE('',#108475,0.127);
#91741=CYLINDRICAL_SURFACE('',#108477,0.127);
#91742=CYLINDRICAL_SURFACE('',#108480,0.12700000030132);
#91743=CYLINDRICAL_SURFACE('',#108481,0.126999999705817);
#91744=CYLINDRICAL_SURFACE('',#108485,0.127);
#91745=CYLINDRICAL_SURFACE('',#108487,0.127);
#91746=CYLINDRICAL_SURFACE('',#108491,0.127000005439081);
#91747=CYLINDRICAL_SURFACE('',#108493,0.127000001278701);
#91748=CYLINDRICAL_SURFACE('',#108496,0.127);
#91749=CYLINDRICAL_SURFACE('',#108502,0.12699999361471);
#91750=CYLINDRICAL_SURFACE('',#108504,0.127000005455995);
#91751=CYLINDRICAL_SURFACE('',#108510,0.127000000000001);
#91752=CYLINDRICAL_SURFACE('',#108513,0.126999998754023);
#91753=CYLINDRICAL_SURFACE('',#108515,0.126999993595822);
#91754=CYLINDRICAL_SURFACE('',#108519,0.127000000000001);
#91755=CYLINDRICAL_SURFACE('',#108521,0.127000000000001);
#91756=CYLINDRICAL_SURFACE('',#108524,0.127000000300876);
#91757=CYLINDRICAL_SURFACE('',#108525,0.126999999707033);
#91758=CYLINDRICAL_SURFACE('',#108529,0.127);
#91759=CYLINDRICAL_SURFACE('',#108531,0.127);
#91760=CYLINDRICAL_SURFACE('',#108535,0.127000005440277);
#91761=CYLINDRICAL_SURFACE('',#108537,0.127000001277889);
#91762=CYLINDRICAL_SURFACE('',#108540,0.127);
#91763=CYLINDRICAL_SURFACE('',#108546,0.126999993612714);
#91764=CYLINDRICAL_SURFACE('',#108548,0.127000005448686);
#91765=CYLINDRICAL_SURFACE('',#108554,0.127);
#91766=CYLINDRICAL_SURFACE('',#108557,0.126999998752826);
#91767=CYLINDRICAL_SURFACE('',#108559,0.126999993595237);
#91768=CYLINDRICAL_SURFACE('',#108563,0.127);
#91769=CYLINDRICAL_SURFACE('',#108565,0.127);
#91770=CYLINDRICAL_SURFACE('',#108568,0.127000000300549);
#91771=CYLINDRICAL_SURFACE('',#108569,0.126999999706643);
#91772=CYLINDRICAL_SURFACE('',#108573,0.127);
#91773=CYLINDRICAL_SURFACE('',#108575,0.127);
#91774=CYLINDRICAL_SURFACE('',#108579,0.127000005436435);
#91775=CYLINDRICAL_SURFACE('',#108581,0.127000001281433);
#91776=CYLINDRICAL_SURFACE('',#108584,0.127);
#91777=CYLINDRICAL_SURFACE('',#108590,0.126999993613013);
#91778=CYLINDRICAL_SURFACE('',#108592,0.127000005453951);
#91779=CYLINDRICAL_SURFACE('',#108598,0.127);
#91780=CYLINDRICAL_SURFACE('',#108601,0.126999998753876);
#91781=CYLINDRICAL_SURFACE('',#108603,0.126999993592809);
#91782=CYLINDRICAL_SURFACE('',#108607,0.127);
#91783=CYLINDRICAL_SURFACE('',#108609,0.127);
#91784=CYLINDRICAL_SURFACE('',#108612,0.127000000301689);
#91785=CYLINDRICAL_SURFACE('',#108613,0.126999999707302);
#91786=CYLINDRICAL_SURFACE('',#108617,0.127);
#91787=CYLINDRICAL_SURFACE('',#108619,0.127);
#91788=CYLINDRICAL_SURFACE('',#108623,0.127000005436606);
#91789=CYLINDRICAL_SURFACE('',#108625,0.127000001276832);
#91790=CYLINDRICAL_SURFACE('',#108628,0.127);
#91791=CYLINDRICAL_SURFACE('',#108634,0.126999993613542);
#91792=CYLINDRICAL_SURFACE('',#108636,0.127000005453435);
#91793=CYLINDRICAL_SURFACE('',#108642,0.127000000000001);
#91794=CYLINDRICAL_SURFACE('',#108645,0.126999998753528);
#91795=CYLINDRICAL_SURFACE('',#108647,0.126999993595165);
#91796=CYLINDRICAL_SURFACE('',#108651,0.127000000000001);
#91797=CYLINDRICAL_SURFACE('',#108653,0.127000000000001);
#91798=CYLINDRICAL_SURFACE('',#108656,0.127000000300756);
#91799=CYLINDRICAL_SURFACE('',#108657,0.126999999707029);
#91800=CYLINDRICAL_SURFACE('',#108661,0.127);
#91801=CYLINDRICAL_SURFACE('',#108663,0.127);
#91802=CYLINDRICAL_SURFACE('',#108667,0.127000005435516);
#91803=CYLINDRICAL_SURFACE('',#108669,0.127000001278317);
#91804=CYLINDRICAL_SURFACE('',#108672,0.127);
#91805=CYLINDRICAL_SURFACE('',#108678,0.126999993613955);
#91806=CYLINDRICAL_SURFACE('',#108680,0.127000005452699);
#91807=CYLINDRICAL_SURFACE('',#108686,0.127);
#91808=CYLINDRICAL_SURFACE('',#108689,0.126999998753515);
#91809=CYLINDRICAL_SURFACE('',#108691,0.126999993596424);
#91810=CYLINDRICAL_SURFACE('',#108695,0.127);
#91811=CYLINDRICAL_SURFACE('',#108697,0.127);
#91812=CYLINDRICAL_SURFACE('',#108700,0.127000000301871);
#91813=CYLINDRICAL_SURFACE('',#108701,0.126999999706675);
#91814=CYLINDRICAL_SURFACE('',#108705,0.127);
#91815=CYLINDRICAL_SURFACE('',#108707,0.127);
#91816=CYLINDRICAL_SURFACE('',#108711,0.127000005439049);
#91817=CYLINDRICAL_SURFACE('',#108713,0.127000001277567);
#91818=CYLINDRICAL_SURFACE('',#108716,0.127);
#91819=CYLINDRICAL_SURFACE('',#108722,0.12699999361663);
#91820=CYLINDRICAL_SURFACE('',#108724,0.127000005453719);
#91821=CYLINDRICAL_SURFACE('',#108730,0.127000000000001);
#91822=CYLINDRICAL_SURFACE('',#108733,0.126999998751427);
#91823=CYLINDRICAL_SURFACE('',#108735,0.126999993596735);
#91824=CYLINDRICAL_SURFACE('',#108739,0.127000000000001);
#91825=CYLINDRICAL_SURFACE('',#108741,0.127000000000001);
#91826=CYLINDRICAL_SURFACE('',#108744,0.127000000301557);
#91827=CYLINDRICAL_SURFACE('',#108745,0.126999999707433);
#91828=CYLINDRICAL_SURFACE('',#108749,0.127);
#91829=CYLINDRICAL_SURFACE('',#108751,0.127);
#91830=CYLINDRICAL_SURFACE('',#108755,0.127000005437756);
#91831=CYLINDRICAL_SURFACE('',#108757,0.127000001278296);
#91832=CYLINDRICAL_SURFACE('',#108760,0.127);
#91833=CYLINDRICAL_SURFACE('',#108766,0.126999993613017);
#91834=CYLINDRICAL_SURFACE('',#108768,0.127000005454635);
#91835=CYLINDRICAL_SURFACE('',#108774,0.127000000000002);
#91836=CYLINDRICAL_SURFACE('',#108777,0.126999998753502);
#91837=CYLINDRICAL_SURFACE('',#108779,0.126999993595);
#91838=CYLINDRICAL_SURFACE('',#108783,0.127000000000002);
#91839=CYLINDRICAL_SURFACE('',#108785,0.127000000000002);
#91840=CYLINDRICAL_SURFACE('',#108788,0.127000000302929);
#91841=CYLINDRICAL_SURFACE('',#108789,0.126999999706685);
#91842=CYLINDRICAL_SURFACE('',#108793,0.127);
#91843=CYLINDRICAL_SURFACE('',#108795,0.127);
#91844=CYLINDRICAL_SURFACE('',#108799,0.127000005439371);
#91845=CYLINDRICAL_SURFACE('',#108801,0.127000001278466);
#91846=CYLINDRICAL_SURFACE('',#108804,0.127);
#91847=CYLINDRICAL_SURFACE('',#108810,0.126999993615652);
#91848=CYLINDRICAL_SURFACE('',#108812,0.127000005453095);
#91849=CYLINDRICAL_SURFACE('',#108818,0.126999999999999);
#91850=CYLINDRICAL_SURFACE('',#108821,0.126999998752404);
#91851=CYLINDRICAL_SURFACE('',#108823,0.126999993593318);
#91852=CYLINDRICAL_SURFACE('',#108827,0.126999999999999);
#91853=CYLINDRICAL_SURFACE('',#108829,0.126999999999999);
#91854=CYLINDRICAL_SURFACE('',#108832,0.12700000030076);
#91855=CYLINDRICAL_SURFACE('',#108833,0.126999999706931);
#91856=CYLINDRICAL_SURFACE('',#108837,0.127);
#91857=CYLINDRICAL_SURFACE('',#108839,0.127);
#91858=CYLINDRICAL_SURFACE('',#108843,0.127000005438782);
#91859=CYLINDRICAL_SURFACE('',#108845,0.127000001278968);
#91860=CYLINDRICAL_SURFACE('',#108848,0.127);
#91861=CYLINDRICAL_SURFACE('',#108854,0.126999993616082);
#91862=CYLINDRICAL_SURFACE('',#108856,0.127000005452452);
#91863=CYLINDRICAL_SURFACE('',#108862,0.126999999999999);
#91864=CYLINDRICAL_SURFACE('',#108865,0.126999998751743);
#91865=CYLINDRICAL_SURFACE('',#108867,0.126999993596233);
#91866=CYLINDRICAL_SURFACE('',#108871,0.126999999999999);
#91867=CYLINDRICAL_SURFACE('',#108873,0.126999999999999);
#91868=CYLINDRICAL_SURFACE('',#108876,0.127000000301475);
#91869=CYLINDRICAL_SURFACE('',#108877,0.126999999707036);
#91870=CYLINDRICAL_SURFACE('',#108881,0.127);
#91871=CYLINDRICAL_SURFACE('',#108883,0.127);
#91872=CYLINDRICAL_SURFACE('',#108887,0.12700000543752);
#91873=CYLINDRICAL_SURFACE('',#108889,0.12700000127917);
#91874=CYLINDRICAL_SURFACE('',#108891,0.127);
#91875=CYLINDRICAL_SURFACE('',#108895,0.126999993614675);
#91876=CYLINDRICAL_SURFACE('',#108897,0.127000005454215);
#91877=CYLINDRICAL_SURFACE('',#108900,0.127);
#91878=CYLINDRICAL_SURFACE('',#108903,0.126999998753483);
#91879=CYLINDRICAL_SURFACE('',#108905,0.126999993594397);
#91880=CYLINDRICAL_SURFACE('',#108909,0.127);
#91881=CYLINDRICAL_SURFACE('',#108911,0.127);
#91882=CYLINDRICAL_SURFACE('',#108914,0.12700000030073);
#91883=CYLINDRICAL_SURFACE('',#108915,0.126999999707031);
#91884=CYLINDRICAL_SURFACE('',#108919,0.127);
#91885=CYLINDRICAL_SURFACE('',#108921,0.127);
#91886=CYLINDRICAL_SURFACE('',#108925,0.127000005436211);
#91887=CYLINDRICAL_SURFACE('',#108927,0.127000001279552);
#91888=CYLINDRICAL_SURFACE('',#108930,0.127);
#91889=CYLINDRICAL_SURFACE('',#108936,0.12699999361449);
#91890=CYLINDRICAL_SURFACE('',#108938,0.127000005453587);
#91891=CYLINDRICAL_SURFACE('',#108944,0.127);
#91892=CYLINDRICAL_SURFACE('',#108947,0.126999998754038);
#91893=CYLINDRICAL_SURFACE('',#108949,0.1269999935941);
#91894=CYLINDRICAL_SURFACE('',#108953,0.127);
#91895=CYLINDRICAL_SURFACE('',#108955,0.127);
#91896=CYLINDRICAL_SURFACE('',#108958,0.127000000302173);
#91897=CYLINDRICAL_SURFACE('',#108959,0.126999999706813);
#91898=CYLINDRICAL_SURFACE('',#108963,0.127);
#91899=CYLINDRICAL_SURFACE('',#108965,0.127);
#91900=CYLINDRICAL_SURFACE('',#108969,0.127000005436503);
#91901=CYLINDRICAL_SURFACE('',#108971,0.127000001279098);
#91902=CYLINDRICAL_SURFACE('',#108974,0.127);
#91903=CYLINDRICAL_SURFACE('',#108980,0.126999993612834);
#91904=CYLINDRICAL_SURFACE('',#108982,0.127000005453372);
#91905=CYLINDRICAL_SURFACE('',#108988,0.126999999999999);
#91906=CYLINDRICAL_SURFACE('',#108991,0.126999998753505);
#91907=CYLINDRICAL_SURFACE('',#108993,0.126999993596201);
#91908=CYLINDRICAL_SURFACE('',#108997,0.126999999999999);
#91909=CYLINDRICAL_SURFACE('',#108999,0.126999999999999);
#91910=CYLINDRICAL_SURFACE('',#109002,0.127000000301212);
#91911=CYLINDRICAL_SURFACE('',#109003,0.126999999705899);
#91912=CYLINDRICAL_SURFACE('',#109007,0.127);
#91913=CYLINDRICAL_SURFACE('',#109009,0.127);
#91914=CYLINDRICAL_SURFACE('',#109013,0.127000005438409);
#91915=CYLINDRICAL_SURFACE('',#109015,0.127000001279442);
#91916=CYLINDRICAL_SURFACE('',#109018,0.127);
#91917=CYLINDRICAL_SURFACE('',#109024,0.12699999361406);
#91918=CYLINDRICAL_SURFACE('',#109026,0.127000005452943);
#91919=CYLINDRICAL_SURFACE('',#109032,0.127000000000002);
#91920=CYLINDRICAL_SURFACE('',#109035,0.126999998753321);
#91921=CYLINDRICAL_SURFACE('',#109037,0.126999993595877);
#91922=CYLINDRICAL_SURFACE('',#109041,0.127000000000002);
#91923=CYLINDRICAL_SURFACE('',#109043,0.127000000000002);
#91924=CYLINDRICAL_SURFACE('',#109046,0.127000000299965);
#91925=CYLINDRICAL_SURFACE('',#109047,0.126999999705897);
#91926=CYLINDRICAL_SURFACE('',#109051,0.127);
#91927=CYLINDRICAL_SURFACE('',#109053,0.127);
#91928=CYLINDRICAL_SURFACE('',#109057,0.127000005435509);
#91929=CYLINDRICAL_SURFACE('',#109059,0.127000001277923);
#91930=CYLINDRICAL_SURFACE('',#109062,0.127);
#91931=CYLINDRICAL_SURFACE('',#109068,0.126999993617466);
#91932=CYLINDRICAL_SURFACE('',#109070,0.127000005455358);
#91933=CYLINDRICAL_SURFACE('',#109076,0.127000000000001);
#91934=CYLINDRICAL_SURFACE('',#109079,0.126999998752887);
#91935=CYLINDRICAL_SURFACE('',#109081,0.126999993594245);
#91936=CYLINDRICAL_SURFACE('',#109085,0.127000000000001);
#91937=CYLINDRICAL_SURFACE('',#109087,0.127000000000001);
#91938=CYLINDRICAL_SURFACE('',#109090,0.127000000304167);
#91939=CYLINDRICAL_SURFACE('',#109091,0.126999999706985);
#91940=CYLINDRICAL_SURFACE('',#109095,0.127);
#91941=CYLINDRICAL_SURFACE('',#109097,0.127);
#91942=CYLINDRICAL_SURFACE('',#109101,0.127000005438515);
#91943=CYLINDRICAL_SURFACE('',#109103,0.127000001279855);
#91944=CYLINDRICAL_SURFACE('',#109106,0.127);
#91945=CYLINDRICAL_SURFACE('',#109112,0.126999993613953);
#91946=CYLINDRICAL_SURFACE('',#109114,0.127000005453777);
#91947=CYLINDRICAL_SURFACE('',#109120,0.127);
#91948=CYLINDRICAL_SURFACE('',#109123,0.126999998753514);
#91949=CYLINDRICAL_SURFACE('',#109125,0.126999993595633);
#91950=CYLINDRICAL_SURFACE('',#109129,0.127);
#91951=CYLINDRICAL_SURFACE('',#109131,0.127);
#91952=CYLINDRICAL_SURFACE('',#109134,0.127000000301529);
#91953=CYLINDRICAL_SURFACE('',#109135,0.126999999707782);
#91954=CYLINDRICAL_SURFACE('',#109139,0.127);
#91955=CYLINDRICAL_SURFACE('',#109141,0.127);
#91956=CYLINDRICAL_SURFACE('',#109145,0.127000005438866);
#91957=CYLINDRICAL_SURFACE('',#109147,0.127000001278808);
#91958=CYLINDRICAL_SURFACE('',#109150,0.127);
#91959=CYLINDRICAL_SURFACE('',#109156,0.126999993614064);
#91960=CYLINDRICAL_SURFACE('',#109158,0.127000005456815);
#91961=CYLINDRICAL_SURFACE('',#109164,0.127000000000001);
#91962=CYLINDRICAL_SURFACE('',#109167,0.126999998754654);
#91963=CYLINDRICAL_SURFACE('',#109169,0.126999993594296);
#91964=CYLINDRICAL_SURFACE('',#109173,0.127000000000001);
#91965=CYLINDRICAL_SURFACE('',#109175,0.127000000000001);
#91966=CYLINDRICAL_SURFACE('',#109178,0.127000000300983);
#91967=CYLINDRICAL_SURFACE('',#109179,0.126999999705392);
#91968=CYLINDRICAL_SURFACE('',#109183,0.127);
#91969=CYLINDRICAL_SURFACE('',#109185,0.127);
#91970=CYLINDRICAL_SURFACE('',#109189,0.127000005439403);
#91971=CYLINDRICAL_SURFACE('',#109191,0.127000001278241);
#91972=CYLINDRICAL_SURFACE('',#109194,0.127);
#91973=CYLINDRICAL_SURFACE('',#109200,0.126999993613067);
#91974=CYLINDRICAL_SURFACE('',#109202,0.127000005450225);
#91975=CYLINDRICAL_SURFACE('',#109208,0.127);
#91976=CYLINDRICAL_SURFACE('',#109211,0.126999998752507);
#91977=CYLINDRICAL_SURFACE('',#109213,0.126999993595906);
#91978=CYLINDRICAL_SURFACE('',#109217,0.126999999999998);
#91979=CYLINDRICAL_SURFACE('',#109219,0.126999999999998);
#91980=CYLINDRICAL_SURFACE('',#109222,0.127000000300819);
#91981=CYLINDRICAL_SURFACE('',#109223,0.12699999970718);
#91982=CYLINDRICAL_SURFACE('',#109227,0.127);
#91983=CYLINDRICAL_SURFACE('',#109229,0.127);
#91984=CYLINDRICAL_SURFACE('',#109233,0.127000005439627);
#91985=CYLINDRICAL_SURFACE('',#109235,0.127000001280374);
#91986=CYLINDRICAL_SURFACE('',#109238,0.127);
#91987=CYLINDRICAL_SURFACE('',#109244,0.126999993617036);
#91988=CYLINDRICAL_SURFACE('',#109246,0.127000005455582);
#91989=CYLINDRICAL_SURFACE('',#109252,0.127);
#91990=CYLINDRICAL_SURFACE('',#109255,0.126999998754372);
#91991=CYLINDRICAL_SURFACE('',#109257,0.126999993594177);
#91992=CYLINDRICAL_SURFACE('',#109261,0.127);
#91993=CYLINDRICAL_SURFACE('',#109263,0.127);
#91994=CYLINDRICAL_SURFACE('',#109266,0.127000000302369);
#91995=CYLINDRICAL_SURFACE('',#109267,0.126999999707532);
#91996=CYLINDRICAL_SURFACE('',#109271,0.127);
#91997=CYLINDRICAL_SURFACE('',#109273,0.127);
#91998=CYLINDRICAL_SURFACE('',#109277,0.127000005437497);
#91999=CYLINDRICAL_SURFACE('',#109279,0.127000001277774);
#92000=CYLINDRICAL_SURFACE('',#109282,0.127);
#92001=CYLINDRICAL_SURFACE('',#109288,0.126999993612577);
#92002=CYLINDRICAL_SURFACE('',#109290,0.127000005453578);
#92003=CYLINDRICAL_SURFACE('',#109296,0.126999999999999);
#92004=CYLINDRICAL_SURFACE('',#109299,0.126999998752716);
#92005=CYLINDRICAL_SURFACE('',#109301,0.126999993596218);
#92006=CYLINDRICAL_SURFACE('',#109305,0.126999999999999);
#92007=CYLINDRICAL_SURFACE('',#109307,0.126999999999999);
#92008=CYLINDRICAL_SURFACE('',#109310,0.127000000300701);
#92009=CYLINDRICAL_SURFACE('',#109311,0.1269999997065);
#92010=CYLINDRICAL_SURFACE('',#109315,0.127);
#92011=CYLINDRICAL_SURFACE('',#109317,0.127);
#92012=CYLINDRICAL_SURFACE('',#109321,0.127000005436142);
#92013=CYLINDRICAL_SURFACE('',#109323,0.127000001277649);
#92014=CYLINDRICAL_SURFACE('',#109326,0.127);
#92015=CYLINDRICAL_SURFACE('',#109332,0.126999993613931);
#92016=CYLINDRICAL_SURFACE('',#109334,0.127000005454595);
#92017=CYLINDRICAL_SURFACE('',#109340,0.126999999999999);
#92018=CYLINDRICAL_SURFACE('',#109343,0.126999998752409);
#92019=CYLINDRICAL_SURFACE('',#109345,0.126999993591051);
#92020=CYLINDRICAL_SURFACE('',#109349,0.126999999999999);
#92021=CYLINDRICAL_SURFACE('',#109351,0.126999999999999);
#92022=CYLINDRICAL_SURFACE('',#109354,0.127000000301064);
#92023=CYLINDRICAL_SURFACE('',#109355,0.126999999706341);
#92024=CYLINDRICAL_SURFACE('',#109359,0.127);
#92025=CYLINDRICAL_SURFACE('',#109361,0.127);
#92026=CYLINDRICAL_SURFACE('',#109365,0.127000005438825);
#92027=CYLINDRICAL_SURFACE('',#109367,0.12700000127896);
#92028=CYLINDRICAL_SURFACE('',#109370,0.127);
#92029=CYLINDRICAL_SURFACE('',#109376,0.12699999361487);
#92030=CYLINDRICAL_SURFACE('',#109378,0.127000005452653);
#92031=CYLINDRICAL_SURFACE('',#109384,0.127);
#92032=CYLINDRICAL_SURFACE('',#109387,0.126999998753426);
#92033=CYLINDRICAL_SURFACE('',#109389,0.126999993597575);
#92034=CYLINDRICAL_SURFACE('',#109393,0.127);
#92035=CYLINDRICAL_SURFACE('',#109395,0.127);
#92036=CYLINDRICAL_SURFACE('',#109398,0.127000000301659);
#92037=CYLINDRICAL_SURFACE('',#109399,0.126999999707843);
#92038=CYLINDRICAL_SURFACE('',#109403,0.127);
#92039=CYLINDRICAL_SURFACE('',#109405,0.127);
#92040=CYLINDRICAL_SURFACE('',#109409,0.127000005437191);
#92041=CYLINDRICAL_SURFACE('',#109411,0.127000001278864);
#92042=CYLINDRICAL_SURFACE('',#109414,0.127);
#92043=CYLINDRICAL_SURFACE('',#109420,0.126999993613427);
#92044=CYLINDRICAL_SURFACE('',#109422,0.12700000545429);
#92045=CYLINDRICAL_SURFACE('',#109428,0.127);
#92046=CYLINDRICAL_SURFACE('',#109431,0.126999998753965);
#92047=CYLINDRICAL_SURFACE('',#109433,0.126999993595399);
#92048=CYLINDRICAL_SURFACE('',#109437,0.127);
#92049=CYLINDRICAL_SURFACE('',#109439,0.127);
#92050=CYLINDRICAL_SURFACE('',#109442,0.127000000301173);
#92051=CYLINDRICAL_SURFACE('',#109443,0.126999999708117);
#92052=CYLINDRICAL_SURFACE('',#109447,0.127);
#92053=CYLINDRICAL_SURFACE('',#109449,0.127);
#92054=CYLINDRICAL_SURFACE('',#109453,0.127000005437342);
#92055=CYLINDRICAL_SURFACE('',#109455,0.127000001278195);
#92056=CYLINDRICAL_SURFACE('',#109458,0.127);
#92057=CYLINDRICAL_SURFACE('',#109464,0.126999993615767);
#92058=CYLINDRICAL_SURFACE('',#109466,0.127000005451853);
#92059=CYLINDRICAL_SURFACE('',#109472,0.127);
#92060=CYLINDRICAL_SURFACE('',#109475,0.126999998752689);
#92061=CYLINDRICAL_SURFACE('',#109477,0.126999993594723);
#92062=CYLINDRICAL_SURFACE('',#109481,0.127);
#92063=CYLINDRICAL_SURFACE('',#109483,0.127);
#92064=CYLINDRICAL_SURFACE('',#109486,0.127000000299924);
#92065=CYLINDRICAL_SURFACE('',#109487,0.126999999704618);
#92066=CYLINDRICAL_SURFACE('',#109491,0.127);
#92067=CYLINDRICAL_SURFACE('',#109493,0.127);
#92068=CYLINDRICAL_SURFACE('',#109497,0.127000005435034);
#92069=CYLINDRICAL_SURFACE('',#109499,0.127000001280224);
#92070=CYLINDRICAL_SURFACE('',#109502,0.127);
#92071=CYLINDRICAL_SURFACE('',#109508,0.126999993615577);
#92072=CYLINDRICAL_SURFACE('',#109510,0.127000005454888);
#92073=CYLINDRICAL_SURFACE('',#109516,0.127);
#92074=CYLINDRICAL_SURFACE('',#109519,0.126999998753446);
#92075=CYLINDRICAL_SURFACE('',#109521,0.12699999359529);
#92076=CYLINDRICAL_SURFACE('',#109525,0.127);
#92077=CYLINDRICAL_SURFACE('',#109527,0.127);
#92078=CYLINDRICAL_SURFACE('',#109530,0.127000000301916);
#92079=CYLINDRICAL_SURFACE('',#109531,0.126999999705462);
#92080=CYLINDRICAL_SURFACE('',#109535,0.127);
#92081=CYLINDRICAL_SURFACE('',#109537,0.127);
#92082=CYLINDRICAL_SURFACE('',#109541,0.127000005439802);
#92083=CYLINDRICAL_SURFACE('',#109543,0.127000001278521);
#92084=CYLINDRICAL_SURFACE('',#109545,0.127);
#92085=CYLINDRICAL_SURFACE('',#109549,0.126999993615003);
#92086=CYLINDRICAL_SURFACE('',#109551,0.12700000545229);
#92087=CYLINDRICAL_SURFACE('',#109554,0.127);
#92088=CYLINDRICAL_SURFACE('',#109557,0.126999998753605);
#92089=CYLINDRICAL_SURFACE('',#109559,0.126999993595434);
#92090=CYLINDRICAL_SURFACE('',#109563,0.127);
#92091=CYLINDRICAL_SURFACE('',#109565,0.127);
#92092=CYLINDRICAL_SURFACE('',#109568,0.127000000301634);
#92093=CYLINDRICAL_SURFACE('',#109569,0.126999999706563);
#92094=CYLINDRICAL_SURFACE('',#109573,0.127);
#92095=CYLINDRICAL_SURFACE('',#109575,0.127);
#92096=CYLINDRICAL_SURFACE('',#109579,0.127000005437472);
#92097=CYLINDRICAL_SURFACE('',#109581,0.127000001278037);
#92098=CYLINDRICAL_SURFACE('',#109584,0.127);
#92099=CYLINDRICAL_SURFACE('',#109590,0.126999993614555);
#92100=CYLINDRICAL_SURFACE('',#109592,0.127000005454137);
#92101=CYLINDRICAL_SURFACE('',#109598,0.127);
#92102=CYLINDRICAL_SURFACE('',#109601,0.126999998754154);
#92103=CYLINDRICAL_SURFACE('',#109603,0.126999993593391);
#92104=CYLINDRICAL_SURFACE('',#109607,0.127);
#92105=CYLINDRICAL_SURFACE('',#109609,0.127);
#92106=CYLINDRICAL_SURFACE('',#109612,0.12700000030181);
#92107=CYLINDRICAL_SURFACE('',#109613,0.126999999708026);
#92108=CYLINDRICAL_SURFACE('',#109617,0.127);
#92109=CYLINDRICAL_SURFACE('',#109619,0.127);
#92110=CYLINDRICAL_SURFACE('',#109623,0.12700000543711);
#92111=CYLINDRICAL_SURFACE('',#109625,0.127000001279361);
#92112=CYLINDRICAL_SURFACE('',#109628,0.127);
#92113=CYLINDRICAL_SURFACE('',#109634,0.126999993615229);
#92114=CYLINDRICAL_SURFACE('',#109636,0.127000005453427);
#92115=CYLINDRICAL_SURFACE('',#109642,0.127);
#92116=CYLINDRICAL_SURFACE('',#109645,0.126999998752725);
#92117=CYLINDRICAL_SURFACE('',#109647,0.126999993597096);
#92118=CYLINDRICAL_SURFACE('',#109651,0.127);
#92119=CYLINDRICAL_SURFACE('',#109653,0.127);
#92120=CYLINDRICAL_SURFACE('',#109656,0.127000000301725);
#92121=CYLINDRICAL_SURFACE('',#109657,0.126999999706422);
#92122=CYLINDRICAL_SURFACE('',#109661,0.127);
#92123=CYLINDRICAL_SURFACE('',#109663,0.127);
#92124=CYLINDRICAL_SURFACE('',#109667,0.127000005439341);
#92125=CYLINDRICAL_SURFACE('',#109669,0.127000001278882);
#92126=CYLINDRICAL_SURFACE('',#109672,0.127);
#92127=CYLINDRICAL_SURFACE('',#109678,0.126999993613762);
#92128=CYLINDRICAL_SURFACE('',#109680,0.127000005452003);
#92129=CYLINDRICAL_SURFACE('',#109686,0.127);
#92130=CYLINDRICAL_SURFACE('',#109689,0.126999998752492);
#92131=CYLINDRICAL_SURFACE('',#109691,0.12699999359364);
#92132=CYLINDRICAL_SURFACE('',#109695,0.127);
#92133=CYLINDRICAL_SURFACE('',#109697,0.127);
#92134=CYLINDRICAL_SURFACE('',#109700,0.127000000300672);
#92135=CYLINDRICAL_SURFACE('',#109701,0.126999999705238);
#92136=CYLINDRICAL_SURFACE('',#109705,0.127);
#92137=CYLINDRICAL_SURFACE('',#109707,0.127);
#92138=CYLINDRICAL_SURFACE('',#109711,0.127000005436153);
#92139=CYLINDRICAL_SURFACE('',#109713,0.127000001278167);
#92140=CYLINDRICAL_SURFACE('',#109716,0.127);
#92141=CYLINDRICAL_SURFACE('',#109722,0.126999993615688);
#92142=CYLINDRICAL_SURFACE('',#109724,0.127000005455986);
#92143=CYLINDRICAL_SURFACE('',#109730,0.126999999999999);
#92144=CYLINDRICAL_SURFACE('',#109733,0.126999998752203);
#92145=CYLINDRICAL_SURFACE('',#109735,0.126999993593721);
#92146=CYLINDRICAL_SURFACE('',#109739,0.126999999999999);
#92147=CYLINDRICAL_SURFACE('',#109741,0.126999999999999);
#92148=CYLINDRICAL_SURFACE('',#109744,0.127000000302232);
#92149=CYLINDRICAL_SURFACE('',#109745,0.126999999704091);
#92150=CYLINDRICAL_SURFACE('',#109749,0.127);
#92151=CYLINDRICAL_SURFACE('',#109751,0.127);
#92152=CYLINDRICAL_SURFACE('',#109755,0.127000005437327);
#92153=CYLINDRICAL_SURFACE('',#109757,0.127000001279529);
#92154=CYLINDRICAL_SURFACE('',#109760,0.127);
#92155=CYLINDRICAL_SURFACE('',#109766,0.126999993615739);
#92156=CYLINDRICAL_SURFACE('',#109768,0.127000005450327);
#92157=CYLINDRICAL_SURFACE('',#109774,0.127);
#92158=CYLINDRICAL_SURFACE('',#109777,0.126999998753158);
#92159=CYLINDRICAL_SURFACE('',#109779,0.126999993595294);
#92160=CYLINDRICAL_SURFACE('',#109783,0.127);
#92161=CYLINDRICAL_SURFACE('',#109785,0.127);
#92162=CYLINDRICAL_SURFACE('',#109788,0.12700000030154);
#92163=CYLINDRICAL_SURFACE('',#109789,0.126999999706558);
#92164=CYLINDRICAL_SURFACE('',#109793,0.127);
#92165=CYLINDRICAL_SURFACE('',#109795,0.127);
#92166=CYLINDRICAL_SURFACE('',#109799,0.127000005438623);
#92167=CYLINDRICAL_SURFACE('',#109801,0.127000001278666);
#92168=CYLINDRICAL_SURFACE('',#109804,0.127);
#92169=CYLINDRICAL_SURFACE('',#109810,0.126999993616145);
#92170=CYLINDRICAL_SURFACE('',#109812,0.127000005453625);
#92171=CYLINDRICAL_SURFACE('',#109818,0.127000000000001);
#92172=CYLINDRICAL_SURFACE('',#109821,0.126999998751993);
#92173=CYLINDRICAL_SURFACE('',#109823,0.126999993594714);
#92174=CYLINDRICAL_SURFACE('',#109827,0.127000000000001);
#92175=CYLINDRICAL_SURFACE('',#109829,0.127000000000001);
#92176=CYLINDRICAL_SURFACE('',#109832,0.127000000299019);
#92177=CYLINDRICAL_SURFACE('',#109833,0.126999999706658);
#92178=CYLINDRICAL_SURFACE('',#109837,0.127);
#92179=CYLINDRICAL_SURFACE('',#109839,0.127);
#92180=CYLINDRICAL_SURFACE('',#109843,0.127000005436539);
#92181=CYLINDRICAL_SURFACE('',#109845,0.127000001278572);
#92182=CYLINDRICAL_SURFACE('',#109848,0.127);
#92183=CYLINDRICAL_SURFACE('',#109854,0.126999993618423);
#92184=CYLINDRICAL_SURFACE('',#109856,0.127000005451247);
#92185=CYLINDRICAL_SURFACE('',#109862,0.127);
#92186=CYLINDRICAL_SURFACE('',#109865,0.126999998752971);
#92187=CYLINDRICAL_SURFACE('',#109867,0.126999993593068);
#92188=CYLINDRICAL_SURFACE('',#109871,0.127);
#92189=CYLINDRICAL_SURFACE('',#109873,0.127);
#92190=CYLINDRICAL_SURFACE('',#109876,0.127000000302318);
#92191=CYLINDRICAL_SURFACE('',#109877,0.126999999707401);
#92192=CYLINDRICAL_SURFACE('',#109881,0.127);
#92193=CYLINDRICAL_SURFACE('',#109883,0.127);
#92194=CYLINDRICAL_SURFACE('',#109887,0.127000005436974);
#92195=CYLINDRICAL_SURFACE('',#109889,0.127000001280052);
#92196=CYLINDRICAL_SURFACE('',#109892,0.127);
#92197=CYLINDRICAL_SURFACE('',#109898,0.126999993617258);
#92198=CYLINDRICAL_SURFACE('',#109900,0.127000005450994);
#92199=CYLINDRICAL_SURFACE('',#109906,0.127);
#92200=CYLINDRICAL_SURFACE('',#109909,0.126999998752549);
#92201=CYLINDRICAL_SURFACE('',#109911,0.126999993591476);
#92202=CYLINDRICAL_SURFACE('',#109915,0.127);
#92203=CYLINDRICAL_SURFACE('',#109917,0.127);
#92204=CYLINDRICAL_SURFACE('',#109920,0.127000000302013);
#92205=CYLINDRICAL_SURFACE('',#109921,0.12699999970701);
#92206=CYLINDRICAL_SURFACE('',#109925,0.127);
#92207=CYLINDRICAL_SURFACE('',#109927,0.127);
#92208=CYLINDRICAL_SURFACE('',#109931,0.127000005437229);
#92209=CYLINDRICAL_SURFACE('',#109933,0.127000001279199);
#92210=CYLINDRICAL_SURFACE('',#109936,0.127);
#92211=CYLINDRICAL_SURFACE('',#109942,0.126999993615815);
#92212=CYLINDRICAL_SURFACE('',#109944,0.127000005452559);
#92213=CYLINDRICAL_SURFACE('',#109950,0.127000000000001);
#92214=CYLINDRICAL_SURFACE('',#109953,0.12699999875498);
#92215=CYLINDRICAL_SURFACE('',#109955,0.126999993591178);
#92216=CYLINDRICAL_SURFACE('',#109959,0.127000000000001);
#92217=CYLINDRICAL_SURFACE('',#109961,0.127000000000001);
#92218=CYLINDRICAL_SURFACE('',#109964,0.127000000300906);
#92219=CYLINDRICAL_SURFACE('',#109965,0.126999999707296);
#92220=CYLINDRICAL_SURFACE('',#109969,0.127);
#92221=CYLINDRICAL_SURFACE('',#109971,0.127);
#92222=CYLINDRICAL_SURFACE('',#109975,0.127000005438382);
#92223=CYLINDRICAL_SURFACE('',#109977,0.127000001277859);
#92224=CYLINDRICAL_SURFACE('',#109980,0.127);
#92225=CYLINDRICAL_SURFACE('',#109986,0.126999993613277);
#92226=CYLINDRICAL_SURFACE('',#109988,0.127000005457096);
#92227=CYLINDRICAL_SURFACE('',#109994,0.127000000000003);
#92228=CYLINDRICAL_SURFACE('',#109997,0.126999998755077);
#92229=CYLINDRICAL_SURFACE('',#109999,0.126999993597932);
#92230=CYLINDRICAL_SURFACE('',#110003,0.127000000000003);
#92231=CYLINDRICAL_SURFACE('',#110005,0.127000000000003);
#92232=CYLINDRICAL_SURFACE('',#110008,0.127000000302244);
#92233=CYLINDRICAL_SURFACE('',#110009,0.126999999705334);
#92234=CYLINDRICAL_SURFACE('',#110013,0.127);
#92235=CYLINDRICAL_SURFACE('',#110015,0.127);
#92236=CYLINDRICAL_SURFACE('',#110019,0.127000005437731);
#92237=CYLINDRICAL_SURFACE('',#110021,0.127000001278277);
#92238=CYLINDRICAL_SURFACE('',#110024,0.127);
#92239=CYLINDRICAL_SURFACE('',#110030,0.126999993613041);
#92240=CYLINDRICAL_SURFACE('',#110032,0.12700000545555);
#92241=CYLINDRICAL_SURFACE('',#110038,0.127000000000001);
#92242=CYLINDRICAL_SURFACE('',#110041,0.126999998754099);
#92243=CYLINDRICAL_SURFACE('',#110043,0.126999993597918);
#92244=CYLINDRICAL_SURFACE('',#110047,0.127000000000001);
#92245=CYLINDRICAL_SURFACE('',#110049,0.127000000000001);
#92246=CYLINDRICAL_SURFACE('',#110052,0.127000000302057);
#92247=CYLINDRICAL_SURFACE('',#110053,0.126999999706135);
#92248=CYLINDRICAL_SURFACE('',#110057,0.127);
#92249=CYLINDRICAL_SURFACE('',#110059,0.127);
#92250=CYLINDRICAL_SURFACE('',#110063,0.12700000543804);
#92251=CYLINDRICAL_SURFACE('',#110065,0.127000001278899);
#92252=CYLINDRICAL_SURFACE('',#110068,0.127);
#92253=CYLINDRICAL_SURFACE('',#110074,0.126999993615389);
#92254=CYLINDRICAL_SURFACE('',#110076,0.127000005454568);
#92255=CYLINDRICAL_SURFACE('',#110082,0.127);
#92256=CYLINDRICAL_SURFACE('',#110085,0.126999998752967);
#92257=CYLINDRICAL_SURFACE('',#110087,0.126999993594804);
#92258=CYLINDRICAL_SURFACE('',#110091,0.127);
#92259=CYLINDRICAL_SURFACE('',#110093,0.127);
#92260=CYLINDRICAL_SURFACE('',#110096,0.127000000301654);
#92261=CYLINDRICAL_SURFACE('',#110097,0.126999999706781);
#92262=CYLINDRICAL_SURFACE('',#110101,0.127);
#92263=CYLINDRICAL_SURFACE('',#110103,0.127);
#92264=CYLINDRICAL_SURFACE('',#110107,0.127000005439673);
#92265=CYLINDRICAL_SURFACE('',#110109,0.127000001277602);
#92266=CYLINDRICAL_SURFACE('',#110112,0.127);
#92267=CYLINDRICAL_SURFACE('',#110118,0.126999993615679);
#92268=CYLINDRICAL_SURFACE('',#110120,0.127000005451513);
#92269=CYLINDRICAL_SURFACE('',#110126,0.127000000000001);
#92270=CYLINDRICAL_SURFACE('',#110129,0.126999998752155);
#92271=CYLINDRICAL_SURFACE('',#110131,0.126999993594889);
#92272=CYLINDRICAL_SURFACE('',#110135,0.127000000000001);
#92273=CYLINDRICAL_SURFACE('',#110137,0.127000000000001);
#92274=CYLINDRICAL_SURFACE('',#110140,0.12700000030033);
#92275=CYLINDRICAL_SURFACE('',#110141,0.126999999705493);
#92276=CYLINDRICAL_SURFACE('',#110145,0.127);
#92277=CYLINDRICAL_SURFACE('',#110147,0.127);
#92278=CYLINDRICAL_SURFACE('',#110151,0.127000005438186);
#92279=CYLINDRICAL_SURFACE('',#110153,0.127000001279353);
#92280=CYLINDRICAL_SURFACE('',#110156,0.127);
#92281=CYLINDRICAL_SURFACE('',#110162,0.126999993616156);
#92282=CYLINDRICAL_SURFACE('',#110164,0.127000005452965);
#92283=CYLINDRICAL_SURFACE('',#110170,0.126999999999999);
#92284=CYLINDRICAL_SURFACE('',#110173,0.126999998753501);
#92285=CYLINDRICAL_SURFACE('',#110175,0.126999993594368);
#92286=CYLINDRICAL_SURFACE('',#110179,0.126999999999999);
#92287=CYLINDRICAL_SURFACE('',#110181,0.126999999999999);
#92288=CYLINDRICAL_SURFACE('',#110184,0.127000000302371);
#92289=CYLINDRICAL_SURFACE('',#110198,65.254);
#92290=CYLINDRICAL_SURFACE('',#110200,68.75);
#92291=CYLINDRICAL_SURFACE('',#110201,72.53);
#92292=CYLINDRICAL_SURFACE('',#110215,65.);
#92293=CYLINDRICAL_SURFACE('',#110217,65.254);
#92294=CYLINDRICAL_SURFACE('',#110259,2.54);
#92295=CYLINDRICAL_SURFACE('',#110261,2.54);
#92296=CYLINDRICAL_SURFACE('',#110266,72.53);
#92297=CYLINDRICAL_SURFACE('',#110269,8.4455);
#92298=CYLINDRICAL_SURFACE('',#110272,8.4455);
#92299=CYLINDRICAL_SURFACE('',#110275,8.4455);
#92300=CYLINDRICAL_SURFACE('',#110278,8.4455);
#92301=CYLINDRICAL_SURFACE('',#110281,80.);
#92302=CYLINDRICAL_SURFACE('',#110292,25.);
#92303=CYLINDRICAL_SURFACE('',#110297,25.);
#92304=CYLINDRICAL_SURFACE('',#110305,25.);
#92305=CYLINDRICAL_SURFACE('',#110309,25.);
#92306=CYLINDRICAL_SURFACE('',#110314,24.492);
#92307=CYLINDRICAL_SURFACE('',#110318,24.492);
#92308=CYLINDRICAL_SURFACE('',#110322,24.492);
#92309=CYLINDRICAL_SURFACE('',#110326,24.492);
#92310=CYLINDRICAL_SURFACE('',#110336,81.2699999999993);
#92311=CYLINDRICAL_SURFACE('',#110338,80.);
#92312=CYLINDRICAL_SURFACE('',#110348,80.);
#92313=CYLINDRICAL_SURFACE('',#110353,80.);
#92314=CYLINDRICAL_SURFACE('',#110358,80.);
#92315=CYLINDRICAL_SURFACE('',#110396,2.54);
#92316=CYLINDRICAL_SURFACE('',#110399,2.54);
#92317=CYLINDRICAL_SURFACE('',#110402,2.54);
#92318=CYLINDRICAL_SURFACE('',#110404,2.54);
#92319=CYLINDRICAL_SURFACE('',#110406,2.54);
#92320=CYLINDRICAL_SURFACE('',#110408,2.54);
#92321=CYLINDRICAL_SURFACE('',#110412,1.905);
#92322=CYLINDRICAL_SURFACE('',#110419,1.905);
#92323=CYLINDRICAL_SURFACE('',#110421,1.905);
#92324=CYLINDRICAL_SURFACE('',#110424,1.905);
#92325=CYLINDRICAL_SURFACE('',#110428,1.905);
#92326=CYLINDRICAL_SURFACE('',#110430,1.905);
#92327=CYLINDRICAL_SURFACE('',#110433,1.905);
#92328=CYLINDRICAL_SURFACE('',#110438,1.905);
#92329=CYLINDRICAL_SURFACE('',#110440,1.905);
#92330=CYLINDRICAL_SURFACE('',#110443,1.905);
#92331=CYLINDRICAL_SURFACE('',#110447,1.905);
#92332=CYLINDRICAL_SURFACE('',#110449,1.27);
#92333=CYLINDRICAL_SURFACE('',#110453,1.27);
#92334=CYLINDRICAL_SURFACE('',#110454,1.27);
#92335=CYLINDRICAL_SURFACE('',#110455,1.27);
#92336=CYLINDRICAL_SURFACE('',#110456,1.27);
#92337=CYLINDRICAL_SURFACE('',#110457,1.27);
#92338=CYLINDRICAL_SURFACE('',#110458,1.27);
#92339=CYLINDRICAL_SURFACE('',#110462,1.27);
#92340=CYLINDRICAL_SURFACE('',#110478,1.27);
#92341=CYLINDRICAL_SURFACE('',#110481,1.27);
#92342=CYLINDRICAL_SURFACE('',#110504,2.54);
#92343=CYLINDRICAL_SURFACE('',#110507,2.54);
#92344=CYLINDRICAL_SURFACE('',#110523,66.0360441972308);
#92345=CYLINDRICAL_SURFACE('',#110524,1.27);
#92346=CYLINDRICAL_SURFACE('',#110527,1.905);
#92347=CYLINDRICAL_SURFACE('',#110541,1.27);
#92348=CYLINDRICAL_SURFACE('',#110542,66.0995441972308);
#92349=CYLINDRICAL_SURFACE('',#110544,66.4805441972308);
#92350=CYLINDRICAL_SURFACE('',#110570,56.875);
#92351=CYLINDRICAL_SURFACE('',#110575,51.27);
#92352=CYLINDRICAL_SURFACE('',#110577,50.);
#92353=CYLINDRICAL_SURFACE('',#110579,65.);
#92354=CYLINDRICAL_SURFACE('',#110587,4.7227367061318);
#92355=CYLINDRICAL_SURFACE('',#110589,4.7227367061318);
#92356=CYLINDRICAL_SURFACE('',#110590,4.7227367061318);
#92357=CYLINDRICAL_SURFACE('',#110591,4.7227367061318);
#92358=CYLINDRICAL_SURFACE('',#110592,4.7227367061318);
#92359=CYLINDRICAL_SURFACE('',#110593,4.7227367061318);
#92360=CYLINDRICAL_SURFACE('',#110594,4.74980000000001);
#92361=CYLINDRICAL_SURFACE('',#110596,4.74980000000001);
#92362=CYLINDRICAL_SURFACE('',#110598,4.74980000000001);
#92363=CYLINDRICAL_SURFACE('',#110599,4.74980000000001);
#92364=CYLINDRICAL_SURFACE('',#110600,4.74980000000001);
#92365=CYLINDRICAL_SURFACE('',#110601,4.74980000000001);
#92366=CYLINDRICAL_SURFACE('',#110602,4.74980000000001);
#92367=CYLINDRICAL_SURFACE('',#110603,4.74980000000001);
#92368=CYLINDRICAL_SURFACE('',#110616,4.74980000000001);
#92369=CYLINDRICAL_SURFACE('',#110638,4.7227367061318);
#92370=CYLINDRICAL_SURFACE('',#110639,4.72273670613179);
#92371=CYLINDRICAL_SURFACE('',#110641,4.72273670613179);
#92372=CYLINDRICAL_SURFACE('',#110642,4.72273670613179);
#92373=CYLINDRICAL_SURFACE('',#110643,4.72273670613179);
#92374=CYLINDRICAL_SURFACE('',#110644,4.72273670613179);
#92375=CYLINDRICAL_SURFACE('',#110645,4.72273670613179);
#92376=CYLINDRICAL_SURFACE('',#110646,4.74980000000001);
#92377=CYLINDRICAL_SURFACE('',#110648,4.74980000000001);
#92378=CYLINDRICAL_SURFACE('',#110650,4.74980000000001);
#92379=CYLINDRICAL_SURFACE('',#110651,4.74980000000001);
#92380=CYLINDRICAL_SURFACE('',#110652,4.74980000000001);
#92381=CYLINDRICAL_SURFACE('',#110653,4.74980000000001);
#92382=CYLINDRICAL_SURFACE('',#110654,4.74980000000001);
#92383=CYLINDRICAL_SURFACE('',#110655,4.74980000000001);
#92384=CYLINDRICAL_SURFACE('',#110668,4.74980000000001);
#92385=CYLINDRICAL_SURFACE('',#110690,4.72273670613179);
#92386=CYLINDRICAL_SURFACE('',#110705,50.);
#92387=CYLINDRICAL_SURFACE('',#110706,4.7625);
#92388=CYLINDRICAL_SURFACE('',#110707,4.7625);
#92389=CYLINDRICAL_SURFACE('',#110708,40.);
#92390=CYLINDRICAL_SURFACE('',#110711,65.0000000000002);
#92391=CYLINDRICAL_SURFACE('',#110714,56.875);
#92392=CYLINDRICAL_SURFACE('',#110722,76.4577478255888);
#92393=CYLINDRICAL_SURFACE('',#110724,66.9885441972308);
#92394=CYLINDRICAL_SURFACE('',#110727,70.625);
#92395=CYLINDRICAL_SURFACE('',#110730,76.5847478255888);
#92396=CYLINDRICAL_SURFACE('',#110733,8.4455);
#92397=CYLINDRICAL_SURFACE('',#110736,8.4455);
#92398=CYLINDRICAL_SURFACE('',#110739,8.4455);
#92399=CYLINDRICAL_SURFACE('',#110742,8.4455);
#92400=CYLINDRICAL_SURFACE('',#110745,7.9375);
#92401=CYLINDRICAL_SURFACE('',#110748,7.9375);
#92402=CYLINDRICAL_SURFACE('',#110751,7.9375);
#92403=CYLINDRICAL_SURFACE('',#110754,7.9375);
#92404=CYLINDRICAL_SURFACE('',#110757,24.492);
#92405=CYLINDRICAL_SURFACE('',#110761,24.492);
#92406=CYLINDRICAL_SURFACE('',#110765,24.492);
#92407=CYLINDRICAL_SURFACE('',#110769,24.492);
#92408=CYLINDRICAL_SURFACE('',#110787,25.);
#92409=CYLINDRICAL_SURFACE('',#110790,25.);
#92410=CYLINDRICAL_SURFACE('',#110793,25.);
#92411=CYLINDRICAL_SURFACE('',#110796,25.);
#92412=CYLINDRICAL_SURFACE('',#110802,0.761999999999999);
#92413=CYLINDRICAL_SURFACE('',#110804,0.762);
#92414=CYLINDRICAL_SURFACE('',#110810,0.762);
#92415=CYLINDRICAL_SURFACE('',#110812,0.762);
#92416=CYLINDRICAL_SURFACE('',#110816,66.9885441972308);
#92417=CYLINDRICAL_SURFACE('',#110825,73.6560441972308);
#92418=CYLINDRICAL_SURFACE('',#110831,73.6560441972308);
#92419=CYLINDRICAL_SURFACE('',#110839,3.4);
#92420=CYLINDRICAL_SURFACE('',#110843,7.49999999999995);
#92421=CYLINDRICAL_SURFACE('',#110845,7.49999999999995);
#92422=CYLINDRICAL_SURFACE('',#110847,7.49999999999995);
#92423=CYLINDRICAL_SURFACE('',#110849,7.49999999999995);
#92424=CYLINDRICAL_SURFACE('',#110851,7.49999999999995);
#92425=CYLINDRICAL_SURFACE('',#110853,7.49999999999995);
#92426=CYLINDRICAL_SURFACE('',#110855,15.);
#92427=CYLINDRICAL_SURFACE('',#110897,5.);
#92428=CYLINDRICAL_SURFACE('',#110900,5.);
#92429=CYLINDRICAL_SURFACE('',#110903,5.);
#92430=CYLINDRICAL_SURFACE('',#110906,5.);
#92431=CYLINDRICAL_SURFACE('',#110911,3.);
#92432=CYLINDRICAL_SURFACE('',#110913,3.);
#92433=CYLINDRICAL_SURFACE('',#110917,3.);
#92434=CYLINDRICAL_SURFACE('',#110919,3.);
#92435=CYLINDRICAL_SURFACE('',#110921,5.);
#92436=CYLINDRICAL_SURFACE('',#110924,5.);
#92437=CYLINDRICAL_SURFACE('',#110927,5.);
#92438=CYLINDRICAL_SURFACE('',#110930,5.);
#92439=CYLINDRICAL_SURFACE('',#110943,5.);
#92440=CYLINDRICAL_SURFACE('',#110945,5.);
#92441=CYLINDRICAL_SURFACE('',#110951,5.);
#92442=CYLINDRICAL_SURFACE('',#110953,5.);
#92443=CYLINDRICAL_SURFACE('',#110960,5.);
#92444=CYLINDRICAL_SURFACE('',#110962,5.);
#92445=CYLINDRICAL_SURFACE('',#110970,5.);
#92446=CYLINDRICAL_SURFACE('',#110972,5.);
#92447=CYLINDRICAL_SURFACE('',#110987,6.3);
#92448=CYLINDRICAL_SURFACE('',#111000,9.92159999999999);
#92449=CYLINDRICAL_SURFACE('',#111003,6.3);
#92450=CYLINDRICAL_SURFACE('',#111006,9.92159999999999);
#92451=CYLINDRICAL_SURFACE('',#111009,6.29999999999999);
#92452=CYLINDRICAL_SURFACE('',#111012,9.92159999999999);
#92453=CYLINDRICAL_SURFACE('',#111015,6.29999999999999);
#92454=CYLINDRICAL_SURFACE('',#111018,9.9216);
#92455=CYLINDRICAL_SURFACE('',#111027,1.8);
#92456=CYLINDRICAL_SURFACE('',#111030,1.8);
#92457=CYLINDRICAL_SURFACE('',#111033,1.8);
#92458=CYLINDRICAL_SURFACE('',#111036,1.8);
#92459=CYLINDRICAL_SURFACE('',#111089,2.7);
#92460=CYLINDRICAL_SURFACE('',#111091,2.69999999999999);
#92461=CYLINDRICAL_SURFACE('',#111093,2.69999999999999);
#92462=CYLINDRICAL_SURFACE('',#111097,2.7);
#92463=CYLINDRICAL_SURFACE('',#111099,2.7);
#92464=CYLINDRICAL_SURFACE('',#111101,2.7);
#92465=CYLINDRICAL_SURFACE('',#111103,2.7);
#92466=CYLINDRICAL_SURFACE('',#111105,2.69999999999999);
#92467=CYLINDRICAL_SURFACE('',#111107,2.69999999999999);
#92468=CYLINDRICAL_SURFACE('',#111111,2.7);
#92469=CYLINDRICAL_SURFACE('',#111113,2.7);
#92470=CYLINDRICAL_SURFACE('',#111115,2.7);
#92471=CYLINDRICAL_SURFACE('',#111117,2.7);
#92472=CYLINDRICAL_SURFACE('',#111119,2.7);
#92473=CYLINDRICAL_SURFACE('',#111121,2.69999999999999);
#92474=CYLINDRICAL_SURFACE('',#111125,2.69999999999999);
#92475=CYLINDRICAL_SURFACE('',#111127,2.7);
#92476=CYLINDRICAL_SURFACE('',#111129,2.7);
#92477=CYLINDRICAL_SURFACE('',#111131,2.7);
#92478=CYLINDRICAL_SURFACE('',#111133,2.69999999999999);
#92479=CYLINDRICAL_SURFACE('',#111135,2.7);
#92480=CYLINDRICAL_SURFACE('',#111139,2.69999999999999);
#92481=CYLINDRICAL_SURFACE('',#111141,2.7);
#92482=CYLINDRICAL_SURFACE('',#111143,2.7);
#92483=CYLINDRICAL_SURFACE('',#111145,6.29999999999999);
#92484=CYLINDRICAL_SURFACE('',#111157,6.3);
#92485=CYLINDRICAL_SURFACE('',#111160,9.92159999999999);
#92486=CYLINDRICAL_SURFACE('',#111163,6.3);
#92487=CYLINDRICAL_SURFACE('',#111166,9.92159999999999);
#92488=CYLINDRICAL_SURFACE('',#111170,9.92159999999999);
#92489=CYLINDRICAL_SURFACE('',#111173,6.29999999999999);
#92490=CYLINDRICAL_SURFACE('',#111176,9.9216);
#92491=CYLINDRICAL_SURFACE('',#111185,1.8);
#92492=CYLINDRICAL_SURFACE('',#111188,1.8);
#92493=CYLINDRICAL_SURFACE('',#111191,1.8);
#92494=CYLINDRICAL_SURFACE('',#111194,1.8);
#92495=CYLINDRICAL_SURFACE('',#111197,6.29999999999999);
#92496=CYLINDRICAL_SURFACE('',#111209,6.3);
#92497=CYLINDRICAL_SURFACE('',#111212,9.92159999999999);
#92498=CYLINDRICAL_SURFACE('',#111215,6.3);
#92499=CYLINDRICAL_SURFACE('',#111218,9.92159999999999);
#92500=CYLINDRICAL_SURFACE('',#111221,6.29999999999999);
#92501=CYLINDRICAL_SURFACE('',#111224,9.92159999999999);
#92502=CYLINDRICAL_SURFACE('',#111228,9.9216);
#92503=CYLINDRICAL_SURFACE('',#111237,1.8);
#92504=CYLINDRICAL_SURFACE('',#111240,1.8);
#92505=CYLINDRICAL_SURFACE('',#111243,1.8);
#92506=CYLINDRICAL_SURFACE('',#111246,1.8);
#92507=CYLINDRICAL_SURFACE('',#111249,6.29999999999999);
#92508=CYLINDRICAL_SURFACE('',#111261,6.3);
#92509=CYLINDRICAL_SURFACE('',#111264,9.92159999999999);
#92510=CYLINDRICAL_SURFACE('',#111267,6.3);
#92511=CYLINDRICAL_SURFACE('',#111270,9.92159999999999);
#92512=CYLINDRICAL_SURFACE('',#111273,6.29999999999999);
#92513=CYLINDRICAL_SURFACE('',#111276,9.92159999999999);
#92514=CYLINDRICAL_SURFACE('',#111280,9.9216);
#92515=CYLINDRICAL_SURFACE('',#111289,1.8);
#92516=CYLINDRICAL_SURFACE('',#111292,1.8);
#92517=CYLINDRICAL_SURFACE('',#111295,1.8);
#92518=CYLINDRICAL_SURFACE('',#111298,1.8);
#92519=CYLINDRICAL_SURFACE('',#111306,0.899999999999998);
#92520=CYLINDRICAL_SURFACE('',#111310,0.899999999999998);
#92521=CYLINDRICAL_SURFACE('',#111314,0.899999999999998);
#92522=CYLINDRICAL_SURFACE('',#111318,0.899999999999991);
#92523=CYLINDRICAL_SURFACE('',#111329,0.899999999999995);
#92524=CYLINDRICAL_SURFACE('',#111333,0.900000000000001);
#92525=CYLINDRICAL_SURFACE('',#111337,0.899999999999996);
#92526=CYLINDRICAL_SURFACE('',#111341,0.899999999999998);
#92527=CYLINDRICAL_SURFACE('',#111348,0.899999999999998);
#92528=CYLINDRICAL_SURFACE('',#111352,0.899999999999998);
#92529=CYLINDRICAL_SURFACE('',#111356,0.899999999999991);
#92530=CYLINDRICAL_SURFACE('',#111360,0.899999999999998);
#92531=CYLINDRICAL_SURFACE('',#111367,3.65760000000007);
#92532=CYLINDRICAL_SURFACE('',#111374,0.899999999999991);
#92533=CYLINDRICAL_SURFACE('',#111378,0.899999999999998);
#92534=CYLINDRICAL_SURFACE('',#111382,0.899999999999998);
#92535=CYLINDRICAL_SURFACE('',#111386,0.899999999999998);
#92536=CYLINDRICAL_SURFACE('',#111393,0.899999999999998);
#92537=CYLINDRICAL_SURFACE('',#111397,0.899999999999998);
#92538=CYLINDRICAL_SURFACE('',#111401,0.899999999999998);
#92539=CYLINDRICAL_SURFACE('',#111405,0.899999999999991);
#92540=CYLINDRICAL_SURFACE('',#111415,0.899999999999995);
#92541=CYLINDRICAL_SURFACE('',#111419,0.900000000000001);
#92542=CYLINDRICAL_SURFACE('',#111423,0.899999999999996);
#92543=CYLINDRICAL_SURFACE('',#111427,0.899999999999998);
#92544=CYLINDRICAL_SURFACE('',#111434,0.899999999999998);
#92545=CYLINDRICAL_SURFACE('',#111438,0.899999999999998);
#92546=CYLINDRICAL_SURFACE('',#111442,0.899999999999991);
#92547=CYLINDRICAL_SURFACE('',#111446,0.899999999999998);
#92548=CYLINDRICAL_SURFACE('',#111453,3.65760000000007);
#92549=CYLINDRICAL_SURFACE('',#111460,0.899999999999991);
#92550=CYLINDRICAL_SURFACE('',#111464,0.899999999999998);
#92551=CYLINDRICAL_SURFACE('',#111468,0.899999999999998);
#92552=CYLINDRICAL_SURFACE('',#111472,0.899999999999998);
#92553=CYLINDRICAL_SURFACE('',#111479,0.899999999999998);
#92554=CYLINDRICAL_SURFACE('',#111483,0.899999999999996);
#92555=CYLINDRICAL_SURFACE('',#111487,0.900000000000001);
#92556=CYLINDRICAL_SURFACE('',#111491,0.899999999999995);
#92557=CYLINDRICAL_SURFACE('',#111501,0.899999999999991);
#92558=CYLINDRICAL_SURFACE('',#111505,0.899999999999998);
#92559=CYLINDRICAL_SURFACE('',#111509,0.899999999999998);
#92560=CYLINDRICAL_SURFACE('',#111513,0.899999999999998);
#92561=CYLINDRICAL_SURFACE('',#111520,0.899999999999998);
#92562=CYLINDRICAL_SURFACE('',#111524,0.899999999999998);
#92563=CYLINDRICAL_SURFACE('',#111528,0.899999999999991);
#92564=CYLINDRICAL_SURFACE('',#111532,0.899999999999998);
#92565=CYLINDRICAL_SURFACE('',#111539,3.65760000000007);
#92566=CYLINDRICAL_SURFACE('',#111546,0.899999999999991);
#92567=CYLINDRICAL_SURFACE('',#111550,0.899999999999998);
#92568=CYLINDRICAL_SURFACE('',#111554,0.899999999999998);
#92569=CYLINDRICAL_SURFACE('',#111558,0.899999999999998);
#92570=CYLINDRICAL_SURFACE('',#111565,0.899999999999998);
#92571=CYLINDRICAL_SURFACE('',#111569,0.899999999999996);
#92572=CYLINDRICAL_SURFACE('',#111573,0.900000000000001);
#92573=CYLINDRICAL_SURFACE('',#111577,0.899999999999995);
#92574=CYLINDRICAL_SURFACE('',#111586,0.899999999999991);
#92575=CYLINDRICAL_SURFACE('',#111590,0.899999999999998);
#92576=CYLINDRICAL_SURFACE('',#111594,0.899999999999998);
#92577=CYLINDRICAL_SURFACE('',#111598,0.899999999999998);
#92578=CYLINDRICAL_SURFACE('',#111605,0.899999999999998);
#92579=CYLINDRICAL_SURFACE('',#111609,0.899999999999998);
#92580=CYLINDRICAL_SURFACE('',#111613,0.899999999999991);
#92581=CYLINDRICAL_SURFACE('',#111617,0.899999999999998);
#92582=CYLINDRICAL_SURFACE('',#111624,3.65760000000007);
#92583=CYLINDRICAL_SURFACE('',#111631,0.899999999999991);
#92584=CYLINDRICAL_SURFACE('',#111635,0.899999999999998);
#92585=CYLINDRICAL_SURFACE('',#111639,0.899999999999998);
#92586=CYLINDRICAL_SURFACE('',#111643,0.899999999999998);
#92587=ADVANCED_FACE('',(#7614),#90293,.F.);
#92588=ADVANCED_FACE('',(#7615),#90294,.F.);
#92589=ADVANCED_FACE('',(#7616),#90295,.F.);
#92590=ADVANCED_FACE('',(#7617),#90296,.F.);
#92591=ADVANCED_FACE('',(#7618),#6446,.T.);
#92592=ADVANCED_FACE('',(#7619),#6447,.T.);
#92593=ADVANCED_FACE('',(#7620),#6448,.T.);
#92594=ADVANCED_FACE('',(#7621),#6449,.T.);
#92595=ADVANCED_FACE('',(#7622,#6322),#6450,.T.);
#92596=ADVANCED_FACE('',(#7623),#6451,.T.);
#92597=ADVANCED_FACE('',(#7624),#6452,.T.);
#92598=ADVANCED_FACE('',(#7625),#6453,.T.);
#92599=ADVANCED_FACE('',(#7626),#6454,.T.);
#92600=ADVANCED_FACE('',(#7627),#6455,.F.);
#92601=ADVANCED_FACE('',(#7628),#6456,.F.);
#92602=ADVANCED_FACE('',(#7629),#6457,.F.);
#92603=ADVANCED_FACE('',(#7630),#6458,.F.);
#92604=ADVANCED_FACE('',(#7631),#6459,.F.);
#92605=ADVANCED_FACE('',(#7632),#6460,.F.);
#92606=ADVANCED_FACE('',(#7633),#6461,.F.);
#92607=ADVANCED_FACE('',(#7634),#6462,.F.);
#92608=ADVANCED_FACE('',(#7635),#6463,.F.);
#92609=ADVANCED_FACE('',(#7636),#6464,.F.);
#92610=ADVANCED_FACE('',(#7637),#6465,.F.);
#92611=ADVANCED_FACE('',(#7638),#6466,.F.);
#92612=ADVANCED_FACE('',(#7639,#6323,#6324,#6325,#6326,#6327),#6467,.F.);
#92613=ADVANCED_FACE('',(#7640,#6328,#6329,#6330,#6331,#6332),#6468,.T.);
#92614=ADVANCED_FACE('',(#7641),#6469,.F.);
#92615=ADVANCED_FACE('',(#7642),#6470,.F.);
#92616=ADVANCED_FACE('',(#7643),#6471,.F.);
#92617=ADVANCED_FACE('',(#7644),#6472,.F.);
#92618=ADVANCED_FACE('',(#7645),#90297,.T.);
#92619=ADVANCED_FACE('',(#7646),#90298,.T.);
#92620=ADVANCED_FACE('',(#7647),#90299,.T.);
#92621=ADVANCED_FACE('',(#7648),#90300,.T.);
#92622=ADVANCED_FACE('',(#7649),#5529,.T.);
#92623=ADVANCED_FACE('',(#7650),#90301,.T.);
#92624=ADVANCED_FACE('',(#7651),#90302,.T.);
#92625=ADVANCED_FACE('',(#7652),#5530,.T.);
#92626=ADVANCED_FACE('',(#7653),#5531,.T.);
#92627=ADVANCED_FACE('',(#7654),#90303,.T.);
#92628=ADVANCED_FACE('',(#7655),#90304,.T.);
#92629=ADVANCED_FACE('',(#7656),#5532,.T.);
#92630=ADVANCED_FACE('',(#7657),#5533,.T.);
#92631=ADVANCED_FACE('',(#7658),#5534,.T.);
#92632=ADVANCED_FACE('',(#7659),#90305,.F.);
#92633=ADVANCED_FACE('',(#7660),#90306,.F.);
#92634=ADVANCED_FACE('',(#7661),#90307,.F.);
#92635=ADVANCED_FACE('',(#7662),#90308,.F.);
#92636=ADVANCED_FACE('',(#7663,#6333,#6334,#6335),#90309,.T.);
#92637=ADVANCED_FACE('',(#7664,#6336,#6337,#6338),#90310,.F.);
#92638=ADVANCED_FACE('',(#7665,#6339),#6473,.T.);
#92639=ADVANCED_FACE('',(#7666,#6340),#6474,.T.);
#92640=ADVANCED_FACE('',(#7667),#90311,.T.);
#92641=ADVANCED_FACE('',(#7668),#90312,.T.);
#92642=ADVANCED_FACE('',(#7669),#90313,.T.);
#92643=ADVANCED_FACE('',(#7670),#90314,.T.);
#92644=ADVANCED_FACE('',(#7671),#90315,.T.);
#92645=ADVANCED_FACE('',(#7672),#90316,.T.);
#92646=ADVANCED_FACE('',(#7673),#90317,.T.);
#92647=ADVANCED_FACE('',(#7674),#90318,.T.);
#92648=ADVANCED_FACE('',(#7675,#6341,#6342),#90319,.T.);
#92649=ADVANCED_FACE('',(#7676,#6343),#90320,.T.);
#92650=ADVANCED_FACE('',(#7677),#90321,.T.);
#92651=ADVANCED_FACE('',(#7678),#90322,.T.);
#92652=ADVANCED_FACE('',(#7679),#90323,.T.);
#92653=ADVANCED_FACE('',(#7680),#90324,.T.);
#92654=ADVANCED_FACE('',(#7681),#90325,.T.);
#92655=ADVANCED_FACE('',(#7682),#90326,.T.);
#92656=ADVANCED_FACE('',(#7683),#90327,.T.);
#92657=ADVANCED_FACE('',(#7684),#90328,.T.);
#92658=ADVANCED_FACE('',(#7685),#90329,.T.);
#92659=ADVANCED_FACE('',(#7686),#90330,.T.);
#92660=ADVANCED_FACE('',(#7687),#90331,.T.);
#92661=ADVANCED_FACE('',(#7688),#90332,.T.);
#92662=ADVANCED_FACE('',(#7689),#90333,.T.);
#92663=ADVANCED_FACE('',(#7690),#90334,.T.);
#92664=ADVANCED_FACE('',(#7691),#90335,.F.);
#92665=ADVANCED_FACE('',(#7692),#90336,.F.);
#92666=ADVANCED_FACE('',(#7693),#90337,.F.);
#92667=ADVANCED_FACE('',(#7694),#90338,.F.);
#92668=ADVANCED_FACE('',(#7695),#90339,.T.);
#92669=ADVANCED_FACE('',(#7696),#90340,.T.);
#92670=ADVANCED_FACE('',(#7697,#6344,#6345,#6346),#90341,.F.);
#92671=ADVANCED_FACE('',(#7698),#2501,.F.);
#92672=ADVANCED_FACE('',(#7699),#2502,.F.);
#92673=ADVANCED_FACE('',(#7700),#2503,.F.);
#92674=ADVANCED_FACE('',(#7701),#2504,.F.);
#92675=ADVANCED_FACE('',(#7702),#2505,.F.);
#92676=ADVANCED_FACE('',(#7703),#90342,.T.);
#92677=ADVANCED_FACE('',(#7704),#6475,.T.);
#92678=ADVANCED_FACE('',(#7705,#6347),#6476,.T.);
#92679=ADVANCED_FACE('',(#7706,#6348),#6477,.T.);
#92680=ADVANCED_FACE('',(#7707),#5535,.F.);
#92681=ADVANCED_FACE('',(#7708),#90343,.T.);
#92682=ADVANCED_FACE('',(#7709),#50,.T.);
#92683=ADVANCED_FACE('',(#7710),#90344,.T.);
#92684=ADVANCED_FACE('',(#7711),#51,.T.);
#92685=ADVANCED_FACE('',(#7712),#52,.T.);
#92686=ADVANCED_FACE('',(#7713,#6349),#45,.T.);
#92687=ADVANCED_FACE('',(#7714),#5536,.T.);
#92688=ADVANCED_FACE('',(#7715),#53,.T.);
#92689=ADVANCED_FACE('',(#7716),#5537,.T.);
#92690=ADVANCED_FACE('',(#7717),#90345,.F.);
#92691=ADVANCED_FACE('',(#7718,#6350),#6478,.T.);
#92692=ADVANCED_FACE('',(#7719),#6479,.T.);
#92693=ADVANCED_FACE('',(#7720),#54,.T.);
#92694=ADVANCED_FACE('',(#7721),#55,.T.);
#92695=ADVANCED_FACE('',(#7722),#56,.T.);
#92696=ADVANCED_FACE('',(#7723),#57,.T.);
#92697=ADVANCED_FACE('',(#7724),#58,.T.);
#92698=ADVANCED_FACE('',(#7725),#6480,.T.);
#92699=ADVANCED_FACE('',(#7726,#6351),#6481,.T.);
#92700=ADVANCED_FACE('',(#7727),#59,.T.);
#92701=ADVANCED_FACE('',(#7728),#60,.T.);
#92702=ADVANCED_FACE('',(#7729),#61,.T.);
#92703=ADVANCED_FACE('',(#7730),#62,.T.);
#92704=ADVANCED_FACE('',(#7731),#63,.T.);
#92705=ADVANCED_FACE('',(#7732),#6482,.T.);
#92706=ADVANCED_FACE('',(#7733),#6483,.T.);
#92707=ADVANCED_FACE('',(#7734),#6484,.T.);
#92708=ADVANCED_FACE('',(#7735),#6485,.T.);
#92709=ADVANCED_FACE('',(#7736),#6486,.T.);
#92710=ADVANCED_FACE('',(#7737),#6487,.T.);
#92711=ADVANCED_FACE('',(#7738),#90346,.T.);
#92712=ADVANCED_FACE('',(#7739),#90347,.T.);
#92713=ADVANCED_FACE('',(#7740),#90348,.T.);
#92714=ADVANCED_FACE('',(#7741),#90349,.T.);
#92715=ADVANCED_FACE('',(#7742),#90350,.T.);
#92716=ADVANCED_FACE('',(#7743),#90351,.F.);
#92717=ADVANCED_FACE('',(#7744),#90352,.T.);
#92718=ADVANCED_FACE('',(#7745,#6352),#6488,.F.);
#92719=ADVANCED_FACE('',(#7746,#6353),#6489,.T.);
#92720=ADVANCED_FACE('',(#7747),#90353,.F.);
#92721=ADVANCED_FACE('',(#7748),#90354,.T.);
#92722=ADVANCED_FACE('',(#7749,#6354),#6490,.F.);
#92723=ADVANCED_FACE('',(#7750,#6355),#6491,.T.);
#92724=ADVANCED_FACE('',(#7751),#90355,.F.);
#92725=ADVANCED_FACE('',(#7752),#90356,.T.);
#92726=ADVANCED_FACE('',(#7753,#6356),#6492,.F.);
#92727=ADVANCED_FACE('',(#7754,#6357),#6493,.T.);
#92728=ADVANCED_FACE('',(#7755),#90357,.F.);
#92729=ADVANCED_FACE('',(#7756),#90358,.T.);
#92730=ADVANCED_FACE('',(#7757,#6358),#6494,.F.);
#92731=ADVANCED_FACE('',(#7758,#6359),#6495,.T.);
#92732=ADVANCED_FACE('',(#7759),#5538,.T.);
#92733=ADVANCED_FACE('',(#7760),#5539,.T.);
#92734=ADVANCED_FACE('',(#7761),#90359,.T.);
#92735=ADVANCED_FACE('',(#7762),#90360,.F.);
#92736=ADVANCED_FACE('',(#7763,#6360),#6496,.F.);
#92737=ADVANCED_FACE('',(#7764,#6361),#6497,.T.);
#92738=ADVANCED_FACE('',(#7765),#5540,.T.);
#92739=ADVANCED_FACE('',(#7766),#5541,.T.);
#92740=ADVANCED_FACE('',(#7767),#90361,.T.);
#92741=ADVANCED_FACE('',(#7768),#90362,.F.);
#92742=ADVANCED_FACE('',(#7769,#6362),#6498,.F.);
#92743=ADVANCED_FACE('',(#7770,#6363),#6499,.T.);
#92744=ADVANCED_FACE('',(#7771),#90363,.F.);
#92745=ADVANCED_FACE('',(#7772),#90364,.T.);
#92746=ADVANCED_FACE('',(#7773,#6364),#6500,.F.);
#92747=ADVANCED_FACE('',(#7774,#6365),#6501,.T.);
#92748=ADVANCED_FACE('',(#7775),#5542,.F.);
#92749=ADVANCED_FACE('',(#7776),#5543,.F.);
#92750=ADVANCED_FACE('',(#7777),#5544,.F.);
#92751=ADVANCED_FACE('',(#7778),#5545,.F.);
#92752=ADVANCED_FACE('',(#7779),#5546,.T.);
#92753=ADVANCED_FACE('',(#7780),#5547,.T.);
#92754=ADVANCED_FACE('',(#7781),#5548,.T.);
#92755=ADVANCED_FACE('',(#7782),#5549,.T.);
#92756=ADVANCED_FACE('',(#7783),#90365,.T.);
#92757=ADVANCED_FACE('',(#7784),#64,.T.);
#92758=ADVANCED_FACE('',(#7785),#65,.F.);
#92759=ADVANCED_FACE('',(#7786),#66,.T.);
#92760=ADVANCED_FACE('',(#7787),#67,.F.);
#92761=ADVANCED_FACE('',(#7788),#90366,.F.);
#92762=ADVANCED_FACE('',(#7789),#6502,.F.);
#92763=ADVANCED_FACE('',(#7790),#68,.F.);
#92764=ADVANCED_FACE('',(#7791),#6503,.F.);
#92765=ADVANCED_FACE('',(#7792),#69,.T.);
#92766=ADVANCED_FACE('',(#7793),#6504,.F.);
#92767=ADVANCED_FACE('',(#7794),#5550,.F.);
#92768=ADVANCED_FACE('',(#7795),#5551,.F.);
#92769=ADVANCED_FACE('',(#7796),#5552,.T.);
#92770=ADVANCED_FACE('',(#7797),#5553,.T.);
#92771=ADVANCED_FACE('',(#7798),#6505,.F.);
#92772=ADVANCED_FACE('',(#7799),#70,.F.);
#92773=ADVANCED_FACE('',(#7800),#6506,.F.);
#92774=ADVANCED_FACE('',(#7801),#71,.T.);
#92775=ADVANCED_FACE('',(#7802),#6507,.F.);
#92776=ADVANCED_FACE('',(#7803),#5554,.F.);
#92777=ADVANCED_FACE('',(#7804),#5555,.F.);
#92778=ADVANCED_FACE('',(#7805),#5556,.T.);
#92779=ADVANCED_FACE('',(#7806),#5557,.T.);
#92780=ADVANCED_FACE('',(#7807),#6508,.F.);
#92781=ADVANCED_FACE('',(#7808),#72,.F.);
#92782=ADVANCED_FACE('',(#7809),#6509,.F.);
#92783=ADVANCED_FACE('',(#7810),#73,.T.);
#92784=ADVANCED_FACE('',(#7811),#6510,.F.);
#92785=ADVANCED_FACE('',(#7812),#5558,.F.);
#92786=ADVANCED_FACE('',(#7813),#5559,.F.);
#92787=ADVANCED_FACE('',(#7814),#5560,.T.);
#92788=ADVANCED_FACE('',(#7815),#5561,.T.);
#92789=ADVANCED_FACE('',(#7816),#6511,.F.);
#92790=ADVANCED_FACE('',(#7817),#74,.F.);
#92791=ADVANCED_FACE('',(#7818),#6512,.F.);
#92792=ADVANCED_FACE('',(#7819),#75,.T.);
#92793=ADVANCED_FACE('',(#7820),#6513,.F.);
#92794=ADVANCED_FACE('',(#7821),#5562,.F.);
#92795=ADVANCED_FACE('',(#7822),#5563,.F.);
#92796=ADVANCED_FACE('',(#7823),#5564,.T.);
#92797=ADVANCED_FACE('',(#7824),#5565,.T.);
#92798=ADVANCED_FACE('',(#7825),#6514,.F.);
#92799=ADVANCED_FACE('',(#7826),#76,.F.);
#92800=ADVANCED_FACE('',(#7827),#6515,.F.);
#92801=ADVANCED_FACE('',(#7828),#77,.T.);
#92802=ADVANCED_FACE('',(#7829),#6516,.F.);
#92803=ADVANCED_FACE('',(#7830),#5566,.F.);
#92804=ADVANCED_FACE('',(#7831),#5567,.F.);
#92805=ADVANCED_FACE('',(#7832),#5568,.T.);
#92806=ADVANCED_FACE('',(#7833),#5569,.T.);
#92807=ADVANCED_FACE('',(#7834),#6517,.F.);
#92808=ADVANCED_FACE('',(#7835),#78,.F.);
#92809=ADVANCED_FACE('',(#7836),#6518,.F.);
#92810=ADVANCED_FACE('',(#7837),#79,.T.);
#92811=ADVANCED_FACE('',(#7838),#6519,.F.);
#92812=ADVANCED_FACE('',(#7839),#5570,.F.);
#92813=ADVANCED_FACE('',(#7840),#5571,.F.);
#92814=ADVANCED_FACE('',(#7841),#5572,.T.);
#92815=ADVANCED_FACE('',(#7842),#5573,.T.);
#92816=ADVANCED_FACE('',(#7843),#6520,.F.);
#92817=ADVANCED_FACE('',(#7844),#80,.F.);
#92818=ADVANCED_FACE('',(#7845),#6521,.F.);
#92819=ADVANCED_FACE('',(#7846),#81,.T.);
#92820=ADVANCED_FACE('',(#7847),#6522,.F.);
#92821=ADVANCED_FACE('',(#7848),#5574,.F.);
#92822=ADVANCED_FACE('',(#7849),#5575,.F.);
#92823=ADVANCED_FACE('',(#7850),#5576,.T.);
#92824=ADVANCED_FACE('',(#7851),#5577,.T.);
#92825=ADVANCED_FACE('',(#7852),#6523,.F.);
#92826=ADVANCED_FACE('',(#7853),#82,.F.);
#92827=ADVANCED_FACE('',(#7854),#6524,.F.);
#92828=ADVANCED_FACE('',(#7855),#83,.T.);
#92829=ADVANCED_FACE('',(#7856),#6525,.F.);
#92830=ADVANCED_FACE('',(#7857),#5578,.F.);
#92831=ADVANCED_FACE('',(#7858),#5579,.F.);
#92832=ADVANCED_FACE('',(#7859),#5580,.T.);
#92833=ADVANCED_FACE('',(#7860),#5581,.T.);
#92834=ADVANCED_FACE('',(#7861),#6526,.F.);
#92835=ADVANCED_FACE('',(#7862),#84,.F.);
#92836=ADVANCED_FACE('',(#7863),#6527,.F.);
#92837=ADVANCED_FACE('',(#7864),#85,.T.);
#92838=ADVANCED_FACE('',(#7865),#6528,.F.);
#92839=ADVANCED_FACE('',(#7866),#5582,.F.);
#92840=ADVANCED_FACE('',(#7867),#5583,.F.);
#92841=ADVANCED_FACE('',(#7868),#5584,.T.);
#92842=ADVANCED_FACE('',(#7869),#5585,.T.);
#92843=ADVANCED_FACE('',(#7870),#6529,.F.);
#92844=ADVANCED_FACE('',(#7871),#86,.F.);
#92845=ADVANCED_FACE('',(#7872),#6530,.F.);
#92846=ADVANCED_FACE('',(#7873),#87,.T.);
#92847=ADVANCED_FACE('',(#7874),#6531,.F.);
#92848=ADVANCED_FACE('',(#7875),#5586,.F.);
#92849=ADVANCED_FACE('',(#7876),#5587,.F.);
#92850=ADVANCED_FACE('',(#7877),#5588,.T.);
#92851=ADVANCED_FACE('',(#7878),#5589,.T.);
#92852=ADVANCED_FACE('',(#7879),#6532,.F.);
#92853=ADVANCED_FACE('',(#7880),#88,.F.);
#92854=ADVANCED_FACE('',(#7881),#6533,.F.);
#92855=ADVANCED_FACE('',(#7882),#89,.T.);
#92856=ADVANCED_FACE('',(#7883),#6534,.F.);
#92857=ADVANCED_FACE('',(#7884),#5590,.F.);
#92858=ADVANCED_FACE('',(#7885),#5591,.F.);
#92859=ADVANCED_FACE('',(#7886),#5592,.T.);
#92860=ADVANCED_FACE('',(#7887),#5593,.T.);
#92861=ADVANCED_FACE('',(#7888),#6535,.F.);
#92862=ADVANCED_FACE('',(#7889),#90,.F.);
#92863=ADVANCED_FACE('',(#7890),#6536,.F.);
#92864=ADVANCED_FACE('',(#7891),#91,.T.);
#92865=ADVANCED_FACE('',(#7892),#6537,.F.);
#92866=ADVANCED_FACE('',(#7893),#5594,.F.);
#92867=ADVANCED_FACE('',(#7894),#5595,.F.);
#92868=ADVANCED_FACE('',(#7895),#5596,.T.);
#92869=ADVANCED_FACE('',(#7896),#5597,.T.);
#92870=ADVANCED_FACE('',(#7897),#6538,.F.);
#92871=ADVANCED_FACE('',(#7898),#92,.F.);
#92872=ADVANCED_FACE('',(#7899),#6539,.F.);
#92873=ADVANCED_FACE('',(#7900),#93,.T.);
#92874=ADVANCED_FACE('',(#7901),#6540,.F.);
#92875=ADVANCED_FACE('',(#7902),#5598,.F.);
#92876=ADVANCED_FACE('',(#7903),#5599,.F.);
#92877=ADVANCED_FACE('',(#7904),#5600,.T.);
#92878=ADVANCED_FACE('',(#7905),#5601,.T.);
#92879=ADVANCED_FACE('',(#7906),#6541,.F.);
#92880=ADVANCED_FACE('',(#7907),#94,.F.);
#92881=ADVANCED_FACE('',(#7908),#6542,.F.);
#92882=ADVANCED_FACE('',(#7909),#95,.T.);
#92883=ADVANCED_FACE('',(#7910),#6543,.F.);
#92884=ADVANCED_FACE('',(#7911),#5602,.F.);
#92885=ADVANCED_FACE('',(#7912),#5603,.F.);
#92886=ADVANCED_FACE('',(#7913),#5604,.T.);
#92887=ADVANCED_FACE('',(#7914),#5605,.T.);
#92888=ADVANCED_FACE('',(#7915),#6544,.F.);
#92889=ADVANCED_FACE('',(#7916),#96,.F.);
#92890=ADVANCED_FACE('',(#7917),#6545,.F.);
#92891=ADVANCED_FACE('',(#7918),#97,.T.);
#92892=ADVANCED_FACE('',(#7919),#6546,.F.);
#92893=ADVANCED_FACE('',(#7920),#5606,.F.);
#92894=ADVANCED_FACE('',(#7921),#5607,.F.);
#92895=ADVANCED_FACE('',(#7922),#5608,.T.);
#92896=ADVANCED_FACE('',(#7923),#5609,.T.);
#92897=ADVANCED_FACE('',(#7924),#6547,.F.);
#92898=ADVANCED_FACE('',(#7925),#98,.F.);
#92899=ADVANCED_FACE('',(#7926),#6548,.F.);
#92900=ADVANCED_FACE('',(#7927),#99,.T.);
#92901=ADVANCED_FACE('',(#7928),#6549,.F.);
#92902=ADVANCED_FACE('',(#7929),#5610,.F.);
#92903=ADVANCED_FACE('',(#7930),#5611,.F.);
#92904=ADVANCED_FACE('',(#7931),#5612,.T.);
#92905=ADVANCED_FACE('',(#7932),#5613,.T.);
#92906=ADVANCED_FACE('',(#7933),#6550,.F.);
#92907=ADVANCED_FACE('',(#7934),#100,.F.);
#92908=ADVANCED_FACE('',(#7935),#6551,.F.);
#92909=ADVANCED_FACE('',(#7936),#101,.T.);
#92910=ADVANCED_FACE('',(#7937),#6552,.F.);
#92911=ADVANCED_FACE('',(#7938),#5614,.F.);
#92912=ADVANCED_FACE('',(#7939),#5615,.F.);
#92913=ADVANCED_FACE('',(#7940),#5616,.T.);
#92914=ADVANCED_FACE('',(#7941),#5617,.T.);
#92915=ADVANCED_FACE('',(#7942),#6553,.F.);
#92916=ADVANCED_FACE('',(#7943),#102,.F.);
#92917=ADVANCED_FACE('',(#7944),#6554,.F.);
#92918=ADVANCED_FACE('',(#7945),#103,.T.);
#92919=ADVANCED_FACE('',(#7946),#6555,.F.);
#92920=ADVANCED_FACE('',(#7947),#5618,.F.);
#92921=ADVANCED_FACE('',(#7948),#5619,.F.);
#92922=ADVANCED_FACE('',(#7949),#5620,.T.);
#92923=ADVANCED_FACE('',(#7950),#5621,.T.);
#92924=ADVANCED_FACE('',(#7951),#6556,.F.);
#92925=ADVANCED_FACE('',(#7952),#104,.F.);
#92926=ADVANCED_FACE('',(#7953),#6557,.F.);
#92927=ADVANCED_FACE('',(#7954),#105,.T.);
#92928=ADVANCED_FACE('',(#7955),#6558,.F.);
#92929=ADVANCED_FACE('',(#7956),#5622,.F.);
#92930=ADVANCED_FACE('',(#7957),#5623,.F.);
#92931=ADVANCED_FACE('',(#7958),#5624,.T.);
#92932=ADVANCED_FACE('',(#7959),#5625,.T.);
#92933=ADVANCED_FACE('',(#7960),#6559,.F.);
#92934=ADVANCED_FACE('',(#7961),#106,.F.);
#92935=ADVANCED_FACE('',(#7962),#6560,.F.);
#92936=ADVANCED_FACE('',(#7963),#107,.T.);
#92937=ADVANCED_FACE('',(#7964),#6561,.F.);
#92938=ADVANCED_FACE('',(#7965),#5626,.F.);
#92939=ADVANCED_FACE('',(#7966),#5627,.F.);
#92940=ADVANCED_FACE('',(#7967),#5628,.T.);
#92941=ADVANCED_FACE('',(#7968),#5629,.T.);
#92942=ADVANCED_FACE('',(#7969),#6562,.F.);
#92943=ADVANCED_FACE('',(#7970),#108,.F.);
#92944=ADVANCED_FACE('',(#7971),#6563,.F.);
#92945=ADVANCED_FACE('',(#7972),#109,.T.);
#92946=ADVANCED_FACE('',(#7973),#6564,.F.);
#92947=ADVANCED_FACE('',(#7974),#5630,.F.);
#92948=ADVANCED_FACE('',(#7975),#5631,.F.);
#92949=ADVANCED_FACE('',(#7976),#5632,.T.);
#92950=ADVANCED_FACE('',(#7977),#5633,.T.);
#92951=ADVANCED_FACE('',(#7978),#6565,.F.);
#92952=ADVANCED_FACE('',(#7979),#110,.F.);
#92953=ADVANCED_FACE('',(#7980),#6566,.F.);
#92954=ADVANCED_FACE('',(#7981),#111,.T.);
#92955=ADVANCED_FACE('',(#7982),#6567,.F.);
#92956=ADVANCED_FACE('',(#7983),#5634,.F.);
#92957=ADVANCED_FACE('',(#7984),#5635,.F.);
#92958=ADVANCED_FACE('',(#7985),#5636,.T.);
#92959=ADVANCED_FACE('',(#7986),#5637,.T.);
#92960=ADVANCED_FACE('',(#7987),#6568,.F.);
#92961=ADVANCED_FACE('',(#7988),#112,.F.);
#92962=ADVANCED_FACE('',(#7989),#6569,.F.);
#92963=ADVANCED_FACE('',(#7990),#113,.T.);
#92964=ADVANCED_FACE('',(#7991),#6570,.F.);
#92965=ADVANCED_FACE('',(#7992),#5638,.F.);
#92966=ADVANCED_FACE('',(#7993),#5639,.F.);
#92967=ADVANCED_FACE('',(#7994),#5640,.T.);
#92968=ADVANCED_FACE('',(#7995),#5641,.T.);
#92969=ADVANCED_FACE('',(#7996),#6571,.F.);
#92970=ADVANCED_FACE('',(#7997),#114,.F.);
#92971=ADVANCED_FACE('',(#7998),#6572,.F.);
#92972=ADVANCED_FACE('',(#7999),#115,.T.);
#92973=ADVANCED_FACE('',(#8000),#6573,.F.);
#92974=ADVANCED_FACE('',(#8001),#5642,.F.);
#92975=ADVANCED_FACE('',(#8002),#5643,.F.);
#92976=ADVANCED_FACE('',(#8003),#5644,.T.);
#92977=ADVANCED_FACE('',(#8004),#5645,.T.);
#92978=ADVANCED_FACE('',(#8005),#6574,.F.);
#92979=ADVANCED_FACE('',(#8006),#116,.F.);
#92980=ADVANCED_FACE('',(#8007),#6575,.F.);
#92981=ADVANCED_FACE('',(#8008),#117,.T.);
#92982=ADVANCED_FACE('',(#8009),#6576,.F.);
#92983=ADVANCED_FACE('',(#8010),#5646,.F.);
#92984=ADVANCED_FACE('',(#8011),#5647,.F.);
#92985=ADVANCED_FACE('',(#8012),#5648,.T.);
#92986=ADVANCED_FACE('',(#8013),#5649,.T.);
#92987=ADVANCED_FACE('',(#8014),#6577,.F.);
#92988=ADVANCED_FACE('',(#8015),#118,.F.);
#92989=ADVANCED_FACE('',(#8016),#6578,.F.);
#92990=ADVANCED_FACE('',(#8017),#119,.T.);
#92991=ADVANCED_FACE('',(#8018),#6579,.F.);
#92992=ADVANCED_FACE('',(#8019),#5650,.F.);
#92993=ADVANCED_FACE('',(#8020),#5651,.F.);
#92994=ADVANCED_FACE('',(#8021),#5652,.T.);
#92995=ADVANCED_FACE('',(#8022),#5653,.T.);
#92996=ADVANCED_FACE('',(#8023),#6580,.F.);
#92997=ADVANCED_FACE('',(#8024),#120,.F.);
#92998=ADVANCED_FACE('',(#8025),#6581,.F.);
#92999=ADVANCED_FACE('',(#8026),#121,.T.);
#93000=ADVANCED_FACE('',(#8027),#6582,.F.);
#93001=ADVANCED_FACE('',(#8028),#5654,.F.);
#93002=ADVANCED_FACE('',(#8029),#5655,.F.);
#93003=ADVANCED_FACE('',(#8030),#5656,.T.);
#93004=ADVANCED_FACE('',(#8031),#5657,.T.);
#93005=ADVANCED_FACE('',(#8032),#6583,.F.);
#93006=ADVANCED_FACE('',(#8033),#122,.F.);
#93007=ADVANCED_FACE('',(#8034),#6584,.F.);
#93008=ADVANCED_FACE('',(#8035),#123,.T.);
#93009=ADVANCED_FACE('',(#8036),#6585,.F.);
#93010=ADVANCED_FACE('',(#8037),#5658,.F.);
#93011=ADVANCED_FACE('',(#8038),#5659,.F.);
#93012=ADVANCED_FACE('',(#8039),#5660,.T.);
#93013=ADVANCED_FACE('',(#8040),#5661,.T.);
#93014=ADVANCED_FACE('',(#8041),#6586,.F.);
#93015=ADVANCED_FACE('',(#8042),#124,.F.);
#93016=ADVANCED_FACE('',(#8043),#6587,.F.);
#93017=ADVANCED_FACE('',(#8044),#125,.T.);
#93018=ADVANCED_FACE('',(#8045),#6588,.F.);
#93019=ADVANCED_FACE('',(#8046),#5662,.F.);
#93020=ADVANCED_FACE('',(#8047),#5663,.F.);
#93021=ADVANCED_FACE('',(#8048),#5664,.T.);
#93022=ADVANCED_FACE('',(#8049),#5665,.T.);
#93023=ADVANCED_FACE('',(#8050),#6589,.F.);
#93024=ADVANCED_FACE('',(#8051),#126,.F.);
#93025=ADVANCED_FACE('',(#8052),#6590,.F.);
#93026=ADVANCED_FACE('',(#8053),#127,.T.);
#93027=ADVANCED_FACE('',(#8054),#6591,.F.);
#93028=ADVANCED_FACE('',(#8055),#5666,.F.);
#93029=ADVANCED_FACE('',(#8056),#5667,.F.);
#93030=ADVANCED_FACE('',(#8057),#5668,.T.);
#93031=ADVANCED_FACE('',(#8058),#5669,.T.);
#93032=ADVANCED_FACE('',(#8059),#6592,.F.);
#93033=ADVANCED_FACE('',(#8060),#128,.F.);
#93034=ADVANCED_FACE('',(#8061),#6593,.F.);
#93035=ADVANCED_FACE('',(#8062),#129,.T.);
#93036=ADVANCED_FACE('',(#8063),#6594,.F.);
#93037=ADVANCED_FACE('',(#8064),#5670,.F.);
#93038=ADVANCED_FACE('',(#8065),#5671,.F.);
#93039=ADVANCED_FACE('',(#8066),#5672,.T.);
#93040=ADVANCED_FACE('',(#8067),#5673,.T.);
#93041=ADVANCED_FACE('',(#8068),#6595,.F.);
#93042=ADVANCED_FACE('',(#8069),#130,.F.);
#93043=ADVANCED_FACE('',(#8070),#6596,.F.);
#93044=ADVANCED_FACE('',(#8071),#131,.T.);
#93045=ADVANCED_FACE('',(#8072),#6597,.F.);
#93046=ADVANCED_FACE('',(#8073),#5674,.F.);
#93047=ADVANCED_FACE('',(#8074),#5675,.F.);
#93048=ADVANCED_FACE('',(#8075),#5676,.T.);
#93049=ADVANCED_FACE('',(#8076),#5677,.T.);
#93050=ADVANCED_FACE('',(#8077),#6598,.F.);
#93051=ADVANCED_FACE('',(#8078),#132,.F.);
#93052=ADVANCED_FACE('',(#8079),#6599,.F.);
#93053=ADVANCED_FACE('',(#8080),#133,.T.);
#93054=ADVANCED_FACE('',(#8081),#6600,.F.);
#93055=ADVANCED_FACE('',(#8082),#5678,.F.);
#93056=ADVANCED_FACE('',(#8083),#5679,.F.);
#93057=ADVANCED_FACE('',(#8084),#5680,.T.);
#93058=ADVANCED_FACE('',(#8085),#5681,.T.);
#93059=ADVANCED_FACE('',(#8086),#6601,.F.);
#93060=ADVANCED_FACE('',(#8087),#134,.F.);
#93061=ADVANCED_FACE('',(#8088),#6602,.F.);
#93062=ADVANCED_FACE('',(#8089),#135,.T.);
#93063=ADVANCED_FACE('',(#8090),#6603,.F.);
#93064=ADVANCED_FACE('',(#8091),#5682,.F.);
#93065=ADVANCED_FACE('',(#8092),#5683,.F.);
#93066=ADVANCED_FACE('',(#8093),#5684,.T.);
#93067=ADVANCED_FACE('',(#8094),#5685,.T.);
#93068=ADVANCED_FACE('',(#8095),#6604,.F.);
#93069=ADVANCED_FACE('',(#8096),#136,.F.);
#93070=ADVANCED_FACE('',(#8097),#6605,.F.);
#93071=ADVANCED_FACE('',(#8098),#137,.T.);
#93072=ADVANCED_FACE('',(#8099),#6606,.F.);
#93073=ADVANCED_FACE('',(#8100),#5686,.F.);
#93074=ADVANCED_FACE('',(#8101),#5687,.F.);
#93075=ADVANCED_FACE('',(#8102),#5688,.T.);
#93076=ADVANCED_FACE('',(#8103),#5689,.T.);
#93077=ADVANCED_FACE('',(#8104),#6607,.F.);
#93078=ADVANCED_FACE('',(#8105),#138,.F.);
#93079=ADVANCED_FACE('',(#8106),#6608,.F.);
#93080=ADVANCED_FACE('',(#8107),#139,.T.);
#93081=ADVANCED_FACE('',(#8108),#6609,.F.);
#93082=ADVANCED_FACE('',(#8109),#5690,.F.);
#93083=ADVANCED_FACE('',(#8110),#5691,.F.);
#93084=ADVANCED_FACE('',(#8111),#5692,.T.);
#93085=ADVANCED_FACE('',(#8112),#5693,.T.);
#93086=ADVANCED_FACE('',(#8113),#6610,.F.);
#93087=ADVANCED_FACE('',(#8114),#140,.F.);
#93088=ADVANCED_FACE('',(#8115),#6611,.F.);
#93089=ADVANCED_FACE('',(#8116),#141,.T.);
#93090=ADVANCED_FACE('',(#8117),#6612,.F.);
#93091=ADVANCED_FACE('',(#8118),#5694,.F.);
#93092=ADVANCED_FACE('',(#8119),#5695,.F.);
#93093=ADVANCED_FACE('',(#8120),#5696,.T.);
#93094=ADVANCED_FACE('',(#8121),#5697,.T.);
#93095=ADVANCED_FACE('',(#8122),#6613,.F.);
#93096=ADVANCED_FACE('',(#8123),#142,.F.);
#93097=ADVANCED_FACE('',(#8124),#6614,.F.);
#93098=ADVANCED_FACE('',(#8125),#143,.T.);
#93099=ADVANCED_FACE('',(#8126),#6615,.F.);
#93100=ADVANCED_FACE('',(#8127),#5698,.F.);
#93101=ADVANCED_FACE('',(#8128),#5699,.F.);
#93102=ADVANCED_FACE('',(#8129),#5700,.T.);
#93103=ADVANCED_FACE('',(#8130),#5701,.T.);
#93104=ADVANCED_FACE('',(#8131),#6616,.F.);
#93105=ADVANCED_FACE('',(#8132),#144,.F.);
#93106=ADVANCED_FACE('',(#8133),#6617,.F.);
#93107=ADVANCED_FACE('',(#8134),#145,.T.);
#93108=ADVANCED_FACE('',(#8135),#6618,.F.);
#93109=ADVANCED_FACE('',(#8136),#5702,.F.);
#93110=ADVANCED_FACE('',(#8137),#5703,.F.);
#93111=ADVANCED_FACE('',(#8138),#5704,.T.);
#93112=ADVANCED_FACE('',(#8139),#5705,.T.);
#93113=ADVANCED_FACE('',(#8140),#6619,.F.);
#93114=ADVANCED_FACE('',(#8141),#146,.F.);
#93115=ADVANCED_FACE('',(#8142),#6620,.F.);
#93116=ADVANCED_FACE('',(#8143),#147,.T.);
#93117=ADVANCED_FACE('',(#8144),#6621,.F.);
#93118=ADVANCED_FACE('',(#8145),#5706,.F.);
#93119=ADVANCED_FACE('',(#8146),#5707,.F.);
#93120=ADVANCED_FACE('',(#8147),#5708,.T.);
#93121=ADVANCED_FACE('',(#8148),#5709,.T.);
#93122=ADVANCED_FACE('',(#8149),#6622,.F.);
#93123=ADVANCED_FACE('',(#8150),#148,.F.);
#93124=ADVANCED_FACE('',(#8151),#6623,.F.);
#93125=ADVANCED_FACE('',(#8152),#149,.T.);
#93126=ADVANCED_FACE('',(#8153),#6624,.F.);
#93127=ADVANCED_FACE('',(#8154),#5710,.F.);
#93128=ADVANCED_FACE('',(#8155),#5711,.F.);
#93129=ADVANCED_FACE('',(#8156),#5712,.T.);
#93130=ADVANCED_FACE('',(#8157),#5713,.T.);
#93131=ADVANCED_FACE('',(#8158),#6625,.F.);
#93132=ADVANCED_FACE('',(#8159),#150,.F.);
#93133=ADVANCED_FACE('',(#8160),#6626,.F.);
#93134=ADVANCED_FACE('',(#8161),#151,.T.);
#93135=ADVANCED_FACE('',(#8162),#6627,.F.);
#93136=ADVANCED_FACE('',(#8163),#5714,.F.);
#93137=ADVANCED_FACE('',(#8164),#5715,.F.);
#93138=ADVANCED_FACE('',(#8165),#5716,.T.);
#93139=ADVANCED_FACE('',(#8166),#5717,.T.);
#93140=ADVANCED_FACE('',(#8167),#6628,.F.);
#93141=ADVANCED_FACE('',(#8168),#152,.F.);
#93142=ADVANCED_FACE('',(#8169),#6629,.F.);
#93143=ADVANCED_FACE('',(#8170),#153,.T.);
#93144=ADVANCED_FACE('',(#8171),#6630,.F.);
#93145=ADVANCED_FACE('',(#8172),#5718,.F.);
#93146=ADVANCED_FACE('',(#8173),#5719,.F.);
#93147=ADVANCED_FACE('',(#8174),#5720,.T.);
#93148=ADVANCED_FACE('',(#8175),#5721,.T.);
#93149=ADVANCED_FACE('',(#8176),#6631,.F.);
#93150=ADVANCED_FACE('',(#8177),#154,.F.);
#93151=ADVANCED_FACE('',(#8178),#6632,.F.);
#93152=ADVANCED_FACE('',(#8179),#155,.T.);
#93153=ADVANCED_FACE('',(#8180),#6633,.F.);
#93154=ADVANCED_FACE('',(#8181),#5722,.F.);
#93155=ADVANCED_FACE('',(#8182),#5723,.F.);
#93156=ADVANCED_FACE('',(#8183),#5724,.T.);
#93157=ADVANCED_FACE('',(#8184),#5725,.T.);
#93158=ADVANCED_FACE('',(#8185),#6634,.F.);
#93159=ADVANCED_FACE('',(#8186),#156,.F.);
#93160=ADVANCED_FACE('',(#8187),#6635,.F.);
#93161=ADVANCED_FACE('',(#8188),#157,.T.);
#93162=ADVANCED_FACE('',(#8189),#6636,.F.);
#93163=ADVANCED_FACE('',(#8190),#5726,.F.);
#93164=ADVANCED_FACE('',(#8191),#5727,.F.);
#93165=ADVANCED_FACE('',(#8192),#5728,.T.);
#93166=ADVANCED_FACE('',(#8193),#5729,.T.);
#93167=ADVANCED_FACE('',(#8194),#6637,.F.);
#93168=ADVANCED_FACE('',(#8195),#158,.F.);
#93169=ADVANCED_FACE('',(#8196),#6638,.F.);
#93170=ADVANCED_FACE('',(#8197),#159,.T.);
#93171=ADVANCED_FACE('',(#8198),#6639,.F.);
#93172=ADVANCED_FACE('',(#8199),#5730,.F.);
#93173=ADVANCED_FACE('',(#8200),#5731,.F.);
#93174=ADVANCED_FACE('',(#8201),#5732,.T.);
#93175=ADVANCED_FACE('',(#8202),#5733,.T.);
#93176=ADVANCED_FACE('',(#8203),#6640,.F.);
#93177=ADVANCED_FACE('',(#8204),#160,.F.);
#93178=ADVANCED_FACE('',(#8205),#6641,.F.);
#93179=ADVANCED_FACE('',(#8206),#161,.T.);
#93180=ADVANCED_FACE('',(#8207),#6642,.F.);
#93181=ADVANCED_FACE('',(#8208),#5734,.F.);
#93182=ADVANCED_FACE('',(#8209),#5735,.F.);
#93183=ADVANCED_FACE('',(#8210),#5736,.T.);
#93184=ADVANCED_FACE('',(#8211),#5737,.T.);
#93185=ADVANCED_FACE('',(#8212),#6643,.F.);
#93186=ADVANCED_FACE('',(#8213),#162,.F.);
#93187=ADVANCED_FACE('',(#8214),#6644,.F.);
#93188=ADVANCED_FACE('',(#8215),#163,.T.);
#93189=ADVANCED_FACE('',(#8216),#6645,.F.);
#93190=ADVANCED_FACE('',(#8217),#5738,.F.);
#93191=ADVANCED_FACE('',(#8218),#5739,.F.);
#93192=ADVANCED_FACE('',(#8219),#5740,.T.);
#93193=ADVANCED_FACE('',(#8220),#5741,.T.);
#93194=ADVANCED_FACE('',(#8221),#6646,.F.);
#93195=ADVANCED_FACE('',(#8222),#164,.F.);
#93196=ADVANCED_FACE('',(#8223),#6647,.F.);
#93197=ADVANCED_FACE('',(#8224),#165,.T.);
#93198=ADVANCED_FACE('',(#8225),#6648,.F.);
#93199=ADVANCED_FACE('',(#8226),#5742,.F.);
#93200=ADVANCED_FACE('',(#8227),#5743,.F.);
#93201=ADVANCED_FACE('',(#8228),#5744,.T.);
#93202=ADVANCED_FACE('',(#8229),#5745,.T.);
#93203=ADVANCED_FACE('',(#8230),#6649,.F.);
#93204=ADVANCED_FACE('',(#8231),#166,.F.);
#93205=ADVANCED_FACE('',(#8232),#6650,.F.);
#93206=ADVANCED_FACE('',(#8233),#167,.T.);
#93207=ADVANCED_FACE('',(#8234),#6651,.F.);
#93208=ADVANCED_FACE('',(#8235),#5746,.F.);
#93209=ADVANCED_FACE('',(#8236),#5747,.F.);
#93210=ADVANCED_FACE('',(#8237),#5748,.T.);
#93211=ADVANCED_FACE('',(#8238),#5749,.T.);
#93212=ADVANCED_FACE('',(#8239),#6652,.F.);
#93213=ADVANCED_FACE('',(#8240),#168,.F.);
#93214=ADVANCED_FACE('',(#8241),#6653,.F.);
#93215=ADVANCED_FACE('',(#8242),#169,.T.);
#93216=ADVANCED_FACE('',(#8243),#6654,.F.);
#93217=ADVANCED_FACE('',(#8244),#5750,.F.);
#93218=ADVANCED_FACE('',(#8245),#5751,.F.);
#93219=ADVANCED_FACE('',(#8246),#5752,.T.);
#93220=ADVANCED_FACE('',(#8247),#5753,.T.);
#93221=ADVANCED_FACE('',(#8248),#6655,.F.);
#93222=ADVANCED_FACE('',(#8249),#170,.F.);
#93223=ADVANCED_FACE('',(#8250),#6656,.F.);
#93224=ADVANCED_FACE('',(#8251),#171,.T.);
#93225=ADVANCED_FACE('',(#8252),#6657,.F.);
#93226=ADVANCED_FACE('',(#8253),#5754,.F.);
#93227=ADVANCED_FACE('',(#8254),#5755,.F.);
#93228=ADVANCED_FACE('',(#8255),#5756,.T.);
#93229=ADVANCED_FACE('',(#8256),#5757,.T.);
#93230=ADVANCED_FACE('',(#8257),#6658,.F.);
#93231=ADVANCED_FACE('',(#8258),#172,.F.);
#93232=ADVANCED_FACE('',(#8259),#6659,.F.);
#93233=ADVANCED_FACE('',(#8260),#173,.T.);
#93234=ADVANCED_FACE('',(#8261),#6660,.F.);
#93235=ADVANCED_FACE('',(#8262),#5758,.F.);
#93236=ADVANCED_FACE('',(#8263),#5759,.F.);
#93237=ADVANCED_FACE('',(#8264),#5760,.T.);
#93238=ADVANCED_FACE('',(#8265),#5761,.T.);
#93239=ADVANCED_FACE('',(#8266),#6661,.F.);
#93240=ADVANCED_FACE('',(#8267),#174,.F.);
#93241=ADVANCED_FACE('',(#8268),#6662,.F.);
#93242=ADVANCED_FACE('',(#8269),#175,.T.);
#93243=ADVANCED_FACE('',(#8270),#6663,.F.);
#93244=ADVANCED_FACE('',(#8271),#5762,.F.);
#93245=ADVANCED_FACE('',(#8272),#5763,.F.);
#93246=ADVANCED_FACE('',(#8273),#5764,.T.);
#93247=ADVANCED_FACE('',(#8274),#5765,.T.);
#93248=ADVANCED_FACE('',(#8275),#6664,.F.);
#93249=ADVANCED_FACE('',(#8276),#176,.F.);
#93250=ADVANCED_FACE('',(#8277),#6665,.F.);
#93251=ADVANCED_FACE('',(#8278),#177,.T.);
#93252=ADVANCED_FACE('',(#8279),#6666,.F.);
#93253=ADVANCED_FACE('',(#8280),#5766,.F.);
#93254=ADVANCED_FACE('',(#8281),#5767,.F.);
#93255=ADVANCED_FACE('',(#8282),#5768,.T.);
#93256=ADVANCED_FACE('',(#8283),#5769,.T.);
#93257=ADVANCED_FACE('',(#8284),#6667,.F.);
#93258=ADVANCED_FACE('',(#8285),#178,.F.);
#93259=ADVANCED_FACE('',(#8286),#6668,.F.);
#93260=ADVANCED_FACE('',(#8287),#179,.T.);
#93261=ADVANCED_FACE('',(#8288),#6669,.F.);
#93262=ADVANCED_FACE('',(#8289),#5770,.F.);
#93263=ADVANCED_FACE('',(#8290),#5771,.F.);
#93264=ADVANCED_FACE('',(#8291),#5772,.T.);
#93265=ADVANCED_FACE('',(#8292),#5773,.T.);
#93266=ADVANCED_FACE('',(#8293),#6670,.F.);
#93267=ADVANCED_FACE('',(#8294),#180,.F.);
#93268=ADVANCED_FACE('',(#8295),#6671,.F.);
#93269=ADVANCED_FACE('',(#8296),#181,.T.);
#93270=ADVANCED_FACE('',(#8297),#6672,.F.);
#93271=ADVANCED_FACE('',(#8298),#5774,.F.);
#93272=ADVANCED_FACE('',(#8299),#5775,.F.);
#93273=ADVANCED_FACE('',(#8300),#5776,.T.);
#93274=ADVANCED_FACE('',(#8301),#5777,.T.);
#93275=ADVANCED_FACE('',(#8302),#6673,.F.);
#93276=ADVANCED_FACE('',(#8303),#182,.F.);
#93277=ADVANCED_FACE('',(#8304),#6674,.F.);
#93278=ADVANCED_FACE('',(#8305),#183,.T.);
#93279=ADVANCED_FACE('',(#8306),#6675,.F.);
#93280=ADVANCED_FACE('',(#8307),#5778,.F.);
#93281=ADVANCED_FACE('',(#8308),#5779,.F.);
#93282=ADVANCED_FACE('',(#8309),#5780,.T.);
#93283=ADVANCED_FACE('',(#8310),#5781,.T.);
#93284=ADVANCED_FACE('',(#8311),#6676,.F.);
#93285=ADVANCED_FACE('',(#8312),#184,.F.);
#93286=ADVANCED_FACE('',(#8313),#6677,.F.);
#93287=ADVANCED_FACE('',(#8314),#185,.T.);
#93288=ADVANCED_FACE('',(#8315),#6678,.F.);
#93289=ADVANCED_FACE('',(#8316),#5782,.F.);
#93290=ADVANCED_FACE('',(#8317),#5783,.F.);
#93291=ADVANCED_FACE('',(#8318),#5784,.T.);
#93292=ADVANCED_FACE('',(#8319),#5785,.T.);
#93293=ADVANCED_FACE('',(#8320,#6366),#6679,.F.);
#93294=ADVANCED_FACE('',(#8321),#6680,.F.);
#93295=ADVANCED_FACE('',(#8322),#186,.F.);
#93296=ADVANCED_FACE('',(#8323),#6681,.F.);
#93297=ADVANCED_FACE('',(#8324),#187,.T.);
#93298=ADVANCED_FACE('',(#8325),#6682,.F.);
#93299=ADVANCED_FACE('',(#8326,#6367),#6683,.F.);
#93300=ADVANCED_FACE('',(#8327,#6368),#6684,.F.);
#93301=ADVANCED_FACE('',(#8328),#5786,.F.);
#93302=ADVANCED_FACE('',(#8329),#5787,.F.);
#93303=ADVANCED_FACE('',(#8330),#5788,.T.);
#93304=ADVANCED_FACE('',(#8331),#5789,.T.);
#93305=ADVANCED_FACE('',(#8332),#6685,.F.);
#93306=ADVANCED_FACE('',(#8333),#6686,.T.);
#93307=ADVANCED_FACE('',(#8334),#6687,.F.);
#93308=ADVANCED_FACE('',(#8335),#90367,.T.);
#93309=ADVANCED_FACE('',(#8336),#90368,.T.);
#93310=ADVANCED_FACE('',(#8337),#90369,.F.);
#93311=ADVANCED_FACE('',(#8338),#2506,.F.);
#93312=ADVANCED_FACE('',(#8339),#90370,.F.);
#93313=ADVANCED_FACE('',(#8340),#90371,.F.);
#93314=ADVANCED_FACE('',(#8341),#2507,.F.);
#93315=ADVANCED_FACE('',(#8342),#2508,.F.);
#93316=ADVANCED_FACE('',(#8343),#90372,.F.);
#93317=ADVANCED_FACE('',(#8344),#90373,.F.);
#93318=ADVANCED_FACE('',(#8345),#2509,.F.);
#93319=ADVANCED_FACE('',(#8346),#90374,.F.);
#93320=ADVANCED_FACE('',(#8347),#5790,.F.);
#93321=ADVANCED_FACE('',(#8348),#2510,.F.);
#93322=ADVANCED_FACE('',(#8349),#2511,.F.);
#93323=ADVANCED_FACE('',(#8350),#90375,.F.);
#93324=ADVANCED_FACE('',(#8351),#90376,.F.);
#93325=ADVANCED_FACE('',(#8352),#2512,.F.);
#93326=ADVANCED_FACE('',(#8353),#2513,.F.);
#93327=ADVANCED_FACE('',(#8354),#5791,.F.);
#93328=ADVANCED_FACE('',(#8355),#90377,.F.);
#93329=ADVANCED_FACE('',(#8356),#2514,.F.);
#93330=ADVANCED_FACE('',(#8357),#90378,.F.);
#93331=ADVANCED_FACE('',(#8358),#90379,.F.);
#93332=ADVANCED_FACE('',(#8359),#2515,.F.);
#93333=ADVANCED_FACE('',(#8360),#2516,.F.);
#93334=ADVANCED_FACE('',(#8361),#90380,.F.);
#93335=ADVANCED_FACE('',(#8362),#90381,.F.);
#93336=ADVANCED_FACE('',(#8363),#2517,.F.);
#93337=ADVANCED_FACE('',(#8364),#90382,.F.);
#93338=ADVANCED_FACE('',(#8365),#6688,.F.);
#93339=ADVANCED_FACE('',(#8366),#6689,.T.);
#93340=ADVANCED_FACE('',(#8367),#6690,.F.);
#93341=ADVANCED_FACE('',(#8368),#6691,.F.);
#93342=ADVANCED_FACE('',(#8369),#6692,.T.);
#93343=ADVANCED_FACE('',(#8370),#6693,.F.);
#93344=ADVANCED_FACE('',(#8371),#6694,.F.);
#93345=ADVANCED_FACE('',(#8372),#6695,.T.);
#93346=ADVANCED_FACE('',(#8373),#6696,.F.);
#93347=ADVANCED_FACE('',(#8374),#6697,.F.);
#93348=ADVANCED_FACE('',(#8375),#6698,.T.);
#93349=ADVANCED_FACE('',(#8376),#6699,.F.);
#93350=ADVANCED_FACE('',(#8377),#6700,.F.);
#93351=ADVANCED_FACE('',(#8378),#6701,.T.);
#93352=ADVANCED_FACE('',(#8379),#6702,.F.);
#93353=ADVANCED_FACE('',(#8380),#6703,.F.);
#93354=ADVANCED_FACE('',(#8381),#6704,.T.);
#93355=ADVANCED_FACE('',(#8382),#6705,.F.);
#93356=ADVANCED_FACE('',(#8383),#6706,.F.);
#93357=ADVANCED_FACE('',(#8384),#6707,.T.);
#93358=ADVANCED_FACE('',(#8385),#6708,.F.);
#93359=ADVANCED_FACE('',(#8386),#6709,.F.);
#93360=ADVANCED_FACE('',(#8387),#6710,.T.);
#93361=ADVANCED_FACE('',(#8388),#6711,.F.);
#93362=ADVANCED_FACE('',(#8389),#6712,.F.);
#93363=ADVANCED_FACE('',(#8390),#6713,.T.);
#93364=ADVANCED_FACE('',(#8391),#6714,.F.);
#93365=ADVANCED_FACE('',(#8392),#6715,.F.);
#93366=ADVANCED_FACE('',(#8393),#6716,.T.);
#93367=ADVANCED_FACE('',(#8394),#6717,.F.);
#93368=ADVANCED_FACE('',(#8395),#6718,.F.);
#93369=ADVANCED_FACE('',(#8396),#6719,.T.);
#93370=ADVANCED_FACE('',(#8397),#6720,.F.);
#93371=ADVANCED_FACE('',(#8398),#6721,.F.);
#93372=ADVANCED_FACE('',(#8399),#6722,.T.);
#93373=ADVANCED_FACE('',(#8400),#6723,.F.);
#93374=ADVANCED_FACE('',(#8401),#6724,.F.);
#93375=ADVANCED_FACE('',(#8402),#6725,.T.);
#93376=ADVANCED_FACE('',(#8403),#6726,.F.);
#93377=ADVANCED_FACE('',(#8404),#6727,.F.);
#93378=ADVANCED_FACE('',(#8405),#6728,.T.);
#93379=ADVANCED_FACE('',(#8406),#6729,.F.);
#93380=ADVANCED_FACE('',(#8407),#6730,.F.);
#93381=ADVANCED_FACE('',(#8408),#6731,.T.);
#93382=ADVANCED_FACE('',(#8409),#6732,.F.);
#93383=ADVANCED_FACE('',(#8410),#6733,.F.);
#93384=ADVANCED_FACE('',(#8411),#6734,.T.);
#93385=ADVANCED_FACE('',(#8412),#6735,.F.);
#93386=ADVANCED_FACE('',(#8413),#6736,.F.);
#93387=ADVANCED_FACE('',(#8414),#6737,.T.);
#93388=ADVANCED_FACE('',(#8415),#6738,.F.);
#93389=ADVANCED_FACE('',(#8416),#6739,.F.);
#93390=ADVANCED_FACE('',(#8417),#6740,.T.);
#93391=ADVANCED_FACE('',(#8418),#6741,.F.);
#93392=ADVANCED_FACE('',(#8419),#6742,.F.);
#93393=ADVANCED_FACE('',(#8420),#6743,.T.);
#93394=ADVANCED_FACE('',(#8421),#6744,.F.);
#93395=ADVANCED_FACE('',(#8422),#6745,.F.);
#93396=ADVANCED_FACE('',(#8423),#6746,.T.);
#93397=ADVANCED_FACE('',(#8424),#6747,.F.);
#93398=ADVANCED_FACE('',(#8425),#6748,.F.);
#93399=ADVANCED_FACE('',(#8426),#6749,.T.);
#93400=ADVANCED_FACE('',(#8427),#6750,.F.);
#93401=ADVANCED_FACE('',(#8428),#6751,.F.);
#93402=ADVANCED_FACE('',(#8429),#6752,.T.);
#93403=ADVANCED_FACE('',(#8430),#6753,.F.);
#93404=ADVANCED_FACE('',(#8431),#6754,.F.);
#93405=ADVANCED_FACE('',(#8432),#6755,.T.);
#93406=ADVANCED_FACE('',(#8433),#6756,.F.);
#93407=ADVANCED_FACE('',(#8434),#6757,.F.);
#93408=ADVANCED_FACE('',(#8435),#6758,.T.);
#93409=ADVANCED_FACE('',(#8436),#6759,.F.);
#93410=ADVANCED_FACE('',(#8437),#6760,.F.);
#93411=ADVANCED_FACE('',(#8438),#6761,.T.);
#93412=ADVANCED_FACE('',(#8439),#6762,.F.);
#93413=ADVANCED_FACE('',(#8440),#6763,.F.);
#93414=ADVANCED_FACE('',(#8441),#6764,.T.);
#93415=ADVANCED_FACE('',(#8442),#6765,.F.);
#93416=ADVANCED_FACE('',(#8443),#6766,.F.);
#93417=ADVANCED_FACE('',(#8444),#6767,.T.);
#93418=ADVANCED_FACE('',(#8445),#6768,.F.);
#93419=ADVANCED_FACE('',(#8446),#6769,.F.);
#93420=ADVANCED_FACE('',(#8447),#6770,.T.);
#93421=ADVANCED_FACE('',(#8448),#6771,.F.);
#93422=ADVANCED_FACE('',(#8449),#6772,.F.);
#93423=ADVANCED_FACE('',(#8450),#6773,.T.);
#93424=ADVANCED_FACE('',(#8451),#6774,.F.);
#93425=ADVANCED_FACE('',(#8452),#6775,.F.);
#93426=ADVANCED_FACE('',(#8453),#6776,.T.);
#93427=ADVANCED_FACE('',(#8454),#6777,.F.);
#93428=ADVANCED_FACE('',(#8455),#6778,.F.);
#93429=ADVANCED_FACE('',(#8456),#6779,.T.);
#93430=ADVANCED_FACE('',(#8457),#6780,.F.);
#93431=ADVANCED_FACE('',(#8458),#6781,.F.);
#93432=ADVANCED_FACE('',(#8459),#6782,.T.);
#93433=ADVANCED_FACE('',(#8460),#6783,.F.);
#93434=ADVANCED_FACE('',(#8461),#6784,.F.);
#93435=ADVANCED_FACE('',(#8462),#6785,.T.);
#93436=ADVANCED_FACE('',(#8463),#6786,.F.);
#93437=ADVANCED_FACE('',(#8464),#6787,.F.);
#93438=ADVANCED_FACE('',(#8465),#6788,.T.);
#93439=ADVANCED_FACE('',(#8466),#6789,.F.);
#93440=ADVANCED_FACE('',(#8467),#6790,.F.);
#93441=ADVANCED_FACE('',(#8468),#6791,.T.);
#93442=ADVANCED_FACE('',(#8469),#6792,.F.);
#93443=ADVANCED_FACE('',(#8470),#6793,.F.);
#93444=ADVANCED_FACE('',(#8471),#6794,.T.);
#93445=ADVANCED_FACE('',(#8472),#6795,.F.);
#93446=ADVANCED_FACE('',(#8473),#6796,.F.);
#93447=ADVANCED_FACE('',(#8474),#6797,.T.);
#93448=ADVANCED_FACE('',(#8475),#6798,.F.);
#93449=ADVANCED_FACE('',(#8476),#6799,.F.);
#93450=ADVANCED_FACE('',(#8477),#6800,.T.);
#93451=ADVANCED_FACE('',(#8478),#6801,.F.);
#93452=ADVANCED_FACE('',(#8479),#6802,.F.);
#93453=ADVANCED_FACE('',(#8480),#6803,.T.);
#93454=ADVANCED_FACE('',(#8481),#6804,.F.);
#93455=ADVANCED_FACE('',(#8482),#6805,.F.);
#93456=ADVANCED_FACE('',(#8483),#6806,.T.);
#93457=ADVANCED_FACE('',(#8484),#6807,.F.);
#93458=ADVANCED_FACE('',(#8485),#6808,.F.);
#93459=ADVANCED_FACE('',(#8486),#6809,.T.);
#93460=ADVANCED_FACE('',(#8487),#6810,.F.);
#93461=ADVANCED_FACE('',(#8488),#6811,.F.);
#93462=ADVANCED_FACE('',(#8489),#6812,.T.);
#93463=ADVANCED_FACE('',(#8490),#6813,.F.);
#93464=ADVANCED_FACE('',(#8491),#6814,.F.);
#93465=ADVANCED_FACE('',(#8492),#6815,.T.);
#93466=ADVANCED_FACE('',(#8493),#6816,.F.);
#93467=ADVANCED_FACE('',(#8494),#6817,.F.);
#93468=ADVANCED_FACE('',(#8495),#6818,.T.);
#93469=ADVANCED_FACE('',(#8496),#6819,.F.);
#93470=ADVANCED_FACE('',(#8497),#6820,.F.);
#93471=ADVANCED_FACE('',(#8498),#6821,.T.);
#93472=ADVANCED_FACE('',(#8499),#6822,.F.);
#93473=ADVANCED_FACE('',(#8500),#6823,.F.);
#93474=ADVANCED_FACE('',(#8501),#6824,.T.);
#93475=ADVANCED_FACE('',(#8502),#6825,.F.);
#93476=ADVANCED_FACE('',(#8503),#6826,.F.);
#93477=ADVANCED_FACE('',(#8504),#6827,.T.);
#93478=ADVANCED_FACE('',(#8505),#6828,.F.);
#93479=ADVANCED_FACE('',(#8506),#6829,.F.);
#93480=ADVANCED_FACE('',(#8507),#6830,.T.);
#93481=ADVANCED_FACE('',(#8508),#6831,.F.);
#93482=ADVANCED_FACE('',(#8509),#6832,.F.);
#93483=ADVANCED_FACE('',(#8510),#6833,.T.);
#93484=ADVANCED_FACE('',(#8511),#6834,.F.);
#93485=ADVANCED_FACE('',(#8512),#6835,.F.);
#93486=ADVANCED_FACE('',(#8513),#6836,.T.);
#93487=ADVANCED_FACE('',(#8514),#6837,.F.);
#93488=ADVANCED_FACE('',(#8515),#6838,.F.);
#93489=ADVANCED_FACE('',(#8516),#6839,.T.);
#93490=ADVANCED_FACE('',(#8517),#6840,.F.);
#93491=ADVANCED_FACE('',(#8518),#6841,.F.);
#93492=ADVANCED_FACE('',(#8519),#6842,.T.);
#93493=ADVANCED_FACE('',(#8520),#6843,.F.);
#93494=ADVANCED_FACE('',(#8521),#6844,.F.);
#93495=ADVANCED_FACE('',(#8522),#6845,.T.);
#93496=ADVANCED_FACE('',(#8523),#6846,.F.);
#93497=ADVANCED_FACE('',(#8524),#6847,.F.);
#93498=ADVANCED_FACE('',(#8525),#6848,.T.);
#93499=ADVANCED_FACE('',(#8526),#6849,.F.);
#93500=ADVANCED_FACE('',(#8527),#6850,.F.);
#93501=ADVANCED_FACE('',(#8528),#6851,.T.);
#93502=ADVANCED_FACE('',(#8529),#6852,.F.);
#93503=ADVANCED_FACE('',(#8530),#6853,.F.);
#93504=ADVANCED_FACE('',(#8531),#6854,.T.);
#93505=ADVANCED_FACE('',(#8532),#6855,.F.);
#93506=ADVANCED_FACE('',(#8533),#6856,.F.);
#93507=ADVANCED_FACE('',(#8534),#6857,.T.);
#93508=ADVANCED_FACE('',(#8535),#6858,.F.);
#93509=ADVANCED_FACE('',(#8536),#6859,.F.);
#93510=ADVANCED_FACE('',(#8537),#6860,.T.);
#93511=ADVANCED_FACE('',(#8538),#6861,.F.);
#93512=ADVANCED_FACE('',(#8539),#6862,.F.);
#93513=ADVANCED_FACE('',(#8540),#6863,.T.);
#93514=ADVANCED_FACE('',(#8541),#6864,.F.);
#93515=ADVANCED_FACE('',(#8542),#90383,.T.);
#93516=ADVANCED_FACE('',(#8543),#90384,.T.);
#93517=ADVANCED_FACE('',(#8544),#90385,.T.);
#93518=ADVANCED_FACE('',(#8545),#90386,.T.);
#93519=ADVANCED_FACE('',(#8546),#90387,.T.);
#93520=ADVANCED_FACE('',(#8547),#90388,.T.);
#93521=ADVANCED_FACE('',(#8548),#90389,.T.);
#93522=ADVANCED_FACE('',(#8549),#90390,.T.);
#93523=ADVANCED_FACE('',(#8550),#90391,.T.);
#93524=ADVANCED_FACE('',(#8551),#90392,.T.);
#93525=ADVANCED_FACE('',(#8552),#90393,.T.);
#93526=ADVANCED_FACE('',(#8553),#90394,.T.);
#93527=ADVANCED_FACE('',(#8554),#90395,.T.);
#93528=ADVANCED_FACE('',(#8555),#90396,.T.);
#93529=ADVANCED_FACE('',(#8556),#90397,.T.);
#93530=ADVANCED_FACE('',(#8557),#90398,.T.);
#93531=ADVANCED_FACE('',(#8558),#90399,.T.);
#93532=ADVANCED_FACE('',(#8559),#90400,.T.);
#93533=ADVANCED_FACE('',(#8560),#90401,.T.);
#93534=ADVANCED_FACE('',(#8561),#90402,.T.);
#93535=ADVANCED_FACE('',(#8562),#90403,.T.);
#93536=ADVANCED_FACE('',(#8563),#90404,.T.);
#93537=ADVANCED_FACE('',(#8564),#90405,.T.);
#93538=ADVANCED_FACE('',(#8565),#90406,.T.);
#93539=ADVANCED_FACE('',(#8566),#90407,.T.);
#93540=ADVANCED_FACE('',(#8567),#90408,.T.);
#93541=ADVANCED_FACE('',(#8568),#90409,.T.);
#93542=ADVANCED_FACE('',(#8569),#90410,.T.);
#93543=ADVANCED_FACE('',(#8570),#90411,.T.);
#93544=ADVANCED_FACE('',(#8571),#90412,.T.);
#93545=ADVANCED_FACE('',(#8572),#90413,.T.);
#93546=ADVANCED_FACE('',(#8573),#90414,.T.);
#93547=ADVANCED_FACE('',(#8574),#90415,.T.);
#93548=ADVANCED_FACE('',(#8575),#90416,.T.);
#93549=ADVANCED_FACE('',(#8576),#90417,.T.);
#93550=ADVANCED_FACE('',(#8577),#90418,.T.);
#93551=ADVANCED_FACE('',(#8578),#90419,.T.);
#93552=ADVANCED_FACE('',(#8579),#90420,.T.);
#93553=ADVANCED_FACE('',(#8580),#90421,.T.);
#93554=ADVANCED_FACE('',(#8581),#90422,.T.);
#93555=ADVANCED_FACE('',(#8582),#90423,.T.);
#93556=ADVANCED_FACE('',(#8583),#90424,.T.);
#93557=ADVANCED_FACE('',(#8584),#90425,.T.);
#93558=ADVANCED_FACE('',(#8585),#90426,.T.);
#93559=ADVANCED_FACE('',(#8586),#90427,.T.);
#93560=ADVANCED_FACE('',(#8587),#90428,.T.);
#93561=ADVANCED_FACE('',(#8588),#90429,.T.);
#93562=ADVANCED_FACE('',(#8589),#90430,.T.);
#93563=ADVANCED_FACE('',(#8590),#90431,.T.);
#93564=ADVANCED_FACE('',(#8591),#90432,.T.);
#93565=ADVANCED_FACE('',(#8592),#90433,.T.);
#93566=ADVANCED_FACE('',(#8593),#90434,.T.);
#93567=ADVANCED_FACE('',(#8594),#90435,.T.);
#93568=ADVANCED_FACE('',(#8595),#90436,.T.);
#93569=ADVANCED_FACE('',(#8596),#90437,.T.);
#93570=ADVANCED_FACE('',(#8597),#90438,.T.);
#93571=ADVANCED_FACE('',(#8598),#90439,.T.);
#93572=ADVANCED_FACE('',(#8599),#90440,.T.);
#93573=ADVANCED_FACE('',(#8600),#90441,.T.);
#93574=ADVANCED_FACE('',(#8601),#90442,.T.);
#93575=ADVANCED_FACE('',(#8602),#90443,.T.);
#93576=ADVANCED_FACE('',(#8603),#90444,.T.);
#93577=ADVANCED_FACE('',(#8604),#90445,.T.);
#93578=ADVANCED_FACE('',(#8605),#90446,.T.);
#93579=ADVANCED_FACE('',(#8606),#90447,.T.);
#93580=ADVANCED_FACE('',(#8607),#90448,.T.);
#93581=ADVANCED_FACE('',(#8608),#90449,.T.);
#93582=ADVANCED_FACE('',(#8609),#90450,.T.);
#93583=ADVANCED_FACE('',(#8610),#90451,.T.);
#93584=ADVANCED_FACE('',(#8611),#90452,.T.);
#93585=ADVANCED_FACE('',(#8612),#90453,.T.);
#93586=ADVANCED_FACE('',(#8613),#90454,.T.);
#93587=ADVANCED_FACE('',(#8614),#90455,.T.);
#93588=ADVANCED_FACE('',(#8615),#90456,.T.);
#93589=ADVANCED_FACE('',(#8616),#90457,.T.);
#93590=ADVANCED_FACE('',(#8617),#90458,.T.);
#93591=ADVANCED_FACE('',(#8618),#90459,.T.);
#93592=ADVANCED_FACE('',(#8619),#90460,.T.);
#93593=ADVANCED_FACE('',(#8620),#90461,.T.);
#93594=ADVANCED_FACE('',(#8621),#90462,.T.);
#93595=ADVANCED_FACE('',(#8622),#90463,.T.);
#93596=ADVANCED_FACE('',(#8623),#90464,.T.);
#93597=ADVANCED_FACE('',(#8624),#90465,.T.);
#93598=ADVANCED_FACE('',(#8625),#90466,.T.);
#93599=ADVANCED_FACE('',(#8626),#90467,.T.);
#93600=ADVANCED_FACE('',(#8627),#90468,.T.);
#93601=ADVANCED_FACE('',(#8628),#90469,.T.);
#93602=ADVANCED_FACE('',(#8629),#90470,.T.);
#93603=ADVANCED_FACE('',(#8630),#90471,.T.);
#93604=ADVANCED_FACE('',(#8631),#90472,.T.);
#93605=ADVANCED_FACE('',(#8632),#90473,.T.);
#93606=ADVANCED_FACE('',(#8633),#90474,.T.);
#93607=ADVANCED_FACE('',(#8634),#90475,.T.);
#93608=ADVANCED_FACE('',(#8635),#90476,.T.);
#93609=ADVANCED_FACE('',(#8636),#90477,.T.);
#93610=ADVANCED_FACE('',(#8637),#90478,.T.);
#93611=ADVANCED_FACE('',(#8638),#90479,.T.);
#93612=ADVANCED_FACE('',(#8639),#90480,.T.);
#93613=ADVANCED_FACE('',(#8640),#90481,.T.);
#93614=ADVANCED_FACE('',(#8641),#90482,.T.);
#93615=ADVANCED_FACE('',(#8642),#90483,.T.);
#93616=ADVANCED_FACE('',(#8643),#90484,.T.);
#93617=ADVANCED_FACE('',(#8644),#90485,.T.);
#93618=ADVANCED_FACE('',(#8645),#90486,.T.);
#93619=ADVANCED_FACE('',(#8646),#90487,.T.);
#93620=ADVANCED_FACE('',(#8647),#90488,.T.);
#93621=ADVANCED_FACE('',(#8648),#90489,.T.);
#93622=ADVANCED_FACE('',(#8649),#90490,.T.);
#93623=ADVANCED_FACE('',(#8650),#90491,.T.);
#93624=ADVANCED_FACE('',(#8651),#90492,.T.);
#93625=ADVANCED_FACE('',(#8652),#90493,.T.);
#93626=ADVANCED_FACE('',(#8653),#90494,.T.);
#93627=ADVANCED_FACE('',(#8654),#90495,.T.);
#93628=ADVANCED_FACE('',(#8655),#90496,.T.);
#93629=ADVANCED_FACE('',(#8656),#90497,.T.);
#93630=ADVANCED_FACE('',(#8657),#90498,.T.);
#93631=ADVANCED_FACE('',(#8658),#90499,.T.);
#93632=ADVANCED_FACE('',(#8659),#90500,.T.);
#93633=ADVANCED_FACE('',(#8660),#90501,.F.);
#93634=ADVANCED_FACE('',(#8661),#2518,.F.);
#93635=ADVANCED_FACE('',(#8662),#90502,.F.);
#93636=ADVANCED_FACE('',(#8663),#90503,.F.);
#93637=ADVANCED_FACE('',(#8664),#2519,.F.);
#93638=ADVANCED_FACE('',(#8665),#2520,.F.);
#93639=ADVANCED_FACE('',(#8666),#90504,.F.);
#93640=ADVANCED_FACE('',(#8667),#90505,.F.);
#93641=ADVANCED_FACE('',(#8668),#2521,.F.);
#93642=ADVANCED_FACE('',(#8669),#90506,.F.);
#93643=ADVANCED_FACE('',(#8670),#5792,.F.);
#93644=ADVANCED_FACE('',(#8671),#2522,.F.);
#93645=ADVANCED_FACE('',(#8672),#2523,.F.);
#93646=ADVANCED_FACE('',(#8673),#90507,.F.);
#93647=ADVANCED_FACE('',(#8674),#90508,.F.);
#93648=ADVANCED_FACE('',(#8675),#2524,.F.);
#93649=ADVANCED_FACE('',(#8676),#2525,.F.);
#93650=ADVANCED_FACE('',(#8677),#5793,.F.);
#93651=ADVANCED_FACE('',(#8678),#90509,.F.);
#93652=ADVANCED_FACE('',(#8679),#2526,.F.);
#93653=ADVANCED_FACE('',(#8680),#90510,.F.);
#93654=ADVANCED_FACE('',(#8681),#90511,.F.);
#93655=ADVANCED_FACE('',(#8682),#2527,.F.);
#93656=ADVANCED_FACE('',(#8683),#2528,.F.);
#93657=ADVANCED_FACE('',(#8684),#90512,.F.);
#93658=ADVANCED_FACE('',(#8685),#90513,.F.);
#93659=ADVANCED_FACE('',(#8686),#2529,.F.);
#93660=ADVANCED_FACE('',(#8687),#90514,.F.);
#93661=ADVANCED_FACE('',(#8688),#90515,.F.);
#93662=ADVANCED_FACE('',(#8689),#2530,.F.);
#93663=ADVANCED_FACE('',(#8690),#90516,.F.);
#93664=ADVANCED_FACE('',(#8691),#90517,.F.);
#93665=ADVANCED_FACE('',(#8692),#2531,.F.);
#93666=ADVANCED_FACE('',(#8693),#2532,.F.);
#93667=ADVANCED_FACE('',(#8694),#90518,.F.);
#93668=ADVANCED_FACE('',(#8695),#90519,.F.);
#93669=ADVANCED_FACE('',(#8696),#2533,.F.);
#93670=ADVANCED_FACE('',(#8697),#90520,.F.);
#93671=ADVANCED_FACE('',(#8698),#5794,.F.);
#93672=ADVANCED_FACE('',(#8699),#2534,.F.);
#93673=ADVANCED_FACE('',(#8700),#2535,.F.);
#93674=ADVANCED_FACE('',(#8701),#90521,.F.);
#93675=ADVANCED_FACE('',(#8702),#90522,.F.);
#93676=ADVANCED_FACE('',(#8703),#2536,.F.);
#93677=ADVANCED_FACE('',(#8704),#2537,.F.);
#93678=ADVANCED_FACE('',(#8705),#5795,.F.);
#93679=ADVANCED_FACE('',(#8706),#90523,.F.);
#93680=ADVANCED_FACE('',(#8707),#2538,.F.);
#93681=ADVANCED_FACE('',(#8708),#90524,.F.);
#93682=ADVANCED_FACE('',(#8709),#90525,.F.);
#93683=ADVANCED_FACE('',(#8710),#2539,.F.);
#93684=ADVANCED_FACE('',(#8711),#2540,.F.);
#93685=ADVANCED_FACE('',(#8712),#90526,.F.);
#93686=ADVANCED_FACE('',(#8713),#90527,.F.);
#93687=ADVANCED_FACE('',(#8714),#2541,.F.);
#93688=ADVANCED_FACE('',(#8715),#90528,.F.);
#93689=ADVANCED_FACE('',(#8716),#90529,.F.);
#93690=ADVANCED_FACE('',(#8717),#2542,.F.);
#93691=ADVANCED_FACE('',(#8718),#90530,.F.);
#93692=ADVANCED_FACE('',(#8719),#90531,.F.);
#93693=ADVANCED_FACE('',(#8720),#2543,.F.);
#93694=ADVANCED_FACE('',(#8721),#2544,.F.);
#93695=ADVANCED_FACE('',(#8722),#90532,.F.);
#93696=ADVANCED_FACE('',(#8723),#90533,.F.);
#93697=ADVANCED_FACE('',(#8724),#2545,.F.);
#93698=ADVANCED_FACE('',(#8725),#90534,.F.);
#93699=ADVANCED_FACE('',(#8726),#5796,.F.);
#93700=ADVANCED_FACE('',(#8727),#2546,.F.);
#93701=ADVANCED_FACE('',(#8728),#2547,.F.);
#93702=ADVANCED_FACE('',(#8729),#90535,.F.);
#93703=ADVANCED_FACE('',(#8730),#90536,.F.);
#93704=ADVANCED_FACE('',(#8731),#2548,.F.);
#93705=ADVANCED_FACE('',(#8732),#2549,.F.);
#93706=ADVANCED_FACE('',(#8733),#5797,.F.);
#93707=ADVANCED_FACE('',(#8734),#90537,.F.);
#93708=ADVANCED_FACE('',(#8735),#2550,.F.);
#93709=ADVANCED_FACE('',(#8736),#90538,.F.);
#93710=ADVANCED_FACE('',(#8737),#90539,.F.);
#93711=ADVANCED_FACE('',(#8738),#2551,.F.);
#93712=ADVANCED_FACE('',(#8739),#2552,.F.);
#93713=ADVANCED_FACE('',(#8740),#90540,.F.);
#93714=ADVANCED_FACE('',(#8741),#90541,.F.);
#93715=ADVANCED_FACE('',(#8742),#2553,.F.);
#93716=ADVANCED_FACE('',(#8743),#90542,.F.);
#93717=ADVANCED_FACE('',(#8744),#90543,.F.);
#93718=ADVANCED_FACE('',(#8745),#2554,.F.);
#93719=ADVANCED_FACE('',(#8746),#90544,.F.);
#93720=ADVANCED_FACE('',(#8747),#90545,.F.);
#93721=ADVANCED_FACE('',(#8748),#2555,.F.);
#93722=ADVANCED_FACE('',(#8749),#2556,.F.);
#93723=ADVANCED_FACE('',(#8750),#90546,.F.);
#93724=ADVANCED_FACE('',(#8751),#90547,.F.);
#93725=ADVANCED_FACE('',(#8752),#2557,.F.);
#93726=ADVANCED_FACE('',(#8753),#90548,.F.);
#93727=ADVANCED_FACE('',(#8754),#5798,.F.);
#93728=ADVANCED_FACE('',(#8755),#2558,.F.);
#93729=ADVANCED_FACE('',(#8756),#2559,.F.);
#93730=ADVANCED_FACE('',(#8757),#90549,.F.);
#93731=ADVANCED_FACE('',(#8758),#90550,.F.);
#93732=ADVANCED_FACE('',(#8759),#2560,.F.);
#93733=ADVANCED_FACE('',(#8760),#2561,.F.);
#93734=ADVANCED_FACE('',(#8761),#5799,.F.);
#93735=ADVANCED_FACE('',(#8762),#90551,.F.);
#93736=ADVANCED_FACE('',(#8763),#2562,.F.);
#93737=ADVANCED_FACE('',(#8764),#90552,.F.);
#93738=ADVANCED_FACE('',(#8765),#90553,.F.);
#93739=ADVANCED_FACE('',(#8766),#2563,.F.);
#93740=ADVANCED_FACE('',(#8767),#2564,.F.);
#93741=ADVANCED_FACE('',(#8768),#90554,.F.);
#93742=ADVANCED_FACE('',(#8769),#90555,.F.);
#93743=ADVANCED_FACE('',(#8770),#2565,.F.);
#93744=ADVANCED_FACE('',(#8771),#90556,.F.);
#93745=ADVANCED_FACE('',(#8772),#90557,.F.);
#93746=ADVANCED_FACE('',(#8773),#2566,.F.);
#93747=ADVANCED_FACE('',(#8774),#90558,.F.);
#93748=ADVANCED_FACE('',(#8775),#90559,.F.);
#93749=ADVANCED_FACE('',(#8776),#2567,.F.);
#93750=ADVANCED_FACE('',(#8777),#2568,.F.);
#93751=ADVANCED_FACE('',(#8778),#90560,.F.);
#93752=ADVANCED_FACE('',(#8779),#90561,.F.);
#93753=ADVANCED_FACE('',(#8780),#2569,.F.);
#93754=ADVANCED_FACE('',(#8781),#90562,.F.);
#93755=ADVANCED_FACE('',(#8782),#5800,.F.);
#93756=ADVANCED_FACE('',(#8783),#2570,.F.);
#93757=ADVANCED_FACE('',(#8784),#2571,.F.);
#93758=ADVANCED_FACE('',(#8785),#90563,.F.);
#93759=ADVANCED_FACE('',(#8786),#90564,.F.);
#93760=ADVANCED_FACE('',(#8787),#2572,.F.);
#93761=ADVANCED_FACE('',(#8788),#2573,.F.);
#93762=ADVANCED_FACE('',(#8789),#5801,.F.);
#93763=ADVANCED_FACE('',(#8790),#90565,.F.);
#93764=ADVANCED_FACE('',(#8791),#2574,.F.);
#93765=ADVANCED_FACE('',(#8792),#90566,.F.);
#93766=ADVANCED_FACE('',(#8793),#90567,.F.);
#93767=ADVANCED_FACE('',(#8794),#2575,.F.);
#93768=ADVANCED_FACE('',(#8795),#2576,.F.);
#93769=ADVANCED_FACE('',(#8796),#90568,.F.);
#93770=ADVANCED_FACE('',(#8797),#90569,.F.);
#93771=ADVANCED_FACE('',(#8798),#2577,.F.);
#93772=ADVANCED_FACE('',(#8799),#90570,.F.);
#93773=ADVANCED_FACE('',(#8800),#90571,.F.);
#93774=ADVANCED_FACE('',(#8801),#2578,.F.);
#93775=ADVANCED_FACE('',(#8802),#90572,.F.);
#93776=ADVANCED_FACE('',(#8803),#90573,.F.);
#93777=ADVANCED_FACE('',(#8804),#2579,.F.);
#93778=ADVANCED_FACE('',(#8805),#2580,.F.);
#93779=ADVANCED_FACE('',(#8806),#90574,.F.);
#93780=ADVANCED_FACE('',(#8807),#90575,.F.);
#93781=ADVANCED_FACE('',(#8808),#2581,.F.);
#93782=ADVANCED_FACE('',(#8809),#90576,.F.);
#93783=ADVANCED_FACE('',(#8810),#5802,.F.);
#93784=ADVANCED_FACE('',(#8811),#2582,.F.);
#93785=ADVANCED_FACE('',(#8812),#2583,.F.);
#93786=ADVANCED_FACE('',(#8813),#90577,.F.);
#93787=ADVANCED_FACE('',(#8814),#90578,.F.);
#93788=ADVANCED_FACE('',(#8815),#2584,.F.);
#93789=ADVANCED_FACE('',(#8816),#2585,.F.);
#93790=ADVANCED_FACE('',(#8817),#5803,.F.);
#93791=ADVANCED_FACE('',(#8818),#90579,.F.);
#93792=ADVANCED_FACE('',(#8819),#2586,.F.);
#93793=ADVANCED_FACE('',(#8820),#90580,.F.);
#93794=ADVANCED_FACE('',(#8821),#90581,.F.);
#93795=ADVANCED_FACE('',(#8822),#2587,.F.);
#93796=ADVANCED_FACE('',(#8823),#2588,.F.);
#93797=ADVANCED_FACE('',(#8824),#90582,.F.);
#93798=ADVANCED_FACE('',(#8825),#90583,.F.);
#93799=ADVANCED_FACE('',(#8826),#2589,.F.);
#93800=ADVANCED_FACE('',(#8827),#90584,.F.);
#93801=ADVANCED_FACE('',(#8828),#90585,.F.);
#93802=ADVANCED_FACE('',(#8829),#2590,.F.);
#93803=ADVANCED_FACE('',(#8830),#90586,.F.);
#93804=ADVANCED_FACE('',(#8831),#90587,.F.);
#93805=ADVANCED_FACE('',(#8832),#2591,.F.);
#93806=ADVANCED_FACE('',(#8833),#2592,.F.);
#93807=ADVANCED_FACE('',(#8834),#90588,.F.);
#93808=ADVANCED_FACE('',(#8835),#90589,.F.);
#93809=ADVANCED_FACE('',(#8836),#2593,.F.);
#93810=ADVANCED_FACE('',(#8837),#90590,.F.);
#93811=ADVANCED_FACE('',(#8838),#5804,.F.);
#93812=ADVANCED_FACE('',(#8839),#2594,.F.);
#93813=ADVANCED_FACE('',(#8840),#2595,.F.);
#93814=ADVANCED_FACE('',(#8841),#90591,.F.);
#93815=ADVANCED_FACE('',(#8842),#90592,.F.);
#93816=ADVANCED_FACE('',(#8843),#2596,.F.);
#93817=ADVANCED_FACE('',(#8844),#2597,.F.);
#93818=ADVANCED_FACE('',(#8845),#5805,.F.);
#93819=ADVANCED_FACE('',(#8846),#90593,.F.);
#93820=ADVANCED_FACE('',(#8847),#2598,.F.);
#93821=ADVANCED_FACE('',(#8848),#90594,.F.);
#93822=ADVANCED_FACE('',(#8849),#90595,.F.);
#93823=ADVANCED_FACE('',(#8850),#2599,.F.);
#93824=ADVANCED_FACE('',(#8851),#2600,.F.);
#93825=ADVANCED_FACE('',(#8852),#90596,.F.);
#93826=ADVANCED_FACE('',(#8853),#90597,.F.);
#93827=ADVANCED_FACE('',(#8854),#2601,.F.);
#93828=ADVANCED_FACE('',(#8855),#90598,.F.);
#93829=ADVANCED_FACE('',(#8856),#90599,.F.);
#93830=ADVANCED_FACE('',(#8857),#2602,.F.);
#93831=ADVANCED_FACE('',(#8858),#90600,.F.);
#93832=ADVANCED_FACE('',(#8859),#90601,.F.);
#93833=ADVANCED_FACE('',(#8860),#2603,.F.);
#93834=ADVANCED_FACE('',(#8861),#2604,.F.);
#93835=ADVANCED_FACE('',(#8862),#90602,.F.);
#93836=ADVANCED_FACE('',(#8863),#90603,.F.);
#93837=ADVANCED_FACE('',(#8864),#2605,.F.);
#93838=ADVANCED_FACE('',(#8865),#90604,.F.);
#93839=ADVANCED_FACE('',(#8866),#5806,.F.);
#93840=ADVANCED_FACE('',(#8867),#2606,.F.);
#93841=ADVANCED_FACE('',(#8868),#2607,.F.);
#93842=ADVANCED_FACE('',(#8869),#90605,.F.);
#93843=ADVANCED_FACE('',(#8870),#90606,.F.);
#93844=ADVANCED_FACE('',(#8871),#2608,.F.);
#93845=ADVANCED_FACE('',(#8872),#2609,.F.);
#93846=ADVANCED_FACE('',(#8873),#5807,.F.);
#93847=ADVANCED_FACE('',(#8874),#90607,.F.);
#93848=ADVANCED_FACE('',(#8875),#2610,.F.);
#93849=ADVANCED_FACE('',(#8876),#90608,.F.);
#93850=ADVANCED_FACE('',(#8877),#90609,.F.);
#93851=ADVANCED_FACE('',(#8878),#2611,.F.);
#93852=ADVANCED_FACE('',(#8879),#2612,.F.);
#93853=ADVANCED_FACE('',(#8880),#90610,.F.);
#93854=ADVANCED_FACE('',(#8881),#90611,.F.);
#93855=ADVANCED_FACE('',(#8882),#2613,.F.);
#93856=ADVANCED_FACE('',(#8883),#90612,.F.);
#93857=ADVANCED_FACE('',(#8884),#90613,.F.);
#93858=ADVANCED_FACE('',(#8885),#2614,.F.);
#93859=ADVANCED_FACE('',(#8886),#90614,.F.);
#93860=ADVANCED_FACE('',(#8887),#90615,.F.);
#93861=ADVANCED_FACE('',(#8888),#2615,.F.);
#93862=ADVANCED_FACE('',(#8889),#2616,.F.);
#93863=ADVANCED_FACE('',(#8890),#90616,.F.);
#93864=ADVANCED_FACE('',(#8891),#90617,.F.);
#93865=ADVANCED_FACE('',(#8892),#2617,.F.);
#93866=ADVANCED_FACE('',(#8893),#90618,.F.);
#93867=ADVANCED_FACE('',(#8894),#5808,.F.);
#93868=ADVANCED_FACE('',(#8895),#2618,.F.);
#93869=ADVANCED_FACE('',(#8896),#2619,.F.);
#93870=ADVANCED_FACE('',(#8897),#90619,.F.);
#93871=ADVANCED_FACE('',(#8898),#90620,.F.);
#93872=ADVANCED_FACE('',(#8899),#2620,.F.);
#93873=ADVANCED_FACE('',(#8900),#2621,.F.);
#93874=ADVANCED_FACE('',(#8901),#5809,.F.);
#93875=ADVANCED_FACE('',(#8902),#90621,.F.);
#93876=ADVANCED_FACE('',(#8903),#2622,.F.);
#93877=ADVANCED_FACE('',(#8904),#90622,.F.);
#93878=ADVANCED_FACE('',(#8905),#90623,.F.);
#93879=ADVANCED_FACE('',(#8906),#2623,.F.);
#93880=ADVANCED_FACE('',(#8907),#2624,.F.);
#93881=ADVANCED_FACE('',(#8908),#90624,.F.);
#93882=ADVANCED_FACE('',(#8909),#90625,.F.);
#93883=ADVANCED_FACE('',(#8910),#2625,.F.);
#93884=ADVANCED_FACE('',(#8911),#90626,.F.);
#93885=ADVANCED_FACE('',(#8912),#90627,.F.);
#93886=ADVANCED_FACE('',(#8913),#2626,.F.);
#93887=ADVANCED_FACE('',(#8914),#90628,.F.);
#93888=ADVANCED_FACE('',(#8915),#90629,.F.);
#93889=ADVANCED_FACE('',(#8916),#2627,.F.);
#93890=ADVANCED_FACE('',(#8917),#2628,.F.);
#93891=ADVANCED_FACE('',(#8918),#90630,.F.);
#93892=ADVANCED_FACE('',(#8919),#90631,.F.);
#93893=ADVANCED_FACE('',(#8920),#2629,.F.);
#93894=ADVANCED_FACE('',(#8921),#90632,.F.);
#93895=ADVANCED_FACE('',(#8922),#5810,.F.);
#93896=ADVANCED_FACE('',(#8923),#2630,.F.);
#93897=ADVANCED_FACE('',(#8924),#2631,.F.);
#93898=ADVANCED_FACE('',(#8925),#90633,.F.);
#93899=ADVANCED_FACE('',(#8926),#90634,.F.);
#93900=ADVANCED_FACE('',(#8927),#2632,.F.);
#93901=ADVANCED_FACE('',(#8928),#2633,.F.);
#93902=ADVANCED_FACE('',(#8929),#5811,.F.);
#93903=ADVANCED_FACE('',(#8930),#90635,.F.);
#93904=ADVANCED_FACE('',(#8931),#2634,.F.);
#93905=ADVANCED_FACE('',(#8932),#90636,.F.);
#93906=ADVANCED_FACE('',(#8933),#90637,.F.);
#93907=ADVANCED_FACE('',(#8934),#2635,.F.);
#93908=ADVANCED_FACE('',(#8935),#2636,.F.);
#93909=ADVANCED_FACE('',(#8936),#90638,.F.);
#93910=ADVANCED_FACE('',(#8937),#90639,.F.);
#93911=ADVANCED_FACE('',(#8938),#2637,.F.);
#93912=ADVANCED_FACE('',(#8939),#90640,.F.);
#93913=ADVANCED_FACE('',(#8940),#90641,.F.);
#93914=ADVANCED_FACE('',(#8941),#2638,.F.);
#93915=ADVANCED_FACE('',(#8942),#90642,.F.);
#93916=ADVANCED_FACE('',(#8943),#90643,.F.);
#93917=ADVANCED_FACE('',(#8944),#2639,.F.);
#93918=ADVANCED_FACE('',(#8945),#2640,.F.);
#93919=ADVANCED_FACE('',(#8946),#90644,.F.);
#93920=ADVANCED_FACE('',(#8947),#90645,.F.);
#93921=ADVANCED_FACE('',(#8948),#2641,.F.);
#93922=ADVANCED_FACE('',(#8949),#90646,.F.);
#93923=ADVANCED_FACE('',(#8950),#5812,.F.);
#93924=ADVANCED_FACE('',(#8951),#2642,.F.);
#93925=ADVANCED_FACE('',(#8952),#2643,.F.);
#93926=ADVANCED_FACE('',(#8953),#90647,.F.);
#93927=ADVANCED_FACE('',(#8954),#90648,.F.);
#93928=ADVANCED_FACE('',(#8955),#2644,.F.);
#93929=ADVANCED_FACE('',(#8956),#2645,.F.);
#93930=ADVANCED_FACE('',(#8957),#5813,.F.);
#93931=ADVANCED_FACE('',(#8958),#90649,.F.);
#93932=ADVANCED_FACE('',(#8959),#2646,.F.);
#93933=ADVANCED_FACE('',(#8960),#90650,.F.);
#93934=ADVANCED_FACE('',(#8961),#90651,.F.);
#93935=ADVANCED_FACE('',(#8962),#2647,.F.);
#93936=ADVANCED_FACE('',(#8963),#2648,.F.);
#93937=ADVANCED_FACE('',(#8964),#90652,.F.);
#93938=ADVANCED_FACE('',(#8965),#90653,.F.);
#93939=ADVANCED_FACE('',(#8966),#2649,.F.);
#93940=ADVANCED_FACE('',(#8967),#90654,.F.);
#93941=ADVANCED_FACE('',(#8968),#90655,.F.);
#93942=ADVANCED_FACE('',(#8969),#2650,.F.);
#93943=ADVANCED_FACE('',(#8970),#90656,.F.);
#93944=ADVANCED_FACE('',(#8971),#90657,.F.);
#93945=ADVANCED_FACE('',(#8972),#2651,.F.);
#93946=ADVANCED_FACE('',(#8973),#2652,.F.);
#93947=ADVANCED_FACE('',(#8974),#90658,.F.);
#93948=ADVANCED_FACE('',(#8975),#90659,.F.);
#93949=ADVANCED_FACE('',(#8976),#2653,.F.);
#93950=ADVANCED_FACE('',(#8977),#90660,.F.);
#93951=ADVANCED_FACE('',(#8978),#5814,.F.);
#93952=ADVANCED_FACE('',(#8979),#2654,.F.);
#93953=ADVANCED_FACE('',(#8980),#2655,.F.);
#93954=ADVANCED_FACE('',(#8981),#90661,.F.);
#93955=ADVANCED_FACE('',(#8982),#90662,.F.);
#93956=ADVANCED_FACE('',(#8983),#2656,.F.);
#93957=ADVANCED_FACE('',(#8984),#2657,.F.);
#93958=ADVANCED_FACE('',(#8985),#5815,.F.);
#93959=ADVANCED_FACE('',(#8986),#90663,.F.);
#93960=ADVANCED_FACE('',(#8987),#2658,.F.);
#93961=ADVANCED_FACE('',(#8988),#90664,.F.);
#93962=ADVANCED_FACE('',(#8989),#90665,.F.);
#93963=ADVANCED_FACE('',(#8990),#2659,.F.);
#93964=ADVANCED_FACE('',(#8991),#2660,.F.);
#93965=ADVANCED_FACE('',(#8992),#90666,.F.);
#93966=ADVANCED_FACE('',(#8993),#90667,.F.);
#93967=ADVANCED_FACE('',(#8994),#2661,.F.);
#93968=ADVANCED_FACE('',(#8995),#90668,.F.);
#93969=ADVANCED_FACE('',(#8996),#90669,.F.);
#93970=ADVANCED_FACE('',(#8997),#2662,.F.);
#93971=ADVANCED_FACE('',(#8998),#90670,.F.);
#93972=ADVANCED_FACE('',(#8999),#90671,.F.);
#93973=ADVANCED_FACE('',(#9000),#2663,.F.);
#93974=ADVANCED_FACE('',(#9001),#2664,.F.);
#93975=ADVANCED_FACE('',(#9002),#90672,.F.);
#93976=ADVANCED_FACE('',(#9003),#90673,.F.);
#93977=ADVANCED_FACE('',(#9004),#2665,.F.);
#93978=ADVANCED_FACE('',(#9005),#90674,.F.);
#93979=ADVANCED_FACE('',(#9006),#5816,.F.);
#93980=ADVANCED_FACE('',(#9007),#2666,.F.);
#93981=ADVANCED_FACE('',(#9008),#2667,.F.);
#93982=ADVANCED_FACE('',(#9009),#90675,.F.);
#93983=ADVANCED_FACE('',(#9010),#90676,.F.);
#93984=ADVANCED_FACE('',(#9011),#2668,.F.);
#93985=ADVANCED_FACE('',(#9012),#2669,.F.);
#93986=ADVANCED_FACE('',(#9013),#5817,.F.);
#93987=ADVANCED_FACE('',(#9014),#90677,.F.);
#93988=ADVANCED_FACE('',(#9015),#2670,.F.);
#93989=ADVANCED_FACE('',(#9016),#90678,.F.);
#93990=ADVANCED_FACE('',(#9017),#90679,.F.);
#93991=ADVANCED_FACE('',(#9018),#2671,.F.);
#93992=ADVANCED_FACE('',(#9019),#2672,.F.);
#93993=ADVANCED_FACE('',(#9020),#90680,.F.);
#93994=ADVANCED_FACE('',(#9021),#90681,.F.);
#93995=ADVANCED_FACE('',(#9022),#2673,.F.);
#93996=ADVANCED_FACE('',(#9023),#90682,.F.);
#93997=ADVANCED_FACE('',(#9024),#90683,.F.);
#93998=ADVANCED_FACE('',(#9025),#2674,.F.);
#93999=ADVANCED_FACE('',(#9026),#90684,.F.);
#94000=ADVANCED_FACE('',(#9027),#90685,.F.);
#94001=ADVANCED_FACE('',(#9028),#2675,.F.);
#94002=ADVANCED_FACE('',(#9029),#2676,.F.);
#94003=ADVANCED_FACE('',(#9030),#90686,.F.);
#94004=ADVANCED_FACE('',(#9031),#90687,.F.);
#94005=ADVANCED_FACE('',(#9032),#2677,.F.);
#94006=ADVANCED_FACE('',(#9033),#90688,.F.);
#94007=ADVANCED_FACE('',(#9034),#5818,.F.);
#94008=ADVANCED_FACE('',(#9035),#2678,.F.);
#94009=ADVANCED_FACE('',(#9036),#2679,.F.);
#94010=ADVANCED_FACE('',(#9037),#90689,.F.);
#94011=ADVANCED_FACE('',(#9038),#90690,.F.);
#94012=ADVANCED_FACE('',(#9039),#2680,.F.);
#94013=ADVANCED_FACE('',(#9040),#2681,.F.);
#94014=ADVANCED_FACE('',(#9041),#5819,.F.);
#94015=ADVANCED_FACE('',(#9042),#90691,.F.);
#94016=ADVANCED_FACE('',(#9043),#2682,.F.);
#94017=ADVANCED_FACE('',(#9044),#90692,.F.);
#94018=ADVANCED_FACE('',(#9045),#90693,.F.);
#94019=ADVANCED_FACE('',(#9046),#2683,.F.);
#94020=ADVANCED_FACE('',(#9047),#2684,.F.);
#94021=ADVANCED_FACE('',(#9048),#90694,.F.);
#94022=ADVANCED_FACE('',(#9049),#90695,.F.);
#94023=ADVANCED_FACE('',(#9050),#2685,.F.);
#94024=ADVANCED_FACE('',(#9051),#90696,.F.);
#94025=ADVANCED_FACE('',(#9052),#90697,.F.);
#94026=ADVANCED_FACE('',(#9053),#2686,.F.);
#94027=ADVANCED_FACE('',(#9054),#90698,.F.);
#94028=ADVANCED_FACE('',(#9055),#90699,.F.);
#94029=ADVANCED_FACE('',(#9056),#2687,.F.);
#94030=ADVANCED_FACE('',(#9057),#2688,.F.);
#94031=ADVANCED_FACE('',(#9058),#90700,.F.);
#94032=ADVANCED_FACE('',(#9059),#90701,.F.);
#94033=ADVANCED_FACE('',(#9060),#2689,.F.);
#94034=ADVANCED_FACE('',(#9061),#90702,.F.);
#94035=ADVANCED_FACE('',(#9062),#5820,.F.);
#94036=ADVANCED_FACE('',(#9063),#2690,.F.);
#94037=ADVANCED_FACE('',(#9064),#2691,.F.);
#94038=ADVANCED_FACE('',(#9065),#90703,.F.);
#94039=ADVANCED_FACE('',(#9066),#90704,.F.);
#94040=ADVANCED_FACE('',(#9067),#2692,.F.);
#94041=ADVANCED_FACE('',(#9068),#2693,.F.);
#94042=ADVANCED_FACE('',(#9069),#5821,.F.);
#94043=ADVANCED_FACE('',(#9070),#90705,.F.);
#94044=ADVANCED_FACE('',(#9071),#2694,.F.);
#94045=ADVANCED_FACE('',(#9072),#90706,.F.);
#94046=ADVANCED_FACE('',(#9073),#90707,.F.);
#94047=ADVANCED_FACE('',(#9074),#2695,.F.);
#94048=ADVANCED_FACE('',(#9075),#2696,.F.);
#94049=ADVANCED_FACE('',(#9076),#90708,.F.);
#94050=ADVANCED_FACE('',(#9077),#90709,.F.);
#94051=ADVANCED_FACE('',(#9078),#2697,.F.);
#94052=ADVANCED_FACE('',(#9079),#90710,.F.);
#94053=ADVANCED_FACE('',(#9080),#90711,.F.);
#94054=ADVANCED_FACE('',(#9081),#2698,.F.);
#94055=ADVANCED_FACE('',(#9082),#90712,.F.);
#94056=ADVANCED_FACE('',(#9083),#90713,.F.);
#94057=ADVANCED_FACE('',(#9084),#2699,.F.);
#94058=ADVANCED_FACE('',(#9085),#2700,.F.);
#94059=ADVANCED_FACE('',(#9086),#90714,.F.);
#94060=ADVANCED_FACE('',(#9087),#90715,.F.);
#94061=ADVANCED_FACE('',(#9088),#2701,.F.);
#94062=ADVANCED_FACE('',(#9089),#90716,.F.);
#94063=ADVANCED_FACE('',(#9090),#5822,.F.);
#94064=ADVANCED_FACE('',(#9091),#2702,.F.);
#94065=ADVANCED_FACE('',(#9092),#2703,.F.);
#94066=ADVANCED_FACE('',(#9093),#90717,.F.);
#94067=ADVANCED_FACE('',(#9094),#90718,.F.);
#94068=ADVANCED_FACE('',(#9095),#2704,.F.);
#94069=ADVANCED_FACE('',(#9096),#2705,.F.);
#94070=ADVANCED_FACE('',(#9097),#5823,.F.);
#94071=ADVANCED_FACE('',(#9098),#90719,.F.);
#94072=ADVANCED_FACE('',(#9099),#2706,.F.);
#94073=ADVANCED_FACE('',(#9100),#90720,.F.);
#94074=ADVANCED_FACE('',(#9101),#90721,.F.);
#94075=ADVANCED_FACE('',(#9102),#2707,.F.);
#94076=ADVANCED_FACE('',(#9103),#2708,.F.);
#94077=ADVANCED_FACE('',(#9104),#90722,.F.);
#94078=ADVANCED_FACE('',(#9105),#90723,.F.);
#94079=ADVANCED_FACE('',(#9106),#2709,.F.);
#94080=ADVANCED_FACE('',(#9107),#90724,.F.);
#94081=ADVANCED_FACE('',(#9108),#90725,.F.);
#94082=ADVANCED_FACE('',(#9109),#2710,.F.);
#94083=ADVANCED_FACE('',(#9110),#90726,.F.);
#94084=ADVANCED_FACE('',(#9111),#90727,.F.);
#94085=ADVANCED_FACE('',(#9112),#2711,.F.);
#94086=ADVANCED_FACE('',(#9113),#2712,.F.);
#94087=ADVANCED_FACE('',(#9114),#90728,.F.);
#94088=ADVANCED_FACE('',(#9115),#90729,.F.);
#94089=ADVANCED_FACE('',(#9116),#2713,.F.);
#94090=ADVANCED_FACE('',(#9117),#90730,.F.);
#94091=ADVANCED_FACE('',(#9118),#5824,.F.);
#94092=ADVANCED_FACE('',(#9119),#2714,.F.);
#94093=ADVANCED_FACE('',(#9120),#2715,.F.);
#94094=ADVANCED_FACE('',(#9121),#90731,.F.);
#94095=ADVANCED_FACE('',(#9122),#90732,.F.);
#94096=ADVANCED_FACE('',(#9123),#2716,.F.);
#94097=ADVANCED_FACE('',(#9124),#2717,.F.);
#94098=ADVANCED_FACE('',(#9125),#5825,.F.);
#94099=ADVANCED_FACE('',(#9126),#90733,.F.);
#94100=ADVANCED_FACE('',(#9127),#2718,.F.);
#94101=ADVANCED_FACE('',(#9128),#90734,.F.);
#94102=ADVANCED_FACE('',(#9129),#90735,.F.);
#94103=ADVANCED_FACE('',(#9130),#2719,.F.);
#94104=ADVANCED_FACE('',(#9131),#2720,.F.);
#94105=ADVANCED_FACE('',(#9132),#90736,.F.);
#94106=ADVANCED_FACE('',(#9133),#90737,.F.);
#94107=ADVANCED_FACE('',(#9134),#2721,.F.);
#94108=ADVANCED_FACE('',(#9135),#90738,.F.);
#94109=ADVANCED_FACE('',(#9136),#90739,.F.);
#94110=ADVANCED_FACE('',(#9137),#2722,.F.);
#94111=ADVANCED_FACE('',(#9138),#90740,.F.);
#94112=ADVANCED_FACE('',(#9139),#90741,.F.);
#94113=ADVANCED_FACE('',(#9140),#2723,.F.);
#94114=ADVANCED_FACE('',(#9141),#2724,.F.);
#94115=ADVANCED_FACE('',(#9142),#90742,.F.);
#94116=ADVANCED_FACE('',(#9143),#90743,.F.);
#94117=ADVANCED_FACE('',(#9144),#2725,.F.);
#94118=ADVANCED_FACE('',(#9145),#90744,.F.);
#94119=ADVANCED_FACE('',(#9146),#5826,.F.);
#94120=ADVANCED_FACE('',(#9147),#2726,.F.);
#94121=ADVANCED_FACE('',(#9148),#2727,.F.);
#94122=ADVANCED_FACE('',(#9149),#90745,.F.);
#94123=ADVANCED_FACE('',(#9150),#90746,.F.);
#94124=ADVANCED_FACE('',(#9151),#2728,.F.);
#94125=ADVANCED_FACE('',(#9152),#2729,.F.);
#94126=ADVANCED_FACE('',(#9153),#5827,.F.);
#94127=ADVANCED_FACE('',(#9154),#90747,.F.);
#94128=ADVANCED_FACE('',(#9155),#2730,.F.);
#94129=ADVANCED_FACE('',(#9156),#90748,.F.);
#94130=ADVANCED_FACE('',(#9157),#90749,.F.);
#94131=ADVANCED_FACE('',(#9158),#2731,.F.);
#94132=ADVANCED_FACE('',(#9159),#2732,.F.);
#94133=ADVANCED_FACE('',(#9160),#90750,.F.);
#94134=ADVANCED_FACE('',(#9161),#90751,.F.);
#94135=ADVANCED_FACE('',(#9162),#2733,.F.);
#94136=ADVANCED_FACE('',(#9163),#90752,.F.);
#94137=ADVANCED_FACE('',(#9164),#90753,.F.);
#94138=ADVANCED_FACE('',(#9165),#2734,.F.);
#94139=ADVANCED_FACE('',(#9166),#90754,.F.);
#94140=ADVANCED_FACE('',(#9167),#90755,.F.);
#94141=ADVANCED_FACE('',(#9168),#2735,.F.);
#94142=ADVANCED_FACE('',(#9169),#2736,.F.);
#94143=ADVANCED_FACE('',(#9170),#90756,.F.);
#94144=ADVANCED_FACE('',(#9171),#90757,.F.);
#94145=ADVANCED_FACE('',(#9172),#2737,.F.);
#94146=ADVANCED_FACE('',(#9173),#90758,.F.);
#94147=ADVANCED_FACE('',(#9174),#5828,.F.);
#94148=ADVANCED_FACE('',(#9175),#2738,.F.);
#94149=ADVANCED_FACE('',(#9176),#2739,.F.);
#94150=ADVANCED_FACE('',(#9177),#90759,.F.);
#94151=ADVANCED_FACE('',(#9178),#90760,.F.);
#94152=ADVANCED_FACE('',(#9179),#2740,.F.);
#94153=ADVANCED_FACE('',(#9180),#2741,.F.);
#94154=ADVANCED_FACE('',(#9181),#5829,.F.);
#94155=ADVANCED_FACE('',(#9182),#90761,.F.);
#94156=ADVANCED_FACE('',(#9183),#2742,.F.);
#94157=ADVANCED_FACE('',(#9184),#90762,.F.);
#94158=ADVANCED_FACE('',(#9185),#90763,.F.);
#94159=ADVANCED_FACE('',(#9186),#2743,.F.);
#94160=ADVANCED_FACE('',(#9187),#2744,.F.);
#94161=ADVANCED_FACE('',(#9188),#90764,.F.);
#94162=ADVANCED_FACE('',(#9189),#90765,.F.);
#94163=ADVANCED_FACE('',(#9190),#2745,.F.);
#94164=ADVANCED_FACE('',(#9191),#90766,.F.);
#94165=ADVANCED_FACE('',(#9192),#90767,.F.);
#94166=ADVANCED_FACE('',(#9193),#2746,.F.);
#94167=ADVANCED_FACE('',(#9194),#90768,.F.);
#94168=ADVANCED_FACE('',(#9195),#90769,.F.);
#94169=ADVANCED_FACE('',(#9196),#2747,.F.);
#94170=ADVANCED_FACE('',(#9197),#2748,.F.);
#94171=ADVANCED_FACE('',(#9198),#90770,.F.);
#94172=ADVANCED_FACE('',(#9199),#90771,.F.);
#94173=ADVANCED_FACE('',(#9200),#2749,.F.);
#94174=ADVANCED_FACE('',(#9201),#90772,.F.);
#94175=ADVANCED_FACE('',(#9202),#5830,.F.);
#94176=ADVANCED_FACE('',(#9203),#2750,.F.);
#94177=ADVANCED_FACE('',(#9204),#2751,.F.);
#94178=ADVANCED_FACE('',(#9205),#90773,.F.);
#94179=ADVANCED_FACE('',(#9206),#90774,.F.);
#94180=ADVANCED_FACE('',(#9207),#2752,.F.);
#94181=ADVANCED_FACE('',(#9208),#2753,.F.);
#94182=ADVANCED_FACE('',(#9209),#5831,.F.);
#94183=ADVANCED_FACE('',(#9210),#90775,.F.);
#94184=ADVANCED_FACE('',(#9211),#2754,.F.);
#94185=ADVANCED_FACE('',(#9212),#90776,.F.);
#94186=ADVANCED_FACE('',(#9213),#90777,.F.);
#94187=ADVANCED_FACE('',(#9214),#2755,.F.);
#94188=ADVANCED_FACE('',(#9215),#2756,.F.);
#94189=ADVANCED_FACE('',(#9216),#90778,.F.);
#94190=ADVANCED_FACE('',(#9217),#90779,.F.);
#94191=ADVANCED_FACE('',(#9218),#2757,.F.);
#94192=ADVANCED_FACE('',(#9219),#90780,.F.);
#94193=ADVANCED_FACE('',(#9220),#90781,.F.);
#94194=ADVANCED_FACE('',(#9221),#2758,.F.);
#94195=ADVANCED_FACE('',(#9222),#90782,.F.);
#94196=ADVANCED_FACE('',(#9223),#90783,.F.);
#94197=ADVANCED_FACE('',(#9224),#2759,.F.);
#94198=ADVANCED_FACE('',(#9225),#2760,.F.);
#94199=ADVANCED_FACE('',(#9226),#90784,.F.);
#94200=ADVANCED_FACE('',(#9227),#90785,.F.);
#94201=ADVANCED_FACE('',(#9228),#2761,.F.);
#94202=ADVANCED_FACE('',(#9229),#90786,.F.);
#94203=ADVANCED_FACE('',(#9230),#5832,.F.);
#94204=ADVANCED_FACE('',(#9231),#2762,.F.);
#94205=ADVANCED_FACE('',(#9232),#2763,.F.);
#94206=ADVANCED_FACE('',(#9233),#90787,.F.);
#94207=ADVANCED_FACE('',(#9234),#90788,.F.);
#94208=ADVANCED_FACE('',(#9235),#2764,.F.);
#94209=ADVANCED_FACE('',(#9236),#2765,.F.);
#94210=ADVANCED_FACE('',(#9237),#5833,.F.);
#94211=ADVANCED_FACE('',(#9238),#90789,.F.);
#94212=ADVANCED_FACE('',(#9239),#2766,.F.);
#94213=ADVANCED_FACE('',(#9240),#90790,.F.);
#94214=ADVANCED_FACE('',(#9241),#90791,.F.);
#94215=ADVANCED_FACE('',(#9242),#2767,.F.);
#94216=ADVANCED_FACE('',(#9243),#2768,.F.);
#94217=ADVANCED_FACE('',(#9244),#90792,.F.);
#94218=ADVANCED_FACE('',(#9245),#90793,.F.);
#94219=ADVANCED_FACE('',(#9246),#2769,.F.);
#94220=ADVANCED_FACE('',(#9247),#90794,.F.);
#94221=ADVANCED_FACE('',(#9248),#90795,.F.);
#94222=ADVANCED_FACE('',(#9249),#2770,.F.);
#94223=ADVANCED_FACE('',(#9250),#90796,.F.);
#94224=ADVANCED_FACE('',(#9251),#90797,.F.);
#94225=ADVANCED_FACE('',(#9252),#2771,.F.);
#94226=ADVANCED_FACE('',(#9253),#2772,.F.);
#94227=ADVANCED_FACE('',(#9254),#90798,.F.);
#94228=ADVANCED_FACE('',(#9255),#90799,.F.);
#94229=ADVANCED_FACE('',(#9256),#2773,.F.);
#94230=ADVANCED_FACE('',(#9257),#90800,.F.);
#94231=ADVANCED_FACE('',(#9258),#5834,.F.);
#94232=ADVANCED_FACE('',(#9259),#2774,.F.);
#94233=ADVANCED_FACE('',(#9260),#2775,.F.);
#94234=ADVANCED_FACE('',(#9261),#90801,.F.);
#94235=ADVANCED_FACE('',(#9262),#90802,.F.);
#94236=ADVANCED_FACE('',(#9263),#2776,.F.);
#94237=ADVANCED_FACE('',(#9264),#2777,.F.);
#94238=ADVANCED_FACE('',(#9265),#5835,.F.);
#94239=ADVANCED_FACE('',(#9266),#90803,.F.);
#94240=ADVANCED_FACE('',(#9267),#2778,.F.);
#94241=ADVANCED_FACE('',(#9268),#90804,.F.);
#94242=ADVANCED_FACE('',(#9269),#90805,.F.);
#94243=ADVANCED_FACE('',(#9270),#2779,.F.);
#94244=ADVANCED_FACE('',(#9271),#2780,.F.);
#94245=ADVANCED_FACE('',(#9272),#90806,.F.);
#94246=ADVANCED_FACE('',(#9273),#90807,.F.);
#94247=ADVANCED_FACE('',(#9274),#2781,.F.);
#94248=ADVANCED_FACE('',(#9275),#90808,.F.);
#94249=ADVANCED_FACE('',(#9276),#90809,.F.);
#94250=ADVANCED_FACE('',(#9277),#2782,.F.);
#94251=ADVANCED_FACE('',(#9278),#90810,.F.);
#94252=ADVANCED_FACE('',(#9279),#90811,.F.);
#94253=ADVANCED_FACE('',(#9280),#2783,.F.);
#94254=ADVANCED_FACE('',(#9281),#2784,.F.);
#94255=ADVANCED_FACE('',(#9282),#90812,.F.);
#94256=ADVANCED_FACE('',(#9283),#90813,.F.);
#94257=ADVANCED_FACE('',(#9284),#2785,.F.);
#94258=ADVANCED_FACE('',(#9285),#90814,.F.);
#94259=ADVANCED_FACE('',(#9286),#5836,.F.);
#94260=ADVANCED_FACE('',(#9287),#2786,.F.);
#94261=ADVANCED_FACE('',(#9288),#2787,.F.);
#94262=ADVANCED_FACE('',(#9289),#90815,.F.);
#94263=ADVANCED_FACE('',(#9290),#90816,.F.);
#94264=ADVANCED_FACE('',(#9291),#2788,.F.);
#94265=ADVANCED_FACE('',(#9292),#2789,.F.);
#94266=ADVANCED_FACE('',(#9293),#5837,.F.);
#94267=ADVANCED_FACE('',(#9294),#90817,.F.);
#94268=ADVANCED_FACE('',(#9295),#2790,.F.);
#94269=ADVANCED_FACE('',(#9296),#90818,.F.);
#94270=ADVANCED_FACE('',(#9297),#90819,.F.);
#94271=ADVANCED_FACE('',(#9298),#2791,.F.);
#94272=ADVANCED_FACE('',(#9299),#2792,.F.);
#94273=ADVANCED_FACE('',(#9300),#90820,.F.);
#94274=ADVANCED_FACE('',(#9301),#90821,.F.);
#94275=ADVANCED_FACE('',(#9302),#2793,.F.);
#94276=ADVANCED_FACE('',(#9303),#90822,.F.);
#94277=ADVANCED_FACE('',(#9304),#90823,.F.);
#94278=ADVANCED_FACE('',(#9305),#2794,.F.);
#94279=ADVANCED_FACE('',(#9306),#90824,.F.);
#94280=ADVANCED_FACE('',(#9307),#90825,.F.);
#94281=ADVANCED_FACE('',(#9308),#2795,.F.);
#94282=ADVANCED_FACE('',(#9309),#2796,.F.);
#94283=ADVANCED_FACE('',(#9310),#90826,.F.);
#94284=ADVANCED_FACE('',(#9311),#90827,.F.);
#94285=ADVANCED_FACE('',(#9312),#2797,.F.);
#94286=ADVANCED_FACE('',(#9313),#90828,.F.);
#94287=ADVANCED_FACE('',(#9314),#5838,.F.);
#94288=ADVANCED_FACE('',(#9315),#2798,.F.);
#94289=ADVANCED_FACE('',(#9316),#2799,.F.);
#94290=ADVANCED_FACE('',(#9317),#90829,.F.);
#94291=ADVANCED_FACE('',(#9318),#90830,.F.);
#94292=ADVANCED_FACE('',(#9319),#2800,.F.);
#94293=ADVANCED_FACE('',(#9320),#2801,.F.);
#94294=ADVANCED_FACE('',(#9321),#5839,.F.);
#94295=ADVANCED_FACE('',(#9322),#90831,.F.);
#94296=ADVANCED_FACE('',(#9323),#2802,.F.);
#94297=ADVANCED_FACE('',(#9324),#90832,.F.);
#94298=ADVANCED_FACE('',(#9325),#90833,.F.);
#94299=ADVANCED_FACE('',(#9326),#2803,.F.);
#94300=ADVANCED_FACE('',(#9327),#2804,.F.);
#94301=ADVANCED_FACE('',(#9328),#90834,.F.);
#94302=ADVANCED_FACE('',(#9329),#90835,.F.);
#94303=ADVANCED_FACE('',(#9330),#2805,.F.);
#94304=ADVANCED_FACE('',(#9331),#90836,.F.);
#94305=ADVANCED_FACE('',(#9332),#90837,.F.);
#94306=ADVANCED_FACE('',(#9333),#2806,.F.);
#94307=ADVANCED_FACE('',(#9334),#90838,.F.);
#94308=ADVANCED_FACE('',(#9335),#90839,.F.);
#94309=ADVANCED_FACE('',(#9336),#2807,.F.);
#94310=ADVANCED_FACE('',(#9337),#2808,.F.);
#94311=ADVANCED_FACE('',(#9338),#90840,.F.);
#94312=ADVANCED_FACE('',(#9339),#90841,.F.);
#94313=ADVANCED_FACE('',(#9340),#2809,.F.);
#94314=ADVANCED_FACE('',(#9341),#90842,.F.);
#94315=ADVANCED_FACE('',(#9342),#5840,.F.);
#94316=ADVANCED_FACE('',(#9343),#2810,.F.);
#94317=ADVANCED_FACE('',(#9344),#2811,.F.);
#94318=ADVANCED_FACE('',(#9345),#90843,.F.);
#94319=ADVANCED_FACE('',(#9346),#90844,.F.);
#94320=ADVANCED_FACE('',(#9347),#2812,.F.);
#94321=ADVANCED_FACE('',(#9348),#2813,.F.);
#94322=ADVANCED_FACE('',(#9349),#5841,.F.);
#94323=ADVANCED_FACE('',(#9350),#90845,.F.);
#94324=ADVANCED_FACE('',(#9351),#2814,.F.);
#94325=ADVANCED_FACE('',(#9352),#90846,.F.);
#94326=ADVANCED_FACE('',(#9353),#90847,.F.);
#94327=ADVANCED_FACE('',(#9354),#2815,.F.);
#94328=ADVANCED_FACE('',(#9355),#2816,.F.);
#94329=ADVANCED_FACE('',(#9356),#90848,.F.);
#94330=ADVANCED_FACE('',(#9357),#90849,.F.);
#94331=ADVANCED_FACE('',(#9358),#2817,.F.);
#94332=ADVANCED_FACE('',(#9359),#90850,.F.);
#94333=ADVANCED_FACE('',(#9360),#90851,.F.);
#94334=ADVANCED_FACE('',(#9361),#2818,.F.);
#94335=ADVANCED_FACE('',(#9362),#90852,.F.);
#94336=ADVANCED_FACE('',(#9363),#90853,.F.);
#94337=ADVANCED_FACE('',(#9364),#2819,.F.);
#94338=ADVANCED_FACE('',(#9365),#2820,.F.);
#94339=ADVANCED_FACE('',(#9366),#90854,.F.);
#94340=ADVANCED_FACE('',(#9367),#90855,.F.);
#94341=ADVANCED_FACE('',(#9368),#2821,.F.);
#94342=ADVANCED_FACE('',(#9369),#90856,.F.);
#94343=ADVANCED_FACE('',(#9370),#5842,.F.);
#94344=ADVANCED_FACE('',(#9371),#2822,.F.);
#94345=ADVANCED_FACE('',(#9372),#2823,.F.);
#94346=ADVANCED_FACE('',(#9373),#90857,.F.);
#94347=ADVANCED_FACE('',(#9374),#90858,.F.);
#94348=ADVANCED_FACE('',(#9375),#2824,.F.);
#94349=ADVANCED_FACE('',(#9376),#2825,.F.);
#94350=ADVANCED_FACE('',(#9377),#5843,.F.);
#94351=ADVANCED_FACE('',(#9378),#90859,.F.);
#94352=ADVANCED_FACE('',(#9379),#2826,.F.);
#94353=ADVANCED_FACE('',(#9380),#90860,.F.);
#94354=ADVANCED_FACE('',(#9381),#90861,.F.);
#94355=ADVANCED_FACE('',(#9382),#2827,.F.);
#94356=ADVANCED_FACE('',(#9383),#2828,.F.);
#94357=ADVANCED_FACE('',(#9384),#90862,.F.);
#94358=ADVANCED_FACE('',(#9385),#90863,.F.);
#94359=ADVANCED_FACE('',(#9386),#2829,.F.);
#94360=ADVANCED_FACE('',(#9387),#90864,.F.);
#94361=ADVANCED_FACE('',(#9388),#90865,.F.);
#94362=ADVANCED_FACE('',(#9389),#2830,.F.);
#94363=ADVANCED_FACE('',(#9390),#90866,.F.);
#94364=ADVANCED_FACE('',(#9391),#90867,.F.);
#94365=ADVANCED_FACE('',(#9392),#2831,.F.);
#94366=ADVANCED_FACE('',(#9393),#2832,.F.);
#94367=ADVANCED_FACE('',(#9394),#90868,.F.);
#94368=ADVANCED_FACE('',(#9395),#90869,.F.);
#94369=ADVANCED_FACE('',(#9396),#2833,.F.);
#94370=ADVANCED_FACE('',(#9397),#90870,.F.);
#94371=ADVANCED_FACE('',(#9398),#5844,.F.);
#94372=ADVANCED_FACE('',(#9399),#2834,.F.);
#94373=ADVANCED_FACE('',(#9400),#2835,.F.);
#94374=ADVANCED_FACE('',(#9401),#90871,.F.);
#94375=ADVANCED_FACE('',(#9402),#90872,.F.);
#94376=ADVANCED_FACE('',(#9403),#2836,.F.);
#94377=ADVANCED_FACE('',(#9404),#2837,.F.);
#94378=ADVANCED_FACE('',(#9405),#5845,.F.);
#94379=ADVANCED_FACE('',(#9406),#90873,.F.);
#94380=ADVANCED_FACE('',(#9407),#2838,.F.);
#94381=ADVANCED_FACE('',(#9408),#90874,.F.);
#94382=ADVANCED_FACE('',(#9409),#90875,.F.);
#94383=ADVANCED_FACE('',(#9410),#2839,.F.);
#94384=ADVANCED_FACE('',(#9411),#2840,.F.);
#94385=ADVANCED_FACE('',(#9412),#90876,.F.);
#94386=ADVANCED_FACE('',(#9413),#90877,.F.);
#94387=ADVANCED_FACE('',(#9414),#2841,.F.);
#94388=ADVANCED_FACE('',(#9415),#90878,.F.);
#94389=ADVANCED_FACE('',(#9416),#90879,.F.);
#94390=ADVANCED_FACE('',(#9417),#2842,.F.);
#94391=ADVANCED_FACE('',(#9418),#90880,.F.);
#94392=ADVANCED_FACE('',(#9419),#90881,.F.);
#94393=ADVANCED_FACE('',(#9420),#2843,.F.);
#94394=ADVANCED_FACE('',(#9421),#2844,.F.);
#94395=ADVANCED_FACE('',(#9422),#90882,.F.);
#94396=ADVANCED_FACE('',(#9423),#90883,.F.);
#94397=ADVANCED_FACE('',(#9424),#2845,.F.);
#94398=ADVANCED_FACE('',(#9425),#90884,.F.);
#94399=ADVANCED_FACE('',(#9426),#5846,.F.);
#94400=ADVANCED_FACE('',(#9427),#2846,.F.);
#94401=ADVANCED_FACE('',(#9428),#2847,.F.);
#94402=ADVANCED_FACE('',(#9429),#90885,.F.);
#94403=ADVANCED_FACE('',(#9430),#90886,.F.);
#94404=ADVANCED_FACE('',(#9431),#2848,.F.);
#94405=ADVANCED_FACE('',(#9432),#2849,.F.);
#94406=ADVANCED_FACE('',(#9433),#5847,.F.);
#94407=ADVANCED_FACE('',(#9434),#90887,.F.);
#94408=ADVANCED_FACE('',(#9435),#2850,.F.);
#94409=ADVANCED_FACE('',(#9436),#90888,.F.);
#94410=ADVANCED_FACE('',(#9437),#90889,.F.);
#94411=ADVANCED_FACE('',(#9438),#2851,.F.);
#94412=ADVANCED_FACE('',(#9439),#2852,.F.);
#94413=ADVANCED_FACE('',(#9440),#90890,.F.);
#94414=ADVANCED_FACE('',(#9441),#90891,.F.);
#94415=ADVANCED_FACE('',(#9442),#2853,.F.);
#94416=ADVANCED_FACE('',(#9443),#90892,.F.);
#94417=ADVANCED_FACE('',(#9444),#90893,.F.);
#94418=ADVANCED_FACE('',(#9445),#2854,.F.);
#94419=ADVANCED_FACE('',(#9446),#90894,.F.);
#94420=ADVANCED_FACE('',(#9447),#90895,.F.);
#94421=ADVANCED_FACE('',(#9448),#2855,.F.);
#94422=ADVANCED_FACE('',(#9449),#2856,.F.);
#94423=ADVANCED_FACE('',(#9450),#90896,.F.);
#94424=ADVANCED_FACE('',(#9451),#90897,.F.);
#94425=ADVANCED_FACE('',(#9452),#2857,.F.);
#94426=ADVANCED_FACE('',(#9453),#90898,.F.);
#94427=ADVANCED_FACE('',(#9454),#5848,.F.);
#94428=ADVANCED_FACE('',(#9455),#2858,.F.);
#94429=ADVANCED_FACE('',(#9456),#2859,.F.);
#94430=ADVANCED_FACE('',(#9457),#90899,.F.);
#94431=ADVANCED_FACE('',(#9458),#90900,.F.);
#94432=ADVANCED_FACE('',(#9459),#2860,.F.);
#94433=ADVANCED_FACE('',(#9460),#2861,.F.);
#94434=ADVANCED_FACE('',(#9461),#5849,.F.);
#94435=ADVANCED_FACE('',(#9462),#90901,.F.);
#94436=ADVANCED_FACE('',(#9463),#2862,.F.);
#94437=ADVANCED_FACE('',(#9464),#90902,.F.);
#94438=ADVANCED_FACE('',(#9465),#90903,.F.);
#94439=ADVANCED_FACE('',(#9466),#2863,.F.);
#94440=ADVANCED_FACE('',(#9467),#2864,.F.);
#94441=ADVANCED_FACE('',(#9468),#90904,.F.);
#94442=ADVANCED_FACE('',(#9469),#90905,.F.);
#94443=ADVANCED_FACE('',(#9470),#2865,.F.);
#94444=ADVANCED_FACE('',(#9471),#90906,.F.);
#94445=ADVANCED_FACE('',(#9472),#90907,.F.);
#94446=ADVANCED_FACE('',(#9473),#2866,.F.);
#94447=ADVANCED_FACE('',(#9474),#90908,.F.);
#94448=ADVANCED_FACE('',(#9475),#90909,.F.);
#94449=ADVANCED_FACE('',(#9476),#2867,.F.);
#94450=ADVANCED_FACE('',(#9477),#2868,.F.);
#94451=ADVANCED_FACE('',(#9478),#90910,.F.);
#94452=ADVANCED_FACE('',(#9479),#90911,.F.);
#94453=ADVANCED_FACE('',(#9480),#2869,.F.);
#94454=ADVANCED_FACE('',(#9481),#90912,.F.);
#94455=ADVANCED_FACE('',(#9482),#2870,.F.);
#94456=ADVANCED_FACE('',(#9483),#2871,.F.);
#94457=ADVANCED_FACE('',(#9484),#90913,.F.);
#94458=ADVANCED_FACE('',(#9485),#90914,.F.);
#94459=ADVANCED_FACE('',(#9486),#2872,.F.);
#94460=ADVANCED_FACE('',(#9487),#2873,.F.);
#94461=ADVANCED_FACE('',(#9488),#90915,.F.);
#94462=ADVANCED_FACE('',(#9489),#2874,.F.);
#94463=ADVANCED_FACE('',(#9490),#90916,.F.);
#94464=ADVANCED_FACE('',(#9491),#90917,.F.);
#94465=ADVANCED_FACE('',(#9492),#2875,.F.);
#94466=ADVANCED_FACE('',(#9493),#2876,.F.);
#94467=ADVANCED_FACE('',(#9494),#90918,.F.);
#94468=ADVANCED_FACE('',(#9495),#90919,.F.);
#94469=ADVANCED_FACE('',(#9496),#2877,.F.);
#94470=ADVANCED_FACE('',(#9497),#90920,.F.);
#94471=ADVANCED_FACE('',(#9498),#90921,.F.);
#94472=ADVANCED_FACE('',(#9499),#2878,.F.);
#94473=ADVANCED_FACE('',(#9500),#90922,.F.);
#94474=ADVANCED_FACE('',(#9501),#90923,.F.);
#94475=ADVANCED_FACE('',(#9502),#2879,.F.);
#94476=ADVANCED_FACE('',(#9503),#2880,.F.);
#94477=ADVANCED_FACE('',(#9504),#90924,.F.);
#94478=ADVANCED_FACE('',(#9505),#90925,.F.);
#94479=ADVANCED_FACE('',(#9506),#2881,.F.);
#94480=ADVANCED_FACE('',(#9507),#90926,.F.);
#94481=ADVANCED_FACE('',(#9508),#5850,.F.);
#94482=ADVANCED_FACE('',(#9509),#2882,.F.);
#94483=ADVANCED_FACE('',(#9510),#2883,.F.);
#94484=ADVANCED_FACE('',(#9511),#90927,.F.);
#94485=ADVANCED_FACE('',(#9512),#90928,.F.);
#94486=ADVANCED_FACE('',(#9513),#2884,.F.);
#94487=ADVANCED_FACE('',(#9514),#2885,.F.);
#94488=ADVANCED_FACE('',(#9515),#5851,.F.);
#94489=ADVANCED_FACE('',(#9516),#90929,.F.);
#94490=ADVANCED_FACE('',(#9517),#2886,.F.);
#94491=ADVANCED_FACE('',(#9518),#90930,.F.);
#94492=ADVANCED_FACE('',(#9519),#90931,.F.);
#94493=ADVANCED_FACE('',(#9520),#2887,.F.);
#94494=ADVANCED_FACE('',(#9521),#2888,.F.);
#94495=ADVANCED_FACE('',(#9522),#90932,.F.);
#94496=ADVANCED_FACE('',(#9523),#90933,.F.);
#94497=ADVANCED_FACE('',(#9524),#2889,.F.);
#94498=ADVANCED_FACE('',(#9525),#90934,.F.);
#94499=ADVANCED_FACE('',(#9526),#90935,.F.);
#94500=ADVANCED_FACE('',(#9527),#2890,.F.);
#94501=ADVANCED_FACE('',(#9528),#90936,.F.);
#94502=ADVANCED_FACE('',(#9529),#90937,.F.);
#94503=ADVANCED_FACE('',(#9530),#2891,.F.);
#94504=ADVANCED_FACE('',(#9531),#2892,.F.);
#94505=ADVANCED_FACE('',(#9532),#90938,.F.);
#94506=ADVANCED_FACE('',(#9533),#90939,.F.);
#94507=ADVANCED_FACE('',(#9534),#2893,.F.);
#94508=ADVANCED_FACE('',(#9535),#90940,.F.);
#94509=ADVANCED_FACE('',(#9536),#5852,.F.);
#94510=ADVANCED_FACE('',(#9537),#2894,.F.);
#94511=ADVANCED_FACE('',(#9538),#2895,.F.);
#94512=ADVANCED_FACE('',(#9539),#90941,.F.);
#94513=ADVANCED_FACE('',(#9540),#90942,.F.);
#94514=ADVANCED_FACE('',(#9541),#2896,.F.);
#94515=ADVANCED_FACE('',(#9542),#2897,.F.);
#94516=ADVANCED_FACE('',(#9543),#5853,.F.);
#94517=ADVANCED_FACE('',(#9544),#90943,.F.);
#94518=ADVANCED_FACE('',(#9545),#2898,.F.);
#94519=ADVANCED_FACE('',(#9546),#90944,.F.);
#94520=ADVANCED_FACE('',(#9547),#90945,.F.);
#94521=ADVANCED_FACE('',(#9548),#2899,.F.);
#94522=ADVANCED_FACE('',(#9549),#2900,.F.);
#94523=ADVANCED_FACE('',(#9550),#90946,.F.);
#94524=ADVANCED_FACE('',(#9551),#90947,.F.);
#94525=ADVANCED_FACE('',(#9552),#2901,.F.);
#94526=ADVANCED_FACE('',(#9553),#90948,.F.);
#94527=ADVANCED_FACE('',(#9554),#90949,.F.);
#94528=ADVANCED_FACE('',(#9555),#2902,.F.);
#94529=ADVANCED_FACE('',(#9556),#90950,.F.);
#94530=ADVANCED_FACE('',(#9557),#90951,.F.);
#94531=ADVANCED_FACE('',(#9558),#2903,.F.);
#94532=ADVANCED_FACE('',(#9559),#2904,.F.);
#94533=ADVANCED_FACE('',(#9560),#90952,.F.);
#94534=ADVANCED_FACE('',(#9561),#90953,.F.);
#94535=ADVANCED_FACE('',(#9562),#2905,.F.);
#94536=ADVANCED_FACE('',(#9563),#90954,.F.);
#94537=ADVANCED_FACE('',(#9564),#5854,.F.);
#94538=ADVANCED_FACE('',(#9565),#2906,.F.);
#94539=ADVANCED_FACE('',(#9566),#2907,.F.);
#94540=ADVANCED_FACE('',(#9567),#90955,.F.);
#94541=ADVANCED_FACE('',(#9568),#90956,.F.);
#94542=ADVANCED_FACE('',(#9569),#2908,.F.);
#94543=ADVANCED_FACE('',(#9570),#2909,.F.);
#94544=ADVANCED_FACE('',(#9571),#5855,.F.);
#94545=ADVANCED_FACE('',(#9572),#90957,.F.);
#94546=ADVANCED_FACE('',(#9573),#2910,.F.);
#94547=ADVANCED_FACE('',(#9574),#90958,.F.);
#94548=ADVANCED_FACE('',(#9575),#90959,.F.);
#94549=ADVANCED_FACE('',(#9576),#2911,.F.);
#94550=ADVANCED_FACE('',(#9577),#2912,.F.);
#94551=ADVANCED_FACE('',(#9578),#90960,.F.);
#94552=ADVANCED_FACE('',(#9579),#90961,.F.);
#94553=ADVANCED_FACE('',(#9580),#2913,.F.);
#94554=ADVANCED_FACE('',(#9581),#90962,.F.);
#94555=ADVANCED_FACE('',(#9582),#90963,.F.);
#94556=ADVANCED_FACE('',(#9583),#2914,.F.);
#94557=ADVANCED_FACE('',(#9584),#90964,.F.);
#94558=ADVANCED_FACE('',(#9585),#90965,.F.);
#94559=ADVANCED_FACE('',(#9586),#2915,.F.);
#94560=ADVANCED_FACE('',(#9587),#2916,.F.);
#94561=ADVANCED_FACE('',(#9588),#90966,.F.);
#94562=ADVANCED_FACE('',(#9589),#90967,.F.);
#94563=ADVANCED_FACE('',(#9590),#2917,.F.);
#94564=ADVANCED_FACE('',(#9591),#90968,.F.);
#94565=ADVANCED_FACE('',(#9592),#5856,.F.);
#94566=ADVANCED_FACE('',(#9593),#2918,.F.);
#94567=ADVANCED_FACE('',(#9594),#2919,.F.);
#94568=ADVANCED_FACE('',(#9595),#90969,.F.);
#94569=ADVANCED_FACE('',(#9596),#90970,.F.);
#94570=ADVANCED_FACE('',(#9597),#2920,.F.);
#94571=ADVANCED_FACE('',(#9598),#2921,.F.);
#94572=ADVANCED_FACE('',(#9599),#5857,.F.);
#94573=ADVANCED_FACE('',(#9600),#90971,.F.);
#94574=ADVANCED_FACE('',(#9601),#2922,.F.);
#94575=ADVANCED_FACE('',(#9602),#90972,.F.);
#94576=ADVANCED_FACE('',(#9603),#90973,.F.);
#94577=ADVANCED_FACE('',(#9604),#2923,.F.);
#94578=ADVANCED_FACE('',(#9605),#2924,.F.);
#94579=ADVANCED_FACE('',(#9606),#90974,.F.);
#94580=ADVANCED_FACE('',(#9607),#90975,.F.);
#94581=ADVANCED_FACE('',(#9608),#2925,.F.);
#94582=ADVANCED_FACE('',(#9609),#90976,.F.);
#94583=ADVANCED_FACE('',(#9610),#90977,.F.);
#94584=ADVANCED_FACE('',(#9611),#2926,.F.);
#94585=ADVANCED_FACE('',(#9612),#90978,.F.);
#94586=ADVANCED_FACE('',(#9613),#90979,.F.);
#94587=ADVANCED_FACE('',(#9614),#2927,.F.);
#94588=ADVANCED_FACE('',(#9615),#2928,.F.);
#94589=ADVANCED_FACE('',(#9616),#90980,.F.);
#94590=ADVANCED_FACE('',(#9617),#90981,.F.);
#94591=ADVANCED_FACE('',(#9618),#2929,.F.);
#94592=ADVANCED_FACE('',(#9619),#90982,.F.);
#94593=ADVANCED_FACE('',(#9620),#5858,.F.);
#94594=ADVANCED_FACE('',(#9621),#2930,.F.);
#94595=ADVANCED_FACE('',(#9622),#2931,.F.);
#94596=ADVANCED_FACE('',(#9623),#90983,.F.);
#94597=ADVANCED_FACE('',(#9624),#90984,.F.);
#94598=ADVANCED_FACE('',(#9625),#2932,.F.);
#94599=ADVANCED_FACE('',(#9626),#2933,.F.);
#94600=ADVANCED_FACE('',(#9627),#5859,.F.);
#94601=ADVANCED_FACE('',(#9628),#90985,.F.);
#94602=ADVANCED_FACE('',(#9629),#2934,.F.);
#94603=ADVANCED_FACE('',(#9630),#90986,.F.);
#94604=ADVANCED_FACE('',(#9631),#90987,.F.);
#94605=ADVANCED_FACE('',(#9632),#2935,.F.);
#94606=ADVANCED_FACE('',(#9633),#2936,.F.);
#94607=ADVANCED_FACE('',(#9634),#90988,.F.);
#94608=ADVANCED_FACE('',(#9635),#90989,.F.);
#94609=ADVANCED_FACE('',(#9636),#2937,.F.);
#94610=ADVANCED_FACE('',(#9637),#90990,.F.);
#94611=ADVANCED_FACE('',(#9638),#90991,.F.);
#94612=ADVANCED_FACE('',(#9639),#2938,.F.);
#94613=ADVANCED_FACE('',(#9640),#90992,.F.);
#94614=ADVANCED_FACE('',(#9641),#90993,.F.);
#94615=ADVANCED_FACE('',(#9642),#2939,.F.);
#94616=ADVANCED_FACE('',(#9643),#2940,.F.);
#94617=ADVANCED_FACE('',(#9644),#90994,.F.);
#94618=ADVANCED_FACE('',(#9645),#90995,.F.);
#94619=ADVANCED_FACE('',(#9646),#2941,.F.);
#94620=ADVANCED_FACE('',(#9647),#90996,.F.);
#94621=ADVANCED_FACE('',(#9648),#5860,.F.);
#94622=ADVANCED_FACE('',(#9649),#2942,.F.);
#94623=ADVANCED_FACE('',(#9650),#2943,.F.);
#94624=ADVANCED_FACE('',(#9651),#90997,.F.);
#94625=ADVANCED_FACE('',(#9652),#90998,.F.);
#94626=ADVANCED_FACE('',(#9653),#2944,.F.);
#94627=ADVANCED_FACE('',(#9654),#2945,.F.);
#94628=ADVANCED_FACE('',(#9655),#5861,.F.);
#94629=ADVANCED_FACE('',(#9656),#90999,.F.);
#94630=ADVANCED_FACE('',(#9657),#2946,.F.);
#94631=ADVANCED_FACE('',(#9658),#91000,.F.);
#94632=ADVANCED_FACE('',(#9659),#91001,.F.);
#94633=ADVANCED_FACE('',(#9660),#2947,.F.);
#94634=ADVANCED_FACE('',(#9661),#2948,.F.);
#94635=ADVANCED_FACE('',(#9662),#91002,.F.);
#94636=ADVANCED_FACE('',(#9663),#91003,.F.);
#94637=ADVANCED_FACE('',(#9664),#2949,.F.);
#94638=ADVANCED_FACE('',(#9665),#91004,.F.);
#94639=ADVANCED_FACE('',(#9666),#91005,.F.);
#94640=ADVANCED_FACE('',(#9667),#2950,.F.);
#94641=ADVANCED_FACE('',(#9668),#91006,.F.);
#94642=ADVANCED_FACE('',(#9669),#91007,.F.);
#94643=ADVANCED_FACE('',(#9670),#2951,.F.);
#94644=ADVANCED_FACE('',(#9671),#2952,.F.);
#94645=ADVANCED_FACE('',(#9672),#91008,.F.);
#94646=ADVANCED_FACE('',(#9673),#91009,.F.);
#94647=ADVANCED_FACE('',(#9674),#2953,.F.);
#94648=ADVANCED_FACE('',(#9675),#91010,.F.);
#94649=ADVANCED_FACE('',(#9676),#5862,.F.);
#94650=ADVANCED_FACE('',(#9677),#2954,.F.);
#94651=ADVANCED_FACE('',(#9678),#2955,.F.);
#94652=ADVANCED_FACE('',(#9679),#91011,.F.);
#94653=ADVANCED_FACE('',(#9680),#91012,.F.);
#94654=ADVANCED_FACE('',(#9681),#2956,.F.);
#94655=ADVANCED_FACE('',(#9682),#2957,.F.);
#94656=ADVANCED_FACE('',(#9683),#5863,.F.);
#94657=ADVANCED_FACE('',(#9684),#91013,.F.);
#94658=ADVANCED_FACE('',(#9685),#2958,.F.);
#94659=ADVANCED_FACE('',(#9686),#91014,.F.);
#94660=ADVANCED_FACE('',(#9687),#91015,.F.);
#94661=ADVANCED_FACE('',(#9688),#2959,.F.);
#94662=ADVANCED_FACE('',(#9689),#2960,.F.);
#94663=ADVANCED_FACE('',(#9690),#91016,.F.);
#94664=ADVANCED_FACE('',(#9691),#91017,.F.);
#94665=ADVANCED_FACE('',(#9692),#2961,.F.);
#94666=ADVANCED_FACE('',(#9693),#91018,.F.);
#94667=ADVANCED_FACE('',(#9694),#91019,.F.);
#94668=ADVANCED_FACE('',(#9695),#2962,.F.);
#94669=ADVANCED_FACE('',(#9696),#91020,.F.);
#94670=ADVANCED_FACE('',(#9697),#91021,.F.);
#94671=ADVANCED_FACE('',(#9698),#2963,.F.);
#94672=ADVANCED_FACE('',(#9699),#2964,.F.);
#94673=ADVANCED_FACE('',(#9700),#91022,.F.);
#94674=ADVANCED_FACE('',(#9701),#91023,.F.);
#94675=ADVANCED_FACE('',(#9702),#2965,.F.);
#94676=ADVANCED_FACE('',(#9703),#91024,.F.);
#94677=ADVANCED_FACE('',(#9704),#5864,.F.);
#94678=ADVANCED_FACE('',(#9705),#2966,.F.);
#94679=ADVANCED_FACE('',(#9706),#2967,.F.);
#94680=ADVANCED_FACE('',(#9707),#91025,.F.);
#94681=ADVANCED_FACE('',(#9708),#91026,.F.);
#94682=ADVANCED_FACE('',(#9709),#2968,.F.);
#94683=ADVANCED_FACE('',(#9710),#2969,.F.);
#94684=ADVANCED_FACE('',(#9711),#5865,.F.);
#94685=ADVANCED_FACE('',(#9712),#91027,.F.);
#94686=ADVANCED_FACE('',(#9713),#2970,.F.);
#94687=ADVANCED_FACE('',(#9714),#91028,.F.);
#94688=ADVANCED_FACE('',(#9715),#91029,.F.);
#94689=ADVANCED_FACE('',(#9716),#2971,.F.);
#94690=ADVANCED_FACE('',(#9717),#2972,.F.);
#94691=ADVANCED_FACE('',(#9718),#91030,.F.);
#94692=ADVANCED_FACE('',(#9719),#91031,.F.);
#94693=ADVANCED_FACE('',(#9720),#2973,.F.);
#94694=ADVANCED_FACE('',(#9721),#91032,.F.);
#94695=ADVANCED_FACE('',(#9722),#91033,.F.);
#94696=ADVANCED_FACE('',(#9723),#2974,.F.);
#94697=ADVANCED_FACE('',(#9724),#91034,.F.);
#94698=ADVANCED_FACE('',(#9725),#91035,.F.);
#94699=ADVANCED_FACE('',(#9726),#2975,.F.);
#94700=ADVANCED_FACE('',(#9727),#2976,.F.);
#94701=ADVANCED_FACE('',(#9728),#91036,.F.);
#94702=ADVANCED_FACE('',(#9729),#91037,.F.);
#94703=ADVANCED_FACE('',(#9730),#2977,.F.);
#94704=ADVANCED_FACE('',(#9731),#91038,.F.);
#94705=ADVANCED_FACE('',(#9732),#5866,.F.);
#94706=ADVANCED_FACE('',(#9733),#2978,.F.);
#94707=ADVANCED_FACE('',(#9734),#2979,.F.);
#94708=ADVANCED_FACE('',(#9735),#91039,.F.);
#94709=ADVANCED_FACE('',(#9736),#91040,.F.);
#94710=ADVANCED_FACE('',(#9737),#2980,.F.);
#94711=ADVANCED_FACE('',(#9738),#2981,.F.);
#94712=ADVANCED_FACE('',(#9739),#5867,.F.);
#94713=ADVANCED_FACE('',(#9740),#91041,.F.);
#94714=ADVANCED_FACE('',(#9741),#2982,.F.);
#94715=ADVANCED_FACE('',(#9742),#91042,.F.);
#94716=ADVANCED_FACE('',(#9743),#91043,.F.);
#94717=ADVANCED_FACE('',(#9744),#2983,.F.);
#94718=ADVANCED_FACE('',(#9745),#2984,.F.);
#94719=ADVANCED_FACE('',(#9746),#91044,.F.);
#94720=ADVANCED_FACE('',(#9747),#91045,.F.);
#94721=ADVANCED_FACE('',(#9748),#2985,.F.);
#94722=ADVANCED_FACE('',(#9749),#91046,.F.);
#94723=ADVANCED_FACE('',(#9750),#91047,.F.);
#94724=ADVANCED_FACE('',(#9751),#2986,.F.);
#94725=ADVANCED_FACE('',(#9752),#91048,.F.);
#94726=ADVANCED_FACE('',(#9753),#91049,.F.);
#94727=ADVANCED_FACE('',(#9754),#2987,.F.);
#94728=ADVANCED_FACE('',(#9755),#2988,.F.);
#94729=ADVANCED_FACE('',(#9756),#91050,.F.);
#94730=ADVANCED_FACE('',(#9757),#91051,.F.);
#94731=ADVANCED_FACE('',(#9758),#2989,.F.);
#94732=ADVANCED_FACE('',(#9759),#91052,.F.);
#94733=ADVANCED_FACE('',(#9760),#5868,.F.);
#94734=ADVANCED_FACE('',(#9761),#2990,.F.);
#94735=ADVANCED_FACE('',(#9762),#2991,.F.);
#94736=ADVANCED_FACE('',(#9763),#91053,.F.);
#94737=ADVANCED_FACE('',(#9764),#91054,.F.);
#94738=ADVANCED_FACE('',(#9765),#2992,.F.);
#94739=ADVANCED_FACE('',(#9766),#2993,.F.);
#94740=ADVANCED_FACE('',(#9767),#5869,.F.);
#94741=ADVANCED_FACE('',(#9768),#91055,.F.);
#94742=ADVANCED_FACE('',(#9769),#2994,.F.);
#94743=ADVANCED_FACE('',(#9770),#91056,.F.);
#94744=ADVANCED_FACE('',(#9771),#91057,.F.);
#94745=ADVANCED_FACE('',(#9772),#2995,.F.);
#94746=ADVANCED_FACE('',(#9773),#2996,.F.);
#94747=ADVANCED_FACE('',(#9774),#91058,.F.);
#94748=ADVANCED_FACE('',(#9775),#91059,.F.);
#94749=ADVANCED_FACE('',(#9776),#2997,.F.);
#94750=ADVANCED_FACE('',(#9777),#91060,.F.);
#94751=ADVANCED_FACE('',(#9778),#91061,.F.);
#94752=ADVANCED_FACE('',(#9779),#2998,.F.);
#94753=ADVANCED_FACE('',(#9780),#91062,.F.);
#94754=ADVANCED_FACE('',(#9781),#91063,.F.);
#94755=ADVANCED_FACE('',(#9782),#2999,.F.);
#94756=ADVANCED_FACE('',(#9783),#3000,.F.);
#94757=ADVANCED_FACE('',(#9784),#91064,.F.);
#94758=ADVANCED_FACE('',(#9785),#91065,.F.);
#94759=ADVANCED_FACE('',(#9786),#3001,.F.);
#94760=ADVANCED_FACE('',(#9787),#91066,.F.);
#94761=ADVANCED_FACE('',(#9788),#5870,.F.);
#94762=ADVANCED_FACE('',(#9789),#3002,.F.);
#94763=ADVANCED_FACE('',(#9790),#3003,.F.);
#94764=ADVANCED_FACE('',(#9791),#91067,.F.);
#94765=ADVANCED_FACE('',(#9792),#91068,.F.);
#94766=ADVANCED_FACE('',(#9793),#3004,.F.);
#94767=ADVANCED_FACE('',(#9794),#3005,.F.);
#94768=ADVANCED_FACE('',(#9795),#5871,.F.);
#94769=ADVANCED_FACE('',(#9796),#91069,.F.);
#94770=ADVANCED_FACE('',(#9797),#3006,.F.);
#94771=ADVANCED_FACE('',(#9798),#91070,.F.);
#94772=ADVANCED_FACE('',(#9799),#91071,.F.);
#94773=ADVANCED_FACE('',(#9800),#3007,.F.);
#94774=ADVANCED_FACE('',(#9801),#3008,.F.);
#94775=ADVANCED_FACE('',(#9802),#91072,.F.);
#94776=ADVANCED_FACE('',(#9803),#91073,.F.);
#94777=ADVANCED_FACE('',(#9804),#3009,.F.);
#94778=ADVANCED_FACE('',(#9805),#91074,.F.);
#94779=ADVANCED_FACE('',(#9806),#91075,.F.);
#94780=ADVANCED_FACE('',(#9807),#3010,.F.);
#94781=ADVANCED_FACE('',(#9808),#91076,.F.);
#94782=ADVANCED_FACE('',(#9809),#91077,.F.);
#94783=ADVANCED_FACE('',(#9810),#3011,.F.);
#94784=ADVANCED_FACE('',(#9811),#3012,.F.);
#94785=ADVANCED_FACE('',(#9812),#91078,.F.);
#94786=ADVANCED_FACE('',(#9813),#91079,.F.);
#94787=ADVANCED_FACE('',(#9814),#3013,.F.);
#94788=ADVANCED_FACE('',(#9815),#91080,.F.);
#94789=ADVANCED_FACE('',(#9816),#5872,.F.);
#94790=ADVANCED_FACE('',(#9817),#3014,.F.);
#94791=ADVANCED_FACE('',(#9818),#3015,.F.);
#94792=ADVANCED_FACE('',(#9819),#91081,.F.);
#94793=ADVANCED_FACE('',(#9820),#91082,.F.);
#94794=ADVANCED_FACE('',(#9821),#3016,.F.);
#94795=ADVANCED_FACE('',(#9822),#3017,.F.);
#94796=ADVANCED_FACE('',(#9823),#5873,.F.);
#94797=ADVANCED_FACE('',(#9824),#91083,.F.);
#94798=ADVANCED_FACE('',(#9825),#3018,.F.);
#94799=ADVANCED_FACE('',(#9826),#91084,.F.);
#94800=ADVANCED_FACE('',(#9827),#91085,.F.);
#94801=ADVANCED_FACE('',(#9828),#3019,.F.);
#94802=ADVANCED_FACE('',(#9829),#3020,.F.);
#94803=ADVANCED_FACE('',(#9830),#91086,.F.);
#94804=ADVANCED_FACE('',(#9831),#91087,.F.);
#94805=ADVANCED_FACE('',(#9832),#3021,.F.);
#94806=ADVANCED_FACE('',(#9833),#91088,.F.);
#94807=ADVANCED_FACE('',(#9834),#91089,.F.);
#94808=ADVANCED_FACE('',(#9835),#3022,.F.);
#94809=ADVANCED_FACE('',(#9836),#91090,.F.);
#94810=ADVANCED_FACE('',(#9837),#91091,.F.);
#94811=ADVANCED_FACE('',(#9838),#3023,.F.);
#94812=ADVANCED_FACE('',(#9839),#3024,.F.);
#94813=ADVANCED_FACE('',(#9840),#91092,.F.);
#94814=ADVANCED_FACE('',(#9841),#91093,.F.);
#94815=ADVANCED_FACE('',(#9842),#3025,.F.);
#94816=ADVANCED_FACE('',(#9843),#91094,.F.);
#94817=ADVANCED_FACE('',(#9844),#5874,.F.);
#94818=ADVANCED_FACE('',(#9845),#3026,.F.);
#94819=ADVANCED_FACE('',(#9846),#3027,.F.);
#94820=ADVANCED_FACE('',(#9847),#91095,.F.);
#94821=ADVANCED_FACE('',(#9848),#91096,.F.);
#94822=ADVANCED_FACE('',(#9849),#3028,.F.);
#94823=ADVANCED_FACE('',(#9850),#3029,.F.);
#94824=ADVANCED_FACE('',(#9851),#5875,.F.);
#94825=ADVANCED_FACE('',(#9852),#91097,.F.);
#94826=ADVANCED_FACE('',(#9853),#3030,.F.);
#94827=ADVANCED_FACE('',(#9854),#91098,.F.);
#94828=ADVANCED_FACE('',(#9855),#91099,.F.);
#94829=ADVANCED_FACE('',(#9856),#3031,.F.);
#94830=ADVANCED_FACE('',(#9857),#3032,.F.);
#94831=ADVANCED_FACE('',(#9858),#91100,.F.);
#94832=ADVANCED_FACE('',(#9859),#91101,.F.);
#94833=ADVANCED_FACE('',(#9860),#3033,.F.);
#94834=ADVANCED_FACE('',(#9861),#91102,.F.);
#94835=ADVANCED_FACE('',(#9862),#91103,.F.);
#94836=ADVANCED_FACE('',(#9863),#3034,.F.);
#94837=ADVANCED_FACE('',(#9864),#91104,.F.);
#94838=ADVANCED_FACE('',(#9865),#91105,.F.);
#94839=ADVANCED_FACE('',(#9866),#3035,.F.);
#94840=ADVANCED_FACE('',(#9867),#3036,.F.);
#94841=ADVANCED_FACE('',(#9868),#91106,.F.);
#94842=ADVANCED_FACE('',(#9869),#91107,.F.);
#94843=ADVANCED_FACE('',(#9870),#3037,.F.);
#94844=ADVANCED_FACE('',(#9871),#91108,.F.);
#94845=ADVANCED_FACE('',(#9872),#5876,.F.);
#94846=ADVANCED_FACE('',(#9873),#3038,.F.);
#94847=ADVANCED_FACE('',(#9874),#3039,.F.);
#94848=ADVANCED_FACE('',(#9875),#91109,.F.);
#94849=ADVANCED_FACE('',(#9876),#91110,.F.);
#94850=ADVANCED_FACE('',(#9877),#3040,.F.);
#94851=ADVANCED_FACE('',(#9878),#3041,.F.);
#94852=ADVANCED_FACE('',(#9879),#5877,.F.);
#94853=ADVANCED_FACE('',(#9880),#91111,.F.);
#94854=ADVANCED_FACE('',(#9881),#3042,.F.);
#94855=ADVANCED_FACE('',(#9882),#91112,.F.);
#94856=ADVANCED_FACE('',(#9883),#91113,.F.);
#94857=ADVANCED_FACE('',(#9884),#3043,.F.);
#94858=ADVANCED_FACE('',(#9885),#3044,.F.);
#94859=ADVANCED_FACE('',(#9886),#91114,.F.);
#94860=ADVANCED_FACE('',(#9887),#91115,.F.);
#94861=ADVANCED_FACE('',(#9888),#3045,.F.);
#94862=ADVANCED_FACE('',(#9889),#91116,.F.);
#94863=ADVANCED_FACE('',(#9890),#91117,.F.);
#94864=ADVANCED_FACE('',(#9891),#3046,.F.);
#94865=ADVANCED_FACE('',(#9892),#91118,.F.);
#94866=ADVANCED_FACE('',(#9893),#91119,.F.);
#94867=ADVANCED_FACE('',(#9894),#3047,.F.);
#94868=ADVANCED_FACE('',(#9895),#3048,.F.);
#94869=ADVANCED_FACE('',(#9896),#91120,.F.);
#94870=ADVANCED_FACE('',(#9897),#91121,.F.);
#94871=ADVANCED_FACE('',(#9898),#3049,.F.);
#94872=ADVANCED_FACE('',(#9899),#91122,.F.);
#94873=ADVANCED_FACE('',(#9900),#3050,.F.);
#94874=ADVANCED_FACE('',(#9901),#3051,.F.);
#94875=ADVANCED_FACE('',(#9902),#91123,.F.);
#94876=ADVANCED_FACE('',(#9903),#91124,.F.);
#94877=ADVANCED_FACE('',(#9904),#3052,.F.);
#94878=ADVANCED_FACE('',(#9905),#3053,.F.);
#94879=ADVANCED_FACE('',(#9906),#91125,.F.);
#94880=ADVANCED_FACE('',(#9907),#3054,.F.);
#94881=ADVANCED_FACE('',(#9908),#91126,.F.);
#94882=ADVANCED_FACE('',(#9909),#91127,.F.);
#94883=ADVANCED_FACE('',(#9910),#3055,.F.);
#94884=ADVANCED_FACE('',(#9911),#3056,.F.);
#94885=ADVANCED_FACE('',(#9912),#91128,.F.);
#94886=ADVANCED_FACE('',(#9913),#91129,.F.);
#94887=ADVANCED_FACE('',(#9914),#3057,.F.);
#94888=ADVANCED_FACE('',(#9915),#91130,.F.);
#94889=ADVANCED_FACE('',(#9916),#91131,.F.);
#94890=ADVANCED_FACE('',(#9917),#3058,.F.);
#94891=ADVANCED_FACE('',(#9918),#91132,.F.);
#94892=ADVANCED_FACE('',(#9919),#91133,.F.);
#94893=ADVANCED_FACE('',(#9920),#3059,.F.);
#94894=ADVANCED_FACE('',(#9921),#3060,.F.);
#94895=ADVANCED_FACE('',(#9922),#91134,.F.);
#94896=ADVANCED_FACE('',(#9923),#91135,.F.);
#94897=ADVANCED_FACE('',(#9924),#3061,.F.);
#94898=ADVANCED_FACE('',(#9925),#91136,.F.);
#94899=ADVANCED_FACE('',(#9926),#5878,.F.);
#94900=ADVANCED_FACE('',(#9927),#3062,.F.);
#94901=ADVANCED_FACE('',(#9928),#3063,.F.);
#94902=ADVANCED_FACE('',(#9929),#91137,.F.);
#94903=ADVANCED_FACE('',(#9930),#91138,.F.);
#94904=ADVANCED_FACE('',(#9931),#3064,.F.);
#94905=ADVANCED_FACE('',(#9932),#3065,.F.);
#94906=ADVANCED_FACE('',(#9933),#5879,.F.);
#94907=ADVANCED_FACE('',(#9934),#91139,.F.);
#94908=ADVANCED_FACE('',(#9935),#3066,.F.);
#94909=ADVANCED_FACE('',(#9936),#91140,.F.);
#94910=ADVANCED_FACE('',(#9937),#91141,.F.);
#94911=ADVANCED_FACE('',(#9938),#3067,.F.);
#94912=ADVANCED_FACE('',(#9939),#3068,.F.);
#94913=ADVANCED_FACE('',(#9940),#91142,.F.);
#94914=ADVANCED_FACE('',(#9941),#91143,.F.);
#94915=ADVANCED_FACE('',(#9942),#3069,.F.);
#94916=ADVANCED_FACE('',(#9943),#91144,.F.);
#94917=ADVANCED_FACE('',(#9944),#91145,.F.);
#94918=ADVANCED_FACE('',(#9945),#3070,.F.);
#94919=ADVANCED_FACE('',(#9946),#91146,.F.);
#94920=ADVANCED_FACE('',(#9947),#91147,.F.);
#94921=ADVANCED_FACE('',(#9948),#3071,.F.);
#94922=ADVANCED_FACE('',(#9949),#3072,.F.);
#94923=ADVANCED_FACE('',(#9950),#91148,.F.);
#94924=ADVANCED_FACE('',(#9951),#91149,.F.);
#94925=ADVANCED_FACE('',(#9952),#3073,.F.);
#94926=ADVANCED_FACE('',(#9953),#91150,.F.);
#94927=ADVANCED_FACE('',(#9954),#5880,.F.);
#94928=ADVANCED_FACE('',(#9955),#3074,.F.);
#94929=ADVANCED_FACE('',(#9956),#3075,.F.);
#94930=ADVANCED_FACE('',(#9957),#91151,.F.);
#94931=ADVANCED_FACE('',(#9958),#91152,.F.);
#94932=ADVANCED_FACE('',(#9959),#3076,.F.);
#94933=ADVANCED_FACE('',(#9960),#3077,.F.);
#94934=ADVANCED_FACE('',(#9961),#5881,.F.);
#94935=ADVANCED_FACE('',(#9962),#91153,.F.);
#94936=ADVANCED_FACE('',(#9963),#3078,.F.);
#94937=ADVANCED_FACE('',(#9964),#91154,.F.);
#94938=ADVANCED_FACE('',(#9965),#91155,.F.);
#94939=ADVANCED_FACE('',(#9966),#3079,.F.);
#94940=ADVANCED_FACE('',(#9967),#3080,.F.);
#94941=ADVANCED_FACE('',(#9968),#91156,.F.);
#94942=ADVANCED_FACE('',(#9969),#91157,.F.);
#94943=ADVANCED_FACE('',(#9970),#3081,.F.);
#94944=ADVANCED_FACE('',(#9971),#91158,.F.);
#94945=ADVANCED_FACE('',(#9972),#91159,.F.);
#94946=ADVANCED_FACE('',(#9973),#3082,.F.);
#94947=ADVANCED_FACE('',(#9974),#91160,.F.);
#94948=ADVANCED_FACE('',(#9975),#91161,.F.);
#94949=ADVANCED_FACE('',(#9976),#3083,.F.);
#94950=ADVANCED_FACE('',(#9977),#3084,.F.);
#94951=ADVANCED_FACE('',(#9978),#91162,.F.);
#94952=ADVANCED_FACE('',(#9979),#91163,.F.);
#94953=ADVANCED_FACE('',(#9980),#3085,.F.);
#94954=ADVANCED_FACE('',(#9981),#91164,.F.);
#94955=ADVANCED_FACE('',(#9982),#5882,.F.);
#94956=ADVANCED_FACE('',(#9983),#3086,.F.);
#94957=ADVANCED_FACE('',(#9984),#3087,.F.);
#94958=ADVANCED_FACE('',(#9985),#91165,.F.);
#94959=ADVANCED_FACE('',(#9986),#91166,.F.);
#94960=ADVANCED_FACE('',(#9987),#3088,.F.);
#94961=ADVANCED_FACE('',(#9988),#3089,.F.);
#94962=ADVANCED_FACE('',(#9989),#5883,.F.);
#94963=ADVANCED_FACE('',(#9990),#91167,.F.);
#94964=ADVANCED_FACE('',(#9991),#3090,.F.);
#94965=ADVANCED_FACE('',(#9992),#91168,.F.);
#94966=ADVANCED_FACE('',(#9993),#91169,.F.);
#94967=ADVANCED_FACE('',(#9994),#3091,.F.);
#94968=ADVANCED_FACE('',(#9995),#3092,.F.);
#94969=ADVANCED_FACE('',(#9996),#91170,.F.);
#94970=ADVANCED_FACE('',(#9997),#91171,.F.);
#94971=ADVANCED_FACE('',(#9998),#3093,.F.);
#94972=ADVANCED_FACE('',(#9999),#91172,.F.);
#94973=ADVANCED_FACE('',(#10000),#91173,.F.);
#94974=ADVANCED_FACE('',(#10001),#3094,.F.);
#94975=ADVANCED_FACE('',(#10002),#91174,.F.);
#94976=ADVANCED_FACE('',(#10003),#91175,.F.);
#94977=ADVANCED_FACE('',(#10004),#3095,.F.);
#94978=ADVANCED_FACE('',(#10005),#3096,.F.);
#94979=ADVANCED_FACE('',(#10006),#91176,.F.);
#94980=ADVANCED_FACE('',(#10007),#91177,.F.);
#94981=ADVANCED_FACE('',(#10008),#3097,.F.);
#94982=ADVANCED_FACE('',(#10009),#91178,.F.);
#94983=ADVANCED_FACE('',(#10010),#5884,.F.);
#94984=ADVANCED_FACE('',(#10011),#3098,.F.);
#94985=ADVANCED_FACE('',(#10012),#3099,.F.);
#94986=ADVANCED_FACE('',(#10013),#91179,.F.);
#94987=ADVANCED_FACE('',(#10014),#91180,.F.);
#94988=ADVANCED_FACE('',(#10015),#3100,.F.);
#94989=ADVANCED_FACE('',(#10016),#3101,.F.);
#94990=ADVANCED_FACE('',(#10017),#5885,.F.);
#94991=ADVANCED_FACE('',(#10018),#91181,.F.);
#94992=ADVANCED_FACE('',(#10019),#3102,.F.);
#94993=ADVANCED_FACE('',(#10020),#91182,.F.);
#94994=ADVANCED_FACE('',(#10021),#91183,.F.);
#94995=ADVANCED_FACE('',(#10022),#3103,.F.);
#94996=ADVANCED_FACE('',(#10023),#3104,.F.);
#94997=ADVANCED_FACE('',(#10024),#91184,.F.);
#94998=ADVANCED_FACE('',(#10025),#91185,.F.);
#94999=ADVANCED_FACE('',(#10026),#3105,.F.);
#95000=ADVANCED_FACE('',(#10027),#91186,.F.);
#95001=ADVANCED_FACE('',(#10028),#91187,.F.);
#95002=ADVANCED_FACE('',(#10029),#3106,.F.);
#95003=ADVANCED_FACE('',(#10030),#91188,.F.);
#95004=ADVANCED_FACE('',(#10031),#91189,.F.);
#95005=ADVANCED_FACE('',(#10032),#3107,.F.);
#95006=ADVANCED_FACE('',(#10033),#3108,.F.);
#95007=ADVANCED_FACE('',(#10034),#91190,.F.);
#95008=ADVANCED_FACE('',(#10035),#91191,.F.);
#95009=ADVANCED_FACE('',(#10036),#3109,.F.);
#95010=ADVANCED_FACE('',(#10037),#91192,.F.);
#95011=ADVANCED_FACE('',(#10038),#5886,.F.);
#95012=ADVANCED_FACE('',(#10039),#3110,.F.);
#95013=ADVANCED_FACE('',(#10040),#3111,.F.);
#95014=ADVANCED_FACE('',(#10041),#91193,.F.);
#95015=ADVANCED_FACE('',(#10042),#91194,.F.);
#95016=ADVANCED_FACE('',(#10043),#3112,.F.);
#95017=ADVANCED_FACE('',(#10044),#3113,.F.);
#95018=ADVANCED_FACE('',(#10045),#5887,.F.);
#95019=ADVANCED_FACE('',(#10046),#91195,.F.);
#95020=ADVANCED_FACE('',(#10047),#3114,.F.);
#95021=ADVANCED_FACE('',(#10048),#91196,.F.);
#95022=ADVANCED_FACE('',(#10049),#91197,.F.);
#95023=ADVANCED_FACE('',(#10050),#3115,.F.);
#95024=ADVANCED_FACE('',(#10051),#3116,.F.);
#95025=ADVANCED_FACE('',(#10052),#91198,.F.);
#95026=ADVANCED_FACE('',(#10053),#91199,.F.);
#95027=ADVANCED_FACE('',(#10054),#3117,.F.);
#95028=ADVANCED_FACE('',(#10055),#91200,.F.);
#95029=ADVANCED_FACE('',(#10056),#91201,.F.);
#95030=ADVANCED_FACE('',(#10057),#3118,.F.);
#95031=ADVANCED_FACE('',(#10058),#91202,.F.);
#95032=ADVANCED_FACE('',(#10059),#91203,.F.);
#95033=ADVANCED_FACE('',(#10060),#3119,.F.);
#95034=ADVANCED_FACE('',(#10061),#3120,.F.);
#95035=ADVANCED_FACE('',(#10062),#91204,.F.);
#95036=ADVANCED_FACE('',(#10063),#91205,.F.);
#95037=ADVANCED_FACE('',(#10064),#3121,.F.);
#95038=ADVANCED_FACE('',(#10065),#91206,.F.);
#95039=ADVANCED_FACE('',(#10066),#5888,.F.);
#95040=ADVANCED_FACE('',(#10067),#3122,.F.);
#95041=ADVANCED_FACE('',(#10068),#3123,.F.);
#95042=ADVANCED_FACE('',(#10069),#91207,.F.);
#95043=ADVANCED_FACE('',(#10070),#91208,.F.);
#95044=ADVANCED_FACE('',(#10071),#3124,.F.);
#95045=ADVANCED_FACE('',(#10072),#3125,.F.);
#95046=ADVANCED_FACE('',(#10073),#5889,.F.);
#95047=ADVANCED_FACE('',(#10074),#91209,.F.);
#95048=ADVANCED_FACE('',(#10075),#3126,.F.);
#95049=ADVANCED_FACE('',(#10076),#91210,.F.);
#95050=ADVANCED_FACE('',(#10077),#91211,.F.);
#95051=ADVANCED_FACE('',(#10078),#3127,.F.);
#95052=ADVANCED_FACE('',(#10079),#3128,.F.);
#95053=ADVANCED_FACE('',(#10080),#91212,.F.);
#95054=ADVANCED_FACE('',(#10081),#91213,.F.);
#95055=ADVANCED_FACE('',(#10082),#3129,.F.);
#95056=ADVANCED_FACE('',(#10083),#91214,.F.);
#95057=ADVANCED_FACE('',(#10084),#91215,.F.);
#95058=ADVANCED_FACE('',(#10085),#3130,.F.);
#95059=ADVANCED_FACE('',(#10086),#91216,.F.);
#95060=ADVANCED_FACE('',(#10087),#91217,.F.);
#95061=ADVANCED_FACE('',(#10088),#3131,.F.);
#95062=ADVANCED_FACE('',(#10089),#3132,.F.);
#95063=ADVANCED_FACE('',(#10090),#91218,.F.);
#95064=ADVANCED_FACE('',(#10091),#91219,.F.);
#95065=ADVANCED_FACE('',(#10092),#3133,.F.);
#95066=ADVANCED_FACE('',(#10093),#91220,.F.);
#95067=ADVANCED_FACE('',(#10094),#5890,.F.);
#95068=ADVANCED_FACE('',(#10095),#3134,.F.);
#95069=ADVANCED_FACE('',(#10096),#3135,.F.);
#95070=ADVANCED_FACE('',(#10097),#91221,.F.);
#95071=ADVANCED_FACE('',(#10098),#91222,.F.);
#95072=ADVANCED_FACE('',(#10099),#3136,.F.);
#95073=ADVANCED_FACE('',(#10100),#3137,.F.);
#95074=ADVANCED_FACE('',(#10101),#5891,.F.);
#95075=ADVANCED_FACE('',(#10102),#91223,.F.);
#95076=ADVANCED_FACE('',(#10103),#3138,.F.);
#95077=ADVANCED_FACE('',(#10104),#91224,.F.);
#95078=ADVANCED_FACE('',(#10105),#91225,.F.);
#95079=ADVANCED_FACE('',(#10106),#3139,.F.);
#95080=ADVANCED_FACE('',(#10107),#3140,.F.);
#95081=ADVANCED_FACE('',(#10108),#91226,.F.);
#95082=ADVANCED_FACE('',(#10109),#91227,.F.);
#95083=ADVANCED_FACE('',(#10110),#3141,.F.);
#95084=ADVANCED_FACE('',(#10111),#91228,.F.);
#95085=ADVANCED_FACE('',(#10112),#91229,.F.);
#95086=ADVANCED_FACE('',(#10113),#3142,.F.);
#95087=ADVANCED_FACE('',(#10114),#91230,.F.);
#95088=ADVANCED_FACE('',(#10115),#91231,.F.);
#95089=ADVANCED_FACE('',(#10116),#3143,.F.);
#95090=ADVANCED_FACE('',(#10117),#3144,.F.);
#95091=ADVANCED_FACE('',(#10118),#91232,.F.);
#95092=ADVANCED_FACE('',(#10119),#91233,.F.);
#95093=ADVANCED_FACE('',(#10120),#3145,.F.);
#95094=ADVANCED_FACE('',(#10121),#91234,.F.);
#95095=ADVANCED_FACE('',(#10122),#5892,.F.);
#95096=ADVANCED_FACE('',(#10123),#3146,.F.);
#95097=ADVANCED_FACE('',(#10124),#3147,.F.);
#95098=ADVANCED_FACE('',(#10125),#91235,.F.);
#95099=ADVANCED_FACE('',(#10126),#91236,.F.);
#95100=ADVANCED_FACE('',(#10127),#3148,.F.);
#95101=ADVANCED_FACE('',(#10128),#3149,.F.);
#95102=ADVANCED_FACE('',(#10129),#5893,.F.);
#95103=ADVANCED_FACE('',(#10130),#91237,.F.);
#95104=ADVANCED_FACE('',(#10131),#3150,.F.);
#95105=ADVANCED_FACE('',(#10132),#91238,.F.);
#95106=ADVANCED_FACE('',(#10133),#91239,.F.);
#95107=ADVANCED_FACE('',(#10134),#3151,.F.);
#95108=ADVANCED_FACE('',(#10135),#3152,.F.);
#95109=ADVANCED_FACE('',(#10136),#91240,.F.);
#95110=ADVANCED_FACE('',(#10137),#91241,.F.);
#95111=ADVANCED_FACE('',(#10138),#3153,.F.);
#95112=ADVANCED_FACE('',(#10139),#91242,.F.);
#95113=ADVANCED_FACE('',(#10140),#91243,.F.);
#95114=ADVANCED_FACE('',(#10141),#3154,.F.);
#95115=ADVANCED_FACE('',(#10142),#91244,.F.);
#95116=ADVANCED_FACE('',(#10143),#91245,.F.);
#95117=ADVANCED_FACE('',(#10144),#3155,.F.);
#95118=ADVANCED_FACE('',(#10145),#3156,.F.);
#95119=ADVANCED_FACE('',(#10146),#91246,.F.);
#95120=ADVANCED_FACE('',(#10147),#91247,.F.);
#95121=ADVANCED_FACE('',(#10148),#3157,.F.);
#95122=ADVANCED_FACE('',(#10149),#91248,.F.);
#95123=ADVANCED_FACE('',(#10150),#5894,.F.);
#95124=ADVANCED_FACE('',(#10151),#3158,.F.);
#95125=ADVANCED_FACE('',(#10152),#3159,.F.);
#95126=ADVANCED_FACE('',(#10153),#91249,.F.);
#95127=ADVANCED_FACE('',(#10154),#91250,.F.);
#95128=ADVANCED_FACE('',(#10155),#3160,.F.);
#95129=ADVANCED_FACE('',(#10156),#3161,.F.);
#95130=ADVANCED_FACE('',(#10157),#5895,.F.);
#95131=ADVANCED_FACE('',(#10158),#91251,.F.);
#95132=ADVANCED_FACE('',(#10159),#3162,.F.);
#95133=ADVANCED_FACE('',(#10160),#91252,.F.);
#95134=ADVANCED_FACE('',(#10161),#91253,.F.);
#95135=ADVANCED_FACE('',(#10162),#3163,.F.);
#95136=ADVANCED_FACE('',(#10163),#3164,.F.);
#95137=ADVANCED_FACE('',(#10164),#91254,.F.);
#95138=ADVANCED_FACE('',(#10165),#91255,.F.);
#95139=ADVANCED_FACE('',(#10166),#3165,.F.);
#95140=ADVANCED_FACE('',(#10167),#91256,.F.);
#95141=ADVANCED_FACE('',(#10168),#91257,.F.);
#95142=ADVANCED_FACE('',(#10169),#3166,.F.);
#95143=ADVANCED_FACE('',(#10170),#91258,.F.);
#95144=ADVANCED_FACE('',(#10171),#91259,.F.);
#95145=ADVANCED_FACE('',(#10172),#3167,.F.);
#95146=ADVANCED_FACE('',(#10173),#3168,.F.);
#95147=ADVANCED_FACE('',(#10174),#91260,.F.);
#95148=ADVANCED_FACE('',(#10175),#91261,.F.);
#95149=ADVANCED_FACE('',(#10176),#3169,.F.);
#95150=ADVANCED_FACE('',(#10177),#91262,.F.);
#95151=ADVANCED_FACE('',(#10178),#5896,.F.);
#95152=ADVANCED_FACE('',(#10179),#3170,.F.);
#95153=ADVANCED_FACE('',(#10180),#3171,.F.);
#95154=ADVANCED_FACE('',(#10181),#91263,.F.);
#95155=ADVANCED_FACE('',(#10182),#91264,.F.);
#95156=ADVANCED_FACE('',(#10183),#3172,.F.);
#95157=ADVANCED_FACE('',(#10184),#3173,.F.);
#95158=ADVANCED_FACE('',(#10185),#5897,.F.);
#95159=ADVANCED_FACE('',(#10186),#91265,.F.);
#95160=ADVANCED_FACE('',(#10187),#3174,.F.);
#95161=ADVANCED_FACE('',(#10188),#91266,.F.);
#95162=ADVANCED_FACE('',(#10189),#91267,.F.);
#95163=ADVANCED_FACE('',(#10190),#3175,.F.);
#95164=ADVANCED_FACE('',(#10191),#3176,.F.);
#95165=ADVANCED_FACE('',(#10192),#91268,.F.);
#95166=ADVANCED_FACE('',(#10193),#91269,.F.);
#95167=ADVANCED_FACE('',(#10194),#3177,.F.);
#95168=ADVANCED_FACE('',(#10195),#91270,.F.);
#95169=ADVANCED_FACE('',(#10196),#91271,.F.);
#95170=ADVANCED_FACE('',(#10197),#3178,.F.);
#95171=ADVANCED_FACE('',(#10198),#91272,.F.);
#95172=ADVANCED_FACE('',(#10199),#91273,.F.);
#95173=ADVANCED_FACE('',(#10200),#3179,.F.);
#95174=ADVANCED_FACE('',(#10201),#3180,.F.);
#95175=ADVANCED_FACE('',(#10202),#91274,.F.);
#95176=ADVANCED_FACE('',(#10203),#91275,.F.);
#95177=ADVANCED_FACE('',(#10204),#3181,.F.);
#95178=ADVANCED_FACE('',(#10205),#91276,.F.);
#95179=ADVANCED_FACE('',(#10206),#5898,.F.);
#95180=ADVANCED_FACE('',(#10207),#3182,.F.);
#95181=ADVANCED_FACE('',(#10208),#3183,.F.);
#95182=ADVANCED_FACE('',(#10209),#91277,.F.);
#95183=ADVANCED_FACE('',(#10210),#91278,.F.);
#95184=ADVANCED_FACE('',(#10211),#3184,.F.);
#95185=ADVANCED_FACE('',(#10212),#3185,.F.);
#95186=ADVANCED_FACE('',(#10213),#5899,.F.);
#95187=ADVANCED_FACE('',(#10214),#91279,.F.);
#95188=ADVANCED_FACE('',(#10215),#3186,.F.);
#95189=ADVANCED_FACE('',(#10216),#91280,.F.);
#95190=ADVANCED_FACE('',(#10217),#91281,.F.);
#95191=ADVANCED_FACE('',(#10218),#3187,.F.);
#95192=ADVANCED_FACE('',(#10219),#3188,.F.);
#95193=ADVANCED_FACE('',(#10220),#91282,.F.);
#95194=ADVANCED_FACE('',(#10221),#91283,.F.);
#95195=ADVANCED_FACE('',(#10222),#3189,.F.);
#95196=ADVANCED_FACE('',(#10223),#91284,.F.);
#95197=ADVANCED_FACE('',(#10224),#91285,.F.);
#95198=ADVANCED_FACE('',(#10225),#3190,.F.);
#95199=ADVANCED_FACE('',(#10226),#91286,.F.);
#95200=ADVANCED_FACE('',(#10227),#91287,.F.);
#95201=ADVANCED_FACE('',(#10228),#3191,.F.);
#95202=ADVANCED_FACE('',(#10229),#3192,.F.);
#95203=ADVANCED_FACE('',(#10230),#91288,.F.);
#95204=ADVANCED_FACE('',(#10231),#91289,.F.);
#95205=ADVANCED_FACE('',(#10232),#3193,.F.);
#95206=ADVANCED_FACE('',(#10233),#91290,.F.);
#95207=ADVANCED_FACE('',(#10234),#5900,.F.);
#95208=ADVANCED_FACE('',(#10235),#3194,.F.);
#95209=ADVANCED_FACE('',(#10236),#3195,.F.);
#95210=ADVANCED_FACE('',(#10237),#91291,.F.);
#95211=ADVANCED_FACE('',(#10238),#91292,.F.);
#95212=ADVANCED_FACE('',(#10239),#3196,.F.);
#95213=ADVANCED_FACE('',(#10240),#3197,.F.);
#95214=ADVANCED_FACE('',(#10241),#5901,.F.);
#95215=ADVANCED_FACE('',(#10242),#91293,.F.);
#95216=ADVANCED_FACE('',(#10243),#3198,.F.);
#95217=ADVANCED_FACE('',(#10244),#91294,.F.);
#95218=ADVANCED_FACE('',(#10245),#91295,.F.);
#95219=ADVANCED_FACE('',(#10246),#3199,.F.);
#95220=ADVANCED_FACE('',(#10247),#3200,.F.);
#95221=ADVANCED_FACE('',(#10248),#91296,.F.);
#95222=ADVANCED_FACE('',(#10249),#91297,.F.);
#95223=ADVANCED_FACE('',(#10250),#3201,.F.);
#95224=ADVANCED_FACE('',(#10251),#91298,.F.);
#95225=ADVANCED_FACE('',(#10252),#91299,.F.);
#95226=ADVANCED_FACE('',(#10253),#3202,.F.);
#95227=ADVANCED_FACE('',(#10254),#91300,.F.);
#95228=ADVANCED_FACE('',(#10255),#91301,.F.);
#95229=ADVANCED_FACE('',(#10256),#3203,.F.);
#95230=ADVANCED_FACE('',(#10257),#3204,.F.);
#95231=ADVANCED_FACE('',(#10258),#91302,.F.);
#95232=ADVANCED_FACE('',(#10259),#91303,.F.);
#95233=ADVANCED_FACE('',(#10260),#3205,.F.);
#95234=ADVANCED_FACE('',(#10261),#91304,.F.);
#95235=ADVANCED_FACE('',(#10262),#5902,.F.);
#95236=ADVANCED_FACE('',(#10263),#3206,.F.);
#95237=ADVANCED_FACE('',(#10264),#3207,.F.);
#95238=ADVANCED_FACE('',(#10265),#91305,.F.);
#95239=ADVANCED_FACE('',(#10266),#91306,.F.);
#95240=ADVANCED_FACE('',(#10267),#3208,.F.);
#95241=ADVANCED_FACE('',(#10268),#3209,.F.);
#95242=ADVANCED_FACE('',(#10269),#5903,.F.);
#95243=ADVANCED_FACE('',(#10270),#91307,.F.);
#95244=ADVANCED_FACE('',(#10271),#3210,.F.);
#95245=ADVANCED_FACE('',(#10272),#91308,.F.);
#95246=ADVANCED_FACE('',(#10273),#91309,.F.);
#95247=ADVANCED_FACE('',(#10274),#3211,.F.);
#95248=ADVANCED_FACE('',(#10275),#3212,.F.);
#95249=ADVANCED_FACE('',(#10276),#91310,.F.);
#95250=ADVANCED_FACE('',(#10277),#91311,.F.);
#95251=ADVANCED_FACE('',(#10278),#3213,.F.);
#95252=ADVANCED_FACE('',(#10279),#91312,.F.);
#95253=ADVANCED_FACE('',(#10280),#91313,.F.);
#95254=ADVANCED_FACE('',(#10281),#3214,.F.);
#95255=ADVANCED_FACE('',(#10282),#91314,.F.);
#95256=ADVANCED_FACE('',(#10283),#91315,.F.);
#95257=ADVANCED_FACE('',(#10284),#3215,.F.);
#95258=ADVANCED_FACE('',(#10285),#3216,.F.);
#95259=ADVANCED_FACE('',(#10286),#91316,.F.);
#95260=ADVANCED_FACE('',(#10287),#91317,.F.);
#95261=ADVANCED_FACE('',(#10288),#3217,.F.);
#95262=ADVANCED_FACE('',(#10289),#91318,.F.);
#95263=ADVANCED_FACE('',(#10290),#5904,.F.);
#95264=ADVANCED_FACE('',(#10291),#3218,.F.);
#95265=ADVANCED_FACE('',(#10292),#3219,.F.);
#95266=ADVANCED_FACE('',(#10293),#91319,.F.);
#95267=ADVANCED_FACE('',(#10294),#91320,.F.);
#95268=ADVANCED_FACE('',(#10295),#3220,.F.);
#95269=ADVANCED_FACE('',(#10296),#3221,.F.);
#95270=ADVANCED_FACE('',(#10297),#5905,.F.);
#95271=ADVANCED_FACE('',(#10298),#91321,.F.);
#95272=ADVANCED_FACE('',(#10299),#3222,.F.);
#95273=ADVANCED_FACE('',(#10300),#91322,.F.);
#95274=ADVANCED_FACE('',(#10301),#91323,.F.);
#95275=ADVANCED_FACE('',(#10302),#3223,.F.);
#95276=ADVANCED_FACE('',(#10303),#3224,.F.);
#95277=ADVANCED_FACE('',(#10304),#91324,.F.);
#95278=ADVANCED_FACE('',(#10305),#91325,.F.);
#95279=ADVANCED_FACE('',(#10306),#3225,.F.);
#95280=ADVANCED_FACE('',(#10307),#91326,.F.);
#95281=ADVANCED_FACE('',(#10308),#5906,.F.);
#95282=ADVANCED_FACE('',(#10309),#5907,.F.);
#95283=ADVANCED_FACE('',(#10310),#5908,.F.);
#95284=ADVANCED_FACE('',(#10311),#5909,.F.);
#95285=ADVANCED_FACE('',(#10312),#5910,.T.);
#95286=ADVANCED_FACE('',(#10313),#5911,.T.);
#95287=ADVANCED_FACE('',(#10314),#5912,.T.);
#95288=ADVANCED_FACE('',(#10315),#5913,.T.);
#95289=ADVANCED_FACE('',(#10316),#91327,.T.);
#95290=ADVANCED_FACE('',(#10317),#188,.T.);
#95291=ADVANCED_FACE('',(#10318),#189,.F.);
#95292=ADVANCED_FACE('',(#10319),#190,.T.);
#95293=ADVANCED_FACE('',(#10320),#191,.F.);
#95294=ADVANCED_FACE('',(#10321),#91328,.F.);
#95295=ADVANCED_FACE('',(#10322),#6865,.F.);
#95296=ADVANCED_FACE('',(#10323),#192,.F.);
#95297=ADVANCED_FACE('',(#10324),#6866,.F.);
#95298=ADVANCED_FACE('',(#10325),#193,.T.);
#95299=ADVANCED_FACE('',(#10326),#6867,.F.);
#95300=ADVANCED_FACE('',(#10327),#5914,.F.);
#95301=ADVANCED_FACE('',(#10328),#5915,.F.);
#95302=ADVANCED_FACE('',(#10329),#5916,.T.);
#95303=ADVANCED_FACE('',(#10330),#5917,.T.);
#95304=ADVANCED_FACE('',(#10331),#6868,.F.);
#95305=ADVANCED_FACE('',(#10332),#194,.F.);
#95306=ADVANCED_FACE('',(#10333),#6869,.F.);
#95307=ADVANCED_FACE('',(#10334),#195,.T.);
#95308=ADVANCED_FACE('',(#10335),#6870,.F.);
#95309=ADVANCED_FACE('',(#10336),#5918,.F.);
#95310=ADVANCED_FACE('',(#10337),#5919,.F.);
#95311=ADVANCED_FACE('',(#10338),#5920,.T.);
#95312=ADVANCED_FACE('',(#10339),#5921,.T.);
#95313=ADVANCED_FACE('',(#10340),#6871,.F.);
#95314=ADVANCED_FACE('',(#10341),#196,.F.);
#95315=ADVANCED_FACE('',(#10342),#6872,.F.);
#95316=ADVANCED_FACE('',(#10343),#197,.T.);
#95317=ADVANCED_FACE('',(#10344),#6873,.F.);
#95318=ADVANCED_FACE('',(#10345),#5922,.F.);
#95319=ADVANCED_FACE('',(#10346),#5923,.F.);
#95320=ADVANCED_FACE('',(#10347),#5924,.T.);
#95321=ADVANCED_FACE('',(#10348),#5925,.T.);
#95322=ADVANCED_FACE('',(#10349),#6874,.F.);
#95323=ADVANCED_FACE('',(#10350),#198,.F.);
#95324=ADVANCED_FACE('',(#10351),#6875,.F.);
#95325=ADVANCED_FACE('',(#10352),#199,.T.);
#95326=ADVANCED_FACE('',(#10353),#6876,.F.);
#95327=ADVANCED_FACE('',(#10354),#5926,.F.);
#95328=ADVANCED_FACE('',(#10355),#5927,.F.);
#95329=ADVANCED_FACE('',(#10356),#5928,.T.);
#95330=ADVANCED_FACE('',(#10357),#5929,.T.);
#95331=ADVANCED_FACE('',(#10358),#6877,.F.);
#95332=ADVANCED_FACE('',(#10359),#200,.F.);
#95333=ADVANCED_FACE('',(#10360),#6878,.F.);
#95334=ADVANCED_FACE('',(#10361),#201,.T.);
#95335=ADVANCED_FACE('',(#10362),#6879,.F.);
#95336=ADVANCED_FACE('',(#10363),#5930,.F.);
#95337=ADVANCED_FACE('',(#10364),#5931,.F.);
#95338=ADVANCED_FACE('',(#10365),#5932,.T.);
#95339=ADVANCED_FACE('',(#10366),#5933,.T.);
#95340=ADVANCED_FACE('',(#10367),#6880,.F.);
#95341=ADVANCED_FACE('',(#10368),#202,.F.);
#95342=ADVANCED_FACE('',(#10369),#6881,.F.);
#95343=ADVANCED_FACE('',(#10370),#203,.T.);
#95344=ADVANCED_FACE('',(#10371),#6882,.F.);
#95345=ADVANCED_FACE('',(#10372),#5934,.F.);
#95346=ADVANCED_FACE('',(#10373),#5935,.F.);
#95347=ADVANCED_FACE('',(#10374),#5936,.T.);
#95348=ADVANCED_FACE('',(#10375),#5937,.T.);
#95349=ADVANCED_FACE('',(#10376),#6883,.F.);
#95350=ADVANCED_FACE('',(#10377),#204,.F.);
#95351=ADVANCED_FACE('',(#10378),#6884,.F.);
#95352=ADVANCED_FACE('',(#10379),#205,.T.);
#95353=ADVANCED_FACE('',(#10380),#6885,.F.);
#95354=ADVANCED_FACE('',(#10381),#5938,.F.);
#95355=ADVANCED_FACE('',(#10382),#5939,.F.);
#95356=ADVANCED_FACE('',(#10383),#5940,.T.);
#95357=ADVANCED_FACE('',(#10384),#5941,.T.);
#95358=ADVANCED_FACE('',(#10385),#6886,.F.);
#95359=ADVANCED_FACE('',(#10386),#206,.F.);
#95360=ADVANCED_FACE('',(#10387),#6887,.F.);
#95361=ADVANCED_FACE('',(#10388),#207,.T.);
#95362=ADVANCED_FACE('',(#10389),#6888,.F.);
#95363=ADVANCED_FACE('',(#10390),#5942,.F.);
#95364=ADVANCED_FACE('',(#10391),#5943,.F.);
#95365=ADVANCED_FACE('',(#10392),#5944,.T.);
#95366=ADVANCED_FACE('',(#10393),#5945,.T.);
#95367=ADVANCED_FACE('',(#10394),#6889,.F.);
#95368=ADVANCED_FACE('',(#10395),#208,.F.);
#95369=ADVANCED_FACE('',(#10396),#6890,.F.);
#95370=ADVANCED_FACE('',(#10397),#209,.T.);
#95371=ADVANCED_FACE('',(#10398),#6891,.F.);
#95372=ADVANCED_FACE('',(#10399),#5946,.F.);
#95373=ADVANCED_FACE('',(#10400),#5947,.F.);
#95374=ADVANCED_FACE('',(#10401),#5948,.T.);
#95375=ADVANCED_FACE('',(#10402),#5949,.T.);
#95376=ADVANCED_FACE('',(#10403),#6892,.F.);
#95377=ADVANCED_FACE('',(#10404),#210,.F.);
#95378=ADVANCED_FACE('',(#10405),#6893,.F.);
#95379=ADVANCED_FACE('',(#10406),#211,.T.);
#95380=ADVANCED_FACE('',(#10407),#6894,.F.);
#95381=ADVANCED_FACE('',(#10408),#5950,.F.);
#95382=ADVANCED_FACE('',(#10409),#5951,.F.);
#95383=ADVANCED_FACE('',(#10410),#5952,.T.);
#95384=ADVANCED_FACE('',(#10411),#5953,.T.);
#95385=ADVANCED_FACE('',(#10412),#6895,.F.);
#95386=ADVANCED_FACE('',(#10413),#212,.F.);
#95387=ADVANCED_FACE('',(#10414),#6896,.F.);
#95388=ADVANCED_FACE('',(#10415),#213,.T.);
#95389=ADVANCED_FACE('',(#10416),#6897,.F.);
#95390=ADVANCED_FACE('',(#10417),#5954,.F.);
#95391=ADVANCED_FACE('',(#10418),#5955,.F.);
#95392=ADVANCED_FACE('',(#10419),#5956,.T.);
#95393=ADVANCED_FACE('',(#10420),#5957,.T.);
#95394=ADVANCED_FACE('',(#10421),#6898,.F.);
#95395=ADVANCED_FACE('',(#10422),#214,.F.);
#95396=ADVANCED_FACE('',(#10423),#6899,.F.);
#95397=ADVANCED_FACE('',(#10424),#215,.T.);
#95398=ADVANCED_FACE('',(#10425),#6900,.F.);
#95399=ADVANCED_FACE('',(#10426),#5958,.F.);
#95400=ADVANCED_FACE('',(#10427),#5959,.F.);
#95401=ADVANCED_FACE('',(#10428),#5960,.T.);
#95402=ADVANCED_FACE('',(#10429),#5961,.T.);
#95403=ADVANCED_FACE('',(#10430),#6901,.F.);
#95404=ADVANCED_FACE('',(#10431),#216,.F.);
#95405=ADVANCED_FACE('',(#10432),#6902,.F.);
#95406=ADVANCED_FACE('',(#10433),#217,.T.);
#95407=ADVANCED_FACE('',(#10434),#6903,.F.);
#95408=ADVANCED_FACE('',(#10435),#5962,.F.);
#95409=ADVANCED_FACE('',(#10436),#5963,.F.);
#95410=ADVANCED_FACE('',(#10437),#5964,.T.);
#95411=ADVANCED_FACE('',(#10438),#5965,.T.);
#95412=ADVANCED_FACE('',(#10439),#6904,.F.);
#95413=ADVANCED_FACE('',(#10440),#218,.F.);
#95414=ADVANCED_FACE('',(#10441),#6905,.F.);
#95415=ADVANCED_FACE('',(#10442),#219,.T.);
#95416=ADVANCED_FACE('',(#10443),#6906,.F.);
#95417=ADVANCED_FACE('',(#10444),#5966,.F.);
#95418=ADVANCED_FACE('',(#10445),#5967,.F.);
#95419=ADVANCED_FACE('',(#10446),#5968,.T.);
#95420=ADVANCED_FACE('',(#10447),#5969,.T.);
#95421=ADVANCED_FACE('',(#10448),#6907,.F.);
#95422=ADVANCED_FACE('',(#10449),#220,.F.);
#95423=ADVANCED_FACE('',(#10450),#6908,.F.);
#95424=ADVANCED_FACE('',(#10451),#221,.T.);
#95425=ADVANCED_FACE('',(#10452),#6909,.F.);
#95426=ADVANCED_FACE('',(#10453),#5970,.F.);
#95427=ADVANCED_FACE('',(#10454),#5971,.F.);
#95428=ADVANCED_FACE('',(#10455),#5972,.T.);
#95429=ADVANCED_FACE('',(#10456),#5973,.T.);
#95430=ADVANCED_FACE('',(#10457),#6910,.F.);
#95431=ADVANCED_FACE('',(#10458),#222,.F.);
#95432=ADVANCED_FACE('',(#10459),#6911,.F.);
#95433=ADVANCED_FACE('',(#10460),#223,.T.);
#95434=ADVANCED_FACE('',(#10461),#6912,.F.);
#95435=ADVANCED_FACE('',(#10462),#5974,.F.);
#95436=ADVANCED_FACE('',(#10463),#5975,.F.);
#95437=ADVANCED_FACE('',(#10464),#5976,.T.);
#95438=ADVANCED_FACE('',(#10465),#5977,.T.);
#95439=ADVANCED_FACE('',(#10466),#6913,.F.);
#95440=ADVANCED_FACE('',(#10467),#224,.F.);
#95441=ADVANCED_FACE('',(#10468),#6914,.F.);
#95442=ADVANCED_FACE('',(#10469),#225,.T.);
#95443=ADVANCED_FACE('',(#10470),#6915,.F.);
#95444=ADVANCED_FACE('',(#10471),#5978,.F.);
#95445=ADVANCED_FACE('',(#10472),#5979,.F.);
#95446=ADVANCED_FACE('',(#10473),#5980,.T.);
#95447=ADVANCED_FACE('',(#10474),#5981,.T.);
#95448=ADVANCED_FACE('',(#10475),#6916,.F.);
#95449=ADVANCED_FACE('',(#10476),#226,.F.);
#95450=ADVANCED_FACE('',(#10477),#6917,.F.);
#95451=ADVANCED_FACE('',(#10478),#227,.T.);
#95452=ADVANCED_FACE('',(#10479),#6918,.F.);
#95453=ADVANCED_FACE('',(#10480),#5982,.F.);
#95454=ADVANCED_FACE('',(#10481),#5983,.F.);
#95455=ADVANCED_FACE('',(#10482),#5984,.T.);
#95456=ADVANCED_FACE('',(#10483),#5985,.T.);
#95457=ADVANCED_FACE('',(#10484),#6919,.F.);
#95458=ADVANCED_FACE('',(#10485),#228,.F.);
#95459=ADVANCED_FACE('',(#10486),#6920,.F.);
#95460=ADVANCED_FACE('',(#10487),#229,.T.);
#95461=ADVANCED_FACE('',(#10488),#6921,.F.);
#95462=ADVANCED_FACE('',(#10489),#5986,.F.);
#95463=ADVANCED_FACE('',(#10490),#5987,.F.);
#95464=ADVANCED_FACE('',(#10491),#5988,.T.);
#95465=ADVANCED_FACE('',(#10492),#5989,.T.);
#95466=ADVANCED_FACE('',(#10493),#6922,.F.);
#95467=ADVANCED_FACE('',(#10494),#230,.F.);
#95468=ADVANCED_FACE('',(#10495),#6923,.F.);
#95469=ADVANCED_FACE('',(#10496),#231,.T.);
#95470=ADVANCED_FACE('',(#10497),#6924,.F.);
#95471=ADVANCED_FACE('',(#10498),#5990,.F.);
#95472=ADVANCED_FACE('',(#10499),#5991,.F.);
#95473=ADVANCED_FACE('',(#10500),#5992,.T.);
#95474=ADVANCED_FACE('',(#10501),#5993,.T.);
#95475=ADVANCED_FACE('',(#10502),#6925,.F.);
#95476=ADVANCED_FACE('',(#10503),#232,.F.);
#95477=ADVANCED_FACE('',(#10504),#6926,.F.);
#95478=ADVANCED_FACE('',(#10505),#233,.T.);
#95479=ADVANCED_FACE('',(#10506),#6927,.F.);
#95480=ADVANCED_FACE('',(#10507),#5994,.F.);
#95481=ADVANCED_FACE('',(#10508),#5995,.F.);
#95482=ADVANCED_FACE('',(#10509),#5996,.T.);
#95483=ADVANCED_FACE('',(#10510),#5997,.T.);
#95484=ADVANCED_FACE('',(#10511),#6928,.F.);
#95485=ADVANCED_FACE('',(#10512),#234,.F.);
#95486=ADVANCED_FACE('',(#10513),#6929,.F.);
#95487=ADVANCED_FACE('',(#10514),#235,.T.);
#95488=ADVANCED_FACE('',(#10515),#6930,.F.);
#95489=ADVANCED_FACE('',(#10516),#5998,.F.);
#95490=ADVANCED_FACE('',(#10517),#5999,.F.);
#95491=ADVANCED_FACE('',(#10518),#6000,.T.);
#95492=ADVANCED_FACE('',(#10519),#6001,.T.);
#95493=ADVANCED_FACE('',(#10520),#6931,.F.);
#95494=ADVANCED_FACE('',(#10521),#236,.F.);
#95495=ADVANCED_FACE('',(#10522),#6932,.F.);
#95496=ADVANCED_FACE('',(#10523),#237,.T.);
#95497=ADVANCED_FACE('',(#10524),#6933,.F.);
#95498=ADVANCED_FACE('',(#10525),#6002,.F.);
#95499=ADVANCED_FACE('',(#10526),#6003,.F.);
#95500=ADVANCED_FACE('',(#10527),#6004,.T.);
#95501=ADVANCED_FACE('',(#10528),#6005,.T.);
#95502=ADVANCED_FACE('',(#10529),#6934,.F.);
#95503=ADVANCED_FACE('',(#10530),#238,.F.);
#95504=ADVANCED_FACE('',(#10531),#6935,.F.);
#95505=ADVANCED_FACE('',(#10532),#239,.T.);
#95506=ADVANCED_FACE('',(#10533),#6936,.F.);
#95507=ADVANCED_FACE('',(#10534),#6006,.F.);
#95508=ADVANCED_FACE('',(#10535),#6007,.F.);
#95509=ADVANCED_FACE('',(#10536),#6008,.T.);
#95510=ADVANCED_FACE('',(#10537),#6009,.T.);
#95511=ADVANCED_FACE('',(#10538),#6937,.F.);
#95512=ADVANCED_FACE('',(#10539),#240,.F.);
#95513=ADVANCED_FACE('',(#10540),#6938,.F.);
#95514=ADVANCED_FACE('',(#10541),#241,.T.);
#95515=ADVANCED_FACE('',(#10542),#6939,.F.);
#95516=ADVANCED_FACE('',(#10543),#6010,.F.);
#95517=ADVANCED_FACE('',(#10544),#6011,.F.);
#95518=ADVANCED_FACE('',(#10545),#6012,.T.);
#95519=ADVANCED_FACE('',(#10546),#6013,.T.);
#95520=ADVANCED_FACE('',(#10547),#6940,.F.);
#95521=ADVANCED_FACE('',(#10548),#242,.F.);
#95522=ADVANCED_FACE('',(#10549),#6941,.F.);
#95523=ADVANCED_FACE('',(#10550),#243,.T.);
#95524=ADVANCED_FACE('',(#10551),#6942,.F.);
#95525=ADVANCED_FACE('',(#10552),#6014,.F.);
#95526=ADVANCED_FACE('',(#10553),#6015,.F.);
#95527=ADVANCED_FACE('',(#10554),#6016,.T.);
#95528=ADVANCED_FACE('',(#10555),#6017,.T.);
#95529=ADVANCED_FACE('',(#10556),#6943,.F.);
#95530=ADVANCED_FACE('',(#10557),#244,.F.);
#95531=ADVANCED_FACE('',(#10558),#6944,.F.);
#95532=ADVANCED_FACE('',(#10559),#245,.T.);
#95533=ADVANCED_FACE('',(#10560),#6945,.F.);
#95534=ADVANCED_FACE('',(#10561),#6018,.F.);
#95535=ADVANCED_FACE('',(#10562),#6019,.F.);
#95536=ADVANCED_FACE('',(#10563),#6020,.T.);
#95537=ADVANCED_FACE('',(#10564),#6021,.T.);
#95538=ADVANCED_FACE('',(#10565),#6946,.F.);
#95539=ADVANCED_FACE('',(#10566),#246,.F.);
#95540=ADVANCED_FACE('',(#10567),#6947,.F.);
#95541=ADVANCED_FACE('',(#10568),#247,.T.);
#95542=ADVANCED_FACE('',(#10569),#6948,.F.);
#95543=ADVANCED_FACE('',(#10570),#6022,.F.);
#95544=ADVANCED_FACE('',(#10571),#6023,.F.);
#95545=ADVANCED_FACE('',(#10572),#6024,.T.);
#95546=ADVANCED_FACE('',(#10573),#6025,.T.);
#95547=ADVANCED_FACE('',(#10574),#6949,.F.);
#95548=ADVANCED_FACE('',(#10575),#248,.F.);
#95549=ADVANCED_FACE('',(#10576),#6950,.F.);
#95550=ADVANCED_FACE('',(#10577),#249,.T.);
#95551=ADVANCED_FACE('',(#10578),#6951,.F.);
#95552=ADVANCED_FACE('',(#10579),#6026,.F.);
#95553=ADVANCED_FACE('',(#10580),#6027,.F.);
#95554=ADVANCED_FACE('',(#10581),#6028,.T.);
#95555=ADVANCED_FACE('',(#10582),#6029,.T.);
#95556=ADVANCED_FACE('',(#10583),#6952,.F.);
#95557=ADVANCED_FACE('',(#10584),#250,.F.);
#95558=ADVANCED_FACE('',(#10585),#6953,.F.);
#95559=ADVANCED_FACE('',(#10586),#251,.T.);
#95560=ADVANCED_FACE('',(#10587),#6954,.F.);
#95561=ADVANCED_FACE('',(#10588),#6030,.F.);
#95562=ADVANCED_FACE('',(#10589),#6031,.F.);
#95563=ADVANCED_FACE('',(#10590),#6032,.T.);
#95564=ADVANCED_FACE('',(#10591),#6033,.T.);
#95565=ADVANCED_FACE('',(#10592),#6955,.F.);
#95566=ADVANCED_FACE('',(#10593),#252,.F.);
#95567=ADVANCED_FACE('',(#10594),#6956,.F.);
#95568=ADVANCED_FACE('',(#10595),#253,.T.);
#95569=ADVANCED_FACE('',(#10596),#6957,.F.);
#95570=ADVANCED_FACE('',(#10597),#6034,.F.);
#95571=ADVANCED_FACE('',(#10598),#6035,.F.);
#95572=ADVANCED_FACE('',(#10599),#6036,.T.);
#95573=ADVANCED_FACE('',(#10600),#6037,.T.);
#95574=ADVANCED_FACE('',(#10601),#6958,.F.);
#95575=ADVANCED_FACE('',(#10602),#254,.F.);
#95576=ADVANCED_FACE('',(#10603),#6959,.F.);
#95577=ADVANCED_FACE('',(#10604),#255,.T.);
#95578=ADVANCED_FACE('',(#10605),#6960,.F.);
#95579=ADVANCED_FACE('',(#10606),#6038,.F.);
#95580=ADVANCED_FACE('',(#10607),#6039,.F.);
#95581=ADVANCED_FACE('',(#10608),#6040,.T.);
#95582=ADVANCED_FACE('',(#10609),#6041,.T.);
#95583=ADVANCED_FACE('',(#10610),#6961,.F.);
#95584=ADVANCED_FACE('',(#10611),#256,.F.);
#95585=ADVANCED_FACE('',(#10612),#6962,.F.);
#95586=ADVANCED_FACE('',(#10613),#257,.T.);
#95587=ADVANCED_FACE('',(#10614),#6963,.F.);
#95588=ADVANCED_FACE('',(#10615),#6042,.F.);
#95589=ADVANCED_FACE('',(#10616),#6043,.F.);
#95590=ADVANCED_FACE('',(#10617),#6044,.T.);
#95591=ADVANCED_FACE('',(#10618),#6045,.T.);
#95592=ADVANCED_FACE('',(#10619),#6964,.F.);
#95593=ADVANCED_FACE('',(#10620),#258,.F.);
#95594=ADVANCED_FACE('',(#10621),#6965,.F.);
#95595=ADVANCED_FACE('',(#10622),#259,.T.);
#95596=ADVANCED_FACE('',(#10623),#6966,.F.);
#95597=ADVANCED_FACE('',(#10624),#6046,.F.);
#95598=ADVANCED_FACE('',(#10625),#6047,.F.);
#95599=ADVANCED_FACE('',(#10626),#6048,.T.);
#95600=ADVANCED_FACE('',(#10627),#6049,.T.);
#95601=ADVANCED_FACE('',(#10628),#6967,.F.);
#95602=ADVANCED_FACE('',(#10629),#260,.F.);
#95603=ADVANCED_FACE('',(#10630),#6968,.F.);
#95604=ADVANCED_FACE('',(#10631),#261,.T.);
#95605=ADVANCED_FACE('',(#10632),#6969,.F.);
#95606=ADVANCED_FACE('',(#10633),#6050,.F.);
#95607=ADVANCED_FACE('',(#10634),#6051,.F.);
#95608=ADVANCED_FACE('',(#10635),#6052,.T.);
#95609=ADVANCED_FACE('',(#10636),#6053,.T.);
#95610=ADVANCED_FACE('',(#10637),#6970,.F.);
#95611=ADVANCED_FACE('',(#10638),#262,.F.);
#95612=ADVANCED_FACE('',(#10639),#6971,.F.);
#95613=ADVANCED_FACE('',(#10640),#263,.T.);
#95614=ADVANCED_FACE('',(#10641),#6972,.F.);
#95615=ADVANCED_FACE('',(#10642),#6054,.F.);
#95616=ADVANCED_FACE('',(#10643),#6055,.F.);
#95617=ADVANCED_FACE('',(#10644),#6056,.T.);
#95618=ADVANCED_FACE('',(#10645),#6057,.T.);
#95619=ADVANCED_FACE('',(#10646),#6973,.F.);
#95620=ADVANCED_FACE('',(#10647),#264,.F.);
#95621=ADVANCED_FACE('',(#10648),#6974,.F.);
#95622=ADVANCED_FACE('',(#10649),#265,.T.);
#95623=ADVANCED_FACE('',(#10650),#6975,.F.);
#95624=ADVANCED_FACE('',(#10651),#6058,.F.);
#95625=ADVANCED_FACE('',(#10652),#6059,.F.);
#95626=ADVANCED_FACE('',(#10653),#6060,.T.);
#95627=ADVANCED_FACE('',(#10654),#6061,.T.);
#95628=ADVANCED_FACE('',(#10655),#6976,.F.);
#95629=ADVANCED_FACE('',(#10656),#266,.F.);
#95630=ADVANCED_FACE('',(#10657),#6977,.F.);
#95631=ADVANCED_FACE('',(#10658),#267,.T.);
#95632=ADVANCED_FACE('',(#10659),#6978,.F.);
#95633=ADVANCED_FACE('',(#10660),#6062,.F.);
#95634=ADVANCED_FACE('',(#10661),#6063,.F.);
#95635=ADVANCED_FACE('',(#10662),#6064,.T.);
#95636=ADVANCED_FACE('',(#10663),#6065,.T.);
#95637=ADVANCED_FACE('',(#10664),#6979,.F.);
#95638=ADVANCED_FACE('',(#10665),#268,.F.);
#95639=ADVANCED_FACE('',(#10666),#6980,.F.);
#95640=ADVANCED_FACE('',(#10667),#269,.T.);
#95641=ADVANCED_FACE('',(#10668),#6981,.F.);
#95642=ADVANCED_FACE('',(#10669),#6066,.F.);
#95643=ADVANCED_FACE('',(#10670),#6067,.F.);
#95644=ADVANCED_FACE('',(#10671),#6068,.T.);
#95645=ADVANCED_FACE('',(#10672),#6069,.T.);
#95646=ADVANCED_FACE('',(#10673),#6982,.F.);
#95647=ADVANCED_FACE('',(#10674),#270,.F.);
#95648=ADVANCED_FACE('',(#10675),#6983,.F.);
#95649=ADVANCED_FACE('',(#10676),#271,.T.);
#95650=ADVANCED_FACE('',(#10677),#6984,.F.);
#95651=ADVANCED_FACE('',(#10678),#6070,.F.);
#95652=ADVANCED_FACE('',(#10679),#6071,.F.);
#95653=ADVANCED_FACE('',(#10680),#6072,.T.);
#95654=ADVANCED_FACE('',(#10681),#6073,.T.);
#95655=ADVANCED_FACE('',(#10682),#6985,.F.);
#95656=ADVANCED_FACE('',(#10683),#272,.F.);
#95657=ADVANCED_FACE('',(#10684),#6986,.F.);
#95658=ADVANCED_FACE('',(#10685),#273,.T.);
#95659=ADVANCED_FACE('',(#10686),#6987,.F.);
#95660=ADVANCED_FACE('',(#10687),#6074,.F.);
#95661=ADVANCED_FACE('',(#10688),#6075,.F.);
#95662=ADVANCED_FACE('',(#10689),#6076,.T.);
#95663=ADVANCED_FACE('',(#10690),#6077,.T.);
#95664=ADVANCED_FACE('',(#10691),#6988,.F.);
#95665=ADVANCED_FACE('',(#10692),#274,.F.);
#95666=ADVANCED_FACE('',(#10693),#6989,.F.);
#95667=ADVANCED_FACE('',(#10694),#275,.T.);
#95668=ADVANCED_FACE('',(#10695),#6990,.F.);
#95669=ADVANCED_FACE('',(#10696),#6078,.F.);
#95670=ADVANCED_FACE('',(#10697),#6079,.F.);
#95671=ADVANCED_FACE('',(#10698),#6080,.T.);
#95672=ADVANCED_FACE('',(#10699),#6081,.T.);
#95673=ADVANCED_FACE('',(#10700),#6991,.F.);
#95674=ADVANCED_FACE('',(#10701),#276,.F.);
#95675=ADVANCED_FACE('',(#10702),#6992,.F.);
#95676=ADVANCED_FACE('',(#10703),#277,.T.);
#95677=ADVANCED_FACE('',(#10704),#6993,.F.);
#95678=ADVANCED_FACE('',(#10705),#6082,.F.);
#95679=ADVANCED_FACE('',(#10706),#6083,.F.);
#95680=ADVANCED_FACE('',(#10707),#6084,.T.);
#95681=ADVANCED_FACE('',(#10708),#6085,.T.);
#95682=ADVANCED_FACE('',(#10709),#6994,.F.);
#95683=ADVANCED_FACE('',(#10710),#278,.F.);
#95684=ADVANCED_FACE('',(#10711),#6995,.F.);
#95685=ADVANCED_FACE('',(#10712),#279,.T.);
#95686=ADVANCED_FACE('',(#10713),#6996,.F.);
#95687=ADVANCED_FACE('',(#10714),#6086,.F.);
#95688=ADVANCED_FACE('',(#10715),#6087,.F.);
#95689=ADVANCED_FACE('',(#10716),#6088,.T.);
#95690=ADVANCED_FACE('',(#10717),#6089,.T.);
#95691=ADVANCED_FACE('',(#10718),#6997,.F.);
#95692=ADVANCED_FACE('',(#10719),#280,.F.);
#95693=ADVANCED_FACE('',(#10720),#6998,.F.);
#95694=ADVANCED_FACE('',(#10721),#281,.T.);
#95695=ADVANCED_FACE('',(#10722),#6999,.F.);
#95696=ADVANCED_FACE('',(#10723),#6090,.F.);
#95697=ADVANCED_FACE('',(#10724),#6091,.F.);
#95698=ADVANCED_FACE('',(#10725),#6092,.T.);
#95699=ADVANCED_FACE('',(#10726),#6093,.T.);
#95700=ADVANCED_FACE('',(#10727),#7000,.F.);
#95701=ADVANCED_FACE('',(#10728),#282,.F.);
#95702=ADVANCED_FACE('',(#10729),#7001,.F.);
#95703=ADVANCED_FACE('',(#10730),#283,.T.);
#95704=ADVANCED_FACE('',(#10731),#7002,.F.);
#95705=ADVANCED_FACE('',(#10732),#6094,.F.);
#95706=ADVANCED_FACE('',(#10733),#6095,.F.);
#95707=ADVANCED_FACE('',(#10734),#6096,.T.);
#95708=ADVANCED_FACE('',(#10735),#6097,.T.);
#95709=ADVANCED_FACE('',(#10736),#7003,.F.);
#95710=ADVANCED_FACE('',(#10737),#284,.F.);
#95711=ADVANCED_FACE('',(#10738),#7004,.F.);
#95712=ADVANCED_FACE('',(#10739),#285,.T.);
#95713=ADVANCED_FACE('',(#10740),#7005,.F.);
#95714=ADVANCED_FACE('',(#10741),#6098,.F.);
#95715=ADVANCED_FACE('',(#10742),#6099,.F.);
#95716=ADVANCED_FACE('',(#10743),#6100,.T.);
#95717=ADVANCED_FACE('',(#10744),#6101,.T.);
#95718=ADVANCED_FACE('',(#10745),#7006,.F.);
#95719=ADVANCED_FACE('',(#10746),#286,.F.);
#95720=ADVANCED_FACE('',(#10747),#7007,.F.);
#95721=ADVANCED_FACE('',(#10748),#287,.T.);
#95722=ADVANCED_FACE('',(#10749),#7008,.F.);
#95723=ADVANCED_FACE('',(#10750),#6102,.F.);
#95724=ADVANCED_FACE('',(#10751),#6103,.F.);
#95725=ADVANCED_FACE('',(#10752),#6104,.T.);
#95726=ADVANCED_FACE('',(#10753),#6105,.T.);
#95727=ADVANCED_FACE('',(#10754),#7009,.F.);
#95728=ADVANCED_FACE('',(#10755),#288,.F.);
#95729=ADVANCED_FACE('',(#10756),#7010,.F.);
#95730=ADVANCED_FACE('',(#10757),#289,.T.);
#95731=ADVANCED_FACE('',(#10758),#7011,.F.);
#95732=ADVANCED_FACE('',(#10759),#6106,.F.);
#95733=ADVANCED_FACE('',(#10760),#6107,.F.);
#95734=ADVANCED_FACE('',(#10761),#6108,.T.);
#95735=ADVANCED_FACE('',(#10762),#6109,.T.);
#95736=ADVANCED_FACE('',(#10763),#7012,.F.);
#95737=ADVANCED_FACE('',(#10764),#290,.F.);
#95738=ADVANCED_FACE('',(#10765),#7013,.F.);
#95739=ADVANCED_FACE('',(#10766),#291,.T.);
#95740=ADVANCED_FACE('',(#10767),#7014,.F.);
#95741=ADVANCED_FACE('',(#10768),#6110,.F.);
#95742=ADVANCED_FACE('',(#10769),#6111,.F.);
#95743=ADVANCED_FACE('',(#10770),#6112,.T.);
#95744=ADVANCED_FACE('',(#10771),#6113,.T.);
#95745=ADVANCED_FACE('',(#10772),#7015,.F.);
#95746=ADVANCED_FACE('',(#10773),#292,.F.);
#95747=ADVANCED_FACE('',(#10774),#7016,.F.);
#95748=ADVANCED_FACE('',(#10775),#293,.T.);
#95749=ADVANCED_FACE('',(#10776),#7017,.F.);
#95750=ADVANCED_FACE('',(#10777),#6114,.F.);
#95751=ADVANCED_FACE('',(#10778),#6115,.F.);
#95752=ADVANCED_FACE('',(#10779),#6116,.T.);
#95753=ADVANCED_FACE('',(#10780),#6117,.T.);
#95754=ADVANCED_FACE('',(#10781),#7018,.F.);
#95755=ADVANCED_FACE('',(#10782),#294,.F.);
#95756=ADVANCED_FACE('',(#10783),#7019,.F.);
#95757=ADVANCED_FACE('',(#10784),#295,.T.);
#95758=ADVANCED_FACE('',(#10785),#7020,.F.);
#95759=ADVANCED_FACE('',(#10786),#6118,.F.);
#95760=ADVANCED_FACE('',(#10787),#6119,.F.);
#95761=ADVANCED_FACE('',(#10788),#6120,.T.);
#95762=ADVANCED_FACE('',(#10789),#6121,.T.);
#95763=ADVANCED_FACE('',(#10790),#7021,.F.);
#95764=ADVANCED_FACE('',(#10791),#296,.F.);
#95765=ADVANCED_FACE('',(#10792),#7022,.F.);
#95766=ADVANCED_FACE('',(#10793),#297,.T.);
#95767=ADVANCED_FACE('',(#10794),#7023,.F.);
#95768=ADVANCED_FACE('',(#10795),#6122,.F.);
#95769=ADVANCED_FACE('',(#10796),#6123,.F.);
#95770=ADVANCED_FACE('',(#10797),#6124,.T.);
#95771=ADVANCED_FACE('',(#10798),#6125,.T.);
#95772=ADVANCED_FACE('',(#10799),#7024,.F.);
#95773=ADVANCED_FACE('',(#10800),#298,.F.);
#95774=ADVANCED_FACE('',(#10801),#7025,.F.);
#95775=ADVANCED_FACE('',(#10802),#299,.T.);
#95776=ADVANCED_FACE('',(#10803),#7026,.F.);
#95777=ADVANCED_FACE('',(#10804),#6126,.F.);
#95778=ADVANCED_FACE('',(#10805),#6127,.F.);
#95779=ADVANCED_FACE('',(#10806),#6128,.T.);
#95780=ADVANCED_FACE('',(#10807),#6129,.T.);
#95781=ADVANCED_FACE('',(#10808),#7027,.F.);
#95782=ADVANCED_FACE('',(#10809),#300,.F.);
#95783=ADVANCED_FACE('',(#10810),#7028,.F.);
#95784=ADVANCED_FACE('',(#10811),#301,.T.);
#95785=ADVANCED_FACE('',(#10812),#7029,.F.);
#95786=ADVANCED_FACE('',(#10813),#6130,.F.);
#95787=ADVANCED_FACE('',(#10814),#6131,.F.);
#95788=ADVANCED_FACE('',(#10815),#6132,.T.);
#95789=ADVANCED_FACE('',(#10816),#6133,.T.);
#95790=ADVANCED_FACE('',(#10817),#7030,.F.);
#95791=ADVANCED_FACE('',(#10818),#302,.F.);
#95792=ADVANCED_FACE('',(#10819),#7031,.F.);
#95793=ADVANCED_FACE('',(#10820),#303,.T.);
#95794=ADVANCED_FACE('',(#10821),#7032,.F.);
#95795=ADVANCED_FACE('',(#10822),#6134,.F.);
#95796=ADVANCED_FACE('',(#10823),#6135,.F.);
#95797=ADVANCED_FACE('',(#10824),#6136,.T.);
#95798=ADVANCED_FACE('',(#10825),#6137,.T.);
#95799=ADVANCED_FACE('',(#10826),#7033,.F.);
#95800=ADVANCED_FACE('',(#10827),#304,.F.);
#95801=ADVANCED_FACE('',(#10828),#7034,.F.);
#95802=ADVANCED_FACE('',(#10829),#305,.T.);
#95803=ADVANCED_FACE('',(#10830),#7035,.F.);
#95804=ADVANCED_FACE('',(#10831),#6138,.F.);
#95805=ADVANCED_FACE('',(#10832),#6139,.F.);
#95806=ADVANCED_FACE('',(#10833),#6140,.T.);
#95807=ADVANCED_FACE('',(#10834),#6141,.T.);
#95808=ADVANCED_FACE('',(#10835),#7036,.F.);
#95809=ADVANCED_FACE('',(#10836),#306,.F.);
#95810=ADVANCED_FACE('',(#10837),#7037,.F.);
#95811=ADVANCED_FACE('',(#10838),#307,.T.);
#95812=ADVANCED_FACE('',(#10839),#7038,.F.);
#95813=ADVANCED_FACE('',(#10840),#6142,.F.);
#95814=ADVANCED_FACE('',(#10841),#6143,.F.);
#95815=ADVANCED_FACE('',(#10842),#6144,.T.);
#95816=ADVANCED_FACE('',(#10843),#6145,.T.);
#95817=ADVANCED_FACE('',(#10844),#7039,.F.);
#95818=ADVANCED_FACE('',(#10845),#308,.F.);
#95819=ADVANCED_FACE('',(#10846),#7040,.F.);
#95820=ADVANCED_FACE('',(#10847),#309,.T.);
#95821=ADVANCED_FACE('',(#10848),#7041,.F.);
#95822=ADVANCED_FACE('',(#10849),#6146,.F.);
#95823=ADVANCED_FACE('',(#10850),#6147,.F.);
#95824=ADVANCED_FACE('',(#10851),#6148,.T.);
#95825=ADVANCED_FACE('',(#10852),#6149,.T.);
#95826=ADVANCED_FACE('',(#10853,#6369),#7042,.F.);
#95827=ADVANCED_FACE('',(#10854),#7043,.F.);
#95828=ADVANCED_FACE('',(#10855),#310,.F.);
#95829=ADVANCED_FACE('',(#10856),#7044,.F.);
#95830=ADVANCED_FACE('',(#10857),#311,.T.);
#95831=ADVANCED_FACE('',(#10858),#7045,.F.);
#95832=ADVANCED_FACE('',(#10859,#6370),#7046,.F.);
#95833=ADVANCED_FACE('',(#10860,#6371),#7047,.F.);
#95834=ADVANCED_FACE('',(#10861),#6150,.F.);
#95835=ADVANCED_FACE('',(#10862),#6151,.F.);
#95836=ADVANCED_FACE('',(#10863),#6152,.T.);
#95837=ADVANCED_FACE('',(#10864),#6153,.T.);
#95838=ADVANCED_FACE('',(#10865),#7048,.F.);
#95839=ADVANCED_FACE('',(#10866),#7049,.T.);
#95840=ADVANCED_FACE('',(#10867),#7050,.F.);
#95841=ADVANCED_FACE('',(#10868),#91329,.T.);
#95842=ADVANCED_FACE('',(#10869),#91330,.T.);
#95843=ADVANCED_FACE('',(#10870),#91331,.F.);
#95844=ADVANCED_FACE('',(#10871),#3226,.F.);
#95845=ADVANCED_FACE('',(#10872),#91332,.F.);
#95846=ADVANCED_FACE('',(#10873),#91333,.F.);
#95847=ADVANCED_FACE('',(#10874),#3227,.F.);
#95848=ADVANCED_FACE('',(#10875),#3228,.F.);
#95849=ADVANCED_FACE('',(#10876),#91334,.F.);
#95850=ADVANCED_FACE('',(#10877),#91335,.F.);
#95851=ADVANCED_FACE('',(#10878),#3229,.F.);
#95852=ADVANCED_FACE('',(#10879),#91336,.F.);
#95853=ADVANCED_FACE('',(#10880),#6154,.F.);
#95854=ADVANCED_FACE('',(#10881),#3230,.F.);
#95855=ADVANCED_FACE('',(#10882),#3231,.F.);
#95856=ADVANCED_FACE('',(#10883),#91337,.F.);
#95857=ADVANCED_FACE('',(#10884),#91338,.F.);
#95858=ADVANCED_FACE('',(#10885),#3232,.F.);
#95859=ADVANCED_FACE('',(#10886),#3233,.F.);
#95860=ADVANCED_FACE('',(#10887),#6155,.F.);
#95861=ADVANCED_FACE('',(#10888),#91339,.F.);
#95862=ADVANCED_FACE('',(#10889),#3234,.F.);
#95863=ADVANCED_FACE('',(#10890),#91340,.F.);
#95864=ADVANCED_FACE('',(#10891),#91341,.F.);
#95865=ADVANCED_FACE('',(#10892),#3235,.F.);
#95866=ADVANCED_FACE('',(#10893),#3236,.F.);
#95867=ADVANCED_FACE('',(#10894),#91342,.F.);
#95868=ADVANCED_FACE('',(#10895),#91343,.F.);
#95869=ADVANCED_FACE('',(#10896),#3237,.F.);
#95870=ADVANCED_FACE('',(#10897),#91344,.F.);
#95871=ADVANCED_FACE('',(#10898),#7051,.F.);
#95872=ADVANCED_FACE('',(#10899),#7052,.T.);
#95873=ADVANCED_FACE('',(#10900),#7053,.F.);
#95874=ADVANCED_FACE('',(#10901),#7054,.F.);
#95875=ADVANCED_FACE('',(#10902),#7055,.T.);
#95876=ADVANCED_FACE('',(#10903),#7056,.F.);
#95877=ADVANCED_FACE('',(#10904),#7057,.F.);
#95878=ADVANCED_FACE('',(#10905),#7058,.T.);
#95879=ADVANCED_FACE('',(#10906),#7059,.F.);
#95880=ADVANCED_FACE('',(#10907),#7060,.F.);
#95881=ADVANCED_FACE('',(#10908),#7061,.T.);
#95882=ADVANCED_FACE('',(#10909),#7062,.F.);
#95883=ADVANCED_FACE('',(#10910),#7063,.F.);
#95884=ADVANCED_FACE('',(#10911),#7064,.T.);
#95885=ADVANCED_FACE('',(#10912),#7065,.F.);
#95886=ADVANCED_FACE('',(#10913),#7066,.F.);
#95887=ADVANCED_FACE('',(#10914),#7067,.T.);
#95888=ADVANCED_FACE('',(#10915),#7068,.F.);
#95889=ADVANCED_FACE('',(#10916),#7069,.F.);
#95890=ADVANCED_FACE('',(#10917),#7070,.T.);
#95891=ADVANCED_FACE('',(#10918),#7071,.F.);
#95892=ADVANCED_FACE('',(#10919),#7072,.F.);
#95893=ADVANCED_FACE('',(#10920),#7073,.T.);
#95894=ADVANCED_FACE('',(#10921),#7074,.F.);
#95895=ADVANCED_FACE('',(#10922),#7075,.F.);
#95896=ADVANCED_FACE('',(#10923),#7076,.T.);
#95897=ADVANCED_FACE('',(#10924),#7077,.F.);
#95898=ADVANCED_FACE('',(#10925),#7078,.F.);
#95899=ADVANCED_FACE('',(#10926),#7079,.T.);
#95900=ADVANCED_FACE('',(#10927),#7080,.F.);
#95901=ADVANCED_FACE('',(#10928),#7081,.F.);
#95902=ADVANCED_FACE('',(#10929),#7082,.T.);
#95903=ADVANCED_FACE('',(#10930),#7083,.F.);
#95904=ADVANCED_FACE('',(#10931),#7084,.F.);
#95905=ADVANCED_FACE('',(#10932),#7085,.T.);
#95906=ADVANCED_FACE('',(#10933),#7086,.F.);
#95907=ADVANCED_FACE('',(#10934),#7087,.F.);
#95908=ADVANCED_FACE('',(#10935),#7088,.T.);
#95909=ADVANCED_FACE('',(#10936),#7089,.F.);
#95910=ADVANCED_FACE('',(#10937),#7090,.F.);
#95911=ADVANCED_FACE('',(#10938),#7091,.T.);
#95912=ADVANCED_FACE('',(#10939),#7092,.F.);
#95913=ADVANCED_FACE('',(#10940),#7093,.F.);
#95914=ADVANCED_FACE('',(#10941),#7094,.T.);
#95915=ADVANCED_FACE('',(#10942),#7095,.F.);
#95916=ADVANCED_FACE('',(#10943),#7096,.F.);
#95917=ADVANCED_FACE('',(#10944),#7097,.T.);
#95918=ADVANCED_FACE('',(#10945),#7098,.F.);
#95919=ADVANCED_FACE('',(#10946),#7099,.F.);
#95920=ADVANCED_FACE('',(#10947),#7100,.T.);
#95921=ADVANCED_FACE('',(#10948),#7101,.F.);
#95922=ADVANCED_FACE('',(#10949),#7102,.F.);
#95923=ADVANCED_FACE('',(#10950),#7103,.T.);
#95924=ADVANCED_FACE('',(#10951),#7104,.F.);
#95925=ADVANCED_FACE('',(#10952),#7105,.F.);
#95926=ADVANCED_FACE('',(#10953),#7106,.T.);
#95927=ADVANCED_FACE('',(#10954),#7107,.F.);
#95928=ADVANCED_FACE('',(#10955),#7108,.F.);
#95929=ADVANCED_FACE('',(#10956),#7109,.T.);
#95930=ADVANCED_FACE('',(#10957),#7110,.F.);
#95931=ADVANCED_FACE('',(#10958),#7111,.F.);
#95932=ADVANCED_FACE('',(#10959),#7112,.T.);
#95933=ADVANCED_FACE('',(#10960),#7113,.F.);
#95934=ADVANCED_FACE('',(#10961),#7114,.F.);
#95935=ADVANCED_FACE('',(#10962),#7115,.T.);
#95936=ADVANCED_FACE('',(#10963),#7116,.F.);
#95937=ADVANCED_FACE('',(#10964),#7117,.F.);
#95938=ADVANCED_FACE('',(#10965),#7118,.T.);
#95939=ADVANCED_FACE('',(#10966),#7119,.F.);
#95940=ADVANCED_FACE('',(#10967),#7120,.F.);
#95941=ADVANCED_FACE('',(#10968),#7121,.T.);
#95942=ADVANCED_FACE('',(#10969),#7122,.F.);
#95943=ADVANCED_FACE('',(#10970),#7123,.F.);
#95944=ADVANCED_FACE('',(#10971),#7124,.T.);
#95945=ADVANCED_FACE('',(#10972),#7125,.F.);
#95946=ADVANCED_FACE('',(#10973),#7126,.F.);
#95947=ADVANCED_FACE('',(#10974),#7127,.T.);
#95948=ADVANCED_FACE('',(#10975),#7128,.F.);
#95949=ADVANCED_FACE('',(#10976),#7129,.F.);
#95950=ADVANCED_FACE('',(#10977),#7130,.T.);
#95951=ADVANCED_FACE('',(#10978),#7131,.F.);
#95952=ADVANCED_FACE('',(#10979),#7132,.F.);
#95953=ADVANCED_FACE('',(#10980),#7133,.T.);
#95954=ADVANCED_FACE('',(#10981),#7134,.F.);
#95955=ADVANCED_FACE('',(#10982),#7135,.F.);
#95956=ADVANCED_FACE('',(#10983),#7136,.T.);
#95957=ADVANCED_FACE('',(#10984),#7137,.F.);
#95958=ADVANCED_FACE('',(#10985),#7138,.F.);
#95959=ADVANCED_FACE('',(#10986),#7139,.T.);
#95960=ADVANCED_FACE('',(#10987),#7140,.F.);
#95961=ADVANCED_FACE('',(#10988),#7141,.F.);
#95962=ADVANCED_FACE('',(#10989),#7142,.T.);
#95963=ADVANCED_FACE('',(#10990),#7143,.F.);
#95964=ADVANCED_FACE('',(#10991),#7144,.F.);
#95965=ADVANCED_FACE('',(#10992),#7145,.T.);
#95966=ADVANCED_FACE('',(#10993),#7146,.F.);
#95967=ADVANCED_FACE('',(#10994),#7147,.F.);
#95968=ADVANCED_FACE('',(#10995),#7148,.T.);
#95969=ADVANCED_FACE('',(#10996),#7149,.F.);
#95970=ADVANCED_FACE('',(#10997),#7150,.F.);
#95971=ADVANCED_FACE('',(#10998),#7151,.T.);
#95972=ADVANCED_FACE('',(#10999),#7152,.F.);
#95973=ADVANCED_FACE('',(#11000),#7153,.F.);
#95974=ADVANCED_FACE('',(#11001),#7154,.T.);
#95975=ADVANCED_FACE('',(#11002),#7155,.F.);
#95976=ADVANCED_FACE('',(#11003),#7156,.F.);
#95977=ADVANCED_FACE('',(#11004),#7157,.T.);
#95978=ADVANCED_FACE('',(#11005),#7158,.F.);
#95979=ADVANCED_FACE('',(#11006),#7159,.F.);
#95980=ADVANCED_FACE('',(#11007),#7160,.T.);
#95981=ADVANCED_FACE('',(#11008),#7161,.F.);
#95982=ADVANCED_FACE('',(#11009),#7162,.F.);
#95983=ADVANCED_FACE('',(#11010),#7163,.T.);
#95984=ADVANCED_FACE('',(#11011),#7164,.F.);
#95985=ADVANCED_FACE('',(#11012),#7165,.F.);
#95986=ADVANCED_FACE('',(#11013),#7166,.T.);
#95987=ADVANCED_FACE('',(#11014),#7167,.F.);
#95988=ADVANCED_FACE('',(#11015),#7168,.F.);
#95989=ADVANCED_FACE('',(#11016),#7169,.T.);
#95990=ADVANCED_FACE('',(#11017),#7170,.F.);
#95991=ADVANCED_FACE('',(#11018),#7171,.F.);
#95992=ADVANCED_FACE('',(#11019),#7172,.T.);
#95993=ADVANCED_FACE('',(#11020),#7173,.F.);
#95994=ADVANCED_FACE('',(#11021),#7174,.F.);
#95995=ADVANCED_FACE('',(#11022),#7175,.T.);
#95996=ADVANCED_FACE('',(#11023),#7176,.F.);
#95997=ADVANCED_FACE('',(#11024),#7177,.F.);
#95998=ADVANCED_FACE('',(#11025),#7178,.T.);
#95999=ADVANCED_FACE('',(#11026),#7179,.F.);
#96000=ADVANCED_FACE('',(#11027),#7180,.F.);
#96001=ADVANCED_FACE('',(#11028),#7181,.T.);
#96002=ADVANCED_FACE('',(#11029),#7182,.F.);
#96003=ADVANCED_FACE('',(#11030),#7183,.F.);
#96004=ADVANCED_FACE('',(#11031),#7184,.T.);
#96005=ADVANCED_FACE('',(#11032),#7185,.F.);
#96006=ADVANCED_FACE('',(#11033),#7186,.F.);
#96007=ADVANCED_FACE('',(#11034),#7187,.T.);
#96008=ADVANCED_FACE('',(#11035),#7188,.F.);
#96009=ADVANCED_FACE('',(#11036),#7189,.F.);
#96010=ADVANCED_FACE('',(#11037),#7190,.T.);
#96011=ADVANCED_FACE('',(#11038),#7191,.F.);
#96012=ADVANCED_FACE('',(#11039),#7192,.F.);
#96013=ADVANCED_FACE('',(#11040),#7193,.T.);
#96014=ADVANCED_FACE('',(#11041),#7194,.F.);
#96015=ADVANCED_FACE('',(#11042),#7195,.F.);
#96016=ADVANCED_FACE('',(#11043),#7196,.T.);
#96017=ADVANCED_FACE('',(#11044),#7197,.F.);
#96018=ADVANCED_FACE('',(#11045),#7198,.F.);
#96019=ADVANCED_FACE('',(#11046),#7199,.T.);
#96020=ADVANCED_FACE('',(#11047),#7200,.F.);
#96021=ADVANCED_FACE('',(#11048),#7201,.F.);
#96022=ADVANCED_FACE('',(#11049),#7202,.T.);
#96023=ADVANCED_FACE('',(#11050),#7203,.F.);
#96024=ADVANCED_FACE('',(#11051),#7204,.F.);
#96025=ADVANCED_FACE('',(#11052),#7205,.T.);
#96026=ADVANCED_FACE('',(#11053),#7206,.F.);
#96027=ADVANCED_FACE('',(#11054),#7207,.F.);
#96028=ADVANCED_FACE('',(#11055),#7208,.T.);
#96029=ADVANCED_FACE('',(#11056),#7209,.F.);
#96030=ADVANCED_FACE('',(#11057),#7210,.F.);
#96031=ADVANCED_FACE('',(#11058),#7211,.T.);
#96032=ADVANCED_FACE('',(#11059),#7212,.F.);
#96033=ADVANCED_FACE('',(#11060),#7213,.F.);
#96034=ADVANCED_FACE('',(#11061),#7214,.T.);
#96035=ADVANCED_FACE('',(#11062),#7215,.F.);
#96036=ADVANCED_FACE('',(#11063),#7216,.F.);
#96037=ADVANCED_FACE('',(#11064),#7217,.T.);
#96038=ADVANCED_FACE('',(#11065),#7218,.F.);
#96039=ADVANCED_FACE('',(#11066),#7219,.F.);
#96040=ADVANCED_FACE('',(#11067),#7220,.T.);
#96041=ADVANCED_FACE('',(#11068),#7221,.F.);
#96042=ADVANCED_FACE('',(#11069),#7222,.F.);
#96043=ADVANCED_FACE('',(#11070),#7223,.T.);
#96044=ADVANCED_FACE('',(#11071),#7224,.F.);
#96045=ADVANCED_FACE('',(#11072),#7225,.F.);
#96046=ADVANCED_FACE('',(#11073),#7226,.T.);
#96047=ADVANCED_FACE('',(#11074),#7227,.F.);
#96048=ADVANCED_FACE('',(#11075),#91345,.T.);
#96049=ADVANCED_FACE('',(#11076),#91346,.T.);
#96050=ADVANCED_FACE('',(#11077),#91347,.T.);
#96051=ADVANCED_FACE('',(#11078),#91348,.T.);
#96052=ADVANCED_FACE('',(#11079),#91349,.T.);
#96053=ADVANCED_FACE('',(#11080),#91350,.T.);
#96054=ADVANCED_FACE('',(#11081),#91351,.T.);
#96055=ADVANCED_FACE('',(#11082),#91352,.T.);
#96056=ADVANCED_FACE('',(#11083),#91353,.T.);
#96057=ADVANCED_FACE('',(#11084),#91354,.T.);
#96058=ADVANCED_FACE('',(#11085),#91355,.T.);
#96059=ADVANCED_FACE('',(#11086),#91356,.T.);
#96060=ADVANCED_FACE('',(#11087),#91357,.T.);
#96061=ADVANCED_FACE('',(#11088),#91358,.T.);
#96062=ADVANCED_FACE('',(#11089),#91359,.T.);
#96063=ADVANCED_FACE('',(#11090),#91360,.T.);
#96064=ADVANCED_FACE('',(#11091),#91361,.T.);
#96065=ADVANCED_FACE('',(#11092),#91362,.T.);
#96066=ADVANCED_FACE('',(#11093),#91363,.T.);
#96067=ADVANCED_FACE('',(#11094),#91364,.T.);
#96068=ADVANCED_FACE('',(#11095),#91365,.T.);
#96069=ADVANCED_FACE('',(#11096),#91366,.T.);
#96070=ADVANCED_FACE('',(#11097),#91367,.T.);
#96071=ADVANCED_FACE('',(#11098),#91368,.T.);
#96072=ADVANCED_FACE('',(#11099),#91369,.T.);
#96073=ADVANCED_FACE('',(#11100),#91370,.T.);
#96074=ADVANCED_FACE('',(#11101),#91371,.T.);
#96075=ADVANCED_FACE('',(#11102),#91372,.T.);
#96076=ADVANCED_FACE('',(#11103),#91373,.T.);
#96077=ADVANCED_FACE('',(#11104),#91374,.T.);
#96078=ADVANCED_FACE('',(#11105),#91375,.T.);
#96079=ADVANCED_FACE('',(#11106),#91376,.T.);
#96080=ADVANCED_FACE('',(#11107),#91377,.T.);
#96081=ADVANCED_FACE('',(#11108),#91378,.T.);
#96082=ADVANCED_FACE('',(#11109),#91379,.T.);
#96083=ADVANCED_FACE('',(#11110),#91380,.T.);
#96084=ADVANCED_FACE('',(#11111),#91381,.T.);
#96085=ADVANCED_FACE('',(#11112),#91382,.T.);
#96086=ADVANCED_FACE('',(#11113),#91383,.T.);
#96087=ADVANCED_FACE('',(#11114),#91384,.T.);
#96088=ADVANCED_FACE('',(#11115),#91385,.T.);
#96089=ADVANCED_FACE('',(#11116),#91386,.T.);
#96090=ADVANCED_FACE('',(#11117),#91387,.T.);
#96091=ADVANCED_FACE('',(#11118),#91388,.T.);
#96092=ADVANCED_FACE('',(#11119),#91389,.T.);
#96093=ADVANCED_FACE('',(#11120),#91390,.T.);
#96094=ADVANCED_FACE('',(#11121),#91391,.T.);
#96095=ADVANCED_FACE('',(#11122),#91392,.T.);
#96096=ADVANCED_FACE('',(#11123),#91393,.T.);
#96097=ADVANCED_FACE('',(#11124),#91394,.T.);
#96098=ADVANCED_FACE('',(#11125),#91395,.T.);
#96099=ADVANCED_FACE('',(#11126),#91396,.T.);
#96100=ADVANCED_FACE('',(#11127),#91397,.T.);
#96101=ADVANCED_FACE('',(#11128),#91398,.T.);
#96102=ADVANCED_FACE('',(#11129),#91399,.T.);
#96103=ADVANCED_FACE('',(#11130),#91400,.T.);
#96104=ADVANCED_FACE('',(#11131),#91401,.T.);
#96105=ADVANCED_FACE('',(#11132),#91402,.T.);
#96106=ADVANCED_FACE('',(#11133),#91403,.T.);
#96107=ADVANCED_FACE('',(#11134),#91404,.T.);
#96108=ADVANCED_FACE('',(#11135),#91405,.T.);
#96109=ADVANCED_FACE('',(#11136),#91406,.T.);
#96110=ADVANCED_FACE('',(#11137),#91407,.T.);
#96111=ADVANCED_FACE('',(#11138),#91408,.T.);
#96112=ADVANCED_FACE('',(#11139),#91409,.T.);
#96113=ADVANCED_FACE('',(#11140),#91410,.T.);
#96114=ADVANCED_FACE('',(#11141),#91411,.T.);
#96115=ADVANCED_FACE('',(#11142),#91412,.T.);
#96116=ADVANCED_FACE('',(#11143),#91413,.T.);
#96117=ADVANCED_FACE('',(#11144),#91414,.T.);
#96118=ADVANCED_FACE('',(#11145),#91415,.T.);
#96119=ADVANCED_FACE('',(#11146),#91416,.T.);
#96120=ADVANCED_FACE('',(#11147),#91417,.T.);
#96121=ADVANCED_FACE('',(#11148),#91418,.T.);
#96122=ADVANCED_FACE('',(#11149),#91419,.T.);
#96123=ADVANCED_FACE('',(#11150),#91420,.T.);
#96124=ADVANCED_FACE('',(#11151),#91421,.T.);
#96125=ADVANCED_FACE('',(#11152),#91422,.T.);
#96126=ADVANCED_FACE('',(#11153),#91423,.T.);
#96127=ADVANCED_FACE('',(#11154),#91424,.T.);
#96128=ADVANCED_FACE('',(#11155),#91425,.T.);
#96129=ADVANCED_FACE('',(#11156),#91426,.T.);
#96130=ADVANCED_FACE('',(#11157),#91427,.T.);
#96131=ADVANCED_FACE('',(#11158),#91428,.T.);
#96132=ADVANCED_FACE('',(#11159),#91429,.T.);
#96133=ADVANCED_FACE('',(#11160),#91430,.T.);
#96134=ADVANCED_FACE('',(#11161),#91431,.T.);
#96135=ADVANCED_FACE('',(#11162),#91432,.T.);
#96136=ADVANCED_FACE('',(#11163),#91433,.T.);
#96137=ADVANCED_FACE('',(#11164),#91434,.T.);
#96138=ADVANCED_FACE('',(#11165),#91435,.T.);
#96139=ADVANCED_FACE('',(#11166),#91436,.T.);
#96140=ADVANCED_FACE('',(#11167),#91437,.T.);
#96141=ADVANCED_FACE('',(#11168),#91438,.T.);
#96142=ADVANCED_FACE('',(#11169),#91439,.T.);
#96143=ADVANCED_FACE('',(#11170),#91440,.T.);
#96144=ADVANCED_FACE('',(#11171),#91441,.T.);
#96145=ADVANCED_FACE('',(#11172),#91442,.T.);
#96146=ADVANCED_FACE('',(#11173),#91443,.T.);
#96147=ADVANCED_FACE('',(#11174),#91444,.T.);
#96148=ADVANCED_FACE('',(#11175),#91445,.T.);
#96149=ADVANCED_FACE('',(#11176),#91446,.T.);
#96150=ADVANCED_FACE('',(#11177),#91447,.T.);
#96151=ADVANCED_FACE('',(#11178),#91448,.T.);
#96152=ADVANCED_FACE('',(#11179),#91449,.T.);
#96153=ADVANCED_FACE('',(#11180),#91450,.T.);
#96154=ADVANCED_FACE('',(#11181),#91451,.T.);
#96155=ADVANCED_FACE('',(#11182),#91452,.T.);
#96156=ADVANCED_FACE('',(#11183),#91453,.T.);
#96157=ADVANCED_FACE('',(#11184),#91454,.T.);
#96158=ADVANCED_FACE('',(#11185),#91455,.T.);
#96159=ADVANCED_FACE('',(#11186),#91456,.T.);
#96160=ADVANCED_FACE('',(#11187),#91457,.T.);
#96161=ADVANCED_FACE('',(#11188),#91458,.T.);
#96162=ADVANCED_FACE('',(#11189),#91459,.T.);
#96163=ADVANCED_FACE('',(#11190),#91460,.T.);
#96164=ADVANCED_FACE('',(#11191),#91461,.T.);
#96165=ADVANCED_FACE('',(#11192),#91462,.T.);
#96166=ADVANCED_FACE('',(#11193),#91463,.F.);
#96167=ADVANCED_FACE('',(#11194),#3238,.F.);
#96168=ADVANCED_FACE('',(#11195),#91464,.F.);
#96169=ADVANCED_FACE('',(#11196),#91465,.F.);
#96170=ADVANCED_FACE('',(#11197),#3239,.F.);
#96171=ADVANCED_FACE('',(#11198),#3240,.F.);
#96172=ADVANCED_FACE('',(#11199),#91466,.F.);
#96173=ADVANCED_FACE('',(#11200),#91467,.F.);
#96174=ADVANCED_FACE('',(#11201),#3241,.F.);
#96175=ADVANCED_FACE('',(#11202),#91468,.F.);
#96176=ADVANCED_FACE('',(#11203),#6156,.F.);
#96177=ADVANCED_FACE('',(#11204),#3242,.F.);
#96178=ADVANCED_FACE('',(#11205),#3243,.F.);
#96179=ADVANCED_FACE('',(#11206),#91469,.F.);
#96180=ADVANCED_FACE('',(#11207),#91470,.F.);
#96181=ADVANCED_FACE('',(#11208),#3244,.F.);
#96182=ADVANCED_FACE('',(#11209),#3245,.F.);
#96183=ADVANCED_FACE('',(#11210),#6157,.F.);
#96184=ADVANCED_FACE('',(#11211),#91471,.F.);
#96185=ADVANCED_FACE('',(#11212),#3246,.F.);
#96186=ADVANCED_FACE('',(#11213),#91472,.F.);
#96187=ADVANCED_FACE('',(#11214),#91473,.F.);
#96188=ADVANCED_FACE('',(#11215),#3247,.F.);
#96189=ADVANCED_FACE('',(#11216),#3248,.F.);
#96190=ADVANCED_FACE('',(#11217),#91474,.F.);
#96191=ADVANCED_FACE('',(#11218),#91475,.F.);
#96192=ADVANCED_FACE('',(#11219),#3249,.F.);
#96193=ADVANCED_FACE('',(#11220),#91476,.F.);
#96194=ADVANCED_FACE('',(#11221),#91477,.F.);
#96195=ADVANCED_FACE('',(#11222),#3250,.F.);
#96196=ADVANCED_FACE('',(#11223),#91478,.F.);
#96197=ADVANCED_FACE('',(#11224),#91479,.F.);
#96198=ADVANCED_FACE('',(#11225),#3251,.F.);
#96199=ADVANCED_FACE('',(#11226),#3252,.F.);
#96200=ADVANCED_FACE('',(#11227),#91480,.F.);
#96201=ADVANCED_FACE('',(#11228),#91481,.F.);
#96202=ADVANCED_FACE('',(#11229),#3253,.F.);
#96203=ADVANCED_FACE('',(#11230),#91482,.F.);
#96204=ADVANCED_FACE('',(#11231),#6158,.F.);
#96205=ADVANCED_FACE('',(#11232),#3254,.F.);
#96206=ADVANCED_FACE('',(#11233),#3255,.F.);
#96207=ADVANCED_FACE('',(#11234),#91483,.F.);
#96208=ADVANCED_FACE('',(#11235),#91484,.F.);
#96209=ADVANCED_FACE('',(#11236),#3256,.F.);
#96210=ADVANCED_FACE('',(#11237),#3257,.F.);
#96211=ADVANCED_FACE('',(#11238),#6159,.F.);
#96212=ADVANCED_FACE('',(#11239),#91485,.F.);
#96213=ADVANCED_FACE('',(#11240),#3258,.F.);
#96214=ADVANCED_FACE('',(#11241),#91486,.F.);
#96215=ADVANCED_FACE('',(#11242),#91487,.F.);
#96216=ADVANCED_FACE('',(#11243),#3259,.F.);
#96217=ADVANCED_FACE('',(#11244),#3260,.F.);
#96218=ADVANCED_FACE('',(#11245),#91488,.F.);
#96219=ADVANCED_FACE('',(#11246),#91489,.F.);
#96220=ADVANCED_FACE('',(#11247),#3261,.F.);
#96221=ADVANCED_FACE('',(#11248),#91490,.F.);
#96222=ADVANCED_FACE('',(#11249),#91491,.F.);
#96223=ADVANCED_FACE('',(#11250),#3262,.F.);
#96224=ADVANCED_FACE('',(#11251),#91492,.F.);
#96225=ADVANCED_FACE('',(#11252),#91493,.F.);
#96226=ADVANCED_FACE('',(#11253),#3263,.F.);
#96227=ADVANCED_FACE('',(#11254),#3264,.F.);
#96228=ADVANCED_FACE('',(#11255),#91494,.F.);
#96229=ADVANCED_FACE('',(#11256),#91495,.F.);
#96230=ADVANCED_FACE('',(#11257),#3265,.F.);
#96231=ADVANCED_FACE('',(#11258),#91496,.F.);
#96232=ADVANCED_FACE('',(#11259),#6160,.F.);
#96233=ADVANCED_FACE('',(#11260),#3266,.F.);
#96234=ADVANCED_FACE('',(#11261),#3267,.F.);
#96235=ADVANCED_FACE('',(#11262),#91497,.F.);
#96236=ADVANCED_FACE('',(#11263),#91498,.F.);
#96237=ADVANCED_FACE('',(#11264),#3268,.F.);
#96238=ADVANCED_FACE('',(#11265),#3269,.F.);
#96239=ADVANCED_FACE('',(#11266),#6161,.F.);
#96240=ADVANCED_FACE('',(#11267),#91499,.F.);
#96241=ADVANCED_FACE('',(#11268),#3270,.F.);
#96242=ADVANCED_FACE('',(#11269),#91500,.F.);
#96243=ADVANCED_FACE('',(#11270),#91501,.F.);
#96244=ADVANCED_FACE('',(#11271),#3271,.F.);
#96245=ADVANCED_FACE('',(#11272),#3272,.F.);
#96246=ADVANCED_FACE('',(#11273),#91502,.F.);
#96247=ADVANCED_FACE('',(#11274),#91503,.F.);
#96248=ADVANCED_FACE('',(#11275),#3273,.F.);
#96249=ADVANCED_FACE('',(#11276),#91504,.F.);
#96250=ADVANCED_FACE('',(#11277),#91505,.F.);
#96251=ADVANCED_FACE('',(#11278),#3274,.F.);
#96252=ADVANCED_FACE('',(#11279),#91506,.F.);
#96253=ADVANCED_FACE('',(#11280),#91507,.F.);
#96254=ADVANCED_FACE('',(#11281),#3275,.F.);
#96255=ADVANCED_FACE('',(#11282),#3276,.F.);
#96256=ADVANCED_FACE('',(#11283),#91508,.F.);
#96257=ADVANCED_FACE('',(#11284),#91509,.F.);
#96258=ADVANCED_FACE('',(#11285),#3277,.F.);
#96259=ADVANCED_FACE('',(#11286),#91510,.F.);
#96260=ADVANCED_FACE('',(#11287),#6162,.F.);
#96261=ADVANCED_FACE('',(#11288),#3278,.F.);
#96262=ADVANCED_FACE('',(#11289),#3279,.F.);
#96263=ADVANCED_FACE('',(#11290),#91511,.F.);
#96264=ADVANCED_FACE('',(#11291),#91512,.F.);
#96265=ADVANCED_FACE('',(#11292),#3280,.F.);
#96266=ADVANCED_FACE('',(#11293),#3281,.F.);
#96267=ADVANCED_FACE('',(#11294),#6163,.F.);
#96268=ADVANCED_FACE('',(#11295),#91513,.F.);
#96269=ADVANCED_FACE('',(#11296),#3282,.F.);
#96270=ADVANCED_FACE('',(#11297),#91514,.F.);
#96271=ADVANCED_FACE('',(#11298),#91515,.F.);
#96272=ADVANCED_FACE('',(#11299),#3283,.F.);
#96273=ADVANCED_FACE('',(#11300),#3284,.F.);
#96274=ADVANCED_FACE('',(#11301),#91516,.F.);
#96275=ADVANCED_FACE('',(#11302),#91517,.F.);
#96276=ADVANCED_FACE('',(#11303),#3285,.F.);
#96277=ADVANCED_FACE('',(#11304),#91518,.F.);
#96278=ADVANCED_FACE('',(#11305),#91519,.F.);
#96279=ADVANCED_FACE('',(#11306),#3286,.F.);
#96280=ADVANCED_FACE('',(#11307),#91520,.F.);
#96281=ADVANCED_FACE('',(#11308),#91521,.F.);
#96282=ADVANCED_FACE('',(#11309),#3287,.F.);
#96283=ADVANCED_FACE('',(#11310),#3288,.F.);
#96284=ADVANCED_FACE('',(#11311),#91522,.F.);
#96285=ADVANCED_FACE('',(#11312),#91523,.F.);
#96286=ADVANCED_FACE('',(#11313),#3289,.F.);
#96287=ADVANCED_FACE('',(#11314),#91524,.F.);
#96288=ADVANCED_FACE('',(#11315),#6164,.F.);
#96289=ADVANCED_FACE('',(#11316),#3290,.F.);
#96290=ADVANCED_FACE('',(#11317),#3291,.F.);
#96291=ADVANCED_FACE('',(#11318),#91525,.F.);
#96292=ADVANCED_FACE('',(#11319),#91526,.F.);
#96293=ADVANCED_FACE('',(#11320),#3292,.F.);
#96294=ADVANCED_FACE('',(#11321),#3293,.F.);
#96295=ADVANCED_FACE('',(#11322),#6165,.F.);
#96296=ADVANCED_FACE('',(#11323),#91527,.F.);
#96297=ADVANCED_FACE('',(#11324),#3294,.F.);
#96298=ADVANCED_FACE('',(#11325),#91528,.F.);
#96299=ADVANCED_FACE('',(#11326),#91529,.F.);
#96300=ADVANCED_FACE('',(#11327),#3295,.F.);
#96301=ADVANCED_FACE('',(#11328),#3296,.F.);
#96302=ADVANCED_FACE('',(#11329),#91530,.F.);
#96303=ADVANCED_FACE('',(#11330),#91531,.F.);
#96304=ADVANCED_FACE('',(#11331),#3297,.F.);
#96305=ADVANCED_FACE('',(#11332),#91532,.F.);
#96306=ADVANCED_FACE('',(#11333),#91533,.F.);
#96307=ADVANCED_FACE('',(#11334),#3298,.F.);
#96308=ADVANCED_FACE('',(#11335),#91534,.F.);
#96309=ADVANCED_FACE('',(#11336),#91535,.F.);
#96310=ADVANCED_FACE('',(#11337),#3299,.F.);
#96311=ADVANCED_FACE('',(#11338),#3300,.F.);
#96312=ADVANCED_FACE('',(#11339),#91536,.F.);
#96313=ADVANCED_FACE('',(#11340),#91537,.F.);
#96314=ADVANCED_FACE('',(#11341),#3301,.F.);
#96315=ADVANCED_FACE('',(#11342),#91538,.F.);
#96316=ADVANCED_FACE('',(#11343),#6166,.F.);
#96317=ADVANCED_FACE('',(#11344),#3302,.F.);
#96318=ADVANCED_FACE('',(#11345),#3303,.F.);
#96319=ADVANCED_FACE('',(#11346),#91539,.F.);
#96320=ADVANCED_FACE('',(#11347),#91540,.F.);
#96321=ADVANCED_FACE('',(#11348),#3304,.F.);
#96322=ADVANCED_FACE('',(#11349),#3305,.F.);
#96323=ADVANCED_FACE('',(#11350),#6167,.F.);
#96324=ADVANCED_FACE('',(#11351),#91541,.F.);
#96325=ADVANCED_FACE('',(#11352),#3306,.F.);
#96326=ADVANCED_FACE('',(#11353),#91542,.F.);
#96327=ADVANCED_FACE('',(#11354),#91543,.F.);
#96328=ADVANCED_FACE('',(#11355),#3307,.F.);
#96329=ADVANCED_FACE('',(#11356),#3308,.F.);
#96330=ADVANCED_FACE('',(#11357),#91544,.F.);
#96331=ADVANCED_FACE('',(#11358),#91545,.F.);
#96332=ADVANCED_FACE('',(#11359),#3309,.F.);
#96333=ADVANCED_FACE('',(#11360),#91546,.F.);
#96334=ADVANCED_FACE('',(#11361),#91547,.F.);
#96335=ADVANCED_FACE('',(#11362),#3310,.F.);
#96336=ADVANCED_FACE('',(#11363),#91548,.F.);
#96337=ADVANCED_FACE('',(#11364),#91549,.F.);
#96338=ADVANCED_FACE('',(#11365),#3311,.F.);
#96339=ADVANCED_FACE('',(#11366),#3312,.F.);
#96340=ADVANCED_FACE('',(#11367),#91550,.F.);
#96341=ADVANCED_FACE('',(#11368),#91551,.F.);
#96342=ADVANCED_FACE('',(#11369),#3313,.F.);
#96343=ADVANCED_FACE('',(#11370),#91552,.F.);
#96344=ADVANCED_FACE('',(#11371),#6168,.F.);
#96345=ADVANCED_FACE('',(#11372),#3314,.F.);
#96346=ADVANCED_FACE('',(#11373),#3315,.F.);
#96347=ADVANCED_FACE('',(#11374),#91553,.F.);
#96348=ADVANCED_FACE('',(#11375),#91554,.F.);
#96349=ADVANCED_FACE('',(#11376),#3316,.F.);
#96350=ADVANCED_FACE('',(#11377),#3317,.F.);
#96351=ADVANCED_FACE('',(#11378),#6169,.F.);
#96352=ADVANCED_FACE('',(#11379),#91555,.F.);
#96353=ADVANCED_FACE('',(#11380),#3318,.F.);
#96354=ADVANCED_FACE('',(#11381),#91556,.F.);
#96355=ADVANCED_FACE('',(#11382),#91557,.F.);
#96356=ADVANCED_FACE('',(#11383),#3319,.F.);
#96357=ADVANCED_FACE('',(#11384),#3320,.F.);
#96358=ADVANCED_FACE('',(#11385),#91558,.F.);
#96359=ADVANCED_FACE('',(#11386),#91559,.F.);
#96360=ADVANCED_FACE('',(#11387),#3321,.F.);
#96361=ADVANCED_FACE('',(#11388),#91560,.F.);
#96362=ADVANCED_FACE('',(#11389),#91561,.F.);
#96363=ADVANCED_FACE('',(#11390),#3322,.F.);
#96364=ADVANCED_FACE('',(#11391),#91562,.F.);
#96365=ADVANCED_FACE('',(#11392),#91563,.F.);
#96366=ADVANCED_FACE('',(#11393),#3323,.F.);
#96367=ADVANCED_FACE('',(#11394),#3324,.F.);
#96368=ADVANCED_FACE('',(#11395),#91564,.F.);
#96369=ADVANCED_FACE('',(#11396),#91565,.F.);
#96370=ADVANCED_FACE('',(#11397),#3325,.F.);
#96371=ADVANCED_FACE('',(#11398),#91566,.F.);
#96372=ADVANCED_FACE('',(#11399),#6170,.F.);
#96373=ADVANCED_FACE('',(#11400),#3326,.F.);
#96374=ADVANCED_FACE('',(#11401),#3327,.F.);
#96375=ADVANCED_FACE('',(#11402),#91567,.F.);
#96376=ADVANCED_FACE('',(#11403),#91568,.F.);
#96377=ADVANCED_FACE('',(#11404),#3328,.F.);
#96378=ADVANCED_FACE('',(#11405),#3329,.F.);
#96379=ADVANCED_FACE('',(#11406),#6171,.F.);
#96380=ADVANCED_FACE('',(#11407),#91569,.F.);
#96381=ADVANCED_FACE('',(#11408),#3330,.F.);
#96382=ADVANCED_FACE('',(#11409),#91570,.F.);
#96383=ADVANCED_FACE('',(#11410),#91571,.F.);
#96384=ADVANCED_FACE('',(#11411),#3331,.F.);
#96385=ADVANCED_FACE('',(#11412),#3332,.F.);
#96386=ADVANCED_FACE('',(#11413),#91572,.F.);
#96387=ADVANCED_FACE('',(#11414),#91573,.F.);
#96388=ADVANCED_FACE('',(#11415),#3333,.F.);
#96389=ADVANCED_FACE('',(#11416),#91574,.F.);
#96390=ADVANCED_FACE('',(#11417),#91575,.F.);
#96391=ADVANCED_FACE('',(#11418),#3334,.F.);
#96392=ADVANCED_FACE('',(#11419),#91576,.F.);
#96393=ADVANCED_FACE('',(#11420),#91577,.F.);
#96394=ADVANCED_FACE('',(#11421),#3335,.F.);
#96395=ADVANCED_FACE('',(#11422),#3336,.F.);
#96396=ADVANCED_FACE('',(#11423),#91578,.F.);
#96397=ADVANCED_FACE('',(#11424),#91579,.F.);
#96398=ADVANCED_FACE('',(#11425),#3337,.F.);
#96399=ADVANCED_FACE('',(#11426),#91580,.F.);
#96400=ADVANCED_FACE('',(#11427),#6172,.F.);
#96401=ADVANCED_FACE('',(#11428),#3338,.F.);
#96402=ADVANCED_FACE('',(#11429),#3339,.F.);
#96403=ADVANCED_FACE('',(#11430),#91581,.F.);
#96404=ADVANCED_FACE('',(#11431),#91582,.F.);
#96405=ADVANCED_FACE('',(#11432),#3340,.F.);
#96406=ADVANCED_FACE('',(#11433),#3341,.F.);
#96407=ADVANCED_FACE('',(#11434),#6173,.F.);
#96408=ADVANCED_FACE('',(#11435),#91583,.F.);
#96409=ADVANCED_FACE('',(#11436),#3342,.F.);
#96410=ADVANCED_FACE('',(#11437),#91584,.F.);
#96411=ADVANCED_FACE('',(#11438),#91585,.F.);
#96412=ADVANCED_FACE('',(#11439),#3343,.F.);
#96413=ADVANCED_FACE('',(#11440),#3344,.F.);
#96414=ADVANCED_FACE('',(#11441),#91586,.F.);
#96415=ADVANCED_FACE('',(#11442),#91587,.F.);
#96416=ADVANCED_FACE('',(#11443),#3345,.F.);
#96417=ADVANCED_FACE('',(#11444),#91588,.F.);
#96418=ADVANCED_FACE('',(#11445),#91589,.F.);
#96419=ADVANCED_FACE('',(#11446),#3346,.F.);
#96420=ADVANCED_FACE('',(#11447),#91590,.F.);
#96421=ADVANCED_FACE('',(#11448),#91591,.F.);
#96422=ADVANCED_FACE('',(#11449),#3347,.F.);
#96423=ADVANCED_FACE('',(#11450),#3348,.F.);
#96424=ADVANCED_FACE('',(#11451),#91592,.F.);
#96425=ADVANCED_FACE('',(#11452),#91593,.F.);
#96426=ADVANCED_FACE('',(#11453),#3349,.F.);
#96427=ADVANCED_FACE('',(#11454),#91594,.F.);
#96428=ADVANCED_FACE('',(#11455),#6174,.F.);
#96429=ADVANCED_FACE('',(#11456),#3350,.F.);
#96430=ADVANCED_FACE('',(#11457),#3351,.F.);
#96431=ADVANCED_FACE('',(#11458),#91595,.F.);
#96432=ADVANCED_FACE('',(#11459),#91596,.F.);
#96433=ADVANCED_FACE('',(#11460),#3352,.F.);
#96434=ADVANCED_FACE('',(#11461),#3353,.F.);
#96435=ADVANCED_FACE('',(#11462),#6175,.F.);
#96436=ADVANCED_FACE('',(#11463),#91597,.F.);
#96437=ADVANCED_FACE('',(#11464),#3354,.F.);
#96438=ADVANCED_FACE('',(#11465),#91598,.F.);
#96439=ADVANCED_FACE('',(#11466),#91599,.F.);
#96440=ADVANCED_FACE('',(#11467),#3355,.F.);
#96441=ADVANCED_FACE('',(#11468),#3356,.F.);
#96442=ADVANCED_FACE('',(#11469),#91600,.F.);
#96443=ADVANCED_FACE('',(#11470),#91601,.F.);
#96444=ADVANCED_FACE('',(#11471),#3357,.F.);
#96445=ADVANCED_FACE('',(#11472),#91602,.F.);
#96446=ADVANCED_FACE('',(#11473),#91603,.F.);
#96447=ADVANCED_FACE('',(#11474),#3358,.F.);
#96448=ADVANCED_FACE('',(#11475),#91604,.F.);
#96449=ADVANCED_FACE('',(#11476),#91605,.F.);
#96450=ADVANCED_FACE('',(#11477),#3359,.F.);
#96451=ADVANCED_FACE('',(#11478),#3360,.F.);
#96452=ADVANCED_FACE('',(#11479),#91606,.F.);
#96453=ADVANCED_FACE('',(#11480),#91607,.F.);
#96454=ADVANCED_FACE('',(#11481),#3361,.F.);
#96455=ADVANCED_FACE('',(#11482),#91608,.F.);
#96456=ADVANCED_FACE('',(#11483),#6176,.F.);
#96457=ADVANCED_FACE('',(#11484),#3362,.F.);
#96458=ADVANCED_FACE('',(#11485),#3363,.F.);
#96459=ADVANCED_FACE('',(#11486),#91609,.F.);
#96460=ADVANCED_FACE('',(#11487),#91610,.F.);
#96461=ADVANCED_FACE('',(#11488),#3364,.F.);
#96462=ADVANCED_FACE('',(#11489),#3365,.F.);
#96463=ADVANCED_FACE('',(#11490),#6177,.F.);
#96464=ADVANCED_FACE('',(#11491),#91611,.F.);
#96465=ADVANCED_FACE('',(#11492),#3366,.F.);
#96466=ADVANCED_FACE('',(#11493),#91612,.F.);
#96467=ADVANCED_FACE('',(#11494),#91613,.F.);
#96468=ADVANCED_FACE('',(#11495),#3367,.F.);
#96469=ADVANCED_FACE('',(#11496),#3368,.F.);
#96470=ADVANCED_FACE('',(#11497),#91614,.F.);
#96471=ADVANCED_FACE('',(#11498),#91615,.F.);
#96472=ADVANCED_FACE('',(#11499),#3369,.F.);
#96473=ADVANCED_FACE('',(#11500),#91616,.F.);
#96474=ADVANCED_FACE('',(#11501),#91617,.F.);
#96475=ADVANCED_FACE('',(#11502),#3370,.F.);
#96476=ADVANCED_FACE('',(#11503),#91618,.F.);
#96477=ADVANCED_FACE('',(#11504),#91619,.F.);
#96478=ADVANCED_FACE('',(#11505),#3371,.F.);
#96479=ADVANCED_FACE('',(#11506),#3372,.F.);
#96480=ADVANCED_FACE('',(#11507),#91620,.F.);
#96481=ADVANCED_FACE('',(#11508),#91621,.F.);
#96482=ADVANCED_FACE('',(#11509),#3373,.F.);
#96483=ADVANCED_FACE('',(#11510),#91622,.F.);
#96484=ADVANCED_FACE('',(#11511),#6178,.F.);
#96485=ADVANCED_FACE('',(#11512),#3374,.F.);
#96486=ADVANCED_FACE('',(#11513),#3375,.F.);
#96487=ADVANCED_FACE('',(#11514),#91623,.F.);
#96488=ADVANCED_FACE('',(#11515),#91624,.F.);
#96489=ADVANCED_FACE('',(#11516),#3376,.F.);
#96490=ADVANCED_FACE('',(#11517),#3377,.F.);
#96491=ADVANCED_FACE('',(#11518),#6179,.F.);
#96492=ADVANCED_FACE('',(#11519),#91625,.F.);
#96493=ADVANCED_FACE('',(#11520),#3378,.F.);
#96494=ADVANCED_FACE('',(#11521),#91626,.F.);
#96495=ADVANCED_FACE('',(#11522),#91627,.F.);
#96496=ADVANCED_FACE('',(#11523),#3379,.F.);
#96497=ADVANCED_FACE('',(#11524),#3380,.F.);
#96498=ADVANCED_FACE('',(#11525),#91628,.F.);
#96499=ADVANCED_FACE('',(#11526),#91629,.F.);
#96500=ADVANCED_FACE('',(#11527),#3381,.F.);
#96501=ADVANCED_FACE('',(#11528),#91630,.F.);
#96502=ADVANCED_FACE('',(#11529),#91631,.F.);
#96503=ADVANCED_FACE('',(#11530),#3382,.F.);
#96504=ADVANCED_FACE('',(#11531),#91632,.F.);
#96505=ADVANCED_FACE('',(#11532),#91633,.F.);
#96506=ADVANCED_FACE('',(#11533),#3383,.F.);
#96507=ADVANCED_FACE('',(#11534),#3384,.F.);
#96508=ADVANCED_FACE('',(#11535),#91634,.F.);
#96509=ADVANCED_FACE('',(#11536),#91635,.F.);
#96510=ADVANCED_FACE('',(#11537),#3385,.F.);
#96511=ADVANCED_FACE('',(#11538),#91636,.F.);
#96512=ADVANCED_FACE('',(#11539),#6180,.F.);
#96513=ADVANCED_FACE('',(#11540),#3386,.F.);
#96514=ADVANCED_FACE('',(#11541),#3387,.F.);
#96515=ADVANCED_FACE('',(#11542),#91637,.F.);
#96516=ADVANCED_FACE('',(#11543),#91638,.F.);
#96517=ADVANCED_FACE('',(#11544),#3388,.F.);
#96518=ADVANCED_FACE('',(#11545),#3389,.F.);
#96519=ADVANCED_FACE('',(#11546),#6181,.F.);
#96520=ADVANCED_FACE('',(#11547),#91639,.F.);
#96521=ADVANCED_FACE('',(#11548),#3390,.F.);
#96522=ADVANCED_FACE('',(#11549),#91640,.F.);
#96523=ADVANCED_FACE('',(#11550),#91641,.F.);
#96524=ADVANCED_FACE('',(#11551),#3391,.F.);
#96525=ADVANCED_FACE('',(#11552),#3392,.F.);
#96526=ADVANCED_FACE('',(#11553),#91642,.F.);
#96527=ADVANCED_FACE('',(#11554),#91643,.F.);
#96528=ADVANCED_FACE('',(#11555),#3393,.F.);
#96529=ADVANCED_FACE('',(#11556),#91644,.F.);
#96530=ADVANCED_FACE('',(#11557),#91645,.F.);
#96531=ADVANCED_FACE('',(#11558),#3394,.F.);
#96532=ADVANCED_FACE('',(#11559),#91646,.F.);
#96533=ADVANCED_FACE('',(#11560),#91647,.F.);
#96534=ADVANCED_FACE('',(#11561),#3395,.F.);
#96535=ADVANCED_FACE('',(#11562),#3396,.F.);
#96536=ADVANCED_FACE('',(#11563),#91648,.F.);
#96537=ADVANCED_FACE('',(#11564),#91649,.F.);
#96538=ADVANCED_FACE('',(#11565),#3397,.F.);
#96539=ADVANCED_FACE('',(#11566),#91650,.F.);
#96540=ADVANCED_FACE('',(#11567),#6182,.F.);
#96541=ADVANCED_FACE('',(#11568),#3398,.F.);
#96542=ADVANCED_FACE('',(#11569),#3399,.F.);
#96543=ADVANCED_FACE('',(#11570),#91651,.F.);
#96544=ADVANCED_FACE('',(#11571),#91652,.F.);
#96545=ADVANCED_FACE('',(#11572),#3400,.F.);
#96546=ADVANCED_FACE('',(#11573),#3401,.F.);
#96547=ADVANCED_FACE('',(#11574),#6183,.F.);
#96548=ADVANCED_FACE('',(#11575),#91653,.F.);
#96549=ADVANCED_FACE('',(#11576),#3402,.F.);
#96550=ADVANCED_FACE('',(#11577),#91654,.F.);
#96551=ADVANCED_FACE('',(#11578),#91655,.F.);
#96552=ADVANCED_FACE('',(#11579),#3403,.F.);
#96553=ADVANCED_FACE('',(#11580),#3404,.F.);
#96554=ADVANCED_FACE('',(#11581),#91656,.F.);
#96555=ADVANCED_FACE('',(#11582),#91657,.F.);
#96556=ADVANCED_FACE('',(#11583),#3405,.F.);
#96557=ADVANCED_FACE('',(#11584),#91658,.F.);
#96558=ADVANCED_FACE('',(#11585),#91659,.F.);
#96559=ADVANCED_FACE('',(#11586),#3406,.F.);
#96560=ADVANCED_FACE('',(#11587),#91660,.F.);
#96561=ADVANCED_FACE('',(#11588),#91661,.F.);
#96562=ADVANCED_FACE('',(#11589),#3407,.F.);
#96563=ADVANCED_FACE('',(#11590),#3408,.F.);
#96564=ADVANCED_FACE('',(#11591),#91662,.F.);
#96565=ADVANCED_FACE('',(#11592),#91663,.F.);
#96566=ADVANCED_FACE('',(#11593),#3409,.F.);
#96567=ADVANCED_FACE('',(#11594),#91664,.F.);
#96568=ADVANCED_FACE('',(#11595),#6184,.F.);
#96569=ADVANCED_FACE('',(#11596),#3410,.F.);
#96570=ADVANCED_FACE('',(#11597),#3411,.F.);
#96571=ADVANCED_FACE('',(#11598),#91665,.F.);
#96572=ADVANCED_FACE('',(#11599),#91666,.F.);
#96573=ADVANCED_FACE('',(#11600),#3412,.F.);
#96574=ADVANCED_FACE('',(#11601),#3413,.F.);
#96575=ADVANCED_FACE('',(#11602),#6185,.F.);
#96576=ADVANCED_FACE('',(#11603),#91667,.F.);
#96577=ADVANCED_FACE('',(#11604),#3414,.F.);
#96578=ADVANCED_FACE('',(#11605),#91668,.F.);
#96579=ADVANCED_FACE('',(#11606),#91669,.F.);
#96580=ADVANCED_FACE('',(#11607),#3415,.F.);
#96581=ADVANCED_FACE('',(#11608),#3416,.F.);
#96582=ADVANCED_FACE('',(#11609),#91670,.F.);
#96583=ADVANCED_FACE('',(#11610),#91671,.F.);
#96584=ADVANCED_FACE('',(#11611),#3417,.F.);
#96585=ADVANCED_FACE('',(#11612),#91672,.F.);
#96586=ADVANCED_FACE('',(#11613),#91673,.F.);
#96587=ADVANCED_FACE('',(#11614),#3418,.F.);
#96588=ADVANCED_FACE('',(#11615),#91674,.F.);
#96589=ADVANCED_FACE('',(#11616),#91675,.F.);
#96590=ADVANCED_FACE('',(#11617),#3419,.F.);
#96591=ADVANCED_FACE('',(#11618),#3420,.F.);
#96592=ADVANCED_FACE('',(#11619),#91676,.F.);
#96593=ADVANCED_FACE('',(#11620),#91677,.F.);
#96594=ADVANCED_FACE('',(#11621),#3421,.F.);
#96595=ADVANCED_FACE('',(#11622),#91678,.F.);
#96596=ADVANCED_FACE('',(#11623),#6186,.F.);
#96597=ADVANCED_FACE('',(#11624),#3422,.F.);
#96598=ADVANCED_FACE('',(#11625),#3423,.F.);
#96599=ADVANCED_FACE('',(#11626),#91679,.F.);
#96600=ADVANCED_FACE('',(#11627),#91680,.F.);
#96601=ADVANCED_FACE('',(#11628),#3424,.F.);
#96602=ADVANCED_FACE('',(#11629),#3425,.F.);
#96603=ADVANCED_FACE('',(#11630),#6187,.F.);
#96604=ADVANCED_FACE('',(#11631),#91681,.F.);
#96605=ADVANCED_FACE('',(#11632),#3426,.F.);
#96606=ADVANCED_FACE('',(#11633),#91682,.F.);
#96607=ADVANCED_FACE('',(#11634),#91683,.F.);
#96608=ADVANCED_FACE('',(#11635),#3427,.F.);
#96609=ADVANCED_FACE('',(#11636),#3428,.F.);
#96610=ADVANCED_FACE('',(#11637),#91684,.F.);
#96611=ADVANCED_FACE('',(#11638),#91685,.F.);
#96612=ADVANCED_FACE('',(#11639),#3429,.F.);
#96613=ADVANCED_FACE('',(#11640),#91686,.F.);
#96614=ADVANCED_FACE('',(#11641),#91687,.F.);
#96615=ADVANCED_FACE('',(#11642),#3430,.F.);
#96616=ADVANCED_FACE('',(#11643),#91688,.F.);
#96617=ADVANCED_FACE('',(#11644),#91689,.F.);
#96618=ADVANCED_FACE('',(#11645),#3431,.F.);
#96619=ADVANCED_FACE('',(#11646),#3432,.F.);
#96620=ADVANCED_FACE('',(#11647),#91690,.F.);
#96621=ADVANCED_FACE('',(#11648),#91691,.F.);
#96622=ADVANCED_FACE('',(#11649),#3433,.F.);
#96623=ADVANCED_FACE('',(#11650),#91692,.F.);
#96624=ADVANCED_FACE('',(#11651),#6188,.F.);
#96625=ADVANCED_FACE('',(#11652),#3434,.F.);
#96626=ADVANCED_FACE('',(#11653),#3435,.F.);
#96627=ADVANCED_FACE('',(#11654),#91693,.F.);
#96628=ADVANCED_FACE('',(#11655),#91694,.F.);
#96629=ADVANCED_FACE('',(#11656),#3436,.F.);
#96630=ADVANCED_FACE('',(#11657),#3437,.F.);
#96631=ADVANCED_FACE('',(#11658),#6189,.F.);
#96632=ADVANCED_FACE('',(#11659),#91695,.F.);
#96633=ADVANCED_FACE('',(#11660),#3438,.F.);
#96634=ADVANCED_FACE('',(#11661),#91696,.F.);
#96635=ADVANCED_FACE('',(#11662),#91697,.F.);
#96636=ADVANCED_FACE('',(#11663),#3439,.F.);
#96637=ADVANCED_FACE('',(#11664),#3440,.F.);
#96638=ADVANCED_FACE('',(#11665),#91698,.F.);
#96639=ADVANCED_FACE('',(#11666),#91699,.F.);
#96640=ADVANCED_FACE('',(#11667),#3441,.F.);
#96641=ADVANCED_FACE('',(#11668),#91700,.F.);
#96642=ADVANCED_FACE('',(#11669),#91701,.F.);
#96643=ADVANCED_FACE('',(#11670),#3442,.F.);
#96644=ADVANCED_FACE('',(#11671),#91702,.F.);
#96645=ADVANCED_FACE('',(#11672),#91703,.F.);
#96646=ADVANCED_FACE('',(#11673),#3443,.F.);
#96647=ADVANCED_FACE('',(#11674),#3444,.F.);
#96648=ADVANCED_FACE('',(#11675),#91704,.F.);
#96649=ADVANCED_FACE('',(#11676),#91705,.F.);
#96650=ADVANCED_FACE('',(#11677),#3445,.F.);
#96651=ADVANCED_FACE('',(#11678),#91706,.F.);
#96652=ADVANCED_FACE('',(#11679),#6190,.F.);
#96653=ADVANCED_FACE('',(#11680),#3446,.F.);
#96654=ADVANCED_FACE('',(#11681),#3447,.F.);
#96655=ADVANCED_FACE('',(#11682),#91707,.F.);
#96656=ADVANCED_FACE('',(#11683),#91708,.F.);
#96657=ADVANCED_FACE('',(#11684),#3448,.F.);
#96658=ADVANCED_FACE('',(#11685),#3449,.F.);
#96659=ADVANCED_FACE('',(#11686),#6191,.F.);
#96660=ADVANCED_FACE('',(#11687),#91709,.F.);
#96661=ADVANCED_FACE('',(#11688),#3450,.F.);
#96662=ADVANCED_FACE('',(#11689),#91710,.F.);
#96663=ADVANCED_FACE('',(#11690),#91711,.F.);
#96664=ADVANCED_FACE('',(#11691),#3451,.F.);
#96665=ADVANCED_FACE('',(#11692),#3452,.F.);
#96666=ADVANCED_FACE('',(#11693),#91712,.F.);
#96667=ADVANCED_FACE('',(#11694),#91713,.F.);
#96668=ADVANCED_FACE('',(#11695),#3453,.F.);
#96669=ADVANCED_FACE('',(#11696),#91714,.F.);
#96670=ADVANCED_FACE('',(#11697),#91715,.F.);
#96671=ADVANCED_FACE('',(#11698),#3454,.F.);
#96672=ADVANCED_FACE('',(#11699),#91716,.F.);
#96673=ADVANCED_FACE('',(#11700),#91717,.F.);
#96674=ADVANCED_FACE('',(#11701),#3455,.F.);
#96675=ADVANCED_FACE('',(#11702),#3456,.F.);
#96676=ADVANCED_FACE('',(#11703),#91718,.F.);
#96677=ADVANCED_FACE('',(#11704),#91719,.F.);
#96678=ADVANCED_FACE('',(#11705),#3457,.F.);
#96679=ADVANCED_FACE('',(#11706),#91720,.F.);
#96680=ADVANCED_FACE('',(#11707),#6192,.F.);
#96681=ADVANCED_FACE('',(#11708),#3458,.F.);
#96682=ADVANCED_FACE('',(#11709),#3459,.F.);
#96683=ADVANCED_FACE('',(#11710),#91721,.F.);
#96684=ADVANCED_FACE('',(#11711),#91722,.F.);
#96685=ADVANCED_FACE('',(#11712),#3460,.F.);
#96686=ADVANCED_FACE('',(#11713),#3461,.F.);
#96687=ADVANCED_FACE('',(#11714),#6193,.F.);
#96688=ADVANCED_FACE('',(#11715),#91723,.F.);
#96689=ADVANCED_FACE('',(#11716),#3462,.F.);
#96690=ADVANCED_FACE('',(#11717),#91724,.F.);
#96691=ADVANCED_FACE('',(#11718),#91725,.F.);
#96692=ADVANCED_FACE('',(#11719),#3463,.F.);
#96693=ADVANCED_FACE('',(#11720),#3464,.F.);
#96694=ADVANCED_FACE('',(#11721),#91726,.F.);
#96695=ADVANCED_FACE('',(#11722),#91727,.F.);
#96696=ADVANCED_FACE('',(#11723),#3465,.F.);
#96697=ADVANCED_FACE('',(#11724),#91728,.F.);
#96698=ADVANCED_FACE('',(#11725),#91729,.F.);
#96699=ADVANCED_FACE('',(#11726),#3466,.F.);
#96700=ADVANCED_FACE('',(#11727),#91730,.F.);
#96701=ADVANCED_FACE('',(#11728),#91731,.F.);
#96702=ADVANCED_FACE('',(#11729),#3467,.F.);
#96703=ADVANCED_FACE('',(#11730),#3468,.F.);
#96704=ADVANCED_FACE('',(#11731),#91732,.F.);
#96705=ADVANCED_FACE('',(#11732),#91733,.F.);
#96706=ADVANCED_FACE('',(#11733),#3469,.F.);
#96707=ADVANCED_FACE('',(#11734),#91734,.F.);
#96708=ADVANCED_FACE('',(#11735),#6194,.F.);
#96709=ADVANCED_FACE('',(#11736),#3470,.F.);
#96710=ADVANCED_FACE('',(#11737),#3471,.F.);
#96711=ADVANCED_FACE('',(#11738),#91735,.F.);
#96712=ADVANCED_FACE('',(#11739),#91736,.F.);
#96713=ADVANCED_FACE('',(#11740),#3472,.F.);
#96714=ADVANCED_FACE('',(#11741),#3473,.F.);
#96715=ADVANCED_FACE('',(#11742),#6195,.F.);
#96716=ADVANCED_FACE('',(#11743),#91737,.F.);
#96717=ADVANCED_FACE('',(#11744),#3474,.F.);
#96718=ADVANCED_FACE('',(#11745),#91738,.F.);
#96719=ADVANCED_FACE('',(#11746),#91739,.F.);
#96720=ADVANCED_FACE('',(#11747),#3475,.F.);
#96721=ADVANCED_FACE('',(#11748),#3476,.F.);
#96722=ADVANCED_FACE('',(#11749),#91740,.F.);
#96723=ADVANCED_FACE('',(#11750),#91741,.F.);
#96724=ADVANCED_FACE('',(#11751),#3477,.F.);
#96725=ADVANCED_FACE('',(#11752),#91742,.F.);
#96726=ADVANCED_FACE('',(#11753),#91743,.F.);
#96727=ADVANCED_FACE('',(#11754),#3478,.F.);
#96728=ADVANCED_FACE('',(#11755),#91744,.F.);
#96729=ADVANCED_FACE('',(#11756),#91745,.F.);
#96730=ADVANCED_FACE('',(#11757),#3479,.F.);
#96731=ADVANCED_FACE('',(#11758),#3480,.F.);
#96732=ADVANCED_FACE('',(#11759),#91746,.F.);
#96733=ADVANCED_FACE('',(#11760),#91747,.F.);
#96734=ADVANCED_FACE('',(#11761),#3481,.F.);
#96735=ADVANCED_FACE('',(#11762),#91748,.F.);
#96736=ADVANCED_FACE('',(#11763),#6196,.F.);
#96737=ADVANCED_FACE('',(#11764),#3482,.F.);
#96738=ADVANCED_FACE('',(#11765),#3483,.F.);
#96739=ADVANCED_FACE('',(#11766),#91749,.F.);
#96740=ADVANCED_FACE('',(#11767),#91750,.F.);
#96741=ADVANCED_FACE('',(#11768),#3484,.F.);
#96742=ADVANCED_FACE('',(#11769),#3485,.F.);
#96743=ADVANCED_FACE('',(#11770),#6197,.F.);
#96744=ADVANCED_FACE('',(#11771),#91751,.F.);
#96745=ADVANCED_FACE('',(#11772),#3486,.F.);
#96746=ADVANCED_FACE('',(#11773),#91752,.F.);
#96747=ADVANCED_FACE('',(#11774),#91753,.F.);
#96748=ADVANCED_FACE('',(#11775),#3487,.F.);
#96749=ADVANCED_FACE('',(#11776),#3488,.F.);
#96750=ADVANCED_FACE('',(#11777),#91754,.F.);
#96751=ADVANCED_FACE('',(#11778),#91755,.F.);
#96752=ADVANCED_FACE('',(#11779),#3489,.F.);
#96753=ADVANCED_FACE('',(#11780),#91756,.F.);
#96754=ADVANCED_FACE('',(#11781),#91757,.F.);
#96755=ADVANCED_FACE('',(#11782),#3490,.F.);
#96756=ADVANCED_FACE('',(#11783),#91758,.F.);
#96757=ADVANCED_FACE('',(#11784),#91759,.F.);
#96758=ADVANCED_FACE('',(#11785),#3491,.F.);
#96759=ADVANCED_FACE('',(#11786),#3492,.F.);
#96760=ADVANCED_FACE('',(#11787),#91760,.F.);
#96761=ADVANCED_FACE('',(#11788),#91761,.F.);
#96762=ADVANCED_FACE('',(#11789),#3493,.F.);
#96763=ADVANCED_FACE('',(#11790),#91762,.F.);
#96764=ADVANCED_FACE('',(#11791),#6198,.F.);
#96765=ADVANCED_FACE('',(#11792),#3494,.F.);
#96766=ADVANCED_FACE('',(#11793),#3495,.F.);
#96767=ADVANCED_FACE('',(#11794),#91763,.F.);
#96768=ADVANCED_FACE('',(#11795),#91764,.F.);
#96769=ADVANCED_FACE('',(#11796),#3496,.F.);
#96770=ADVANCED_FACE('',(#11797),#3497,.F.);
#96771=ADVANCED_FACE('',(#11798),#6199,.F.);
#96772=ADVANCED_FACE('',(#11799),#91765,.F.);
#96773=ADVANCED_FACE('',(#11800),#3498,.F.);
#96774=ADVANCED_FACE('',(#11801),#91766,.F.);
#96775=ADVANCED_FACE('',(#11802),#91767,.F.);
#96776=ADVANCED_FACE('',(#11803),#3499,.F.);
#96777=ADVANCED_FACE('',(#11804),#3500,.F.);
#96778=ADVANCED_FACE('',(#11805),#91768,.F.);
#96779=ADVANCED_FACE('',(#11806),#91769,.F.);
#96780=ADVANCED_FACE('',(#11807),#3501,.F.);
#96781=ADVANCED_FACE('',(#11808),#91770,.F.);
#96782=ADVANCED_FACE('',(#11809),#91771,.F.);
#96783=ADVANCED_FACE('',(#11810),#3502,.F.);
#96784=ADVANCED_FACE('',(#11811),#91772,.F.);
#96785=ADVANCED_FACE('',(#11812),#91773,.F.);
#96786=ADVANCED_FACE('',(#11813),#3503,.F.);
#96787=ADVANCED_FACE('',(#11814),#3504,.F.);
#96788=ADVANCED_FACE('',(#11815),#91774,.F.);
#96789=ADVANCED_FACE('',(#11816),#91775,.F.);
#96790=ADVANCED_FACE('',(#11817),#3505,.F.);
#96791=ADVANCED_FACE('',(#11818),#91776,.F.);
#96792=ADVANCED_FACE('',(#11819),#6200,.F.);
#96793=ADVANCED_FACE('',(#11820),#3506,.F.);
#96794=ADVANCED_FACE('',(#11821),#3507,.F.);
#96795=ADVANCED_FACE('',(#11822),#91777,.F.);
#96796=ADVANCED_FACE('',(#11823),#91778,.F.);
#96797=ADVANCED_FACE('',(#11824),#3508,.F.);
#96798=ADVANCED_FACE('',(#11825),#3509,.F.);
#96799=ADVANCED_FACE('',(#11826),#6201,.F.);
#96800=ADVANCED_FACE('',(#11827),#91779,.F.);
#96801=ADVANCED_FACE('',(#11828),#3510,.F.);
#96802=ADVANCED_FACE('',(#11829),#91780,.F.);
#96803=ADVANCED_FACE('',(#11830),#91781,.F.);
#96804=ADVANCED_FACE('',(#11831),#3511,.F.);
#96805=ADVANCED_FACE('',(#11832),#3512,.F.);
#96806=ADVANCED_FACE('',(#11833),#91782,.F.);
#96807=ADVANCED_FACE('',(#11834),#91783,.F.);
#96808=ADVANCED_FACE('',(#11835),#3513,.F.);
#96809=ADVANCED_FACE('',(#11836),#91784,.F.);
#96810=ADVANCED_FACE('',(#11837),#91785,.F.);
#96811=ADVANCED_FACE('',(#11838),#3514,.F.);
#96812=ADVANCED_FACE('',(#11839),#91786,.F.);
#96813=ADVANCED_FACE('',(#11840),#91787,.F.);
#96814=ADVANCED_FACE('',(#11841),#3515,.F.);
#96815=ADVANCED_FACE('',(#11842),#3516,.F.);
#96816=ADVANCED_FACE('',(#11843),#91788,.F.);
#96817=ADVANCED_FACE('',(#11844),#91789,.F.);
#96818=ADVANCED_FACE('',(#11845),#3517,.F.);
#96819=ADVANCED_FACE('',(#11846),#91790,.F.);
#96820=ADVANCED_FACE('',(#11847),#6202,.F.);
#96821=ADVANCED_FACE('',(#11848),#3518,.F.);
#96822=ADVANCED_FACE('',(#11849),#3519,.F.);
#96823=ADVANCED_FACE('',(#11850),#91791,.F.);
#96824=ADVANCED_FACE('',(#11851),#91792,.F.);
#96825=ADVANCED_FACE('',(#11852),#3520,.F.);
#96826=ADVANCED_FACE('',(#11853),#3521,.F.);
#96827=ADVANCED_FACE('',(#11854),#6203,.F.);
#96828=ADVANCED_FACE('',(#11855),#91793,.F.);
#96829=ADVANCED_FACE('',(#11856),#3522,.F.);
#96830=ADVANCED_FACE('',(#11857),#91794,.F.);
#96831=ADVANCED_FACE('',(#11858),#91795,.F.);
#96832=ADVANCED_FACE('',(#11859),#3523,.F.);
#96833=ADVANCED_FACE('',(#11860),#3524,.F.);
#96834=ADVANCED_FACE('',(#11861),#91796,.F.);
#96835=ADVANCED_FACE('',(#11862),#91797,.F.);
#96836=ADVANCED_FACE('',(#11863),#3525,.F.);
#96837=ADVANCED_FACE('',(#11864),#91798,.F.);
#96838=ADVANCED_FACE('',(#11865),#91799,.F.);
#96839=ADVANCED_FACE('',(#11866),#3526,.F.);
#96840=ADVANCED_FACE('',(#11867),#91800,.F.);
#96841=ADVANCED_FACE('',(#11868),#91801,.F.);
#96842=ADVANCED_FACE('',(#11869),#3527,.F.);
#96843=ADVANCED_FACE('',(#11870),#3528,.F.);
#96844=ADVANCED_FACE('',(#11871),#91802,.F.);
#96845=ADVANCED_FACE('',(#11872),#91803,.F.);
#96846=ADVANCED_FACE('',(#11873),#3529,.F.);
#96847=ADVANCED_FACE('',(#11874),#91804,.F.);
#96848=ADVANCED_FACE('',(#11875),#6204,.F.);
#96849=ADVANCED_FACE('',(#11876),#3530,.F.);
#96850=ADVANCED_FACE('',(#11877),#3531,.F.);
#96851=ADVANCED_FACE('',(#11878),#91805,.F.);
#96852=ADVANCED_FACE('',(#11879),#91806,.F.);
#96853=ADVANCED_FACE('',(#11880),#3532,.F.);
#96854=ADVANCED_FACE('',(#11881),#3533,.F.);
#96855=ADVANCED_FACE('',(#11882),#6205,.F.);
#96856=ADVANCED_FACE('',(#11883),#91807,.F.);
#96857=ADVANCED_FACE('',(#11884),#3534,.F.);
#96858=ADVANCED_FACE('',(#11885),#91808,.F.);
#96859=ADVANCED_FACE('',(#11886),#91809,.F.);
#96860=ADVANCED_FACE('',(#11887),#3535,.F.);
#96861=ADVANCED_FACE('',(#11888),#3536,.F.);
#96862=ADVANCED_FACE('',(#11889),#91810,.F.);
#96863=ADVANCED_FACE('',(#11890),#91811,.F.);
#96864=ADVANCED_FACE('',(#11891),#3537,.F.);
#96865=ADVANCED_FACE('',(#11892),#91812,.F.);
#96866=ADVANCED_FACE('',(#11893),#91813,.F.);
#96867=ADVANCED_FACE('',(#11894),#3538,.F.);
#96868=ADVANCED_FACE('',(#11895),#91814,.F.);
#96869=ADVANCED_FACE('',(#11896),#91815,.F.);
#96870=ADVANCED_FACE('',(#11897),#3539,.F.);
#96871=ADVANCED_FACE('',(#11898),#3540,.F.);
#96872=ADVANCED_FACE('',(#11899),#91816,.F.);
#96873=ADVANCED_FACE('',(#11900),#91817,.F.);
#96874=ADVANCED_FACE('',(#11901),#3541,.F.);
#96875=ADVANCED_FACE('',(#11902),#91818,.F.);
#96876=ADVANCED_FACE('',(#11903),#6206,.F.);
#96877=ADVANCED_FACE('',(#11904),#3542,.F.);
#96878=ADVANCED_FACE('',(#11905),#3543,.F.);
#96879=ADVANCED_FACE('',(#11906),#91819,.F.);
#96880=ADVANCED_FACE('',(#11907),#91820,.F.);
#96881=ADVANCED_FACE('',(#11908),#3544,.F.);
#96882=ADVANCED_FACE('',(#11909),#3545,.F.);
#96883=ADVANCED_FACE('',(#11910),#6207,.F.);
#96884=ADVANCED_FACE('',(#11911),#91821,.F.);
#96885=ADVANCED_FACE('',(#11912),#3546,.F.);
#96886=ADVANCED_FACE('',(#11913),#91822,.F.);
#96887=ADVANCED_FACE('',(#11914),#91823,.F.);
#96888=ADVANCED_FACE('',(#11915),#3547,.F.);
#96889=ADVANCED_FACE('',(#11916),#3548,.F.);
#96890=ADVANCED_FACE('',(#11917),#91824,.F.);
#96891=ADVANCED_FACE('',(#11918),#91825,.F.);
#96892=ADVANCED_FACE('',(#11919),#3549,.F.);
#96893=ADVANCED_FACE('',(#11920),#91826,.F.);
#96894=ADVANCED_FACE('',(#11921),#91827,.F.);
#96895=ADVANCED_FACE('',(#11922),#3550,.F.);
#96896=ADVANCED_FACE('',(#11923),#91828,.F.);
#96897=ADVANCED_FACE('',(#11924),#91829,.F.);
#96898=ADVANCED_FACE('',(#11925),#3551,.F.);
#96899=ADVANCED_FACE('',(#11926),#3552,.F.);
#96900=ADVANCED_FACE('',(#11927),#91830,.F.);
#96901=ADVANCED_FACE('',(#11928),#91831,.F.);
#96902=ADVANCED_FACE('',(#11929),#3553,.F.);
#96903=ADVANCED_FACE('',(#11930),#91832,.F.);
#96904=ADVANCED_FACE('',(#11931),#6208,.F.);
#96905=ADVANCED_FACE('',(#11932),#3554,.F.);
#96906=ADVANCED_FACE('',(#11933),#3555,.F.);
#96907=ADVANCED_FACE('',(#11934),#91833,.F.);
#96908=ADVANCED_FACE('',(#11935),#91834,.F.);
#96909=ADVANCED_FACE('',(#11936),#3556,.F.);
#96910=ADVANCED_FACE('',(#11937),#3557,.F.);
#96911=ADVANCED_FACE('',(#11938),#6209,.F.);
#96912=ADVANCED_FACE('',(#11939),#91835,.F.);
#96913=ADVANCED_FACE('',(#11940),#3558,.F.);
#96914=ADVANCED_FACE('',(#11941),#91836,.F.);
#96915=ADVANCED_FACE('',(#11942),#91837,.F.);
#96916=ADVANCED_FACE('',(#11943),#3559,.F.);
#96917=ADVANCED_FACE('',(#11944),#3560,.F.);
#96918=ADVANCED_FACE('',(#11945),#91838,.F.);
#96919=ADVANCED_FACE('',(#11946),#91839,.F.);
#96920=ADVANCED_FACE('',(#11947),#3561,.F.);
#96921=ADVANCED_FACE('',(#11948),#91840,.F.);
#96922=ADVANCED_FACE('',(#11949),#91841,.F.);
#96923=ADVANCED_FACE('',(#11950),#3562,.F.);
#96924=ADVANCED_FACE('',(#11951),#91842,.F.);
#96925=ADVANCED_FACE('',(#11952),#91843,.F.);
#96926=ADVANCED_FACE('',(#11953),#3563,.F.);
#96927=ADVANCED_FACE('',(#11954),#3564,.F.);
#96928=ADVANCED_FACE('',(#11955),#91844,.F.);
#96929=ADVANCED_FACE('',(#11956),#91845,.F.);
#96930=ADVANCED_FACE('',(#11957),#3565,.F.);
#96931=ADVANCED_FACE('',(#11958),#91846,.F.);
#96932=ADVANCED_FACE('',(#11959),#6210,.F.);
#96933=ADVANCED_FACE('',(#11960),#3566,.F.);
#96934=ADVANCED_FACE('',(#11961),#3567,.F.);
#96935=ADVANCED_FACE('',(#11962),#91847,.F.);
#96936=ADVANCED_FACE('',(#11963),#91848,.F.);
#96937=ADVANCED_FACE('',(#11964),#3568,.F.);
#96938=ADVANCED_FACE('',(#11965),#3569,.F.);
#96939=ADVANCED_FACE('',(#11966),#6211,.F.);
#96940=ADVANCED_FACE('',(#11967),#91849,.F.);
#96941=ADVANCED_FACE('',(#11968),#3570,.F.);
#96942=ADVANCED_FACE('',(#11969),#91850,.F.);
#96943=ADVANCED_FACE('',(#11970),#91851,.F.);
#96944=ADVANCED_FACE('',(#11971),#3571,.F.);
#96945=ADVANCED_FACE('',(#11972),#3572,.F.);
#96946=ADVANCED_FACE('',(#11973),#91852,.F.);
#96947=ADVANCED_FACE('',(#11974),#91853,.F.);
#96948=ADVANCED_FACE('',(#11975),#3573,.F.);
#96949=ADVANCED_FACE('',(#11976),#91854,.F.);
#96950=ADVANCED_FACE('',(#11977),#91855,.F.);
#96951=ADVANCED_FACE('',(#11978),#3574,.F.);
#96952=ADVANCED_FACE('',(#11979),#91856,.F.);
#96953=ADVANCED_FACE('',(#11980),#91857,.F.);
#96954=ADVANCED_FACE('',(#11981),#3575,.F.);
#96955=ADVANCED_FACE('',(#11982),#3576,.F.);
#96956=ADVANCED_FACE('',(#11983),#91858,.F.);
#96957=ADVANCED_FACE('',(#11984),#91859,.F.);
#96958=ADVANCED_FACE('',(#11985),#3577,.F.);
#96959=ADVANCED_FACE('',(#11986),#91860,.F.);
#96960=ADVANCED_FACE('',(#11987),#6212,.F.);
#96961=ADVANCED_FACE('',(#11988),#3578,.F.);
#96962=ADVANCED_FACE('',(#11989),#3579,.F.);
#96963=ADVANCED_FACE('',(#11990),#91861,.F.);
#96964=ADVANCED_FACE('',(#11991),#91862,.F.);
#96965=ADVANCED_FACE('',(#11992),#3580,.F.);
#96966=ADVANCED_FACE('',(#11993),#3581,.F.);
#96967=ADVANCED_FACE('',(#11994),#6213,.F.);
#96968=ADVANCED_FACE('',(#11995),#91863,.F.);
#96969=ADVANCED_FACE('',(#11996),#3582,.F.);
#96970=ADVANCED_FACE('',(#11997),#91864,.F.);
#96971=ADVANCED_FACE('',(#11998),#91865,.F.);
#96972=ADVANCED_FACE('',(#11999),#3583,.F.);
#96973=ADVANCED_FACE('',(#12000),#3584,.F.);
#96974=ADVANCED_FACE('',(#12001),#91866,.F.);
#96975=ADVANCED_FACE('',(#12002),#91867,.F.);
#96976=ADVANCED_FACE('',(#12003),#3585,.F.);
#96977=ADVANCED_FACE('',(#12004),#91868,.F.);
#96978=ADVANCED_FACE('',(#12005),#91869,.F.);
#96979=ADVANCED_FACE('',(#12006),#3586,.F.);
#96980=ADVANCED_FACE('',(#12007),#91870,.F.);
#96981=ADVANCED_FACE('',(#12008),#91871,.F.);
#96982=ADVANCED_FACE('',(#12009),#3587,.F.);
#96983=ADVANCED_FACE('',(#12010),#3588,.F.);
#96984=ADVANCED_FACE('',(#12011),#91872,.F.);
#96985=ADVANCED_FACE('',(#12012),#91873,.F.);
#96986=ADVANCED_FACE('',(#12013),#3589,.F.);
#96987=ADVANCED_FACE('',(#12014),#91874,.F.);
#96988=ADVANCED_FACE('',(#12015),#3590,.F.);
#96989=ADVANCED_FACE('',(#12016),#3591,.F.);
#96990=ADVANCED_FACE('',(#12017),#91875,.F.);
#96991=ADVANCED_FACE('',(#12018),#91876,.F.);
#96992=ADVANCED_FACE('',(#12019),#3592,.F.);
#96993=ADVANCED_FACE('',(#12020),#3593,.F.);
#96994=ADVANCED_FACE('',(#12021),#91877,.F.);
#96995=ADVANCED_FACE('',(#12022),#3594,.F.);
#96996=ADVANCED_FACE('',(#12023),#91878,.F.);
#96997=ADVANCED_FACE('',(#12024),#91879,.F.);
#96998=ADVANCED_FACE('',(#12025),#3595,.F.);
#96999=ADVANCED_FACE('',(#12026),#3596,.F.);
#97000=ADVANCED_FACE('',(#12027),#91880,.F.);
#97001=ADVANCED_FACE('',(#12028),#91881,.F.);
#97002=ADVANCED_FACE('',(#12029),#3597,.F.);
#97003=ADVANCED_FACE('',(#12030),#91882,.F.);
#97004=ADVANCED_FACE('',(#12031),#91883,.F.);
#97005=ADVANCED_FACE('',(#12032),#3598,.F.);
#97006=ADVANCED_FACE('',(#12033),#91884,.F.);
#97007=ADVANCED_FACE('',(#12034),#91885,.F.);
#97008=ADVANCED_FACE('',(#12035),#3599,.F.);
#97009=ADVANCED_FACE('',(#12036),#3600,.F.);
#97010=ADVANCED_FACE('',(#12037),#91886,.F.);
#97011=ADVANCED_FACE('',(#12038),#91887,.F.);
#97012=ADVANCED_FACE('',(#12039),#3601,.F.);
#97013=ADVANCED_FACE('',(#12040),#91888,.F.);
#97014=ADVANCED_FACE('',(#12041),#6214,.F.);
#97015=ADVANCED_FACE('',(#12042),#3602,.F.);
#97016=ADVANCED_FACE('',(#12043),#3603,.F.);
#97017=ADVANCED_FACE('',(#12044),#91889,.F.);
#97018=ADVANCED_FACE('',(#12045),#91890,.F.);
#97019=ADVANCED_FACE('',(#12046),#3604,.F.);
#97020=ADVANCED_FACE('',(#12047),#3605,.F.);
#97021=ADVANCED_FACE('',(#12048),#6215,.F.);
#97022=ADVANCED_FACE('',(#12049),#91891,.F.);
#97023=ADVANCED_FACE('',(#12050),#3606,.F.);
#97024=ADVANCED_FACE('',(#12051),#91892,.F.);
#97025=ADVANCED_FACE('',(#12052),#91893,.F.);
#97026=ADVANCED_FACE('',(#12053),#3607,.F.);
#97027=ADVANCED_FACE('',(#12054),#3608,.F.);
#97028=ADVANCED_FACE('',(#12055),#91894,.F.);
#97029=ADVANCED_FACE('',(#12056),#91895,.F.);
#97030=ADVANCED_FACE('',(#12057),#3609,.F.);
#97031=ADVANCED_FACE('',(#12058),#91896,.F.);
#97032=ADVANCED_FACE('',(#12059),#91897,.F.);
#97033=ADVANCED_FACE('',(#12060),#3610,.F.);
#97034=ADVANCED_FACE('',(#12061),#91898,.F.);
#97035=ADVANCED_FACE('',(#12062),#91899,.F.);
#97036=ADVANCED_FACE('',(#12063),#3611,.F.);
#97037=ADVANCED_FACE('',(#12064),#3612,.F.);
#97038=ADVANCED_FACE('',(#12065),#91900,.F.);
#97039=ADVANCED_FACE('',(#12066),#91901,.F.);
#97040=ADVANCED_FACE('',(#12067),#3613,.F.);
#97041=ADVANCED_FACE('',(#12068),#91902,.F.);
#97042=ADVANCED_FACE('',(#12069),#6216,.F.);
#97043=ADVANCED_FACE('',(#12070),#3614,.F.);
#97044=ADVANCED_FACE('',(#12071),#3615,.F.);
#97045=ADVANCED_FACE('',(#12072),#91903,.F.);
#97046=ADVANCED_FACE('',(#12073),#91904,.F.);
#97047=ADVANCED_FACE('',(#12074),#3616,.F.);
#97048=ADVANCED_FACE('',(#12075),#3617,.F.);
#97049=ADVANCED_FACE('',(#12076),#6217,.F.);
#97050=ADVANCED_FACE('',(#12077),#91905,.F.);
#97051=ADVANCED_FACE('',(#12078),#3618,.F.);
#97052=ADVANCED_FACE('',(#12079),#91906,.F.);
#97053=ADVANCED_FACE('',(#12080),#91907,.F.);
#97054=ADVANCED_FACE('',(#12081),#3619,.F.);
#97055=ADVANCED_FACE('',(#12082),#3620,.F.);
#97056=ADVANCED_FACE('',(#12083),#91908,.F.);
#97057=ADVANCED_FACE('',(#12084),#91909,.F.);
#97058=ADVANCED_FACE('',(#12085),#3621,.F.);
#97059=ADVANCED_FACE('',(#12086),#91910,.F.);
#97060=ADVANCED_FACE('',(#12087),#91911,.F.);
#97061=ADVANCED_FACE('',(#12088),#3622,.F.);
#97062=ADVANCED_FACE('',(#12089),#91912,.F.);
#97063=ADVANCED_FACE('',(#12090),#91913,.F.);
#97064=ADVANCED_FACE('',(#12091),#3623,.F.);
#97065=ADVANCED_FACE('',(#12092),#3624,.F.);
#97066=ADVANCED_FACE('',(#12093),#91914,.F.);
#97067=ADVANCED_FACE('',(#12094),#91915,.F.);
#97068=ADVANCED_FACE('',(#12095),#3625,.F.);
#97069=ADVANCED_FACE('',(#12096),#91916,.F.);
#97070=ADVANCED_FACE('',(#12097),#6218,.F.);
#97071=ADVANCED_FACE('',(#12098),#3626,.F.);
#97072=ADVANCED_FACE('',(#12099),#3627,.F.);
#97073=ADVANCED_FACE('',(#12100),#91917,.F.);
#97074=ADVANCED_FACE('',(#12101),#91918,.F.);
#97075=ADVANCED_FACE('',(#12102),#3628,.F.);
#97076=ADVANCED_FACE('',(#12103),#3629,.F.);
#97077=ADVANCED_FACE('',(#12104),#6219,.F.);
#97078=ADVANCED_FACE('',(#12105),#91919,.F.);
#97079=ADVANCED_FACE('',(#12106),#3630,.F.);
#97080=ADVANCED_FACE('',(#12107),#91920,.F.);
#97081=ADVANCED_FACE('',(#12108),#91921,.F.);
#97082=ADVANCED_FACE('',(#12109),#3631,.F.);
#97083=ADVANCED_FACE('',(#12110),#3632,.F.);
#97084=ADVANCED_FACE('',(#12111),#91922,.F.);
#97085=ADVANCED_FACE('',(#12112),#91923,.F.);
#97086=ADVANCED_FACE('',(#12113),#3633,.F.);
#97087=ADVANCED_FACE('',(#12114),#91924,.F.);
#97088=ADVANCED_FACE('',(#12115),#91925,.F.);
#97089=ADVANCED_FACE('',(#12116),#3634,.F.);
#97090=ADVANCED_FACE('',(#12117),#91926,.F.);
#97091=ADVANCED_FACE('',(#12118),#91927,.F.);
#97092=ADVANCED_FACE('',(#12119),#3635,.F.);
#97093=ADVANCED_FACE('',(#12120),#3636,.F.);
#97094=ADVANCED_FACE('',(#12121),#91928,.F.);
#97095=ADVANCED_FACE('',(#12122),#91929,.F.);
#97096=ADVANCED_FACE('',(#12123),#3637,.F.);
#97097=ADVANCED_FACE('',(#12124),#91930,.F.);
#97098=ADVANCED_FACE('',(#12125),#6220,.F.);
#97099=ADVANCED_FACE('',(#12126),#3638,.F.);
#97100=ADVANCED_FACE('',(#12127),#3639,.F.);
#97101=ADVANCED_FACE('',(#12128),#91931,.F.);
#97102=ADVANCED_FACE('',(#12129),#91932,.F.);
#97103=ADVANCED_FACE('',(#12130),#3640,.F.);
#97104=ADVANCED_FACE('',(#12131),#3641,.F.);
#97105=ADVANCED_FACE('',(#12132),#6221,.F.);
#97106=ADVANCED_FACE('',(#12133),#91933,.F.);
#97107=ADVANCED_FACE('',(#12134),#3642,.F.);
#97108=ADVANCED_FACE('',(#12135),#91934,.F.);
#97109=ADVANCED_FACE('',(#12136),#91935,.F.);
#97110=ADVANCED_FACE('',(#12137),#3643,.F.);
#97111=ADVANCED_FACE('',(#12138),#3644,.F.);
#97112=ADVANCED_FACE('',(#12139),#91936,.F.);
#97113=ADVANCED_FACE('',(#12140),#91937,.F.);
#97114=ADVANCED_FACE('',(#12141),#3645,.F.);
#97115=ADVANCED_FACE('',(#12142),#91938,.F.);
#97116=ADVANCED_FACE('',(#12143),#91939,.F.);
#97117=ADVANCED_FACE('',(#12144),#3646,.F.);
#97118=ADVANCED_FACE('',(#12145),#91940,.F.);
#97119=ADVANCED_FACE('',(#12146),#91941,.F.);
#97120=ADVANCED_FACE('',(#12147),#3647,.F.);
#97121=ADVANCED_FACE('',(#12148),#3648,.F.);
#97122=ADVANCED_FACE('',(#12149),#91942,.F.);
#97123=ADVANCED_FACE('',(#12150),#91943,.F.);
#97124=ADVANCED_FACE('',(#12151),#3649,.F.);
#97125=ADVANCED_FACE('',(#12152),#91944,.F.);
#97126=ADVANCED_FACE('',(#12153),#6222,.F.);
#97127=ADVANCED_FACE('',(#12154),#3650,.F.);
#97128=ADVANCED_FACE('',(#12155),#3651,.F.);
#97129=ADVANCED_FACE('',(#12156),#91945,.F.);
#97130=ADVANCED_FACE('',(#12157),#91946,.F.);
#97131=ADVANCED_FACE('',(#12158),#3652,.F.);
#97132=ADVANCED_FACE('',(#12159),#3653,.F.);
#97133=ADVANCED_FACE('',(#12160),#6223,.F.);
#97134=ADVANCED_FACE('',(#12161),#91947,.F.);
#97135=ADVANCED_FACE('',(#12162),#3654,.F.);
#97136=ADVANCED_FACE('',(#12163),#91948,.F.);
#97137=ADVANCED_FACE('',(#12164),#91949,.F.);
#97138=ADVANCED_FACE('',(#12165),#3655,.F.);
#97139=ADVANCED_FACE('',(#12166),#3656,.F.);
#97140=ADVANCED_FACE('',(#12167),#91950,.F.);
#97141=ADVANCED_FACE('',(#12168),#91951,.F.);
#97142=ADVANCED_FACE('',(#12169),#3657,.F.);
#97143=ADVANCED_FACE('',(#12170),#91952,.F.);
#97144=ADVANCED_FACE('',(#12171),#91953,.F.);
#97145=ADVANCED_FACE('',(#12172),#3658,.F.);
#97146=ADVANCED_FACE('',(#12173),#91954,.F.);
#97147=ADVANCED_FACE('',(#12174),#91955,.F.);
#97148=ADVANCED_FACE('',(#12175),#3659,.F.);
#97149=ADVANCED_FACE('',(#12176),#3660,.F.);
#97150=ADVANCED_FACE('',(#12177),#91956,.F.);
#97151=ADVANCED_FACE('',(#12178),#91957,.F.);
#97152=ADVANCED_FACE('',(#12179),#3661,.F.);
#97153=ADVANCED_FACE('',(#12180),#91958,.F.);
#97154=ADVANCED_FACE('',(#12181),#6224,.F.);
#97155=ADVANCED_FACE('',(#12182),#3662,.F.);
#97156=ADVANCED_FACE('',(#12183),#3663,.F.);
#97157=ADVANCED_FACE('',(#12184),#91959,.F.);
#97158=ADVANCED_FACE('',(#12185),#91960,.F.);
#97159=ADVANCED_FACE('',(#12186),#3664,.F.);
#97160=ADVANCED_FACE('',(#12187),#3665,.F.);
#97161=ADVANCED_FACE('',(#12188),#6225,.F.);
#97162=ADVANCED_FACE('',(#12189),#91961,.F.);
#97163=ADVANCED_FACE('',(#12190),#3666,.F.);
#97164=ADVANCED_FACE('',(#12191),#91962,.F.);
#97165=ADVANCED_FACE('',(#12192),#91963,.F.);
#97166=ADVANCED_FACE('',(#12193),#3667,.F.);
#97167=ADVANCED_FACE('',(#12194),#3668,.F.);
#97168=ADVANCED_FACE('',(#12195),#91964,.F.);
#97169=ADVANCED_FACE('',(#12196),#91965,.F.);
#97170=ADVANCED_FACE('',(#12197),#3669,.F.);
#97171=ADVANCED_FACE('',(#12198),#91966,.F.);
#97172=ADVANCED_FACE('',(#12199),#91967,.F.);
#97173=ADVANCED_FACE('',(#12200),#3670,.F.);
#97174=ADVANCED_FACE('',(#12201),#91968,.F.);
#97175=ADVANCED_FACE('',(#12202),#91969,.F.);
#97176=ADVANCED_FACE('',(#12203),#3671,.F.);
#97177=ADVANCED_FACE('',(#12204),#3672,.F.);
#97178=ADVANCED_FACE('',(#12205),#91970,.F.);
#97179=ADVANCED_FACE('',(#12206),#91971,.F.);
#97180=ADVANCED_FACE('',(#12207),#3673,.F.);
#97181=ADVANCED_FACE('',(#12208),#91972,.F.);
#97182=ADVANCED_FACE('',(#12209),#6226,.F.);
#97183=ADVANCED_FACE('',(#12210),#3674,.F.);
#97184=ADVANCED_FACE('',(#12211),#3675,.F.);
#97185=ADVANCED_FACE('',(#12212),#91973,.F.);
#97186=ADVANCED_FACE('',(#12213),#91974,.F.);
#97187=ADVANCED_FACE('',(#12214),#3676,.F.);
#97188=ADVANCED_FACE('',(#12215),#3677,.F.);
#97189=ADVANCED_FACE('',(#12216),#6227,.F.);
#97190=ADVANCED_FACE('',(#12217),#91975,.F.);
#97191=ADVANCED_FACE('',(#12218),#3678,.F.);
#97192=ADVANCED_FACE('',(#12219),#91976,.F.);
#97193=ADVANCED_FACE('',(#12220),#91977,.F.);
#97194=ADVANCED_FACE('',(#12221),#3679,.F.);
#97195=ADVANCED_FACE('',(#12222),#3680,.F.);
#97196=ADVANCED_FACE('',(#12223),#91978,.F.);
#97197=ADVANCED_FACE('',(#12224),#91979,.F.);
#97198=ADVANCED_FACE('',(#12225),#3681,.F.);
#97199=ADVANCED_FACE('',(#12226),#91980,.F.);
#97200=ADVANCED_FACE('',(#12227),#91981,.F.);
#97201=ADVANCED_FACE('',(#12228),#3682,.F.);
#97202=ADVANCED_FACE('',(#12229),#91982,.F.);
#97203=ADVANCED_FACE('',(#12230),#91983,.F.);
#97204=ADVANCED_FACE('',(#12231),#3683,.F.);
#97205=ADVANCED_FACE('',(#12232),#3684,.F.);
#97206=ADVANCED_FACE('',(#12233),#91984,.F.);
#97207=ADVANCED_FACE('',(#12234),#91985,.F.);
#97208=ADVANCED_FACE('',(#12235),#3685,.F.);
#97209=ADVANCED_FACE('',(#12236),#91986,.F.);
#97210=ADVANCED_FACE('',(#12237),#6228,.F.);
#97211=ADVANCED_FACE('',(#12238),#3686,.F.);
#97212=ADVANCED_FACE('',(#12239),#3687,.F.);
#97213=ADVANCED_FACE('',(#12240),#91987,.F.);
#97214=ADVANCED_FACE('',(#12241),#91988,.F.);
#97215=ADVANCED_FACE('',(#12242),#3688,.F.);
#97216=ADVANCED_FACE('',(#12243),#3689,.F.);
#97217=ADVANCED_FACE('',(#12244),#6229,.F.);
#97218=ADVANCED_FACE('',(#12245),#91989,.F.);
#97219=ADVANCED_FACE('',(#12246),#3690,.F.);
#97220=ADVANCED_FACE('',(#12247),#91990,.F.);
#97221=ADVANCED_FACE('',(#12248),#91991,.F.);
#97222=ADVANCED_FACE('',(#12249),#3691,.F.);
#97223=ADVANCED_FACE('',(#12250),#3692,.F.);
#97224=ADVANCED_FACE('',(#12251),#91992,.F.);
#97225=ADVANCED_FACE('',(#12252),#91993,.F.);
#97226=ADVANCED_FACE('',(#12253),#3693,.F.);
#97227=ADVANCED_FACE('',(#12254),#91994,.F.);
#97228=ADVANCED_FACE('',(#12255),#91995,.F.);
#97229=ADVANCED_FACE('',(#12256),#3694,.F.);
#97230=ADVANCED_FACE('',(#12257),#91996,.F.);
#97231=ADVANCED_FACE('',(#12258),#91997,.F.);
#97232=ADVANCED_FACE('',(#12259),#3695,.F.);
#97233=ADVANCED_FACE('',(#12260),#3696,.F.);
#97234=ADVANCED_FACE('',(#12261),#91998,.F.);
#97235=ADVANCED_FACE('',(#12262),#91999,.F.);
#97236=ADVANCED_FACE('',(#12263),#3697,.F.);
#97237=ADVANCED_FACE('',(#12264),#92000,.F.);
#97238=ADVANCED_FACE('',(#12265),#6230,.F.);
#97239=ADVANCED_FACE('',(#12266),#3698,.F.);
#97240=ADVANCED_FACE('',(#12267),#3699,.F.);
#97241=ADVANCED_FACE('',(#12268),#92001,.F.);
#97242=ADVANCED_FACE('',(#12269),#92002,.F.);
#97243=ADVANCED_FACE('',(#12270),#3700,.F.);
#97244=ADVANCED_FACE('',(#12271),#3701,.F.);
#97245=ADVANCED_FACE('',(#12272),#6231,.F.);
#97246=ADVANCED_FACE('',(#12273),#92003,.F.);
#97247=ADVANCED_FACE('',(#12274),#3702,.F.);
#97248=ADVANCED_FACE('',(#12275),#92004,.F.);
#97249=ADVANCED_FACE('',(#12276),#92005,.F.);
#97250=ADVANCED_FACE('',(#12277),#3703,.F.);
#97251=ADVANCED_FACE('',(#12278),#3704,.F.);
#97252=ADVANCED_FACE('',(#12279),#92006,.F.);
#97253=ADVANCED_FACE('',(#12280),#92007,.F.);
#97254=ADVANCED_FACE('',(#12281),#3705,.F.);
#97255=ADVANCED_FACE('',(#12282),#92008,.F.);
#97256=ADVANCED_FACE('',(#12283),#92009,.F.);
#97257=ADVANCED_FACE('',(#12284),#3706,.F.);
#97258=ADVANCED_FACE('',(#12285),#92010,.F.);
#97259=ADVANCED_FACE('',(#12286),#92011,.F.);
#97260=ADVANCED_FACE('',(#12287),#3707,.F.);
#97261=ADVANCED_FACE('',(#12288),#3708,.F.);
#97262=ADVANCED_FACE('',(#12289),#92012,.F.);
#97263=ADVANCED_FACE('',(#12290),#92013,.F.);
#97264=ADVANCED_FACE('',(#12291),#3709,.F.);
#97265=ADVANCED_FACE('',(#12292),#92014,.F.);
#97266=ADVANCED_FACE('',(#12293),#6232,.F.);
#97267=ADVANCED_FACE('',(#12294),#3710,.F.);
#97268=ADVANCED_FACE('',(#12295),#3711,.F.);
#97269=ADVANCED_FACE('',(#12296),#92015,.F.);
#97270=ADVANCED_FACE('',(#12297),#92016,.F.);
#97271=ADVANCED_FACE('',(#12298),#3712,.F.);
#97272=ADVANCED_FACE('',(#12299),#3713,.F.);
#97273=ADVANCED_FACE('',(#12300),#6233,.F.);
#97274=ADVANCED_FACE('',(#12301),#92017,.F.);
#97275=ADVANCED_FACE('',(#12302),#3714,.F.);
#97276=ADVANCED_FACE('',(#12303),#92018,.F.);
#97277=ADVANCED_FACE('',(#12304),#92019,.F.);
#97278=ADVANCED_FACE('',(#12305),#3715,.F.);
#97279=ADVANCED_FACE('',(#12306),#3716,.F.);
#97280=ADVANCED_FACE('',(#12307),#92020,.F.);
#97281=ADVANCED_FACE('',(#12308),#92021,.F.);
#97282=ADVANCED_FACE('',(#12309),#3717,.F.);
#97283=ADVANCED_FACE('',(#12310),#92022,.F.);
#97284=ADVANCED_FACE('',(#12311),#92023,.F.);
#97285=ADVANCED_FACE('',(#12312),#3718,.F.);
#97286=ADVANCED_FACE('',(#12313),#92024,.F.);
#97287=ADVANCED_FACE('',(#12314),#92025,.F.);
#97288=ADVANCED_FACE('',(#12315),#3719,.F.);
#97289=ADVANCED_FACE('',(#12316),#3720,.F.);
#97290=ADVANCED_FACE('',(#12317),#92026,.F.);
#97291=ADVANCED_FACE('',(#12318),#92027,.F.);
#97292=ADVANCED_FACE('',(#12319),#3721,.F.);
#97293=ADVANCED_FACE('',(#12320),#92028,.F.);
#97294=ADVANCED_FACE('',(#12321),#6234,.F.);
#97295=ADVANCED_FACE('',(#12322),#3722,.F.);
#97296=ADVANCED_FACE('',(#12323),#3723,.F.);
#97297=ADVANCED_FACE('',(#12324),#92029,.F.);
#97298=ADVANCED_FACE('',(#12325),#92030,.F.);
#97299=ADVANCED_FACE('',(#12326),#3724,.F.);
#97300=ADVANCED_FACE('',(#12327),#3725,.F.);
#97301=ADVANCED_FACE('',(#12328),#6235,.F.);
#97302=ADVANCED_FACE('',(#12329),#92031,.F.);
#97303=ADVANCED_FACE('',(#12330),#3726,.F.);
#97304=ADVANCED_FACE('',(#12331),#92032,.F.);
#97305=ADVANCED_FACE('',(#12332),#92033,.F.);
#97306=ADVANCED_FACE('',(#12333),#3727,.F.);
#97307=ADVANCED_FACE('',(#12334),#3728,.F.);
#97308=ADVANCED_FACE('',(#12335),#92034,.F.);
#97309=ADVANCED_FACE('',(#12336),#92035,.F.);
#97310=ADVANCED_FACE('',(#12337),#3729,.F.);
#97311=ADVANCED_FACE('',(#12338),#92036,.F.);
#97312=ADVANCED_FACE('',(#12339),#92037,.F.);
#97313=ADVANCED_FACE('',(#12340),#3730,.F.);
#97314=ADVANCED_FACE('',(#12341),#92038,.F.);
#97315=ADVANCED_FACE('',(#12342),#92039,.F.);
#97316=ADVANCED_FACE('',(#12343),#3731,.F.);
#97317=ADVANCED_FACE('',(#12344),#3732,.F.);
#97318=ADVANCED_FACE('',(#12345),#92040,.F.);
#97319=ADVANCED_FACE('',(#12346),#92041,.F.);
#97320=ADVANCED_FACE('',(#12347),#3733,.F.);
#97321=ADVANCED_FACE('',(#12348),#92042,.F.);
#97322=ADVANCED_FACE('',(#12349),#6236,.F.);
#97323=ADVANCED_FACE('',(#12350),#3734,.F.);
#97324=ADVANCED_FACE('',(#12351),#3735,.F.);
#97325=ADVANCED_FACE('',(#12352),#92043,.F.);
#97326=ADVANCED_FACE('',(#12353),#92044,.F.);
#97327=ADVANCED_FACE('',(#12354),#3736,.F.);
#97328=ADVANCED_FACE('',(#12355),#3737,.F.);
#97329=ADVANCED_FACE('',(#12356),#6237,.F.);
#97330=ADVANCED_FACE('',(#12357),#92045,.F.);
#97331=ADVANCED_FACE('',(#12358),#3738,.F.);
#97332=ADVANCED_FACE('',(#12359),#92046,.F.);
#97333=ADVANCED_FACE('',(#12360),#92047,.F.);
#97334=ADVANCED_FACE('',(#12361),#3739,.F.);
#97335=ADVANCED_FACE('',(#12362),#3740,.F.);
#97336=ADVANCED_FACE('',(#12363),#92048,.F.);
#97337=ADVANCED_FACE('',(#12364),#92049,.F.);
#97338=ADVANCED_FACE('',(#12365),#3741,.F.);
#97339=ADVANCED_FACE('',(#12366),#92050,.F.);
#97340=ADVANCED_FACE('',(#12367),#92051,.F.);
#97341=ADVANCED_FACE('',(#12368),#3742,.F.);
#97342=ADVANCED_FACE('',(#12369),#92052,.F.);
#97343=ADVANCED_FACE('',(#12370),#92053,.F.);
#97344=ADVANCED_FACE('',(#12371),#3743,.F.);
#97345=ADVANCED_FACE('',(#12372),#3744,.F.);
#97346=ADVANCED_FACE('',(#12373),#92054,.F.);
#97347=ADVANCED_FACE('',(#12374),#92055,.F.);
#97348=ADVANCED_FACE('',(#12375),#3745,.F.);
#97349=ADVANCED_FACE('',(#12376),#92056,.F.);
#97350=ADVANCED_FACE('',(#12377),#6238,.F.);
#97351=ADVANCED_FACE('',(#12378),#3746,.F.);
#97352=ADVANCED_FACE('',(#12379),#3747,.F.);
#97353=ADVANCED_FACE('',(#12380),#92057,.F.);
#97354=ADVANCED_FACE('',(#12381),#92058,.F.);
#97355=ADVANCED_FACE('',(#12382),#3748,.F.);
#97356=ADVANCED_FACE('',(#12383),#3749,.F.);
#97357=ADVANCED_FACE('',(#12384),#6239,.F.);
#97358=ADVANCED_FACE('',(#12385),#92059,.F.);
#97359=ADVANCED_FACE('',(#12386),#3750,.F.);
#97360=ADVANCED_FACE('',(#12387),#92060,.F.);
#97361=ADVANCED_FACE('',(#12388),#92061,.F.);
#97362=ADVANCED_FACE('',(#12389),#3751,.F.);
#97363=ADVANCED_FACE('',(#12390),#3752,.F.);
#97364=ADVANCED_FACE('',(#12391),#92062,.F.);
#97365=ADVANCED_FACE('',(#12392),#92063,.F.);
#97366=ADVANCED_FACE('',(#12393),#3753,.F.);
#97367=ADVANCED_FACE('',(#12394),#92064,.F.);
#97368=ADVANCED_FACE('',(#12395),#92065,.F.);
#97369=ADVANCED_FACE('',(#12396),#3754,.F.);
#97370=ADVANCED_FACE('',(#12397),#92066,.F.);
#97371=ADVANCED_FACE('',(#12398),#92067,.F.);
#97372=ADVANCED_FACE('',(#12399),#3755,.F.);
#97373=ADVANCED_FACE('',(#12400),#3756,.F.);
#97374=ADVANCED_FACE('',(#12401),#92068,.F.);
#97375=ADVANCED_FACE('',(#12402),#92069,.F.);
#97376=ADVANCED_FACE('',(#12403),#3757,.F.);
#97377=ADVANCED_FACE('',(#12404),#92070,.F.);
#97378=ADVANCED_FACE('',(#12405),#6240,.F.);
#97379=ADVANCED_FACE('',(#12406),#3758,.F.);
#97380=ADVANCED_FACE('',(#12407),#3759,.F.);
#97381=ADVANCED_FACE('',(#12408),#92071,.F.);
#97382=ADVANCED_FACE('',(#12409),#92072,.F.);
#97383=ADVANCED_FACE('',(#12410),#3760,.F.);
#97384=ADVANCED_FACE('',(#12411),#3761,.F.);
#97385=ADVANCED_FACE('',(#12412),#6241,.F.);
#97386=ADVANCED_FACE('',(#12413),#92073,.F.);
#97387=ADVANCED_FACE('',(#12414),#3762,.F.);
#97388=ADVANCED_FACE('',(#12415),#92074,.F.);
#97389=ADVANCED_FACE('',(#12416),#92075,.F.);
#97390=ADVANCED_FACE('',(#12417),#3763,.F.);
#97391=ADVANCED_FACE('',(#12418),#3764,.F.);
#97392=ADVANCED_FACE('',(#12419),#92076,.F.);
#97393=ADVANCED_FACE('',(#12420),#92077,.F.);
#97394=ADVANCED_FACE('',(#12421),#3765,.F.);
#97395=ADVANCED_FACE('',(#12422),#92078,.F.);
#97396=ADVANCED_FACE('',(#12423),#92079,.F.);
#97397=ADVANCED_FACE('',(#12424),#3766,.F.);
#97398=ADVANCED_FACE('',(#12425),#92080,.F.);
#97399=ADVANCED_FACE('',(#12426),#92081,.F.);
#97400=ADVANCED_FACE('',(#12427),#3767,.F.);
#97401=ADVANCED_FACE('',(#12428),#3768,.F.);
#97402=ADVANCED_FACE('',(#12429),#92082,.F.);
#97403=ADVANCED_FACE('',(#12430),#92083,.F.);
#97404=ADVANCED_FACE('',(#12431),#3769,.F.);
#97405=ADVANCED_FACE('',(#12432),#92084,.F.);
#97406=ADVANCED_FACE('',(#12433),#3770,.F.);
#97407=ADVANCED_FACE('',(#12434),#3771,.F.);
#97408=ADVANCED_FACE('',(#12435),#92085,.F.);
#97409=ADVANCED_FACE('',(#12436),#92086,.F.);
#97410=ADVANCED_FACE('',(#12437),#3772,.F.);
#97411=ADVANCED_FACE('',(#12438),#3773,.F.);
#97412=ADVANCED_FACE('',(#12439),#92087,.F.);
#97413=ADVANCED_FACE('',(#12440),#3774,.F.);
#97414=ADVANCED_FACE('',(#12441),#92088,.F.);
#97415=ADVANCED_FACE('',(#12442),#92089,.F.);
#97416=ADVANCED_FACE('',(#12443),#3775,.F.);
#97417=ADVANCED_FACE('',(#12444),#3776,.F.);
#97418=ADVANCED_FACE('',(#12445),#92090,.F.);
#97419=ADVANCED_FACE('',(#12446),#92091,.F.);
#97420=ADVANCED_FACE('',(#12447),#3777,.F.);
#97421=ADVANCED_FACE('',(#12448),#92092,.F.);
#97422=ADVANCED_FACE('',(#12449),#92093,.F.);
#97423=ADVANCED_FACE('',(#12450),#3778,.F.);
#97424=ADVANCED_FACE('',(#12451),#92094,.F.);
#97425=ADVANCED_FACE('',(#12452),#92095,.F.);
#97426=ADVANCED_FACE('',(#12453),#3779,.F.);
#97427=ADVANCED_FACE('',(#12454),#3780,.F.);
#97428=ADVANCED_FACE('',(#12455),#92096,.F.);
#97429=ADVANCED_FACE('',(#12456),#92097,.F.);
#97430=ADVANCED_FACE('',(#12457),#3781,.F.);
#97431=ADVANCED_FACE('',(#12458),#92098,.F.);
#97432=ADVANCED_FACE('',(#12459),#6242,.F.);
#97433=ADVANCED_FACE('',(#12460),#3782,.F.);
#97434=ADVANCED_FACE('',(#12461),#3783,.F.);
#97435=ADVANCED_FACE('',(#12462),#92099,.F.);
#97436=ADVANCED_FACE('',(#12463),#92100,.F.);
#97437=ADVANCED_FACE('',(#12464),#3784,.F.);
#97438=ADVANCED_FACE('',(#12465),#3785,.F.);
#97439=ADVANCED_FACE('',(#12466),#6243,.F.);
#97440=ADVANCED_FACE('',(#12467),#92101,.F.);
#97441=ADVANCED_FACE('',(#12468),#3786,.F.);
#97442=ADVANCED_FACE('',(#12469),#92102,.F.);
#97443=ADVANCED_FACE('',(#12470),#92103,.F.);
#97444=ADVANCED_FACE('',(#12471),#3787,.F.);
#97445=ADVANCED_FACE('',(#12472),#3788,.F.);
#97446=ADVANCED_FACE('',(#12473),#92104,.F.);
#97447=ADVANCED_FACE('',(#12474),#92105,.F.);
#97448=ADVANCED_FACE('',(#12475),#3789,.F.);
#97449=ADVANCED_FACE('',(#12476),#92106,.F.);
#97450=ADVANCED_FACE('',(#12477),#92107,.F.);
#97451=ADVANCED_FACE('',(#12478),#3790,.F.);
#97452=ADVANCED_FACE('',(#12479),#92108,.F.);
#97453=ADVANCED_FACE('',(#12480),#92109,.F.);
#97454=ADVANCED_FACE('',(#12481),#3791,.F.);
#97455=ADVANCED_FACE('',(#12482),#3792,.F.);
#97456=ADVANCED_FACE('',(#12483),#92110,.F.);
#97457=ADVANCED_FACE('',(#12484),#92111,.F.);
#97458=ADVANCED_FACE('',(#12485),#3793,.F.);
#97459=ADVANCED_FACE('',(#12486),#92112,.F.);
#97460=ADVANCED_FACE('',(#12487),#6244,.F.);
#97461=ADVANCED_FACE('',(#12488),#3794,.F.);
#97462=ADVANCED_FACE('',(#12489),#3795,.F.);
#97463=ADVANCED_FACE('',(#12490),#92113,.F.);
#97464=ADVANCED_FACE('',(#12491),#92114,.F.);
#97465=ADVANCED_FACE('',(#12492),#3796,.F.);
#97466=ADVANCED_FACE('',(#12493),#3797,.F.);
#97467=ADVANCED_FACE('',(#12494),#6245,.F.);
#97468=ADVANCED_FACE('',(#12495),#92115,.F.);
#97469=ADVANCED_FACE('',(#12496),#3798,.F.);
#97470=ADVANCED_FACE('',(#12497),#92116,.F.);
#97471=ADVANCED_FACE('',(#12498),#92117,.F.);
#97472=ADVANCED_FACE('',(#12499),#3799,.F.);
#97473=ADVANCED_FACE('',(#12500),#3800,.F.);
#97474=ADVANCED_FACE('',(#12501),#92118,.F.);
#97475=ADVANCED_FACE('',(#12502),#92119,.F.);
#97476=ADVANCED_FACE('',(#12503),#3801,.F.);
#97477=ADVANCED_FACE('',(#12504),#92120,.F.);
#97478=ADVANCED_FACE('',(#12505),#92121,.F.);
#97479=ADVANCED_FACE('',(#12506),#3802,.F.);
#97480=ADVANCED_FACE('',(#12507),#92122,.F.);
#97481=ADVANCED_FACE('',(#12508),#92123,.F.);
#97482=ADVANCED_FACE('',(#12509),#3803,.F.);
#97483=ADVANCED_FACE('',(#12510),#3804,.F.);
#97484=ADVANCED_FACE('',(#12511),#92124,.F.);
#97485=ADVANCED_FACE('',(#12512),#92125,.F.);
#97486=ADVANCED_FACE('',(#12513),#3805,.F.);
#97487=ADVANCED_FACE('',(#12514),#92126,.F.);
#97488=ADVANCED_FACE('',(#12515),#6246,.F.);
#97489=ADVANCED_FACE('',(#12516),#3806,.F.);
#97490=ADVANCED_FACE('',(#12517),#3807,.F.);
#97491=ADVANCED_FACE('',(#12518),#92127,.F.);
#97492=ADVANCED_FACE('',(#12519),#92128,.F.);
#97493=ADVANCED_FACE('',(#12520),#3808,.F.);
#97494=ADVANCED_FACE('',(#12521),#3809,.F.);
#97495=ADVANCED_FACE('',(#12522),#6247,.F.);
#97496=ADVANCED_FACE('',(#12523),#92129,.F.);
#97497=ADVANCED_FACE('',(#12524),#3810,.F.);
#97498=ADVANCED_FACE('',(#12525),#92130,.F.);
#97499=ADVANCED_FACE('',(#12526),#92131,.F.);
#97500=ADVANCED_FACE('',(#12527),#3811,.F.);
#97501=ADVANCED_FACE('',(#12528),#3812,.F.);
#97502=ADVANCED_FACE('',(#12529),#92132,.F.);
#97503=ADVANCED_FACE('',(#12530),#92133,.F.);
#97504=ADVANCED_FACE('',(#12531),#3813,.F.);
#97505=ADVANCED_FACE('',(#12532),#92134,.F.);
#97506=ADVANCED_FACE('',(#12533),#92135,.F.);
#97507=ADVANCED_FACE('',(#12534),#3814,.F.);
#97508=ADVANCED_FACE('',(#12535),#92136,.F.);
#97509=ADVANCED_FACE('',(#12536),#92137,.F.);
#97510=ADVANCED_FACE('',(#12537),#3815,.F.);
#97511=ADVANCED_FACE('',(#12538),#3816,.F.);
#97512=ADVANCED_FACE('',(#12539),#92138,.F.);
#97513=ADVANCED_FACE('',(#12540),#92139,.F.);
#97514=ADVANCED_FACE('',(#12541),#3817,.F.);
#97515=ADVANCED_FACE('',(#12542),#92140,.F.);
#97516=ADVANCED_FACE('',(#12543),#6248,.F.);
#97517=ADVANCED_FACE('',(#12544),#3818,.F.);
#97518=ADVANCED_FACE('',(#12545),#3819,.F.);
#97519=ADVANCED_FACE('',(#12546),#92141,.F.);
#97520=ADVANCED_FACE('',(#12547),#92142,.F.);
#97521=ADVANCED_FACE('',(#12548),#3820,.F.);
#97522=ADVANCED_FACE('',(#12549),#3821,.F.);
#97523=ADVANCED_FACE('',(#12550),#6249,.F.);
#97524=ADVANCED_FACE('',(#12551),#92143,.F.);
#97525=ADVANCED_FACE('',(#12552),#3822,.F.);
#97526=ADVANCED_FACE('',(#12553),#92144,.F.);
#97527=ADVANCED_FACE('',(#12554),#92145,.F.);
#97528=ADVANCED_FACE('',(#12555),#3823,.F.);
#97529=ADVANCED_FACE('',(#12556),#3824,.F.);
#97530=ADVANCED_FACE('',(#12557),#92146,.F.);
#97531=ADVANCED_FACE('',(#12558),#92147,.F.);
#97532=ADVANCED_FACE('',(#12559),#3825,.F.);
#97533=ADVANCED_FACE('',(#12560),#92148,.F.);
#97534=ADVANCED_FACE('',(#12561),#92149,.F.);
#97535=ADVANCED_FACE('',(#12562),#3826,.F.);
#97536=ADVANCED_FACE('',(#12563),#92150,.F.);
#97537=ADVANCED_FACE('',(#12564),#92151,.F.);
#97538=ADVANCED_FACE('',(#12565),#3827,.F.);
#97539=ADVANCED_FACE('',(#12566),#3828,.F.);
#97540=ADVANCED_FACE('',(#12567),#92152,.F.);
#97541=ADVANCED_FACE('',(#12568),#92153,.F.);
#97542=ADVANCED_FACE('',(#12569),#3829,.F.);
#97543=ADVANCED_FACE('',(#12570),#92154,.F.);
#97544=ADVANCED_FACE('',(#12571),#6250,.F.);
#97545=ADVANCED_FACE('',(#12572),#3830,.F.);
#97546=ADVANCED_FACE('',(#12573),#3831,.F.);
#97547=ADVANCED_FACE('',(#12574),#92155,.F.);
#97548=ADVANCED_FACE('',(#12575),#92156,.F.);
#97549=ADVANCED_FACE('',(#12576),#3832,.F.);
#97550=ADVANCED_FACE('',(#12577),#3833,.F.);
#97551=ADVANCED_FACE('',(#12578),#6251,.F.);
#97552=ADVANCED_FACE('',(#12579),#92157,.F.);
#97553=ADVANCED_FACE('',(#12580),#3834,.F.);
#97554=ADVANCED_FACE('',(#12581),#92158,.F.);
#97555=ADVANCED_FACE('',(#12582),#92159,.F.);
#97556=ADVANCED_FACE('',(#12583),#3835,.F.);
#97557=ADVANCED_FACE('',(#12584),#3836,.F.);
#97558=ADVANCED_FACE('',(#12585),#92160,.F.);
#97559=ADVANCED_FACE('',(#12586),#92161,.F.);
#97560=ADVANCED_FACE('',(#12587),#3837,.F.);
#97561=ADVANCED_FACE('',(#12588),#92162,.F.);
#97562=ADVANCED_FACE('',(#12589),#92163,.F.);
#97563=ADVANCED_FACE('',(#12590),#3838,.F.);
#97564=ADVANCED_FACE('',(#12591),#92164,.F.);
#97565=ADVANCED_FACE('',(#12592),#92165,.F.);
#97566=ADVANCED_FACE('',(#12593),#3839,.F.);
#97567=ADVANCED_FACE('',(#12594),#3840,.F.);
#97568=ADVANCED_FACE('',(#12595),#92166,.F.);
#97569=ADVANCED_FACE('',(#12596),#92167,.F.);
#97570=ADVANCED_FACE('',(#12597),#3841,.F.);
#97571=ADVANCED_FACE('',(#12598),#92168,.F.);
#97572=ADVANCED_FACE('',(#12599),#6252,.F.);
#97573=ADVANCED_FACE('',(#12600),#3842,.F.);
#97574=ADVANCED_FACE('',(#12601),#3843,.F.);
#97575=ADVANCED_FACE('',(#12602),#92169,.F.);
#97576=ADVANCED_FACE('',(#12603),#92170,.F.);
#97577=ADVANCED_FACE('',(#12604),#3844,.F.);
#97578=ADVANCED_FACE('',(#12605),#3845,.F.);
#97579=ADVANCED_FACE('',(#12606),#6253,.F.);
#97580=ADVANCED_FACE('',(#12607),#92171,.F.);
#97581=ADVANCED_FACE('',(#12608),#3846,.F.);
#97582=ADVANCED_FACE('',(#12609),#92172,.F.);
#97583=ADVANCED_FACE('',(#12610),#92173,.F.);
#97584=ADVANCED_FACE('',(#12611),#3847,.F.);
#97585=ADVANCED_FACE('',(#12612),#3848,.F.);
#97586=ADVANCED_FACE('',(#12613),#92174,.F.);
#97587=ADVANCED_FACE('',(#12614),#92175,.F.);
#97588=ADVANCED_FACE('',(#12615),#3849,.F.);
#97589=ADVANCED_FACE('',(#12616),#92176,.F.);
#97590=ADVANCED_FACE('',(#12617),#92177,.F.);
#97591=ADVANCED_FACE('',(#12618),#3850,.F.);
#97592=ADVANCED_FACE('',(#12619),#92178,.F.);
#97593=ADVANCED_FACE('',(#12620),#92179,.F.);
#97594=ADVANCED_FACE('',(#12621),#3851,.F.);
#97595=ADVANCED_FACE('',(#12622),#3852,.F.);
#97596=ADVANCED_FACE('',(#12623),#92180,.F.);
#97597=ADVANCED_FACE('',(#12624),#92181,.F.);
#97598=ADVANCED_FACE('',(#12625),#3853,.F.);
#97599=ADVANCED_FACE('',(#12626),#92182,.F.);
#97600=ADVANCED_FACE('',(#12627),#6254,.F.);
#97601=ADVANCED_FACE('',(#12628),#3854,.F.);
#97602=ADVANCED_FACE('',(#12629),#3855,.F.);
#97603=ADVANCED_FACE('',(#12630),#92183,.F.);
#97604=ADVANCED_FACE('',(#12631),#92184,.F.);
#97605=ADVANCED_FACE('',(#12632),#3856,.F.);
#97606=ADVANCED_FACE('',(#12633),#3857,.F.);
#97607=ADVANCED_FACE('',(#12634),#6255,.F.);
#97608=ADVANCED_FACE('',(#12635),#92185,.F.);
#97609=ADVANCED_FACE('',(#12636),#3858,.F.);
#97610=ADVANCED_FACE('',(#12637),#92186,.F.);
#97611=ADVANCED_FACE('',(#12638),#92187,.F.);
#97612=ADVANCED_FACE('',(#12639),#3859,.F.);
#97613=ADVANCED_FACE('',(#12640),#3860,.F.);
#97614=ADVANCED_FACE('',(#12641),#92188,.F.);
#97615=ADVANCED_FACE('',(#12642),#92189,.F.);
#97616=ADVANCED_FACE('',(#12643),#3861,.F.);
#97617=ADVANCED_FACE('',(#12644),#92190,.F.);
#97618=ADVANCED_FACE('',(#12645),#92191,.F.);
#97619=ADVANCED_FACE('',(#12646),#3862,.F.);
#97620=ADVANCED_FACE('',(#12647),#92192,.F.);
#97621=ADVANCED_FACE('',(#12648),#92193,.F.);
#97622=ADVANCED_FACE('',(#12649),#3863,.F.);
#97623=ADVANCED_FACE('',(#12650),#3864,.F.);
#97624=ADVANCED_FACE('',(#12651),#92194,.F.);
#97625=ADVANCED_FACE('',(#12652),#92195,.F.);
#97626=ADVANCED_FACE('',(#12653),#3865,.F.);
#97627=ADVANCED_FACE('',(#12654),#92196,.F.);
#97628=ADVANCED_FACE('',(#12655),#6256,.F.);
#97629=ADVANCED_FACE('',(#12656),#3866,.F.);
#97630=ADVANCED_FACE('',(#12657),#3867,.F.);
#97631=ADVANCED_FACE('',(#12658),#92197,.F.);
#97632=ADVANCED_FACE('',(#12659),#92198,.F.);
#97633=ADVANCED_FACE('',(#12660),#3868,.F.);
#97634=ADVANCED_FACE('',(#12661),#3869,.F.);
#97635=ADVANCED_FACE('',(#12662),#6257,.F.);
#97636=ADVANCED_FACE('',(#12663),#92199,.F.);
#97637=ADVANCED_FACE('',(#12664),#3870,.F.);
#97638=ADVANCED_FACE('',(#12665),#92200,.F.);
#97639=ADVANCED_FACE('',(#12666),#92201,.F.);
#97640=ADVANCED_FACE('',(#12667),#3871,.F.);
#97641=ADVANCED_FACE('',(#12668),#3872,.F.);
#97642=ADVANCED_FACE('',(#12669),#92202,.F.);
#97643=ADVANCED_FACE('',(#12670),#92203,.F.);
#97644=ADVANCED_FACE('',(#12671),#3873,.F.);
#97645=ADVANCED_FACE('',(#12672),#92204,.F.);
#97646=ADVANCED_FACE('',(#12673),#92205,.F.);
#97647=ADVANCED_FACE('',(#12674),#3874,.F.);
#97648=ADVANCED_FACE('',(#12675),#92206,.F.);
#97649=ADVANCED_FACE('',(#12676),#92207,.F.);
#97650=ADVANCED_FACE('',(#12677),#3875,.F.);
#97651=ADVANCED_FACE('',(#12678),#3876,.F.);
#97652=ADVANCED_FACE('',(#12679),#92208,.F.);
#97653=ADVANCED_FACE('',(#12680),#92209,.F.);
#97654=ADVANCED_FACE('',(#12681),#3877,.F.);
#97655=ADVANCED_FACE('',(#12682),#92210,.F.);
#97656=ADVANCED_FACE('',(#12683),#6258,.F.);
#97657=ADVANCED_FACE('',(#12684),#3878,.F.);
#97658=ADVANCED_FACE('',(#12685),#3879,.F.);
#97659=ADVANCED_FACE('',(#12686),#92211,.F.);
#97660=ADVANCED_FACE('',(#12687),#92212,.F.);
#97661=ADVANCED_FACE('',(#12688),#3880,.F.);
#97662=ADVANCED_FACE('',(#12689),#3881,.F.);
#97663=ADVANCED_FACE('',(#12690),#6259,.F.);
#97664=ADVANCED_FACE('',(#12691),#92213,.F.);
#97665=ADVANCED_FACE('',(#12692),#3882,.F.);
#97666=ADVANCED_FACE('',(#12693),#92214,.F.);
#97667=ADVANCED_FACE('',(#12694),#92215,.F.);
#97668=ADVANCED_FACE('',(#12695),#3883,.F.);
#97669=ADVANCED_FACE('',(#12696),#3884,.F.);
#97670=ADVANCED_FACE('',(#12697),#92216,.F.);
#97671=ADVANCED_FACE('',(#12698),#92217,.F.);
#97672=ADVANCED_FACE('',(#12699),#3885,.F.);
#97673=ADVANCED_FACE('',(#12700),#92218,.F.);
#97674=ADVANCED_FACE('',(#12701),#92219,.F.);
#97675=ADVANCED_FACE('',(#12702),#3886,.F.);
#97676=ADVANCED_FACE('',(#12703),#92220,.F.);
#97677=ADVANCED_FACE('',(#12704),#92221,.F.);
#97678=ADVANCED_FACE('',(#12705),#3887,.F.);
#97679=ADVANCED_FACE('',(#12706),#3888,.F.);
#97680=ADVANCED_FACE('',(#12707),#92222,.F.);
#97681=ADVANCED_FACE('',(#12708),#92223,.F.);
#97682=ADVANCED_FACE('',(#12709),#3889,.F.);
#97683=ADVANCED_FACE('',(#12710),#92224,.F.);
#97684=ADVANCED_FACE('',(#12711),#6260,.F.);
#97685=ADVANCED_FACE('',(#12712),#3890,.F.);
#97686=ADVANCED_FACE('',(#12713),#3891,.F.);
#97687=ADVANCED_FACE('',(#12714),#92225,.F.);
#97688=ADVANCED_FACE('',(#12715),#92226,.F.);
#97689=ADVANCED_FACE('',(#12716),#3892,.F.);
#97690=ADVANCED_FACE('',(#12717),#3893,.F.);
#97691=ADVANCED_FACE('',(#12718),#6261,.F.);
#97692=ADVANCED_FACE('',(#12719),#92227,.F.);
#97693=ADVANCED_FACE('',(#12720),#3894,.F.);
#97694=ADVANCED_FACE('',(#12721),#92228,.F.);
#97695=ADVANCED_FACE('',(#12722),#92229,.F.);
#97696=ADVANCED_FACE('',(#12723),#3895,.F.);
#97697=ADVANCED_FACE('',(#12724),#3896,.F.);
#97698=ADVANCED_FACE('',(#12725),#92230,.F.);
#97699=ADVANCED_FACE('',(#12726),#92231,.F.);
#97700=ADVANCED_FACE('',(#12727),#3897,.F.);
#97701=ADVANCED_FACE('',(#12728),#92232,.F.);
#97702=ADVANCED_FACE('',(#12729),#92233,.F.);
#97703=ADVANCED_FACE('',(#12730),#3898,.F.);
#97704=ADVANCED_FACE('',(#12731),#92234,.F.);
#97705=ADVANCED_FACE('',(#12732),#92235,.F.);
#97706=ADVANCED_FACE('',(#12733),#3899,.F.);
#97707=ADVANCED_FACE('',(#12734),#3900,.F.);
#97708=ADVANCED_FACE('',(#12735),#92236,.F.);
#97709=ADVANCED_FACE('',(#12736),#92237,.F.);
#97710=ADVANCED_FACE('',(#12737),#3901,.F.);
#97711=ADVANCED_FACE('',(#12738),#92238,.F.);
#97712=ADVANCED_FACE('',(#12739),#6262,.F.);
#97713=ADVANCED_FACE('',(#12740),#3902,.F.);
#97714=ADVANCED_FACE('',(#12741),#3903,.F.);
#97715=ADVANCED_FACE('',(#12742),#92239,.F.);
#97716=ADVANCED_FACE('',(#12743),#92240,.F.);
#97717=ADVANCED_FACE('',(#12744),#3904,.F.);
#97718=ADVANCED_FACE('',(#12745),#3905,.F.);
#97719=ADVANCED_FACE('',(#12746),#6263,.F.);
#97720=ADVANCED_FACE('',(#12747),#92241,.F.);
#97721=ADVANCED_FACE('',(#12748),#3906,.F.);
#97722=ADVANCED_FACE('',(#12749),#92242,.F.);
#97723=ADVANCED_FACE('',(#12750),#92243,.F.);
#97724=ADVANCED_FACE('',(#12751),#3907,.F.);
#97725=ADVANCED_FACE('',(#12752),#3908,.F.);
#97726=ADVANCED_FACE('',(#12753),#92244,.F.);
#97727=ADVANCED_FACE('',(#12754),#92245,.F.);
#97728=ADVANCED_FACE('',(#12755),#3909,.F.);
#97729=ADVANCED_FACE('',(#12756),#92246,.F.);
#97730=ADVANCED_FACE('',(#12757),#92247,.F.);
#97731=ADVANCED_FACE('',(#12758),#3910,.F.);
#97732=ADVANCED_FACE('',(#12759),#92248,.F.);
#97733=ADVANCED_FACE('',(#12760),#92249,.F.);
#97734=ADVANCED_FACE('',(#12761),#3911,.F.);
#97735=ADVANCED_FACE('',(#12762),#3912,.F.);
#97736=ADVANCED_FACE('',(#12763),#92250,.F.);
#97737=ADVANCED_FACE('',(#12764),#92251,.F.);
#97738=ADVANCED_FACE('',(#12765),#3913,.F.);
#97739=ADVANCED_FACE('',(#12766),#92252,.F.);
#97740=ADVANCED_FACE('',(#12767),#6264,.F.);
#97741=ADVANCED_FACE('',(#12768),#3914,.F.);
#97742=ADVANCED_FACE('',(#12769),#3915,.F.);
#97743=ADVANCED_FACE('',(#12770),#92253,.F.);
#97744=ADVANCED_FACE('',(#12771),#92254,.F.);
#97745=ADVANCED_FACE('',(#12772),#3916,.F.);
#97746=ADVANCED_FACE('',(#12773),#3917,.F.);
#97747=ADVANCED_FACE('',(#12774),#6265,.F.);
#97748=ADVANCED_FACE('',(#12775),#92255,.F.);
#97749=ADVANCED_FACE('',(#12776),#3918,.F.);
#97750=ADVANCED_FACE('',(#12777),#92256,.F.);
#97751=ADVANCED_FACE('',(#12778),#92257,.F.);
#97752=ADVANCED_FACE('',(#12779),#3919,.F.);
#97753=ADVANCED_FACE('',(#12780),#3920,.F.);
#97754=ADVANCED_FACE('',(#12781),#92258,.F.);
#97755=ADVANCED_FACE('',(#12782),#92259,.F.);
#97756=ADVANCED_FACE('',(#12783),#3921,.F.);
#97757=ADVANCED_FACE('',(#12784),#92260,.F.);
#97758=ADVANCED_FACE('',(#12785),#92261,.F.);
#97759=ADVANCED_FACE('',(#12786),#3922,.F.);
#97760=ADVANCED_FACE('',(#12787),#92262,.F.);
#97761=ADVANCED_FACE('',(#12788),#92263,.F.);
#97762=ADVANCED_FACE('',(#12789),#3923,.F.);
#97763=ADVANCED_FACE('',(#12790),#3924,.F.);
#97764=ADVANCED_FACE('',(#12791),#92264,.F.);
#97765=ADVANCED_FACE('',(#12792),#92265,.F.);
#97766=ADVANCED_FACE('',(#12793),#3925,.F.);
#97767=ADVANCED_FACE('',(#12794),#92266,.F.);
#97768=ADVANCED_FACE('',(#12795),#6266,.F.);
#97769=ADVANCED_FACE('',(#12796),#3926,.F.);
#97770=ADVANCED_FACE('',(#12797),#3927,.F.);
#97771=ADVANCED_FACE('',(#12798),#92267,.F.);
#97772=ADVANCED_FACE('',(#12799),#92268,.F.);
#97773=ADVANCED_FACE('',(#12800),#3928,.F.);
#97774=ADVANCED_FACE('',(#12801),#3929,.F.);
#97775=ADVANCED_FACE('',(#12802),#6267,.F.);
#97776=ADVANCED_FACE('',(#12803),#92269,.F.);
#97777=ADVANCED_FACE('',(#12804),#3930,.F.);
#97778=ADVANCED_FACE('',(#12805),#92270,.F.);
#97779=ADVANCED_FACE('',(#12806),#92271,.F.);
#97780=ADVANCED_FACE('',(#12807),#3931,.F.);
#97781=ADVANCED_FACE('',(#12808),#3932,.F.);
#97782=ADVANCED_FACE('',(#12809),#92272,.F.);
#97783=ADVANCED_FACE('',(#12810),#92273,.F.);
#97784=ADVANCED_FACE('',(#12811),#3933,.F.);
#97785=ADVANCED_FACE('',(#12812),#92274,.F.);
#97786=ADVANCED_FACE('',(#12813),#92275,.F.);
#97787=ADVANCED_FACE('',(#12814),#3934,.F.);
#97788=ADVANCED_FACE('',(#12815),#92276,.F.);
#97789=ADVANCED_FACE('',(#12816),#92277,.F.);
#97790=ADVANCED_FACE('',(#12817),#3935,.F.);
#97791=ADVANCED_FACE('',(#12818),#3936,.F.);
#97792=ADVANCED_FACE('',(#12819),#92278,.F.);
#97793=ADVANCED_FACE('',(#12820),#92279,.F.);
#97794=ADVANCED_FACE('',(#12821),#3937,.F.);
#97795=ADVANCED_FACE('',(#12822),#92280,.F.);
#97796=ADVANCED_FACE('',(#12823),#6268,.F.);
#97797=ADVANCED_FACE('',(#12824),#3938,.F.);
#97798=ADVANCED_FACE('',(#12825),#3939,.F.);
#97799=ADVANCED_FACE('',(#12826),#92281,.F.);
#97800=ADVANCED_FACE('',(#12827),#92282,.F.);
#97801=ADVANCED_FACE('',(#12828),#3940,.F.);
#97802=ADVANCED_FACE('',(#12829),#3941,.F.);
#97803=ADVANCED_FACE('',(#12830),#6269,.F.);
#97804=ADVANCED_FACE('',(#12831),#92283,.F.);
#97805=ADVANCED_FACE('',(#12832),#3942,.F.);
#97806=ADVANCED_FACE('',(#12833),#92284,.F.);
#97807=ADVANCED_FACE('',(#12834),#92285,.F.);
#97808=ADVANCED_FACE('',(#12835),#3943,.F.);
#97809=ADVANCED_FACE('',(#12836),#3944,.F.);
#97810=ADVANCED_FACE('',(#12837),#92286,.F.);
#97811=ADVANCED_FACE('',(#12838),#92287,.F.);
#97812=ADVANCED_FACE('',(#12839),#3945,.F.);
#97813=ADVANCED_FACE('',(#12840),#92288,.F.);
#97814=ADVANCED_FACE('',(#12841),#6270,.T.);
#97815=ADVANCED_FACE('',(#12842),#6271,.F.);
#97816=ADVANCED_FACE('',(#12843),#6272,.T.);
#97817=ADVANCED_FACE('',(#12844),#92289,.F.);
#97818=ADVANCED_FACE('',(#12845),#92290,.F.);
#97819=ADVANCED_FACE('',(#12846),#92291,.T.);
#97820=ADVANCED_FACE('',(#12847,#6372),#7228,.T.);
#97821=ADVANCED_FACE('',(#12848,#6373),#7229,.F.);
#97822=ADVANCED_FACE('',(#12849,#6374),#7230,.T.);
#97823=ADVANCED_FACE('',(#12850),#6273,.T.);
#97824=ADVANCED_FACE('',(#12851),#6274,.T.);
#97825=ADVANCED_FACE('',(#12852),#92292,.F.);
#97826=ADVANCED_FACE('',(#12853),#92293,.T.);
#97827=ADVANCED_FACE('',(#12854,#6375),#7231,.F.);
#97828=ADVANCED_FACE('',(#12855,#6376),#7232,.T.);
#97829=ADVANCED_FACE('',(#12856),#6275,.T.);
#97830=ADVANCED_FACE('',(#12857),#6276,.T.);
#97831=ADVANCED_FACE('',(#12858),#6277,.T.);
#97832=ADVANCED_FACE('',(#12859),#6278,.T.);
#97833=ADVANCED_FACE('',(#12860),#3946,.T.);
#97834=ADVANCED_FACE('',(#12861),#3947,.T.);
#97835=ADVANCED_FACE('',(#12862),#3948,.T.);
#97836=ADVANCED_FACE('',(#12863),#6279,.F.);
#97837=ADVANCED_FACE('',(#12864),#3949,.T.);
#97838=ADVANCED_FACE('',(#12865),#92294,.F.);
#97839=ADVANCED_FACE('',(#12866),#92295,.F.);
#97840=ADVANCED_FACE('',(#12867),#6280,.T.);
#97841=ADVANCED_FACE('',(#12868),#92296,.F.);
#97842=ADVANCED_FACE('',(#12869),#92297,.F.);
#97843=ADVANCED_FACE('',(#12870),#92298,.F.);
#97844=ADVANCED_FACE('',(#12871),#92299,.F.);
#97845=ADVANCED_FACE('',(#12872),#92300,.F.);
#97846=ADVANCED_FACE('',(#12873),#92301,.T.);
#97847=ADVANCED_FACE('',(#12874),#312,.T.);
#97848=ADVANCED_FACE('',(#12875),#92302,.T.);
#97849=ADVANCED_FACE('',(#12876),#92303,.T.);
#97850=ADVANCED_FACE('',(#12877),#7233,.F.);
#97851=ADVANCED_FACE('',(#12878),#7234,.F.);
#97852=ADVANCED_FACE('',(#12879),#7235,.F.);
#97853=ADVANCED_FACE('',(#12880),#92304,.T.);
#97854=ADVANCED_FACE('',(#12881),#92305,.T.);
#97855=ADVANCED_FACE('',(#12882),#7236,.F.);
#97856=ADVANCED_FACE('',(#12883),#92306,.F.);
#97857=ADVANCED_FACE('',(#12884),#7237,.T.);
#97858=ADVANCED_FACE('',(#12885),#92307,.F.);
#97859=ADVANCED_FACE('',(#12886),#7238,.T.);
#97860=ADVANCED_FACE('',(#12887),#92308,.F.);
#97861=ADVANCED_FACE('',(#12888),#7239,.T.);
#97862=ADVANCED_FACE('',(#12889),#92309,.F.);
#97863=ADVANCED_FACE('',(#12890),#7240,.T.);
#97864=ADVANCED_FACE('',(#12891,#6377),#7241,.T.);
#97865=ADVANCED_FACE('',(#12892),#7242,.F.);
#97866=ADVANCED_FACE('',(#12893),#7243,.T.);
#97867=ADVANCED_FACE('',(#12894),#92310,.T.);
#97868=ADVANCED_FACE('',(#12895),#3950,.F.);
#97869=ADVANCED_FACE('',(#12896),#92311,.T.);
#97870=ADVANCED_FACE('',(#12897),#7244,.T.);
#97871=ADVANCED_FACE('',(#12898),#7245,.T.);
#97872=ADVANCED_FACE('',(#12899),#92312,.T.);
#97873=ADVANCED_FACE('',(#12900,#6378),#7246,.T.);
#97874=ADVANCED_FACE('',(#12901),#92313,.T.);
#97875=ADVANCED_FACE('',(#12902,#6379),#7247,.T.);
#97876=ADVANCED_FACE('',(#12903),#92314,.T.);
#97877=ADVANCED_FACE('',(#12904,#6380),#7248,.T.);
#97878=ADVANCED_FACE('',(#12905,#6381),#7249,.T.);
#97879=ADVANCED_FACE('',(#12906),#7250,.T.);
#97880=ADVANCED_FACE('',(#12907),#7251,.T.);
#97881=ADVANCED_FACE('',(#12908),#7252,.T.);
#97882=ADVANCED_FACE('',(#12909),#7253,.T.);
#97883=ADVANCED_FACE('',(#12910),#7254,.T.);
#97884=ADVANCED_FACE('',(#12911),#7255,.T.);
#97885=ADVANCED_FACE('',(#12912),#7256,.T.);
#97886=ADVANCED_FACE('',(#12913),#7257,.T.);
#97887=ADVANCED_FACE('',(#12914),#7258,.T.);
#97888=ADVANCED_FACE('',(#12915),#7259,.T.);
#97889=ADVANCED_FACE('',(#12916),#7260,.T.);
#97890=ADVANCED_FACE('',(#12917,#6382,#6383,#6384,#6385,#6386),#7261,.T.);
#97891=ADVANCED_FACE('',(#12918,#6387),#7262,.F.);
#97892=ADVANCED_FACE('',(#12919,#6388),#7263,.T.);
#97893=ADVANCED_FACE('',(#12920),#6281,.T.);
#97894=ADVANCED_FACE('',(#12921),#6282,.T.);
#97895=ADVANCED_FACE('',(#12922),#6283,.T.);
#97896=ADVANCED_FACE('',(#12923),#6284,.T.);
#97897=ADVANCED_FACE('',(#12924),#92315,.F.);
#97898=ADVANCED_FACE('',(#12925),#3951,.F.);
#97899=ADVANCED_FACE('',(#12926),#92316,.F.);
#97900=ADVANCED_FACE('',(#12927),#3952,.F.);
#97901=ADVANCED_FACE('',(#12928),#92317,.F.);
#97902=ADVANCED_FACE('',(#12929),#3953,.F.);
#97903=ADVANCED_FACE('',(#12930),#92318,.F.);
#97904=ADVANCED_FACE('',(#12931),#3954,.F.);
#97905=ADVANCED_FACE('',(#12932),#92319,.F.);
#97906=ADVANCED_FACE('',(#12933),#3955,.F.);
#97907=ADVANCED_FACE('',(#12934),#92320,.F.);
#97908=ADVANCED_FACE('',(#12935),#3956,.F.);
#97909=ADVANCED_FACE('',(#12936),#3957,.F.);
#97910=ADVANCED_FACE('',(#12937),#3958,.F.);
#97911=ADVANCED_FACE('',(#12938),#3959,.T.);
#97912=ADVANCED_FACE('',(#12939),#92321,.F.);
#97913=ADVANCED_FACE('',(#12940),#6285,.F.);
#97914=ADVANCED_FACE('',(#12941),#6286,.F.);
#97915=ADVANCED_FACE('',(#12942),#3960,.T.);
#97916=ADVANCED_FACE('',(#12943),#3961,.F.);
#97917=ADVANCED_FACE('',(#12944),#92322,.F.);
#97918=ADVANCED_FACE('',(#12945),#92323,.T.);
#97919=ADVANCED_FACE('',(#12946),#6287,.F.);
#97920=ADVANCED_FACE('',(#12947),#3962,.F.);
#97921=ADVANCED_FACE('',(#12948),#92324,.F.);
#97922=ADVANCED_FACE('',(#12949),#6288,.F.);
#97923=ADVANCED_FACE('',(#12950),#3963,.F.);
#97924=ADVANCED_FACE('',(#12951),#92325,.F.);
#97925=ADVANCED_FACE('',(#12952),#92326,.T.);
#97926=ADVANCED_FACE('',(#12953),#6289,.F.);
#97927=ADVANCED_FACE('',(#12954),#3964,.F.);
#97928=ADVANCED_FACE('',(#12955),#92327,.F.);
#97929=ADVANCED_FACE('',(#12956),#6290,.F.);
#97930=ADVANCED_FACE('',(#12957),#6291,.F.);
#97931=ADVANCED_FACE('',(#12958),#3965,.F.);
#97932=ADVANCED_FACE('',(#12959),#92328,.F.);
#97933=ADVANCED_FACE('',(#12960),#92329,.T.);
#97934=ADVANCED_FACE('',(#12961),#6292,.F.);
#97935=ADVANCED_FACE('',(#12962),#3966,.F.);
#97936=ADVANCED_FACE('',(#12963),#92330,.T.);
#97937=ADVANCED_FACE('',(#12964),#3967,.T.);
#97938=ADVANCED_FACE('',(#12965),#92331,.T.);
#97939=ADVANCED_FACE('',(#12966),#92332,.T.);
#97940=ADVANCED_FACE('',(#12967),#6293,.T.);
#97941=ADVANCED_FACE('',(#12968),#92333,.T.);
#97942=ADVANCED_FACE('',(#12969),#92334,.T.);
#97943=ADVANCED_FACE('',(#12970),#92335,.T.);
#97944=ADVANCED_FACE('',(#12971),#92336,.T.);
#97945=ADVANCED_FACE('',(#12972),#92337,.T.);
#97946=ADVANCED_FACE('',(#12973),#92338,.T.);
#97947=ADVANCED_FACE('',(#12974),#6294,.T.);
#97948=ADVANCED_FACE('',(#12975),#92339,.T.);
#97949=ADVANCED_FACE('',(#12976),#3968,.F.);
#97950=ADVANCED_FACE('',(#12977),#6295,.F.);
#97951=ADVANCED_FACE('',(#12978),#3969,.F.);
#97952=ADVANCED_FACE('',(#12979),#3970,.F.);
#97953=ADVANCED_FACE('',(#12980),#6296,.F.);
#97954=ADVANCED_FACE('',(#12981),#3971,.F.);
#97955=ADVANCED_FACE('',(#12982),#3972,.F.);
#97956=ADVANCED_FACE('',(#12983),#6297,.F.);
#97957=ADVANCED_FACE('',(#12984),#3973,.F.);
#97958=ADVANCED_FACE('',(#12985),#3974,.F.);
#97959=ADVANCED_FACE('',(#12986),#6298,.F.);
#97960=ADVANCED_FACE('',(#12987),#3975,.F.);
#97961=ADVANCED_FACE('',(#12988),#3976,.F.);
#97962=ADVANCED_FACE('',(#12989),#3977,.F.);
#97963=ADVANCED_FACE('',(#12990),#92340,.F.);
#97964=ADVANCED_FACE('',(#12991),#3978,.F.);
#97965=ADVANCED_FACE('',(#12992),#3979,.F.);
#97966=ADVANCED_FACE('',(#12993),#92341,.F.);
#97967=ADVANCED_FACE('',(#12994),#3980,.T.);
#97968=ADVANCED_FACE('',(#12995),#46,.T.);
#97969=ADVANCED_FACE('',(#12996),#3981,.T.);
#97970=ADVANCED_FACE('',(#12997),#47,.T.);
#97971=ADVANCED_FACE('',(#12998),#3982,.F.);
#97972=ADVANCED_FACE('',(#12999),#3983,.F.);
#97973=ADVANCED_FACE('',(#13000),#3984,.T.);
#97974=ADVANCED_FACE('',(#13001),#3985,.T.);
#97975=ADVANCED_FACE('',(#13002),#3986,.T.);
#97976=ADVANCED_FACE('',(#13003),#3987,.T.);
#97977=ADVANCED_FACE('',(#13004),#3988,.T.);
#97978=ADVANCED_FACE('',(#13005),#3989,.T.);
#97979=ADVANCED_FACE('',(#13006),#3990,.T.);
#97980=ADVANCED_FACE('',(#13007),#3991,.T.);
#97981=ADVANCED_FACE('',(#13008),#3992,.T.);
#97982=ADVANCED_FACE('',(#13009),#3993,.T.);
#97983=ADVANCED_FACE('',(#13010),#3994,.T.);
#97984=ADVANCED_FACE('',(#13011),#3995,.T.);
#97985=ADVANCED_FACE('',(#13012),#3996,.T.);
#97986=ADVANCED_FACE('',(#13013),#3997,.T.);
#97987=ADVANCED_FACE('',(#13014),#3998,.T.);
#97988=ADVANCED_FACE('',(#13015),#3999,.T.);
#97989=ADVANCED_FACE('',(#13016),#4000,.T.);
#97990=ADVANCED_FACE('',(#13017),#4001,.T.);
#97991=ADVANCED_FACE('',(#13018),#4002,.T.);
#97992=ADVANCED_FACE('',(#13019),#4003,.T.);
#97993=ADVANCED_FACE('',(#13020),#4004,.T.);
#97994=ADVANCED_FACE('',(#13021),#4005,.T.);
#97995=ADVANCED_FACE('',(#13022),#4006,.T.);
#97996=ADVANCED_FACE('',(#13023),#4007,.T.);
#97997=ADVANCED_FACE('',(#13024),#4008,.T.);
#97998=ADVANCED_FACE('',(#13025),#4009,.T.);
#97999=ADVANCED_FACE('',(#13026),#92342,.T.);
#98000=ADVANCED_FACE('',(#13027),#4010,.T.);
#98001=ADVANCED_FACE('',(#13028),#6299,.T.);
#98002=ADVANCED_FACE('',(#13029),#92343,.T.);
#98003=ADVANCED_FACE('',(#13030),#48,.T.);
#98004=ADVANCED_FACE('',(#13031),#6300,.T.);
#98005=ADVANCED_FACE('',(#13032),#6301,.T.);
#98006=ADVANCED_FACE('',(#13033),#4011,.T.);
#98007=ADVANCED_FACE('',(#13034),#92344,.F.);
#98008=ADVANCED_FACE('',(#13035),#92345,.T.);
#98009=ADVANCED_FACE('',(#13036),#92346,.T.);
#98010=ADVANCED_FACE('',(#13037),#49,.T.);
#98011=ADVANCED_FACE('',(#13038,#6389),#7264,.F.);
#98012=ADVANCED_FACE('',(#13039),#4012,.T.);
#98013=ADVANCED_FACE('',(#13040),#6302,.T.);
#98014=ADVANCED_FACE('',(#13041),#6303,.T.);
#98015=ADVANCED_FACE('',(#13042),#92347,.F.);
#98016=ADVANCED_FACE('',(#13043,#6390),#92348,.F.);
#98017=ADVANCED_FACE('',(#13044,#6391),#92349,.T.);
#98018=ADVANCED_FACE('',(#13045,#6392),#7265,.F.);
#98019=ADVANCED_FACE('',(#13046,#6393),#7266,.T.);
#98020=ADVANCED_FACE('',(#13047),#6304,.F.);
#98021=ADVANCED_FACE('',(#13048),#6305,.T.);
#98022=ADVANCED_FACE('',(#13049),#6306,.T.);
#98023=ADVANCED_FACE('',(#13050),#6307,.T.);
#98024=ADVANCED_FACE('',(#13051),#6308,.T.);
#98025=ADVANCED_FACE('',(#13052),#92350,.T.);
#98026=ADVANCED_FACE('',(#13053),#313,.F.);
#98027=ADVANCED_FACE('',(#13054),#314,.T.);
#98028=ADVANCED_FACE('',(#13055),#92351,.T.);
#98029=ADVANCED_FACE('',(#13056),#92352,.F.);
#98030=ADVANCED_FACE('',(#13057),#92353,.T.);
#98031=ADVANCED_FACE('',(#13058,#6394),#7267,.T.);
#98032=ADVANCED_FACE('',(#13059,#6395),#7268,.T.);
#98033=ADVANCED_FACE('',(#13060,#6396),#7269,.T.);
#98034=ADVANCED_FACE('',(#13061,#6397),#7270,.T.);
#98035=ADVANCED_FACE('',(#13062,#6398),#7271,.T.);
#98036=ADVANCED_FACE('',(#13063),#92354,.T.);
#98037=ADVANCED_FACE('',(#13064),#92355,.T.);
#98038=ADVANCED_FACE('',(#13065),#92356,.T.);
#98039=ADVANCED_FACE('',(#13066),#92357,.T.);
#98040=ADVANCED_FACE('',(#13067),#92358,.T.);
#98041=ADVANCED_FACE('',(#13068),#92359,.T.);
#98042=ADVANCED_FACE('',(#13069),#92360,.T.);
#98043=ADVANCED_FACE('',(#13070),#92361,.T.);
#98044=ADVANCED_FACE('',(#13071),#92362,.T.);
#98045=ADVANCED_FACE('',(#13072),#92363,.T.);
#98046=ADVANCED_FACE('',(#13073),#92364,.T.);
#98047=ADVANCED_FACE('',(#13074),#92365,.T.);
#98048=ADVANCED_FACE('',(#13075),#92366,.T.);
#98049=ADVANCED_FACE('',(#13076),#92367,.T.);
#98050=ADVANCED_FACE('',(#13077),#315,.T.);
#98051=ADVANCED_FACE('',(#13078),#316,.T.);
#98052=ADVANCED_FACE('',(#13079),#92368,.T.);
#98053=ADVANCED_FACE('',(#13080),#7272,.F.);
#98054=ADVANCED_FACE('',(#13081,#6399),#7273,.T.);
#98055=ADVANCED_FACE('',(#13082),#317,.F.);
#98056=ADVANCED_FACE('',(#13083),#318,.F.);
#98057=ADVANCED_FACE('',(#13084),#319,.F.);
#98058=ADVANCED_FACE('',(#13085),#320,.F.);
#98059=ADVANCED_FACE('',(#13086),#321,.F.);
#98060=ADVANCED_FACE('',(#13087),#322,.F.);
#98061=ADVANCED_FACE('',(#13088),#7274,.F.);
#98062=ADVANCED_FACE('',(#13089),#7275,.F.);
#98063=ADVANCED_FACE('',(#13090),#7276,.F.);
#98064=ADVANCED_FACE('',(#13091),#7277,.F.);
#98065=ADVANCED_FACE('',(#13092),#7278,.F.);
#98066=ADVANCED_FACE('',(#13093),#7279,.F.);
#98067=ADVANCED_FACE('',(#13094),#7280,.F.);
#98068=ADVANCED_FACE('',(#13095),#4013,.F.);
#98069=ADVANCED_FACE('',(#13096),#92369,.T.);
#98070=ADVANCED_FACE('',(#13097),#4014,.F.);
#98071=ADVANCED_FACE('',(#13098),#92370,.T.);
#98072=ADVANCED_FACE('',(#13099),#92371,.T.);
#98073=ADVANCED_FACE('',(#13100),#92372,.T.);
#98074=ADVANCED_FACE('',(#13101),#92373,.T.);
#98075=ADVANCED_FACE('',(#13102),#92374,.T.);
#98076=ADVANCED_FACE('',(#13103),#92375,.T.);
#98077=ADVANCED_FACE('',(#13104),#92376,.T.);
#98078=ADVANCED_FACE('',(#13105),#92377,.T.);
#98079=ADVANCED_FACE('',(#13106),#92378,.T.);
#98080=ADVANCED_FACE('',(#13107),#92379,.T.);
#98081=ADVANCED_FACE('',(#13108),#92380,.T.);
#98082=ADVANCED_FACE('',(#13109),#92381,.T.);
#98083=ADVANCED_FACE('',(#13110),#92382,.T.);
#98084=ADVANCED_FACE('',(#13111),#92383,.T.);
#98085=ADVANCED_FACE('',(#13112),#323,.T.);
#98086=ADVANCED_FACE('',(#13113),#324,.T.);
#98087=ADVANCED_FACE('',(#13114),#92384,.T.);
#98088=ADVANCED_FACE('',(#13115),#7281,.F.);
#98089=ADVANCED_FACE('',(#13116,#6400),#7282,.T.);
#98090=ADVANCED_FACE('',(#13117),#325,.F.);
#98091=ADVANCED_FACE('',(#13118),#326,.F.);
#98092=ADVANCED_FACE('',(#13119),#327,.F.);
#98093=ADVANCED_FACE('',(#13120),#328,.F.);
#98094=ADVANCED_FACE('',(#13121),#329,.F.);
#98095=ADVANCED_FACE('',(#13122),#330,.F.);
#98096=ADVANCED_FACE('',(#13123),#7283,.F.);
#98097=ADVANCED_FACE('',(#13124),#7284,.F.);
#98098=ADVANCED_FACE('',(#13125),#7285,.F.);
#98099=ADVANCED_FACE('',(#13126),#7286,.F.);
#98100=ADVANCED_FACE('',(#13127),#7287,.F.);
#98101=ADVANCED_FACE('',(#13128),#7288,.F.);
#98102=ADVANCED_FACE('',(#13129),#7289,.F.);
#98103=ADVANCED_FACE('',(#13130),#4015,.F.);
#98104=ADVANCED_FACE('',(#13131),#92385,.T.);
#98105=ADVANCED_FACE('',(#13132),#4016,.F.);
#98106=ADVANCED_FACE('',(#13133),#331,.F.);
#98107=ADVANCED_FACE('',(#13134),#332,.F.);
#98108=ADVANCED_FACE('',(#13135),#333,.T.);
#98109=ADVANCED_FACE('',(#13136),#334,.T.);
#98110=ADVANCED_FACE('',(#13137,#6401),#92386,.T.);
#98111=ADVANCED_FACE('',(#13138),#92387,.F.);
#98112=ADVANCED_FACE('',(#13139),#92388,.F.);
#98113=ADVANCED_FACE('',(#13140,#6402),#92389,.F.);
#98114=ADVANCED_FACE('',(#13141,#6403),#7290,.T.);
#98115=ADVANCED_FACE('',(#13142,#6404),#7291,.T.);
#98116=ADVANCED_FACE('',(#13143),#92390,.T.);
#98117=ADVANCED_FACE('',(#13144),#92391,.F.);
#98118=ADVANCED_FACE('',(#13145),#6309,.F.);
#98119=ADVANCED_FACE('',(#13146),#92392,.F.);
#98120=ADVANCED_FACE('',(#13147),#92393,.F.);
#98121=ADVANCED_FACE('',(#13148),#92394,.T.);
#98122=ADVANCED_FACE('',(#13149),#92395,.F.);
#98123=ADVANCED_FACE('',(#13150),#92396,.F.);
#98124=ADVANCED_FACE('',(#13151),#92397,.F.);
#98125=ADVANCED_FACE('',(#13152),#92398,.F.);
#98126=ADVANCED_FACE('',(#13153),#92399,.F.);
#98127=ADVANCED_FACE('',(#13154),#92400,.F.);
#98128=ADVANCED_FACE('',(#13155),#92401,.F.);
#98129=ADVANCED_FACE('',(#13156),#92402,.F.);
#98130=ADVANCED_FACE('',(#13157),#92403,.F.);
#98131=ADVANCED_FACE('',(#13158),#92404,.T.);
#98132=ADVANCED_FACE('',(#13159),#7292,.F.);
#98133=ADVANCED_FACE('',(#13160),#92405,.T.);
#98134=ADVANCED_FACE('',(#13161),#7293,.F.);
#98135=ADVANCED_FACE('',(#13162),#92406,.T.);
#98136=ADVANCED_FACE('',(#13163),#7294,.F.);
#98137=ADVANCED_FACE('',(#13164),#92407,.T.);
#98138=ADVANCED_FACE('',(#13165),#7295,.F.);
#98139=ADVANCED_FACE('',(#13166,#6405,#6406,#6407,#6408,#6409),#7296,.F.);
#98140=ADVANCED_FACE('',(#13167,#6410),#7297,.F.);
#98141=ADVANCED_FACE('',(#13168,#6411),#7298,.F.);
#98142=ADVANCED_FACE('',(#13169,#6412),#7299,.F.);
#98143=ADVANCED_FACE('',(#13170,#6413),#7300,.F.);
#98144=ADVANCED_FACE('',(#13171,#6414),#7301,.F.);
#98145=ADVANCED_FACE('',(#13172),#92408,.T.);
#98146=ADVANCED_FACE('',(#13173),#7302,.F.);
#98147=ADVANCED_FACE('',(#13174),#92409,.T.);
#98148=ADVANCED_FACE('',(#13175),#7303,.F.);
#98149=ADVANCED_FACE('',(#13176),#92410,.T.);
#98150=ADVANCED_FACE('',(#13177),#7304,.F.);
#98151=ADVANCED_FACE('',(#13178),#92411,.T.);
#98152=ADVANCED_FACE('',(#13179),#7305,.F.);
#98153=ADVANCED_FACE('',(#13180),#6310,.T.);
#98154=ADVANCED_FACE('',(#13181),#92412,.T.);
#98155=ADVANCED_FACE('',(#13182),#92413,.T.);
#98156=ADVANCED_FACE('',(#13183),#6311,.T.);
#98157=ADVANCED_FACE('',(#13184),#6312,.T.);
#98158=ADVANCED_FACE('',(#13185),#92414,.T.);
#98159=ADVANCED_FACE('',(#13186),#92415,.T.);
#98160=ADVANCED_FACE('',(#13187),#6313,.T.);
#98161=ADVANCED_FACE('',(#13188,#6415,#6416,#6417,#6418,#6419),#7306,.T.);
#98162=ADVANCED_FACE('',(#13189),#92416,.F.);
#98163=ADVANCED_FACE('',(#13190,#6420),#7307,.T.);
#98164=ADVANCED_FACE('',(#13191,#6421),#7308,.F.);
#98165=ADVANCED_FACE('',(#13192,#6422),#7309,.T.);
#98166=ADVANCED_FACE('',(#13193,#6423),#7310,.T.);
#98167=ADVANCED_FACE('',(#13194),#92417,.F.);
#98168=ADVANCED_FACE('',(#13195),#7311,.F.);
#98169=ADVANCED_FACE('',(#13196),#7312,.F.);
#98170=ADVANCED_FACE('',(#13197,#6424),#7313,.F.);
#98171=ADVANCED_FACE('',(#13198),#92418,.F.);
#98172=ADVANCED_FACE('',(#13199),#7314,.F.);
#98173=ADVANCED_FACE('',(#13200),#7315,.F.);
#98174=ADVANCED_FACE('',(#13201),#4017,.T.);
#98175=ADVANCED_FACE('',(#13202),#4018,.T.);
#98176=ADVANCED_FACE('',(#13203),#4019,.T.);
#98177=ADVANCED_FACE('',(#13204),#4020,.T.);
#98178=ADVANCED_FACE('',(#13205),#7316,.F.);
#98179=ADVANCED_FACE('',(#13206),#7317,.F.);
#98180=ADVANCED_FACE('',(#13207),#4021,.T.);
#98181=ADVANCED_FACE('',(#13208),#4022,.T.);
#98182=ADVANCED_FACE('',(#13209),#4023,.T.);
#98183=ADVANCED_FACE('',(#13210),#4024,.T.);
#98184=ADVANCED_FACE('',(#13211),#7318,.F.);
#98185=ADVANCED_FACE('',(#13212),#7319,.F.);
#98186=ADVANCED_FACE('',(#13213),#92419,.F.);
#98187=ADVANCED_FACE('',(#13214),#335,.F.);
#98188=ADVANCED_FACE('',(#13215,#6425),#92420,.T.);
#98189=ADVANCED_FACE('',(#13216,#6426),#92421,.T.);
#98190=ADVANCED_FACE('',(#13217,#6427),#92422,.T.);
#98191=ADVANCED_FACE('',(#13218,#6428),#92423,.T.);
#98192=ADVANCED_FACE('',(#13219,#6429,#6430),#92424,.T.);
#98193=ADVANCED_FACE('',(#13220,#6431,#6432),#92425,.T.);
#98194=ADVANCED_FACE('',(#13221,#6433,#6434),#92426,.T.);
#98195=ADVANCED_FACE('',(#13222),#4025,.T.);
#98196=ADVANCED_FACE('',(#13223),#4026,.T.);
#98197=ADVANCED_FACE('',(#13224),#4027,.T.);
#98198=ADVANCED_FACE('',(#13225),#4028,.T.);
#98199=ADVANCED_FACE('',(#13226,#6435),#7320,.F.);
#98200=ADVANCED_FACE('',(#13227),#4029,.T.);
#98201=ADVANCED_FACE('',(#13228),#4030,.T.);
#98202=ADVANCED_FACE('',(#13229),#4031,.T.);
#98203=ADVANCED_FACE('',(#13230),#4032,.T.);
#98204=ADVANCED_FACE('',(#13231),#4033,.T.);
#98205=ADVANCED_FACE('',(#13232),#4034,.T.);
#98206=ADVANCED_FACE('',(#13233),#4035,.T.);
#98207=ADVANCED_FACE('',(#13234),#4036,.T.);
#98208=ADVANCED_FACE('',(#13235),#4037,.T.);
#98209=ADVANCED_FACE('',(#13236),#4038,.T.);
#98210=ADVANCED_FACE('',(#13237),#4039,.T.);
#98211=ADVANCED_FACE('',(#13238),#4040,.T.);
#98212=ADVANCED_FACE('',(#13239),#4041,.T.);
#98213=ADVANCED_FACE('',(#13240),#4042,.T.);
#98214=ADVANCED_FACE('',(#13241),#4043,.T.);
#98215=ADVANCED_FACE('',(#13242),#4044,.T.);
#98216=ADVANCED_FACE('',(#13243,#6436),#7321,.T.);
#98217=ADVANCED_FACE('',(#13244),#4045,.T.);
#98218=ADVANCED_FACE('',(#13245),#4046,.T.);
#98219=ADVANCED_FACE('',(#13246),#4047,.T.);
#98220=ADVANCED_FACE('',(#13247),#4048,.T.);
#98221=ADVANCED_FACE('',(#13248,#6437),#7322,.T.);
#98222=ADVANCED_FACE('',(#13249),#4049,.T.);
#98223=ADVANCED_FACE('',(#13250),#4050,.T.);
#98224=ADVANCED_FACE('',(#13251,#6438),#7323,.T.);
#98225=ADVANCED_FACE('',(#13252),#4051,.T.);
#98226=ADVANCED_FACE('',(#13253),#4052,.T.);
#98227=ADVANCED_FACE('',(#13254,#6439),#7324,.F.);
#98228=ADVANCED_FACE('',(#13255),#4053,.T.);
#98229=ADVANCED_FACE('',(#13256),#4054,.T.);
#98230=ADVANCED_FACE('',(#13257,#6440),#7325,.F.);
#98231=ADVANCED_FACE('',(#13258),#4055,.T.);
#98232=ADVANCED_FACE('',(#13259),#4056,.T.);
#98233=ADVANCED_FACE('',(#13260,#6441),#7326,.F.);
#98234=ADVANCED_FACE('',(#13261),#7327,.F.);
#98235=ADVANCED_FACE('',(#13262),#7328,.F.);
#98236=ADVANCED_FACE('',(#13263),#7329,.F.);
#98237=ADVANCED_FACE('',(#13264),#7330,.F.);
#98238=ADVANCED_FACE('',(#13265),#7331,.F.);
#98239=ADVANCED_FACE('',(#13266),#7332,.F.);
#98240=ADVANCED_FACE('',(#13267),#7333,.F.);
#98241=ADVANCED_FACE('',(#13268,#6442),#7334,.T.);
#98242=ADVANCED_FACE('',(#13269),#7335,.F.);
#98243=ADVANCED_FACE('',(#13270),#7336,.F.);
#98244=ADVANCED_FACE('',(#13271),#7337,.F.);
#98245=ADVANCED_FACE('',(#13272),#7338,.F.);
#98246=ADVANCED_FACE('',(#13273),#92427,.T.);
#98247=ADVANCED_FACE('',(#13274),#92428,.T.);
#98248=ADVANCED_FACE('',(#13275),#92429,.T.);
#98249=ADVANCED_FACE('',(#13276),#92430,.T.);
#98250=ADVANCED_FACE('',(#13277),#4057,.F.);
#98251=ADVANCED_FACE('',(#13278),#92431,.T.);
#98252=ADVANCED_FACE('',(#13279),#92432,.T.);
#98253=ADVANCED_FACE('',(#13280),#4058,.F.);
#98254=ADVANCED_FACE('',(#13281),#4059,.F.);
#98255=ADVANCED_FACE('',(#13282),#92433,.T.);
#98256=ADVANCED_FACE('',(#13283),#92434,.T.);
#98257=ADVANCED_FACE('',(#13284),#4060,.F.);
#98258=ADVANCED_FACE('',(#13285),#92435,.T.);
#98259=ADVANCED_FACE('',(#13286),#92436,.T.);
#98260=ADVANCED_FACE('',(#13287),#92437,.T.);
#98261=ADVANCED_FACE('',(#13288),#92438,.T.);
#98262=ADVANCED_FACE('',(#13289),#7339,.F.);
#98263=ADVANCED_FACE('',(#13290),#7340,.F.);
#98264=ADVANCED_FACE('',(#13291),#7341,.F.);
#98265=ADVANCED_FACE('',(#13292),#7342,.F.);
#98266=ADVANCED_FACE('',(#13293),#7343,.F.);
#98267=ADVANCED_FACE('',(#13294),#6314,.F.);
#98268=ADVANCED_FACE('',(#13295),#92439,.F.);
#98269=ADVANCED_FACE('',(#13296),#92440,.F.);
#98270=ADVANCED_FACE('',(#13297),#6315,.F.);
#98271=ADVANCED_FACE('',(#13298),#6316,.F.);
#98272=ADVANCED_FACE('',(#13299),#92441,.F.);
#98273=ADVANCED_FACE('',(#13300),#92442,.F.);
#98274=ADVANCED_FACE('',(#13301),#6317,.F.);
#98275=ADVANCED_FACE('',(#13302),#6318,.F.);
#98276=ADVANCED_FACE('',(#13303),#4061,.F.);
#98277=ADVANCED_FACE('',(#13304),#92443,.F.);
#98278=ADVANCED_FACE('',(#13305),#92444,.F.);
#98279=ADVANCED_FACE('',(#13306),#6319,.F.);
#98280=ADVANCED_FACE('',(#13307),#4062,.F.);
#98281=ADVANCED_FACE('',(#13308),#4063,.F.);
#98282=ADVANCED_FACE('',(#13309),#6320,.F.);
#98283=ADVANCED_FACE('',(#13310),#92445,.F.);
#98284=ADVANCED_FACE('',(#13311),#92446,.F.);
#98285=ADVANCED_FACE('',(#13312),#4064,.F.);
#98286=ADVANCED_FACE('',(#13313),#6321,.F.);
#98287=ADVANCED_FACE('',(#13314,#6443),#7344,.F.);
#98288=ADVANCED_FACE('',(#13315),#7345,.F.);
#98289=ADVANCED_FACE('',(#13316),#7346,.F.);
#98290=ADVANCED_FACE('',(#13317),#7347,.F.);
#98291=ADVANCED_FACE('',(#13318),#7348,.F.);
#98292=ADVANCED_FACE('',(#13319),#7349,.T.);
#98293=ADVANCED_FACE('',(#13320),#7350,.F.);
#98294=ADVANCED_FACE('',(#13321),#7351,.T.);
#98295=ADVANCED_FACE('',(#13322),#7352,.F.);
#98296=ADVANCED_FACE('',(#13323),#7353,.T.);
#98297=ADVANCED_FACE('',(#13324),#92447,.F.);
#98298=ADVANCED_FACE('',(#13325),#7354,.F.);
#98299=ADVANCED_FACE('',(#13326),#7355,.T.);
#98300=ADVANCED_FACE('',(#13327),#7356,.T.);
#98301=ADVANCED_FACE('',(#13328),#92448,.F.);
#98302=ADVANCED_FACE('',(#13329),#7357,.T.);
#98303=ADVANCED_FACE('',(#13330),#92449,.F.);
#98304=ADVANCED_FACE('',(#13331),#7358,.T.);
#98305=ADVANCED_FACE('',(#13332),#92450,.F.);
#98306=ADVANCED_FACE('',(#13333),#7359,.T.);
#98307=ADVANCED_FACE('',(#13334),#92451,.F.);
#98308=ADVANCED_FACE('',(#13335),#7360,.T.);
#98309=ADVANCED_FACE('',(#13336),#92452,.F.);
#98310=ADVANCED_FACE('',(#13337),#7361,.T.);
#98311=ADVANCED_FACE('',(#13338),#92453,.F.);
#98312=ADVANCED_FACE('',(#13339),#7362,.T.);
#98313=ADVANCED_FACE('',(#13340),#92454,.F.);
#98314=ADVANCED_FACE('',(#13341),#7363,.F.);
#98315=ADVANCED_FACE('',(#13342),#7364,.F.);
#98316=ADVANCED_FACE('',(#13343),#7365,.T.);
#98317=ADVANCED_FACE('',(#13344),#92455,.F.);
#98318=ADVANCED_FACE('',(#13345),#7366,.T.);
#98319=ADVANCED_FACE('',(#13346),#92456,.F.);
#98320=ADVANCED_FACE('',(#13347),#7367,.T.);
#98321=ADVANCED_FACE('',(#13348),#92457,.F.);
#98322=ADVANCED_FACE('',(#13349),#7368,.T.);
#98323=ADVANCED_FACE('',(#13350),#92458,.F.);
#98324=ADVANCED_FACE('',(#13351),#7369,.F.);
#98325=ADVANCED_FACE('',(#13352),#7370,.F.);
#98326=ADVANCED_FACE('',(#13353),#7371,.F.);
#98327=ADVANCED_FACE('',(#13354),#92459,.F.);
#98328=ADVANCED_FACE('',(#13355),#7372,.F.);
#98329=ADVANCED_FACE('',(#13356),#92460,.T.);
#98330=ADVANCED_FACE('',(#13357),#7373,.F.);
#98331=ADVANCED_FACE('',(#13358),#92461,.F.);
#98332=ADVANCED_FACE('',(#13359),#7374,.F.);
#98333=ADVANCED_FACE('',(#13360),#7375,.F.);
#98334=ADVANCED_FACE('',(#13361),#7376,.F.);
#98335=ADVANCED_FACE('',(#13362),#92462,.F.);
#98336=ADVANCED_FACE('',(#13363),#7377,.F.);
#98337=ADVANCED_FACE('',(#13364),#92463,.T.);
#98338=ADVANCED_FACE('',(#13365),#7378,.F.);
#98339=ADVANCED_FACE('',(#13366),#92464,.F.);
#98340=ADVANCED_FACE('',(#13367),#7379,.F.);
#98341=ADVANCED_FACE('',(#13368),#92465,.F.);
#98342=ADVANCED_FACE('',(#13369),#7380,.F.);
#98343=ADVANCED_FACE('',(#13370),#92466,.T.);
#98344=ADVANCED_FACE('',(#13371),#7381,.F.);
#98345=ADVANCED_FACE('',(#13372),#92467,.F.);
#98346=ADVANCED_FACE('',(#13373),#7382,.F.);
#98347=ADVANCED_FACE('',(#13374),#7383,.F.);
#98348=ADVANCED_FACE('',(#13375),#7384,.F.);
#98349=ADVANCED_FACE('',(#13376),#92468,.F.);
#98350=ADVANCED_FACE('',(#13377),#7385,.F.);
#98351=ADVANCED_FACE('',(#13378),#92469,.T.);
#98352=ADVANCED_FACE('',(#13379),#7386,.F.);
#98353=ADVANCED_FACE('',(#13380),#92470,.F.);
#98354=ADVANCED_FACE('',(#13381),#7387,.F.);
#98355=ADVANCED_FACE('',(#13382),#92471,.F.);
#98356=ADVANCED_FACE('',(#13383),#7388,.F.);
#98357=ADVANCED_FACE('',(#13384),#92472,.T.);
#98358=ADVANCED_FACE('',(#13385),#7389,.F.);
#98359=ADVANCED_FACE('',(#13386),#92473,.F.);
#98360=ADVANCED_FACE('',(#13387),#7390,.F.);
#98361=ADVANCED_FACE('',(#13388),#7391,.F.);
#98362=ADVANCED_FACE('',(#13389),#7392,.F.);
#98363=ADVANCED_FACE('',(#13390),#92474,.F.);
#98364=ADVANCED_FACE('',(#13391),#7393,.F.);
#98365=ADVANCED_FACE('',(#13392),#92475,.T.);
#98366=ADVANCED_FACE('',(#13393),#7394,.F.);
#98367=ADVANCED_FACE('',(#13394),#92476,.F.);
#98368=ADVANCED_FACE('',(#13395),#7395,.F.);
#98369=ADVANCED_FACE('',(#13396),#92477,.F.);
#98370=ADVANCED_FACE('',(#13397),#7396,.F.);
#98371=ADVANCED_FACE('',(#13398),#92478,.T.);
#98372=ADVANCED_FACE('',(#13399),#7397,.F.);
#98373=ADVANCED_FACE('',(#13400),#92479,.F.);
#98374=ADVANCED_FACE('',(#13401),#7398,.F.);
#98375=ADVANCED_FACE('',(#13402),#7399,.F.);
#98376=ADVANCED_FACE('',(#13403),#7400,.F.);
#98377=ADVANCED_FACE('',(#13404),#92480,.F.);
#98378=ADVANCED_FACE('',(#13405),#7401,.F.);
#98379=ADVANCED_FACE('',(#13406),#92481,.T.);
#98380=ADVANCED_FACE('',(#13407),#7402,.F.);
#98381=ADVANCED_FACE('',(#13408),#92482,.F.);
#98382=ADVANCED_FACE('',(#13409),#7403,.F.);
#98383=ADVANCED_FACE('',(#13410),#92483,.F.);
#98384=ADVANCED_FACE('',(#13411),#7404,.F.);
#98385=ADVANCED_FACE('',(#13412),#7405,.T.);
#98386=ADVANCED_FACE('',(#13413),#92484,.F.);
#98387=ADVANCED_FACE('',(#13414),#7406,.T.);
#98388=ADVANCED_FACE('',(#13415),#92485,.F.);
#98389=ADVANCED_FACE('',(#13416),#7407,.T.);
#98390=ADVANCED_FACE('',(#13417),#92486,.F.);
#98391=ADVANCED_FACE('',(#13418),#7408,.T.);
#98392=ADVANCED_FACE('',(#13419),#92487,.F.);
#98393=ADVANCED_FACE('',(#13420),#7409,.T.);
#98394=ADVANCED_FACE('',(#13421),#7410,.T.);
#98395=ADVANCED_FACE('',(#13422),#92488,.F.);
#98396=ADVANCED_FACE('',(#13423),#7411,.T.);
#98397=ADVANCED_FACE('',(#13424),#92489,.F.);
#98398=ADVANCED_FACE('',(#13425),#7412,.T.);
#98399=ADVANCED_FACE('',(#13426),#92490,.F.);
#98400=ADVANCED_FACE('',(#13427),#7413,.F.);
#98401=ADVANCED_FACE('',(#13428),#7414,.F.);
#98402=ADVANCED_FACE('',(#13429),#7415,.T.);
#98403=ADVANCED_FACE('',(#13430),#92491,.F.);
#98404=ADVANCED_FACE('',(#13431),#7416,.T.);
#98405=ADVANCED_FACE('',(#13432),#92492,.F.);
#98406=ADVANCED_FACE('',(#13433),#7417,.T.);
#98407=ADVANCED_FACE('',(#13434),#92493,.F.);
#98408=ADVANCED_FACE('',(#13435),#7418,.T.);
#98409=ADVANCED_FACE('',(#13436),#92494,.F.);
#98410=ADVANCED_FACE('',(#13437),#7419,.F.);
#98411=ADVANCED_FACE('',(#13438),#92495,.F.);
#98412=ADVANCED_FACE('',(#13439),#7420,.F.);
#98413=ADVANCED_FACE('',(#13440),#7421,.T.);
#98414=ADVANCED_FACE('',(#13441),#92496,.F.);
#98415=ADVANCED_FACE('',(#13442),#7422,.T.);
#98416=ADVANCED_FACE('',(#13443),#92497,.F.);
#98417=ADVANCED_FACE('',(#13444),#7423,.T.);
#98418=ADVANCED_FACE('',(#13445),#92498,.F.);
#98419=ADVANCED_FACE('',(#13446),#7424,.T.);
#98420=ADVANCED_FACE('',(#13447),#92499,.F.);
#98421=ADVANCED_FACE('',(#13448),#7425,.T.);
#98422=ADVANCED_FACE('',(#13449),#92500,.F.);
#98423=ADVANCED_FACE('',(#13450),#7426,.T.);
#98424=ADVANCED_FACE('',(#13451),#92501,.F.);
#98425=ADVANCED_FACE('',(#13452),#7427,.T.);
#98426=ADVANCED_FACE('',(#13453),#7428,.T.);
#98427=ADVANCED_FACE('',(#13454),#92502,.F.);
#98428=ADVANCED_FACE('',(#13455),#7429,.F.);
#98429=ADVANCED_FACE('',(#13456),#7430,.F.);
#98430=ADVANCED_FACE('',(#13457),#7431,.T.);
#98431=ADVANCED_FACE('',(#13458),#92503,.F.);
#98432=ADVANCED_FACE('',(#13459),#7432,.T.);
#98433=ADVANCED_FACE('',(#13460),#92504,.F.);
#98434=ADVANCED_FACE('',(#13461),#7433,.T.);
#98435=ADVANCED_FACE('',(#13462),#92505,.F.);
#98436=ADVANCED_FACE('',(#13463),#7434,.T.);
#98437=ADVANCED_FACE('',(#13464),#92506,.F.);
#98438=ADVANCED_FACE('',(#13465),#7435,.F.);
#98439=ADVANCED_FACE('',(#13466),#92507,.F.);
#98440=ADVANCED_FACE('',(#13467),#7436,.F.);
#98441=ADVANCED_FACE('',(#13468),#7437,.T.);
#98442=ADVANCED_FACE('',(#13469),#92508,.F.);
#98443=ADVANCED_FACE('',(#13470),#7438,.T.);
#98444=ADVANCED_FACE('',(#13471),#92509,.F.);
#98445=ADVANCED_FACE('',(#13472),#7439,.T.);
#98446=ADVANCED_FACE('',(#13473),#92510,.F.);
#98447=ADVANCED_FACE('',(#13474),#7440,.T.);
#98448=ADVANCED_FACE('',(#13475),#92511,.F.);
#98449=ADVANCED_FACE('',(#13476),#7441,.T.);
#98450=ADVANCED_FACE('',(#13477),#92512,.F.);
#98451=ADVANCED_FACE('',(#13478),#7442,.T.);
#98452=ADVANCED_FACE('',(#13479),#92513,.F.);
#98453=ADVANCED_FACE('',(#13480),#7443,.T.);
#98454=ADVANCED_FACE('',(#13481),#7444,.T.);
#98455=ADVANCED_FACE('',(#13482),#92514,.F.);
#98456=ADVANCED_FACE('',(#13483),#7445,.F.);
#98457=ADVANCED_FACE('',(#13484),#7446,.F.);
#98458=ADVANCED_FACE('',(#13485),#7447,.T.);
#98459=ADVANCED_FACE('',(#13486),#92515,.F.);
#98460=ADVANCED_FACE('',(#13487),#7448,.T.);
#98461=ADVANCED_FACE('',(#13488),#92516,.F.);
#98462=ADVANCED_FACE('',(#13489),#7449,.T.);
#98463=ADVANCED_FACE('',(#13490),#92517,.F.);
#98464=ADVANCED_FACE('',(#13491),#7450,.T.);
#98465=ADVANCED_FACE('',(#13492),#92518,.F.);
#98466=ADVANCED_FACE('',(#13493),#7451,.F.);
#98467=ADVANCED_FACE('',(#13494),#7452,.F.);
#98468=ADVANCED_FACE('',(#13495),#7453,.F.);
#98469=ADVANCED_FACE('',(#13496),#7454,.F.);
#98470=ADVANCED_FACE('',(#13497),#7455,.F.);
#98471=ADVANCED_FACE('',(#13498),#7456,.F.);
#98472=ADVANCED_FACE('',(#13499),#92519,.F.);
#98473=ADVANCED_FACE('',(#13500),#7457,.F.);
#98474=ADVANCED_FACE('',(#13501),#92520,.F.);
#98475=ADVANCED_FACE('',(#13502),#7458,.F.);
#98476=ADVANCED_FACE('',(#13503),#92521,.F.);
#98477=ADVANCED_FACE('',(#13504),#7459,.F.);
#98478=ADVANCED_FACE('',(#13505),#92522,.T.);
#98479=ADVANCED_FACE('',(#13506),#7460,.F.);
#98480=ADVANCED_FACE('',(#13507),#7461,.F.);
#98481=ADVANCED_FACE('',(#13508),#7462,.F.);
#98482=ADVANCED_FACE('',(#13509),#7463,.F.);
#98483=ADVANCED_FACE('',(#13510),#7464,.F.);
#98484=ADVANCED_FACE('',(#13511),#7465,.F.);
#98485=ADVANCED_FACE('',(#13512),#7466,.F.);
#98486=ADVANCED_FACE('',(#13513),#7467,.F.);
#98487=ADVANCED_FACE('',(#13514),#92523,.T.);
#98488=ADVANCED_FACE('',(#13515),#7468,.F.);
#98489=ADVANCED_FACE('',(#13516),#92524,.F.);
#98490=ADVANCED_FACE('',(#13517),#7469,.F.);
#98491=ADVANCED_FACE('',(#13518),#92525,.F.);
#98492=ADVANCED_FACE('',(#13519),#7470,.F.);
#98493=ADVANCED_FACE('',(#13520),#92526,.F.);
#98494=ADVANCED_FACE('',(#13521),#7471,.F.);
#98495=ADVANCED_FACE('',(#13522),#7472,.F.);
#98496=ADVANCED_FACE('',(#13523),#7473,.F.);
#98497=ADVANCED_FACE('',(#13524),#7474,.F.);
#98498=ADVANCED_FACE('',(#13525),#92527,.F.);
#98499=ADVANCED_FACE('',(#13526),#7475,.F.);
#98500=ADVANCED_FACE('',(#13527),#92528,.F.);
#98501=ADVANCED_FACE('',(#13528),#7476,.F.);
#98502=ADVANCED_FACE('',(#13529),#92529,.F.);
#98503=ADVANCED_FACE('',(#13530),#7477,.F.);
#98504=ADVANCED_FACE('',(#13531),#92530,.T.);
#98505=ADVANCED_FACE('',(#13532),#7478,.F.);
#98506=ADVANCED_FACE('',(#13533),#7479,.F.);
#98507=ADVANCED_FACE('',(#13534),#7480,.F.);
#98508=ADVANCED_FACE('',(#13535),#7481,.F.);
#98509=ADVANCED_FACE('',(#13536),#92531,.T.);
#98510=ADVANCED_FACE('',(#13537),#7482,.F.);
#98511=ADVANCED_FACE('',(#13538),#7483,.F.);
#98512=ADVANCED_FACE('',(#13539),#7484,.F.);
#98513=ADVANCED_FACE('',(#13540),#7485,.F.);
#98514=ADVANCED_FACE('',(#13541),#92532,.T.);
#98515=ADVANCED_FACE('',(#13542),#7486,.F.);
#98516=ADVANCED_FACE('',(#13543),#92533,.F.);
#98517=ADVANCED_FACE('',(#13544),#7487,.F.);
#98518=ADVANCED_FACE('',(#13545),#92534,.F.);
#98519=ADVANCED_FACE('',(#13546),#7488,.F.);
#98520=ADVANCED_FACE('',(#13547),#92535,.F.);
#98521=ADVANCED_FACE('',(#13548),#7489,.F.);
#98522=ADVANCED_FACE('',(#13549),#7490,.F.);
#98523=ADVANCED_FACE('',(#13550),#7491,.F.);
#98524=ADVANCED_FACE('',(#13551),#7492,.F.);
#98525=ADVANCED_FACE('',(#13552),#92536,.F.);
#98526=ADVANCED_FACE('',(#13553),#7493,.F.);
#98527=ADVANCED_FACE('',(#13554),#92537,.F.);
#98528=ADVANCED_FACE('',(#13555),#7494,.F.);
#98529=ADVANCED_FACE('',(#13556),#92538,.F.);
#98530=ADVANCED_FACE('',(#13557),#7495,.F.);
#98531=ADVANCED_FACE('',(#13558),#92539,.T.);
#98532=ADVANCED_FACE('',(#13559),#7496,.F.);
#98533=ADVANCED_FACE('',(#13560),#7497,.F.);
#98534=ADVANCED_FACE('',(#13561),#7498,.F.);
#98535=ADVANCED_FACE('',(#13562),#7499,.F.);
#98536=ADVANCED_FACE('',(#13563),#7500,.F.);
#98537=ADVANCED_FACE('',(#13564),#7501,.F.);
#98538=ADVANCED_FACE('',(#13565),#7502,.F.);
#98539=ADVANCED_FACE('',(#13566),#92540,.T.);
#98540=ADVANCED_FACE('',(#13567),#7503,.F.);
#98541=ADVANCED_FACE('',(#13568),#92541,.F.);
#98542=ADVANCED_FACE('',(#13569),#7504,.F.);
#98543=ADVANCED_FACE('',(#13570),#92542,.F.);
#98544=ADVANCED_FACE('',(#13571),#7505,.F.);
#98545=ADVANCED_FACE('',(#13572),#92543,.F.);
#98546=ADVANCED_FACE('',(#13573),#7506,.F.);
#98547=ADVANCED_FACE('',(#13574),#7507,.F.);
#98548=ADVANCED_FACE('',(#13575),#7508,.F.);
#98549=ADVANCED_FACE('',(#13576),#7509,.F.);
#98550=ADVANCED_FACE('',(#13577),#92544,.F.);
#98551=ADVANCED_FACE('',(#13578),#7510,.F.);
#98552=ADVANCED_FACE('',(#13579),#92545,.F.);
#98553=ADVANCED_FACE('',(#13580),#7511,.F.);
#98554=ADVANCED_FACE('',(#13581),#92546,.F.);
#98555=ADVANCED_FACE('',(#13582),#7512,.F.);
#98556=ADVANCED_FACE('',(#13583),#92547,.T.);
#98557=ADVANCED_FACE('',(#13584),#7513,.F.);
#98558=ADVANCED_FACE('',(#13585),#7514,.F.);
#98559=ADVANCED_FACE('',(#13586),#7515,.F.);
#98560=ADVANCED_FACE('',(#13587),#7516,.F.);
#98561=ADVANCED_FACE('',(#13588),#92548,.T.);
#98562=ADVANCED_FACE('',(#13589),#7517,.F.);
#98563=ADVANCED_FACE('',(#13590),#7518,.F.);
#98564=ADVANCED_FACE('',(#13591),#7519,.F.);
#98565=ADVANCED_FACE('',(#13592),#7520,.F.);
#98566=ADVANCED_FACE('',(#13593),#92549,.T.);
#98567=ADVANCED_FACE('',(#13594),#7521,.F.);
#98568=ADVANCED_FACE('',(#13595),#92550,.F.);
#98569=ADVANCED_FACE('',(#13596),#7522,.F.);
#98570=ADVANCED_FACE('',(#13597),#92551,.F.);
#98571=ADVANCED_FACE('',(#13598),#7523,.F.);
#98572=ADVANCED_FACE('',(#13599),#92552,.F.);
#98573=ADVANCED_FACE('',(#13600),#7524,.F.);
#98574=ADVANCED_FACE('',(#13601),#7525,.F.);
#98575=ADVANCED_FACE('',(#13602),#7526,.F.);
#98576=ADVANCED_FACE('',(#13603),#7527,.F.);
#98577=ADVANCED_FACE('',(#13604),#92553,.F.);
#98578=ADVANCED_FACE('',(#13605),#7528,.F.);
#98579=ADVANCED_FACE('',(#13606),#92554,.F.);
#98580=ADVANCED_FACE('',(#13607),#7529,.F.);
#98581=ADVANCED_FACE('',(#13608),#92555,.F.);
#98582=ADVANCED_FACE('',(#13609),#7530,.F.);
#98583=ADVANCED_FACE('',(#13610),#92556,.T.);
#98584=ADVANCED_FACE('',(#13611),#7531,.F.);
#98585=ADVANCED_FACE('',(#13612),#7532,.F.);
#98586=ADVANCED_FACE('',(#13613),#7533,.F.);
#98587=ADVANCED_FACE('',(#13614),#7534,.F.);
#98588=ADVANCED_FACE('',(#13615),#7535,.F.);
#98589=ADVANCED_FACE('',(#13616),#7536,.F.);
#98590=ADVANCED_FACE('',(#13617),#7537,.F.);
#98591=ADVANCED_FACE('',(#13618),#92557,.T.);
#98592=ADVANCED_FACE('',(#13619),#7538,.F.);
#98593=ADVANCED_FACE('',(#13620),#92558,.F.);
#98594=ADVANCED_FACE('',(#13621),#7539,.F.);
#98595=ADVANCED_FACE('',(#13622),#92559,.F.);
#98596=ADVANCED_FACE('',(#13623),#7540,.F.);
#98597=ADVANCED_FACE('',(#13624),#92560,.F.);
#98598=ADVANCED_FACE('',(#13625),#7541,.F.);
#98599=ADVANCED_FACE('',(#13626),#7542,.F.);
#98600=ADVANCED_FACE('',(#13627),#7543,.F.);
#98601=ADVANCED_FACE('',(#13628),#7544,.F.);
#98602=ADVANCED_FACE('',(#13629),#92561,.F.);
#98603=ADVANCED_FACE('',(#13630),#7545,.F.);
#98604=ADVANCED_FACE('',(#13631),#92562,.F.);
#98605=ADVANCED_FACE('',(#13632),#7546,.F.);
#98606=ADVANCED_FACE('',(#13633),#92563,.F.);
#98607=ADVANCED_FACE('',(#13634),#7547,.F.);
#98608=ADVANCED_FACE('',(#13635),#92564,.T.);
#98609=ADVANCED_FACE('',(#13636),#7548,.F.);
#98610=ADVANCED_FACE('',(#13637),#7549,.F.);
#98611=ADVANCED_FACE('',(#13638),#7550,.F.);
#98612=ADVANCED_FACE('',(#13639),#7551,.F.);
#98613=ADVANCED_FACE('',(#13640),#92565,.T.);
#98614=ADVANCED_FACE('',(#13641),#7552,.F.);
#98615=ADVANCED_FACE('',(#13642),#7553,.F.);
#98616=ADVANCED_FACE('',(#13643),#7554,.F.);
#98617=ADVANCED_FACE('',(#13644),#7555,.F.);
#98618=ADVANCED_FACE('',(#13645),#92566,.T.);
#98619=ADVANCED_FACE('',(#13646),#7556,.F.);
#98620=ADVANCED_FACE('',(#13647),#92567,.F.);
#98621=ADVANCED_FACE('',(#13648),#7557,.F.);
#98622=ADVANCED_FACE('',(#13649),#92568,.F.);
#98623=ADVANCED_FACE('',(#13650),#7558,.F.);
#98624=ADVANCED_FACE('',(#13651),#92569,.F.);
#98625=ADVANCED_FACE('',(#13652),#7559,.F.);
#98626=ADVANCED_FACE('',(#13653),#7560,.F.);
#98627=ADVANCED_FACE('',(#13654),#7561,.F.);
#98628=ADVANCED_FACE('',(#13655),#7562,.F.);
#98629=ADVANCED_FACE('',(#13656),#92570,.F.);
#98630=ADVANCED_FACE('',(#13657),#7563,.F.);
#98631=ADVANCED_FACE('',(#13658),#92571,.F.);
#98632=ADVANCED_FACE('',(#13659),#7564,.F.);
#98633=ADVANCED_FACE('',(#13660),#92572,.F.);
#98634=ADVANCED_FACE('',(#13661),#7565,.F.);
#98635=ADVANCED_FACE('',(#13662),#92573,.T.);
#98636=ADVANCED_FACE('',(#13663),#7566,.F.);
#98637=ADVANCED_FACE('',(#13664),#7567,.F.);
#98638=ADVANCED_FACE('',(#13665),#7568,.F.);
#98639=ADVANCED_FACE('',(#13666),#7569,.F.);
#98640=ADVANCED_FACE('',(#13667),#7570,.F.);
#98641=ADVANCED_FACE('',(#13668),#7571,.F.);
#98642=ADVANCED_FACE('',(#13669),#92574,.T.);
#98643=ADVANCED_FACE('',(#13670),#7572,.F.);
#98644=ADVANCED_FACE('',(#13671),#92575,.F.);
#98645=ADVANCED_FACE('',(#13672),#7573,.F.);
#98646=ADVANCED_FACE('',(#13673),#92576,.F.);
#98647=ADVANCED_FACE('',(#13674),#7574,.F.);
#98648=ADVANCED_FACE('',(#13675),#92577,.F.);
#98649=ADVANCED_FACE('',(#13676),#7575,.F.);
#98650=ADVANCED_FACE('',(#13677),#7576,.F.);
#98651=ADVANCED_FACE('',(#13678),#7577,.F.);
#98652=ADVANCED_FACE('',(#13679),#7578,.F.);
#98653=ADVANCED_FACE('',(#13680),#92578,.F.);
#98654=ADVANCED_FACE('',(#13681),#7579,.F.);
#98655=ADVANCED_FACE('',(#13682),#92579,.F.);
#98656=ADVANCED_FACE('',(#13683),#7580,.F.);
#98657=ADVANCED_FACE('',(#13684),#92580,.F.);
#98658=ADVANCED_FACE('',(#13685),#7581,.F.);
#98659=ADVANCED_FACE('',(#13686),#92581,.T.);
#98660=ADVANCED_FACE('',(#13687),#7582,.F.);
#98661=ADVANCED_FACE('',(#13688),#7583,.F.);
#98662=ADVANCED_FACE('',(#13689),#7584,.F.);
#98663=ADVANCED_FACE('',(#13690),#7585,.F.);
#98664=ADVANCED_FACE('',(#13691),#92582,.T.);
#98665=ADVANCED_FACE('',(#13692),#7586,.F.);
#98666=ADVANCED_FACE('',(#13693),#7587,.F.);
#98667=ADVANCED_FACE('',(#13694),#7588,.F.);
#98668=ADVANCED_FACE('',(#13695),#7589,.F.);
#98669=ADVANCED_FACE('',(#13696),#92583,.T.);
#98670=ADVANCED_FACE('',(#13697),#7590,.F.);
#98671=ADVANCED_FACE('',(#13698),#92584,.F.);
#98672=ADVANCED_FACE('',(#13699),#7591,.F.);
#98673=ADVANCED_FACE('',(#13700),#92585,.F.);
#98674=ADVANCED_FACE('',(#13701),#7592,.F.);
#98675=ADVANCED_FACE('',(#13702),#92586,.F.);
#98676=ADVANCED_FACE('',(#13703),#7593,.F.);
#98677=ADVANCED_FACE('',(#13704),#7594,.F.);
#98678=ADVANCED_FACE('',(#13705),#7595,.F.);
#98679=ADVANCED_FACE('',(#13706),#7596,.F.);
#98680=ADVANCED_FACE('',(#13707),#7597,.F.);
#98681=ADVANCED_FACE('',(#13708),#7598,.T.);
#98682=ADVANCED_FACE('',(#13709),#7599,.T.);
#98683=ADVANCED_FACE('',(#13710),#7600,.F.);
#98684=ADVANCED_FACE('',(#13711),#7601,.F.);
#98685=ADVANCED_FACE('',(#13712),#7602,.T.);
#98686=ADVANCED_FACE('',(#13713),#7603,.F.);
#98687=ADVANCED_FACE('',(#13714),#7604,.T.);
#98688=ADVANCED_FACE('',(#13715),#7605,.T.);
#98689=ADVANCED_FACE('',(#13716),#7606,.T.);
#98690=ADVANCED_FACE('',(#13717,#6444),#7607,.F.);
#98691=ADVANCED_FACE('',(#13718),#7608,.T.);
#98692=ADVANCED_FACE('',(#13719),#7609,.T.);
#98693=ADVANCED_FACE('',(#13720),#7610,.T.);
#98694=ADVANCED_FACE('',(#13721),#7611,.T.);
#98695=ADVANCED_FACE('',(#13722,#6445),#7612,.F.);
#98696=ADVANCED_FACE('',(#13723),#7613,.F.);
#98697=CLOSED_SHELL('',(#92587,#92588,#92589,#92590,#92591,#92592,#92593,
#92594,#92595,#92596,#92597,#92598,#92599,#92600,#92601,#92602,#92603,#92604,
#92605,#92606,#92607,#92608,#92609,#92610,#92611,#92612,#92613,#92614,#92615,
#92616,#92617,#92618,#92619,#92620,#92621,#92622,#92623,#92624,#92625,#92626,
#92627,#92628,#92629));
#98698=CLOSED_SHELL('',(#92630,#92631,#92632,#92633,#92634,#92635,#92636,
#92637,#92638,#92639));
#98699=CLOSED_SHELL('',(#92640,#92641,#92642,#92643,#92644,#92645,#92646,
#92647,#92648,#92649,#92650,#92651,#92652,#92653,#92654,#92655,#92656,#92657,
#92658,#92659,#92660,#92661,#92662,#92663,#92664,#92665,#92666,#92667,#92668,
#92669,#92670,#92671,#92672,#92673,#92674,#92675,#92676,#92677,#92678,#92679));
#98700=CLOSED_SHELL('',(#92680,#92681,#92682,#92683,#92684,#92685,#92686,
#92687,#92688,#92689,#92690,#92691,#92692,#92693,#92694,#92695,#92696,#92697,
#92698,#92699,#92700,#92701,#92702,#92703,#92704,#92705,#92706,#92707,#92708,
#92709,#92710,#92711,#92712,#92713,#92714,#92715));
#98701=CLOSED_SHELL('',(#92716,#92717,#92718,#92719));
#98702=CLOSED_SHELL('',(#92720,#92721,#92722,#92723));
#98703=CLOSED_SHELL('',(#92724,#92725,#92726,#92727));
#98704=CLOSED_SHELL('',(#92728,#92729,#92730,#92731));
#98705=CLOSED_SHELL('',(#92732,#92733,#92734,#92735,#92736,#92737));
#98706=CLOSED_SHELL('',(#92738,#92739,#92740,#92741,#92742,#92743));
#98707=CLOSED_SHELL('',(#92744,#92745,#92746,#92747));
#98708=CLOSED_SHELL('',(#92748,#92749,#92750,#92751,#92752,#92753,#92754,
#92755,#92756,#92757,#92758,#92759,#92760,#92761,#92762,#92763,#92764,#92765,
#92766,#92767,#92768,#92769,#92770,#92771,#92772,#92773,#92774,#92775,#92776,
#92777,#92778,#92779,#92780,#92781,#92782,#92783,#92784,#92785,#92786,#92787,
#92788,#92789,#92790,#92791,#92792,#92793,#92794,#92795,#92796,#92797,#92798,
#92799,#92800,#92801,#92802,#92803,#92804,#92805,#92806,#92807,#92808,#92809,
#92810,#92811,#92812,#92813,#92814,#92815,#92816,#92817,#92818,#92819,#92820,
#92821,#92822,#92823,#92824,#92825,#92826,#92827,#92828,#92829,#92830,#92831,
#92832,#92833,#92834,#92835,#92836,#92837,#92838,#92839,#92840,#92841,#92842,
#92843,#92844,#92845,#92846,#92847,#92848,#92849,#92850,#92851,#92852,#92853,
#92854,#92855,#92856,#92857,#92858,#92859,#92860,#92861,#92862,#92863,#92864,
#92865,#92866,#92867,#92868,#92869,#92870,#92871,#92872,#92873,#92874,#92875,
#92876,#92877,#92878,#92879,#92880,#92881,#92882,#92883,#92884,#92885,#92886,
#92887,#92888,#92889,#92890,#92891,#92892,#92893,#92894,#92895,#92896,#92897,
#92898,#92899,#92900,#92901,#92902,#92903,#92904,#92905,#92906,#92907,#92908,
#92909,#92910,#92911,#92912,#92913,#92914,#92915,#92916,#92917,#92918,#92919,
#92920,#92921,#92922,#92923,#92924,#92925,#92926,#92927,#92928,#92929,#92930,
#92931,#92932,#92933,#92934,#92935,#92936,#92937,#92938,#92939,#92940,#92941,
#92942,#92943,#92944,#92945,#92946,#92947,#92948,#92949,#92950,#92951,#92952,
#92953,#92954,#92955,#92956,#92957,#92958,#92959,#92960,#92961,#92962,#92963,
#92964,#92965,#92966,#92967,#92968,#92969,#92970,#92971,#92972,#92973,#92974,
#92975,#92976,#92977,#92978,#92979,#92980,#92981,#92982,#92983,#92984,#92985,
#92986,#92987,#92988,#92989,#92990,#92991,#92992,#92993,#92994,#92995,#92996,
#92997,#92998,#92999,#93000,#93001,#93002,#93003,#93004,#93005,#93006,#93007,
#93008,#93009,#93010,#93011,#93012,#93013,#93014,#93015,#93016,#93017,#93018,
#93019,#93020,#93021,#93022,#93023,#93024,#93025,#93026,#93027,#93028,#93029,
#93030,#93031,#93032,#93033,#93034,#93035,#93036,#93037,#93038,#93039,#93040,
#93041,#93042,#93043,#93044,#93045,#93046,#93047,#93048,#93049,#93050,#93051,
#93052,#93053,#93054,#93055,#93056,#93057,#93058,#93059,#93060,#93061,#93062,
#93063,#93064,#93065,#93066,#93067,#93068,#93069,#93070,#93071,#93072,#93073,
#93074,#93075,#93076,#93077,#93078,#93079,#93080,#93081,#93082,#93083,#93084,
#93085,#93086,#93087,#93088,#93089,#93090,#93091,#93092,#93093,#93094,#93095,
#93096,#93097,#93098,#93099,#93100,#93101,#93102,#93103,#93104,#93105,#93106,
#93107,#93108,#93109,#93110,#93111,#93112,#93113,#93114,#93115,#93116,#93117,
#93118,#93119,#93120,#93121,#93122,#93123,#93124,#93125,#93126,#93127,#93128,
#93129,#93130,#93131,#93132,#93133,#93134,#93135,#93136,#93137,#93138,#93139,
#93140,#93141,#93142,#93143,#93144,#93145,#93146,#93147,#93148,#93149,#93150,
#93151,#93152,#93153,#93154,#93155,#93156,#93157,#93158,#93159,#93160,#93161,
#93162,#93163,#93164,#93165,#93166,#93167,#93168,#93169,#93170,#93171,#93172,
#93173,#93174,#93175,#93176,#93177,#93178,#93179,#93180,#93181,#93182,#93183,
#93184,#93185,#93186,#93187,#93188,#93189,#93190,#93191,#93192,#93193,#93194,
#93195,#93196,#93197,#93198,#93199,#93200,#93201,#93202,#93203,#93204,#93205,
#93206,#93207,#93208,#93209,#93210,#93211,#93212,#93213,#93214,#93215,#93216,
#93217,#93218,#93219,#93220,#93221,#93222,#93223,#93224,#93225,#93226,#93227,
#93228,#93229,#93230,#93231,#93232,#93233,#93234,#93235,#93236,#93237,#93238,
#93239,#93240,#93241,#93242,#93243,#93244,#93245,#93246,#93247,#93248,#93249,
#93250,#93251,#93252,#93253,#93254,#93255,#93256,#93257,#93258,#93259,#93260,
#93261,#93262,#93263,#93264,#93265,#93266,#93267,#93268,#93269,#93270,#93271,
#93272,#93273,#93274,#93275,#93276,#93277,#93278,#93279,#93280,#93281,#93282,
#93283,#93284,#93285,#93286,#93287,#93288,#93289,#93290,#93291,#93292,#93293,
#93294,#93295,#93296,#93297,#93298,#93299,#93300,#93301,#93302,#93303,#93304,
#93305,#93306,#93307,#93308,#93309,#93310,#93311,#93312,#93313,#93314,#93315,
#93316,#93317,#93318,#93319,#93320,#93321,#93322,#93323,#93324,#93325,#93326,
#93327,#93328,#93329,#93330,#93331,#93332,#93333,#93334,#93335,#93336,#93337,
#93338,#93339,#93340,#93341,#93342,#93343,#93344,#93345,#93346,#93347,#93348,
#93349,#93350,#93351,#93352,#93353,#93354,#93355,#93356,#93357,#93358,#93359,
#93360,#93361,#93362,#93363,#93364,#93365,#93366,#93367,#93368,#93369,#93370,
#93371,#93372,#93373,#93374,#93375,#93376,#93377,#93378,#93379,#93380,#93381,
#93382,#93383,#93384,#93385,#93386,#93387,#93388,#93389,#93390,#93391,#93392,
#93393,#93394,#93395,#93396,#93397,#93398,#93399,#93400,#93401,#93402,#93403,
#93404,#93405,#93406,#93407,#93408,#93409,#93410,#93411,#93412,#93413,#93414,
#93415,#93416,#93417,#93418,#93419,#93420,#93421,#93422,#93423,#93424,#93425,
#93426,#93427,#93428,#93429,#93430,#93431,#93432,#93433,#93434,#93435,#93436,
#93437,#93438,#93439,#93440,#93441,#93442,#93443,#93444,#93445,#93446,#93447,
#93448,#93449,#93450,#93451,#93452,#93453,#93454,#93455,#93456,#93457,#93458,
#93459,#93460,#93461,#93462,#93463,#93464,#93465,#93466,#93467,#93468,#93469,
#93470,#93471,#93472,#93473,#93474,#93475,#93476,#93477,#93478,#93479,#93480,
#93481,#93482,#93483,#93484,#93485,#93486,#93487,#93488,#93489,#93490,#93491,
#93492,#93493,#93494,#93495,#93496,#93497,#93498,#93499,#93500,#93501,#93502,
#93503,#93504,#93505,#93506,#93507,#93508,#93509,#93510,#93511,#93512,#93513,
#93514,#93515,#93516,#93517,#93518,#93519,#93520,#93521,#93522,#93523,#93524,
#93525,#93526,#93527,#93528,#93529,#93530,#93531,#93532,#93533,#93534,#93535,
#93536,#93537,#93538,#93539,#93540,#93541,#93542,#93543,#93544,#93545,#93546,
#93547,#93548,#93549,#93550,#93551,#93552,#93553,#93554,#93555,#93556,#93557,
#93558,#93559,#93560,#93561,#93562,#93563,#93564,#93565,#93566,#93567,#93568,
#93569,#93570,#93571,#93572,#93573,#93574,#93575,#93576,#93577,#93578,#93579,
#93580,#93581,#93582,#93583,#93584,#93585,#93586,#93587,#93588,#93589,#93590,
#93591,#93592,#93593,#93594,#93595,#93596,#93597,#93598,#93599,#93600,#93601,
#93602,#93603,#93604,#93605,#93606,#93607,#93608,#93609,#93610,#93611,#93612,
#93613,#93614,#93615,#93616,#93617,#93618,#93619,#93620,#93621,#93622,#93623,
#93624,#93625,#93626,#93627,#93628,#93629,#93630,#93631,#93632,#93633,#93634,
#93635,#93636,#93637,#93638,#93639,#93640,#93641,#93642,#93643,#93644,#93645,
#93646,#93647,#93648,#93649,#93650,#93651,#93652,#93653,#93654,#93655,#93656,
#93657,#93658,#93659,#93660,#93661,#93662,#93663,#93664,#93665,#93666,#93667,
#93668,#93669,#93670,#93671,#93672,#93673,#93674,#93675,#93676,#93677,#93678,
#93679,#93680,#93681,#93682,#93683,#93684,#93685,#93686,#93687,#93688,#93689,
#93690,#93691,#93692,#93693,#93694,#93695,#93696,#93697,#93698,#93699,#93700,
#93701,#93702,#93703,#93704,#93705,#93706,#93707,#93708,#93709,#93710,#93711,
#93712,#93713,#93714,#93715,#93716,#93717,#93718,#93719,#93720,#93721,#93722,
#93723,#93724,#93725,#93726,#93727,#93728,#93729,#93730,#93731,#93732,#93733,
#93734,#93735,#93736,#93737,#93738,#93739,#93740,#93741,#93742,#93743,#93744,
#93745,#93746,#93747,#93748,#93749,#93750,#93751,#93752,#93753,#93754,#93755,
#93756,#93757,#93758,#93759,#93760,#93761,#93762,#93763,#93764,#93765,#93766,
#93767,#93768,#93769,#93770,#93771,#93772,#93773,#93774,#93775,#93776,#93777,
#93778,#93779,#93780,#93781,#93782,#93783,#93784,#93785,#93786,#93787,#93788,
#93789,#93790,#93791,#93792,#93793,#93794,#93795,#93796,#93797,#93798,#93799,
#93800,#93801,#93802,#93803,#93804,#93805,#93806,#93807,#93808,#93809,#93810,
#93811,#93812,#93813,#93814,#93815,#93816,#93817,#93818,#93819,#93820,#93821,
#93822,#93823,#93824,#93825,#93826,#93827,#93828,#93829,#93830,#93831,#93832,
#93833,#93834,#93835,#93836,#93837,#93838,#93839,#93840,#93841,#93842,#93843,
#93844,#93845,#93846,#93847,#93848,#93849,#93850,#93851,#93852,#93853,#93854,
#93855,#93856,#93857,#93858,#93859,#93860,#93861,#93862,#93863,#93864,#93865,
#93866,#93867,#93868,#93869,#93870,#93871,#93872,#93873,#93874,#93875,#93876,
#93877,#93878,#93879,#93880,#93881,#93882,#93883,#93884,#93885,#93886,#93887,
#93888,#93889,#93890,#93891,#93892,#93893,#93894,#93895,#93896,#93897,#93898,
#93899,#93900,#93901,#93902,#93903,#93904,#93905,#93906,#93907,#93908,#93909,
#93910,#93911,#93912,#93913,#93914,#93915,#93916,#93917,#93918,#93919,#93920,
#93921,#93922,#93923,#93924,#93925,#93926,#93927,#93928,#93929,#93930,#93931,
#93932,#93933,#93934,#93935,#93936,#93937,#93938,#93939,#93940,#93941,#93942,
#93943,#93944,#93945,#93946,#93947,#93948,#93949,#93950,#93951,#93952,#93953,
#93954,#93955,#93956,#93957,#93958,#93959,#93960,#93961,#93962,#93963,#93964,
#93965,#93966,#93967,#93968,#93969,#93970,#93971,#93972,#93973,#93974,#93975,
#93976,#93977,#93978,#93979,#93980,#93981,#93982,#93983,#93984,#93985,#93986,
#93987,#93988,#93989,#93990,#93991,#93992,#93993,#93994,#93995,#93996,#93997,
#93998,#93999,#94000,#94001,#94002,#94003,#94004,#94005,#94006,#94007,#94008,
#94009,#94010,#94011,#94012,#94013,#94014,#94015,#94016,#94017,#94018,#94019,
#94020,#94021,#94022,#94023,#94024,#94025,#94026,#94027,#94028,#94029,#94030,
#94031,#94032,#94033,#94034,#94035,#94036,#94037,#94038,#94039,#94040,#94041,
#94042,#94043,#94044,#94045,#94046,#94047,#94048,#94049,#94050,#94051,#94052,
#94053,#94054,#94055,#94056,#94057,#94058,#94059,#94060,#94061,#94062,#94063,
#94064,#94065,#94066,#94067,#94068,#94069,#94070,#94071,#94072,#94073,#94074,
#94075,#94076,#94077,#94078,#94079,#94080,#94081,#94082,#94083,#94084,#94085,
#94086,#94087,#94088,#94089,#94090,#94091,#94092,#94093,#94094,#94095,#94096,
#94097,#94098,#94099,#94100,#94101,#94102,#94103,#94104,#94105,#94106,#94107,
#94108,#94109,#94110,#94111,#94112,#94113,#94114,#94115,#94116,#94117,#94118,
#94119,#94120,#94121,#94122,#94123,#94124,#94125,#94126,#94127,#94128,#94129,
#94130,#94131,#94132,#94133,#94134,#94135,#94136,#94137,#94138,#94139,#94140,
#94141,#94142,#94143,#94144,#94145,#94146,#94147,#94148,#94149,#94150,#94151,
#94152,#94153,#94154,#94155,#94156,#94157,#94158,#94159,#94160,#94161,#94162,
#94163,#94164,#94165,#94166,#94167,#94168,#94169,#94170,#94171,#94172,#94173,
#94174,#94175,#94176,#94177,#94178,#94179,#94180,#94181,#94182,#94183,#94184,
#94185,#94186,#94187,#94188,#94189,#94190,#94191,#94192,#94193,#94194,#94195,
#94196,#94197,#94198,#94199,#94200,#94201,#94202,#94203,#94204,#94205,#94206,
#94207,#94208,#94209,#94210,#94211,#94212,#94213,#94214,#94215,#94216,#94217,
#94218,#94219,#94220,#94221,#94222,#94223,#94224,#94225,#94226,#94227,#94228,
#94229,#94230,#94231,#94232,#94233,#94234,#94235,#94236,#94237,#94238,#94239,
#94240,#94241,#94242,#94243,#94244,#94245,#94246,#94247,#94248,#94249,#94250,
#94251,#94252,#94253,#94254,#94255,#94256,#94257,#94258,#94259,#94260,#94261,
#94262,#94263,#94264,#94265,#94266,#94267,#94268,#94269,#94270,#94271,#94272,
#94273,#94274,#94275,#94276,#94277,#94278,#94279,#94280,#94281,#94282,#94283,
#94284,#94285,#94286,#94287,#94288,#94289,#94290,#94291,#94292,#94293,#94294,
#94295,#94296,#94297,#94298,#94299,#94300,#94301,#94302,#94303,#94304,#94305,
#94306,#94307,#94308,#94309,#94310,#94311,#94312,#94313,#94314,#94315,#94316,
#94317,#94318,#94319,#94320,#94321,#94322,#94323,#94324,#94325,#94326,#94327,
#94328,#94329,#94330,#94331,#94332,#94333,#94334,#94335,#94336,#94337,#94338,
#94339,#94340,#94341,#94342,#94343,#94344,#94345,#94346,#94347,#94348,#94349,
#94350,#94351,#94352,#94353,#94354,#94355,#94356,#94357,#94358,#94359,#94360,
#94361,#94362,#94363,#94364,#94365,#94366,#94367,#94368,#94369,#94370,#94371,
#94372,#94373,#94374,#94375,#94376,#94377,#94378,#94379,#94380,#94381,#94382,
#94383,#94384,#94385,#94386,#94387,#94388,#94389,#94390,#94391,#94392,#94393,
#94394,#94395,#94396,#94397,#94398,#94399,#94400,#94401,#94402,#94403,#94404,
#94405,#94406,#94407,#94408,#94409,#94410,#94411,#94412,#94413,#94414,#94415,
#94416,#94417,#94418,#94419,#94420,#94421,#94422,#94423,#94424,#94425,#94426,
#94427,#94428,#94429,#94430,#94431,#94432,#94433,#94434,#94435,#94436,#94437,
#94438,#94439,#94440,#94441,#94442,#94443,#94444,#94445,#94446,#94447,#94448,
#94449,#94450,#94451,#94452,#94453,#94454,#94455,#94456,#94457,#94458,#94459,
#94460,#94461,#94462,#94463,#94464,#94465,#94466,#94467,#94468,#94469,#94470,
#94471,#94472,#94473,#94474,#94475,#94476,#94477,#94478,#94479,#94480,#94481,
#94482,#94483,#94484,#94485,#94486,#94487,#94488,#94489,#94490,#94491,#94492,
#94493,#94494,#94495,#94496,#94497,#94498,#94499,#94500,#94501,#94502,#94503,
#94504,#94505,#94506,#94507,#94508,#94509,#94510,#94511,#94512,#94513,#94514,
#94515,#94516,#94517,#94518,#94519,#94520,#94521,#94522,#94523,#94524,#94525,
#94526,#94527,#94528,#94529,#94530,#94531,#94532,#94533,#94534,#94535,#94536,
#94537,#94538,#94539,#94540,#94541,#94542,#94543,#94544,#94545,#94546,#94547,
#94548,#94549,#94550,#94551,#94552,#94553,#94554,#94555,#94556,#94557,#94558,
#94559,#94560,#94561,#94562,#94563,#94564,#94565,#94566,#94567,#94568,#94569,
#94570,#94571,#94572,#94573,#94574,#94575,#94576,#94577,#94578,#94579,#94580,
#94581,#94582,#94583,#94584,#94585,#94586,#94587,#94588,#94589,#94590,#94591,
#94592,#94593,#94594,#94595,#94596,#94597,#94598,#94599,#94600,#94601,#94602,
#94603,#94604,#94605,#94606,#94607,#94608,#94609,#94610,#94611,#94612,#94613,
#94614,#94615,#94616,#94617,#94618,#94619,#94620,#94621,#94622,#94623,#94624,
#94625,#94626,#94627,#94628,#94629,#94630,#94631,#94632,#94633,#94634,#94635,
#94636,#94637,#94638,#94639,#94640,#94641,#94642,#94643,#94644,#94645,#94646,
#94647,#94648,#94649,#94650,#94651,#94652,#94653,#94654,#94655,#94656,#94657,
#94658,#94659,#94660,#94661,#94662,#94663,#94664,#94665,#94666,#94667,#94668,
#94669,#94670,#94671,#94672,#94673,#94674,#94675,#94676,#94677,#94678,#94679,
#94680,#94681,#94682,#94683,#94684,#94685,#94686,#94687,#94688,#94689,#94690,
#94691,#94692,#94693,#94694,#94695,#94696,#94697,#94698,#94699,#94700,#94701,
#94702,#94703,#94704,#94705,#94706,#94707,#94708,#94709,#94710,#94711,#94712,
#94713,#94714,#94715,#94716,#94717,#94718,#94719,#94720,#94721,#94722,#94723,
#94724,#94725,#94726,#94727,#94728,#94729,#94730,#94731,#94732,#94733,#94734,
#94735,#94736,#94737,#94738,#94739,#94740,#94741,#94742,#94743,#94744,#94745,
#94746,#94747,#94748,#94749,#94750,#94751,#94752,#94753,#94754,#94755,#94756,
#94757,#94758,#94759,#94760,#94761,#94762,#94763,#94764,#94765,#94766,#94767,
#94768,#94769,#94770,#94771,#94772,#94773,#94774,#94775,#94776,#94777,#94778,
#94779,#94780,#94781,#94782,#94783,#94784,#94785,#94786,#94787,#94788,#94789,
#94790,#94791,#94792,#94793,#94794,#94795,#94796,#94797,#94798,#94799,#94800,
#94801,#94802,#94803,#94804,#94805,#94806,#94807,#94808,#94809,#94810,#94811,
#94812,#94813,#94814,#94815,#94816,#94817,#94818,#94819,#94820,#94821,#94822,
#94823,#94824,#94825,#94826,#94827,#94828,#94829,#94830,#94831,#94832,#94833,
#94834,#94835,#94836,#94837,#94838,#94839,#94840,#94841,#94842,#94843,#94844,
#94845,#94846,#94847,#94848,#94849,#94850,#94851,#94852,#94853,#94854,#94855,
#94856,#94857,#94858,#94859,#94860,#94861,#94862,#94863,#94864,#94865,#94866,
#94867,#94868,#94869,#94870,#94871,#94872,#94873,#94874,#94875,#94876,#94877,
#94878,#94879,#94880,#94881,#94882,#94883,#94884,#94885,#94886,#94887,#94888,
#94889,#94890,#94891,#94892,#94893,#94894,#94895,#94896,#94897,#94898,#94899,
#94900,#94901,#94902,#94903,#94904,#94905,#94906,#94907,#94908,#94909,#94910,
#94911,#94912,#94913,#94914,#94915,#94916,#94917,#94918,#94919,#94920,#94921,
#94922,#94923,#94924,#94925,#94926,#94927,#94928,#94929,#94930,#94931,#94932,
#94933,#94934,#94935,#94936,#94937,#94938,#94939,#94940,#94941,#94942,#94943,
#94944,#94945,#94946,#94947,#94948,#94949,#94950,#94951,#94952,#94953,#94954,
#94955,#94956,#94957,#94958,#94959,#94960,#94961,#94962,#94963,#94964,#94965,
#94966,#94967,#94968,#94969,#94970,#94971,#94972,#94973,#94974,#94975,#94976,
#94977,#94978,#94979,#94980,#94981,#94982,#94983,#94984,#94985,#94986,#94987,
#94988,#94989,#94990,#94991,#94992,#94993,#94994,#94995,#94996,#94997,#94998,
#94999,#95000,#95001,#95002,#95003,#95004,#95005,#95006,#95007,#95008,#95009,
#95010,#95011,#95012,#95013,#95014,#95015,#95016,#95017,#95018,#95019,#95020,
#95021,#95022,#95023,#95024,#95025,#95026,#95027,#95028,#95029,#95030,#95031,
#95032,#95033,#95034,#95035,#95036,#95037,#95038,#95039,#95040,#95041,#95042,
#95043,#95044,#95045,#95046,#95047,#95048,#95049,#95050,#95051,#95052,#95053,
#95054,#95055,#95056,#95057,#95058,#95059,#95060,#95061,#95062,#95063,#95064,
#95065,#95066,#95067,#95068,#95069,#95070,#95071,#95072,#95073,#95074,#95075,
#95076,#95077,#95078,#95079,#95080,#95081,#95082,#95083,#95084,#95085,#95086,
#95087,#95088,#95089,#95090,#95091,#95092,#95093,#95094,#95095,#95096,#95097,
#95098,#95099,#95100,#95101,#95102,#95103,#95104,#95105,#95106,#95107,#95108,
#95109,#95110,#95111,#95112,#95113,#95114,#95115,#95116,#95117,#95118,#95119,
#95120,#95121,#95122,#95123,#95124,#95125,#95126,#95127,#95128,#95129,#95130,
#95131,#95132,#95133,#95134,#95135,#95136,#95137,#95138,#95139,#95140,#95141,
#95142,#95143,#95144,#95145,#95146,#95147,#95148,#95149,#95150,#95151,#95152,
#95153,#95154,#95155,#95156,#95157,#95158,#95159,#95160,#95161,#95162,#95163,
#95164,#95165,#95166,#95167,#95168,#95169,#95170,#95171,#95172,#95173,#95174,
#95175,#95176,#95177,#95178,#95179,#95180,#95181,#95182,#95183,#95184,#95185,
#95186,#95187,#95188,#95189,#95190,#95191,#95192,#95193,#95194,#95195,#95196,
#95197,#95198,#95199,#95200,#95201,#95202,#95203,#95204,#95205,#95206,#95207,
#95208,#95209,#95210,#95211,#95212,#95213,#95214,#95215,#95216,#95217,#95218,
#95219,#95220,#95221,#95222,#95223,#95224,#95225,#95226,#95227,#95228,#95229,
#95230,#95231,#95232,#95233,#95234,#95235,#95236,#95237,#95238,#95239,#95240,
#95241,#95242,#95243,#95244,#95245,#95246,#95247,#95248,#95249,#95250,#95251,
#95252,#95253,#95254,#95255,#95256,#95257,#95258,#95259,#95260,#95261,#95262,
#95263,#95264,#95265,#95266,#95267,#95268,#95269,#95270,#95271,#95272,#95273,
#95274,#95275,#95276,#95277,#95278,#95279,#95280));
#98709=CLOSED_SHELL('',(#95281,#95282,#95283,#95284,#95285,#95286,#95287,
#95288,#95289,#95290,#95291,#95292,#95293,#95294,#95295,#95296,#95297,#95298,
#95299,#95300,#95301,#95302,#95303,#95304,#95305,#95306,#95307,#95308,#95309,
#95310,#95311,#95312,#95313,#95314,#95315,#95316,#95317,#95318,#95319,#95320,
#95321,#95322,#95323,#95324,#95325,#95326,#95327,#95328,#95329,#95330,#95331,
#95332,#95333,#95334,#95335,#95336,#95337,#95338,#95339,#95340,#95341,#95342,
#95343,#95344,#95345,#95346,#95347,#95348,#95349,#95350,#95351,#95352,#95353,
#95354,#95355,#95356,#95357,#95358,#95359,#95360,#95361,#95362,#95363,#95364,
#95365,#95366,#95367,#95368,#95369,#95370,#95371,#95372,#95373,#95374,#95375,
#95376,#95377,#95378,#95379,#95380,#95381,#95382,#95383,#95384,#95385,#95386,
#95387,#95388,#95389,#95390,#95391,#95392,#95393,#95394,#95395,#95396,#95397,
#95398,#95399,#95400,#95401,#95402,#95403,#95404,#95405,#95406,#95407,#95408,
#95409,#95410,#95411,#95412,#95413,#95414,#95415,#95416,#95417,#95418,#95419,
#95420,#95421,#95422,#95423,#95424,#95425,#95426,#95427,#95428,#95429,#95430,
#95431,#95432,#95433,#95434,#95435,#95436,#95437,#95438,#95439,#95440,#95441,
#95442,#95443,#95444,#95445,#95446,#95447,#95448,#95449,#95450,#95451,#95452,
#95453,#95454,#95455,#95456,#95457,#95458,#95459,#95460,#95461,#95462,#95463,
#95464,#95465,#95466,#95467,#95468,#95469,#95470,#95471,#95472,#95473,#95474,
#95475,#95476,#95477,#95478,#95479,#95480,#95481,#95482,#95483,#95484,#95485,
#95486,#95487,#95488,#95489,#95490,#95491,#95492,#95493,#95494,#95495,#95496,
#95497,#95498,#95499,#95500,#95501,#95502,#95503,#95504,#95505,#95506,#95507,
#95508,#95509,#95510,#95511,#95512,#95513,#95514,#95515,#95516,#95517,#95518,
#95519,#95520,#95521,#95522,#95523,#95524,#95525,#95526,#95527,#95528,#95529,
#95530,#95531,#95532,#95533,#95534,#95535,#95536,#95537,#95538,#95539,#95540,
#95541,#95542,#95543,#95544,#95545,#95546,#95547,#95548,#95549,#95550,#95551,
#95552,#95553,#95554,#95555,#95556,#95557,#95558,#95559,#95560,#95561,#95562,
#95563,#95564,#95565,#95566,#95567,#95568,#95569,#95570,#95571,#95572,#95573,
#95574,#95575,#95576,#95577,#95578,#95579,#95580,#95581,#95582,#95583,#95584,
#95585,#95586,#95587,#95588,#95589,#95590,#95591,#95592,#95593,#95594,#95595,
#95596,#95597,#95598,#95599,#95600,#95601,#95602,#95603,#95604,#95605,#95606,
#95607,#95608,#95609,#95610,#95611,#95612,#95613,#95614,#95615,#95616,#95617,
#95618,#95619,#95620,#95621,#95622,#95623,#95624,#95625,#95626,#95627,#95628,
#95629,#95630,#95631,#95632,#95633,#95634,#95635,#95636,#95637,#95638,#95639,
#95640,#95641,#95642,#95643,#95644,#95645,#95646,#95647,#95648,#95649,#95650,
#95651,#95652,#95653,#95654,#95655,#95656,#95657,#95658,#95659,#95660,#95661,
#95662,#95663,#95664,#95665,#95666,#95667,#95668,#95669,#95670,#95671,#95672,
#95673,#95674,#95675,#95676,#95677,#95678,#95679,#95680,#95681,#95682,#95683,
#95684,#95685,#95686,#95687,#95688,#95689,#95690,#95691,#95692,#95693,#95694,
#95695,#95696,#95697,#95698,#95699,#95700,#95701,#95702,#95703,#95704,#95705,
#95706,#95707,#95708,#95709,#95710,#95711,#95712,#95713,#95714,#95715,#95716,
#95717,#95718,#95719,#95720,#95721,#95722,#95723,#95724,#95725,#95726,#95727,
#95728,#95729,#95730,#95731,#95732,#95733,#95734,#95735,#95736,#95737,#95738,
#95739,#95740,#95741,#95742,#95743,#95744,#95745,#95746,#95747,#95748,#95749,
#95750,#95751,#95752,#95753,#95754,#95755,#95756,#95757,#95758,#95759,#95760,
#95761,#95762,#95763,#95764,#95765,#95766,#95767,#95768,#95769,#95770,#95771,
#95772,#95773,#95774,#95775,#95776,#95777,#95778,#95779,#95780,#95781,#95782,
#95783,#95784,#95785,#95786,#95787,#95788,#95789,#95790,#95791,#95792,#95793,
#95794,#95795,#95796,#95797,#95798,#95799,#95800,#95801,#95802,#95803,#95804,
#95805,#95806,#95807,#95808,#95809,#95810,#95811,#95812,#95813,#95814,#95815,
#95816,#95817,#95818,#95819,#95820,#95821,#95822,#95823,#95824,#95825,#95826,
#95827,#95828,#95829,#95830,#95831,#95832,#95833,#95834,#95835,#95836,#95837,
#95838,#95839,#95840,#95841,#95842,#95843,#95844,#95845,#95846,#95847,#95848,
#95849,#95850,#95851,#95852,#95853,#95854,#95855,#95856,#95857,#95858,#95859,
#95860,#95861,#95862,#95863,#95864,#95865,#95866,#95867,#95868,#95869,#95870,
#95871,#95872,#95873,#95874,#95875,#95876,#95877,#95878,#95879,#95880,#95881,
#95882,#95883,#95884,#95885,#95886,#95887,#95888,#95889,#95890,#95891,#95892,
#95893,#95894,#95895,#95896,#95897,#95898,#95899,#95900,#95901,#95902,#95903,
#95904,#95905,#95906,#95907,#95908,#95909,#95910,#95911,#95912,#95913,#95914,
#95915,#95916,#95917,#95918,#95919,#95920,#95921,#95922,#95923,#95924,#95925,
#95926,#95927,#95928,#95929,#95930,#95931,#95932,#95933,#95934,#95935,#95936,
#95937,#95938,#95939,#95940,#95941,#95942,#95943,#95944,#95945,#95946,#95947,
#95948,#95949,#95950,#95951,#95952,#95953,#95954,#95955,#95956,#95957,#95958,
#95959,#95960,#95961,#95962,#95963,#95964,#95965,#95966,#95967,#95968,#95969,
#95970,#95971,#95972,#95973,#95974,#95975,#95976,#95977,#95978,#95979,#95980,
#95981,#95982,#95983,#95984,#95985,#95986,#95987,#95988,#95989,#95990,#95991,
#95992,#95993,#95994,#95995,#95996,#95997,#95998,#95999,#96000,#96001,#96002,
#96003,#96004,#96005,#96006,#96007,#96008,#96009,#96010,#96011,#96012,#96013,
#96014,#96015,#96016,#96017,#96018,#96019,#96020,#96021,#96022,#96023,#96024,
#96025,#96026,#96027,#96028,#96029,#96030,#96031,#96032,#96033,#96034,#96035,
#96036,#96037,#96038,#96039,#96040,#96041,#96042,#96043,#96044,#96045,#96046,
#96047,#96048,#96049,#96050,#96051,#96052,#96053,#96054,#96055,#96056,#96057,
#96058,#96059,#96060,#96061,#96062,#96063,#96064,#96065,#96066,#96067,#96068,
#96069,#96070,#96071,#96072,#96073,#96074,#96075,#96076,#96077,#96078,#96079,
#96080,#96081,#96082,#96083,#96084,#96085,#96086,#96087,#96088,#96089,#96090,
#96091,#96092,#96093,#96094,#96095,#96096,#96097,#96098,#96099,#96100,#96101,
#96102,#96103,#96104,#96105,#96106,#96107,#96108,#96109,#96110,#96111,#96112,
#96113,#96114,#96115,#96116,#96117,#96118,#96119,#96120,#96121,#96122,#96123,
#96124,#96125,#96126,#96127,#96128,#96129,#96130,#96131,#96132,#96133,#96134,
#96135,#96136,#96137,#96138,#96139,#96140,#96141,#96142,#96143,#96144,#96145,
#96146,#96147,#96148,#96149,#96150,#96151,#96152,#96153,#96154,#96155,#96156,
#96157,#96158,#96159,#96160,#96161,#96162,#96163,#96164,#96165,#96166,#96167,
#96168,#96169,#96170,#96171,#96172,#96173,#96174,#96175,#96176,#96177,#96178,
#96179,#96180,#96181,#96182,#96183,#96184,#96185,#96186,#96187,#96188,#96189,
#96190,#96191,#96192,#96193,#96194,#96195,#96196,#96197,#96198,#96199,#96200,
#96201,#96202,#96203,#96204,#96205,#96206,#96207,#96208,#96209,#96210,#96211,
#96212,#96213,#96214,#96215,#96216,#96217,#96218,#96219,#96220,#96221,#96222,
#96223,#96224,#96225,#96226,#96227,#96228,#96229,#96230,#96231,#96232,#96233,
#96234,#96235,#96236,#96237,#96238,#96239,#96240,#96241,#96242,#96243,#96244,
#96245,#96246,#96247,#96248,#96249,#96250,#96251,#96252,#96253,#96254,#96255,
#96256,#96257,#96258,#96259,#96260,#96261,#96262,#96263,#96264,#96265,#96266,
#96267,#96268,#96269,#96270,#96271,#96272,#96273,#96274,#96275,#96276,#96277,
#96278,#96279,#96280,#96281,#96282,#96283,#96284,#96285,#96286,#96287,#96288,
#96289,#96290,#96291,#96292,#96293,#96294,#96295,#96296,#96297,#96298,#96299,
#96300,#96301,#96302,#96303,#96304,#96305,#96306,#96307,#96308,#96309,#96310,
#96311,#96312,#96313,#96314,#96315,#96316,#96317,#96318,#96319,#96320,#96321,
#96322,#96323,#96324,#96325,#96326,#96327,#96328,#96329,#96330,#96331,#96332,
#96333,#96334,#96335,#96336,#96337,#96338,#96339,#96340,#96341,#96342,#96343,
#96344,#96345,#96346,#96347,#96348,#96349,#96350,#96351,#96352,#96353,#96354,
#96355,#96356,#96357,#96358,#96359,#96360,#96361,#96362,#96363,#96364,#96365,
#96366,#96367,#96368,#96369,#96370,#96371,#96372,#96373,#96374,#96375,#96376,
#96377,#96378,#96379,#96380,#96381,#96382,#96383,#96384,#96385,#96386,#96387,
#96388,#96389,#96390,#96391,#96392,#96393,#96394,#96395,#96396,#96397,#96398,
#96399,#96400,#96401,#96402,#96403,#96404,#96405,#96406,#96407,#96408,#96409,
#96410,#96411,#96412,#96413,#96414,#96415,#96416,#96417,#96418,#96419,#96420,
#96421,#96422,#96423,#96424,#96425,#96426,#96427,#96428,#96429,#96430,#96431,
#96432,#96433,#96434,#96435,#96436,#96437,#96438,#96439,#96440,#96441,#96442,
#96443,#96444,#96445,#96446,#96447,#96448,#96449,#96450,#96451,#96452,#96453,
#96454,#96455,#96456,#96457,#96458,#96459,#96460,#96461,#96462,#96463,#96464,
#96465,#96466,#96467,#96468,#96469,#96470,#96471,#96472,#96473,#96474,#96475,
#96476,#96477,#96478,#96479,#96480,#96481,#96482,#96483,#96484,#96485,#96486,
#96487,#96488,#96489,#96490,#96491,#96492,#96493,#96494,#96495,#96496,#96497,
#96498,#96499,#96500,#96501,#96502,#96503,#96504,#96505,#96506,#96507,#96508,
#96509,#96510,#96511,#96512,#96513,#96514,#96515,#96516,#96517,#96518,#96519,
#96520,#96521,#96522,#96523,#96524,#96525,#96526,#96527,#96528,#96529,#96530,
#96531,#96532,#96533,#96534,#96535,#96536,#96537,#96538,#96539,#96540,#96541,
#96542,#96543,#96544,#96545,#96546,#96547,#96548,#96549,#96550,#96551,#96552,
#96553,#96554,#96555,#96556,#96557,#96558,#96559,#96560,#96561,#96562,#96563,
#96564,#96565,#96566,#96567,#96568,#96569,#96570,#96571,#96572,#96573,#96574,
#96575,#96576,#96577,#96578,#96579,#96580,#96581,#96582,#96583,#96584,#96585,
#96586,#96587,#96588,#96589,#96590,#96591,#96592,#96593,#96594,#96595,#96596,
#96597,#96598,#96599,#96600,#96601,#96602,#96603,#96604,#96605,#96606,#96607,
#96608,#96609,#96610,#96611,#96612,#96613,#96614,#96615,#96616,#96617,#96618,
#96619,#96620,#96621,#96622,#96623,#96624,#96625,#96626,#96627,#96628,#96629,
#96630,#96631,#96632,#96633,#96634,#96635,#96636,#96637,#96638,#96639,#96640,
#96641,#96642,#96643,#96644,#96645,#96646,#96647,#96648,#96649,#96650,#96651,
#96652,#96653,#96654,#96655,#96656,#96657,#96658,#96659,#96660,#96661,#96662,
#96663,#96664,#96665,#96666,#96667,#96668,#96669,#96670,#96671,#96672,#96673,
#96674,#96675,#96676,#96677,#96678,#96679,#96680,#96681,#96682,#96683,#96684,
#96685,#96686,#96687,#96688,#96689,#96690,#96691,#96692,#96693,#96694,#96695,
#96696,#96697,#96698,#96699,#96700,#96701,#96702,#96703,#96704,#96705,#96706,
#96707,#96708,#96709,#96710,#96711,#96712,#96713,#96714,#96715,#96716,#96717,
#96718,#96719,#96720,#96721,#96722,#96723,#96724,#96725,#96726,#96727,#96728,
#96729,#96730,#96731,#96732,#96733,#96734,#96735,#96736,#96737,#96738,#96739,
#96740,#96741,#96742,#96743,#96744,#96745,#96746,#96747,#96748,#96749,#96750,
#96751,#96752,#96753,#96754,#96755,#96756,#96757,#96758,#96759,#96760,#96761,
#96762,#96763,#96764,#96765,#96766,#96767,#96768,#96769,#96770,#96771,#96772,
#96773,#96774,#96775,#96776,#96777,#96778,#96779,#96780,#96781,#96782,#96783,
#96784,#96785,#96786,#96787,#96788,#96789,#96790,#96791,#96792,#96793,#96794,
#96795,#96796,#96797,#96798,#96799,#96800,#96801,#96802,#96803,#96804,#96805,
#96806,#96807,#96808,#96809,#96810,#96811,#96812,#96813,#96814,#96815,#96816,
#96817,#96818,#96819,#96820,#96821,#96822,#96823,#96824,#96825,#96826,#96827,
#96828,#96829,#96830,#96831,#96832,#96833,#96834,#96835,#96836,#96837,#96838,
#96839,#96840,#96841,#96842,#96843,#96844,#96845,#96846,#96847,#96848,#96849,
#96850,#96851,#96852,#96853,#96854,#96855,#96856,#96857,#96858,#96859,#96860,
#96861,#96862,#96863,#96864,#96865,#96866,#96867,#96868,#96869,#96870,#96871,
#96872,#96873,#96874,#96875,#96876,#96877,#96878,#96879,#96880,#96881,#96882,
#96883,#96884,#96885,#96886,#96887,#96888,#96889,#96890,#96891,#96892,#96893,
#96894,#96895,#96896,#96897,#96898,#96899,#96900,#96901,#96902,#96903,#96904,
#96905,#96906,#96907,#96908,#96909,#96910,#96911,#96912,#96913,#96914,#96915,
#96916,#96917,#96918,#96919,#96920,#96921,#96922,#96923,#96924,#96925,#96926,
#96927,#96928,#96929,#96930,#96931,#96932,#96933,#96934,#96935,#96936,#96937,
#96938,#96939,#96940,#96941,#96942,#96943,#96944,#96945,#96946,#96947,#96948,
#96949,#96950,#96951,#96952,#96953,#96954,#96955,#96956,#96957,#96958,#96959,
#96960,#96961,#96962,#96963,#96964,#96965,#96966,#96967,#96968,#96969,#96970,
#96971,#96972,#96973,#96974,#96975,#96976,#96977,#96978,#96979,#96980,#96981,
#96982,#96983,#96984,#96985,#96986,#96987,#96988,#96989,#96990,#96991,#96992,
#96993,#96994,#96995,#96996,#96997,#96998,#96999,#97000,#97001,#97002,#97003,
#97004,#97005,#97006,#97007,#97008,#97009,#97010,#97011,#97012,#97013,#97014,
#97015,#97016,#97017,#97018,#97019,#97020,#97021,#97022,#97023,#97024,#97025,
#97026,#97027,#97028,#97029,#97030,#97031,#97032,#97033,#97034,#97035,#97036,
#97037,#97038,#97039,#97040,#97041,#97042,#97043,#97044,#97045,#97046,#97047,
#97048,#97049,#97050,#97051,#97052,#97053,#97054,#97055,#97056,#97057,#97058,
#97059,#97060,#97061,#97062,#97063,#97064,#97065,#97066,#97067,#97068,#97069,
#97070,#97071,#97072,#97073,#97074,#97075,#97076,#97077,#97078,#97079,#97080,
#97081,#97082,#97083,#97084,#97085,#97086,#97087,#97088,#97089,#97090,#97091,
#97092,#97093,#97094,#97095,#97096,#97097,#97098,#97099,#97100,#97101,#97102,
#97103,#97104,#97105,#97106,#97107,#97108,#97109,#97110,#97111,#97112,#97113,
#97114,#97115,#97116,#97117,#97118,#97119,#97120,#97121,#97122,#97123,#97124,
#97125,#97126,#97127,#97128,#97129,#97130,#97131,#97132,#97133,#97134,#97135,
#97136,#97137,#97138,#97139,#97140,#97141,#97142,#97143,#97144,#97145,#97146,
#97147,#97148,#97149,#97150,#97151,#97152,#97153,#97154,#97155,#97156,#97157,
#97158,#97159,#97160,#97161,#97162,#97163,#97164,#97165,#97166,#97167,#97168,
#97169,#97170,#97171,#97172,#97173,#97174,#97175,#97176,#97177,#97178,#97179,
#97180,#97181,#97182,#97183,#97184,#97185,#97186,#97187,#97188,#97189,#97190,
#97191,#97192,#97193,#97194,#97195,#97196,#97197,#97198,#97199,#97200,#97201,
#97202,#97203,#97204,#97205,#97206,#97207,#97208,#97209,#97210,#97211,#97212,
#97213,#97214,#97215,#97216,#97217,#97218,#97219,#97220,#97221,#97222,#97223,
#97224,#97225,#97226,#97227,#97228,#97229,#97230,#97231,#97232,#97233,#97234,
#97235,#97236,#97237,#97238,#97239,#97240,#97241,#97242,#97243,#97244,#97245,
#97246,#97247,#97248,#97249,#97250,#97251,#97252,#97253,#97254,#97255,#97256,
#97257,#97258,#97259,#97260,#97261,#97262,#97263,#97264,#97265,#97266,#97267,
#97268,#97269,#97270,#97271,#97272,#97273,#97274,#97275,#97276,#97277,#97278,
#97279,#97280,#97281,#97282,#97283,#97284,#97285,#97286,#97287,#97288,#97289,
#97290,#97291,#97292,#97293,#97294,#97295,#97296,#97297,#97298,#97299,#97300,
#97301,#97302,#97303,#97304,#97305,#97306,#97307,#97308,#97309,#97310,#97311,
#97312,#97313,#97314,#97315,#97316,#97317,#97318,#97319,#97320,#97321,#97322,
#97323,#97324,#97325,#97326,#97327,#97328,#97329,#97330,#97331,#97332,#97333,
#97334,#97335,#97336,#97337,#97338,#97339,#97340,#97341,#97342,#97343,#97344,
#97345,#97346,#97347,#97348,#97349,#97350,#97351,#97352,#97353,#97354,#97355,
#97356,#97357,#97358,#97359,#97360,#97361,#97362,#97363,#97364,#97365,#97366,
#97367,#97368,#97369,#97370,#97371,#97372,#97373,#97374,#97375,#97376,#97377,
#97378,#97379,#97380,#97381,#97382,#97383,#97384,#97385,#97386,#97387,#97388,
#97389,#97390,#97391,#97392,#97393,#97394,#97395,#97396,#97397,#97398,#97399,
#97400,#97401,#97402,#97403,#97404,#97405,#97406,#97407,#97408,#97409,#97410,
#97411,#97412,#97413,#97414,#97415,#97416,#97417,#97418,#97419,#97420,#97421,
#97422,#97423,#97424,#97425,#97426,#97427,#97428,#97429,#97430,#97431,#97432,
#97433,#97434,#97435,#97436,#97437,#97438,#97439,#97440,#97441,#97442,#97443,
#97444,#97445,#97446,#97447,#97448,#97449,#97450,#97451,#97452,#97453,#97454,
#97455,#97456,#97457,#97458,#97459,#97460,#97461,#97462,#97463,#97464,#97465,
#97466,#97467,#97468,#97469,#97470,#97471,#97472,#97473,#97474,#97475,#97476,
#97477,#97478,#97479,#97480,#97481,#97482,#97483,#97484,#97485,#97486,#97487,
#97488,#97489,#97490,#97491,#97492,#97493,#97494,#97495,#97496,#97497,#97498,
#97499,#97500,#97501,#97502,#97503,#97504,#97505,#97506,#97507,#97508,#97509,
#97510,#97511,#97512,#97513,#97514,#97515,#97516,#97517,#97518,#97519,#97520,
#97521,#97522,#97523,#97524,#97525,#97526,#97527,#97528,#97529,#97530,#97531,
#97532,#97533,#97534,#97535,#97536,#97537,#97538,#97539,#97540,#97541,#97542,
#97543,#97544,#97545,#97546,#97547,#97548,#97549,#97550,#97551,#97552,#97553,
#97554,#97555,#97556,#97557,#97558,#97559,#97560,#97561,#97562,#97563,#97564,
#97565,#97566,#97567,#97568,#97569,#97570,#97571,#97572,#97573,#97574,#97575,
#97576,#97577,#97578,#97579,#97580,#97581,#97582,#97583,#97584,#97585,#97586,
#97587,#97588,#97589,#97590,#97591,#97592,#97593,#97594,#97595,#97596,#97597,
#97598,#97599,#97600,#97601,#97602,#97603,#97604,#97605,#97606,#97607,#97608,
#97609,#97610,#97611,#97612,#97613,#97614,#97615,#97616,#97617,#97618,#97619,
#97620,#97621,#97622,#97623,#97624,#97625,#97626,#97627,#97628,#97629,#97630,
#97631,#97632,#97633,#97634,#97635,#97636,#97637,#97638,#97639,#97640,#97641,
#97642,#97643,#97644,#97645,#97646,#97647,#97648,#97649,#97650,#97651,#97652,
#97653,#97654,#97655,#97656,#97657,#97658,#97659,#97660,#97661,#97662,#97663,
#97664,#97665,#97666,#97667,#97668,#97669,#97670,#97671,#97672,#97673,#97674,
#97675,#97676,#97677,#97678,#97679,#97680,#97681,#97682,#97683,#97684,#97685,
#97686,#97687,#97688,#97689,#97690,#97691,#97692,#97693,#97694,#97695,#97696,
#97697,#97698,#97699,#97700,#97701,#97702,#97703,#97704,#97705,#97706,#97707,
#97708,#97709,#97710,#97711,#97712,#97713,#97714,#97715,#97716,#97717,#97718,
#97719,#97720,#97721,#97722,#97723,#97724,#97725,#97726,#97727,#97728,#97729,
#97730,#97731,#97732,#97733,#97734,#97735,#97736,#97737,#97738,#97739,#97740,
#97741,#97742,#97743,#97744,#97745,#97746,#97747,#97748,#97749,#97750,#97751,
#97752,#97753,#97754,#97755,#97756,#97757,#97758,#97759,#97760,#97761,#97762,
#97763,#97764,#97765,#97766,#97767,#97768,#97769,#97770,#97771,#97772,#97773,
#97774,#97775,#97776,#97777,#97778,#97779,#97780,#97781,#97782,#97783,#97784,
#97785,#97786,#97787,#97788,#97789,#97790,#97791,#97792,#97793,#97794,#97795,
#97796,#97797,#97798,#97799,#97800,#97801,#97802,#97803,#97804,#97805,#97806,
#97807,#97808,#97809,#97810,#97811,#97812,#97813));
#98710=CLOSED_SHELL('',(#97814,#97815,#97816,#97817,#97818,#97819,#97820,
#97821,#97822));
#98711=CLOSED_SHELL('',(#97823,#97824,#97825,#97826,#97827,#97828));
#98712=CLOSED_SHELL('',(#97829,#97830,#97831,#97832,#97833,#97834,#97835,
#97836,#97837,#97838,#97839,#97840,#97841,#97842,#97843,#97844,#97845,#97846,
#97847,#97848,#97849,#97850,#97851,#97852,#97853,#97854,#97855,#97856,#97857,
#97858,#97859,#97860,#97861,#97862,#97863,#97864,#97865,#97866,#97867,#97868,
#97869,#97870,#97871,#97872,#97873,#97874,#97875,#97876,#97877,#97878,#97879,
#97880,#97881,#97882,#97883,#97884,#97885,#97886,#97887,#97888,#97889,#97890,
#97891,#97892,#97893,#97894,#97895,#97896,#97897,#97898,#97899,#97900,#97901,
#97902,#97903,#97904,#97905,#97906,#97907,#97908,#97909,#97910,#97911,#97912,
#97913,#97914,#97915,#97916,#97917,#97918,#97919,#97920,#97921,#97922,#97923,
#97924,#97925,#97926,#97927,#97928,#97929,#97930,#97931,#97932,#97933,#97934,
#97935,#97936,#97937,#97938,#97939,#97940,#97941,#97942,#97943,#97944,#97945,
#97946,#97947,#97948,#97949,#97950,#97951,#97952,#97953,#97954,#97955,#97956,
#97957,#97958,#97959,#97960,#97961,#97962,#97963,#97964,#97965,#97966,#97967,
#97968,#97969,#97970,#97971,#97972,#97973,#97974,#97975,#97976,#97977,#97978,
#97979,#97980,#97981,#97982,#97983,#97984,#97985,#97986,#97987,#97988,#97989,
#97990,#97991,#97992,#97993,#97994,#97995,#97996,#97997,#97998,#97999,#98000,
#98001,#98002));
#98713=CLOSED_SHELL('',(#98003));
#98714=CLOSED_SHELL('',(#98004,#98005,#98006,#98007,#98008,#98009,#98010,
#98011,#98012));
#98715=CLOSED_SHELL('',(#98013,#98014,#98015,#98016,#98017,#98018,#98019));
#98716=CLOSED_SHELL('',(#98020,#98021,#98022,#98023,#98024,#98025,#98026,
#98027,#98028,#98029,#98030,#98031,#98032,#98033,#98034,#98035));
#98717=CLOSED_SHELL('',(#98036,#98037,#98038,#98039,#98040,#98041,#98042,
#98043,#98044,#98045,#98046,#98047,#98048,#98049,#98050,#98051,#98052,#98053,
#98054,#98055,#98056,#98057,#98058,#98059,#98060,#98061,#98062,#98063,#98064,
#98065,#98066,#98067,#98068,#98069,#98070));
#98718=CLOSED_SHELL('',(#98071,#98072,#98073,#98074,#98075,#98076,#98077,
#98078,#98079,#98080,#98081,#98082,#98083,#98084,#98085,#98086,#98087,#98088,
#98089,#98090,#98091,#98092,#98093,#98094,#98095,#98096,#98097,#98098,#98099,
#98100,#98101,#98102,#98103,#98104,#98105));
#98719=CLOSED_SHELL('',(#98106,#98107,#98108,#98109,#98110,#98111,#98112,
#98113,#98114,#98115));
#98720=CLOSED_SHELL('',(#98116,#98117,#98118,#98119,#98120,#98121,#98122,
#98123,#98124,#98125,#98126,#98127,#98128,#98129,#98130,#98131,#98132,#98133,
#98134,#98135,#98136,#98137,#98138,#98139,#98140,#98141,#98142,#98143,#98144,
#98145,#98146,#98147,#98148,#98149,#98150,#98151,#98152,#98153,#98154,#98155,
#98156,#98157,#98158,#98159,#98160,#98161,#98162,#98163,#98164,#98165,#98166,
#98167,#98168,#98169,#98170,#98171,#98172,#98173));
#98721=CLOSED_SHELL('',(#98174,#98175,#98176,#98177,#98178,#98179));
#98722=CLOSED_SHELL('',(#98180,#98181,#98182,#98183,#98184,#98185));
#98723=CLOSED_SHELL('',(#98186,#98187,#98188,#98189,#98190,#98191,#98192,
#98193,#98194,#98195,#98196,#98197,#98198,#98199,#98200,#98201,#98202,#98203,
#98204,#98205,#98206,#98207,#98208,#98209,#98210,#98211,#98212,#98213,#98214,
#98215,#98216,#98217,#98218,#98219,#98220,#98221,#98222,#98223,#98224,#98225,
#98226,#98227,#98228,#98229,#98230,#98231,#98232,#98233,#98234));
#98724=CLOSED_SHELL('',(#98235,#98236,#98237,#98238,#98239,#98240,#98241,
#98242,#98243,#98244,#98245,#98246,#98247,#98248,#98249,#98250,#98251,#98252,
#98253,#98254,#98255,#98256,#98257,#98258,#98259,#98260,#98261,#98262,#98263,
#98264,#98265,#98266,#98267,#98268,#98269,#98270,#98271,#98272,#98273,#98274,
#98275,#98276,#98277,#98278,#98279,#98280,#98281,#98282,#98283,#98284,#98285,
#98286,#98287,#98288,#98289,#98290,#98291,#98292,#98293,#98294,#98295,#98296));
#98725=CLOSED_SHELL('',(#98297,#98298,#98299,#98300,#98301,#98302,#98303,
#98304,#98305,#98306,#98307,#98308,#98309,#98310,#98311,#98312,#98313,#98314));
#98726=CLOSED_SHELL('',(#98315,#98316,#98317,#98318,#98319,#98320,#98321,
#98322,#98323,#98324));
#98727=CLOSED_SHELL('',(#98325,#98326,#98327,#98328,#98329,#98330,#98331,
#98332,#98333,#98334,#98335,#98336,#98337,#98338,#98339,#98340,#98341,#98342,
#98343,#98344,#98345,#98346,#98347,#98348,#98349,#98350,#98351,#98352,#98353,
#98354,#98355,#98356,#98357,#98358,#98359,#98360,#98361,#98362,#98363,#98364,
#98365,#98366,#98367,#98368,#98369,#98370,#98371,#98372,#98373,#98374,#98375,
#98376,#98377,#98378,#98379,#98380,#98381,#98382));
#98728=CLOSED_SHELL('',(#98383,#98384,#98385,#98386,#98387,#98388,#98389,
#98390,#98391,#98392,#98393,#98394,#98395,#98396,#98397,#98398,#98399,#98400));
#98729=CLOSED_SHELL('',(#98401,#98402,#98403,#98404,#98405,#98406,#98407,
#98408,#98409,#98410));
#98730=CLOSED_SHELL('',(#98411,#98412,#98413,#98414,#98415,#98416,#98417,
#98418,#98419,#98420,#98421,#98422,#98423,#98424,#98425,#98426,#98427,#98428));
#98731=CLOSED_SHELL('',(#98429,#98430,#98431,#98432,#98433,#98434,#98435,
#98436,#98437,#98438));
#98732=CLOSED_SHELL('',(#98439,#98440,#98441,#98442,#98443,#98444,#98445,
#98446,#98447,#98448,#98449,#98450,#98451,#98452,#98453,#98454,#98455,#98456));
#98733=CLOSED_SHELL('',(#98457,#98458,#98459,#98460,#98461,#98462,#98463,
#98464,#98465,#98466));
#98734=CLOSED_SHELL('',(#98467,#98468,#98469,#98470,#98471,#98472,#98473,
#98474,#98475,#98476,#98477,#98478,#98479,#98480,#98481,#98482,#98483,#98484,
#98485,#98486,#98487,#98488,#98489,#98490,#98491,#98492,#98493,#98494,#98495,
#98496,#98497,#98498,#98499,#98500,#98501,#98502,#98503,#98504,#98505,#98506,
#98507,#98508,#98509,#98510,#98511,#98512,#98513,#98514,#98515,#98516,#98517,
#98518,#98519,#98520,#98521,#98522,#98523,#98524,#98525,#98526,#98527,#98528,
#98529,#98530,#98531,#98532,#98533,#98534,#98535,#98536,#98537,#98538,#98539,
#98540,#98541,#98542,#98543,#98544,#98545,#98546,#98547,#98548,#98549,#98550,
#98551,#98552,#98553,#98554,#98555,#98556,#98557,#98558,#98559,#98560,#98561,
#98562,#98563,#98564,#98565,#98566,#98567,#98568,#98569,#98570,#98571,#98572,
#98573,#98574,#98575,#98576,#98577,#98578,#98579,#98580,#98581,#98582,#98583,
#98584,#98585,#98586,#98587,#98588,#98589,#98590,#98591,#98592,#98593,#98594,
#98595,#98596,#98597,#98598,#98599,#98600,#98601,#98602,#98603,#98604,#98605,
#98606,#98607,#98608,#98609,#98610,#98611,#98612,#98613,#98614,#98615,#98616,
#98617,#98618,#98619,#98620,#98621,#98622,#98623,#98624,#98625,#98626,#98627,
#98628,#98629,#98630,#98631,#98632,#98633,#98634,#98635,#98636,#98637,#98638,
#98639,#98640,#98641,#98642,#98643,#98644,#98645,#98646,#98647,#98648,#98649,
#98650,#98651,#98652,#98653,#98654,#98655,#98656,#98657,#98658,#98659,#98660,
#98661,#98662,#98663,#98664,#98665,#98666,#98667,#98668,#98669,#98670,#98671,
#98672,#98673,#98674,#98675,#98676,#98677,#98678,#98679,#98680,#98681,#98682,
#98683,#98684,#98685,#98686,#98687,#98688,#98689,#98690,#98691,#98692,#98693,
#98694,#98695,#98696));
#98735=DERIVED_UNIT_ELEMENT(#98747,1.);
#98736=DERIVED_UNIT_ELEMENT(#276464,-3.);
#98737=DERIVED_UNIT_ELEMENT(#98747,1.);
#98738=DERIVED_UNIT_ELEMENT(#276464,-3.);
#98739=DERIVED_UNIT_ELEMENT(#98747,1.);
#98740=DERIVED_UNIT_ELEMENT(#276464,-3.);
#98741=DERIVED_UNIT_ELEMENT(#98747,1.);
#98742=DERIVED_UNIT_ELEMENT(#276464,-3.);
#98743=DERIVED_UNIT_ELEMENT(#98747,1.);
#98744=DERIVED_UNIT_ELEMENT(#276464,-3.);
#98745=DERIVED_UNIT_ELEMENT(#98747,1.);
#98746=DERIVED_UNIT_ELEMENT(#276464,-3.);
#98747=(
MASS_UNIT()
NAMED_UNIT(*)
SI_UNIT(.KILO.,.GRAM.)
);
#98748=DERIVED_UNIT((#98735,#98736));
#98749=DERIVED_UNIT((#98737,#98738));
#98750=DERIVED_UNIT((#98739,#98740));
#98751=DERIVED_UNIT((#98741,#98742));
#98752=DERIVED_UNIT((#98743,#98744));
#98753=DERIVED_UNIT((#98745,#98746));
#98754=MEASURE_REPRESENTATION_ITEM('density measure',
POSITIVE_RATIO_MEASURE(7850.),#98748);
#98755=MEASURE_REPRESENTATION_ITEM('density measure',
POSITIVE_RATIO_MEASURE(7850.),#98749);
#98756=MEASURE_REPRESENTATION_ITEM('density measure',
POSITIVE_RATIO_MEASURE(7850.),#98750);
#98757=MEASURE_REPRESENTATION_ITEM('density measure',
POSITIVE_RATIO_MEASURE(7850.),#98751);
#98758=MEASURE_REPRESENTATION_ITEM('density measure',
POSITIVE_RATIO_MEASURE(7850.),#98752);
#98759=MEASURE_REPRESENTATION_ITEM('density measure',
POSITIVE_RATIO_MEASURE(7850.),#98753);
#98760=PROPERTY_DEFINITION_REPRESENTATION(#98790,#98772);
#98761=PROPERTY_DEFINITION_REPRESENTATION(#98791,#98773);
#98762=PROPERTY_DEFINITION_REPRESENTATION(#98792,#98774);
#98763=PROPERTY_DEFINITION_REPRESENTATION(#98793,#98775);
#98764=PROPERTY_DEFINITION_REPRESENTATION(#98794,#98776);
#98765=PROPERTY_DEFINITION_REPRESENTATION(#98795,#98777);
#98766=PROPERTY_DEFINITION_REPRESENTATION(#98796,#98778);
#98767=PROPERTY_DEFINITION_REPRESENTATION(#98797,#98779);
#98768=PROPERTY_DEFINITION_REPRESENTATION(#98798,#98780);
#98769=PROPERTY_DEFINITION_REPRESENTATION(#98799,#98781);
#98770=PROPERTY_DEFINITION_REPRESENTATION(#98800,#98782);
#98771=PROPERTY_DEFINITION_REPRESENTATION(#98801,#98783);
#98772=REPRESENTATION('material name',(#98784),#276456);
#98773=REPRESENTATION('density',(#98754),#276456);
#98774=REPRESENTATION('material name',(#98785),#276457);
#98775=REPRESENTATION('density',(#98755),#276457);
#98776=REPRESENTATION('material name',(#98786),#276458);
#98777=REPRESENTATION('density',(#98756),#276458);
#98778=REPRESENTATION('material name',(#98787),#276459);
#98779=REPRESENTATION('density',(#98757),#276459);
#98780=REPRESENTATION('material name',(#98788),#276460);
#98781=REPRESENTATION('density',(#98758),#276460);
#98782=REPRESENTATION('material name',(#98789),#276461);
#98783=REPRESENTATION('density',(#98759),#276461);
#98784=DESCRIPTIVE_REPRESENTATION_ITEM('Steel','Steel');
#98785=DESCRIPTIVE_REPRESENTATION_ITEM('Steel','Steel');
#98786=DESCRIPTIVE_REPRESENTATION_ITEM('Steel','Steel');
#98787=DESCRIPTIVE_REPRESENTATION_ITEM('Steel','Steel');
#98788=DESCRIPTIVE_REPRESENTATION_ITEM('Steel','Steel');
#98789=DESCRIPTIVE_REPRESENTATION_ITEM('Steel','Steel');
#98790=PROPERTY_DEFINITION('material property','material name',#276496);
#98791=PROPERTY_DEFINITION('material property','density of part',#276496);
#98792=PROPERTY_DEFINITION('material property','material name',#276497);
#98793=PROPERTY_DEFINITION('material property','density of part',#276497);
#98794=PROPERTY_DEFINITION('material property','material name',#276498);
#98795=PROPERTY_DEFINITION('material property','density of part',#276498);
#98796=PROPERTY_DEFINITION('material property','material name',#276499);
#98797=PROPERTY_DEFINITION('material property','density of part',#276499);
#98798=PROPERTY_DEFINITION('material property','material name',#276500);
#98799=PROPERTY_DEFINITION('material property','density of part',#276500);
#98800=PROPERTY_DEFINITION('material property','material name',#276501);
#98801=PROPERTY_DEFINITION('material property','density of part',#276501);
#98802=AXIS2_PLACEMENT_3D('',#142642,#111673,#111674);
#98803=AXIS2_PLACEMENT_3D('',#142643,#111675,#111676);
#98804=AXIS2_PLACEMENT_3D('',#142644,#111677,#111678);
#98805=AXIS2_PLACEMENT_3D('',#142646,#111679,#111680);
#98806=AXIS2_PLACEMENT_3D('',#142649,#111682,#111683);
#98807=AXIS2_PLACEMENT_3D('',#142650,#111684,#111685);
#98808=AXIS2_PLACEMENT_3D('',#142652,#111686,#111687);
#98809=AXIS2_PLACEMENT_3D('',#142655,#111689,#111690);
#98810=AXIS2_PLACEMENT_3D('',#142656,#111691,#111692);
#98811=AXIS2_PLACEMENT_3D('',#142658,#111693,#111694);
#98812=AXIS2_PLACEMENT_3D('',#142661,#111696,#111697);
#98813=AXIS2_PLACEMENT_3D('',#142662,#111698,#111699);
#98814=AXIS2_PLACEMENT_3D('',#142664,#111700,#111701);
#98815=AXIS2_PLACEMENT_3D('',#142667,#111703,#111704);
#98816=AXIS2_PLACEMENT_3D('',#142668,#111705,#111706);
#98817=AXIS2_PLACEMENT_3D('',#142677,#111711,#111712);
#98818=AXIS2_PLACEMENT_3D('',#142683,#111716,#111717);
#98819=AXIS2_PLACEMENT_3D('',#142689,#111721,#111722);
#98820=AXIS2_PLACEMENT_3D('',#142692,#111725,#111726);
#98821=AXIS2_PLACEMENT_3D('',#142701,#111731,#111732);
#98822=AXIS2_PLACEMENT_3D('',#142707,#111736,#111737);
#98823=AXIS2_PLACEMENT_3D('',#142711,#111740,#111741);
#98824=AXIS2_PLACEMENT_3D('',#142715,#111744,#111745);
#98825=AXIS2_PLACEMENT_3D('',#142717,#111747,#111748);
#98826=AXIS2_PLACEMENT_3D('',#142723,#111752,#111753);
#98827=AXIS2_PLACEMENT_3D('',#142727,#111756,#111757);
#98828=AXIS2_PLACEMENT_3D('',#142731,#111760,#111761);
#98829=AXIS2_PLACEMENT_3D('',#142733,#111763,#111764);
#98830=AXIS2_PLACEMENT_3D('',#142739,#111768,#111769);
#98831=AXIS2_PLACEMENT_3D('',#142743,#111772,#111773);
#98832=AXIS2_PLACEMENT_3D('',#142747,#111776,#111777);
#98833=AXIS2_PLACEMENT_3D('',#142749,#111779,#111780);
#98834=AXIS2_PLACEMENT_3D('',#142755,#111784,#111785);
#98835=AXIS2_PLACEMENT_3D('',#142759,#111788,#111789);
#98836=AXIS2_PLACEMENT_3D('',#142763,#111792,#111793);
#98837=AXIS2_PLACEMENT_3D('',#142765,#111795,#111796);
#98838=AXIS2_PLACEMENT_3D('',#142770,#111798,#111799);
#98839=AXIS2_PLACEMENT_3D('',#142774,#111801,#111802);
#98840=AXIS2_PLACEMENT_3D('',#142778,#111804,#111805);
#98841=AXIS2_PLACEMENT_3D('',#142781,#111807,#111808);
#98842=AXIS2_PLACEMENT_3D('',#142782,#111809,#111810);
#98843=AXIS2_PLACEMENT_3D('',#142787,#111812,#111813);
#98844=AXIS2_PLACEMENT_3D('',#142791,#111815,#111816);
#98845=AXIS2_PLACEMENT_3D('',#142795,#111818,#111819);
#98846=AXIS2_PLACEMENT_3D('',#142798,#111821,#111822);
#98847=AXIS2_PLACEMENT_3D('',#142799,#111823,#111824);
#98848=AXIS2_PLACEMENT_3D('',#142805,#111828,#111829);
#98849=AXIS2_PLACEMENT_3D('',#142811,#111833,#111834);
#98850=AXIS2_PLACEMENT_3D('',#142817,#111838,#111839);
#98851=AXIS2_PLACEMENT_3D('',#142823,#111843,#111844);
#98852=AXIS2_PLACEMENT_3D('',#142824,#111845,#111846);
#98853=AXIS2_PLACEMENT_3D('',#142825,#111847,#111848);
#98854=AXIS2_PLACEMENT_3D('',#142826,#111849,#111850);
#98855=AXIS2_PLACEMENT_3D('',#142827,#111851,#111852);
#98856=AXIS2_PLACEMENT_3D('',#142828,#111853,#111854);
#98857=AXIS2_PLACEMENT_3D('',#142829,#111855,#111856);
#98858=AXIS2_PLACEMENT_3D('',#142830,#111857,#111858);
#98859=AXIS2_PLACEMENT_3D('',#142831,#111859,#111860);
#98860=AXIS2_PLACEMENT_3D('',#142832,#111861,#111862);
#98861=AXIS2_PLACEMENT_3D('',#142833,#111863,#111864);
#98862=AXIS2_PLACEMENT_3D('',#142834,#111865,#111866);
#98863=AXIS2_PLACEMENT_3D('',#142835,#111867,#111868);
#98864=AXIS2_PLACEMENT_3D('',#142836,#111869,#111870);
#98865=AXIS2_PLACEMENT_3D('',#142837,#111871,#111872);
#98866=AXIS2_PLACEMENT_3D('',#142838,#111873,#111874);
#98867=AXIS2_PLACEMENT_3D('',#142839,#111875,#111876);
#98868=AXIS2_PLACEMENT_3D('',#142840,#111877,#111878);
#98869=AXIS2_PLACEMENT_3D('',#142841,#111879,#111880);
#98870=AXIS2_PLACEMENT_3D('',#142842,#111881,#111882);
#98871=AXIS2_PLACEMENT_3D('',#142843,#111883,#111884);
#98872=AXIS2_PLACEMENT_3D('',#142844,#111885,#111886);
#98873=AXIS2_PLACEMENT_3D('',#142845,#111887,#111888);
#98874=AXIS2_PLACEMENT_3D('',#142846,#111889,#111890);
#98875=AXIS2_PLACEMENT_3D('',#142847,#111891,#111892);
#98876=AXIS2_PLACEMENT_3D('',#142848,#111893,#111894);
#98877=AXIS2_PLACEMENT_3D('',#142851,#111895,#111896);
#98878=AXIS2_PLACEMENT_3D('',#142852,#111897,#111898);
#98879=AXIS2_PLACEMENT_3D('',#142854,#111899,#111900);
#98880=AXIS2_PLACEMENT_3D('',#142855,#111901,#111902);
#98881=AXIS2_PLACEMENT_3D('',#142856,#111903,#111904);
#98882=AXIS2_PLACEMENT_3D('',#142858,#111905,#111906);
#98883=AXIS2_PLACEMENT_3D('',#142860,#111907,#111908);
#98884=AXIS2_PLACEMENT_3D('',#142862,#111909,#111910);
#98885=AXIS2_PLACEMENT_3D('',#142863,#111911,#111912);
#98886=AXIS2_PLACEMENT_3D('',#142864,#111913,#111914);
#98887=AXIS2_PLACEMENT_3D('',#142942,#111916,#111917);
#98888=AXIS2_PLACEMENT_3D('',#143020,#111919,#111920);
#98889=AXIS2_PLACEMENT_3D('',#143100,#111922,#111923);
#98890=AXIS2_PLACEMENT_3D('',#143180,#111925,#111926);
#98891=AXIS2_PLACEMENT_3D('',#143182,#111927,#111928);
#98892=AXIS2_PLACEMENT_3D('',#143185,#111931,#111932);
#98893=AXIS2_PLACEMENT_3D('',#143189,#111935,#111936);
#98894=AXIS2_PLACEMENT_3D('',#143190,#111937,#111938);
#98895=AXIS2_PLACEMENT_3D('',#143191,#111939,#111940);
#98896=AXIS2_PLACEMENT_3D('',#143192,#111941,#111942);
#98897=AXIS2_PLACEMENT_3D('',#143269,#111945,#111946);
#98898=AXIS2_PLACEMENT_3D('',#143411,#111948,#111949);
#98899=AXIS2_PLACEMENT_3D('',#143553,#111951,#111952);
#98900=AXIS2_PLACEMENT_3D('',#143695,#111954,#111955);
#98901=AXIS2_PLACEMENT_3D('',#143837,#111957,#111958);
#98902=AXIS2_PLACEMENT_3D('',#143979,#111960,#111961);
#98903=AXIS2_PLACEMENT_3D('',#144121,#111963,#111964);
#98904=AXIS2_PLACEMENT_3D('',#144263,#111966,#111967);
#98905=AXIS2_PLACEMENT_3D('',#144294,#111969,#111970);
#98906=AXIS2_PLACEMENT_3D('',#144393,#111973,#111974);
#98907=AXIS2_PLACEMENT_3D('',#144507,#111976,#111977);
#98908=AXIS2_PLACEMENT_3D('',#144563,#111979,#111980);
#98909=AXIS2_PLACEMENT_3D('',#144619,#111982,#111983);
#98910=AXIS2_PLACEMENT_3D('',#144675,#111985,#111986);
#98911=AXIS2_PLACEMENT_3D('',#144731,#111988,#111989);
#98912=AXIS2_PLACEMENT_3D('',#144787,#111991,#111992);
#98913=AXIS2_PLACEMENT_3D('',#144843,#111994,#111995);
#98914=AXIS2_PLACEMENT_3D('',#144875,#111997,#111998);
#98915=AXIS2_PLACEMENT_3D('',#144900,#111999,#112000);
#98916=AXIS2_PLACEMENT_3D('',#144970,#112002,#112003);
#98917=AXIS2_PLACEMENT_3D('',#145042,#112005,#112006);
#98918=AXIS2_PLACEMENT_3D('',#145114,#112008,#112009);
#98919=AXIS2_PLACEMENT_3D('',#145186,#112011,#112012);
#98920=AXIS2_PLACEMENT_3D('',#145258,#112014,#112015);
#98921=AXIS2_PLACEMENT_3D('',#145330,#112017,#112018);
#98922=AXIS2_PLACEMENT_3D('',#145402,#112020,#112021);
#98923=AXIS2_PLACEMENT_3D('',#145442,#112023,#112024);
#98924=AXIS2_PLACEMENT_3D('',#145482,#112026,#112027);
#98925=AXIS2_PLACEMENT_3D('',#145523,#112029,#112030);
#98926=AXIS2_PLACEMENT_3D('',#145564,#112032,#112033);
#98927=AXIS2_PLACEMENT_3D('',#145590,#112035,#112036);
#98928=AXIS2_PLACEMENT_3D('',#145803,#112037,#112038);
#98929=AXIS2_PLACEMENT_3D('',#145808,#112039,#112040);
#98930=AXIS2_PLACEMENT_3D('',#145810,#112041,#112042);
#98931=AXIS2_PLACEMENT_3D('',#145814,#112045,#112046);
#98932=AXIS2_PLACEMENT_3D('',#149842,#112047,#112048);
#98933=AXIS2_PLACEMENT_3D('',#167137,#112054,#112055);
#98934=AXIS2_PLACEMENT_3D('',#167139,#112057,#112058);
#98935=AXIS2_PLACEMENT_3D('',#167140,#112059,#112060);
#98936=AXIS2_PLACEMENT_3D('',#167141,#112061,#112062);
#98937=AXIS2_PLACEMENT_3D('',#167142,#112063,#112064);
#98938=AXIS2_PLACEMENT_3D('',#167143,#112065,#112066);
#98939=AXIS2_PLACEMENT_3D('',#167144,#112067,#112068);
#98940=AXIS2_PLACEMENT_3D('',#167145,#112069,#112070);
#98941=AXIS2_PLACEMENT_3D('',#167147,#112071,#112072);
#98942=AXIS2_PLACEMENT_3D('',#167149,#112073,#112074);
#98943=AXIS2_PLACEMENT_3D('',#167151,#112075,#112076);
#98944=AXIS2_PLACEMENT_3D('',#167152,#112077,#112078);
#98945=AXIS2_PLACEMENT_3D('',#167153,#112079,#112080);
#98946=AXIS2_PLACEMENT_3D('',#167180,#112083,#112084);
#98947=AXIS2_PLACEMENT_3D('',#167183,#112085,#112086);
#98948=AXIS2_PLACEMENT_3D('',#167190,#112087,#112088);
#98949=AXIS2_PLACEMENT_3D('',#167192,#112089,#112090);
#98950=AXIS2_PLACEMENT_3D('',#167195,#112092,#112093);
#98951=AXIS2_PLACEMENT_3D('',#167196,#112094,#112095);
#98952=AXIS2_PLACEMENT_3D('',#167199,#112096,#112097);
#98953=AXIS2_PLACEMENT_3D('',#167219,#112098,#112099);
#98954=AXIS2_PLACEMENT_3D('',#167220,#112100,#112101);
#98955=AXIS2_PLACEMENT_3D('',#167223,#112102,#112103);
#98956=AXIS2_PLACEMENT_3D('',#167225,#112104,#112105);
#98957=AXIS2_PLACEMENT_3D('',#167226,#112106,#112107);
#98958=AXIS2_PLACEMENT_3D('',#167229,#112109,#112110);
#98959=AXIS2_PLACEMENT_3D('',#167230,#112111,#112112);
#98960=AXIS2_PLACEMENT_3D('',#167231,#112113,#112114);
#98961=AXIS2_PLACEMENT_3D('',#167233,#112115,#112116);
#98962=AXIS2_PLACEMENT_3D('',#167234,#112117,#112118);
#98963=AXIS2_PLACEMENT_3D('',#167237,#112119,#112120);
#98964=AXIS2_PLACEMENT_3D('',#167238,#112121,#112122);
#98965=AXIS2_PLACEMENT_3D('',#167239,#112123,#112124);
#98966=AXIS2_PLACEMENT_3D('',#167240,#112125,#112126);
#98967=AXIS2_PLACEMENT_3D('',#167244,#112128,#112129);
#98968=AXIS2_PLACEMENT_3D('',#167245,#112130,#112131);
#98969=AXIS2_PLACEMENT_3D('',#167246,#112132,#112133);
#98970=AXIS2_PLACEMENT_3D('',#167248,#112134,#112135);
#98971=AXIS2_PLACEMENT_3D('',#167249,#112136,#112137);
#98972=AXIS2_PLACEMENT_3D('',#167250,#112138,#112139);
#98973=AXIS2_PLACEMENT_3D('',#167252,#112140,#112141);
#98974=AXIS2_PLACEMENT_3D('',#167255,#112143,#112144);
#98975=AXIS2_PLACEMENT_3D('',#167256,#112145,#112146);
#98976=AXIS2_PLACEMENT_3D('',#167257,#112147,#112148);
#98977=AXIS2_PLACEMENT_3D('',#167258,#112149,#112150);
#98978=AXIS2_PLACEMENT_3D('',#167265,#112151,#112152);
#98979=AXIS2_PLACEMENT_3D('',#167284,#112153,#112154);
#98980=AXIS2_PLACEMENT_3D('',#167303,#112155,#112156);
#98981=AXIS2_PLACEMENT_3D('',#167322,#112157,#112158);
#98982=AXIS2_PLACEMENT_3D('',#167341,#112159,#112160);
#98983=AXIS2_PLACEMENT_3D('',#167342,#112161,#112162);
#98984=AXIS2_PLACEMENT_3D('',#167344,#112163,#112164);
#98985=AXIS2_PLACEMENT_3D('',#167346,#112165,#112166);
#98986=AXIS2_PLACEMENT_3D('',#167348,#112167,#112168);
#98987=AXIS2_PLACEMENT_3D('',#167350,#112169,#112170);
#98988=AXIS2_PLACEMENT_3D('',#167351,#112171,#112172);
#98989=AXIS2_PLACEMENT_3D('',#167352,#112173,#112174);
#98990=AXIS2_PLACEMENT_3D('',#167371,#112175,#112176);
#98991=AXIS2_PLACEMENT_3D('',#167390,#112177,#112178);
#98992=AXIS2_PLACEMENT_3D('',#167409,#112179,#112180);
#98993=AXIS2_PLACEMENT_3D('',#167428,#112181,#112182);
#98994=AXIS2_PLACEMENT_3D('',#167447,#112183,#112184);
#98995=AXIS2_PLACEMENT_3D('',#167449,#112186,#112187);
#98996=AXIS2_PLACEMENT_3D('',#167452,#112190,#112191);
#98997=AXIS2_PLACEMENT_3D('',#167455,#112194,#112195);
#98998=AXIS2_PLACEMENT_3D('',#167458,#112198,#112199);
#98999=AXIS2_PLACEMENT_3D('',#167461,#112202,#112203);
#99000=AXIS2_PLACEMENT_3D('',#167463,#112205,#112206);
#99001=AXIS2_PLACEMENT_3D('',#167464,#112207,#112208);
#99002=AXIS2_PLACEMENT_3D('',#167465,#112209,#112210);
#99003=AXIS2_PLACEMENT_3D('',#167466,#112211,#112212);
#99004=AXIS2_PLACEMENT_3D('',#167467,#112213,#112214);
#99005=AXIS2_PLACEMENT_3D('',#167468,#112215,#112216);
#99006=AXIS2_PLACEMENT_3D('',#167470,#112217,#112218);
#99007=AXIS2_PLACEMENT_3D('',#167473,#112220,#112221);
#99008=AXIS2_PLACEMENT_3D('',#167474,#112222,#112223);
#99009=AXIS2_PLACEMENT_3D('',#167476,#112224,#112225);
#99010=AXIS2_PLACEMENT_3D('',#167479,#112227,#112228);
#99011=AXIS2_PLACEMENT_3D('',#167480,#112229,#112230);
#99012=AXIS2_PLACEMENT_3D('',#167481,#112231,#112232);
#99013=AXIS2_PLACEMENT_3D('',#167482,#112233,#112234);
#99014=AXIS2_PLACEMENT_3D('',#167484,#112235,#112236);
#99015=AXIS2_PLACEMENT_3D('',#167487,#112238,#112239);
#99016=AXIS2_PLACEMENT_3D('',#167488,#112240,#112241);
#99017=AXIS2_PLACEMENT_3D('',#167490,#112242,#112243);
#99018=AXIS2_PLACEMENT_3D('',#167493,#112245,#112246);
#99019=AXIS2_PLACEMENT_3D('',#167494,#112247,#112248);
#99020=AXIS2_PLACEMENT_3D('',#167495,#112249,#112250);
#99021=AXIS2_PLACEMENT_3D('',#167496,#112251,#112252);
#99022=AXIS2_PLACEMENT_3D('',#167498,#112253,#112254);
#99023=AXIS2_PLACEMENT_3D('',#167501,#112256,#112257);
#99024=AXIS2_PLACEMENT_3D('',#167502,#112258,#112259);
#99025=AXIS2_PLACEMENT_3D('',#167504,#112260,#112261);
#99026=AXIS2_PLACEMENT_3D('',#167507,#112263,#112264);
#99027=AXIS2_PLACEMENT_3D('',#167508,#112265,#112266);
#99028=AXIS2_PLACEMENT_3D('',#167509,#112267,#112268);
#99029=AXIS2_PLACEMENT_3D('',#167510,#112269,#112270);
#99030=AXIS2_PLACEMENT_3D('',#167512,#112271,#112272);
#99031=AXIS2_PLACEMENT_3D('',#167515,#112274,#112275);
#99032=AXIS2_PLACEMENT_3D('',#167516,#112276,#112277);
#99033=AXIS2_PLACEMENT_3D('',#167518,#112278,#112279);
#99034=AXIS2_PLACEMENT_3D('',#167521,#112281,#112282);
#99035=AXIS2_PLACEMENT_3D('',#167522,#112283,#112284);
#99036=AXIS2_PLACEMENT_3D('',#167523,#112285,#112286);
#99037=AXIS2_PLACEMENT_3D('',#167524,#112287,#112288);
#99038=AXIS2_PLACEMENT_3D('',#167527,#112289,#112290);
#99039=AXIS2_PLACEMENT_3D('',#167528,#112291,#112292);
#99040=AXIS2_PLACEMENT_3D('',#167530,#112293,#112294);
#99041=AXIS2_PLACEMENT_3D('',#167531,#112295,#112296);
#99042=AXIS2_PLACEMENT_3D('',#167532,#112297,#112298);
#99043=AXIS2_PLACEMENT_3D('',#167534,#112299,#112300);
#99044=AXIS2_PLACEMENT_3D('',#167536,#112301,#112302);
#99045=AXIS2_PLACEMENT_3D('',#167538,#112303,#112304);
#99046=AXIS2_PLACEMENT_3D('',#167539,#112305,#112306);
#99047=AXIS2_PLACEMENT_3D('',#167540,#112307,#112308);
#99048=AXIS2_PLACEMENT_3D('',#167542,#112309,#112310);
#99049=AXIS2_PLACEMENT_3D('',#167544,#112312,#112313);
#99050=AXIS2_PLACEMENT_3D('',#167547,#112315,#112316);
#99051=AXIS2_PLACEMENT_3D('',#167548,#112317,#112318);
#99052=AXIS2_PLACEMENT_3D('',#167549,#112319,#112320);
#99053=AXIS2_PLACEMENT_3D('',#167550,#112321,#112322);
#99054=AXIS2_PLACEMENT_3D('',#167552,#112323,#112324);
#99055=AXIS2_PLACEMENT_3D('',#167554,#112325,#112326);
#99056=AXIS2_PLACEMENT_3D('',#167556,#112327,#112328);
#99057=AXIS2_PLACEMENT_3D('',#167557,#112329,#112330);
#99058=AXIS2_PLACEMENT_3D('',#167558,#112331,#112332);
#99059=AXIS2_PLACEMENT_3D('',#167561,#112333,#112334);
#99060=AXIS2_PLACEMENT_3D('',#167562,#112335,#112336);
#99061=AXIS2_PLACEMENT_3D('',#167564,#112337,#112338);
#99062=AXIS2_PLACEMENT_3D('',#167565,#112339,#112340);
#99063=AXIS2_PLACEMENT_3D('',#167566,#112341,#112342);
#99064=AXIS2_PLACEMENT_3D('',#167568,#112343,#112344);
#99065=AXIS2_PLACEMENT_3D('',#167570,#112346,#112347);
#99066=AXIS2_PLACEMENT_3D('',#167573,#112349,#112350);
#99067=AXIS2_PLACEMENT_3D('',#167574,#112351,#112352);
#99068=AXIS2_PLACEMENT_3D('',#167575,#112353,#112354);
#99069=AXIS2_PLACEMENT_3D('',#167576,#112355,#112356);
#99070=AXIS2_PLACEMENT_3D('',#167578,#112357,#112358);
#99071=AXIS2_PLACEMENT_3D('',#167581,#112360,#112361);
#99072=AXIS2_PLACEMENT_3D('',#167582,#112362,#112363);
#99073=AXIS2_PLACEMENT_3D('',#167584,#112364,#112365);
#99074=AXIS2_PLACEMENT_3D('',#167587,#112367,#112368);
#99075=AXIS2_PLACEMENT_3D('',#167588,#112369,#112370);
#99076=AXIS2_PLACEMENT_3D('',#167589,#112371,#112372);
#99077=AXIS2_PLACEMENT_3D('',#167590,#112373,#112374);
#99078=AXIS2_PLACEMENT_3D('',#167593,#112375,#112376);
#99079=AXIS2_PLACEMENT_3D('',#167595,#112377,#112378);
#99080=AXIS2_PLACEMENT_3D('',#167597,#112379,#112380);
#99081=AXIS2_PLACEMENT_3D('',#167598,#112381,#112382);
#99082=AXIS2_PLACEMENT_3D('',#167599,#112383,#112384);
#99083=AXIS2_PLACEMENT_3D('',#167602,#112385,#112386);
#99084=AXIS2_PLACEMENT_3D('',#167604,#112387,#112388);
#99085=AXIS2_PLACEMENT_3D('',#167606,#112389,#112390);
#99086=AXIS2_PLACEMENT_3D('',#167607,#112391,#112392);
#99087=AXIS2_PLACEMENT_3D('',#167608,#112393,#112394);
#99088=AXIS2_PLACEMENT_3D('',#167611,#112395,#112396);
#99089=AXIS2_PLACEMENT_3D('',#167613,#112397,#112398);
#99090=AXIS2_PLACEMENT_3D('',#167615,#112399,#112400);
#99091=AXIS2_PLACEMENT_3D('',#167616,#112401,#112402);
#99092=AXIS2_PLACEMENT_3D('',#167617,#112403,#112404);
#99093=AXIS2_PLACEMENT_3D('',#167620,#112405,#112406);
#99094=AXIS2_PLACEMENT_3D('',#167622,#112407,#112408);
#99095=AXIS2_PLACEMENT_3D('',#167624,#112409,#112410);
#99096=AXIS2_PLACEMENT_3D('',#167626,#112411,#112412);
#99097=AXIS2_PLACEMENT_3D('',#167627,#112413,#112414);
#99098=AXIS2_PLACEMENT_3D('',#167628,#112415,#112416);
#99099=AXIS2_PLACEMENT_3D('',#167630,#112417,#112418);
#99100=AXIS2_PLACEMENT_3D('',#167632,#112419,#112420);
#99101=AXIS2_PLACEMENT_3D('',#167634,#112421,#112422);
#99102=AXIS2_PLACEMENT_3D('',#167635,#112423,#112424);
#99103=AXIS2_PLACEMENT_3D('',#167636,#112425,#112426);
#99104=AXIS2_PLACEMENT_3D('',#167638,#112427,#112428);
#99105=AXIS2_PLACEMENT_3D('',#167640,#112429,#112430);
#99106=AXIS2_PLACEMENT_3D('',#167641,#112431,#112432);
#99107=AXIS2_PLACEMENT_3D('',#167642,#112433,#112434);
#99108=AXIS2_PLACEMENT_3D('',#167644,#112435,#112436);
#99109=AXIS2_PLACEMENT_3D('',#167646,#112437,#112438);
#99110=AXIS2_PLACEMENT_3D('',#167648,#112439,#112440);
#99111=AXIS2_PLACEMENT_3D('',#167649,#112441,#112442);
#99112=AXIS2_PLACEMENT_3D('',#167650,#112443,#112444);
#99113=AXIS2_PLACEMENT_3D('',#167652,#112445,#112446);
#99114=AXIS2_PLACEMENT_3D('',#167654,#112447,#112448);
#99115=AXIS2_PLACEMENT_3D('',#167655,#112449,#112450);
#99116=AXIS2_PLACEMENT_3D('',#167656,#112451,#112452);
#99117=AXIS2_PLACEMENT_3D('',#167658,#112453,#112454);
#99118=AXIS2_PLACEMENT_3D('',#167661,#112456,#112457);
#99119=AXIS2_PLACEMENT_3D('',#167662,#112458,#112459);
#99120=AXIS2_PLACEMENT_3D('',#167664,#112461,#112462);
#99121=AXIS2_PLACEMENT_3D('',#167667,#112463,#112464);
#99122=AXIS2_PLACEMENT_3D('',#167715,#112466,#112467);
#99123=AXIS2_PLACEMENT_3D('',#167760,#112469,#112470);
#99124=AXIS2_PLACEMENT_3D('',#167808,#112472,#112473);
#99125=AXIS2_PLACEMENT_3D('',#167853,#112475,#112476);
#99126=AXIS2_PLACEMENT_3D('',#167901,#112478,#112479);
#99127=AXIS2_PLACEMENT_3D('',#167946,#112481,#112482);
#99128=AXIS2_PLACEMENT_3D('',#167994,#112484,#112485);
#99129=AXIS2_PLACEMENT_3D('',#168039,#112487,#112488);
#99130=AXIS2_PLACEMENT_3D('',#168087,#112490,#112491);
#99131=AXIS2_PLACEMENT_3D('',#168132,#112493,#112494);
#99132=AXIS2_PLACEMENT_3D('',#168180,#112496,#112497);
#99133=AXIS2_PLACEMENT_3D('',#168225,#112499,#112500);
#99134=AXIS2_PLACEMENT_3D('',#168273,#112502,#112503);
#99135=AXIS2_PLACEMENT_3D('',#168318,#112505,#112506);
#99136=AXIS2_PLACEMENT_3D('',#168366,#112508,#112509);
#99137=AXIS2_PLACEMENT_3D('',#168411,#112511,#112512);
#99138=AXIS2_PLACEMENT_3D('',#168459,#112514,#112515);
#99139=AXIS2_PLACEMENT_3D('',#168504,#112517,#112518);
#99140=AXIS2_PLACEMENT_3D('',#168552,#112520,#112521);
#99141=AXIS2_PLACEMENT_3D('',#168597,#112523,#112524);
#99142=AXIS2_PLACEMENT_3D('',#168645,#112526,#112527);
#99143=AXIS2_PLACEMENT_3D('',#168690,#112529,#112530);
#99144=AXIS2_PLACEMENT_3D('',#168738,#112532,#112533);
#99145=AXIS2_PLACEMENT_3D('',#168783,#112535,#112536);
#99146=AXIS2_PLACEMENT_3D('',#168831,#112538,#112539);
#99147=AXIS2_PLACEMENT_3D('',#168876,#112541,#112542);
#99148=AXIS2_PLACEMENT_3D('',#168924,#112544,#112545);
#99149=AXIS2_PLACEMENT_3D('',#168969,#112547,#112548);
#99150=AXIS2_PLACEMENT_3D('',#169017,#112550,#112551);
#99151=AXIS2_PLACEMENT_3D('',#169062,#112553,#112554);
#99152=AXIS2_PLACEMENT_3D('',#169110,#112556,#112557);
#99153=AXIS2_PLACEMENT_3D('',#169155,#112559,#112560);
#99154=AXIS2_PLACEMENT_3D('',#169203,#112562,#112563);
#99155=AXIS2_PLACEMENT_3D('',#169248,#112565,#112566);
#99156=AXIS2_PLACEMENT_3D('',#169296,#112568,#112569);
#99157=AXIS2_PLACEMENT_3D('',#169341,#112571,#112572);
#99158=AXIS2_PLACEMENT_3D('',#169389,#112574,#112575);
#99159=AXIS2_PLACEMENT_3D('',#169434,#112577,#112578);
#99160=AXIS2_PLACEMENT_3D('',#169482,#112580,#112581);
#99161=AXIS2_PLACEMENT_3D('',#169527,#112583,#112584);
#99162=AXIS2_PLACEMENT_3D('',#169575,#112586,#112587);
#99163=AXIS2_PLACEMENT_3D('',#169620,#112589,#112590);
#99164=AXIS2_PLACEMENT_3D('',#169668,#112592,#112593);
#99165=AXIS2_PLACEMENT_3D('',#169713,#112595,#112596);
#99166=AXIS2_PLACEMENT_3D('',#169761,#112598,#112599);
#99167=AXIS2_PLACEMENT_3D('',#169806,#112601,#112602);
#99168=AXIS2_PLACEMENT_3D('',#169854,#112604,#112605);
#99169=AXIS2_PLACEMENT_3D('',#169899,#112607,#112608);
#99170=AXIS2_PLACEMENT_3D('',#169947,#112610,#112611);
#99171=AXIS2_PLACEMENT_3D('',#169992,#112613,#112614);
#99172=AXIS2_PLACEMENT_3D('',#170040,#112616,#112617);
#99173=AXIS2_PLACEMENT_3D('',#170085,#112619,#112620);
#99174=AXIS2_PLACEMENT_3D('',#170133,#112622,#112623);
#99175=AXIS2_PLACEMENT_3D('',#170178,#112625,#112626);
#99176=AXIS2_PLACEMENT_3D('',#170226,#112628,#112629);
#99177=AXIS2_PLACEMENT_3D('',#170271,#112631,#112632);
#99178=AXIS2_PLACEMENT_3D('',#170319,#112634,#112635);
#99179=AXIS2_PLACEMENT_3D('',#170364,#112637,#112638);
#99180=AXIS2_PLACEMENT_3D('',#170412,#112640,#112641);
#99181=AXIS2_PLACEMENT_3D('',#170503,#112645,#112646);
#99182=AXIS2_PLACEMENT_3D('',#170548,#112648,#112649);
#99183=AXIS2_PLACEMENT_3D('',#170596,#112651,#112652);
#99184=AXIS2_PLACEMENT_3D('',#170641,#112654,#112655);
#99185=AXIS2_PLACEMENT_3D('',#170689,#112657,#112658);
#99186=AXIS2_PLACEMENT_3D('',#170734,#112660,#112661);
#99187=AXIS2_PLACEMENT_3D('',#170782,#112663,#112664);
#99188=AXIS2_PLACEMENT_3D('',#170827,#112666,#112667);
#99189=AXIS2_PLACEMENT_3D('',#170875,#112669,#112670);
#99190=AXIS2_PLACEMENT_3D('',#170920,#112672,#112673);
#99191=AXIS2_PLACEMENT_3D('',#170968,#112675,#112676);
#99192=AXIS2_PLACEMENT_3D('',#171013,#112678,#112679);
#99193=AXIS2_PLACEMENT_3D('',#171061,#112681,#112682);
#99194=AXIS2_PLACEMENT_3D('',#171106,#112684,#112685);
#99195=AXIS2_PLACEMENT_3D('',#171154,#112687,#112688);
#99196=AXIS2_PLACEMENT_3D('',#171199,#112690,#112691);
#99197=AXIS2_PLACEMENT_3D('',#171247,#112693,#112694);
#99198=AXIS2_PLACEMENT_3D('',#171292,#112696,#112697);
#99199=AXIS2_PLACEMENT_3D('',#171340,#112699,#112700);
#99200=AXIS2_PLACEMENT_3D('',#171385,#112702,#112703);
#99201=AXIS2_PLACEMENT_3D('',#171433,#112705,#112706);
#99202=AXIS2_PLACEMENT_3D('',#171478,#112708,#112709);
#99203=AXIS2_PLACEMENT_3D('',#171526,#112711,#112712);
#99204=AXIS2_PLACEMENT_3D('',#171571,#112714,#112715);
#99205=AXIS2_PLACEMENT_3D('',#171619,#112717,#112718);
#99206=AXIS2_PLACEMENT_3D('',#171664,#112720,#112721);
#99207=AXIS2_PLACEMENT_3D('',#171712,#112723,#112724);
#99208=AXIS2_PLACEMENT_3D('',#171757,#112726,#112727);
#99209=AXIS2_PLACEMENT_3D('',#171805,#112729,#112730);
#99210=AXIS2_PLACEMENT_3D('',#171895,#112733,#112734);
#99211=AXIS2_PLACEMENT_3D('',#171940,#112736,#112737);
#99212=AXIS2_PLACEMENT_3D('',#171988,#112739,#112740);
#99213=AXIS2_PLACEMENT_3D('',#172033,#112742,#112743);
#99214=AXIS2_PLACEMENT_3D('',#172081,#112745,#112746);
#99215=AXIS2_PLACEMENT_3D('',#172126,#112748,#112749);
#99216=AXIS2_PLACEMENT_3D('',#172174,#112751,#112752);
#99217=AXIS2_PLACEMENT_3D('',#172219,#112754,#112755);
#99218=AXIS2_PLACEMENT_3D('',#172267,#112757,#112758);
#99219=AXIS2_PLACEMENT_3D('',#172312,#112760,#112761);
#99220=AXIS2_PLACEMENT_3D('',#172360,#112763,#112764);
#99221=AXIS2_PLACEMENT_3D('',#172405,#112766,#112767);
#99222=AXIS2_PLACEMENT_3D('',#172453,#112769,#112770);
#99223=AXIS2_PLACEMENT_3D('',#172498,#112772,#112773);
#99224=AXIS2_PLACEMENT_3D('',#172546,#112775,#112776);
#99225=AXIS2_PLACEMENT_3D('',#172591,#112778,#112779);
#99226=AXIS2_PLACEMENT_3D('',#172639,#112781,#112782);
#99227=AXIS2_PLACEMENT_3D('',#172684,#112784,#112785);
#99228=AXIS2_PLACEMENT_3D('',#172732,#112787,#112788);
#99229=AXIS2_PLACEMENT_3D('',#172777,#112790,#112791);
#99230=AXIS2_PLACEMENT_3D('',#172825,#112793,#112794);
#99231=AXIS2_PLACEMENT_3D('',#172870,#112796,#112797);
#99232=AXIS2_PLACEMENT_3D('',#172918,#112799,#112800);
#99233=AXIS2_PLACEMENT_3D('',#172963,#112802,#112803);
#99234=AXIS2_PLACEMENT_3D('',#173011,#112805,#112806);
#99235=AXIS2_PLACEMENT_3D('',#173056,#112808,#112809);
#99236=AXIS2_PLACEMENT_3D('',#173104,#112811,#112812);
#99237=AXIS2_PLACEMENT_3D('',#173149,#112814,#112815);
#99238=AXIS2_PLACEMENT_3D('',#173197,#112817,#112818);
#99239=AXIS2_PLACEMENT_3D('',#173240,#112820,#112821);
#99240=AXIS2_PLACEMENT_3D('',#173282,#112823,#112824);
#99241=AXIS2_PLACEMENT_3D('',#173327,#112826,#112827);
#99242=AXIS2_PLACEMENT_3D('',#173369,#112829,#112830);
#99243=AXIS2_PLACEMENT_3D('',#173414,#112832,#112833);
#99244=AXIS2_PLACEMENT_3D('',#173456,#112835,#112836);
#99245=AXIS2_PLACEMENT_3D('',#173501,#112838,#112839);
#99246=AXIS2_PLACEMENT_3D('',#173543,#112841,#112842);
#99247=AXIS2_PLACEMENT_3D('',#173588,#112844,#112845);
#99248=AXIS2_PLACEMENT_3D('',#173630,#112847,#112848);
#99249=AXIS2_PLACEMENT_3D('',#173675,#112850,#112851);
#99250=AXIS2_PLACEMENT_3D('',#173717,#112853,#112854);
#99251=AXIS2_PLACEMENT_3D('',#173762,#112856,#112857);
#99252=AXIS2_PLACEMENT_3D('',#173804,#112859,#112860);
#99253=AXIS2_PLACEMENT_3D('',#173849,#112862,#112863);
#99254=AXIS2_PLACEMENT_3D('',#173891,#112865,#112866);
#99255=AXIS2_PLACEMENT_3D('',#173936,#112868,#112869);
#99256=AXIS2_PLACEMENT_3D('',#173978,#112871,#112872);
#99257=AXIS2_PLACEMENT_3D('',#174023,#112874,#112875);
#99258=AXIS2_PLACEMENT_3D('',#174065,#112877,#112878);
#99259=AXIS2_PLACEMENT_3D('',#174110,#112880,#112881);
#99260=AXIS2_PLACEMENT_3D('',#174152,#112883,#112884);
#99261=AXIS2_PLACEMENT_3D('',#174197,#112886,#112887);
#99262=AXIS2_PLACEMENT_3D('',#174239,#112889,#112890);
#99263=AXIS2_PLACEMENT_3D('',#174284,#112892,#112893);
#99264=AXIS2_PLACEMENT_3D('',#174326,#112895,#112896);
#99265=AXIS2_PLACEMENT_3D('',#174371,#112898,#112899);
#99266=AXIS2_PLACEMENT_3D('',#174413,#112901,#112902);
#99267=AXIS2_PLACEMENT_3D('',#174458,#112904,#112905);
#99268=AXIS2_PLACEMENT_3D('',#174500,#112907,#112908);
#99269=AXIS2_PLACEMENT_3D('',#174545,#112910,#112911);
#99270=AXIS2_PLACEMENT_3D('',#174587,#112913,#112914);
#99271=AXIS2_PLACEMENT_3D('',#174632,#112916,#112917);
#99272=AXIS2_PLACEMENT_3D('',#174674,#112919,#112920);
#99273=AXIS2_PLACEMENT_3D('',#174719,#112922,#112923);
#99274=AXIS2_PLACEMENT_3D('',#174761,#112925,#112926);
#99275=AXIS2_PLACEMENT_3D('',#174806,#112928,#112929);
#99276=AXIS2_PLACEMENT_3D('',#174848,#112931,#112932);
#99277=AXIS2_PLACEMENT_3D('',#174893,#112934,#112935);
#99278=AXIS2_PLACEMENT_3D('',#174935,#112937,#112938);
#99279=AXIS2_PLACEMENT_3D('',#174980,#112940,#112941);
#99280=AXIS2_PLACEMENT_3D('',#175022,#112943,#112944);
#99281=AXIS2_PLACEMENT_3D('',#175067,#112946,#112947);
#99282=AXIS2_PLACEMENT_3D('',#175109,#112949,#112950);
#99283=AXIS2_PLACEMENT_3D('',#175154,#112952,#112953);
#99284=AXIS2_PLACEMENT_3D('',#175196,#112955,#112956);
#99285=AXIS2_PLACEMENT_3D('',#175241,#112958,#112959);
#99286=AXIS2_PLACEMENT_3D('',#175283,#112961,#112962);
#99287=AXIS2_PLACEMENT_3D('',#175328,#112964,#112965);
#99288=AXIS2_PLACEMENT_3D('',#175370,#112967,#112968);
#99289=AXIS2_PLACEMENT_3D('',#175415,#112970,#112971);
#99290=AXIS2_PLACEMENT_3D('',#175457,#112973,#112974);
#99291=AXIS2_PLACEMENT_3D('',#175502,#112976,#112977);
#99292=AXIS2_PLACEMENT_3D('',#175544,#112979,#112980);
#99293=AXIS2_PLACEMENT_3D('',#175589,#112982,#112983);
#99294=AXIS2_PLACEMENT_3D('',#175631,#112985,#112986);
#99295=AXIS2_PLACEMENT_3D('',#175676,#112988,#112989);
#99296=AXIS2_PLACEMENT_3D('',#175718,#112991,#112992);
#99297=AXIS2_PLACEMENT_3D('',#175763,#112994,#112995);
#99298=AXIS2_PLACEMENT_3D('',#175805,#112997,#112998);
#99299=AXIS2_PLACEMENT_3D('',#175850,#113000,#113001);
#99300=AXIS2_PLACEMENT_3D('',#175853,#113003,#113004);
#99301=AXIS2_PLACEMENT_3D('',#175895,#113006,#113007);
#99302=AXIS2_PLACEMENT_3D('',#175940,#113009,#113010);
#99303=AXIS2_PLACEMENT_3D('',#175982,#113012,#113013);
#99304=AXIS2_PLACEMENT_3D('',#176027,#113015,#113016);
#99305=AXIS2_PLACEMENT_3D('',#176069,#113018,#113019);
#99306=AXIS2_PLACEMENT_3D('',#176114,#113021,#113022);
#99307=AXIS2_PLACEMENT_3D('',#176156,#113024,#113025);
#99308=AXIS2_PLACEMENT_3D('',#176201,#113027,#113028);
#99309=AXIS2_PLACEMENT_3D('',#176243,#113030,#113031);
#99310=AXIS2_PLACEMENT_3D('',#176288,#113033,#113034);
#99311=AXIS2_PLACEMENT_3D('',#176330,#113036,#113037);
#99312=AXIS2_PLACEMENT_3D('',#176375,#113039,#113040);
#99313=AXIS2_PLACEMENT_3D('',#176417,#113042,#113043);
#99314=AXIS2_PLACEMENT_3D('',#176462,#113045,#113046);
#99315=AXIS2_PLACEMENT_3D('',#176504,#113048,#113049);
#99316=AXIS2_PLACEMENT_3D('',#176549,#113051,#113052);
#99317=AXIS2_PLACEMENT_3D('',#176591,#113054,#113055);
#99318=AXIS2_PLACEMENT_3D('',#176636,#113057,#113058);
#99319=AXIS2_PLACEMENT_3D('',#176678,#113060,#113061);
#99320=AXIS2_PLACEMENT_3D('',#176723,#113063,#113064);
#99321=AXIS2_PLACEMENT_3D('',#176765,#113066,#113067);
#99322=AXIS2_PLACEMENT_3D('',#176810,#113069,#113070);
#99323=AXIS2_PLACEMENT_3D('',#176852,#113072,#113073);
#99324=AXIS2_PLACEMENT_3D('',#176897,#113075,#113076);
#99325=AXIS2_PLACEMENT_3D('',#176939,#113078,#113079);
#99326=AXIS2_PLACEMENT_3D('',#176984,#113081,#113082);
#99327=AXIS2_PLACEMENT_3D('',#177026,#113084,#113085);
#99328=AXIS2_PLACEMENT_3D('',#177071,#113087,#113088);
#99329=AXIS2_PLACEMENT_3D('',#177113,#113090,#113091);
#99330=AXIS2_PLACEMENT_3D('',#177197,#113094,#113095);
#99331=AXIS2_PLACEMENT_3D('',#177242,#113097,#113098);
#99332=AXIS2_PLACEMENT_3D('',#177284,#113100,#113101);
#99333=AXIS2_PLACEMENT_3D('',#177329,#113103,#113104);
#99334=AXIS2_PLACEMENT_3D('',#177371,#113106,#113107);
#99335=AXIS2_PLACEMENT_3D('',#177416,#113109,#113110);
#99336=AXIS2_PLACEMENT_3D('',#177458,#113112,#113113);
#99337=AXIS2_PLACEMENT_3D('',#177503,#113115,#113116);
#99338=AXIS2_PLACEMENT_3D('',#177545,#113118,#113119);
#99339=AXIS2_PLACEMENT_3D('',#177590,#113121,#113122);
#99340=AXIS2_PLACEMENT_3D('',#177632,#113124,#113125);
#99341=AXIS2_PLACEMENT_3D('',#177677,#113127,#113128);
#99342=AXIS2_PLACEMENT_3D('',#177719,#113130,#113131);
#99343=AXIS2_PLACEMENT_3D('',#177764,#113133,#113134);
#99344=AXIS2_PLACEMENT_3D('',#177806,#113136,#113137);
#99345=AXIS2_PLACEMENT_3D('',#177851,#113139,#113140);
#99346=AXIS2_PLACEMENT_3D('',#177893,#113142,#113143);
#99347=AXIS2_PLACEMENT_3D('',#177938,#113145,#113146);
#99348=AXIS2_PLACEMENT_3D('',#177980,#113148,#113149);
#99349=AXIS2_PLACEMENT_3D('',#178025,#113151,#113152);
#99350=AXIS2_PLACEMENT_3D('',#178067,#113154,#113155);
#99351=AXIS2_PLACEMENT_3D('',#178112,#113157,#113158);
#99352=AXIS2_PLACEMENT_3D('',#178154,#113160,#113161);
#99353=AXIS2_PLACEMENT_3D('',#178199,#113163,#113164);
#99354=AXIS2_PLACEMENT_3D('',#178241,#113166,#113167);
#99355=AXIS2_PLACEMENT_3D('',#178286,#113169,#113170);
#99356=AXIS2_PLACEMENT_3D('',#178328,#113172,#113173);
#99357=AXIS2_PLACEMENT_3D('',#178373,#113175,#113176);
#99358=AXIS2_PLACEMENT_3D('',#178415,#113178,#113179);
#99359=AXIS2_PLACEMENT_3D('',#178458,#113181,#113182);
#99360=AXIS2_PLACEMENT_3D('',#178461,#113183,#113184);
#99361=AXIS2_PLACEMENT_3D('',#178463,#113186,#113187);
#99362=AXIS2_PLACEMENT_3D('',#178464,#113188,#113189);
#99363=AXIS2_PLACEMENT_3D('',#178467,#113191,#113192);
#99364=AXIS2_PLACEMENT_3D('',#178468,#113193,#113194);
#99365=AXIS2_PLACEMENT_3D('',#178471,#113195,#113196);
#99366=AXIS2_PLACEMENT_3D('',#178475,#113198,#113199);
#99367=AXIS2_PLACEMENT_3D('',#178479,#113201,#113202);
#99368=AXIS2_PLACEMENT_3D('',#178480,#113203,#113204);
#99369=AXIS2_PLACEMENT_3D('',#178481,#113205,#113206);
#99370=AXIS2_PLACEMENT_3D('',#178484,#113207,#113208);
#99371=AXIS2_PLACEMENT_3D('',#178487,#113211,#113212);
#99372=AXIS2_PLACEMENT_3D('',#178490,#113213,#113214);
#99373=AXIS2_PLACEMENT_3D('',#178494,#113216,#113217);
#99374=AXIS2_PLACEMENT_3D('',#178496,#113219,#113220);
#99375=AXIS2_PLACEMENT_3D('',#178499,#113221,#113222);
#99376=AXIS2_PLACEMENT_3D('',#178503,#113224,#113225);
#99377=AXIS2_PLACEMENT_3D('',#178507,#113227,#113228);
#99378=AXIS2_PLACEMENT_3D('',#178508,#113229,#113230);
#99379=AXIS2_PLACEMENT_3D('',#178509,#113231,#113232);
#99380=AXIS2_PLACEMENT_3D('',#178512,#113233,#113234);
#99381=AXIS2_PLACEMENT_3D('',#178515,#113237,#113238);
#99382=AXIS2_PLACEMENT_3D('',#178516,#113239,#113240);
#99383=AXIS2_PLACEMENT_3D('',#178517,#113241,#113242);
#99384=AXIS2_PLACEMENT_3D('',#178518,#113243,#113244);
#99385=AXIS2_PLACEMENT_3D('',#178519,#113245,#113246);
#99386=AXIS2_PLACEMENT_3D('',#178520,#113247,#113248);
#99387=AXIS2_PLACEMENT_3D('',#178521,#113249,#113250);
#99388=AXIS2_PLACEMENT_3D('',#178522,#113251,#113252);
#99389=AXIS2_PLACEMENT_3D('',#178523,#113253,#113254);
#99390=AXIS2_PLACEMENT_3D('',#178524,#113255,#113256);
#99391=AXIS2_PLACEMENT_3D('',#178525,#113257,#113258);
#99392=AXIS2_PLACEMENT_3D('',#178526,#113259,#113260);
#99393=AXIS2_PLACEMENT_3D('',#178527,#113261,#113262);
#99394=AXIS2_PLACEMENT_3D('',#178530,#113263,#113264);
#99395=AXIS2_PLACEMENT_3D('',#178534,#113266,#113267);
#99396=AXIS2_PLACEMENT_3D('',#178536,#113268,#113269);
#99397=AXIS2_PLACEMENT_3D('',#178538,#113270,#113271);
#99398=AXIS2_PLACEMENT_3D('',#178540,#113273,#113274);
#99399=AXIS2_PLACEMENT_3D('',#178544,#113276,#113277);
#99400=AXIS2_PLACEMENT_3D('',#178546,#113279,#113280);
#99401=AXIS2_PLACEMENT_3D('',#178549,#113281,#113282);
#99402=AXIS2_PLACEMENT_3D('',#178553,#113284,#113285);
#99403=AXIS2_PLACEMENT_3D('',#178555,#113287,#113288);
#99404=AXIS2_PLACEMENT_3D('',#178558,#113289,#113290);
#99405=AXIS2_PLACEMENT_3D('',#178562,#113292,#113293);
#99406=AXIS2_PLACEMENT_3D('',#178564,#113294,#113295);
#99407=AXIS2_PLACEMENT_3D('',#178566,#113296,#113297);
#99408=AXIS2_PLACEMENT_3D('',#178568,#113299,#113300);
#99409=AXIS2_PLACEMENT_3D('',#178572,#113302,#113303);
#99410=AXIS2_PLACEMENT_3D('',#178574,#113305,#113306);
#99411=AXIS2_PLACEMENT_3D('',#178575,#113307,#113308);
#99412=AXIS2_PLACEMENT_3D('',#178576,#113309,#113310);
#99413=AXIS2_PLACEMENT_3D('',#178577,#113311,#113312);
#99414=AXIS2_PLACEMENT_3D('',#178578,#113313,#113314);
#99415=AXIS2_PLACEMENT_3D('',#178579,#113315,#113316);
#99416=AXIS2_PLACEMENT_3D('',#178580,#113317,#113318);
#99417=AXIS2_PLACEMENT_3D('',#178581,#113319,#113320);
#99418=AXIS2_PLACEMENT_3D('',#178582,#113321,#113322);
#99419=AXIS2_PLACEMENT_3D('',#178583,#113323,#113324);
#99420=AXIS2_PLACEMENT_3D('',#178584,#113325,#113326);
#99421=AXIS2_PLACEMENT_3D('',#178585,#113327,#113328);
#99422=AXIS2_PLACEMENT_3D('',#178586,#113329,#113330);
#99423=AXIS2_PLACEMENT_3D('',#178589,#113331,#113332);
#99424=AXIS2_PLACEMENT_3D('',#178593,#113334,#113335);
#99425=AXIS2_PLACEMENT_3D('',#178595,#113336,#113337);
#99426=AXIS2_PLACEMENT_3D('',#178597,#113338,#113339);
#99427=AXIS2_PLACEMENT_3D('',#178599,#113341,#113342);
#99428=AXIS2_PLACEMENT_3D('',#178603,#113344,#113345);
#99429=AXIS2_PLACEMENT_3D('',#178605,#113347,#113348);
#99430=AXIS2_PLACEMENT_3D('',#178608,#113349,#113350);
#99431=AXIS2_PLACEMENT_3D('',#178612,#113352,#113353);
#99432=AXIS2_PLACEMENT_3D('',#178614,#113355,#113356);
#99433=AXIS2_PLACEMENT_3D('',#178617,#113357,#113358);
#99434=AXIS2_PLACEMENT_3D('',#178621,#113360,#113361);
#99435=AXIS2_PLACEMENT_3D('',#178623,#113362,#113363);
#99436=AXIS2_PLACEMENT_3D('',#178625,#113364,#113365);
#99437=AXIS2_PLACEMENT_3D('',#178627,#113367,#113368);
#99438=AXIS2_PLACEMENT_3D('',#178631,#113370,#113371);
#99439=AXIS2_PLACEMENT_3D('',#178633,#113373,#113374);
#99440=AXIS2_PLACEMENT_3D('',#178634,#113375,#113376);
#99441=AXIS2_PLACEMENT_3D('',#178635,#113377,#113378);
#99442=AXIS2_PLACEMENT_3D('',#178636,#113379,#113380);
#99443=AXIS2_PLACEMENT_3D('',#178637,#113381,#113382);
#99444=AXIS2_PLACEMENT_3D('',#178638,#113383,#113384);
#99445=AXIS2_PLACEMENT_3D('',#178639,#113385,#113386);
#99446=AXIS2_PLACEMENT_3D('',#178640,#113387,#113388);
#99447=AXIS2_PLACEMENT_3D('',#178641,#113389,#113390);
#99448=AXIS2_PLACEMENT_3D('',#178642,#113391,#113392);
#99449=AXIS2_PLACEMENT_3D('',#178643,#113393,#113394);
#99450=AXIS2_PLACEMENT_3D('',#178644,#113395,#113396);
#99451=AXIS2_PLACEMENT_3D('',#178645,#113397,#113398);
#99452=AXIS2_PLACEMENT_3D('',#178648,#113399,#113400);
#99453=AXIS2_PLACEMENT_3D('',#178652,#113402,#113403);
#99454=AXIS2_PLACEMENT_3D('',#178654,#113404,#113405);
#99455=AXIS2_PLACEMENT_3D('',#178656,#113406,#113407);
#99456=AXIS2_PLACEMENT_3D('',#178658,#113409,#113410);
#99457=AXIS2_PLACEMENT_3D('',#178662,#113412,#113413);
#99458=AXIS2_PLACEMENT_3D('',#178664,#113415,#113416);
#99459=AXIS2_PLACEMENT_3D('',#178667,#113417,#113418);
#99460=AXIS2_PLACEMENT_3D('',#178671,#113420,#113421);
#99461=AXIS2_PLACEMENT_3D('',#178673,#113423,#113424);
#99462=AXIS2_PLACEMENT_3D('',#178676,#113425,#113426);
#99463=AXIS2_PLACEMENT_3D('',#178680,#113428,#113429);
#99464=AXIS2_PLACEMENT_3D('',#178682,#113430,#113431);
#99465=AXIS2_PLACEMENT_3D('',#178684,#113432,#113433);
#99466=AXIS2_PLACEMENT_3D('',#178686,#113435,#113436);
#99467=AXIS2_PLACEMENT_3D('',#178690,#113438,#113439);
#99468=AXIS2_PLACEMENT_3D('',#178692,#113441,#113442);
#99469=AXIS2_PLACEMENT_3D('',#178693,#113443,#113444);
#99470=AXIS2_PLACEMENT_3D('',#178694,#113445,#113446);
#99471=AXIS2_PLACEMENT_3D('',#178695,#113447,#113448);
#99472=AXIS2_PLACEMENT_3D('',#178696,#113449,#113450);
#99473=AXIS2_PLACEMENT_3D('',#178697,#113451,#113452);
#99474=AXIS2_PLACEMENT_3D('',#178698,#113453,#113454);
#99475=AXIS2_PLACEMENT_3D('',#178699,#113455,#113456);
#99476=AXIS2_PLACEMENT_3D('',#178700,#113457,#113458);
#99477=AXIS2_PLACEMENT_3D('',#178701,#113459,#113460);
#99478=AXIS2_PLACEMENT_3D('',#178702,#113461,#113462);
#99479=AXIS2_PLACEMENT_3D('',#178703,#113463,#113464);
#99480=AXIS2_PLACEMENT_3D('',#178704,#113465,#113466);
#99481=AXIS2_PLACEMENT_3D('',#178707,#113467,#113468);
#99482=AXIS2_PLACEMENT_3D('',#178711,#113470,#113471);
#99483=AXIS2_PLACEMENT_3D('',#178713,#113472,#113473);
#99484=AXIS2_PLACEMENT_3D('',#178715,#113474,#113475);
#99485=AXIS2_PLACEMENT_3D('',#178717,#113477,#113478);
#99486=AXIS2_PLACEMENT_3D('',#178721,#113480,#113481);
#99487=AXIS2_PLACEMENT_3D('',#178723,#113483,#113484);
#99488=AXIS2_PLACEMENT_3D('',#178726,#113485,#113486);
#99489=AXIS2_PLACEMENT_3D('',#178730,#113488,#113489);
#99490=AXIS2_PLACEMENT_3D('',#178732,#113491,#113492);
#99491=AXIS2_PLACEMENT_3D('',#178735,#113493,#113494);
#99492=AXIS2_PLACEMENT_3D('',#178739,#113496,#113497);
#99493=AXIS2_PLACEMENT_3D('',#178741,#113498,#113499);
#99494=AXIS2_PLACEMENT_3D('',#178743,#113500,#113501);
#99495=AXIS2_PLACEMENT_3D('',#178745,#113503,#113504);
#99496=AXIS2_PLACEMENT_3D('',#178749,#113506,#113507);
#99497=AXIS2_PLACEMENT_3D('',#178751,#113509,#113510);
#99498=AXIS2_PLACEMENT_3D('',#178752,#113511,#113512);
#99499=AXIS2_PLACEMENT_3D('',#178753,#113513,#113514);
#99500=AXIS2_PLACEMENT_3D('',#178754,#113515,#113516);
#99501=AXIS2_PLACEMENT_3D('',#178755,#113517,#113518);
#99502=AXIS2_PLACEMENT_3D('',#178756,#113519,#113520);
#99503=AXIS2_PLACEMENT_3D('',#178757,#113521,#113522);
#99504=AXIS2_PLACEMENT_3D('',#178758,#113523,#113524);
#99505=AXIS2_PLACEMENT_3D('',#178759,#113525,#113526);
#99506=AXIS2_PLACEMENT_3D('',#178760,#113527,#113528);
#99507=AXIS2_PLACEMENT_3D('',#178761,#113529,#113530);
#99508=AXIS2_PLACEMENT_3D('',#178762,#113531,#113532);
#99509=AXIS2_PLACEMENT_3D('',#178763,#113533,#113534);
#99510=AXIS2_PLACEMENT_3D('',#178766,#113535,#113536);
#99511=AXIS2_PLACEMENT_3D('',#178770,#113538,#113539);
#99512=AXIS2_PLACEMENT_3D('',#178772,#113540,#113541);
#99513=AXIS2_PLACEMENT_3D('',#178774,#113542,#113543);
#99514=AXIS2_PLACEMENT_3D('',#178776,#113545,#113546);
#99515=AXIS2_PLACEMENT_3D('',#178780,#113548,#113549);
#99516=AXIS2_PLACEMENT_3D('',#178782,#113551,#113552);
#99517=AXIS2_PLACEMENT_3D('',#178785,#113553,#113554);
#99518=AXIS2_PLACEMENT_3D('',#178789,#113556,#113557);
#99519=AXIS2_PLACEMENT_3D('',#178791,#113559,#113560);
#99520=AXIS2_PLACEMENT_3D('',#178794,#113561,#113562);
#99521=AXIS2_PLACEMENT_3D('',#178798,#113564,#113565);
#99522=AXIS2_PLACEMENT_3D('',#178800,#113566,#113567);
#99523=AXIS2_PLACEMENT_3D('',#178802,#113568,#113569);
#99524=AXIS2_PLACEMENT_3D('',#178804,#113571,#113572);
#99525=AXIS2_PLACEMENT_3D('',#178808,#113574,#113575);
#99526=AXIS2_PLACEMENT_3D('',#178810,#113577,#113578);
#99527=AXIS2_PLACEMENT_3D('',#178811,#113579,#113580);
#99528=AXIS2_PLACEMENT_3D('',#178812,#113581,#113582);
#99529=AXIS2_PLACEMENT_3D('',#178813,#113583,#113584);
#99530=AXIS2_PLACEMENT_3D('',#178814,#113585,#113586);
#99531=AXIS2_PLACEMENT_3D('',#178815,#113587,#113588);
#99532=AXIS2_PLACEMENT_3D('',#178816,#113589,#113590);
#99533=AXIS2_PLACEMENT_3D('',#178817,#113591,#113592);
#99534=AXIS2_PLACEMENT_3D('',#178818,#113593,#113594);
#99535=AXIS2_PLACEMENT_3D('',#178819,#113595,#113596);
#99536=AXIS2_PLACEMENT_3D('',#178820,#113597,#113598);
#99537=AXIS2_PLACEMENT_3D('',#178821,#113599,#113600);
#99538=AXIS2_PLACEMENT_3D('',#178822,#113601,#113602);
#99539=AXIS2_PLACEMENT_3D('',#178825,#113603,#113604);
#99540=AXIS2_PLACEMENT_3D('',#178829,#113606,#113607);
#99541=AXIS2_PLACEMENT_3D('',#178831,#113608,#113609);
#99542=AXIS2_PLACEMENT_3D('',#178833,#113610,#113611);
#99543=AXIS2_PLACEMENT_3D('',#178835,#113613,#113614);
#99544=AXIS2_PLACEMENT_3D('',#178839,#113616,#113617);
#99545=AXIS2_PLACEMENT_3D('',#178841,#113619,#113620);
#99546=AXIS2_PLACEMENT_3D('',#178844,#113621,#113622);
#99547=AXIS2_PLACEMENT_3D('',#178848,#113624,#113625);
#99548=AXIS2_PLACEMENT_3D('',#178850,#113627,#113628);
#99549=AXIS2_PLACEMENT_3D('',#178853,#113629,#113630);
#99550=AXIS2_PLACEMENT_3D('',#178857,#113632,#113633);
#99551=AXIS2_PLACEMENT_3D('',#178859,#113634,#113635);
#99552=AXIS2_PLACEMENT_3D('',#178861,#113636,#113637);
#99553=AXIS2_PLACEMENT_3D('',#178863,#113639,#113640);
#99554=AXIS2_PLACEMENT_3D('',#178867,#113642,#113643);
#99555=AXIS2_PLACEMENT_3D('',#178869,#113645,#113646);
#99556=AXIS2_PLACEMENT_3D('',#178870,#113647,#113648);
#99557=AXIS2_PLACEMENT_3D('',#178871,#113649,#113650);
#99558=AXIS2_PLACEMENT_3D('',#178872,#113651,#113652);
#99559=AXIS2_PLACEMENT_3D('',#178873,#113653,#113654);
#99560=AXIS2_PLACEMENT_3D('',#178874,#113655,#113656);
#99561=AXIS2_PLACEMENT_3D('',#178875,#113657,#113658);
#99562=AXIS2_PLACEMENT_3D('',#178876,#113659,#113660);
#99563=AXIS2_PLACEMENT_3D('',#178877,#113661,#113662);
#99564=AXIS2_PLACEMENT_3D('',#178878,#113663,#113664);
#99565=AXIS2_PLACEMENT_3D('',#178879,#113665,#113666);
#99566=AXIS2_PLACEMENT_3D('',#178880,#113667,#113668);
#99567=AXIS2_PLACEMENT_3D('',#178881,#113669,#113670);
#99568=AXIS2_PLACEMENT_3D('',#178884,#113671,#113672);
#99569=AXIS2_PLACEMENT_3D('',#178888,#113674,#113675);
#99570=AXIS2_PLACEMENT_3D('',#178890,#113676,#113677);
#99571=AXIS2_PLACEMENT_3D('',#178892,#113678,#113679);
#99572=AXIS2_PLACEMENT_3D('',#178894,#113681,#113682);
#99573=AXIS2_PLACEMENT_3D('',#178898,#113684,#113685);
#99574=AXIS2_PLACEMENT_3D('',#178900,#113687,#113688);
#99575=AXIS2_PLACEMENT_3D('',#178903,#113689,#113690);
#99576=AXIS2_PLACEMENT_3D('',#178907,#113692,#113693);
#99577=AXIS2_PLACEMENT_3D('',#178909,#113695,#113696);
#99578=AXIS2_PLACEMENT_3D('',#178912,#113697,#113698);
#99579=AXIS2_PLACEMENT_3D('',#178916,#113700,#113701);
#99580=AXIS2_PLACEMENT_3D('',#178918,#113702,#113703);
#99581=AXIS2_PLACEMENT_3D('',#178920,#113704,#113705);
#99582=AXIS2_PLACEMENT_3D('',#178922,#113707,#113708);
#99583=AXIS2_PLACEMENT_3D('',#178926,#113710,#113711);
#99584=AXIS2_PLACEMENT_3D('',#178928,#113713,#113714);
#99585=AXIS2_PLACEMENT_3D('',#178929,#113715,#113716);
#99586=AXIS2_PLACEMENT_3D('',#178930,#113717,#113718);
#99587=AXIS2_PLACEMENT_3D('',#178931,#113719,#113720);
#99588=AXIS2_PLACEMENT_3D('',#178932,#113721,#113722);
#99589=AXIS2_PLACEMENT_3D('',#178933,#113723,#113724);
#99590=AXIS2_PLACEMENT_3D('',#178934,#113725,#113726);
#99591=AXIS2_PLACEMENT_3D('',#178935,#113727,#113728);
#99592=AXIS2_PLACEMENT_3D('',#178936,#113729,#113730);
#99593=AXIS2_PLACEMENT_3D('',#178937,#113731,#113732);
#99594=AXIS2_PLACEMENT_3D('',#178938,#113733,#113734);
#99595=AXIS2_PLACEMENT_3D('',#178939,#113735,#113736);
#99596=AXIS2_PLACEMENT_3D('',#178940,#113737,#113738);
#99597=AXIS2_PLACEMENT_3D('',#178943,#113739,#113740);
#99598=AXIS2_PLACEMENT_3D('',#178947,#113742,#113743);
#99599=AXIS2_PLACEMENT_3D('',#178949,#113744,#113745);
#99600=AXIS2_PLACEMENT_3D('',#178951,#113746,#113747);
#99601=AXIS2_PLACEMENT_3D('',#178953,#113749,#113750);
#99602=AXIS2_PLACEMENT_3D('',#178957,#113752,#113753);
#99603=AXIS2_PLACEMENT_3D('',#178959,#113755,#113756);
#99604=AXIS2_PLACEMENT_3D('',#178962,#113757,#113758);
#99605=AXIS2_PLACEMENT_3D('',#178966,#113760,#113761);
#99606=AXIS2_PLACEMENT_3D('',#178968,#113763,#113764);
#99607=AXIS2_PLACEMENT_3D('',#178971,#113765,#113766);
#99608=AXIS2_PLACEMENT_3D('',#178975,#113768,#113769);
#99609=AXIS2_PLACEMENT_3D('',#178977,#113770,#113771);
#99610=AXIS2_PLACEMENT_3D('',#178979,#113772,#113773);
#99611=AXIS2_PLACEMENT_3D('',#178981,#113775,#113776);
#99612=AXIS2_PLACEMENT_3D('',#178985,#113778,#113779);
#99613=AXIS2_PLACEMENT_3D('',#178987,#113781,#113782);
#99614=AXIS2_PLACEMENT_3D('',#178988,#113783,#113784);
#99615=AXIS2_PLACEMENT_3D('',#178989,#113785,#113786);
#99616=AXIS2_PLACEMENT_3D('',#178990,#113787,#113788);
#99617=AXIS2_PLACEMENT_3D('',#178991,#113789,#113790);
#99618=AXIS2_PLACEMENT_3D('',#178992,#113791,#113792);
#99619=AXIS2_PLACEMENT_3D('',#178993,#113793,#113794);
#99620=AXIS2_PLACEMENT_3D('',#178994,#113795,#113796);
#99621=AXIS2_PLACEMENT_3D('',#178995,#113797,#113798);
#99622=AXIS2_PLACEMENT_3D('',#178996,#113799,#113800);
#99623=AXIS2_PLACEMENT_3D('',#178997,#113801,#113802);
#99624=AXIS2_PLACEMENT_3D('',#178998,#113803,#113804);
#99625=AXIS2_PLACEMENT_3D('',#178999,#113805,#113806);
#99626=AXIS2_PLACEMENT_3D('',#179002,#113807,#113808);
#99627=AXIS2_PLACEMENT_3D('',#179006,#113810,#113811);
#99628=AXIS2_PLACEMENT_3D('',#179008,#113812,#113813);
#99629=AXIS2_PLACEMENT_3D('',#179010,#113814,#113815);
#99630=AXIS2_PLACEMENT_3D('',#179012,#113817,#113818);
#99631=AXIS2_PLACEMENT_3D('',#179016,#113820,#113821);
#99632=AXIS2_PLACEMENT_3D('',#179018,#113823,#113824);
#99633=AXIS2_PLACEMENT_3D('',#179021,#113825,#113826);
#99634=AXIS2_PLACEMENT_3D('',#179025,#113828,#113829);
#99635=AXIS2_PLACEMENT_3D('',#179027,#113831,#113832);
#99636=AXIS2_PLACEMENT_3D('',#179030,#113833,#113834);
#99637=AXIS2_PLACEMENT_3D('',#179034,#113836,#113837);
#99638=AXIS2_PLACEMENT_3D('',#179036,#113838,#113839);
#99639=AXIS2_PLACEMENT_3D('',#179038,#113840,#113841);
#99640=AXIS2_PLACEMENT_3D('',#179040,#113843,#113844);
#99641=AXIS2_PLACEMENT_3D('',#179044,#113846,#113847);
#99642=AXIS2_PLACEMENT_3D('',#179046,#113849,#113850);
#99643=AXIS2_PLACEMENT_3D('',#179047,#113851,#113852);
#99644=AXIS2_PLACEMENT_3D('',#179048,#113853,#113854);
#99645=AXIS2_PLACEMENT_3D('',#179049,#113855,#113856);
#99646=AXIS2_PLACEMENT_3D('',#179050,#113857,#113858);
#99647=AXIS2_PLACEMENT_3D('',#179051,#113859,#113860);
#99648=AXIS2_PLACEMENT_3D('',#179052,#113861,#113862);
#99649=AXIS2_PLACEMENT_3D('',#179053,#113863,#113864);
#99650=AXIS2_PLACEMENT_3D('',#179054,#113865,#113866);
#99651=AXIS2_PLACEMENT_3D('',#179055,#113867,#113868);
#99652=AXIS2_PLACEMENT_3D('',#179056,#113869,#113870);
#99653=AXIS2_PLACEMENT_3D('',#179057,#113871,#113872);
#99654=AXIS2_PLACEMENT_3D('',#179058,#113873,#113874);
#99655=AXIS2_PLACEMENT_3D('',#179061,#113875,#113876);
#99656=AXIS2_PLACEMENT_3D('',#179065,#113878,#113879);
#99657=AXIS2_PLACEMENT_3D('',#179067,#113880,#113881);
#99658=AXIS2_PLACEMENT_3D('',#179069,#113882,#113883);
#99659=AXIS2_PLACEMENT_3D('',#179071,#113885,#113886);
#99660=AXIS2_PLACEMENT_3D('',#179075,#113888,#113889);
#99661=AXIS2_PLACEMENT_3D('',#179077,#113891,#113892);
#99662=AXIS2_PLACEMENT_3D('',#179080,#113893,#113894);
#99663=AXIS2_PLACEMENT_3D('',#179084,#113896,#113897);
#99664=AXIS2_PLACEMENT_3D('',#179086,#113899,#113900);
#99665=AXIS2_PLACEMENT_3D('',#179089,#113901,#113902);
#99666=AXIS2_PLACEMENT_3D('',#179093,#113904,#113905);
#99667=AXIS2_PLACEMENT_3D('',#179095,#113906,#113907);
#99668=AXIS2_PLACEMENT_3D('',#179097,#113908,#113909);
#99669=AXIS2_PLACEMENT_3D('',#179099,#113911,#113912);
#99670=AXIS2_PLACEMENT_3D('',#179103,#113914,#113915);
#99671=AXIS2_PLACEMENT_3D('',#179105,#113917,#113918);
#99672=AXIS2_PLACEMENT_3D('',#179106,#113919,#113920);
#99673=AXIS2_PLACEMENT_3D('',#179107,#113921,#113922);
#99674=AXIS2_PLACEMENT_3D('',#179108,#113923,#113924);
#99675=AXIS2_PLACEMENT_3D('',#179109,#113925,#113926);
#99676=AXIS2_PLACEMENT_3D('',#179110,#113927,#113928);
#99677=AXIS2_PLACEMENT_3D('',#179111,#113929,#113930);
#99678=AXIS2_PLACEMENT_3D('',#179112,#113931,#113932);
#99679=AXIS2_PLACEMENT_3D('',#179113,#113933,#113934);
#99680=AXIS2_PLACEMENT_3D('',#179114,#113935,#113936);
#99681=AXIS2_PLACEMENT_3D('',#179115,#113937,#113938);
#99682=AXIS2_PLACEMENT_3D('',#179116,#113939,#113940);
#99683=AXIS2_PLACEMENT_3D('',#179117,#113941,#113942);
#99684=AXIS2_PLACEMENT_3D('',#179120,#113943,#113944);
#99685=AXIS2_PLACEMENT_3D('',#179124,#113946,#113947);
#99686=AXIS2_PLACEMENT_3D('',#179126,#113948,#113949);
#99687=AXIS2_PLACEMENT_3D('',#179128,#113950,#113951);
#99688=AXIS2_PLACEMENT_3D('',#179130,#113953,#113954);
#99689=AXIS2_PLACEMENT_3D('',#179134,#113956,#113957);
#99690=AXIS2_PLACEMENT_3D('',#179136,#113959,#113960);
#99691=AXIS2_PLACEMENT_3D('',#179139,#113961,#113962);
#99692=AXIS2_PLACEMENT_3D('',#179143,#113964,#113965);
#99693=AXIS2_PLACEMENT_3D('',#179145,#113967,#113968);
#99694=AXIS2_PLACEMENT_3D('',#179148,#113969,#113970);
#99695=AXIS2_PLACEMENT_3D('',#179152,#113972,#113973);
#99696=AXIS2_PLACEMENT_3D('',#179154,#113974,#113975);
#99697=AXIS2_PLACEMENT_3D('',#179156,#113976,#113977);
#99698=AXIS2_PLACEMENT_3D('',#179158,#113979,#113980);
#99699=AXIS2_PLACEMENT_3D('',#179162,#113982,#113983);
#99700=AXIS2_PLACEMENT_3D('',#179164,#113985,#113986);
#99701=AXIS2_PLACEMENT_3D('',#179165,#113987,#113988);
#99702=AXIS2_PLACEMENT_3D('',#179166,#113989,#113990);
#99703=AXIS2_PLACEMENT_3D('',#179167,#113991,#113992);
#99704=AXIS2_PLACEMENT_3D('',#179168,#113993,#113994);
#99705=AXIS2_PLACEMENT_3D('',#179169,#113995,#113996);
#99706=AXIS2_PLACEMENT_3D('',#179170,#113997,#113998);
#99707=AXIS2_PLACEMENT_3D('',#179171,#113999,#114000);
#99708=AXIS2_PLACEMENT_3D('',#179172,#114001,#114002);
#99709=AXIS2_PLACEMENT_3D('',#179173,#114003,#114004);
#99710=AXIS2_PLACEMENT_3D('',#179174,#114005,#114006);
#99711=AXIS2_PLACEMENT_3D('',#179175,#114007,#114008);
#99712=AXIS2_PLACEMENT_3D('',#179176,#114009,#114010);
#99713=AXIS2_PLACEMENT_3D('',#179179,#114011,#114012);
#99714=AXIS2_PLACEMENT_3D('',#179183,#114014,#114015);
#99715=AXIS2_PLACEMENT_3D('',#179185,#114016,#114017);
#99716=AXIS2_PLACEMENT_3D('',#179187,#114018,#114019);
#99717=AXIS2_PLACEMENT_3D('',#179189,#114021,#114022);
#99718=AXIS2_PLACEMENT_3D('',#179193,#114024,#114025);
#99719=AXIS2_PLACEMENT_3D('',#179195,#114027,#114028);
#99720=AXIS2_PLACEMENT_3D('',#179198,#114029,#114030);
#99721=AXIS2_PLACEMENT_3D('',#179202,#114032,#114033);
#99722=AXIS2_PLACEMENT_3D('',#179204,#114035,#114036);
#99723=AXIS2_PLACEMENT_3D('',#179207,#114037,#114038);
#99724=AXIS2_PLACEMENT_3D('',#179211,#114040,#114041);
#99725=AXIS2_PLACEMENT_3D('',#179213,#114042,#114043);
#99726=AXIS2_PLACEMENT_3D('',#179215,#114044,#114045);
#99727=AXIS2_PLACEMENT_3D('',#179217,#114047,#114048);
#99728=AXIS2_PLACEMENT_3D('',#179221,#114050,#114051);
#99729=AXIS2_PLACEMENT_3D('',#179223,#114053,#114054);
#99730=AXIS2_PLACEMENT_3D('',#179224,#114055,#114056);
#99731=AXIS2_PLACEMENT_3D('',#179225,#114057,#114058);
#99732=AXIS2_PLACEMENT_3D('',#179226,#114059,#114060);
#99733=AXIS2_PLACEMENT_3D('',#179227,#114061,#114062);
#99734=AXIS2_PLACEMENT_3D('',#179228,#114063,#114064);
#99735=AXIS2_PLACEMENT_3D('',#179229,#114065,#114066);
#99736=AXIS2_PLACEMENT_3D('',#179230,#114067,#114068);
#99737=AXIS2_PLACEMENT_3D('',#179231,#114069,#114070);
#99738=AXIS2_PLACEMENT_3D('',#179232,#114071,#114072);
#99739=AXIS2_PLACEMENT_3D('',#179233,#114073,#114074);
#99740=AXIS2_PLACEMENT_3D('',#179234,#114075,#114076);
#99741=AXIS2_PLACEMENT_3D('',#179235,#114077,#114078);
#99742=AXIS2_PLACEMENT_3D('',#179238,#114079,#114080);
#99743=AXIS2_PLACEMENT_3D('',#179242,#114082,#114083);
#99744=AXIS2_PLACEMENT_3D('',#179244,#114084,#114085);
#99745=AXIS2_PLACEMENT_3D('',#179246,#114086,#114087);
#99746=AXIS2_PLACEMENT_3D('',#179248,#114089,#114090);
#99747=AXIS2_PLACEMENT_3D('',#179252,#114092,#114093);
#99748=AXIS2_PLACEMENT_3D('',#179254,#114095,#114096);
#99749=AXIS2_PLACEMENT_3D('',#179257,#114097,#114098);
#99750=AXIS2_PLACEMENT_3D('',#179261,#114100,#114101);
#99751=AXIS2_PLACEMENT_3D('',#179263,#114103,#114104);
#99752=AXIS2_PLACEMENT_3D('',#179266,#114105,#114106);
#99753=AXIS2_PLACEMENT_3D('',#179270,#114108,#114109);
#99754=AXIS2_PLACEMENT_3D('',#179272,#114110,#114111);
#99755=AXIS2_PLACEMENT_3D('',#179274,#114112,#114113);
#99756=AXIS2_PLACEMENT_3D('',#179276,#114115,#114116);
#99757=AXIS2_PLACEMENT_3D('',#179280,#114118,#114119);
#99758=AXIS2_PLACEMENT_3D('',#179282,#114121,#114122);
#99759=AXIS2_PLACEMENT_3D('',#179283,#114123,#114124);
#99760=AXIS2_PLACEMENT_3D('',#179284,#114125,#114126);
#99761=AXIS2_PLACEMENT_3D('',#179285,#114127,#114128);
#99762=AXIS2_PLACEMENT_3D('',#179286,#114129,#114130);
#99763=AXIS2_PLACEMENT_3D('',#179287,#114131,#114132);
#99764=AXIS2_PLACEMENT_3D('',#179288,#114133,#114134);
#99765=AXIS2_PLACEMENT_3D('',#179289,#114135,#114136);
#99766=AXIS2_PLACEMENT_3D('',#179290,#114137,#114138);
#99767=AXIS2_PLACEMENT_3D('',#179291,#114139,#114140);
#99768=AXIS2_PLACEMENT_3D('',#179292,#114141,#114142);
#99769=AXIS2_PLACEMENT_3D('',#179293,#114143,#114144);
#99770=AXIS2_PLACEMENT_3D('',#179294,#114145,#114146);
#99771=AXIS2_PLACEMENT_3D('',#179297,#114147,#114148);
#99772=AXIS2_PLACEMENT_3D('',#179301,#114150,#114151);
#99773=AXIS2_PLACEMENT_3D('',#179303,#114152,#114153);
#99774=AXIS2_PLACEMENT_3D('',#179305,#114154,#114155);
#99775=AXIS2_PLACEMENT_3D('',#179307,#114157,#114158);
#99776=AXIS2_PLACEMENT_3D('',#179311,#114160,#114161);
#99777=AXIS2_PLACEMENT_3D('',#179313,#114163,#114164);
#99778=AXIS2_PLACEMENT_3D('',#179316,#114165,#114166);
#99779=AXIS2_PLACEMENT_3D('',#179320,#114168,#114169);
#99780=AXIS2_PLACEMENT_3D('',#179322,#114171,#114172);
#99781=AXIS2_PLACEMENT_3D('',#179325,#114173,#114174);
#99782=AXIS2_PLACEMENT_3D('',#179329,#114176,#114177);
#99783=AXIS2_PLACEMENT_3D('',#179331,#114178,#114179);
#99784=AXIS2_PLACEMENT_3D('',#179333,#114180,#114181);
#99785=AXIS2_PLACEMENT_3D('',#179335,#114183,#114184);
#99786=AXIS2_PLACEMENT_3D('',#179339,#114186,#114187);
#99787=AXIS2_PLACEMENT_3D('',#179341,#114189,#114190);
#99788=AXIS2_PLACEMENT_3D('',#179342,#114191,#114192);
#99789=AXIS2_PLACEMENT_3D('',#179343,#114193,#114194);
#99790=AXIS2_PLACEMENT_3D('',#179344,#114195,#114196);
#99791=AXIS2_PLACEMENT_3D('',#179345,#114197,#114198);
#99792=AXIS2_PLACEMENT_3D('',#179346,#114199,#114200);
#99793=AXIS2_PLACEMENT_3D('',#179347,#114201,#114202);
#99794=AXIS2_PLACEMENT_3D('',#179348,#114203,#114204);
#99795=AXIS2_PLACEMENT_3D('',#179349,#114205,#114206);
#99796=AXIS2_PLACEMENT_3D('',#179350,#114207,#114208);
#99797=AXIS2_PLACEMENT_3D('',#179351,#114209,#114210);
#99798=AXIS2_PLACEMENT_3D('',#179352,#114211,#114212);
#99799=AXIS2_PLACEMENT_3D('',#179353,#114213,#114214);
#99800=AXIS2_PLACEMENT_3D('',#179356,#114215,#114216);
#99801=AXIS2_PLACEMENT_3D('',#179360,#114218,#114219);
#99802=AXIS2_PLACEMENT_3D('',#179362,#114220,#114221);
#99803=AXIS2_PLACEMENT_3D('',#179364,#114222,#114223);
#99804=AXIS2_PLACEMENT_3D('',#179366,#114225,#114226);
#99805=AXIS2_PLACEMENT_3D('',#179370,#114228,#114229);
#99806=AXIS2_PLACEMENT_3D('',#179372,#114231,#114232);
#99807=AXIS2_PLACEMENT_3D('',#179375,#114233,#114234);
#99808=AXIS2_PLACEMENT_3D('',#179379,#114236,#114237);
#99809=AXIS2_PLACEMENT_3D('',#179381,#114239,#114240);
#99810=AXIS2_PLACEMENT_3D('',#179384,#114241,#114242);
#99811=AXIS2_PLACEMENT_3D('',#179388,#114244,#114245);
#99812=AXIS2_PLACEMENT_3D('',#179390,#114246,#114247);
#99813=AXIS2_PLACEMENT_3D('',#179392,#114248,#114249);
#99814=AXIS2_PLACEMENT_3D('',#179394,#114251,#114252);
#99815=AXIS2_PLACEMENT_3D('',#179398,#114254,#114255);
#99816=AXIS2_PLACEMENT_3D('',#179400,#114257,#114258);
#99817=AXIS2_PLACEMENT_3D('',#179401,#114259,#114260);
#99818=AXIS2_PLACEMENT_3D('',#179402,#114261,#114262);
#99819=AXIS2_PLACEMENT_3D('',#179403,#114263,#114264);
#99820=AXIS2_PLACEMENT_3D('',#179404,#114265,#114266);
#99821=AXIS2_PLACEMENT_3D('',#179405,#114267,#114268);
#99822=AXIS2_PLACEMENT_3D('',#179406,#114269,#114270);
#99823=AXIS2_PLACEMENT_3D('',#179407,#114271,#114272);
#99824=AXIS2_PLACEMENT_3D('',#179408,#114273,#114274);
#99825=AXIS2_PLACEMENT_3D('',#179409,#114275,#114276);
#99826=AXIS2_PLACEMENT_3D('',#179410,#114277,#114278);
#99827=AXIS2_PLACEMENT_3D('',#179411,#114279,#114280);
#99828=AXIS2_PLACEMENT_3D('',#179412,#114281,#114282);
#99829=AXIS2_PLACEMENT_3D('',#179415,#114283,#114284);
#99830=AXIS2_PLACEMENT_3D('',#179419,#114286,#114287);
#99831=AXIS2_PLACEMENT_3D('',#179421,#114288,#114289);
#99832=AXIS2_PLACEMENT_3D('',#179423,#114290,#114291);
#99833=AXIS2_PLACEMENT_3D('',#179425,#114293,#114294);
#99834=AXIS2_PLACEMENT_3D('',#179429,#114296,#114297);
#99835=AXIS2_PLACEMENT_3D('',#179431,#114299,#114300);
#99836=AXIS2_PLACEMENT_3D('',#179434,#114301,#114302);
#99837=AXIS2_PLACEMENT_3D('',#179438,#114304,#114305);
#99838=AXIS2_PLACEMENT_3D('',#179440,#114307,#114308);
#99839=AXIS2_PLACEMENT_3D('',#179443,#114309,#114310);
#99840=AXIS2_PLACEMENT_3D('',#179447,#114312,#114313);
#99841=AXIS2_PLACEMENT_3D('',#179449,#114314,#114315);
#99842=AXIS2_PLACEMENT_3D('',#179451,#114316,#114317);
#99843=AXIS2_PLACEMENT_3D('',#179453,#114319,#114320);
#99844=AXIS2_PLACEMENT_3D('',#179457,#114322,#114323);
#99845=AXIS2_PLACEMENT_3D('',#179459,#114325,#114326);
#99846=AXIS2_PLACEMENT_3D('',#179460,#114327,#114328);
#99847=AXIS2_PLACEMENT_3D('',#179461,#114329,#114330);
#99848=AXIS2_PLACEMENT_3D('',#179462,#114331,#114332);
#99849=AXIS2_PLACEMENT_3D('',#179463,#114333,#114334);
#99850=AXIS2_PLACEMENT_3D('',#179464,#114335,#114336);
#99851=AXIS2_PLACEMENT_3D('',#179465,#114337,#114338);
#99852=AXIS2_PLACEMENT_3D('',#179466,#114339,#114340);
#99853=AXIS2_PLACEMENT_3D('',#179467,#114341,#114342);
#99854=AXIS2_PLACEMENT_3D('',#179468,#114343,#114344);
#99855=AXIS2_PLACEMENT_3D('',#179469,#114345,#114346);
#99856=AXIS2_PLACEMENT_3D('',#179470,#114347,#114348);
#99857=AXIS2_PLACEMENT_3D('',#179471,#114349,#114350);
#99858=AXIS2_PLACEMENT_3D('',#179474,#114351,#114352);
#99859=AXIS2_PLACEMENT_3D('',#179478,#114354,#114355);
#99860=AXIS2_PLACEMENT_3D('',#179480,#114356,#114357);
#99861=AXIS2_PLACEMENT_3D('',#179482,#114358,#114359);
#99862=AXIS2_PLACEMENT_3D('',#179484,#114361,#114362);
#99863=AXIS2_PLACEMENT_3D('',#179488,#114364,#114365);
#99864=AXIS2_PLACEMENT_3D('',#179490,#114367,#114368);
#99865=AXIS2_PLACEMENT_3D('',#179493,#114369,#114370);
#99866=AXIS2_PLACEMENT_3D('',#179497,#114372,#114373);
#99867=AXIS2_PLACEMENT_3D('',#179499,#114375,#114376);
#99868=AXIS2_PLACEMENT_3D('',#179502,#114377,#114378);
#99869=AXIS2_PLACEMENT_3D('',#179506,#114380,#114381);
#99870=AXIS2_PLACEMENT_3D('',#179508,#114382,#114383);
#99871=AXIS2_PLACEMENT_3D('',#179510,#114384,#114385);
#99872=AXIS2_PLACEMENT_3D('',#179512,#114387,#114388);
#99873=AXIS2_PLACEMENT_3D('',#179516,#114390,#114391);
#99874=AXIS2_PLACEMENT_3D('',#179518,#114393,#114394);
#99875=AXIS2_PLACEMENT_3D('',#179519,#114395,#114396);
#99876=AXIS2_PLACEMENT_3D('',#179520,#114397,#114398);
#99877=AXIS2_PLACEMENT_3D('',#179521,#114399,#114400);
#99878=AXIS2_PLACEMENT_3D('',#179522,#114401,#114402);
#99879=AXIS2_PLACEMENT_3D('',#179523,#114403,#114404);
#99880=AXIS2_PLACEMENT_3D('',#179524,#114405,#114406);
#99881=AXIS2_PLACEMENT_3D('',#179525,#114407,#114408);
#99882=AXIS2_PLACEMENT_3D('',#179526,#114409,#114410);
#99883=AXIS2_PLACEMENT_3D('',#179527,#114411,#114412);
#99884=AXIS2_PLACEMENT_3D('',#179528,#114413,#114414);
#99885=AXIS2_PLACEMENT_3D('',#179529,#114415,#114416);
#99886=AXIS2_PLACEMENT_3D('',#179530,#114417,#114418);
#99887=AXIS2_PLACEMENT_3D('',#179533,#114419,#114420);
#99888=AXIS2_PLACEMENT_3D('',#179537,#114422,#114423);
#99889=AXIS2_PLACEMENT_3D('',#179539,#114424,#114425);
#99890=AXIS2_PLACEMENT_3D('',#179541,#114426,#114427);
#99891=AXIS2_PLACEMENT_3D('',#179543,#114429,#114430);
#99892=AXIS2_PLACEMENT_3D('',#179547,#114432,#114433);
#99893=AXIS2_PLACEMENT_3D('',#179549,#114435,#114436);
#99894=AXIS2_PLACEMENT_3D('',#179552,#114437,#114438);
#99895=AXIS2_PLACEMENT_3D('',#179556,#114440,#114441);
#99896=AXIS2_PLACEMENT_3D('',#179558,#114443,#114444);
#99897=AXIS2_PLACEMENT_3D('',#179561,#114445,#114446);
#99898=AXIS2_PLACEMENT_3D('',#179565,#114448,#114449);
#99899=AXIS2_PLACEMENT_3D('',#179567,#114450,#114451);
#99900=AXIS2_PLACEMENT_3D('',#179569,#114452,#114453);
#99901=AXIS2_PLACEMENT_3D('',#179571,#114455,#114456);
#99902=AXIS2_PLACEMENT_3D('',#179575,#114458,#114459);
#99903=AXIS2_PLACEMENT_3D('',#179577,#114461,#114462);
#99904=AXIS2_PLACEMENT_3D('',#179578,#114463,#114464);
#99905=AXIS2_PLACEMENT_3D('',#179579,#114465,#114466);
#99906=AXIS2_PLACEMENT_3D('',#179580,#114467,#114468);
#99907=AXIS2_PLACEMENT_3D('',#179581,#114469,#114470);
#99908=AXIS2_PLACEMENT_3D('',#179582,#114471,#114472);
#99909=AXIS2_PLACEMENT_3D('',#179583,#114473,#114474);
#99910=AXIS2_PLACEMENT_3D('',#179584,#114475,#114476);
#99911=AXIS2_PLACEMENT_3D('',#179585,#114477,#114478);
#99912=AXIS2_PLACEMENT_3D('',#179586,#114479,#114480);
#99913=AXIS2_PLACEMENT_3D('',#179587,#114481,#114482);
#99914=AXIS2_PLACEMENT_3D('',#179588,#114483,#114484);
#99915=AXIS2_PLACEMENT_3D('',#179589,#114485,#114486);
#99916=AXIS2_PLACEMENT_3D('',#179592,#114487,#114488);
#99917=AXIS2_PLACEMENT_3D('',#179596,#114490,#114491);
#99918=AXIS2_PLACEMENT_3D('',#179598,#114492,#114493);
#99919=AXIS2_PLACEMENT_3D('',#179600,#114494,#114495);
#99920=AXIS2_PLACEMENT_3D('',#179602,#114497,#114498);
#99921=AXIS2_PLACEMENT_3D('',#179606,#114500,#114501);
#99922=AXIS2_PLACEMENT_3D('',#179608,#114503,#114504);
#99923=AXIS2_PLACEMENT_3D('',#179611,#114505,#114506);
#99924=AXIS2_PLACEMENT_3D('',#179615,#114508,#114509);
#99925=AXIS2_PLACEMENT_3D('',#179617,#114511,#114512);
#99926=AXIS2_PLACEMENT_3D('',#179620,#114513,#114514);
#99927=AXIS2_PLACEMENT_3D('',#179624,#114516,#114517);
#99928=AXIS2_PLACEMENT_3D('',#179626,#114518,#114519);
#99929=AXIS2_PLACEMENT_3D('',#179628,#114520,#114521);
#99930=AXIS2_PLACEMENT_3D('',#179630,#114523,#114524);
#99931=AXIS2_PLACEMENT_3D('',#179634,#114526,#114527);
#99932=AXIS2_PLACEMENT_3D('',#179636,#114529,#114530);
#99933=AXIS2_PLACEMENT_3D('',#179637,#114531,#114532);
#99934=AXIS2_PLACEMENT_3D('',#179638,#114533,#114534);
#99935=AXIS2_PLACEMENT_3D('',#179639,#114535,#114536);
#99936=AXIS2_PLACEMENT_3D('',#179640,#114537,#114538);
#99937=AXIS2_PLACEMENT_3D('',#179641,#114539,#114540);
#99938=AXIS2_PLACEMENT_3D('',#179642,#114541,#114542);
#99939=AXIS2_PLACEMENT_3D('',#179643,#114543,#114544);
#99940=AXIS2_PLACEMENT_3D('',#179644,#114545,#114546);
#99941=AXIS2_PLACEMENT_3D('',#179645,#114547,#114548);
#99942=AXIS2_PLACEMENT_3D('',#179646,#114549,#114550);
#99943=AXIS2_PLACEMENT_3D('',#179647,#114551,#114552);
#99944=AXIS2_PLACEMENT_3D('',#179648,#114553,#114554);
#99945=AXIS2_PLACEMENT_3D('',#179651,#114555,#114556);
#99946=AXIS2_PLACEMENT_3D('',#179655,#114558,#114559);
#99947=AXIS2_PLACEMENT_3D('',#179657,#114560,#114561);
#99948=AXIS2_PLACEMENT_3D('',#179659,#114562,#114563);
#99949=AXIS2_PLACEMENT_3D('',#179661,#114565,#114566);
#99950=AXIS2_PLACEMENT_3D('',#179665,#114568,#114569);
#99951=AXIS2_PLACEMENT_3D('',#179667,#114571,#114572);
#99952=AXIS2_PLACEMENT_3D('',#179670,#114573,#114574);
#99953=AXIS2_PLACEMENT_3D('',#179674,#114576,#114577);
#99954=AXIS2_PLACEMENT_3D('',#179676,#114579,#114580);
#99955=AXIS2_PLACEMENT_3D('',#179679,#114581,#114582);
#99956=AXIS2_PLACEMENT_3D('',#179683,#114584,#114585);
#99957=AXIS2_PLACEMENT_3D('',#179685,#114586,#114587);
#99958=AXIS2_PLACEMENT_3D('',#179687,#114588,#114589);
#99959=AXIS2_PLACEMENT_3D('',#179689,#114591,#114592);
#99960=AXIS2_PLACEMENT_3D('',#179693,#114594,#114595);
#99961=AXIS2_PLACEMENT_3D('',#179695,#114597,#114598);
#99962=AXIS2_PLACEMENT_3D('',#179696,#114599,#114600);
#99963=AXIS2_PLACEMENT_3D('',#179697,#114601,#114602);
#99964=AXIS2_PLACEMENT_3D('',#179698,#114603,#114604);
#99965=AXIS2_PLACEMENT_3D('',#179699,#114605,#114606);
#99966=AXIS2_PLACEMENT_3D('',#179700,#114607,#114608);
#99967=AXIS2_PLACEMENT_3D('',#179701,#114609,#114610);
#99968=AXIS2_PLACEMENT_3D('',#179702,#114611,#114612);
#99969=AXIS2_PLACEMENT_3D('',#179703,#114613,#114614);
#99970=AXIS2_PLACEMENT_3D('',#179704,#114615,#114616);
#99971=AXIS2_PLACEMENT_3D('',#179705,#114617,#114618);
#99972=AXIS2_PLACEMENT_3D('',#179706,#114619,#114620);
#99973=AXIS2_PLACEMENT_3D('',#179707,#114621,#114622);
#99974=AXIS2_PLACEMENT_3D('',#179710,#114623,#114624);
#99975=AXIS2_PLACEMENT_3D('',#179714,#114626,#114627);
#99976=AXIS2_PLACEMENT_3D('',#179716,#114628,#114629);
#99977=AXIS2_PLACEMENT_3D('',#179718,#114630,#114631);
#99978=AXIS2_PLACEMENT_3D('',#179720,#114633,#114634);
#99979=AXIS2_PLACEMENT_3D('',#179724,#114636,#114637);
#99980=AXIS2_PLACEMENT_3D('',#179726,#114639,#114640);
#99981=AXIS2_PLACEMENT_3D('',#179729,#114641,#114642);
#99982=AXIS2_PLACEMENT_3D('',#179733,#114644,#114645);
#99983=AXIS2_PLACEMENT_3D('',#179735,#114647,#114648);
#99984=AXIS2_PLACEMENT_3D('',#179738,#114649,#114650);
#99985=AXIS2_PLACEMENT_3D('',#179742,#114652,#114653);
#99986=AXIS2_PLACEMENT_3D('',#179744,#114654,#114655);
#99987=AXIS2_PLACEMENT_3D('',#179746,#114656,#114657);
#99988=AXIS2_PLACEMENT_3D('',#179748,#114659,#114660);
#99989=AXIS2_PLACEMENT_3D('',#179752,#114662,#114663);
#99990=AXIS2_PLACEMENT_3D('',#179754,#114665,#114666);
#99991=AXIS2_PLACEMENT_3D('',#179755,#114667,#114668);
#99992=AXIS2_PLACEMENT_3D('',#179756,#114669,#114670);
#99993=AXIS2_PLACEMENT_3D('',#179757,#114671,#114672);
#99994=AXIS2_PLACEMENT_3D('',#179758,#114673,#114674);
#99995=AXIS2_PLACEMENT_3D('',#179759,#114675,#114676);
#99996=AXIS2_PLACEMENT_3D('',#179760,#114677,#114678);
#99997=AXIS2_PLACEMENT_3D('',#179761,#114679,#114680);
#99998=AXIS2_PLACEMENT_3D('',#179762,#114681,#114682);
#99999=AXIS2_PLACEMENT_3D('',#179763,#114683,#114684);
#100000=AXIS2_PLACEMENT_3D('',#179764,#114685,#114686);
#100001=AXIS2_PLACEMENT_3D('',#179765,#114687,#114688);
#100002=AXIS2_PLACEMENT_3D('',#179766,#114689,#114690);
#100003=AXIS2_PLACEMENT_3D('',#179769,#114691,#114692);
#100004=AXIS2_PLACEMENT_3D('',#179773,#114694,#114695);
#100005=AXIS2_PLACEMENT_3D('',#179775,#114696,#114697);
#100006=AXIS2_PLACEMENT_3D('',#179777,#114698,#114699);
#100007=AXIS2_PLACEMENT_3D('',#179779,#114701,#114702);
#100008=AXIS2_PLACEMENT_3D('',#179783,#114704,#114705);
#100009=AXIS2_PLACEMENT_3D('',#179785,#114707,#114708);
#100010=AXIS2_PLACEMENT_3D('',#179788,#114709,#114710);
#100011=AXIS2_PLACEMENT_3D('',#179792,#114712,#114713);
#100012=AXIS2_PLACEMENT_3D('',#179794,#114715,#114716);
#100013=AXIS2_PLACEMENT_3D('',#179797,#114717,#114718);
#100014=AXIS2_PLACEMENT_3D('',#179801,#114720,#114721);
#100015=AXIS2_PLACEMENT_3D('',#179803,#114722,#114723);
#100016=AXIS2_PLACEMENT_3D('',#179805,#114724,#114725);
#100017=AXIS2_PLACEMENT_3D('',#179807,#114727,#114728);
#100018=AXIS2_PLACEMENT_3D('',#179811,#114730,#114731);
#100019=AXIS2_PLACEMENT_3D('',#179813,#114733,#114734);
#100020=AXIS2_PLACEMENT_3D('',#179814,#114735,#114736);
#100021=AXIS2_PLACEMENT_3D('',#179815,#114737,#114738);
#100022=AXIS2_PLACEMENT_3D('',#179816,#114739,#114740);
#100023=AXIS2_PLACEMENT_3D('',#179817,#114741,#114742);
#100024=AXIS2_PLACEMENT_3D('',#179818,#114743,#114744);
#100025=AXIS2_PLACEMENT_3D('',#179819,#114745,#114746);
#100026=AXIS2_PLACEMENT_3D('',#179820,#114747,#114748);
#100027=AXIS2_PLACEMENT_3D('',#179821,#114749,#114750);
#100028=AXIS2_PLACEMENT_3D('',#179822,#114751,#114752);
#100029=AXIS2_PLACEMENT_3D('',#179823,#114753,#114754);
#100030=AXIS2_PLACEMENT_3D('',#179824,#114755,#114756);
#100031=AXIS2_PLACEMENT_3D('',#179825,#114757,#114758);
#100032=AXIS2_PLACEMENT_3D('',#179828,#114759,#114760);
#100033=AXIS2_PLACEMENT_3D('',#179832,#114762,#114763);
#100034=AXIS2_PLACEMENT_3D('',#179834,#114764,#114765);
#100035=AXIS2_PLACEMENT_3D('',#179836,#114766,#114767);
#100036=AXIS2_PLACEMENT_3D('',#179838,#114769,#114770);
#100037=AXIS2_PLACEMENT_3D('',#179842,#114772,#114773);
#100038=AXIS2_PLACEMENT_3D('',#179844,#114775,#114776);
#100039=AXIS2_PLACEMENT_3D('',#179847,#114777,#114778);
#100040=AXIS2_PLACEMENT_3D('',#179851,#114780,#114781);
#100041=AXIS2_PLACEMENT_3D('',#179853,#114783,#114784);
#100042=AXIS2_PLACEMENT_3D('',#179856,#114785,#114786);
#100043=AXIS2_PLACEMENT_3D('',#179860,#114788,#114789);
#100044=AXIS2_PLACEMENT_3D('',#179862,#114790,#114791);
#100045=AXIS2_PLACEMENT_3D('',#179864,#114792,#114793);
#100046=AXIS2_PLACEMENT_3D('',#179866,#114795,#114796);
#100047=AXIS2_PLACEMENT_3D('',#179870,#114798,#114799);
#100048=AXIS2_PLACEMENT_3D('',#179872,#114801,#114802);
#100049=AXIS2_PLACEMENT_3D('',#179873,#114803,#114804);
#100050=AXIS2_PLACEMENT_3D('',#179874,#114805,#114806);
#100051=AXIS2_PLACEMENT_3D('',#179875,#114807,#114808);
#100052=AXIS2_PLACEMENT_3D('',#179876,#114809,#114810);
#100053=AXIS2_PLACEMENT_3D('',#179877,#114811,#114812);
#100054=AXIS2_PLACEMENT_3D('',#179878,#114813,#114814);
#100055=AXIS2_PLACEMENT_3D('',#179879,#114815,#114816);
#100056=AXIS2_PLACEMENT_3D('',#179880,#114817,#114818);
#100057=AXIS2_PLACEMENT_3D('',#179881,#114819,#114820);
#100058=AXIS2_PLACEMENT_3D('',#179882,#114821,#114822);
#100059=AXIS2_PLACEMENT_3D('',#179883,#114823,#114824);
#100060=AXIS2_PLACEMENT_3D('',#179884,#114825,#114826);
#100061=AXIS2_PLACEMENT_3D('',#179887,#114827,#114828);
#100062=AXIS2_PLACEMENT_3D('',#179891,#114830,#114831);
#100063=AXIS2_PLACEMENT_3D('',#179893,#114832,#114833);
#100064=AXIS2_PLACEMENT_3D('',#179895,#114834,#114835);
#100065=AXIS2_PLACEMENT_3D('',#179897,#114837,#114838);
#100066=AXIS2_PLACEMENT_3D('',#179901,#114840,#114841);
#100067=AXIS2_PLACEMENT_3D('',#179903,#114843,#114844);
#100068=AXIS2_PLACEMENT_3D('',#179906,#114845,#114846);
#100069=AXIS2_PLACEMENT_3D('',#179910,#114848,#114849);
#100070=AXIS2_PLACEMENT_3D('',#179912,#114851,#114852);
#100071=AXIS2_PLACEMENT_3D('',#179915,#114853,#114854);
#100072=AXIS2_PLACEMENT_3D('',#179919,#114856,#114857);
#100073=AXIS2_PLACEMENT_3D('',#179921,#114858,#114859);
#100074=AXIS2_PLACEMENT_3D('',#179923,#114860,#114861);
#100075=AXIS2_PLACEMENT_3D('',#179925,#114863,#114864);
#100076=AXIS2_PLACEMENT_3D('',#179929,#114866,#114867);
#100077=AXIS2_PLACEMENT_3D('',#179931,#114869,#114870);
#100078=AXIS2_PLACEMENT_3D('',#179932,#114871,#114872);
#100079=AXIS2_PLACEMENT_3D('',#179933,#114873,#114874);
#100080=AXIS2_PLACEMENT_3D('',#179934,#114875,#114876);
#100081=AXIS2_PLACEMENT_3D('',#179935,#114877,#114878);
#100082=AXIS2_PLACEMENT_3D('',#179936,#114879,#114880);
#100083=AXIS2_PLACEMENT_3D('',#179937,#114881,#114882);
#100084=AXIS2_PLACEMENT_3D('',#179938,#114883,#114884);
#100085=AXIS2_PLACEMENT_3D('',#179939,#114885,#114886);
#100086=AXIS2_PLACEMENT_3D('',#179940,#114887,#114888);
#100087=AXIS2_PLACEMENT_3D('',#179941,#114889,#114890);
#100088=AXIS2_PLACEMENT_3D('',#179942,#114891,#114892);
#100089=AXIS2_PLACEMENT_3D('',#179943,#114893,#114894);
#100090=AXIS2_PLACEMENT_3D('',#179946,#114895,#114896);
#100091=AXIS2_PLACEMENT_3D('',#179950,#114898,#114899);
#100092=AXIS2_PLACEMENT_3D('',#179952,#114900,#114901);
#100093=AXIS2_PLACEMENT_3D('',#179954,#114902,#114903);
#100094=AXIS2_PLACEMENT_3D('',#179956,#114905,#114906);
#100095=AXIS2_PLACEMENT_3D('',#179960,#114908,#114909);
#100096=AXIS2_PLACEMENT_3D('',#179962,#114911,#114912);
#100097=AXIS2_PLACEMENT_3D('',#179965,#114913,#114914);
#100098=AXIS2_PLACEMENT_3D('',#179969,#114916,#114917);
#100099=AXIS2_PLACEMENT_3D('',#179971,#114919,#114920);
#100100=AXIS2_PLACEMENT_3D('',#179974,#114921,#114922);
#100101=AXIS2_PLACEMENT_3D('',#179978,#114924,#114925);
#100102=AXIS2_PLACEMENT_3D('',#179980,#114926,#114927);
#100103=AXIS2_PLACEMENT_3D('',#179982,#114928,#114929);
#100104=AXIS2_PLACEMENT_3D('',#179984,#114931,#114932);
#100105=AXIS2_PLACEMENT_3D('',#179988,#114934,#114935);
#100106=AXIS2_PLACEMENT_3D('',#179990,#114937,#114938);
#100107=AXIS2_PLACEMENT_3D('',#179991,#114939,#114940);
#100108=AXIS2_PLACEMENT_3D('',#179992,#114941,#114942);
#100109=AXIS2_PLACEMENT_3D('',#179993,#114943,#114944);
#100110=AXIS2_PLACEMENT_3D('',#179994,#114945,#114946);
#100111=AXIS2_PLACEMENT_3D('',#179995,#114947,#114948);
#100112=AXIS2_PLACEMENT_3D('',#179996,#114949,#114950);
#100113=AXIS2_PLACEMENT_3D('',#179997,#114951,#114952);
#100114=AXIS2_PLACEMENT_3D('',#179998,#114953,#114954);
#100115=AXIS2_PLACEMENT_3D('',#179999,#114955,#114956);
#100116=AXIS2_PLACEMENT_3D('',#180000,#114957,#114958);
#100117=AXIS2_PLACEMENT_3D('',#180001,#114959,#114960);
#100118=AXIS2_PLACEMENT_3D('',#180002,#114961,#114962);
#100119=AXIS2_PLACEMENT_3D('',#180005,#114963,#114964);
#100120=AXIS2_PLACEMENT_3D('',#180009,#114966,#114967);
#100121=AXIS2_PLACEMENT_3D('',#180011,#114968,#114969);
#100122=AXIS2_PLACEMENT_3D('',#180013,#114970,#114971);
#100123=AXIS2_PLACEMENT_3D('',#180015,#114973,#114974);
#100124=AXIS2_PLACEMENT_3D('',#180019,#114976,#114977);
#100125=AXIS2_PLACEMENT_3D('',#180021,#114979,#114980);
#100126=AXIS2_PLACEMENT_3D('',#180024,#114981,#114982);
#100127=AXIS2_PLACEMENT_3D('',#180028,#114984,#114985);
#100128=AXIS2_PLACEMENT_3D('',#180030,#114987,#114988);
#100129=AXIS2_PLACEMENT_3D('',#180033,#114989,#114990);
#100130=AXIS2_PLACEMENT_3D('',#180037,#114992,#114993);
#100131=AXIS2_PLACEMENT_3D('',#180039,#114994,#114995);
#100132=AXIS2_PLACEMENT_3D('',#180041,#114996,#114997);
#100133=AXIS2_PLACEMENT_3D('',#180043,#114999,#115000);
#100134=AXIS2_PLACEMENT_3D('',#180047,#115002,#115003);
#100135=AXIS2_PLACEMENT_3D('',#180049,#115005,#115006);
#100136=AXIS2_PLACEMENT_3D('',#180050,#115007,#115008);
#100137=AXIS2_PLACEMENT_3D('',#180051,#115009,#115010);
#100138=AXIS2_PLACEMENT_3D('',#180052,#115011,#115012);
#100139=AXIS2_PLACEMENT_3D('',#180053,#115013,#115014);
#100140=AXIS2_PLACEMENT_3D('',#180054,#115015,#115016);
#100141=AXIS2_PLACEMENT_3D('',#180055,#115017,#115018);
#100142=AXIS2_PLACEMENT_3D('',#180056,#115019,#115020);
#100143=AXIS2_PLACEMENT_3D('',#180057,#115021,#115022);
#100144=AXIS2_PLACEMENT_3D('',#180058,#115023,#115024);
#100145=AXIS2_PLACEMENT_3D('',#180059,#115025,#115026);
#100146=AXIS2_PLACEMENT_3D('',#180060,#115027,#115028);
#100147=AXIS2_PLACEMENT_3D('',#180061,#115029,#115030);
#100148=AXIS2_PLACEMENT_3D('',#180064,#115031,#115032);
#100149=AXIS2_PLACEMENT_3D('',#180068,#115034,#115035);
#100150=AXIS2_PLACEMENT_3D('',#180070,#115036,#115037);
#100151=AXIS2_PLACEMENT_3D('',#180072,#115038,#115039);
#100152=AXIS2_PLACEMENT_3D('',#180074,#115041,#115042);
#100153=AXIS2_PLACEMENT_3D('',#180078,#115044,#115045);
#100154=AXIS2_PLACEMENT_3D('',#180080,#115047,#115048);
#100155=AXIS2_PLACEMENT_3D('',#180083,#115049,#115050);
#100156=AXIS2_PLACEMENT_3D('',#180087,#115052,#115053);
#100157=AXIS2_PLACEMENT_3D('',#180089,#115055,#115056);
#100158=AXIS2_PLACEMENT_3D('',#180092,#115057,#115058);
#100159=AXIS2_PLACEMENT_3D('',#180096,#115060,#115061);
#100160=AXIS2_PLACEMENT_3D('',#180098,#115062,#115063);
#100161=AXIS2_PLACEMENT_3D('',#180100,#115064,#115065);
#100162=AXIS2_PLACEMENT_3D('',#180102,#115067,#115068);
#100163=AXIS2_PLACEMENT_3D('',#180106,#115070,#115071);
#100164=AXIS2_PLACEMENT_3D('',#180108,#115073,#115074);
#100165=AXIS2_PLACEMENT_3D('',#180109,#115075,#115076);
#100166=AXIS2_PLACEMENT_3D('',#180110,#115077,#115078);
#100167=AXIS2_PLACEMENT_3D('',#180111,#115079,#115080);
#100168=AXIS2_PLACEMENT_3D('',#180112,#115081,#115082);
#100169=AXIS2_PLACEMENT_3D('',#180113,#115083,#115084);
#100170=AXIS2_PLACEMENT_3D('',#180114,#115085,#115086);
#100171=AXIS2_PLACEMENT_3D('',#180115,#115087,#115088);
#100172=AXIS2_PLACEMENT_3D('',#180116,#115089,#115090);
#100173=AXIS2_PLACEMENT_3D('',#180117,#115091,#115092);
#100174=AXIS2_PLACEMENT_3D('',#180118,#115093,#115094);
#100175=AXIS2_PLACEMENT_3D('',#180119,#115095,#115096);
#100176=AXIS2_PLACEMENT_3D('',#180120,#115097,#115098);
#100177=AXIS2_PLACEMENT_3D('',#180123,#115099,#115100);
#100178=AXIS2_PLACEMENT_3D('',#180127,#115102,#115103);
#100179=AXIS2_PLACEMENT_3D('',#180129,#115104,#115105);
#100180=AXIS2_PLACEMENT_3D('',#180131,#115106,#115107);
#100181=AXIS2_PLACEMENT_3D('',#180133,#115109,#115110);
#100182=AXIS2_PLACEMENT_3D('',#180137,#115112,#115113);
#100183=AXIS2_PLACEMENT_3D('',#180139,#115115,#115116);
#100184=AXIS2_PLACEMENT_3D('',#180142,#115117,#115118);
#100185=AXIS2_PLACEMENT_3D('',#180146,#115120,#115121);
#100186=AXIS2_PLACEMENT_3D('',#180148,#115123,#115124);
#100187=AXIS2_PLACEMENT_3D('',#180151,#115125,#115126);
#100188=AXIS2_PLACEMENT_3D('',#180155,#115128,#115129);
#100189=AXIS2_PLACEMENT_3D('',#180157,#115130,#115131);
#100190=AXIS2_PLACEMENT_3D('',#180159,#115132,#115133);
#100191=AXIS2_PLACEMENT_3D('',#180161,#115135,#115136);
#100192=AXIS2_PLACEMENT_3D('',#180165,#115138,#115139);
#100193=AXIS2_PLACEMENT_3D('',#180167,#115141,#115142);
#100194=AXIS2_PLACEMENT_3D('',#180168,#115143,#115144);
#100195=AXIS2_PLACEMENT_3D('',#180169,#115145,#115146);
#100196=AXIS2_PLACEMENT_3D('',#180170,#115147,#115148);
#100197=AXIS2_PLACEMENT_3D('',#180171,#115149,#115150);
#100198=AXIS2_PLACEMENT_3D('',#180172,#115151,#115152);
#100199=AXIS2_PLACEMENT_3D('',#180173,#115153,#115154);
#100200=AXIS2_PLACEMENT_3D('',#180174,#115155,#115156);
#100201=AXIS2_PLACEMENT_3D('',#180175,#115157,#115158);
#100202=AXIS2_PLACEMENT_3D('',#180176,#115159,#115160);
#100203=AXIS2_PLACEMENT_3D('',#180177,#115161,#115162);
#100204=AXIS2_PLACEMENT_3D('',#180178,#115163,#115164);
#100205=AXIS2_PLACEMENT_3D('',#180179,#115165,#115166);
#100206=AXIS2_PLACEMENT_3D('',#180182,#115167,#115168);
#100207=AXIS2_PLACEMENT_3D('',#180186,#115170,#115171);
#100208=AXIS2_PLACEMENT_3D('',#180188,#115172,#115173);
#100209=AXIS2_PLACEMENT_3D('',#180190,#115174,#115175);
#100210=AXIS2_PLACEMENT_3D('',#180192,#115177,#115178);
#100211=AXIS2_PLACEMENT_3D('',#180196,#115180,#115181);
#100212=AXIS2_PLACEMENT_3D('',#180198,#115183,#115184);
#100213=AXIS2_PLACEMENT_3D('',#180201,#115185,#115186);
#100214=AXIS2_PLACEMENT_3D('',#180205,#115188,#115189);
#100215=AXIS2_PLACEMENT_3D('',#180207,#115191,#115192);
#100216=AXIS2_PLACEMENT_3D('',#180210,#115193,#115194);
#100217=AXIS2_PLACEMENT_3D('',#180214,#115196,#115197);
#100218=AXIS2_PLACEMENT_3D('',#180216,#115198,#115199);
#100219=AXIS2_PLACEMENT_3D('',#180218,#115200,#115201);
#100220=AXIS2_PLACEMENT_3D('',#180220,#115203,#115204);
#100221=AXIS2_PLACEMENT_3D('',#180224,#115206,#115207);
#100222=AXIS2_PLACEMENT_3D('',#180226,#115209,#115210);
#100223=AXIS2_PLACEMENT_3D('',#180227,#115211,#115212);
#100224=AXIS2_PLACEMENT_3D('',#180228,#115213,#115214);
#100225=AXIS2_PLACEMENT_3D('',#180229,#115215,#115216);
#100226=AXIS2_PLACEMENT_3D('',#180230,#115217,#115218);
#100227=AXIS2_PLACEMENT_3D('',#180231,#115219,#115220);
#100228=AXIS2_PLACEMENT_3D('',#180232,#115221,#115222);
#100229=AXIS2_PLACEMENT_3D('',#180233,#115223,#115224);
#100230=AXIS2_PLACEMENT_3D('',#180234,#115225,#115226);
#100231=AXIS2_PLACEMENT_3D('',#180235,#115227,#115228);
#100232=AXIS2_PLACEMENT_3D('',#180236,#115229,#115230);
#100233=AXIS2_PLACEMENT_3D('',#180237,#115231,#115232);
#100234=AXIS2_PLACEMENT_3D('',#180238,#115233,#115234);
#100235=AXIS2_PLACEMENT_3D('',#180241,#115235,#115236);
#100236=AXIS2_PLACEMENT_3D('',#180245,#115238,#115239);
#100237=AXIS2_PLACEMENT_3D('',#180247,#115240,#115241);
#100238=AXIS2_PLACEMENT_3D('',#180249,#115242,#115243);
#100239=AXIS2_PLACEMENT_3D('',#180251,#115245,#115246);
#100240=AXIS2_PLACEMENT_3D('',#180255,#115248,#115249);
#100241=AXIS2_PLACEMENT_3D('',#180257,#115251,#115252);
#100242=AXIS2_PLACEMENT_3D('',#180260,#115253,#115254);
#100243=AXIS2_PLACEMENT_3D('',#180264,#115256,#115257);
#100244=AXIS2_PLACEMENT_3D('',#180266,#115259,#115260);
#100245=AXIS2_PLACEMENT_3D('',#180269,#115261,#115262);
#100246=AXIS2_PLACEMENT_3D('',#180273,#115264,#115265);
#100247=AXIS2_PLACEMENT_3D('',#180275,#115266,#115267);
#100248=AXIS2_PLACEMENT_3D('',#180277,#115268,#115269);
#100249=AXIS2_PLACEMENT_3D('',#180279,#115271,#115272);
#100250=AXIS2_PLACEMENT_3D('',#180283,#115274,#115275);
#100251=AXIS2_PLACEMENT_3D('',#180285,#115277,#115278);
#100252=AXIS2_PLACEMENT_3D('',#180286,#115279,#115280);
#100253=AXIS2_PLACEMENT_3D('',#180287,#115281,#115282);
#100254=AXIS2_PLACEMENT_3D('',#180288,#115283,#115284);
#100255=AXIS2_PLACEMENT_3D('',#180289,#115285,#115286);
#100256=AXIS2_PLACEMENT_3D('',#180290,#115287,#115288);
#100257=AXIS2_PLACEMENT_3D('',#180291,#115289,#115290);
#100258=AXIS2_PLACEMENT_3D('',#180292,#115291,#115292);
#100259=AXIS2_PLACEMENT_3D('',#180293,#115293,#115294);
#100260=AXIS2_PLACEMENT_3D('',#180294,#115295,#115296);
#100261=AXIS2_PLACEMENT_3D('',#180295,#115297,#115298);
#100262=AXIS2_PLACEMENT_3D('',#180296,#115299,#115300);
#100263=AXIS2_PLACEMENT_3D('',#180297,#115301,#115302);
#100264=AXIS2_PLACEMENT_3D('',#180300,#115303,#115304);
#100265=AXIS2_PLACEMENT_3D('',#180304,#115306,#115307);
#100266=AXIS2_PLACEMENT_3D('',#180306,#115308,#115309);
#100267=AXIS2_PLACEMENT_3D('',#180308,#115310,#115311);
#100268=AXIS2_PLACEMENT_3D('',#180310,#115313,#115314);
#100269=AXIS2_PLACEMENT_3D('',#180314,#115316,#115317);
#100270=AXIS2_PLACEMENT_3D('',#180316,#115319,#115320);
#100271=AXIS2_PLACEMENT_3D('',#180319,#115321,#115322);
#100272=AXIS2_PLACEMENT_3D('',#180323,#115324,#115325);
#100273=AXIS2_PLACEMENT_3D('',#180325,#115327,#115328);
#100274=AXIS2_PLACEMENT_3D('',#180328,#115329,#115330);
#100275=AXIS2_PLACEMENT_3D('',#180332,#115332,#115333);
#100276=AXIS2_PLACEMENT_3D('',#180334,#115334,#115335);
#100277=AXIS2_PLACEMENT_3D('',#180336,#115336,#115337);
#100278=AXIS2_PLACEMENT_3D('',#180338,#115339,#115340);
#100279=AXIS2_PLACEMENT_3D('',#180342,#115342,#115343);
#100280=AXIS2_PLACEMENT_3D('',#180344,#115345,#115346);
#100281=AXIS2_PLACEMENT_3D('',#180345,#115347,#115348);
#100282=AXIS2_PLACEMENT_3D('',#180346,#115349,#115350);
#100283=AXIS2_PLACEMENT_3D('',#180347,#115351,#115352);
#100284=AXIS2_PLACEMENT_3D('',#180348,#115353,#115354);
#100285=AXIS2_PLACEMENT_3D('',#180349,#115355,#115356);
#100286=AXIS2_PLACEMENT_3D('',#180350,#115357,#115358);
#100287=AXIS2_PLACEMENT_3D('',#180351,#115359,#115360);
#100288=AXIS2_PLACEMENT_3D('',#180352,#115361,#115362);
#100289=AXIS2_PLACEMENT_3D('',#180353,#115363,#115364);
#100290=AXIS2_PLACEMENT_3D('',#180354,#115365,#115366);
#100291=AXIS2_PLACEMENT_3D('',#180355,#115367,#115368);
#100292=AXIS2_PLACEMENT_3D('',#180356,#115369,#115370);
#100293=AXIS2_PLACEMENT_3D('',#180359,#115371,#115372);
#100294=AXIS2_PLACEMENT_3D('',#180363,#115374,#115375);
#100295=AXIS2_PLACEMENT_3D('',#180365,#115376,#115377);
#100296=AXIS2_PLACEMENT_3D('',#180367,#115378,#115379);
#100297=AXIS2_PLACEMENT_3D('',#180369,#115381,#115382);
#100298=AXIS2_PLACEMENT_3D('',#180373,#115384,#115385);
#100299=AXIS2_PLACEMENT_3D('',#180375,#115387,#115388);
#100300=AXIS2_PLACEMENT_3D('',#180378,#115389,#115390);
#100301=AXIS2_PLACEMENT_3D('',#180382,#115392,#115393);
#100302=AXIS2_PLACEMENT_3D('',#180384,#115395,#115396);
#100303=AXIS2_PLACEMENT_3D('',#180387,#115397,#115398);
#100304=AXIS2_PLACEMENT_3D('',#180391,#115400,#115401);
#100305=AXIS2_PLACEMENT_3D('',#180393,#115402,#115403);
#100306=AXIS2_PLACEMENT_3D('',#180395,#115404,#115405);
#100307=AXIS2_PLACEMENT_3D('',#180397,#115407,#115408);
#100308=AXIS2_PLACEMENT_3D('',#180401,#115410,#115411);
#100309=AXIS2_PLACEMENT_3D('',#180403,#115413,#115414);
#100310=AXIS2_PLACEMENT_3D('',#180404,#115415,#115416);
#100311=AXIS2_PLACEMENT_3D('',#180405,#115417,#115418);
#100312=AXIS2_PLACEMENT_3D('',#180406,#115419,#115420);
#100313=AXIS2_PLACEMENT_3D('',#180407,#115421,#115422);
#100314=AXIS2_PLACEMENT_3D('',#180408,#115423,#115424);
#100315=AXIS2_PLACEMENT_3D('',#180409,#115425,#115426);
#100316=AXIS2_PLACEMENT_3D('',#180410,#115427,#115428);
#100317=AXIS2_PLACEMENT_3D('',#180411,#115429,#115430);
#100318=AXIS2_PLACEMENT_3D('',#180412,#115431,#115432);
#100319=AXIS2_PLACEMENT_3D('',#180413,#115433,#115434);
#100320=AXIS2_PLACEMENT_3D('',#180414,#115435,#115436);
#100321=AXIS2_PLACEMENT_3D('',#180415,#115437,#115438);
#100322=AXIS2_PLACEMENT_3D('',#180418,#115439,#115440);
#100323=AXIS2_PLACEMENT_3D('',#180422,#115442,#115443);
#100324=AXIS2_PLACEMENT_3D('',#180424,#115444,#115445);
#100325=AXIS2_PLACEMENT_3D('',#180426,#115446,#115447);
#100326=AXIS2_PLACEMENT_3D('',#180428,#115449,#115450);
#100327=AXIS2_PLACEMENT_3D('',#180432,#115452,#115453);
#100328=AXIS2_PLACEMENT_3D('',#180434,#115455,#115456);
#100329=AXIS2_PLACEMENT_3D('',#180437,#115457,#115458);
#100330=AXIS2_PLACEMENT_3D('',#180441,#115460,#115461);
#100331=AXIS2_PLACEMENT_3D('',#180443,#115463,#115464);
#100332=AXIS2_PLACEMENT_3D('',#180446,#115465,#115466);
#100333=AXIS2_PLACEMENT_3D('',#180450,#115468,#115469);
#100334=AXIS2_PLACEMENT_3D('',#180452,#115470,#115471);
#100335=AXIS2_PLACEMENT_3D('',#180454,#115472,#115473);
#100336=AXIS2_PLACEMENT_3D('',#180456,#115475,#115476);
#100337=AXIS2_PLACEMENT_3D('',#180460,#115478,#115479);
#100338=AXIS2_PLACEMENT_3D('',#180462,#115481,#115482);
#100339=AXIS2_PLACEMENT_3D('',#180463,#115483,#115484);
#100340=AXIS2_PLACEMENT_3D('',#180464,#115485,#115486);
#100341=AXIS2_PLACEMENT_3D('',#180465,#115487,#115488);
#100342=AXIS2_PLACEMENT_3D('',#180466,#115489,#115490);
#100343=AXIS2_PLACEMENT_3D('',#180467,#115491,#115492);
#100344=AXIS2_PLACEMENT_3D('',#180468,#115493,#115494);
#100345=AXIS2_PLACEMENT_3D('',#180469,#115495,#115496);
#100346=AXIS2_PLACEMENT_3D('',#180470,#115497,#115498);
#100347=AXIS2_PLACEMENT_3D('',#180471,#115499,#115500);
#100348=AXIS2_PLACEMENT_3D('',#180472,#115501,#115502);
#100349=AXIS2_PLACEMENT_3D('',#180473,#115503,#115504);
#100350=AXIS2_PLACEMENT_3D('',#180474,#115505,#115506);
#100351=AXIS2_PLACEMENT_3D('',#180477,#115507,#115508);
#100352=AXIS2_PLACEMENT_3D('',#180481,#115510,#115511);
#100353=AXIS2_PLACEMENT_3D('',#180483,#115512,#115513);
#100354=AXIS2_PLACEMENT_3D('',#180485,#115514,#115515);
#100355=AXIS2_PLACEMENT_3D('',#180487,#115517,#115518);
#100356=AXIS2_PLACEMENT_3D('',#180491,#115520,#115521);
#100357=AXIS2_PLACEMENT_3D('',#180493,#115523,#115524);
#100358=AXIS2_PLACEMENT_3D('',#180496,#115525,#115526);
#100359=AXIS2_PLACEMENT_3D('',#180500,#115528,#115529);
#100360=AXIS2_PLACEMENT_3D('',#180502,#115531,#115532);
#100361=AXIS2_PLACEMENT_3D('',#180505,#115533,#115534);
#100362=AXIS2_PLACEMENT_3D('',#180509,#115536,#115537);
#100363=AXIS2_PLACEMENT_3D('',#180511,#115538,#115539);
#100364=AXIS2_PLACEMENT_3D('',#180513,#115540,#115541);
#100365=AXIS2_PLACEMENT_3D('',#180515,#115543,#115544);
#100366=AXIS2_PLACEMENT_3D('',#180519,#115546,#115547);
#100367=AXIS2_PLACEMENT_3D('',#180521,#115549,#115550);
#100368=AXIS2_PLACEMENT_3D('',#180522,#115551,#115552);
#100369=AXIS2_PLACEMENT_3D('',#180523,#115553,#115554);
#100370=AXIS2_PLACEMENT_3D('',#180524,#115555,#115556);
#100371=AXIS2_PLACEMENT_3D('',#180525,#115557,#115558);
#100372=AXIS2_PLACEMENT_3D('',#180526,#115559,#115560);
#100373=AXIS2_PLACEMENT_3D('',#180527,#115561,#115562);
#100374=AXIS2_PLACEMENT_3D('',#180528,#115563,#115564);
#100375=AXIS2_PLACEMENT_3D('',#180529,#115565,#115566);
#100376=AXIS2_PLACEMENT_3D('',#180530,#115567,#115568);
#100377=AXIS2_PLACEMENT_3D('',#180531,#115569,#115570);
#100378=AXIS2_PLACEMENT_3D('',#180532,#115571,#115572);
#100379=AXIS2_PLACEMENT_3D('',#180533,#115573,#115574);
#100380=AXIS2_PLACEMENT_3D('',#180536,#115575,#115576);
#100381=AXIS2_PLACEMENT_3D('',#180540,#115578,#115579);
#100382=AXIS2_PLACEMENT_3D('',#180542,#115580,#115581);
#100383=AXIS2_PLACEMENT_3D('',#180544,#115582,#115583);
#100384=AXIS2_PLACEMENT_3D('',#180546,#115585,#115586);
#100385=AXIS2_PLACEMENT_3D('',#180550,#115588,#115589);
#100386=AXIS2_PLACEMENT_3D('',#180552,#115591,#115592);
#100387=AXIS2_PLACEMENT_3D('',#180555,#115593,#115594);
#100388=AXIS2_PLACEMENT_3D('',#180559,#115596,#115597);
#100389=AXIS2_PLACEMENT_3D('',#180561,#115599,#115600);
#100390=AXIS2_PLACEMENT_3D('',#180564,#115601,#115602);
#100391=AXIS2_PLACEMENT_3D('',#180568,#115604,#115605);
#100392=AXIS2_PLACEMENT_3D('',#180570,#115606,#115607);
#100393=AXIS2_PLACEMENT_3D('',#180572,#115608,#115609);
#100394=AXIS2_PLACEMENT_3D('',#180574,#115611,#115612);
#100395=AXIS2_PLACEMENT_3D('',#180578,#115614,#115615);
#100396=AXIS2_PLACEMENT_3D('',#180580,#115617,#115618);
#100397=AXIS2_PLACEMENT_3D('',#180581,#115619,#115620);
#100398=AXIS2_PLACEMENT_3D('',#180582,#115621,#115622);
#100399=AXIS2_PLACEMENT_3D('',#180583,#115623,#115624);
#100400=AXIS2_PLACEMENT_3D('',#180584,#115625,#115626);
#100401=AXIS2_PLACEMENT_3D('',#180585,#115627,#115628);
#100402=AXIS2_PLACEMENT_3D('',#180586,#115629,#115630);
#100403=AXIS2_PLACEMENT_3D('',#180587,#115631,#115632);
#100404=AXIS2_PLACEMENT_3D('',#180588,#115633,#115634);
#100405=AXIS2_PLACEMENT_3D('',#180589,#115635,#115636);
#100406=AXIS2_PLACEMENT_3D('',#180590,#115637,#115638);
#100407=AXIS2_PLACEMENT_3D('',#180591,#115639,#115640);
#100408=AXIS2_PLACEMENT_3D('',#180592,#115641,#115642);
#100409=AXIS2_PLACEMENT_3D('',#180595,#115643,#115644);
#100410=AXIS2_PLACEMENT_3D('',#180599,#115646,#115647);
#100411=AXIS2_PLACEMENT_3D('',#180601,#115648,#115649);
#100412=AXIS2_PLACEMENT_3D('',#180603,#115650,#115651);
#100413=AXIS2_PLACEMENT_3D('',#180605,#115653,#115654);
#100414=AXIS2_PLACEMENT_3D('',#180609,#115656,#115657);
#100415=AXIS2_PLACEMENT_3D('',#180611,#115659,#115660);
#100416=AXIS2_PLACEMENT_3D('',#180614,#115661,#115662);
#100417=AXIS2_PLACEMENT_3D('',#180618,#115664,#115665);
#100418=AXIS2_PLACEMENT_3D('',#180620,#115667,#115668);
#100419=AXIS2_PLACEMENT_3D('',#180623,#115669,#115670);
#100420=AXIS2_PLACEMENT_3D('',#180627,#115672,#115673);
#100421=AXIS2_PLACEMENT_3D('',#180629,#115674,#115675);
#100422=AXIS2_PLACEMENT_3D('',#180631,#115676,#115677);
#100423=AXIS2_PLACEMENT_3D('',#180633,#115679,#115680);
#100424=AXIS2_PLACEMENT_3D('',#180637,#115682,#115683);
#100425=AXIS2_PLACEMENT_3D('',#180639,#115685,#115686);
#100426=AXIS2_PLACEMENT_3D('',#180640,#115687,#115688);
#100427=AXIS2_PLACEMENT_3D('',#180641,#115689,#115690);
#100428=AXIS2_PLACEMENT_3D('',#180642,#115691,#115692);
#100429=AXIS2_PLACEMENT_3D('',#180643,#115693,#115694);
#100430=AXIS2_PLACEMENT_3D('',#180644,#115695,#115696);
#100431=AXIS2_PLACEMENT_3D('',#180645,#115697,#115698);
#100432=AXIS2_PLACEMENT_3D('',#180646,#115699,#115700);
#100433=AXIS2_PLACEMENT_3D('',#180647,#115701,#115702);
#100434=AXIS2_PLACEMENT_3D('',#180648,#115703,#115704);
#100435=AXIS2_PLACEMENT_3D('',#180649,#115705,#115706);
#100436=AXIS2_PLACEMENT_3D('',#180650,#115707,#115708);
#100437=AXIS2_PLACEMENT_3D('',#180651,#115709,#115710);
#100438=AXIS2_PLACEMENT_3D('',#180654,#115711,#115712);
#100439=AXIS2_PLACEMENT_3D('',#180658,#115714,#115715);
#100440=AXIS2_PLACEMENT_3D('',#180660,#115716,#115717);
#100441=AXIS2_PLACEMENT_3D('',#180662,#115718,#115719);
#100442=AXIS2_PLACEMENT_3D('',#180664,#115721,#115722);
#100443=AXIS2_PLACEMENT_3D('',#180668,#115724,#115725);
#100444=AXIS2_PLACEMENT_3D('',#180670,#115727,#115728);
#100445=AXIS2_PLACEMENT_3D('',#180673,#115729,#115730);
#100446=AXIS2_PLACEMENT_3D('',#180677,#115732,#115733);
#100447=AXIS2_PLACEMENT_3D('',#180679,#115735,#115736);
#100448=AXIS2_PLACEMENT_3D('',#180682,#115737,#115738);
#100449=AXIS2_PLACEMENT_3D('',#180686,#115740,#115741);
#100450=AXIS2_PLACEMENT_3D('',#180688,#115742,#115743);
#100451=AXIS2_PLACEMENT_3D('',#180690,#115744,#115745);
#100452=AXIS2_PLACEMENT_3D('',#180692,#115747,#115748);
#100453=AXIS2_PLACEMENT_3D('',#180696,#115750,#115751);
#100454=AXIS2_PLACEMENT_3D('',#180698,#115753,#115754);
#100455=AXIS2_PLACEMENT_3D('',#180699,#115755,#115756);
#100456=AXIS2_PLACEMENT_3D('',#180700,#115757,#115758);
#100457=AXIS2_PLACEMENT_3D('',#180701,#115759,#115760);
#100458=AXIS2_PLACEMENT_3D('',#180702,#115761,#115762);
#100459=AXIS2_PLACEMENT_3D('',#180703,#115763,#115764);
#100460=AXIS2_PLACEMENT_3D('',#180704,#115765,#115766);
#100461=AXIS2_PLACEMENT_3D('',#180705,#115767,#115768);
#100462=AXIS2_PLACEMENT_3D('',#180706,#115769,#115770);
#100463=AXIS2_PLACEMENT_3D('',#180707,#115771,#115772);
#100464=AXIS2_PLACEMENT_3D('',#180708,#115773,#115774);
#100465=AXIS2_PLACEMENT_3D('',#180709,#115775,#115776);
#100466=AXIS2_PLACEMENT_3D('',#180710,#115777,#115778);
#100467=AXIS2_PLACEMENT_3D('',#180713,#115779,#115780);
#100468=AXIS2_PLACEMENT_3D('',#180717,#115782,#115783);
#100469=AXIS2_PLACEMENT_3D('',#180719,#115784,#115785);
#100470=AXIS2_PLACEMENT_3D('',#180721,#115786,#115787);
#100471=AXIS2_PLACEMENT_3D('',#180723,#115789,#115790);
#100472=AXIS2_PLACEMENT_3D('',#180727,#115792,#115793);
#100473=AXIS2_PLACEMENT_3D('',#180729,#115795,#115796);
#100474=AXIS2_PLACEMENT_3D('',#180732,#115797,#115798);
#100475=AXIS2_PLACEMENT_3D('',#180736,#115800,#115801);
#100476=AXIS2_PLACEMENT_3D('',#180738,#115803,#115804);
#100477=AXIS2_PLACEMENT_3D('',#180741,#115805,#115806);
#100478=AXIS2_PLACEMENT_3D('',#180745,#115808,#115809);
#100479=AXIS2_PLACEMENT_3D('',#180747,#115810,#115811);
#100480=AXIS2_PLACEMENT_3D('',#180749,#115812,#115813);
#100481=AXIS2_PLACEMENT_3D('',#180751,#115815,#115816);
#100482=AXIS2_PLACEMENT_3D('',#180755,#115818,#115819);
#100483=AXIS2_PLACEMENT_3D('',#180757,#115821,#115822);
#100484=AXIS2_PLACEMENT_3D('',#180758,#115823,#115824);
#100485=AXIS2_PLACEMENT_3D('',#180759,#115825,#115826);
#100486=AXIS2_PLACEMENT_3D('',#180760,#115827,#115828);
#100487=AXIS2_PLACEMENT_3D('',#180761,#115829,#115830);
#100488=AXIS2_PLACEMENT_3D('',#180762,#115831,#115832);
#100489=AXIS2_PLACEMENT_3D('',#180763,#115833,#115834);
#100490=AXIS2_PLACEMENT_3D('',#180764,#115835,#115836);
#100491=AXIS2_PLACEMENT_3D('',#180765,#115837,#115838);
#100492=AXIS2_PLACEMENT_3D('',#180766,#115839,#115840);
#100493=AXIS2_PLACEMENT_3D('',#180767,#115841,#115842);
#100494=AXIS2_PLACEMENT_3D('',#180768,#115843,#115844);
#100495=AXIS2_PLACEMENT_3D('',#180769,#115845,#115846);
#100496=AXIS2_PLACEMENT_3D('',#180772,#115847,#115848);
#100497=AXIS2_PLACEMENT_3D('',#180776,#115850,#115851);
#100498=AXIS2_PLACEMENT_3D('',#180778,#115852,#115853);
#100499=AXIS2_PLACEMENT_3D('',#180780,#115854,#115855);
#100500=AXIS2_PLACEMENT_3D('',#180782,#115857,#115858);
#100501=AXIS2_PLACEMENT_3D('',#180786,#115860,#115861);
#100502=AXIS2_PLACEMENT_3D('',#180788,#115863,#115864);
#100503=AXIS2_PLACEMENT_3D('',#180791,#115865,#115866);
#100504=AXIS2_PLACEMENT_3D('',#180795,#115868,#115869);
#100505=AXIS2_PLACEMENT_3D('',#180797,#115871,#115872);
#100506=AXIS2_PLACEMENT_3D('',#180800,#115873,#115874);
#100507=AXIS2_PLACEMENT_3D('',#180804,#115876,#115877);
#100508=AXIS2_PLACEMENT_3D('',#180806,#115878,#115879);
#100509=AXIS2_PLACEMENT_3D('',#180808,#115880,#115881);
#100510=AXIS2_PLACEMENT_3D('',#180810,#115883,#115884);
#100511=AXIS2_PLACEMENT_3D('',#180814,#115886,#115887);
#100512=AXIS2_PLACEMENT_3D('',#180816,#115889,#115890);
#100513=AXIS2_PLACEMENT_3D('',#180817,#115891,#115892);
#100514=AXIS2_PLACEMENT_3D('',#180818,#115893,#115894);
#100515=AXIS2_PLACEMENT_3D('',#180819,#115895,#115896);
#100516=AXIS2_PLACEMENT_3D('',#180820,#115897,#115898);
#100517=AXIS2_PLACEMENT_3D('',#180821,#115899,#115900);
#100518=AXIS2_PLACEMENT_3D('',#180822,#115901,#115902);
#100519=AXIS2_PLACEMENT_3D('',#180823,#115903,#115904);
#100520=AXIS2_PLACEMENT_3D('',#180824,#115905,#115906);
#100521=AXIS2_PLACEMENT_3D('',#180825,#115907,#115908);
#100522=AXIS2_PLACEMENT_3D('',#180826,#115909,#115910);
#100523=AXIS2_PLACEMENT_3D('',#180827,#115911,#115912);
#100524=AXIS2_PLACEMENT_3D('',#180828,#115913,#115914);
#100525=AXIS2_PLACEMENT_3D('',#180831,#115915,#115916);
#100526=AXIS2_PLACEMENT_3D('',#180835,#115918,#115919);
#100527=AXIS2_PLACEMENT_3D('',#180837,#115920,#115921);
#100528=AXIS2_PLACEMENT_3D('',#180839,#115922,#115923);
#100529=AXIS2_PLACEMENT_3D('',#180841,#115925,#115926);
#100530=AXIS2_PLACEMENT_3D('',#180845,#115928,#115929);
#100531=AXIS2_PLACEMENT_3D('',#180847,#115931,#115932);
#100532=AXIS2_PLACEMENT_3D('',#180850,#115933,#115934);
#100533=AXIS2_PLACEMENT_3D('',#180854,#115936,#115937);
#100534=AXIS2_PLACEMENT_3D('',#180856,#115939,#115940);
#100535=AXIS2_PLACEMENT_3D('',#180859,#115941,#115942);
#100536=AXIS2_PLACEMENT_3D('',#180863,#115944,#115945);
#100537=AXIS2_PLACEMENT_3D('',#180865,#115946,#115947);
#100538=AXIS2_PLACEMENT_3D('',#180867,#115948,#115949);
#100539=AXIS2_PLACEMENT_3D('',#180869,#115951,#115952);
#100540=AXIS2_PLACEMENT_3D('',#180873,#115954,#115955);
#100541=AXIS2_PLACEMENT_3D('',#180875,#115957,#115958);
#100542=AXIS2_PLACEMENT_3D('',#180876,#115959,#115960);
#100543=AXIS2_PLACEMENT_3D('',#180877,#115961,#115962);
#100544=AXIS2_PLACEMENT_3D('',#180878,#115963,#115964);
#100545=AXIS2_PLACEMENT_3D('',#180879,#115965,#115966);
#100546=AXIS2_PLACEMENT_3D('',#180880,#115967,#115968);
#100547=AXIS2_PLACEMENT_3D('',#180881,#115969,#115970);
#100548=AXIS2_PLACEMENT_3D('',#180882,#115971,#115972);
#100549=AXIS2_PLACEMENT_3D('',#180883,#115973,#115974);
#100550=AXIS2_PLACEMENT_3D('',#180884,#115975,#115976);
#100551=AXIS2_PLACEMENT_3D('',#180885,#115977,#115978);
#100552=AXIS2_PLACEMENT_3D('',#180886,#115979,#115980);
#100553=AXIS2_PLACEMENT_3D('',#180887,#115981,#115982);
#100554=AXIS2_PLACEMENT_3D('',#180890,#115983,#115984);
#100555=AXIS2_PLACEMENT_3D('',#180894,#115986,#115987);
#100556=AXIS2_PLACEMENT_3D('',#180896,#115988,#115989);
#100557=AXIS2_PLACEMENT_3D('',#180898,#115990,#115991);
#100558=AXIS2_PLACEMENT_3D('',#180900,#115993,#115994);
#100559=AXIS2_PLACEMENT_3D('',#180904,#115996,#115997);
#100560=AXIS2_PLACEMENT_3D('',#180906,#115999,#116000);
#100561=AXIS2_PLACEMENT_3D('',#180909,#116001,#116002);
#100562=AXIS2_PLACEMENT_3D('',#180913,#116004,#116005);
#100563=AXIS2_PLACEMENT_3D('',#180915,#116007,#116008);
#100564=AXIS2_PLACEMENT_3D('',#180918,#116009,#116010);
#100565=AXIS2_PLACEMENT_3D('',#180922,#116012,#116013);
#100566=AXIS2_PLACEMENT_3D('',#180924,#116014,#116015);
#100567=AXIS2_PLACEMENT_3D('',#180926,#116016,#116017);
#100568=AXIS2_PLACEMENT_3D('',#180928,#116019,#116020);
#100569=AXIS2_PLACEMENT_3D('',#180932,#116022,#116023);
#100570=AXIS2_PLACEMENT_3D('',#180934,#116025,#116026);
#100571=AXIS2_PLACEMENT_3D('',#180935,#116027,#116028);
#100572=AXIS2_PLACEMENT_3D('',#180936,#116029,#116030);
#100573=AXIS2_PLACEMENT_3D('',#180937,#116031,#116032);
#100574=AXIS2_PLACEMENT_3D('',#180938,#116033,#116034);
#100575=AXIS2_PLACEMENT_3D('',#180939,#116035,#116036);
#100576=AXIS2_PLACEMENT_3D('',#180940,#116037,#116038);
#100577=AXIS2_PLACEMENT_3D('',#180941,#116039,#116040);
#100578=AXIS2_PLACEMENT_3D('',#180942,#116041,#116042);
#100579=AXIS2_PLACEMENT_3D('',#180943,#116043,#116044);
#100580=AXIS2_PLACEMENT_3D('',#180944,#116045,#116046);
#100581=AXIS2_PLACEMENT_3D('',#180945,#116047,#116048);
#100582=AXIS2_PLACEMENT_3D('',#180946,#116049,#116050);
#100583=AXIS2_PLACEMENT_3D('',#180949,#116051,#116052);
#100584=AXIS2_PLACEMENT_3D('',#180953,#116054,#116055);
#100585=AXIS2_PLACEMENT_3D('',#180955,#116056,#116057);
#100586=AXIS2_PLACEMENT_3D('',#180957,#116058,#116059);
#100587=AXIS2_PLACEMENT_3D('',#180959,#116061,#116062);
#100588=AXIS2_PLACEMENT_3D('',#180963,#116064,#116065);
#100589=AXIS2_PLACEMENT_3D('',#180965,#116067,#116068);
#100590=AXIS2_PLACEMENT_3D('',#180968,#116069,#116070);
#100591=AXIS2_PLACEMENT_3D('',#180972,#116072,#116073);
#100592=AXIS2_PLACEMENT_3D('',#180974,#116075,#116076);
#100593=AXIS2_PLACEMENT_3D('',#180977,#116077,#116078);
#100594=AXIS2_PLACEMENT_3D('',#180981,#116080,#116081);
#100595=AXIS2_PLACEMENT_3D('',#180983,#116082,#116083);
#100596=AXIS2_PLACEMENT_3D('',#180985,#116084,#116085);
#100597=AXIS2_PLACEMENT_3D('',#180987,#116087,#116088);
#100598=AXIS2_PLACEMENT_3D('',#180991,#116090,#116091);
#100599=AXIS2_PLACEMENT_3D('',#180993,#116093,#116094);
#100600=AXIS2_PLACEMENT_3D('',#180994,#116095,#116096);
#100601=AXIS2_PLACEMENT_3D('',#180995,#116097,#116098);
#100602=AXIS2_PLACEMENT_3D('',#180996,#116099,#116100);
#100603=AXIS2_PLACEMENT_3D('',#180997,#116101,#116102);
#100604=AXIS2_PLACEMENT_3D('',#180998,#116103,#116104);
#100605=AXIS2_PLACEMENT_3D('',#180999,#116105,#116106);
#100606=AXIS2_PLACEMENT_3D('',#181000,#116107,#116108);
#100607=AXIS2_PLACEMENT_3D('',#181001,#116109,#116110);
#100608=AXIS2_PLACEMENT_3D('',#181002,#116111,#116112);
#100609=AXIS2_PLACEMENT_3D('',#181003,#116113,#116114);
#100610=AXIS2_PLACEMENT_3D('',#181004,#116115,#116116);
#100611=AXIS2_PLACEMENT_3D('',#181005,#116117,#116118);
#100612=AXIS2_PLACEMENT_3D('',#181008,#116119,#116120);
#100613=AXIS2_PLACEMENT_3D('',#181012,#116122,#116123);
#100614=AXIS2_PLACEMENT_3D('',#181014,#116124,#116125);
#100615=AXIS2_PLACEMENT_3D('',#181016,#116126,#116127);
#100616=AXIS2_PLACEMENT_3D('',#181018,#116129,#116130);
#100617=AXIS2_PLACEMENT_3D('',#181022,#116132,#116133);
#100618=AXIS2_PLACEMENT_3D('',#181024,#116135,#116136);
#100619=AXIS2_PLACEMENT_3D('',#181027,#116137,#116138);
#100620=AXIS2_PLACEMENT_3D('',#181031,#116140,#116141);
#100621=AXIS2_PLACEMENT_3D('',#181033,#116143,#116144);
#100622=AXIS2_PLACEMENT_3D('',#181036,#116145,#116146);
#100623=AXIS2_PLACEMENT_3D('',#181040,#116148,#116149);
#100624=AXIS2_PLACEMENT_3D('',#181042,#116150,#116151);
#100625=AXIS2_PLACEMENT_3D('',#181044,#116152,#116153);
#100626=AXIS2_PLACEMENT_3D('',#181046,#116155,#116156);
#100627=AXIS2_PLACEMENT_3D('',#181050,#116158,#116159);
#100628=AXIS2_PLACEMENT_3D('',#181052,#116161,#116162);
#100629=AXIS2_PLACEMENT_3D('',#181053,#116163,#116164);
#100630=AXIS2_PLACEMENT_3D('',#181054,#116165,#116166);
#100631=AXIS2_PLACEMENT_3D('',#181055,#116167,#116168);
#100632=AXIS2_PLACEMENT_3D('',#181056,#116169,#116170);
#100633=AXIS2_PLACEMENT_3D('',#181057,#116171,#116172);
#100634=AXIS2_PLACEMENT_3D('',#181058,#116173,#116174);
#100635=AXIS2_PLACEMENT_3D('',#181059,#116175,#116176);
#100636=AXIS2_PLACEMENT_3D('',#181060,#116177,#116178);
#100637=AXIS2_PLACEMENT_3D('',#181061,#116179,#116180);
#100638=AXIS2_PLACEMENT_3D('',#181062,#116181,#116182);
#100639=AXIS2_PLACEMENT_3D('',#181063,#116183,#116184);
#100640=AXIS2_PLACEMENT_3D('',#181064,#116185,#116186);
#100641=AXIS2_PLACEMENT_3D('',#181067,#116187,#116188);
#100642=AXIS2_PLACEMENT_3D('',#181071,#116190,#116191);
#100643=AXIS2_PLACEMENT_3D('',#181073,#116192,#116193);
#100644=AXIS2_PLACEMENT_3D('',#181075,#116194,#116195);
#100645=AXIS2_PLACEMENT_3D('',#181077,#116197,#116198);
#100646=AXIS2_PLACEMENT_3D('',#181081,#116200,#116201);
#100647=AXIS2_PLACEMENT_3D('',#181083,#116203,#116204);
#100648=AXIS2_PLACEMENT_3D('',#181086,#116205,#116206);
#100649=AXIS2_PLACEMENT_3D('',#181090,#116208,#116209);
#100650=AXIS2_PLACEMENT_3D('',#181092,#116211,#116212);
#100651=AXIS2_PLACEMENT_3D('',#181095,#116213,#116214);
#100652=AXIS2_PLACEMENT_3D('',#181099,#116216,#116217);
#100653=AXIS2_PLACEMENT_3D('',#181101,#116218,#116219);
#100654=AXIS2_PLACEMENT_3D('',#181103,#116220,#116221);
#100655=AXIS2_PLACEMENT_3D('',#181105,#116223,#116224);
#100656=AXIS2_PLACEMENT_3D('',#181109,#116226,#116227);
#100657=AXIS2_PLACEMENT_3D('',#181111,#116229,#116230);
#100658=AXIS2_PLACEMENT_3D('',#181112,#116231,#116232);
#100659=AXIS2_PLACEMENT_3D('',#181113,#116233,#116234);
#100660=AXIS2_PLACEMENT_3D('',#181114,#116235,#116236);
#100661=AXIS2_PLACEMENT_3D('',#181115,#116237,#116238);
#100662=AXIS2_PLACEMENT_3D('',#181116,#116239,#116240);
#100663=AXIS2_PLACEMENT_3D('',#181117,#116241,#116242);
#100664=AXIS2_PLACEMENT_3D('',#181118,#116243,#116244);
#100665=AXIS2_PLACEMENT_3D('',#181119,#116245,#116246);
#100666=AXIS2_PLACEMENT_3D('',#181120,#116247,#116248);
#100667=AXIS2_PLACEMENT_3D('',#181121,#116249,#116250);
#100668=AXIS2_PLACEMENT_3D('',#181122,#116251,#116252);
#100669=AXIS2_PLACEMENT_3D('',#181123,#116253,#116254);
#100670=AXIS2_PLACEMENT_3D('',#181126,#116255,#116256);
#100671=AXIS2_PLACEMENT_3D('',#181130,#116258,#116259);
#100672=AXIS2_PLACEMENT_3D('',#181132,#116260,#116261);
#100673=AXIS2_PLACEMENT_3D('',#181134,#116262,#116263);
#100674=AXIS2_PLACEMENT_3D('',#181136,#116265,#116266);
#100675=AXIS2_PLACEMENT_3D('',#181140,#116268,#116269);
#100676=AXIS2_PLACEMENT_3D('',#181142,#116271,#116272);
#100677=AXIS2_PLACEMENT_3D('',#181145,#116273,#116274);
#100678=AXIS2_PLACEMENT_3D('',#181149,#116276,#116277);
#100679=AXIS2_PLACEMENT_3D('',#181151,#116279,#116280);
#100680=AXIS2_PLACEMENT_3D('',#181154,#116281,#116282);
#100681=AXIS2_PLACEMENT_3D('',#181158,#116284,#116285);
#100682=AXIS2_PLACEMENT_3D('',#181160,#116286,#116287);
#100683=AXIS2_PLACEMENT_3D('',#181162,#116288,#116289);
#100684=AXIS2_PLACEMENT_3D('',#181164,#116291,#116292);
#100685=AXIS2_PLACEMENT_3D('',#181168,#116294,#116295);
#100686=AXIS2_PLACEMENT_3D('',#181170,#116297,#116298);
#100687=AXIS2_PLACEMENT_3D('',#181171,#116299,#116300);
#100688=AXIS2_PLACEMENT_3D('',#181172,#116301,#116302);
#100689=AXIS2_PLACEMENT_3D('',#181173,#116303,#116304);
#100690=AXIS2_PLACEMENT_3D('',#181174,#116305,#116306);
#100691=AXIS2_PLACEMENT_3D('',#181175,#116307,#116308);
#100692=AXIS2_PLACEMENT_3D('',#181176,#116309,#116310);
#100693=AXIS2_PLACEMENT_3D('',#181177,#116311,#116312);
#100694=AXIS2_PLACEMENT_3D('',#181178,#116313,#116314);
#100695=AXIS2_PLACEMENT_3D('',#181179,#116315,#116316);
#100696=AXIS2_PLACEMENT_3D('',#181180,#116317,#116318);
#100697=AXIS2_PLACEMENT_3D('',#181181,#116319,#116320);
#100698=AXIS2_PLACEMENT_3D('',#181182,#116321,#116322);
#100699=AXIS2_PLACEMENT_3D('',#181185,#116323,#116324);
#100700=AXIS2_PLACEMENT_3D('',#181189,#116326,#116327);
#100701=AXIS2_PLACEMENT_3D('',#181191,#116328,#116329);
#100702=AXIS2_PLACEMENT_3D('',#181193,#116330,#116331);
#100703=AXIS2_PLACEMENT_3D('',#181195,#116333,#116334);
#100704=AXIS2_PLACEMENT_3D('',#181199,#116336,#116337);
#100705=AXIS2_PLACEMENT_3D('',#181201,#116339,#116340);
#100706=AXIS2_PLACEMENT_3D('',#181204,#116341,#116342);
#100707=AXIS2_PLACEMENT_3D('',#181208,#116344,#116345);
#100708=AXIS2_PLACEMENT_3D('',#181210,#116347,#116348);
#100709=AXIS2_PLACEMENT_3D('',#181213,#116349,#116350);
#100710=AXIS2_PLACEMENT_3D('',#181217,#116352,#116353);
#100711=AXIS2_PLACEMENT_3D('',#181219,#116354,#116355);
#100712=AXIS2_PLACEMENT_3D('',#181221,#116356,#116357);
#100713=AXIS2_PLACEMENT_3D('',#181223,#116359,#116360);
#100714=AXIS2_PLACEMENT_3D('',#181227,#116362,#116363);
#100715=AXIS2_PLACEMENT_3D('',#181229,#116365,#116366);
#100716=AXIS2_PLACEMENT_3D('',#181230,#116367,#116368);
#100717=AXIS2_PLACEMENT_3D('',#181231,#116369,#116370);
#100718=AXIS2_PLACEMENT_3D('',#181232,#116371,#116372);
#100719=AXIS2_PLACEMENT_3D('',#181233,#116373,#116374);
#100720=AXIS2_PLACEMENT_3D('',#181234,#116375,#116376);
#100721=AXIS2_PLACEMENT_3D('',#181235,#116377,#116378);
#100722=AXIS2_PLACEMENT_3D('',#181236,#116379,#116380);
#100723=AXIS2_PLACEMENT_3D('',#181237,#116381,#116382);
#100724=AXIS2_PLACEMENT_3D('',#181238,#116383,#116384);
#100725=AXIS2_PLACEMENT_3D('',#181239,#116385,#116386);
#100726=AXIS2_PLACEMENT_3D('',#181240,#116387,#116388);
#100727=AXIS2_PLACEMENT_3D('',#181241,#116389,#116390);
#100728=AXIS2_PLACEMENT_3D('',#181244,#116391,#116392);
#100729=AXIS2_PLACEMENT_3D('',#181248,#116394,#116395);
#100730=AXIS2_PLACEMENT_3D('',#181250,#116396,#116397);
#100731=AXIS2_PLACEMENT_3D('',#181252,#116398,#116399);
#100732=AXIS2_PLACEMENT_3D('',#181254,#116401,#116402);
#100733=AXIS2_PLACEMENT_3D('',#181258,#116404,#116405);
#100734=AXIS2_PLACEMENT_3D('',#181260,#116407,#116408);
#100735=AXIS2_PLACEMENT_3D('',#181263,#116409,#116410);
#100736=AXIS2_PLACEMENT_3D('',#181267,#116412,#116413);
#100737=AXIS2_PLACEMENT_3D('',#181269,#116415,#116416);
#100738=AXIS2_PLACEMENT_3D('',#181272,#116417,#116418);
#100739=AXIS2_PLACEMENT_3D('',#181276,#116420,#116421);
#100740=AXIS2_PLACEMENT_3D('',#181278,#116422,#116423);
#100741=AXIS2_PLACEMENT_3D('',#181280,#116424,#116425);
#100742=AXIS2_PLACEMENT_3D('',#181282,#116427,#116428);
#100743=AXIS2_PLACEMENT_3D('',#181286,#116430,#116431);
#100744=AXIS2_PLACEMENT_3D('',#181288,#116433,#116434);
#100745=AXIS2_PLACEMENT_3D('',#181289,#116435,#116436);
#100746=AXIS2_PLACEMENT_3D('',#181290,#116437,#116438);
#100747=AXIS2_PLACEMENT_3D('',#181291,#116439,#116440);
#100748=AXIS2_PLACEMENT_3D('',#181292,#116441,#116442);
#100749=AXIS2_PLACEMENT_3D('',#181293,#116443,#116444);
#100750=AXIS2_PLACEMENT_3D('',#181294,#116445,#116446);
#100751=AXIS2_PLACEMENT_3D('',#181295,#116447,#116448);
#100752=AXIS2_PLACEMENT_3D('',#181296,#116449,#116450);
#100753=AXIS2_PLACEMENT_3D('',#181297,#116451,#116452);
#100754=AXIS2_PLACEMENT_3D('',#181298,#116453,#116454);
#100755=AXIS2_PLACEMENT_3D('',#181299,#116455,#116456);
#100756=AXIS2_PLACEMENT_3D('',#181300,#116457,#116458);
#100757=AXIS2_PLACEMENT_3D('',#181303,#116459,#116460);
#100758=AXIS2_PLACEMENT_3D('',#181307,#116462,#116463);
#100759=AXIS2_PLACEMENT_3D('',#181309,#116464,#116465);
#100760=AXIS2_PLACEMENT_3D('',#181311,#116466,#116467);
#100761=AXIS2_PLACEMENT_3D('',#181313,#116469,#116470);
#100762=AXIS2_PLACEMENT_3D('',#181317,#116472,#116473);
#100763=AXIS2_PLACEMENT_3D('',#181319,#116475,#116476);
#100764=AXIS2_PLACEMENT_3D('',#181322,#116477,#116478);
#100765=AXIS2_PLACEMENT_3D('',#181326,#116480,#116481);
#100766=AXIS2_PLACEMENT_3D('',#181328,#116483,#116484);
#100767=AXIS2_PLACEMENT_3D('',#181331,#116485,#116486);
#100768=AXIS2_PLACEMENT_3D('',#181335,#116488,#116489);
#100769=AXIS2_PLACEMENT_3D('',#181337,#116490,#116491);
#100770=AXIS2_PLACEMENT_3D('',#181339,#116492,#116493);
#100771=AXIS2_PLACEMENT_3D('',#181341,#116495,#116496);
#100772=AXIS2_PLACEMENT_3D('',#181345,#116498,#116499);
#100773=AXIS2_PLACEMENT_3D('',#181347,#116501,#116502);
#100774=AXIS2_PLACEMENT_3D('',#181348,#116503,#116504);
#100775=AXIS2_PLACEMENT_3D('',#181349,#116505,#116506);
#100776=AXIS2_PLACEMENT_3D('',#181350,#116507,#116508);
#100777=AXIS2_PLACEMENT_3D('',#181351,#116509,#116510);
#100778=AXIS2_PLACEMENT_3D('',#181352,#116511,#116512);
#100779=AXIS2_PLACEMENT_3D('',#181353,#116513,#116514);
#100780=AXIS2_PLACEMENT_3D('',#181354,#116515,#116516);
#100781=AXIS2_PLACEMENT_3D('',#181355,#116517,#116518);
#100782=AXIS2_PLACEMENT_3D('',#181356,#116519,#116520);
#100783=AXIS2_PLACEMENT_3D('',#181357,#116521,#116522);
#100784=AXIS2_PLACEMENT_3D('',#181358,#116523,#116524);
#100785=AXIS2_PLACEMENT_3D('',#181359,#116525,#116526);
#100786=AXIS2_PLACEMENT_3D('',#181362,#116527,#116528);
#100787=AXIS2_PLACEMENT_3D('',#181366,#116530,#116531);
#100788=AXIS2_PLACEMENT_3D('',#181368,#116532,#116533);
#100789=AXIS2_PLACEMENT_3D('',#181370,#116534,#116535);
#100790=AXIS2_PLACEMENT_3D('',#181372,#116537,#116538);
#100791=AXIS2_PLACEMENT_3D('',#181376,#116540,#116541);
#100792=AXIS2_PLACEMENT_3D('',#181378,#116543,#116544);
#100793=AXIS2_PLACEMENT_3D('',#181381,#116545,#116546);
#100794=AXIS2_PLACEMENT_3D('',#181385,#116548,#116549);
#100795=AXIS2_PLACEMENT_3D('',#181387,#116551,#116552);
#100796=AXIS2_PLACEMENT_3D('',#181390,#116553,#116554);
#100797=AXIS2_PLACEMENT_3D('',#181394,#116556,#116557);
#100798=AXIS2_PLACEMENT_3D('',#181396,#116558,#116559);
#100799=AXIS2_PLACEMENT_3D('',#181398,#116560,#116561);
#100800=AXIS2_PLACEMENT_3D('',#181400,#116563,#116564);
#100801=AXIS2_PLACEMENT_3D('',#181404,#116566,#116567);
#100802=AXIS2_PLACEMENT_3D('',#181406,#116569,#116570);
#100803=AXIS2_PLACEMENT_3D('',#181407,#116571,#116572);
#100804=AXIS2_PLACEMENT_3D('',#181408,#116573,#116574);
#100805=AXIS2_PLACEMENT_3D('',#181409,#116575,#116576);
#100806=AXIS2_PLACEMENT_3D('',#181410,#116577,#116578);
#100807=AXIS2_PLACEMENT_3D('',#181411,#116579,#116580);
#100808=AXIS2_PLACEMENT_3D('',#181412,#116581,#116582);
#100809=AXIS2_PLACEMENT_3D('',#181413,#116583,#116584);
#100810=AXIS2_PLACEMENT_3D('',#181414,#116585,#116586);
#100811=AXIS2_PLACEMENT_3D('',#181415,#116587,#116588);
#100812=AXIS2_PLACEMENT_3D('',#181416,#116589,#116590);
#100813=AXIS2_PLACEMENT_3D('',#181417,#116591,#116592);
#100814=AXIS2_PLACEMENT_3D('',#181418,#116593,#116594);
#100815=AXIS2_PLACEMENT_3D('',#181421,#116595,#116596);
#100816=AXIS2_PLACEMENT_3D('',#181425,#116598,#116599);
#100817=AXIS2_PLACEMENT_3D('',#181427,#116600,#116601);
#100818=AXIS2_PLACEMENT_3D('',#181429,#116602,#116603);
#100819=AXIS2_PLACEMENT_3D('',#181431,#116605,#116606);
#100820=AXIS2_PLACEMENT_3D('',#181435,#116608,#116609);
#100821=AXIS2_PLACEMENT_3D('',#181437,#116611,#116612);
#100822=AXIS2_PLACEMENT_3D('',#181440,#116613,#116614);
#100823=AXIS2_PLACEMENT_3D('',#181444,#116616,#116617);
#100824=AXIS2_PLACEMENT_3D('',#181446,#116619,#116620);
#100825=AXIS2_PLACEMENT_3D('',#181449,#116621,#116622);
#100826=AXIS2_PLACEMENT_3D('',#181453,#116624,#116625);
#100827=AXIS2_PLACEMENT_3D('',#181455,#116626,#116627);
#100828=AXIS2_PLACEMENT_3D('',#181457,#116628,#116629);
#100829=AXIS2_PLACEMENT_3D('',#181459,#116631,#116632);
#100830=AXIS2_PLACEMENT_3D('',#181463,#116634,#116635);
#100831=AXIS2_PLACEMENT_3D('',#181465,#116637,#116638);
#100832=AXIS2_PLACEMENT_3D('',#181466,#116639,#116640);
#100833=AXIS2_PLACEMENT_3D('',#181467,#116641,#116642);
#100834=AXIS2_PLACEMENT_3D('',#181468,#116643,#116644);
#100835=AXIS2_PLACEMENT_3D('',#181469,#116645,#116646);
#100836=AXIS2_PLACEMENT_3D('',#181470,#116647,#116648);
#100837=AXIS2_PLACEMENT_3D('',#181471,#116649,#116650);
#100838=AXIS2_PLACEMENT_3D('',#181472,#116651,#116652);
#100839=AXIS2_PLACEMENT_3D('',#181473,#116653,#116654);
#100840=AXIS2_PLACEMENT_3D('',#181474,#116655,#116656);
#100841=AXIS2_PLACEMENT_3D('',#181475,#116657,#116658);
#100842=AXIS2_PLACEMENT_3D('',#181476,#116659,#116660);
#100843=AXIS2_PLACEMENT_3D('',#181477,#116661,#116662);
#100844=AXIS2_PLACEMENT_3D('',#181480,#116663,#116664);
#100845=AXIS2_PLACEMENT_3D('',#181484,#116666,#116667);
#100846=AXIS2_PLACEMENT_3D('',#181486,#116668,#116669);
#100847=AXIS2_PLACEMENT_3D('',#181488,#116670,#116671);
#100848=AXIS2_PLACEMENT_3D('',#181490,#116673,#116674);
#100849=AXIS2_PLACEMENT_3D('',#181494,#116676,#116677);
#100850=AXIS2_PLACEMENT_3D('',#181496,#116679,#116680);
#100851=AXIS2_PLACEMENT_3D('',#181499,#116681,#116682);
#100852=AXIS2_PLACEMENT_3D('',#181503,#116684,#116685);
#100853=AXIS2_PLACEMENT_3D('',#181505,#116687,#116688);
#100854=AXIS2_PLACEMENT_3D('',#181508,#116689,#116690);
#100855=AXIS2_PLACEMENT_3D('',#181512,#116692,#116693);
#100856=AXIS2_PLACEMENT_3D('',#181514,#116694,#116695);
#100857=AXIS2_PLACEMENT_3D('',#181516,#116696,#116697);
#100858=AXIS2_PLACEMENT_3D('',#181518,#116699,#116700);
#100859=AXIS2_PLACEMENT_3D('',#181522,#116702,#116703);
#100860=AXIS2_PLACEMENT_3D('',#181524,#116705,#116706);
#100861=AXIS2_PLACEMENT_3D('',#181525,#116707,#116708);
#100862=AXIS2_PLACEMENT_3D('',#181526,#116709,#116710);
#100863=AXIS2_PLACEMENT_3D('',#181527,#116711,#116712);
#100864=AXIS2_PLACEMENT_3D('',#181528,#116713,#116714);
#100865=AXIS2_PLACEMENT_3D('',#181529,#116715,#116716);
#100866=AXIS2_PLACEMENT_3D('',#181530,#116717,#116718);
#100867=AXIS2_PLACEMENT_3D('',#181531,#116719,#116720);
#100868=AXIS2_PLACEMENT_3D('',#181532,#116721,#116722);
#100869=AXIS2_PLACEMENT_3D('',#181533,#116723,#116724);
#100870=AXIS2_PLACEMENT_3D('',#181534,#116725,#116726);
#100871=AXIS2_PLACEMENT_3D('',#181535,#116727,#116728);
#100872=AXIS2_PLACEMENT_3D('',#181536,#116729,#116730);
#100873=AXIS2_PLACEMENT_3D('',#181539,#116731,#116732);
#100874=AXIS2_PLACEMENT_3D('',#181543,#116734,#116735);
#100875=AXIS2_PLACEMENT_3D('',#181545,#116736,#116737);
#100876=AXIS2_PLACEMENT_3D('',#181547,#116738,#116739);
#100877=AXIS2_PLACEMENT_3D('',#181549,#116741,#116742);
#100878=AXIS2_PLACEMENT_3D('',#181553,#116744,#116745);
#100879=AXIS2_PLACEMENT_3D('',#181555,#116747,#116748);
#100880=AXIS2_PLACEMENT_3D('',#181558,#116749,#116750);
#100881=AXIS2_PLACEMENT_3D('',#181562,#116752,#116753);
#100882=AXIS2_PLACEMENT_3D('',#181564,#116755,#116756);
#100883=AXIS2_PLACEMENT_3D('',#181567,#116757,#116758);
#100884=AXIS2_PLACEMENT_3D('',#181571,#116760,#116761);
#100885=AXIS2_PLACEMENT_3D('',#181573,#116762,#116763);
#100886=AXIS2_PLACEMENT_3D('',#181575,#116764,#116765);
#100887=AXIS2_PLACEMENT_3D('',#181577,#116767,#116768);
#100888=AXIS2_PLACEMENT_3D('',#181581,#116770,#116771);
#100889=AXIS2_PLACEMENT_3D('',#181583,#116773,#116774);
#100890=AXIS2_PLACEMENT_3D('',#181584,#116775,#116776);
#100891=AXIS2_PLACEMENT_3D('',#181585,#116777,#116778);
#100892=AXIS2_PLACEMENT_3D('',#181586,#116779,#116780);
#100893=AXIS2_PLACEMENT_3D('',#181587,#116781,#116782);
#100894=AXIS2_PLACEMENT_3D('',#181588,#116783,#116784);
#100895=AXIS2_PLACEMENT_3D('',#181589,#116785,#116786);
#100896=AXIS2_PLACEMENT_3D('',#181590,#116787,#116788);
#100897=AXIS2_PLACEMENT_3D('',#181591,#116789,#116790);
#100898=AXIS2_PLACEMENT_3D('',#181592,#116791,#116792);
#100899=AXIS2_PLACEMENT_3D('',#181593,#116793,#116794);
#100900=AXIS2_PLACEMENT_3D('',#181594,#116795,#116796);
#100901=AXIS2_PLACEMENT_3D('',#181595,#116797,#116798);
#100902=AXIS2_PLACEMENT_3D('',#181598,#116799,#116800);
#100903=AXIS2_PLACEMENT_3D('',#181602,#116802,#116803);
#100904=AXIS2_PLACEMENT_3D('',#181604,#116804,#116805);
#100905=AXIS2_PLACEMENT_3D('',#181606,#116806,#116807);
#100906=AXIS2_PLACEMENT_3D('',#181608,#116809,#116810);
#100907=AXIS2_PLACEMENT_3D('',#181612,#116812,#116813);
#100908=AXIS2_PLACEMENT_3D('',#181614,#116815,#116816);
#100909=AXIS2_PLACEMENT_3D('',#181617,#116817,#116818);
#100910=AXIS2_PLACEMENT_3D('',#181621,#116820,#116821);
#100911=AXIS2_PLACEMENT_3D('',#181623,#116823,#116824);
#100912=AXIS2_PLACEMENT_3D('',#181626,#116825,#116826);
#100913=AXIS2_PLACEMENT_3D('',#181630,#116828,#116829);
#100914=AXIS2_PLACEMENT_3D('',#181632,#116830,#116831);
#100915=AXIS2_PLACEMENT_3D('',#181634,#116832,#116833);
#100916=AXIS2_PLACEMENT_3D('',#181636,#116835,#116836);
#100917=AXIS2_PLACEMENT_3D('',#181640,#116838,#116839);
#100918=AXIS2_PLACEMENT_3D('',#181642,#116841,#116842);
#100919=AXIS2_PLACEMENT_3D('',#181643,#116843,#116844);
#100920=AXIS2_PLACEMENT_3D('',#181644,#116845,#116846);
#100921=AXIS2_PLACEMENT_3D('',#181645,#116847,#116848);
#100922=AXIS2_PLACEMENT_3D('',#181646,#116849,#116850);
#100923=AXIS2_PLACEMENT_3D('',#181647,#116851,#116852);
#100924=AXIS2_PLACEMENT_3D('',#181648,#116853,#116854);
#100925=AXIS2_PLACEMENT_3D('',#181649,#116855,#116856);
#100926=AXIS2_PLACEMENT_3D('',#181650,#116857,#116858);
#100927=AXIS2_PLACEMENT_3D('',#181651,#116859,#116860);
#100928=AXIS2_PLACEMENT_3D('',#181652,#116861,#116862);
#100929=AXIS2_PLACEMENT_3D('',#181653,#116863,#116864);
#100930=AXIS2_PLACEMENT_3D('',#181654,#116865,#116866);
#100931=AXIS2_PLACEMENT_3D('',#181657,#116867,#116868);
#100932=AXIS2_PLACEMENT_3D('',#181661,#116870,#116871);
#100933=AXIS2_PLACEMENT_3D('',#181663,#116872,#116873);
#100934=AXIS2_PLACEMENT_3D('',#181665,#116874,#116875);
#100935=AXIS2_PLACEMENT_3D('',#181667,#116877,#116878);
#100936=AXIS2_PLACEMENT_3D('',#181671,#116880,#116881);
#100937=AXIS2_PLACEMENT_3D('',#181673,#116883,#116884);
#100938=AXIS2_PLACEMENT_3D('',#181676,#116885,#116886);
#100939=AXIS2_PLACEMENT_3D('',#181680,#116888,#116889);
#100940=AXIS2_PLACEMENT_3D('',#181682,#116891,#116892);
#100941=AXIS2_PLACEMENT_3D('',#181685,#116893,#116894);
#100942=AXIS2_PLACEMENT_3D('',#181689,#116896,#116897);
#100943=AXIS2_PLACEMENT_3D('',#181691,#116898,#116899);
#100944=AXIS2_PLACEMENT_3D('',#181693,#116900,#116901);
#100945=AXIS2_PLACEMENT_3D('',#181695,#116903,#116904);
#100946=AXIS2_PLACEMENT_3D('',#181699,#116906,#116907);
#100947=AXIS2_PLACEMENT_3D('',#181701,#116909,#116910);
#100948=AXIS2_PLACEMENT_3D('',#181702,#116911,#116912);
#100949=AXIS2_PLACEMENT_3D('',#181703,#116913,#116914);
#100950=AXIS2_PLACEMENT_3D('',#181704,#116915,#116916);
#100951=AXIS2_PLACEMENT_3D('',#181705,#116917,#116918);
#100952=AXIS2_PLACEMENT_3D('',#181706,#116919,#116920);
#100953=AXIS2_PLACEMENT_3D('',#181707,#116921,#116922);
#100954=AXIS2_PLACEMENT_3D('',#181708,#116923,#116924);
#100955=AXIS2_PLACEMENT_3D('',#181709,#116925,#116926);
#100956=AXIS2_PLACEMENT_3D('',#181710,#116927,#116928);
#100957=AXIS2_PLACEMENT_3D('',#181711,#116929,#116930);
#100958=AXIS2_PLACEMENT_3D('',#181712,#116931,#116932);
#100959=AXIS2_PLACEMENT_3D('',#181713,#116933,#116934);
#100960=AXIS2_PLACEMENT_3D('',#181716,#116935,#116936);
#100961=AXIS2_PLACEMENT_3D('',#181720,#116938,#116939);
#100962=AXIS2_PLACEMENT_3D('',#181722,#116940,#116941);
#100963=AXIS2_PLACEMENT_3D('',#181724,#116942,#116943);
#100964=AXIS2_PLACEMENT_3D('',#181726,#116945,#116946);
#100965=AXIS2_PLACEMENT_3D('',#181730,#116948,#116949);
#100966=AXIS2_PLACEMENT_3D('',#181732,#116951,#116952);
#100967=AXIS2_PLACEMENT_3D('',#181735,#116953,#116954);
#100968=AXIS2_PLACEMENT_3D('',#181739,#116956,#116957);
#100969=AXIS2_PLACEMENT_3D('',#181741,#116959,#116960);
#100970=AXIS2_PLACEMENT_3D('',#181744,#116961,#116962);
#100971=AXIS2_PLACEMENT_3D('',#181748,#116964,#116965);
#100972=AXIS2_PLACEMENT_3D('',#181750,#116966,#116967);
#100973=AXIS2_PLACEMENT_3D('',#181752,#116968,#116969);
#100974=AXIS2_PLACEMENT_3D('',#181754,#116971,#116972);
#100975=AXIS2_PLACEMENT_3D('',#181758,#116974,#116975);
#100976=AXIS2_PLACEMENT_3D('',#181760,#116977,#116978);
#100977=AXIS2_PLACEMENT_3D('',#181761,#116979,#116980);
#100978=AXIS2_PLACEMENT_3D('',#181762,#116981,#116982);
#100979=AXIS2_PLACEMENT_3D('',#181763,#116983,#116984);
#100980=AXIS2_PLACEMENT_3D('',#181764,#116985,#116986);
#100981=AXIS2_PLACEMENT_3D('',#181765,#116987,#116988);
#100982=AXIS2_PLACEMENT_3D('',#181766,#116989,#116990);
#100983=AXIS2_PLACEMENT_3D('',#181767,#116991,#116992);
#100984=AXIS2_PLACEMENT_3D('',#181768,#116993,#116994);
#100985=AXIS2_PLACEMENT_3D('',#181769,#116995,#116996);
#100986=AXIS2_PLACEMENT_3D('',#181770,#116997,#116998);
#100987=AXIS2_PLACEMENT_3D('',#181771,#116999,#117000);
#100988=AXIS2_PLACEMENT_3D('',#181772,#117001,#117002);
#100989=AXIS2_PLACEMENT_3D('',#181775,#117003,#117004);
#100990=AXIS2_PLACEMENT_3D('',#181779,#117006,#117007);
#100991=AXIS2_PLACEMENT_3D('',#181781,#117008,#117009);
#100992=AXIS2_PLACEMENT_3D('',#181783,#117010,#117011);
#100993=AXIS2_PLACEMENT_3D('',#181785,#117013,#117014);
#100994=AXIS2_PLACEMENT_3D('',#181789,#117016,#117017);
#100995=AXIS2_PLACEMENT_3D('',#181791,#117019,#117020);
#100996=AXIS2_PLACEMENT_3D('',#181794,#117021,#117022);
#100997=AXIS2_PLACEMENT_3D('',#181798,#117024,#117025);
#100998=AXIS2_PLACEMENT_3D('',#181800,#117027,#117028);
#100999=AXIS2_PLACEMENT_3D('',#181803,#117029,#117030);
#101000=AXIS2_PLACEMENT_3D('',#181807,#117032,#117033);
#101001=AXIS2_PLACEMENT_3D('',#181809,#117034,#117035);
#101002=AXIS2_PLACEMENT_3D('',#181811,#117036,#117037);
#101003=AXIS2_PLACEMENT_3D('',#181813,#117039,#117040);
#101004=AXIS2_PLACEMENT_3D('',#181817,#117042,#117043);
#101005=AXIS2_PLACEMENT_3D('',#181819,#117045,#117046);
#101006=AXIS2_PLACEMENT_3D('',#181820,#117047,#117048);
#101007=AXIS2_PLACEMENT_3D('',#181821,#117049,#117050);
#101008=AXIS2_PLACEMENT_3D('',#181822,#117051,#117052);
#101009=AXIS2_PLACEMENT_3D('',#181823,#117053,#117054);
#101010=AXIS2_PLACEMENT_3D('',#181824,#117055,#117056);
#101011=AXIS2_PLACEMENT_3D('',#181825,#117057,#117058);
#101012=AXIS2_PLACEMENT_3D('',#181826,#117059,#117060);
#101013=AXIS2_PLACEMENT_3D('',#181827,#117061,#117062);
#101014=AXIS2_PLACEMENT_3D('',#181828,#117063,#117064);
#101015=AXIS2_PLACEMENT_3D('',#181829,#117065,#117066);
#101016=AXIS2_PLACEMENT_3D('',#181830,#117067,#117068);
#101017=AXIS2_PLACEMENT_3D('',#181831,#117069,#117070);
#101018=AXIS2_PLACEMENT_3D('',#181834,#117071,#117072);
#101019=AXIS2_PLACEMENT_3D('',#181838,#117074,#117075);
#101020=AXIS2_PLACEMENT_3D('',#181840,#117076,#117077);
#101021=AXIS2_PLACEMENT_3D('',#181842,#117078,#117079);
#101022=AXIS2_PLACEMENT_3D('',#181844,#117081,#117082);
#101023=AXIS2_PLACEMENT_3D('',#181848,#117084,#117085);
#101024=AXIS2_PLACEMENT_3D('',#181850,#117087,#117088);
#101025=AXIS2_PLACEMENT_3D('',#181853,#117089,#117090);
#101026=AXIS2_PLACEMENT_3D('',#181857,#117092,#117093);
#101027=AXIS2_PLACEMENT_3D('',#181859,#117095,#117096);
#101028=AXIS2_PLACEMENT_3D('',#181862,#117097,#117098);
#101029=AXIS2_PLACEMENT_3D('',#181866,#117100,#117101);
#101030=AXIS2_PLACEMENT_3D('',#181868,#117102,#117103);
#101031=AXIS2_PLACEMENT_3D('',#181870,#117104,#117105);
#101032=AXIS2_PLACEMENT_3D('',#181872,#117107,#117108);
#101033=AXIS2_PLACEMENT_3D('',#181876,#117110,#117111);
#101034=AXIS2_PLACEMENT_3D('',#181878,#117113,#117114);
#101035=AXIS2_PLACEMENT_3D('',#181879,#117115,#117116);
#101036=AXIS2_PLACEMENT_3D('',#181880,#117117,#117118);
#101037=AXIS2_PLACEMENT_3D('',#181881,#117119,#117120);
#101038=AXIS2_PLACEMENT_3D('',#181882,#117121,#117122);
#101039=AXIS2_PLACEMENT_3D('',#181883,#117123,#117124);
#101040=AXIS2_PLACEMENT_3D('',#181884,#117125,#117126);
#101041=AXIS2_PLACEMENT_3D('',#181885,#117127,#117128);
#101042=AXIS2_PLACEMENT_3D('',#181886,#117129,#117130);
#101043=AXIS2_PLACEMENT_3D('',#181887,#117131,#117132);
#101044=AXIS2_PLACEMENT_3D('',#181888,#117133,#117134);
#101045=AXIS2_PLACEMENT_3D('',#181889,#117135,#117136);
#101046=AXIS2_PLACEMENT_3D('',#181890,#117137,#117138);
#101047=AXIS2_PLACEMENT_3D('',#181893,#117139,#117140);
#101048=AXIS2_PLACEMENT_3D('',#181897,#117142,#117143);
#101049=AXIS2_PLACEMENT_3D('',#181899,#117144,#117145);
#101050=AXIS2_PLACEMENT_3D('',#181901,#117146,#117147);
#101051=AXIS2_PLACEMENT_3D('',#181903,#117149,#117150);
#101052=AXIS2_PLACEMENT_3D('',#181907,#117152,#117153);
#101053=AXIS2_PLACEMENT_3D('',#181909,#117155,#117156);
#101054=AXIS2_PLACEMENT_3D('',#181912,#117157,#117158);
#101055=AXIS2_PLACEMENT_3D('',#181916,#117160,#117161);
#101056=AXIS2_PLACEMENT_3D('',#181918,#117163,#117164);
#101057=AXIS2_PLACEMENT_3D('',#181921,#117165,#117166);
#101058=AXIS2_PLACEMENT_3D('',#181925,#117168,#117169);
#101059=AXIS2_PLACEMENT_3D('',#181927,#117170,#117171);
#101060=AXIS2_PLACEMENT_3D('',#181929,#117172,#117173);
#101061=AXIS2_PLACEMENT_3D('',#181931,#117175,#117176);
#101062=AXIS2_PLACEMENT_3D('',#181935,#117178,#117179);
#101063=AXIS2_PLACEMENT_3D('',#181937,#117181,#117182);
#101064=AXIS2_PLACEMENT_3D('',#181938,#117183,#117184);
#101065=AXIS2_PLACEMENT_3D('',#181939,#117185,#117186);
#101066=AXIS2_PLACEMENT_3D('',#181940,#117187,#117188);
#101067=AXIS2_PLACEMENT_3D('',#181941,#117189,#117190);
#101068=AXIS2_PLACEMENT_3D('',#181942,#117191,#117192);
#101069=AXIS2_PLACEMENT_3D('',#181943,#117193,#117194);
#101070=AXIS2_PLACEMENT_3D('',#181944,#117195,#117196);
#101071=AXIS2_PLACEMENT_3D('',#181945,#117197,#117198);
#101072=AXIS2_PLACEMENT_3D('',#181946,#117199,#117200);
#101073=AXIS2_PLACEMENT_3D('',#181947,#117201,#117202);
#101074=AXIS2_PLACEMENT_3D('',#181948,#117203,#117204);
#101075=AXIS2_PLACEMENT_3D('',#181949,#117205,#117206);
#101076=AXIS2_PLACEMENT_3D('',#181950,#117207,#117208);
#101077=AXIS2_PLACEMENT_3D('',#181953,#117209,#117210);
#101078=AXIS2_PLACEMENT_3D('',#181957,#117212,#117213);
#101079=AXIS2_PLACEMENT_3D('',#181959,#117214,#117215);
#101080=AXIS2_PLACEMENT_3D('',#181961,#117216,#117217);
#101081=AXIS2_PLACEMENT_3D('',#181963,#117219,#117220);
#101082=AXIS2_PLACEMENT_3D('',#181967,#117222,#117223);
#101083=AXIS2_PLACEMENT_3D('',#181969,#117225,#117226);
#101084=AXIS2_PLACEMENT_3D('',#181972,#117227,#117228);
#101085=AXIS2_PLACEMENT_3D('',#181976,#117230,#117231);
#101086=AXIS2_PLACEMENT_3D('',#181978,#117233,#117234);
#101087=AXIS2_PLACEMENT_3D('',#181981,#117235,#117236);
#101088=AXIS2_PLACEMENT_3D('',#181985,#117238,#117239);
#101089=AXIS2_PLACEMENT_3D('',#181987,#117240,#117241);
#101090=AXIS2_PLACEMENT_3D('',#181989,#117242,#117243);
#101091=AXIS2_PLACEMENT_3D('',#181991,#117245,#117246);
#101092=AXIS2_PLACEMENT_3D('',#181995,#117248,#117249);
#101093=AXIS2_PLACEMENT_3D('',#181997,#117251,#117252);
#101094=AXIS2_PLACEMENT_3D('',#181998,#117253,#117254);
#101095=AXIS2_PLACEMENT_3D('',#181999,#117255,#117256);
#101096=AXIS2_PLACEMENT_3D('',#182000,#117257,#117258);
#101097=AXIS2_PLACEMENT_3D('',#182001,#117259,#117260);
#101098=AXIS2_PLACEMENT_3D('',#182002,#117261,#117262);
#101099=AXIS2_PLACEMENT_3D('',#182003,#117263,#117264);
#101100=AXIS2_PLACEMENT_3D('',#182004,#117265,#117266);
#101101=AXIS2_PLACEMENT_3D('',#182005,#117267,#117268);
#101102=AXIS2_PLACEMENT_3D('',#182006,#117269,#117270);
#101103=AXIS2_PLACEMENT_3D('',#182007,#117271,#117272);
#101104=AXIS2_PLACEMENT_3D('',#182008,#117273,#117274);
#101105=AXIS2_PLACEMENT_3D('',#182009,#117275,#117276);
#101106=AXIS2_PLACEMENT_3D('',#182010,#117277,#117278);
#101107=AXIS2_PLACEMENT_3D('',#182011,#117279,#117280);
#101108=AXIS2_PLACEMENT_3D('',#182016,#117282,#117283);
#101109=AXIS2_PLACEMENT_3D('',#182019,#117285,#117286);
#101110=AXIS2_PLACEMENT_3D('',#182020,#117287,#117288);
#101111=AXIS2_PLACEMENT_3D('',#182023,#117289,#117290);
#101112=AXIS2_PLACEMENT_3D('',#182031,#117294,#117295);
#101113=AXIS2_PLACEMENT_3D('',#182037,#117298,#117299);
#101114=AXIS2_PLACEMENT_3D('',#182041,#117301,#117302);
#101115=AXIS2_PLACEMENT_3D('',#182045,#117305,#117306);
#101116=AXIS2_PLACEMENT_3D('',#182048,#117307,#117308);
#101117=AXIS2_PLACEMENT_3D('',#182056,#117312,#117313);
#101118=AXIS2_PLACEMENT_3D('',#182062,#117316,#117317);
#101119=AXIS2_PLACEMENT_3D('',#182066,#117319,#117320);
#101120=AXIS2_PLACEMENT_3D('',#182070,#117323,#117324);
#101121=AXIS2_PLACEMENT_3D('',#182175,#117325,#117326);
#101122=AXIS2_PLACEMENT_3D('',#182274,#117327,#117328);
#101123=AXIS2_PLACEMENT_3D('',#182275,#117329,#117330);
#101124=AXIS2_PLACEMENT_3D('',#182276,#117331,#117332);
#101125=AXIS2_PLACEMENT_3D('',#182289,#117333,#117334);
#101126=AXIS2_PLACEMENT_3D('',#182290,#117335,#117336);
#101127=AXIS2_PLACEMENT_3D('',#182291,#117337,#117338);
#101128=AXIS2_PLACEMENT_3D('',#182292,#117339,#117340);
#101129=AXIS2_PLACEMENT_3D('',#182293,#117341,#117342);
#101130=AXIS2_PLACEMENT_3D('',#182306,#117343,#117344);
#101131=AXIS2_PLACEMENT_3D('',#182319,#117345,#117346);
#101132=AXIS2_PLACEMENT_3D('',#182320,#117347,#117348);
#101133=AXIS2_PLACEMENT_3D('',#182321,#117349,#117350);
#101134=AXIS2_PLACEMENT_3D('',#182322,#117351,#117352);
#101135=AXIS2_PLACEMENT_3D('',#182323,#117353,#117354);
#101136=AXIS2_PLACEMENT_3D('',#182342,#117355,#117356);
#101137=AXIS2_PLACEMENT_3D('',#182343,#117357,#117358);
#101138=AXIS2_PLACEMENT_3D('',#182344,#117359,#117360);
#101139=AXIS2_PLACEMENT_3D('',#182345,#117361,#117362);
#101140=AXIS2_PLACEMENT_3D('',#182346,#117363,#117364);
#101141=AXIS2_PLACEMENT_3D('',#182359,#117365,#117366);
#101142=AXIS2_PLACEMENT_3D('',#182378,#117367,#117368);
#101143=AXIS2_PLACEMENT_3D('',#182379,#117369,#117370);
#101144=AXIS2_PLACEMENT_3D('',#182380,#117371,#117372);
#101145=AXIS2_PLACEMENT_3D('',#182381,#117373,#117374);
#101146=AXIS2_PLACEMENT_3D('',#182382,#117375,#117376);
#101147=AXIS2_PLACEMENT_3D('',#182401,#117377,#117378);
#101148=AXIS2_PLACEMENT_3D('',#182414,#117379,#117380);
#101149=AXIS2_PLACEMENT_3D('',#182415,#117381,#117382);
#101150=AXIS2_PLACEMENT_3D('',#182416,#117383,#117384);
#101151=AXIS2_PLACEMENT_3D('',#182417,#117385,#117386);
#101152=AXIS2_PLACEMENT_3D('',#182418,#117387,#117388);
#101153=AXIS2_PLACEMENT_3D('',#182437,#117389,#117390);
#101154=AXIS2_PLACEMENT_3D('',#182438,#117391,#117392);
#101155=AXIS2_PLACEMENT_3D('',#182439,#117393,#117394);
#101156=AXIS2_PLACEMENT_3D('',#182440,#117395,#117396);
#101157=AXIS2_PLACEMENT_3D('',#182441,#117397,#117398);
#101158=AXIS2_PLACEMENT_3D('',#182454,#117399,#117400);
#101159=AXIS2_PLACEMENT_3D('',#182467,#117401,#117402);
#101160=AXIS2_PLACEMENT_3D('',#182468,#117403,#117404);
#101161=AXIS2_PLACEMENT_3D('',#182469,#117405,#117406);
#101162=AXIS2_PLACEMENT_3D('',#182470,#117407,#117408);
#101163=AXIS2_PLACEMENT_3D('',#182471,#117409,#117410);
#101164=AXIS2_PLACEMENT_3D('',#182484,#117411,#117412);
#101165=AXIS2_PLACEMENT_3D('',#182485,#117413,#117414);
#101166=AXIS2_PLACEMENT_3D('',#182486,#117415,#117416);
#101167=AXIS2_PLACEMENT_3D('',#182491,#117418,#117419);
#101168=AXIS2_PLACEMENT_3D('',#182494,#117421,#117422);
#101169=AXIS2_PLACEMENT_3D('',#182495,#117423,#117424);
#101170=AXIS2_PLACEMENT_3D('',#182498,#117425,#117426);
#101171=AXIS2_PLACEMENT_3D('',#182506,#117430,#117431);
#101172=AXIS2_PLACEMENT_3D('',#182512,#117434,#117435);
#101173=AXIS2_PLACEMENT_3D('',#182516,#117437,#117438);
#101174=AXIS2_PLACEMENT_3D('',#182520,#117441,#117442);
#101175=AXIS2_PLACEMENT_3D('',#182523,#117443,#117444);
#101176=AXIS2_PLACEMENT_3D('',#182531,#117448,#117449);
#101177=AXIS2_PLACEMENT_3D('',#182537,#117452,#117453);
#101178=AXIS2_PLACEMENT_3D('',#182541,#117455,#117456);
#101179=AXIS2_PLACEMENT_3D('',#182545,#117459,#117460);
#101180=AXIS2_PLACEMENT_3D('',#182550,#117462,#117463);
#101181=AXIS2_PLACEMENT_3D('',#182553,#117465,#117466);
#101182=AXIS2_PLACEMENT_3D('',#182554,#117467,#117468);
#101183=AXIS2_PLACEMENT_3D('',#182557,#117469,#117470);
#101184=AXIS2_PLACEMENT_3D('',#182565,#117474,#117475);
#101185=AXIS2_PLACEMENT_3D('',#182571,#117478,#117479);
#101186=AXIS2_PLACEMENT_3D('',#182575,#117481,#117482);
#101187=AXIS2_PLACEMENT_3D('',#182579,#117485,#117486);
#101188=AXIS2_PLACEMENT_3D('',#182582,#117487,#117488);
#101189=AXIS2_PLACEMENT_3D('',#182590,#117492,#117493);
#101190=AXIS2_PLACEMENT_3D('',#182596,#117496,#117497);
#101191=AXIS2_PLACEMENT_3D('',#182600,#117499,#117500);
#101192=AXIS2_PLACEMENT_3D('',#182604,#117503,#117504);
#101193=AXIS2_PLACEMENT_3D('',#182609,#117506,#117507);
#101194=AXIS2_PLACEMENT_3D('',#182612,#117509,#117510);
#101195=AXIS2_PLACEMENT_3D('',#182613,#117511,#117512);
#101196=AXIS2_PLACEMENT_3D('',#182616,#117513,#117514);
#101197=AXIS2_PLACEMENT_3D('',#182624,#117518,#117519);
#101198=AXIS2_PLACEMENT_3D('',#182630,#117522,#117523);
#101199=AXIS2_PLACEMENT_3D('',#182634,#117525,#117526);
#101200=AXIS2_PLACEMENT_3D('',#182638,#117529,#117530);
#101201=AXIS2_PLACEMENT_3D('',#182641,#117531,#117532);
#101202=AXIS2_PLACEMENT_3D('',#182649,#117536,#117537);
#101203=AXIS2_PLACEMENT_3D('',#182655,#117540,#117541);
#101204=AXIS2_PLACEMENT_3D('',#182659,#117543,#117544);
#101205=AXIS2_PLACEMENT_3D('',#182663,#117547,#117548);
#101206=AXIS2_PLACEMENT_3D('',#182668,#117550,#117551);
#101207=AXIS2_PLACEMENT_3D('',#182671,#117553,#117554);
#101208=AXIS2_PLACEMENT_3D('',#182672,#117555,#117556);
#101209=AXIS2_PLACEMENT_3D('',#182675,#117557,#117558);
#101210=AXIS2_PLACEMENT_3D('',#182683,#117562,#117563);
#101211=AXIS2_PLACEMENT_3D('',#182689,#117566,#117567);
#101212=AXIS2_PLACEMENT_3D('',#182693,#117569,#117570);
#101213=AXIS2_PLACEMENT_3D('',#182697,#117573,#117574);
#101214=AXIS2_PLACEMENT_3D('',#182700,#117575,#117576);
#101215=AXIS2_PLACEMENT_3D('',#182708,#117580,#117581);
#101216=AXIS2_PLACEMENT_3D('',#182714,#117584,#117585);
#101217=AXIS2_PLACEMENT_3D('',#182718,#117587,#117588);
#101218=AXIS2_PLACEMENT_3D('',#182722,#117591,#117592);
#101219=AXIS2_PLACEMENT_3D('',#182727,#117594,#117595);
#101220=AXIS2_PLACEMENT_3D('',#182730,#117597,#117598);
#101221=AXIS2_PLACEMENT_3D('',#182731,#117599,#117600);
#101222=AXIS2_PLACEMENT_3D('',#182734,#117601,#117602);
#101223=AXIS2_PLACEMENT_3D('',#182742,#117606,#117607);
#101224=AXIS2_PLACEMENT_3D('',#182748,#117610,#117611);
#101225=AXIS2_PLACEMENT_3D('',#182752,#117613,#117614);
#101226=AXIS2_PLACEMENT_3D('',#182756,#117617,#117618);
#101227=AXIS2_PLACEMENT_3D('',#182759,#117619,#117620);
#101228=AXIS2_PLACEMENT_3D('',#182767,#117624,#117625);
#101229=AXIS2_PLACEMENT_3D('',#182773,#117628,#117629);
#101230=AXIS2_PLACEMENT_3D('',#182777,#117631,#117632);
#101231=AXIS2_PLACEMENT_3D('',#182781,#117635,#117636);
#101232=AXIS2_PLACEMENT_3D('',#182786,#117638,#117639);
#101233=AXIS2_PLACEMENT_3D('',#182789,#117641,#117642);
#101234=AXIS2_PLACEMENT_3D('',#182790,#117643,#117644);
#101235=AXIS2_PLACEMENT_3D('',#182793,#117645,#117646);
#101236=AXIS2_PLACEMENT_3D('',#182801,#117650,#117651);
#101237=AXIS2_PLACEMENT_3D('',#182807,#117654,#117655);
#101238=AXIS2_PLACEMENT_3D('',#182811,#117657,#117658);
#101239=AXIS2_PLACEMENT_3D('',#182815,#117661,#117662);
#101240=AXIS2_PLACEMENT_3D('',#182818,#117663,#117664);
#101241=AXIS2_PLACEMENT_3D('',#182826,#117668,#117669);
#101242=AXIS2_PLACEMENT_3D('',#182832,#117672,#117673);
#101243=AXIS2_PLACEMENT_3D('',#182836,#117675,#117676);
#101244=AXIS2_PLACEMENT_3D('',#182840,#117679,#117680);
#101245=AXIS2_PLACEMENT_3D('',#182845,#117682,#117683);
#101246=AXIS2_PLACEMENT_3D('',#182848,#117685,#117686);
#101247=AXIS2_PLACEMENT_3D('',#182849,#117687,#117688);
#101248=AXIS2_PLACEMENT_3D('',#182852,#117689,#117690);
#101249=AXIS2_PLACEMENT_3D('',#182860,#117694,#117695);
#101250=AXIS2_PLACEMENT_3D('',#182866,#117698,#117699);
#101251=AXIS2_PLACEMENT_3D('',#182870,#117701,#117702);
#101252=AXIS2_PLACEMENT_3D('',#182874,#117705,#117706);
#101253=AXIS2_PLACEMENT_3D('',#182877,#117707,#117708);
#101254=AXIS2_PLACEMENT_3D('',#182885,#117712,#117713);
#101255=AXIS2_PLACEMENT_3D('',#182891,#117716,#117717);
#101256=AXIS2_PLACEMENT_3D('',#182895,#117719,#117720);
#101257=AXIS2_PLACEMENT_3D('',#182899,#117723,#117724);
#101258=AXIS2_PLACEMENT_3D('',#182904,#117726,#117727);
#101259=AXIS2_PLACEMENT_3D('',#182907,#117729,#117730);
#101260=AXIS2_PLACEMENT_3D('',#182908,#117731,#117732);
#101261=AXIS2_PLACEMENT_3D('',#182911,#117733,#117734);
#101262=AXIS2_PLACEMENT_3D('',#182919,#117738,#117739);
#101263=AXIS2_PLACEMENT_3D('',#182925,#117742,#117743);
#101264=AXIS2_PLACEMENT_3D('',#182929,#117745,#117746);
#101265=AXIS2_PLACEMENT_3D('',#182933,#117749,#117750);
#101266=AXIS2_PLACEMENT_3D('',#182936,#117751,#117752);
#101267=AXIS2_PLACEMENT_3D('',#182944,#117756,#117757);
#101268=AXIS2_PLACEMENT_3D('',#182950,#117760,#117761);
#101269=AXIS2_PLACEMENT_3D('',#182954,#117763,#117764);
#101270=AXIS2_PLACEMENT_3D('',#182958,#117767,#117768);
#101271=AXIS2_PLACEMENT_3D('',#182963,#117770,#117771);
#101272=AXIS2_PLACEMENT_3D('',#182966,#117773,#117774);
#101273=AXIS2_PLACEMENT_3D('',#182967,#117775,#117776);
#101274=AXIS2_PLACEMENT_3D('',#182970,#117777,#117778);
#101275=AXIS2_PLACEMENT_3D('',#182978,#117782,#117783);
#101276=AXIS2_PLACEMENT_3D('',#182984,#117786,#117787);
#101277=AXIS2_PLACEMENT_3D('',#182988,#117789,#117790);
#101278=AXIS2_PLACEMENT_3D('',#182992,#117793,#117794);
#101279=AXIS2_PLACEMENT_3D('',#182995,#117795,#117796);
#101280=AXIS2_PLACEMENT_3D('',#183003,#117800,#117801);
#101281=AXIS2_PLACEMENT_3D('',#183009,#117804,#117805);
#101282=AXIS2_PLACEMENT_3D('',#183013,#117807,#117808);
#101283=AXIS2_PLACEMENT_3D('',#183017,#117811,#117812);
#101284=AXIS2_PLACEMENT_3D('',#183022,#117814,#117815);
#101285=AXIS2_PLACEMENT_3D('',#183025,#117817,#117818);
#101286=AXIS2_PLACEMENT_3D('',#183026,#117819,#117820);
#101287=AXIS2_PLACEMENT_3D('',#183029,#117821,#117822);
#101288=AXIS2_PLACEMENT_3D('',#183037,#117826,#117827);
#101289=AXIS2_PLACEMENT_3D('',#183043,#117830,#117831);
#101290=AXIS2_PLACEMENT_3D('',#183047,#117833,#117834);
#101291=AXIS2_PLACEMENT_3D('',#183051,#117837,#117838);
#101292=AXIS2_PLACEMENT_3D('',#183054,#117839,#117840);
#101293=AXIS2_PLACEMENT_3D('',#183062,#117844,#117845);
#101294=AXIS2_PLACEMENT_3D('',#183068,#117848,#117849);
#101295=AXIS2_PLACEMENT_3D('',#183072,#117851,#117852);
#101296=AXIS2_PLACEMENT_3D('',#183076,#117855,#117856);
#101297=AXIS2_PLACEMENT_3D('',#183081,#117858,#117859);
#101298=AXIS2_PLACEMENT_3D('',#183084,#117861,#117862);
#101299=AXIS2_PLACEMENT_3D('',#183085,#117863,#117864);
#101300=AXIS2_PLACEMENT_3D('',#183088,#117865,#117866);
#101301=AXIS2_PLACEMENT_3D('',#183096,#117870,#117871);
#101302=AXIS2_PLACEMENT_3D('',#183102,#117874,#117875);
#101303=AXIS2_PLACEMENT_3D('',#183106,#117877,#117878);
#101304=AXIS2_PLACEMENT_3D('',#183110,#117881,#117882);
#101305=AXIS2_PLACEMENT_3D('',#183113,#117883,#117884);
#101306=AXIS2_PLACEMENT_3D('',#183121,#117888,#117889);
#101307=AXIS2_PLACEMENT_3D('',#183127,#117892,#117893);
#101308=AXIS2_PLACEMENT_3D('',#183131,#117895,#117896);
#101309=AXIS2_PLACEMENT_3D('',#183135,#117899,#117900);
#101310=AXIS2_PLACEMENT_3D('',#183140,#117902,#117903);
#101311=AXIS2_PLACEMENT_3D('',#183143,#117905,#117906);
#101312=AXIS2_PLACEMENT_3D('',#183144,#117907,#117908);
#101313=AXIS2_PLACEMENT_3D('',#183147,#117909,#117910);
#101314=AXIS2_PLACEMENT_3D('',#183155,#117914,#117915);
#101315=AXIS2_PLACEMENT_3D('',#183161,#117918,#117919);
#101316=AXIS2_PLACEMENT_3D('',#183165,#117921,#117922);
#101317=AXIS2_PLACEMENT_3D('',#183169,#117925,#117926);
#101318=AXIS2_PLACEMENT_3D('',#183172,#117927,#117928);
#101319=AXIS2_PLACEMENT_3D('',#183180,#117932,#117933);
#101320=AXIS2_PLACEMENT_3D('',#183186,#117936,#117937);
#101321=AXIS2_PLACEMENT_3D('',#183190,#117939,#117940);
#101322=AXIS2_PLACEMENT_3D('',#183194,#117943,#117944);
#101323=AXIS2_PLACEMENT_3D('',#183199,#117946,#117947);
#101324=AXIS2_PLACEMENT_3D('',#183202,#117949,#117950);
#101325=AXIS2_PLACEMENT_3D('',#183203,#117951,#117952);
#101326=AXIS2_PLACEMENT_3D('',#183206,#117953,#117954);
#101327=AXIS2_PLACEMENT_3D('',#183214,#117958,#117959);
#101328=AXIS2_PLACEMENT_3D('',#183220,#117962,#117963);
#101329=AXIS2_PLACEMENT_3D('',#183224,#117965,#117966);
#101330=AXIS2_PLACEMENT_3D('',#183228,#117969,#117970);
#101331=AXIS2_PLACEMENT_3D('',#183231,#117971,#117972);
#101332=AXIS2_PLACEMENT_3D('',#183239,#117976,#117977);
#101333=AXIS2_PLACEMENT_3D('',#183245,#117980,#117981);
#101334=AXIS2_PLACEMENT_3D('',#183249,#117983,#117984);
#101335=AXIS2_PLACEMENT_3D('',#183253,#117987,#117988);
#101336=AXIS2_PLACEMENT_3D('',#183258,#117990,#117991);
#101337=AXIS2_PLACEMENT_3D('',#183261,#117993,#117994);
#101338=AXIS2_PLACEMENT_3D('',#183262,#117995,#117996);
#101339=AXIS2_PLACEMENT_3D('',#183265,#117997,#117998);
#101340=AXIS2_PLACEMENT_3D('',#183273,#118002,#118003);
#101341=AXIS2_PLACEMENT_3D('',#183279,#118006,#118007);
#101342=AXIS2_PLACEMENT_3D('',#183283,#118009,#118010);
#101343=AXIS2_PLACEMENT_3D('',#183287,#118013,#118014);
#101344=AXIS2_PLACEMENT_3D('',#183290,#118015,#118016);
#101345=AXIS2_PLACEMENT_3D('',#183298,#118020,#118021);
#101346=AXIS2_PLACEMENT_3D('',#183304,#118024,#118025);
#101347=AXIS2_PLACEMENT_3D('',#183308,#118027,#118028);
#101348=AXIS2_PLACEMENT_3D('',#183312,#118031,#118032);
#101349=AXIS2_PLACEMENT_3D('',#183317,#118034,#118035);
#101350=AXIS2_PLACEMENT_3D('',#183320,#118037,#118038);
#101351=AXIS2_PLACEMENT_3D('',#183321,#118039,#118040);
#101352=AXIS2_PLACEMENT_3D('',#183324,#118041,#118042);
#101353=AXIS2_PLACEMENT_3D('',#183332,#118046,#118047);
#101354=AXIS2_PLACEMENT_3D('',#183338,#118050,#118051);
#101355=AXIS2_PLACEMENT_3D('',#183342,#118053,#118054);
#101356=AXIS2_PLACEMENT_3D('',#183346,#118057,#118058);
#101357=AXIS2_PLACEMENT_3D('',#183349,#118059,#118060);
#101358=AXIS2_PLACEMENT_3D('',#183357,#118064,#118065);
#101359=AXIS2_PLACEMENT_3D('',#183363,#118068,#118069);
#101360=AXIS2_PLACEMENT_3D('',#183367,#118071,#118072);
#101361=AXIS2_PLACEMENT_3D('',#183371,#118075,#118076);
#101362=AXIS2_PLACEMENT_3D('',#183376,#118078,#118079);
#101363=AXIS2_PLACEMENT_3D('',#183379,#118081,#118082);
#101364=AXIS2_PLACEMENT_3D('',#183380,#118083,#118084);
#101365=AXIS2_PLACEMENT_3D('',#183383,#118085,#118086);
#101366=AXIS2_PLACEMENT_3D('',#183391,#118090,#118091);
#101367=AXIS2_PLACEMENT_3D('',#183397,#118094,#118095);
#101368=AXIS2_PLACEMENT_3D('',#183401,#118097,#118098);
#101369=AXIS2_PLACEMENT_3D('',#183405,#118101,#118102);
#101370=AXIS2_PLACEMENT_3D('',#183408,#118103,#118104);
#101371=AXIS2_PLACEMENT_3D('',#183416,#118108,#118109);
#101372=AXIS2_PLACEMENT_3D('',#183422,#118112,#118113);
#101373=AXIS2_PLACEMENT_3D('',#183426,#118115,#118116);
#101374=AXIS2_PLACEMENT_3D('',#183430,#118119,#118120);
#101375=AXIS2_PLACEMENT_3D('',#183435,#118122,#118123);
#101376=AXIS2_PLACEMENT_3D('',#183438,#118125,#118126);
#101377=AXIS2_PLACEMENT_3D('',#183439,#118127,#118128);
#101378=AXIS2_PLACEMENT_3D('',#183442,#118129,#118130);
#101379=AXIS2_PLACEMENT_3D('',#183450,#118134,#118135);
#101380=AXIS2_PLACEMENT_3D('',#183456,#118138,#118139);
#101381=AXIS2_PLACEMENT_3D('',#183460,#118141,#118142);
#101382=AXIS2_PLACEMENT_3D('',#183464,#118145,#118146);
#101383=AXIS2_PLACEMENT_3D('',#183467,#118147,#118148);
#101384=AXIS2_PLACEMENT_3D('',#183475,#118152,#118153);
#101385=AXIS2_PLACEMENT_3D('',#183481,#118156,#118157);
#101386=AXIS2_PLACEMENT_3D('',#183485,#118159,#118160);
#101387=AXIS2_PLACEMENT_3D('',#183489,#118163,#118164);
#101388=AXIS2_PLACEMENT_3D('',#183494,#118166,#118167);
#101389=AXIS2_PLACEMENT_3D('',#183497,#118169,#118170);
#101390=AXIS2_PLACEMENT_3D('',#183498,#118171,#118172);
#101391=AXIS2_PLACEMENT_3D('',#183501,#118173,#118174);
#101392=AXIS2_PLACEMENT_3D('',#183509,#118178,#118179);
#101393=AXIS2_PLACEMENT_3D('',#183515,#118182,#118183);
#101394=AXIS2_PLACEMENT_3D('',#183519,#118185,#118186);
#101395=AXIS2_PLACEMENT_3D('',#183523,#118189,#118190);
#101396=AXIS2_PLACEMENT_3D('',#183526,#118191,#118192);
#101397=AXIS2_PLACEMENT_3D('',#183534,#118196,#118197);
#101398=AXIS2_PLACEMENT_3D('',#183540,#118200,#118201);
#101399=AXIS2_PLACEMENT_3D('',#183544,#118203,#118204);
#101400=AXIS2_PLACEMENT_3D('',#183548,#118207,#118208);
#101401=AXIS2_PLACEMENT_3D('',#183553,#118210,#118211);
#101402=AXIS2_PLACEMENT_3D('',#183556,#118213,#118214);
#101403=AXIS2_PLACEMENT_3D('',#183557,#118215,#118216);
#101404=AXIS2_PLACEMENT_3D('',#183560,#118217,#118218);
#101405=AXIS2_PLACEMENT_3D('',#183568,#118222,#118223);
#101406=AXIS2_PLACEMENT_3D('',#183574,#118226,#118227);
#101407=AXIS2_PLACEMENT_3D('',#183578,#118229,#118230);
#101408=AXIS2_PLACEMENT_3D('',#183582,#118233,#118234);
#101409=AXIS2_PLACEMENT_3D('',#183585,#118235,#118236);
#101410=AXIS2_PLACEMENT_3D('',#183593,#118240,#118241);
#101411=AXIS2_PLACEMENT_3D('',#183599,#118244,#118245);
#101412=AXIS2_PLACEMENT_3D('',#183603,#118247,#118248);
#101413=AXIS2_PLACEMENT_3D('',#183607,#118251,#118252);
#101414=AXIS2_PLACEMENT_3D('',#183612,#118254,#118255);
#101415=AXIS2_PLACEMENT_3D('',#183615,#118257,#118258);
#101416=AXIS2_PLACEMENT_3D('',#183616,#118259,#118260);
#101417=AXIS2_PLACEMENT_3D('',#183619,#118261,#118262);
#101418=AXIS2_PLACEMENT_3D('',#183627,#118266,#118267);
#101419=AXIS2_PLACEMENT_3D('',#183633,#118270,#118271);
#101420=AXIS2_PLACEMENT_3D('',#183637,#118273,#118274);
#101421=AXIS2_PLACEMENT_3D('',#183641,#118277,#118278);
#101422=AXIS2_PLACEMENT_3D('',#183644,#118279,#118280);
#101423=AXIS2_PLACEMENT_3D('',#183652,#118284,#118285);
#101424=AXIS2_PLACEMENT_3D('',#183658,#118288,#118289);
#101425=AXIS2_PLACEMENT_3D('',#183662,#118291,#118292);
#101426=AXIS2_PLACEMENT_3D('',#183666,#118295,#118296);
#101427=AXIS2_PLACEMENT_3D('',#183671,#118298,#118299);
#101428=AXIS2_PLACEMENT_3D('',#183674,#118301,#118302);
#101429=AXIS2_PLACEMENT_3D('',#183675,#118303,#118304);
#101430=AXIS2_PLACEMENT_3D('',#183678,#118305,#118306);
#101431=AXIS2_PLACEMENT_3D('',#183686,#118310,#118311);
#101432=AXIS2_PLACEMENT_3D('',#183692,#118314,#118315);
#101433=AXIS2_PLACEMENT_3D('',#183696,#118317,#118318);
#101434=AXIS2_PLACEMENT_3D('',#183700,#118321,#118322);
#101435=AXIS2_PLACEMENT_3D('',#183703,#118323,#118324);
#101436=AXIS2_PLACEMENT_3D('',#183711,#118328,#118329);
#101437=AXIS2_PLACEMENT_3D('',#183717,#118332,#118333);
#101438=AXIS2_PLACEMENT_3D('',#183721,#118335,#118336);
#101439=AXIS2_PLACEMENT_3D('',#183725,#118339,#118340);
#101440=AXIS2_PLACEMENT_3D('',#183730,#118342,#118343);
#101441=AXIS2_PLACEMENT_3D('',#183733,#118345,#118346);
#101442=AXIS2_PLACEMENT_3D('',#183734,#118347,#118348);
#101443=AXIS2_PLACEMENT_3D('',#183737,#118349,#118350);
#101444=AXIS2_PLACEMENT_3D('',#183745,#118354,#118355);
#101445=AXIS2_PLACEMENT_3D('',#183751,#118358,#118359);
#101446=AXIS2_PLACEMENT_3D('',#183755,#118361,#118362);
#101447=AXIS2_PLACEMENT_3D('',#183759,#118365,#118366);
#101448=AXIS2_PLACEMENT_3D('',#183762,#118367,#118368);
#101449=AXIS2_PLACEMENT_3D('',#183770,#118372,#118373);
#101450=AXIS2_PLACEMENT_3D('',#183776,#118376,#118377);
#101451=AXIS2_PLACEMENT_3D('',#183780,#118379,#118380);
#101452=AXIS2_PLACEMENT_3D('',#183784,#118383,#118384);
#101453=AXIS2_PLACEMENT_3D('',#183789,#118386,#118387);
#101454=AXIS2_PLACEMENT_3D('',#183792,#118389,#118390);
#101455=AXIS2_PLACEMENT_3D('',#183793,#118391,#118392);
#101456=AXIS2_PLACEMENT_3D('',#183796,#118393,#118394);
#101457=AXIS2_PLACEMENT_3D('',#183804,#118398,#118399);
#101458=AXIS2_PLACEMENT_3D('',#183810,#118402,#118403);
#101459=AXIS2_PLACEMENT_3D('',#183814,#118405,#118406);
#101460=AXIS2_PLACEMENT_3D('',#183818,#118409,#118410);
#101461=AXIS2_PLACEMENT_3D('',#183821,#118411,#118412);
#101462=AXIS2_PLACEMENT_3D('',#183829,#118416,#118417);
#101463=AXIS2_PLACEMENT_3D('',#183835,#118420,#118421);
#101464=AXIS2_PLACEMENT_3D('',#183839,#118423,#118424);
#101465=AXIS2_PLACEMENT_3D('',#183843,#118427,#118428);
#101466=AXIS2_PLACEMENT_3D('',#183848,#118430,#118431);
#101467=AXIS2_PLACEMENT_3D('',#183851,#118433,#118434);
#101468=AXIS2_PLACEMENT_3D('',#183852,#118435,#118436);
#101469=AXIS2_PLACEMENT_3D('',#183855,#118437,#118438);
#101470=AXIS2_PLACEMENT_3D('',#183863,#118442,#118443);
#101471=AXIS2_PLACEMENT_3D('',#183869,#118446,#118447);
#101472=AXIS2_PLACEMENT_3D('',#183873,#118449,#118450);
#101473=AXIS2_PLACEMENT_3D('',#183877,#118453,#118454);
#101474=AXIS2_PLACEMENT_3D('',#183880,#118455,#118456);
#101475=AXIS2_PLACEMENT_3D('',#183888,#118460,#118461);
#101476=AXIS2_PLACEMENT_3D('',#183894,#118464,#118465);
#101477=AXIS2_PLACEMENT_3D('',#183898,#118467,#118468);
#101478=AXIS2_PLACEMENT_3D('',#183902,#118471,#118472);
#101479=AXIS2_PLACEMENT_3D('',#183907,#118474,#118475);
#101480=AXIS2_PLACEMENT_3D('',#183910,#118477,#118478);
#101481=AXIS2_PLACEMENT_3D('',#183911,#118479,#118480);
#101482=AXIS2_PLACEMENT_3D('',#183914,#118481,#118482);
#101483=AXIS2_PLACEMENT_3D('',#183922,#118486,#118487);
#101484=AXIS2_PLACEMENT_3D('',#183928,#118490,#118491);
#101485=AXIS2_PLACEMENT_3D('',#183932,#118493,#118494);
#101486=AXIS2_PLACEMENT_3D('',#183936,#118497,#118498);
#101487=AXIS2_PLACEMENT_3D('',#183939,#118499,#118500);
#101488=AXIS2_PLACEMENT_3D('',#183947,#118504,#118505);
#101489=AXIS2_PLACEMENT_3D('',#183953,#118508,#118509);
#101490=AXIS2_PLACEMENT_3D('',#183957,#118511,#118512);
#101491=AXIS2_PLACEMENT_3D('',#183961,#118515,#118516);
#101492=AXIS2_PLACEMENT_3D('',#183966,#118518,#118519);
#101493=AXIS2_PLACEMENT_3D('',#183969,#118521,#118522);
#101494=AXIS2_PLACEMENT_3D('',#183970,#118523,#118524);
#101495=AXIS2_PLACEMENT_3D('',#183973,#118525,#118526);
#101496=AXIS2_PLACEMENT_3D('',#183981,#118530,#118531);
#101497=AXIS2_PLACEMENT_3D('',#183987,#118534,#118535);
#101498=AXIS2_PLACEMENT_3D('',#183991,#118537,#118538);
#101499=AXIS2_PLACEMENT_3D('',#183995,#118541,#118542);
#101500=AXIS2_PLACEMENT_3D('',#183998,#118543,#118544);
#101501=AXIS2_PLACEMENT_3D('',#184006,#118548,#118549);
#101502=AXIS2_PLACEMENT_3D('',#184012,#118552,#118553);
#101503=AXIS2_PLACEMENT_3D('',#184016,#118555,#118556);
#101504=AXIS2_PLACEMENT_3D('',#184020,#118559,#118560);
#101505=AXIS2_PLACEMENT_3D('',#184025,#118562,#118563);
#101506=AXIS2_PLACEMENT_3D('',#184028,#118565,#118566);
#101507=AXIS2_PLACEMENT_3D('',#184029,#118567,#118568);
#101508=AXIS2_PLACEMENT_3D('',#184032,#118569,#118570);
#101509=AXIS2_PLACEMENT_3D('',#184040,#118574,#118575);
#101510=AXIS2_PLACEMENT_3D('',#184046,#118578,#118579);
#101511=AXIS2_PLACEMENT_3D('',#184050,#118581,#118582);
#101512=AXIS2_PLACEMENT_3D('',#184054,#118585,#118586);
#101513=AXIS2_PLACEMENT_3D('',#184057,#118587,#118588);
#101514=AXIS2_PLACEMENT_3D('',#184065,#118592,#118593);
#101515=AXIS2_PLACEMENT_3D('',#184071,#118596,#118597);
#101516=AXIS2_PLACEMENT_3D('',#184075,#118599,#118600);
#101517=AXIS2_PLACEMENT_3D('',#184079,#118603,#118604);
#101518=AXIS2_PLACEMENT_3D('',#184084,#118606,#118607);
#101519=AXIS2_PLACEMENT_3D('',#184087,#118609,#118610);
#101520=AXIS2_PLACEMENT_3D('',#184088,#118611,#118612);
#101521=AXIS2_PLACEMENT_3D('',#184091,#118613,#118614);
#101522=AXIS2_PLACEMENT_3D('',#184099,#118618,#118619);
#101523=AXIS2_PLACEMENT_3D('',#184105,#118622,#118623);
#101524=AXIS2_PLACEMENT_3D('',#184109,#118625,#118626);
#101525=AXIS2_PLACEMENT_3D('',#184113,#118629,#118630);
#101526=AXIS2_PLACEMENT_3D('',#184116,#118631,#118632);
#101527=AXIS2_PLACEMENT_3D('',#184124,#118636,#118637);
#101528=AXIS2_PLACEMENT_3D('',#184130,#118640,#118641);
#101529=AXIS2_PLACEMENT_3D('',#184134,#118643,#118644);
#101530=AXIS2_PLACEMENT_3D('',#184138,#118647,#118648);
#101531=AXIS2_PLACEMENT_3D('',#184143,#118650,#118651);
#101532=AXIS2_PLACEMENT_3D('',#184146,#118653,#118654);
#101533=AXIS2_PLACEMENT_3D('',#184147,#118655,#118656);
#101534=AXIS2_PLACEMENT_3D('',#184150,#118657,#118658);
#101535=AXIS2_PLACEMENT_3D('',#184158,#118662,#118663);
#101536=AXIS2_PLACEMENT_3D('',#184164,#118666,#118667);
#101537=AXIS2_PLACEMENT_3D('',#184168,#118669,#118670);
#101538=AXIS2_PLACEMENT_3D('',#184172,#118673,#118674);
#101539=AXIS2_PLACEMENT_3D('',#184175,#118675,#118676);
#101540=AXIS2_PLACEMENT_3D('',#184183,#118680,#118681);
#101541=AXIS2_PLACEMENT_3D('',#184189,#118684,#118685);
#101542=AXIS2_PLACEMENT_3D('',#184193,#118687,#118688);
#101543=AXIS2_PLACEMENT_3D('',#184197,#118691,#118692);
#101544=AXIS2_PLACEMENT_3D('',#184200,#118695,#118696);
#101545=AXIS2_PLACEMENT_3D('',#184203,#118697,#118698);
#101546=AXIS2_PLACEMENT_3D('',#184211,#118702,#118703);
#101547=AXIS2_PLACEMENT_3D('',#184217,#118706,#118707);
#101548=AXIS2_PLACEMENT_3D('',#184221,#118709,#118710);
#101549=AXIS2_PLACEMENT_3D('',#184225,#118713,#118714);
#101550=AXIS2_PLACEMENT_3D('',#184228,#118715,#118716);
#101551=AXIS2_PLACEMENT_3D('',#184236,#118720,#118721);
#101552=AXIS2_PLACEMENT_3D('',#184242,#118724,#118725);
#101553=AXIS2_PLACEMENT_3D('',#184246,#118727,#118728);
#101554=AXIS2_PLACEMENT_3D('',#184250,#118731,#118732);
#101555=AXIS2_PLACEMENT_3D('',#184255,#118734,#118735);
#101556=AXIS2_PLACEMENT_3D('',#184258,#118737,#118738);
#101557=AXIS2_PLACEMENT_3D('',#184259,#118739,#118740);
#101558=AXIS2_PLACEMENT_3D('',#184262,#118741,#118742);
#101559=AXIS2_PLACEMENT_3D('',#184270,#118746,#118747);
#101560=AXIS2_PLACEMENT_3D('',#184276,#118750,#118751);
#101561=AXIS2_PLACEMENT_3D('',#184280,#118753,#118754);
#101562=AXIS2_PLACEMENT_3D('',#184284,#118757,#118758);
#101563=AXIS2_PLACEMENT_3D('',#184287,#118759,#118760);
#101564=AXIS2_PLACEMENT_3D('',#184295,#118764,#118765);
#101565=AXIS2_PLACEMENT_3D('',#184301,#118768,#118769);
#101566=AXIS2_PLACEMENT_3D('',#184305,#118771,#118772);
#101567=AXIS2_PLACEMENT_3D('',#184309,#118775,#118776);
#101568=AXIS2_PLACEMENT_3D('',#184314,#118778,#118779);
#101569=AXIS2_PLACEMENT_3D('',#184317,#118781,#118782);
#101570=AXIS2_PLACEMENT_3D('',#184318,#118783,#118784);
#101571=AXIS2_PLACEMENT_3D('',#184321,#118785,#118786);
#101572=AXIS2_PLACEMENT_3D('',#184329,#118790,#118791);
#101573=AXIS2_PLACEMENT_3D('',#184335,#118794,#118795);
#101574=AXIS2_PLACEMENT_3D('',#184339,#118797,#118798);
#101575=AXIS2_PLACEMENT_3D('',#184343,#118801,#118802);
#101576=AXIS2_PLACEMENT_3D('',#184346,#118803,#118804);
#101577=AXIS2_PLACEMENT_3D('',#184354,#118808,#118809);
#101578=AXIS2_PLACEMENT_3D('',#184360,#118812,#118813);
#101579=AXIS2_PLACEMENT_3D('',#184364,#118815,#118816);
#101580=AXIS2_PLACEMENT_3D('',#184368,#118819,#118820);
#101581=AXIS2_PLACEMENT_3D('',#184373,#118822,#118823);
#101582=AXIS2_PLACEMENT_3D('',#184376,#118825,#118826);
#101583=AXIS2_PLACEMENT_3D('',#184377,#118827,#118828);
#101584=AXIS2_PLACEMENT_3D('',#184380,#118829,#118830);
#101585=AXIS2_PLACEMENT_3D('',#184388,#118834,#118835);
#101586=AXIS2_PLACEMENT_3D('',#184394,#118838,#118839);
#101587=AXIS2_PLACEMENT_3D('',#184398,#118841,#118842);
#101588=AXIS2_PLACEMENT_3D('',#184402,#118845,#118846);
#101589=AXIS2_PLACEMENT_3D('',#184405,#118847,#118848);
#101590=AXIS2_PLACEMENT_3D('',#184413,#118852,#118853);
#101591=AXIS2_PLACEMENT_3D('',#184419,#118856,#118857);
#101592=AXIS2_PLACEMENT_3D('',#184423,#118859,#118860);
#101593=AXIS2_PLACEMENT_3D('',#184427,#118863,#118864);
#101594=AXIS2_PLACEMENT_3D('',#184432,#118866,#118867);
#101595=AXIS2_PLACEMENT_3D('',#184435,#118869,#118870);
#101596=AXIS2_PLACEMENT_3D('',#184436,#118871,#118872);
#101597=AXIS2_PLACEMENT_3D('',#184439,#118873,#118874);
#101598=AXIS2_PLACEMENT_3D('',#184447,#118878,#118879);
#101599=AXIS2_PLACEMENT_3D('',#184453,#118882,#118883);
#101600=AXIS2_PLACEMENT_3D('',#184457,#118885,#118886);
#101601=AXIS2_PLACEMENT_3D('',#184461,#118889,#118890);
#101602=AXIS2_PLACEMENT_3D('',#184464,#118891,#118892);
#101603=AXIS2_PLACEMENT_3D('',#184472,#118896,#118897);
#101604=AXIS2_PLACEMENT_3D('',#184478,#118900,#118901);
#101605=AXIS2_PLACEMENT_3D('',#184482,#118903,#118904);
#101606=AXIS2_PLACEMENT_3D('',#184486,#118907,#118908);
#101607=AXIS2_PLACEMENT_3D('',#184491,#118910,#118911);
#101608=AXIS2_PLACEMENT_3D('',#184494,#118913,#118914);
#101609=AXIS2_PLACEMENT_3D('',#184495,#118915,#118916);
#101610=AXIS2_PLACEMENT_3D('',#184498,#118917,#118918);
#101611=AXIS2_PLACEMENT_3D('',#184506,#118922,#118923);
#101612=AXIS2_PLACEMENT_3D('',#184512,#118926,#118927);
#101613=AXIS2_PLACEMENT_3D('',#184516,#118929,#118930);
#101614=AXIS2_PLACEMENT_3D('',#184520,#118933,#118934);
#101615=AXIS2_PLACEMENT_3D('',#184523,#118935,#118936);
#101616=AXIS2_PLACEMENT_3D('',#184531,#118940,#118941);
#101617=AXIS2_PLACEMENT_3D('',#184537,#118944,#118945);
#101618=AXIS2_PLACEMENT_3D('',#184541,#118947,#118948);
#101619=AXIS2_PLACEMENT_3D('',#184545,#118951,#118952);
#101620=AXIS2_PLACEMENT_3D('',#184550,#118954,#118955);
#101621=AXIS2_PLACEMENT_3D('',#184553,#118957,#118958);
#101622=AXIS2_PLACEMENT_3D('',#184554,#118959,#118960);
#101623=AXIS2_PLACEMENT_3D('',#184557,#118961,#118962);
#101624=AXIS2_PLACEMENT_3D('',#184565,#118966,#118967);
#101625=AXIS2_PLACEMENT_3D('',#184571,#118970,#118971);
#101626=AXIS2_PLACEMENT_3D('',#184575,#118973,#118974);
#101627=AXIS2_PLACEMENT_3D('',#184579,#118977,#118978);
#101628=AXIS2_PLACEMENT_3D('',#184582,#118979,#118980);
#101629=AXIS2_PLACEMENT_3D('',#184590,#118984,#118985);
#101630=AXIS2_PLACEMENT_3D('',#184596,#118988,#118989);
#101631=AXIS2_PLACEMENT_3D('',#184600,#118991,#118992);
#101632=AXIS2_PLACEMENT_3D('',#184604,#118995,#118996);
#101633=AXIS2_PLACEMENT_3D('',#184609,#118998,#118999);
#101634=AXIS2_PLACEMENT_3D('',#184612,#119001,#119002);
#101635=AXIS2_PLACEMENT_3D('',#184613,#119003,#119004);
#101636=AXIS2_PLACEMENT_3D('',#184616,#119005,#119006);
#101637=AXIS2_PLACEMENT_3D('',#184624,#119010,#119011);
#101638=AXIS2_PLACEMENT_3D('',#184630,#119014,#119015);
#101639=AXIS2_PLACEMENT_3D('',#184634,#119017,#119018);
#101640=AXIS2_PLACEMENT_3D('',#184638,#119021,#119022);
#101641=AXIS2_PLACEMENT_3D('',#184641,#119023,#119024);
#101642=AXIS2_PLACEMENT_3D('',#184649,#119028,#119029);
#101643=AXIS2_PLACEMENT_3D('',#184655,#119032,#119033);
#101644=AXIS2_PLACEMENT_3D('',#184659,#119035,#119036);
#101645=AXIS2_PLACEMENT_3D('',#184663,#119039,#119040);
#101646=AXIS2_PLACEMENT_3D('',#184668,#119042,#119043);
#101647=AXIS2_PLACEMENT_3D('',#184671,#119045,#119046);
#101648=AXIS2_PLACEMENT_3D('',#184672,#119047,#119048);
#101649=AXIS2_PLACEMENT_3D('',#184675,#119049,#119050);
#101650=AXIS2_PLACEMENT_3D('',#184683,#119054,#119055);
#101651=AXIS2_PLACEMENT_3D('',#184689,#119058,#119059);
#101652=AXIS2_PLACEMENT_3D('',#184693,#119061,#119062);
#101653=AXIS2_PLACEMENT_3D('',#184697,#119065,#119066);
#101654=AXIS2_PLACEMENT_3D('',#184700,#119067,#119068);
#101655=AXIS2_PLACEMENT_3D('',#184708,#119072,#119073);
#101656=AXIS2_PLACEMENT_3D('',#184714,#119076,#119077);
#101657=AXIS2_PLACEMENT_3D('',#184718,#119079,#119080);
#101658=AXIS2_PLACEMENT_3D('',#184722,#119083,#119084);
#101659=AXIS2_PLACEMENT_3D('',#184727,#119086,#119087);
#101660=AXIS2_PLACEMENT_3D('',#184730,#119089,#119090);
#101661=AXIS2_PLACEMENT_3D('',#184731,#119091,#119092);
#101662=AXIS2_PLACEMENT_3D('',#184734,#119093,#119094);
#101663=AXIS2_PLACEMENT_3D('',#184742,#119098,#119099);
#101664=AXIS2_PLACEMENT_3D('',#184748,#119102,#119103);
#101665=AXIS2_PLACEMENT_3D('',#184752,#119105,#119106);
#101666=AXIS2_PLACEMENT_3D('',#184756,#119109,#119110);
#101667=AXIS2_PLACEMENT_3D('',#184759,#119111,#119112);
#101668=AXIS2_PLACEMENT_3D('',#184767,#119116,#119117);
#101669=AXIS2_PLACEMENT_3D('',#184773,#119120,#119121);
#101670=AXIS2_PLACEMENT_3D('',#184777,#119123,#119124);
#101671=AXIS2_PLACEMENT_3D('',#184781,#119127,#119128);
#101672=AXIS2_PLACEMENT_3D('',#184786,#119130,#119131);
#101673=AXIS2_PLACEMENT_3D('',#184789,#119133,#119134);
#101674=AXIS2_PLACEMENT_3D('',#184790,#119135,#119136);
#101675=AXIS2_PLACEMENT_3D('',#184793,#119137,#119138);
#101676=AXIS2_PLACEMENT_3D('',#184801,#119142,#119143);
#101677=AXIS2_PLACEMENT_3D('',#184807,#119146,#119147);
#101678=AXIS2_PLACEMENT_3D('',#184811,#119149,#119150);
#101679=AXIS2_PLACEMENT_3D('',#184815,#119153,#119154);
#101680=AXIS2_PLACEMENT_3D('',#184818,#119155,#119156);
#101681=AXIS2_PLACEMENT_3D('',#184826,#119160,#119161);
#101682=AXIS2_PLACEMENT_3D('',#184832,#119164,#119165);
#101683=AXIS2_PLACEMENT_3D('',#184836,#119167,#119168);
#101684=AXIS2_PLACEMENT_3D('',#184840,#119171,#119172);
#101685=AXIS2_PLACEMENT_3D('',#184845,#119174,#119175);
#101686=AXIS2_PLACEMENT_3D('',#184848,#119177,#119178);
#101687=AXIS2_PLACEMENT_3D('',#184849,#119179,#119180);
#101688=AXIS2_PLACEMENT_3D('',#184852,#119181,#119182);
#101689=AXIS2_PLACEMENT_3D('',#184860,#119186,#119187);
#101690=AXIS2_PLACEMENT_3D('',#184866,#119190,#119191);
#101691=AXIS2_PLACEMENT_3D('',#184870,#119193,#119194);
#101692=AXIS2_PLACEMENT_3D('',#184874,#119197,#119198);
#101693=AXIS2_PLACEMENT_3D('',#184877,#119199,#119200);
#101694=AXIS2_PLACEMENT_3D('',#184885,#119204,#119205);
#101695=AXIS2_PLACEMENT_3D('',#184891,#119208,#119209);
#101696=AXIS2_PLACEMENT_3D('',#184895,#119211,#119212);
#101697=AXIS2_PLACEMENT_3D('',#184899,#119215,#119216);
#101698=AXIS2_PLACEMENT_3D('',#184904,#119218,#119219);
#101699=AXIS2_PLACEMENT_3D('',#184907,#119221,#119222);
#101700=AXIS2_PLACEMENT_3D('',#184908,#119223,#119224);
#101701=AXIS2_PLACEMENT_3D('',#184911,#119225,#119226);
#101702=AXIS2_PLACEMENT_3D('',#184919,#119230,#119231);
#101703=AXIS2_PLACEMENT_3D('',#184925,#119234,#119235);
#101704=AXIS2_PLACEMENT_3D('',#184929,#119237,#119238);
#101705=AXIS2_PLACEMENT_3D('',#184933,#119241,#119242);
#101706=AXIS2_PLACEMENT_3D('',#184936,#119243,#119244);
#101707=AXIS2_PLACEMENT_3D('',#184944,#119248,#119249);
#101708=AXIS2_PLACEMENT_3D('',#184950,#119252,#119253);
#101709=AXIS2_PLACEMENT_3D('',#184954,#119255,#119256);
#101710=AXIS2_PLACEMENT_3D('',#184958,#119259,#119260);
#101711=AXIS2_PLACEMENT_3D('',#184963,#119262,#119263);
#101712=AXIS2_PLACEMENT_3D('',#184966,#119265,#119266);
#101713=AXIS2_PLACEMENT_3D('',#184967,#119267,#119268);
#101714=AXIS2_PLACEMENT_3D('',#184970,#119269,#119270);
#101715=AXIS2_PLACEMENT_3D('',#184978,#119274,#119275);
#101716=AXIS2_PLACEMENT_3D('',#184984,#119278,#119279);
#101717=AXIS2_PLACEMENT_3D('',#184988,#119281,#119282);
#101718=AXIS2_PLACEMENT_3D('',#184992,#119285,#119286);
#101719=AXIS2_PLACEMENT_3D('',#184995,#119287,#119288);
#101720=AXIS2_PLACEMENT_3D('',#185003,#119292,#119293);
#101721=AXIS2_PLACEMENT_3D('',#185009,#119296,#119297);
#101722=AXIS2_PLACEMENT_3D('',#185013,#119299,#119300);
#101723=AXIS2_PLACEMENT_3D('',#185017,#119303,#119304);
#101724=AXIS2_PLACEMENT_3D('',#185022,#119306,#119307);
#101725=AXIS2_PLACEMENT_3D('',#185025,#119309,#119310);
#101726=AXIS2_PLACEMENT_3D('',#185026,#119311,#119312);
#101727=AXIS2_PLACEMENT_3D('',#185029,#119313,#119314);
#101728=AXIS2_PLACEMENT_3D('',#185037,#119318,#119319);
#101729=AXIS2_PLACEMENT_3D('',#185043,#119322,#119323);
#101730=AXIS2_PLACEMENT_3D('',#185047,#119325,#119326);
#101731=AXIS2_PLACEMENT_3D('',#185051,#119329,#119330);
#101732=AXIS2_PLACEMENT_3D('',#185054,#119331,#119332);
#101733=AXIS2_PLACEMENT_3D('',#185062,#119336,#119337);
#101734=AXIS2_PLACEMENT_3D('',#185068,#119340,#119341);
#101735=AXIS2_PLACEMENT_3D('',#185072,#119343,#119344);
#101736=AXIS2_PLACEMENT_3D('',#185076,#119347,#119348);
#101737=AXIS2_PLACEMENT_3D('',#185079,#119351,#119352);
#101738=AXIS2_PLACEMENT_3D('',#185082,#119353,#119354);
#101739=AXIS2_PLACEMENT_3D('',#185090,#119358,#119359);
#101740=AXIS2_PLACEMENT_3D('',#185096,#119362,#119363);
#101741=AXIS2_PLACEMENT_3D('',#185100,#119365,#119366);
#101742=AXIS2_PLACEMENT_3D('',#185104,#119369,#119370);
#101743=AXIS2_PLACEMENT_3D('',#185107,#119371,#119372);
#101744=AXIS2_PLACEMENT_3D('',#185115,#119376,#119377);
#101745=AXIS2_PLACEMENT_3D('',#185121,#119380,#119381);
#101746=AXIS2_PLACEMENT_3D('',#185125,#119383,#119384);
#101747=AXIS2_PLACEMENT_3D('',#185129,#119387,#119388);
#101748=AXIS2_PLACEMENT_3D('',#185134,#119390,#119391);
#101749=AXIS2_PLACEMENT_3D('',#185137,#119393,#119394);
#101750=AXIS2_PLACEMENT_3D('',#185138,#119395,#119396);
#101751=AXIS2_PLACEMENT_3D('',#185141,#119397,#119398);
#101752=AXIS2_PLACEMENT_3D('',#185149,#119402,#119403);
#101753=AXIS2_PLACEMENT_3D('',#185155,#119406,#119407);
#101754=AXIS2_PLACEMENT_3D('',#185159,#119409,#119410);
#101755=AXIS2_PLACEMENT_3D('',#185163,#119413,#119414);
#101756=AXIS2_PLACEMENT_3D('',#185166,#119415,#119416);
#101757=AXIS2_PLACEMENT_3D('',#185174,#119420,#119421);
#101758=AXIS2_PLACEMENT_3D('',#185180,#119424,#119425);
#101759=AXIS2_PLACEMENT_3D('',#185184,#119427,#119428);
#101760=AXIS2_PLACEMENT_3D('',#185188,#119431,#119432);
#101761=AXIS2_PLACEMENT_3D('',#185193,#119434,#119435);
#101762=AXIS2_PLACEMENT_3D('',#185196,#119437,#119438);
#101763=AXIS2_PLACEMENT_3D('',#185197,#119439,#119440);
#101764=AXIS2_PLACEMENT_3D('',#185200,#119441,#119442);
#101765=AXIS2_PLACEMENT_3D('',#185208,#119446,#119447);
#101766=AXIS2_PLACEMENT_3D('',#185214,#119450,#119451);
#101767=AXIS2_PLACEMENT_3D('',#185218,#119453,#119454);
#101768=AXIS2_PLACEMENT_3D('',#185222,#119457,#119458);
#101769=AXIS2_PLACEMENT_3D('',#185225,#119459,#119460);
#101770=AXIS2_PLACEMENT_3D('',#185233,#119464,#119465);
#101771=AXIS2_PLACEMENT_3D('',#185239,#119468,#119469);
#101772=AXIS2_PLACEMENT_3D('',#185243,#119471,#119472);
#101773=AXIS2_PLACEMENT_3D('',#185247,#119475,#119476);
#101774=AXIS2_PLACEMENT_3D('',#185252,#119478,#119479);
#101775=AXIS2_PLACEMENT_3D('',#185255,#119481,#119482);
#101776=AXIS2_PLACEMENT_3D('',#185256,#119483,#119484);
#101777=AXIS2_PLACEMENT_3D('',#185259,#119485,#119486);
#101778=AXIS2_PLACEMENT_3D('',#185267,#119490,#119491);
#101779=AXIS2_PLACEMENT_3D('',#185273,#119494,#119495);
#101780=AXIS2_PLACEMENT_3D('',#185277,#119497,#119498);
#101781=AXIS2_PLACEMENT_3D('',#185281,#119501,#119502);
#101782=AXIS2_PLACEMENT_3D('',#185284,#119503,#119504);
#101783=AXIS2_PLACEMENT_3D('',#185292,#119508,#119509);
#101784=AXIS2_PLACEMENT_3D('',#185298,#119512,#119513);
#101785=AXIS2_PLACEMENT_3D('',#185302,#119515,#119516);
#101786=AXIS2_PLACEMENT_3D('',#185306,#119519,#119520);
#101787=AXIS2_PLACEMENT_3D('',#185311,#119522,#119523);
#101788=AXIS2_PLACEMENT_3D('',#185314,#119525,#119526);
#101789=AXIS2_PLACEMENT_3D('',#185315,#119527,#119528);
#101790=AXIS2_PLACEMENT_3D('',#185318,#119529,#119530);
#101791=AXIS2_PLACEMENT_3D('',#185326,#119534,#119535);
#101792=AXIS2_PLACEMENT_3D('',#185332,#119538,#119539);
#101793=AXIS2_PLACEMENT_3D('',#185336,#119541,#119542);
#101794=AXIS2_PLACEMENT_3D('',#185340,#119545,#119546);
#101795=AXIS2_PLACEMENT_3D('',#185343,#119547,#119548);
#101796=AXIS2_PLACEMENT_3D('',#185351,#119552,#119553);
#101797=AXIS2_PLACEMENT_3D('',#185357,#119556,#119557);
#101798=AXIS2_PLACEMENT_3D('',#185361,#119559,#119560);
#101799=AXIS2_PLACEMENT_3D('',#185365,#119563,#119564);
#101800=AXIS2_PLACEMENT_3D('',#185370,#119566,#119567);
#101801=AXIS2_PLACEMENT_3D('',#185373,#119569,#119570);
#101802=AXIS2_PLACEMENT_3D('',#185374,#119571,#119572);
#101803=AXIS2_PLACEMENT_3D('',#185377,#119573,#119574);
#101804=AXIS2_PLACEMENT_3D('',#185385,#119578,#119579);
#101805=AXIS2_PLACEMENT_3D('',#185391,#119582,#119583);
#101806=AXIS2_PLACEMENT_3D('',#185395,#119585,#119586);
#101807=AXIS2_PLACEMENT_3D('',#185399,#119589,#119590);
#101808=AXIS2_PLACEMENT_3D('',#185402,#119591,#119592);
#101809=AXIS2_PLACEMENT_3D('',#185410,#119596,#119597);
#101810=AXIS2_PLACEMENT_3D('',#185416,#119600,#119601);
#101811=AXIS2_PLACEMENT_3D('',#185420,#119603,#119604);
#101812=AXIS2_PLACEMENT_3D('',#185424,#119607,#119608);
#101813=AXIS2_PLACEMENT_3D('',#185429,#119610,#119611);
#101814=AXIS2_PLACEMENT_3D('',#185432,#119613,#119614);
#101815=AXIS2_PLACEMENT_3D('',#185433,#119615,#119616);
#101816=AXIS2_PLACEMENT_3D('',#185436,#119617,#119618);
#101817=AXIS2_PLACEMENT_3D('',#185444,#119622,#119623);
#101818=AXIS2_PLACEMENT_3D('',#185450,#119626,#119627);
#101819=AXIS2_PLACEMENT_3D('',#185454,#119629,#119630);
#101820=AXIS2_PLACEMENT_3D('',#185458,#119633,#119634);
#101821=AXIS2_PLACEMENT_3D('',#185461,#119635,#119636);
#101822=AXIS2_PLACEMENT_3D('',#185469,#119640,#119641);
#101823=AXIS2_PLACEMENT_3D('',#185475,#119644,#119645);
#101824=AXIS2_PLACEMENT_3D('',#185479,#119647,#119648);
#101825=AXIS2_PLACEMENT_3D('',#185483,#119651,#119652);
#101826=AXIS2_PLACEMENT_3D('',#185488,#119654,#119655);
#101827=AXIS2_PLACEMENT_3D('',#185491,#119657,#119658);
#101828=AXIS2_PLACEMENT_3D('',#185492,#119659,#119660);
#101829=AXIS2_PLACEMENT_3D('',#185495,#119661,#119662);
#101830=AXIS2_PLACEMENT_3D('',#185503,#119666,#119667);
#101831=AXIS2_PLACEMENT_3D('',#185509,#119670,#119671);
#101832=AXIS2_PLACEMENT_3D('',#185513,#119673,#119674);
#101833=AXIS2_PLACEMENT_3D('',#185517,#119677,#119678);
#101834=AXIS2_PLACEMENT_3D('',#185520,#119679,#119680);
#101835=AXIS2_PLACEMENT_3D('',#185528,#119684,#119685);
#101836=AXIS2_PLACEMENT_3D('',#185534,#119688,#119689);
#101837=AXIS2_PLACEMENT_3D('',#185538,#119691,#119692);
#101838=AXIS2_PLACEMENT_3D('',#185542,#119695,#119696);
#101839=AXIS2_PLACEMENT_3D('',#185547,#119698,#119699);
#101840=AXIS2_PLACEMENT_3D('',#185550,#119701,#119702);
#101841=AXIS2_PLACEMENT_3D('',#185551,#119703,#119704);
#101842=AXIS2_PLACEMENT_3D('',#185554,#119705,#119706);
#101843=AXIS2_PLACEMENT_3D('',#185562,#119710,#119711);
#101844=AXIS2_PLACEMENT_3D('',#185568,#119714,#119715);
#101845=AXIS2_PLACEMENT_3D('',#185572,#119717,#119718);
#101846=AXIS2_PLACEMENT_3D('',#185576,#119721,#119722);
#101847=AXIS2_PLACEMENT_3D('',#185579,#119723,#119724);
#101848=AXIS2_PLACEMENT_3D('',#185587,#119728,#119729);
#101849=AXIS2_PLACEMENT_3D('',#185593,#119732,#119733);
#101850=AXIS2_PLACEMENT_3D('',#185597,#119735,#119736);
#101851=AXIS2_PLACEMENT_3D('',#185601,#119739,#119740);
#101852=AXIS2_PLACEMENT_3D('',#185606,#119742,#119743);
#101853=AXIS2_PLACEMENT_3D('',#185609,#119745,#119746);
#101854=AXIS2_PLACEMENT_3D('',#185610,#119747,#119748);
#101855=AXIS2_PLACEMENT_3D('',#185613,#119749,#119750);
#101856=AXIS2_PLACEMENT_3D('',#185621,#119754,#119755);
#101857=AXIS2_PLACEMENT_3D('',#185627,#119758,#119759);
#101858=AXIS2_PLACEMENT_3D('',#185631,#119761,#119762);
#101859=AXIS2_PLACEMENT_3D('',#185635,#119765,#119766);
#101860=AXIS2_PLACEMENT_3D('',#185638,#119767,#119768);
#101861=AXIS2_PLACEMENT_3D('',#185646,#119772,#119773);
#101862=AXIS2_PLACEMENT_3D('',#185652,#119776,#119777);
#101863=AXIS2_PLACEMENT_3D('',#185656,#119779,#119780);
#101864=AXIS2_PLACEMENT_3D('',#185660,#119783,#119784);
#101865=AXIS2_PLACEMENT_3D('',#185665,#119786,#119787);
#101866=AXIS2_PLACEMENT_3D('',#185668,#119789,#119790);
#101867=AXIS2_PLACEMENT_3D('',#185669,#119791,#119792);
#101868=AXIS2_PLACEMENT_3D('',#185672,#119793,#119794);
#101869=AXIS2_PLACEMENT_3D('',#185680,#119798,#119799);
#101870=AXIS2_PLACEMENT_3D('',#185686,#119802,#119803);
#101871=AXIS2_PLACEMENT_3D('',#185690,#119805,#119806);
#101872=AXIS2_PLACEMENT_3D('',#185694,#119809,#119810);
#101873=AXIS2_PLACEMENT_3D('',#185697,#119811,#119812);
#101874=AXIS2_PLACEMENT_3D('',#185705,#119816,#119817);
#101875=AXIS2_PLACEMENT_3D('',#185711,#119820,#119821);
#101876=AXIS2_PLACEMENT_3D('',#185715,#119823,#119824);
#101877=AXIS2_PLACEMENT_3D('',#185719,#119827,#119828);
#101878=AXIS2_PLACEMENT_3D('',#185724,#119830,#119831);
#101879=AXIS2_PLACEMENT_3D('',#185727,#119833,#119834);
#101880=AXIS2_PLACEMENT_3D('',#185728,#119835,#119836);
#101881=AXIS2_PLACEMENT_3D('',#185731,#119837,#119838);
#101882=AXIS2_PLACEMENT_3D('',#185739,#119842,#119843);
#101883=AXIS2_PLACEMENT_3D('',#185745,#119846,#119847);
#101884=AXIS2_PLACEMENT_3D('',#185749,#119849,#119850);
#101885=AXIS2_PLACEMENT_3D('',#185753,#119853,#119854);
#101886=AXIS2_PLACEMENT_3D('',#185756,#119855,#119856);
#101887=AXIS2_PLACEMENT_3D('',#185764,#119860,#119861);
#101888=AXIS2_PLACEMENT_3D('',#185770,#119864,#119865);
#101889=AXIS2_PLACEMENT_3D('',#185774,#119867,#119868);
#101890=AXIS2_PLACEMENT_3D('',#185778,#119871,#119872);
#101891=AXIS2_PLACEMENT_3D('',#185783,#119874,#119875);
#101892=AXIS2_PLACEMENT_3D('',#185786,#119877,#119878);
#101893=AXIS2_PLACEMENT_3D('',#185787,#119879,#119880);
#101894=AXIS2_PLACEMENT_3D('',#185790,#119881,#119882);
#101895=AXIS2_PLACEMENT_3D('',#185798,#119886,#119887);
#101896=AXIS2_PLACEMENT_3D('',#185804,#119890,#119891);
#101897=AXIS2_PLACEMENT_3D('',#185808,#119893,#119894);
#101898=AXIS2_PLACEMENT_3D('',#185812,#119897,#119898);
#101899=AXIS2_PLACEMENT_3D('',#185815,#119899,#119900);
#101900=AXIS2_PLACEMENT_3D('',#185823,#119904,#119905);
#101901=AXIS2_PLACEMENT_3D('',#185829,#119908,#119909);
#101902=AXIS2_PLACEMENT_3D('',#185833,#119911,#119912);
#101903=AXIS2_PLACEMENT_3D('',#185837,#119915,#119916);
#101904=AXIS2_PLACEMENT_3D('',#185842,#119918,#119919);
#101905=AXIS2_PLACEMENT_3D('',#185845,#119921,#119922);
#101906=AXIS2_PLACEMENT_3D('',#185846,#119923,#119924);
#101907=AXIS2_PLACEMENT_3D('',#185849,#119925,#119926);
#101908=AXIS2_PLACEMENT_3D('',#185857,#119930,#119931);
#101909=AXIS2_PLACEMENT_3D('',#185863,#119934,#119935);
#101910=AXIS2_PLACEMENT_3D('',#185867,#119937,#119938);
#101911=AXIS2_PLACEMENT_3D('',#185871,#119941,#119942);
#101912=AXIS2_PLACEMENT_3D('',#185874,#119943,#119944);
#101913=AXIS2_PLACEMENT_3D('',#185882,#119948,#119949);
#101914=AXIS2_PLACEMENT_3D('',#185888,#119952,#119953);
#101915=AXIS2_PLACEMENT_3D('',#185892,#119955,#119956);
#101916=AXIS2_PLACEMENT_3D('',#185896,#119959,#119960);
#101917=AXIS2_PLACEMENT_3D('',#185901,#119962,#119963);
#101918=AXIS2_PLACEMENT_3D('',#185904,#119965,#119966);
#101919=AXIS2_PLACEMENT_3D('',#185905,#119967,#119968);
#101920=AXIS2_PLACEMENT_3D('',#185908,#119969,#119970);
#101921=AXIS2_PLACEMENT_3D('',#185916,#119974,#119975);
#101922=AXIS2_PLACEMENT_3D('',#185922,#119978,#119979);
#101923=AXIS2_PLACEMENT_3D('',#185926,#119981,#119982);
#101924=AXIS2_PLACEMENT_3D('',#185930,#119985,#119986);
#101925=AXIS2_PLACEMENT_3D('',#185933,#119987,#119988);
#101926=AXIS2_PLACEMENT_3D('',#185941,#119992,#119993);
#101927=AXIS2_PLACEMENT_3D('',#185947,#119996,#119997);
#101928=AXIS2_PLACEMENT_3D('',#185951,#119999,#120000);
#101929=AXIS2_PLACEMENT_3D('',#185955,#120003,#120004);
#101930=AXIS2_PLACEMENT_3D('',#186060,#120005,#120006);
#101931=AXIS2_PLACEMENT_3D('',#186159,#120007,#120008);
#101932=AXIS2_PLACEMENT_3D('',#186264,#120009,#120010);
#101933=AXIS2_PLACEMENT_3D('',#186363,#120011,#120012);
#101934=AXIS2_PLACEMENT_3D('',#186468,#120013,#120014);
#101935=AXIS2_PLACEMENT_3D('',#186567,#120015,#120016);
#101936=AXIS2_PLACEMENT_3D('',#186672,#120017,#120018);
#101937=AXIS2_PLACEMENT_3D('',#186771,#120019,#120020);
#101938=AXIS2_PLACEMENT_3D('',#186876,#120021,#120022);
#101939=AXIS2_PLACEMENT_3D('',#186975,#120023,#120024);
#101940=AXIS2_PLACEMENT_3D('',#187080,#120025,#120026);
#101941=AXIS2_PLACEMENT_3D('',#187179,#120027,#120028);
#101942=AXIS2_PLACEMENT_3D('',#187284,#120029,#120030);
#101943=AXIS2_PLACEMENT_3D('',#187383,#120031,#120032);
#101944=AXIS2_PLACEMENT_3D('',#187488,#120033,#120034);
#101945=AXIS2_PLACEMENT_3D('',#187587,#120035,#120036);
#101946=AXIS2_PLACEMENT_3D('',#187692,#120037,#120038);
#101947=AXIS2_PLACEMENT_3D('',#187791,#120039,#120040);
#101948=AXIS2_PLACEMENT_3D('',#187896,#120041,#120042);
#101949=AXIS2_PLACEMENT_3D('',#187995,#120043,#120044);
#101950=AXIS2_PLACEMENT_3D('',#188100,#120045,#120046);
#101951=AXIS2_PLACEMENT_3D('',#188199,#120047,#120048);
#101952=AXIS2_PLACEMENT_3D('',#188304,#120049,#120050);
#101953=AXIS2_PLACEMENT_3D('',#188403,#120051,#120052);
#101954=AXIS2_PLACEMENT_3D('',#188508,#120053,#120054);
#101955=AXIS2_PLACEMENT_3D('',#188607,#120055,#120056);
#101956=AXIS2_PLACEMENT_3D('',#188712,#120057,#120058);
#101957=AXIS2_PLACEMENT_3D('',#188811,#120059,#120060);
#101958=AXIS2_PLACEMENT_3D('',#188916,#120061,#120062);
#101959=AXIS2_PLACEMENT_3D('',#189015,#120063,#120064);
#101960=AXIS2_PLACEMENT_3D('',#189120,#120065,#120066);
#101961=AXIS2_PLACEMENT_3D('',#189219,#120067,#120068);
#101962=AXIS2_PLACEMENT_3D('',#189324,#120069,#120070);
#101963=AXIS2_PLACEMENT_3D('',#189423,#120071,#120072);
#101964=AXIS2_PLACEMENT_3D('',#189528,#120073,#120074);
#101965=AXIS2_PLACEMENT_3D('',#189627,#120075,#120076);
#101966=AXIS2_PLACEMENT_3D('',#189732,#120077,#120078);
#101967=AXIS2_PLACEMENT_3D('',#189831,#120079,#120080);
#101968=AXIS2_PLACEMENT_3D('',#189936,#120081,#120082);
#101969=AXIS2_PLACEMENT_3D('',#190035,#120083,#120084);
#101970=AXIS2_PLACEMENT_3D('',#190140,#120085,#120086);
#101971=AXIS2_PLACEMENT_3D('',#190239,#120087,#120088);
#101972=AXIS2_PLACEMENT_3D('',#190344,#120089,#120090);
#101973=AXIS2_PLACEMENT_3D('',#190443,#120091,#120092);
#101974=AXIS2_PLACEMENT_3D('',#190548,#120093,#120094);
#101975=AXIS2_PLACEMENT_3D('',#190647,#120095,#120096);
#101976=AXIS2_PLACEMENT_3D('',#190752,#120097,#120098);
#101977=AXIS2_PLACEMENT_3D('',#190851,#120099,#120100);
#101978=AXIS2_PLACEMENT_3D('',#190956,#120101,#120102);
#101979=AXIS2_PLACEMENT_3D('',#191055,#120103,#120104);
#101980=AXIS2_PLACEMENT_3D('',#191160,#120105,#120106);
#101981=AXIS2_PLACEMENT_3D('',#191259,#120107,#120108);
#101982=AXIS2_PLACEMENT_3D('',#191364,#120109,#120110);
#101983=AXIS2_PLACEMENT_3D('',#191463,#120111,#120112);
#101984=AXIS2_PLACEMENT_3D('',#191568,#120113,#120114);
#101985=AXIS2_PLACEMENT_3D('',#191667,#120115,#120116);
#101986=AXIS2_PLACEMENT_3D('',#191772,#120117,#120118);
#101987=AXIS2_PLACEMENT_3D('',#191871,#120119,#120120);
#101988=AXIS2_PLACEMENT_3D('',#191976,#120121,#120122);
#101989=AXIS2_PLACEMENT_3D('',#192075,#120123,#120124);
#101990=AXIS2_PLACEMENT_3D('',#192180,#120125,#120126);
#101991=AXIS2_PLACEMENT_3D('',#192279,#120127,#120128);
#101992=AXIS2_PLACEMENT_3D('',#192384,#120129,#120130);
#101993=AXIS2_PLACEMENT_3D('',#192483,#120131,#120132);
#101994=AXIS2_PLACEMENT_3D('',#192588,#120133,#120134);
#101995=AXIS2_PLACEMENT_3D('',#192687,#120135,#120136);
#101996=AXIS2_PLACEMENT_3D('',#192792,#120137,#120138);
#101997=AXIS2_PLACEMENT_3D('',#192891,#120139,#120140);
#101998=AXIS2_PLACEMENT_3D('',#192996,#120141,#120142);
#101999=AXIS2_PLACEMENT_3D('',#193095,#120143,#120144);
#102000=AXIS2_PLACEMENT_3D('',#193200,#120145,#120146);
#102001=AXIS2_PLACEMENT_3D('',#193299,#120147,#120148);
#102002=AXIS2_PLACEMENT_3D('',#193404,#120149,#120150);
#102003=AXIS2_PLACEMENT_3D('',#193503,#120151,#120152);
#102004=AXIS2_PLACEMENT_3D('',#193608,#120153,#120154);
#102005=AXIS2_PLACEMENT_3D('',#193707,#120155,#120156);
#102006=AXIS2_PLACEMENT_3D('',#193812,#120157,#120158);
#102007=AXIS2_PLACEMENT_3D('',#193911,#120159,#120160);
#102008=AXIS2_PLACEMENT_3D('',#194016,#120161,#120162);
#102009=AXIS2_PLACEMENT_3D('',#194115,#120163,#120164);
#102010=AXIS2_PLACEMENT_3D('',#194220,#120165,#120166);
#102011=AXIS2_PLACEMENT_3D('',#194319,#120167,#120168);
#102012=AXIS2_PLACEMENT_3D('',#194424,#120169,#120170);
#102013=AXIS2_PLACEMENT_3D('',#194523,#120171,#120172);
#102014=AXIS2_PLACEMENT_3D('',#194628,#120173,#120174);
#102015=AXIS2_PLACEMENT_3D('',#194727,#120175,#120176);
#102016=AXIS2_PLACEMENT_3D('',#194832,#120177,#120178);
#102017=AXIS2_PLACEMENT_3D('',#194931,#120179,#120180);
#102018=AXIS2_PLACEMENT_3D('',#195036,#120181,#120182);
#102019=AXIS2_PLACEMENT_3D('',#195135,#120183,#120184);
#102020=AXIS2_PLACEMENT_3D('',#195240,#120185,#120186);
#102021=AXIS2_PLACEMENT_3D('',#195339,#120187,#120188);
#102022=AXIS2_PLACEMENT_3D('',#195444,#120189,#120190);
#102023=AXIS2_PLACEMENT_3D('',#195543,#120191,#120192);
#102024=AXIS2_PLACEMENT_3D('',#195648,#120193,#120194);
#102025=AXIS2_PLACEMENT_3D('',#195747,#120195,#120196);
#102026=AXIS2_PLACEMENT_3D('',#195852,#120197,#120198);
#102027=AXIS2_PLACEMENT_3D('',#195951,#120199,#120200);
#102028=AXIS2_PLACEMENT_3D('',#196056,#120201,#120202);
#102029=AXIS2_PLACEMENT_3D('',#196155,#120203,#120204);
#102030=AXIS2_PLACEMENT_3D('',#196260,#120205,#120206);
#102031=AXIS2_PLACEMENT_3D('',#196359,#120207,#120208);
#102032=AXIS2_PLACEMENT_3D('',#196464,#120209,#120210);
#102033=AXIS2_PLACEMENT_3D('',#196563,#120211,#120212);
#102034=AXIS2_PLACEMENT_3D('',#196668,#120213,#120214);
#102035=AXIS2_PLACEMENT_3D('',#196767,#120215,#120216);
#102036=AXIS2_PLACEMENT_3D('',#196872,#120217,#120218);
#102037=AXIS2_PLACEMENT_3D('',#196971,#120219,#120220);
#102038=AXIS2_PLACEMENT_3D('',#197076,#120221,#120222);
#102039=AXIS2_PLACEMENT_3D('',#197175,#120223,#120224);
#102040=AXIS2_PLACEMENT_3D('',#197280,#120225,#120226);
#102041=AXIS2_PLACEMENT_3D('',#197379,#120227,#120228);
#102042=AXIS2_PLACEMENT_3D('',#197484,#120229,#120230);
#102043=AXIS2_PLACEMENT_3D('',#197583,#120231,#120232);
#102044=AXIS2_PLACEMENT_3D('',#197688,#120233,#120234);
#102045=AXIS2_PLACEMENT_3D('',#197787,#120235,#120236);
#102046=AXIS2_PLACEMENT_3D('',#197892,#120237,#120238);
#102047=AXIS2_PLACEMENT_3D('',#197991,#120239,#120240);
#102048=AXIS2_PLACEMENT_3D('',#197992,#120241,#120242);
#102049=AXIS2_PLACEMENT_3D('',#197993,#120243,#120244);
#102050=AXIS2_PLACEMENT_3D('',#198006,#120245,#120246);
#102051=AXIS2_PLACEMENT_3D('',#198007,#120247,#120248);
#102052=AXIS2_PLACEMENT_3D('',#198008,#120249,#120250);
#102053=AXIS2_PLACEMENT_3D('',#198009,#120251,#120252);
#102054=AXIS2_PLACEMENT_3D('',#198010,#120253,#120254);
#102055=AXIS2_PLACEMENT_3D('',#198023,#120255,#120256);
#102056=AXIS2_PLACEMENT_3D('',#198036,#120257,#120258);
#102057=AXIS2_PLACEMENT_3D('',#198037,#120259,#120260);
#102058=AXIS2_PLACEMENT_3D('',#198038,#120261,#120262);
#102059=AXIS2_PLACEMENT_3D('',#198039,#120263,#120264);
#102060=AXIS2_PLACEMENT_3D('',#198040,#120265,#120266);
#102061=AXIS2_PLACEMENT_3D('',#198059,#120267,#120268);
#102062=AXIS2_PLACEMENT_3D('',#198060,#120269,#120270);
#102063=AXIS2_PLACEMENT_3D('',#198061,#120271,#120272);
#102064=AXIS2_PLACEMENT_3D('',#198062,#120273,#120274);
#102065=AXIS2_PLACEMENT_3D('',#198063,#120275,#120276);
#102066=AXIS2_PLACEMENT_3D('',#198076,#120277,#120278);
#102067=AXIS2_PLACEMENT_3D('',#198095,#120279,#120280);
#102068=AXIS2_PLACEMENT_3D('',#198096,#120281,#120282);
#102069=AXIS2_PLACEMENT_3D('',#198097,#120283,#120284);
#102070=AXIS2_PLACEMENT_3D('',#198098,#120285,#120286);
#102071=AXIS2_PLACEMENT_3D('',#198099,#120287,#120288);
#102072=AXIS2_PLACEMENT_3D('',#198118,#120289,#120290);
#102073=AXIS2_PLACEMENT_3D('',#198131,#120291,#120292);
#102074=AXIS2_PLACEMENT_3D('',#198132,#120293,#120294);
#102075=AXIS2_PLACEMENT_3D('',#198133,#120295,#120296);
#102076=AXIS2_PLACEMENT_3D('',#198134,#120297,#120298);
#102077=AXIS2_PLACEMENT_3D('',#198135,#120299,#120300);
#102078=AXIS2_PLACEMENT_3D('',#198154,#120301,#120302);
#102079=AXIS2_PLACEMENT_3D('',#198155,#120303,#120304);
#102080=AXIS2_PLACEMENT_3D('',#198156,#120305,#120306);
#102081=AXIS2_PLACEMENT_3D('',#198157,#120307,#120308);
#102082=AXIS2_PLACEMENT_3D('',#198158,#120309,#120310);
#102083=AXIS2_PLACEMENT_3D('',#198171,#120311,#120312);
#102084=AXIS2_PLACEMENT_3D('',#198184,#120313,#120314);
#102085=AXIS2_PLACEMENT_3D('',#198185,#120315,#120316);
#102086=AXIS2_PLACEMENT_3D('',#198186,#120317,#120318);
#102087=AXIS2_PLACEMENT_3D('',#198187,#120319,#120320);
#102088=AXIS2_PLACEMENT_3D('',#198188,#120321,#120322);
#102089=AXIS2_PLACEMENT_3D('',#198201,#120323,#120324);
#102090=AXIS2_PLACEMENT_3D('',#198202,#120325,#120326);
#102091=AXIS2_PLACEMENT_3D('',#198203,#120327,#120328);
#102092=AXIS2_PLACEMENT_3D('',#198204,#120329,#120330);
#102093=AXIS2_PLACEMENT_3D('',#198205,#120331,#120332);
#102094=AXIS2_PLACEMENT_3D('',#198218,#120333,#120334);
#102095=AXIS2_PLACEMENT_3D('',#198219,#120335,#120336);
#102096=AXIS2_PLACEMENT_3D('',#198220,#120337,#120338);
#102097=AXIS2_PLACEMENT_3D('',#198221,#120339,#120340);
#102098=AXIS2_PLACEMENT_3D('',#198222,#120341,#120342);
#102099=AXIS2_PLACEMENT_3D('',#198235,#120343,#120344);
#102100=AXIS2_PLACEMENT_3D('',#198248,#120345,#120346);
#102101=AXIS2_PLACEMENT_3D('',#198249,#120347,#120348);
#102102=AXIS2_PLACEMENT_3D('',#198250,#120349,#120350);
#102103=AXIS2_PLACEMENT_3D('',#198251,#120351,#120352);
#102104=AXIS2_PLACEMENT_3D('',#198252,#120353,#120354);
#102105=AXIS2_PLACEMENT_3D('',#198271,#120355,#120356);
#102106=AXIS2_PLACEMENT_3D('',#198272,#120357,#120358);
#102107=AXIS2_PLACEMENT_3D('',#198273,#120359,#120360);
#102108=AXIS2_PLACEMENT_3D('',#198274,#120361,#120362);
#102109=AXIS2_PLACEMENT_3D('',#198275,#120363,#120364);
#102110=AXIS2_PLACEMENT_3D('',#198288,#120365,#120366);
#102111=AXIS2_PLACEMENT_3D('',#198307,#120367,#120368);
#102112=AXIS2_PLACEMENT_3D('',#198308,#120369,#120370);
#102113=AXIS2_PLACEMENT_3D('',#198309,#120371,#120372);
#102114=AXIS2_PLACEMENT_3D('',#198310,#120373,#120374);
#102115=AXIS2_PLACEMENT_3D('',#198311,#120375,#120376);
#102116=AXIS2_PLACEMENT_3D('',#198330,#120377,#120378);
#102117=AXIS2_PLACEMENT_3D('',#198343,#120379,#120380);
#102118=AXIS2_PLACEMENT_3D('',#198344,#120381,#120382);
#102119=AXIS2_PLACEMENT_3D('',#198345,#120383,#120384);
#102120=AXIS2_PLACEMENT_3D('',#198346,#120385,#120386);
#102121=AXIS2_PLACEMENT_3D('',#198347,#120387,#120388);
#102122=AXIS2_PLACEMENT_3D('',#198366,#120389,#120390);
#102123=AXIS2_PLACEMENT_3D('',#198367,#120391,#120392);
#102124=AXIS2_PLACEMENT_3D('',#198368,#120393,#120394);
#102125=AXIS2_PLACEMENT_3D('',#198369,#120395,#120396);
#102126=AXIS2_PLACEMENT_3D('',#198370,#120397,#120398);
#102127=AXIS2_PLACEMENT_3D('',#198383,#120399,#120400);
#102128=AXIS2_PLACEMENT_3D('',#198396,#120401,#120402);
#102129=AXIS2_PLACEMENT_3D('',#198397,#120403,#120404);
#102130=AXIS2_PLACEMENT_3D('',#198398,#120405,#120406);
#102131=AXIS2_PLACEMENT_3D('',#198399,#120407,#120408);
#102132=AXIS2_PLACEMENT_3D('',#198400,#120409,#120410);
#102133=AXIS2_PLACEMENT_3D('',#198413,#120411,#120412);
#102134=AXIS2_PLACEMENT_3D('',#198414,#120413,#120414);
#102135=AXIS2_PLACEMENT_3D('',#198415,#120415,#120416);
#102136=AXIS2_PLACEMENT_3D('',#198416,#120417,#120418);
#102137=AXIS2_PLACEMENT_3D('',#198417,#120419,#120420);
#102138=AXIS2_PLACEMENT_3D('',#198430,#120421,#120422);
#102139=AXIS2_PLACEMENT_3D('',#198431,#120423,#120424);
#102140=AXIS2_PLACEMENT_3D('',#198432,#120425,#120426);
#102141=AXIS2_PLACEMENT_3D('',#198433,#120427,#120428);
#102142=AXIS2_PLACEMENT_3D('',#198434,#120429,#120430);
#102143=AXIS2_PLACEMENT_3D('',#198447,#120431,#120432);
#102144=AXIS2_PLACEMENT_3D('',#198460,#120433,#120434);
#102145=AXIS2_PLACEMENT_3D('',#198461,#120435,#120436);
#102146=AXIS2_PLACEMENT_3D('',#198462,#120437,#120438);
#102147=AXIS2_PLACEMENT_3D('',#198463,#120439,#120440);
#102148=AXIS2_PLACEMENT_3D('',#198464,#120441,#120442);
#102149=AXIS2_PLACEMENT_3D('',#198483,#120443,#120444);
#102150=AXIS2_PLACEMENT_3D('',#198484,#120445,#120446);
#102151=AXIS2_PLACEMENT_3D('',#198485,#120447,#120448);
#102152=AXIS2_PLACEMENT_3D('',#198486,#120449,#120450);
#102153=AXIS2_PLACEMENT_3D('',#198487,#120451,#120452);
#102154=AXIS2_PLACEMENT_3D('',#198500,#120453,#120454);
#102155=AXIS2_PLACEMENT_3D('',#198519,#120455,#120456);
#102156=AXIS2_PLACEMENT_3D('',#198520,#120457,#120458);
#102157=AXIS2_PLACEMENT_3D('',#198521,#120459,#120460);
#102158=AXIS2_PLACEMENT_3D('',#198522,#120461,#120462);
#102159=AXIS2_PLACEMENT_3D('',#198523,#120463,#120464);
#102160=AXIS2_PLACEMENT_3D('',#198542,#120465,#120466);
#102161=AXIS2_PLACEMENT_3D('',#198555,#120467,#120468);
#102162=AXIS2_PLACEMENT_3D('',#198556,#120469,#120470);
#102163=AXIS2_PLACEMENT_3D('',#198557,#120471,#120472);
#102164=AXIS2_PLACEMENT_3D('',#198558,#120473,#120474);
#102165=AXIS2_PLACEMENT_3D('',#198559,#120475,#120476);
#102166=AXIS2_PLACEMENT_3D('',#198578,#120477,#120478);
#102167=AXIS2_PLACEMENT_3D('',#198579,#120479,#120480);
#102168=AXIS2_PLACEMENT_3D('',#198580,#120481,#120482);
#102169=AXIS2_PLACEMENT_3D('',#198581,#120483,#120484);
#102170=AXIS2_PLACEMENT_3D('',#198582,#120485,#120486);
#102171=AXIS2_PLACEMENT_3D('',#198595,#120487,#120488);
#102172=AXIS2_PLACEMENT_3D('',#198608,#120489,#120490);
#102173=AXIS2_PLACEMENT_3D('',#198609,#120491,#120492);
#102174=AXIS2_PLACEMENT_3D('',#198610,#120493,#120494);
#102175=AXIS2_PLACEMENT_3D('',#198611,#120495,#120496);
#102176=AXIS2_PLACEMENT_3D('',#198612,#120497,#120498);
#102177=AXIS2_PLACEMENT_3D('',#198625,#120499,#120500);
#102178=AXIS2_PLACEMENT_3D('',#198626,#120501,#120502);
#102179=AXIS2_PLACEMENT_3D('',#198627,#120503,#120504);
#102180=AXIS2_PLACEMENT_3D('',#198628,#120505,#120506);
#102181=AXIS2_PLACEMENT_3D('',#198629,#120507,#120508);
#102182=AXIS2_PLACEMENT_3D('',#198642,#120509,#120510);
#102183=AXIS2_PLACEMENT_3D('',#198643,#120511,#120512);
#102184=AXIS2_PLACEMENT_3D('',#198644,#120513,#120514);
#102185=AXIS2_PLACEMENT_3D('',#198645,#120515,#120516);
#102186=AXIS2_PLACEMENT_3D('',#198646,#120517,#120518);
#102187=AXIS2_PLACEMENT_3D('',#198659,#120519,#120520);
#102188=AXIS2_PLACEMENT_3D('',#198672,#120521,#120522);
#102189=AXIS2_PLACEMENT_3D('',#198673,#120523,#120524);
#102190=AXIS2_PLACEMENT_3D('',#198674,#120525,#120526);
#102191=AXIS2_PLACEMENT_3D('',#198675,#120527,#120528);
#102192=AXIS2_PLACEMENT_3D('',#198676,#120529,#120530);
#102193=AXIS2_PLACEMENT_3D('',#198695,#120531,#120532);
#102194=AXIS2_PLACEMENT_3D('',#198696,#120533,#120534);
#102195=AXIS2_PLACEMENT_3D('',#198697,#120535,#120536);
#102196=AXIS2_PLACEMENT_3D('',#198698,#120537,#120538);
#102197=AXIS2_PLACEMENT_3D('',#198699,#120539,#120540);
#102198=AXIS2_PLACEMENT_3D('',#198712,#120541,#120542);
#102199=AXIS2_PLACEMENT_3D('',#198731,#120543,#120544);
#102200=AXIS2_PLACEMENT_3D('',#198732,#120545,#120546);
#102201=AXIS2_PLACEMENT_3D('',#198733,#120547,#120548);
#102202=AXIS2_PLACEMENT_3D('',#198734,#120549,#120550);
#102203=AXIS2_PLACEMENT_3D('',#198735,#120551,#120552);
#102204=AXIS2_PLACEMENT_3D('',#198754,#120553,#120554);
#102205=AXIS2_PLACEMENT_3D('',#198767,#120555,#120556);
#102206=AXIS2_PLACEMENT_3D('',#198768,#120557,#120558);
#102207=AXIS2_PLACEMENT_3D('',#198769,#120559,#120560);
#102208=AXIS2_PLACEMENT_3D('',#198770,#120561,#120562);
#102209=AXIS2_PLACEMENT_3D('',#198771,#120563,#120564);
#102210=AXIS2_PLACEMENT_3D('',#198790,#120565,#120566);
#102211=AXIS2_PLACEMENT_3D('',#198791,#120567,#120568);
#102212=AXIS2_PLACEMENT_3D('',#198792,#120569,#120570);
#102213=AXIS2_PLACEMENT_3D('',#198793,#120571,#120572);
#102214=AXIS2_PLACEMENT_3D('',#198794,#120573,#120574);
#102215=AXIS2_PLACEMENT_3D('',#198807,#120575,#120576);
#102216=AXIS2_PLACEMENT_3D('',#198820,#120577,#120578);
#102217=AXIS2_PLACEMENT_3D('',#198821,#120579,#120580);
#102218=AXIS2_PLACEMENT_3D('',#198822,#120581,#120582);
#102219=AXIS2_PLACEMENT_3D('',#198823,#120583,#120584);
#102220=AXIS2_PLACEMENT_3D('',#198824,#120585,#120586);
#102221=AXIS2_PLACEMENT_3D('',#198837,#120587,#120588);
#102222=AXIS2_PLACEMENT_3D('',#198838,#120589,#120590);
#102223=AXIS2_PLACEMENT_3D('',#198839,#120591,#120592);
#102224=AXIS2_PLACEMENT_3D('',#198840,#120593,#120594);
#102225=AXIS2_PLACEMENT_3D('',#198841,#120595,#120596);
#102226=AXIS2_PLACEMENT_3D('',#198854,#120597,#120598);
#102227=AXIS2_PLACEMENT_3D('',#198855,#120599,#120600);
#102228=AXIS2_PLACEMENT_3D('',#198856,#120601,#120602);
#102229=AXIS2_PLACEMENT_3D('',#198857,#120603,#120604);
#102230=AXIS2_PLACEMENT_3D('',#198858,#120605,#120606);
#102231=AXIS2_PLACEMENT_3D('',#198871,#120607,#120608);
#102232=AXIS2_PLACEMENT_3D('',#198884,#120609,#120610);
#102233=AXIS2_PLACEMENT_3D('',#198885,#120611,#120612);
#102234=AXIS2_PLACEMENT_3D('',#198886,#120613,#120614);
#102235=AXIS2_PLACEMENT_3D('',#198887,#120615,#120616);
#102236=AXIS2_PLACEMENT_3D('',#198888,#120617,#120618);
#102237=AXIS2_PLACEMENT_3D('',#198907,#120619,#120620);
#102238=AXIS2_PLACEMENT_3D('',#198908,#120621,#120622);
#102239=AXIS2_PLACEMENT_3D('',#198909,#120623,#120624);
#102240=AXIS2_PLACEMENT_3D('',#198910,#120625,#120626);
#102241=AXIS2_PLACEMENT_3D('',#198911,#120627,#120628);
#102242=AXIS2_PLACEMENT_3D('',#198924,#120629,#120630);
#102243=AXIS2_PLACEMENT_3D('',#198943,#120631,#120632);
#102244=AXIS2_PLACEMENT_3D('',#198944,#120633,#120634);
#102245=AXIS2_PLACEMENT_3D('',#198945,#120635,#120636);
#102246=AXIS2_PLACEMENT_3D('',#198946,#120637,#120638);
#102247=AXIS2_PLACEMENT_3D('',#198947,#120639,#120640);
#102248=AXIS2_PLACEMENT_3D('',#198966,#120641,#120642);
#102249=AXIS2_PLACEMENT_3D('',#198979,#120643,#120644);
#102250=AXIS2_PLACEMENT_3D('',#198980,#120645,#120646);
#102251=AXIS2_PLACEMENT_3D('',#198981,#120647,#120648);
#102252=AXIS2_PLACEMENT_3D('',#198982,#120649,#120650);
#102253=AXIS2_PLACEMENT_3D('',#198983,#120651,#120652);
#102254=AXIS2_PLACEMENT_3D('',#199002,#120653,#120654);
#102255=AXIS2_PLACEMENT_3D('',#199003,#120655,#120656);
#102256=AXIS2_PLACEMENT_3D('',#199004,#120657,#120658);
#102257=AXIS2_PLACEMENT_3D('',#199005,#120659,#120660);
#102258=AXIS2_PLACEMENT_3D('',#199006,#120661,#120662);
#102259=AXIS2_PLACEMENT_3D('',#199019,#120663,#120664);
#102260=AXIS2_PLACEMENT_3D('',#199032,#120665,#120666);
#102261=AXIS2_PLACEMENT_3D('',#199033,#120667,#120668);
#102262=AXIS2_PLACEMENT_3D('',#199034,#120669,#120670);
#102263=AXIS2_PLACEMENT_3D('',#199035,#120671,#120672);
#102264=AXIS2_PLACEMENT_3D('',#199036,#120673,#120674);
#102265=AXIS2_PLACEMENT_3D('',#199049,#120675,#120676);
#102266=AXIS2_PLACEMENT_3D('',#199050,#120677,#120678);
#102267=AXIS2_PLACEMENT_3D('',#199051,#120679,#120680);
#102268=AXIS2_PLACEMENT_3D('',#199052,#120681,#120682);
#102269=AXIS2_PLACEMENT_3D('',#199053,#120683,#120684);
#102270=AXIS2_PLACEMENT_3D('',#199066,#120685,#120686);
#102271=AXIS2_PLACEMENT_3D('',#199067,#120687,#120688);
#102272=AXIS2_PLACEMENT_3D('',#199068,#120689,#120690);
#102273=AXIS2_PLACEMENT_3D('',#199069,#120691,#120692);
#102274=AXIS2_PLACEMENT_3D('',#199070,#120693,#120694);
#102275=AXIS2_PLACEMENT_3D('',#199083,#120695,#120696);
#102276=AXIS2_PLACEMENT_3D('',#199096,#120697,#120698);
#102277=AXIS2_PLACEMENT_3D('',#199097,#120699,#120700);
#102278=AXIS2_PLACEMENT_3D('',#199098,#120701,#120702);
#102279=AXIS2_PLACEMENT_3D('',#199099,#120703,#120704);
#102280=AXIS2_PLACEMENT_3D('',#199100,#120705,#120706);
#102281=AXIS2_PLACEMENT_3D('',#199119,#120707,#120708);
#102282=AXIS2_PLACEMENT_3D('',#199120,#120709,#120710);
#102283=AXIS2_PLACEMENT_3D('',#199121,#120711,#120712);
#102284=AXIS2_PLACEMENT_3D('',#199122,#120713,#120714);
#102285=AXIS2_PLACEMENT_3D('',#199123,#120715,#120716);
#102286=AXIS2_PLACEMENT_3D('',#199136,#120717,#120718);
#102287=AXIS2_PLACEMENT_3D('',#199155,#120719,#120720);
#102288=AXIS2_PLACEMENT_3D('',#199156,#120721,#120722);
#102289=AXIS2_PLACEMENT_3D('',#199157,#120723,#120724);
#102290=AXIS2_PLACEMENT_3D('',#199158,#120725,#120726);
#102291=AXIS2_PLACEMENT_3D('',#199159,#120727,#120728);
#102292=AXIS2_PLACEMENT_3D('',#199178,#120729,#120730);
#102293=AXIS2_PLACEMENT_3D('',#199191,#120731,#120732);
#102294=AXIS2_PLACEMENT_3D('',#199192,#120733,#120734);
#102295=AXIS2_PLACEMENT_3D('',#199193,#120735,#120736);
#102296=AXIS2_PLACEMENT_3D('',#199194,#120737,#120738);
#102297=AXIS2_PLACEMENT_3D('',#199195,#120739,#120740);
#102298=AXIS2_PLACEMENT_3D('',#199214,#120741,#120742);
#102299=AXIS2_PLACEMENT_3D('',#199215,#120743,#120744);
#102300=AXIS2_PLACEMENT_3D('',#199216,#120745,#120746);
#102301=AXIS2_PLACEMENT_3D('',#199217,#120747,#120748);
#102302=AXIS2_PLACEMENT_3D('',#199218,#120749,#120750);
#102303=AXIS2_PLACEMENT_3D('',#199231,#120751,#120752);
#102304=AXIS2_PLACEMENT_3D('',#199244,#120753,#120754);
#102305=AXIS2_PLACEMENT_3D('',#199245,#120755,#120756);
#102306=AXIS2_PLACEMENT_3D('',#199246,#120757,#120758);
#102307=AXIS2_PLACEMENT_3D('',#199247,#120759,#120760);
#102308=AXIS2_PLACEMENT_3D('',#199248,#120761,#120762);
#102309=AXIS2_PLACEMENT_3D('',#199261,#120763,#120764);
#102310=AXIS2_PLACEMENT_3D('',#199262,#120765,#120766);
#102311=AXIS2_PLACEMENT_3D('',#199263,#120767,#120768);
#102312=AXIS2_PLACEMENT_3D('',#199264,#120769,#120770);
#102313=AXIS2_PLACEMENT_3D('',#199265,#120771,#120772);
#102314=AXIS2_PLACEMENT_3D('',#199278,#120773,#120774);
#102315=AXIS2_PLACEMENT_3D('',#199279,#120775,#120776);
#102316=AXIS2_PLACEMENT_3D('',#199280,#120777,#120778);
#102317=AXIS2_PLACEMENT_3D('',#199281,#120779,#120780);
#102318=AXIS2_PLACEMENT_3D('',#199282,#120781,#120782);
#102319=AXIS2_PLACEMENT_3D('',#199295,#120783,#120784);
#102320=AXIS2_PLACEMENT_3D('',#199308,#120785,#120786);
#102321=AXIS2_PLACEMENT_3D('',#199309,#120787,#120788);
#102322=AXIS2_PLACEMENT_3D('',#199310,#120789,#120790);
#102323=AXIS2_PLACEMENT_3D('',#199311,#120791,#120792);
#102324=AXIS2_PLACEMENT_3D('',#199312,#120793,#120794);
#102325=AXIS2_PLACEMENT_3D('',#199331,#120795,#120796);
#102326=AXIS2_PLACEMENT_3D('',#199332,#120797,#120798);
#102327=AXIS2_PLACEMENT_3D('',#199333,#120799,#120800);
#102328=AXIS2_PLACEMENT_3D('',#199334,#120801,#120802);
#102329=AXIS2_PLACEMENT_3D('',#199335,#120803,#120804);
#102330=AXIS2_PLACEMENT_3D('',#199348,#120805,#120806);
#102331=AXIS2_PLACEMENT_3D('',#199367,#120807,#120808);
#102332=AXIS2_PLACEMENT_3D('',#199368,#120809,#120810);
#102333=AXIS2_PLACEMENT_3D('',#199369,#120811,#120812);
#102334=AXIS2_PLACEMENT_3D('',#199370,#120813,#120814);
#102335=AXIS2_PLACEMENT_3D('',#199371,#120815,#120816);
#102336=AXIS2_PLACEMENT_3D('',#199390,#120817,#120818);
#102337=AXIS2_PLACEMENT_3D('',#199403,#120819,#120820);
#102338=AXIS2_PLACEMENT_3D('',#199404,#120821,#120822);
#102339=AXIS2_PLACEMENT_3D('',#199405,#120823,#120824);
#102340=AXIS2_PLACEMENT_3D('',#199406,#120825,#120826);
#102341=AXIS2_PLACEMENT_3D('',#199407,#120827,#120828);
#102342=AXIS2_PLACEMENT_3D('',#199426,#120829,#120830);
#102343=AXIS2_PLACEMENT_3D('',#199427,#120831,#120832);
#102344=AXIS2_PLACEMENT_3D('',#199428,#120833,#120834);
#102345=AXIS2_PLACEMENT_3D('',#199429,#120835,#120836);
#102346=AXIS2_PLACEMENT_3D('',#199430,#120837,#120838);
#102347=AXIS2_PLACEMENT_3D('',#199443,#120839,#120840);
#102348=AXIS2_PLACEMENT_3D('',#199456,#120841,#120842);
#102349=AXIS2_PLACEMENT_3D('',#199457,#120843,#120844);
#102350=AXIS2_PLACEMENT_3D('',#199458,#120845,#120846);
#102351=AXIS2_PLACEMENT_3D('',#199459,#120847,#120848);
#102352=AXIS2_PLACEMENT_3D('',#199460,#120849,#120850);
#102353=AXIS2_PLACEMENT_3D('',#199473,#120851,#120852);
#102354=AXIS2_PLACEMENT_3D('',#199474,#120853,#120854);
#102355=AXIS2_PLACEMENT_3D('',#199475,#120855,#120856);
#102356=AXIS2_PLACEMENT_3D('',#199476,#120857,#120858);
#102357=AXIS2_PLACEMENT_3D('',#199477,#120859,#120860);
#102358=AXIS2_PLACEMENT_3D('',#199490,#120861,#120862);
#102359=AXIS2_PLACEMENT_3D('',#199491,#120863,#120864);
#102360=AXIS2_PLACEMENT_3D('',#199492,#120865,#120866);
#102361=AXIS2_PLACEMENT_3D('',#199493,#120867,#120868);
#102362=AXIS2_PLACEMENT_3D('',#199494,#120869,#120870);
#102363=AXIS2_PLACEMENT_3D('',#199507,#120871,#120872);
#102364=AXIS2_PLACEMENT_3D('',#199520,#120873,#120874);
#102365=AXIS2_PLACEMENT_3D('',#199521,#120875,#120876);
#102366=AXIS2_PLACEMENT_3D('',#199522,#120877,#120878);
#102367=AXIS2_PLACEMENT_3D('',#199523,#120879,#120880);
#102368=AXIS2_PLACEMENT_3D('',#199524,#120881,#120882);
#102369=AXIS2_PLACEMENT_3D('',#199543,#120883,#120884);
#102370=AXIS2_PLACEMENT_3D('',#199544,#120885,#120886);
#102371=AXIS2_PLACEMENT_3D('',#199545,#120887,#120888);
#102372=AXIS2_PLACEMENT_3D('',#199546,#120889,#120890);
#102373=AXIS2_PLACEMENT_3D('',#199547,#120891,#120892);
#102374=AXIS2_PLACEMENT_3D('',#199560,#120893,#120894);
#102375=AXIS2_PLACEMENT_3D('',#199579,#120895,#120896);
#102376=AXIS2_PLACEMENT_3D('',#199580,#120897,#120898);
#102377=AXIS2_PLACEMENT_3D('',#199581,#120899,#120900);
#102378=AXIS2_PLACEMENT_3D('',#199582,#120901,#120902);
#102379=AXIS2_PLACEMENT_3D('',#199583,#120903,#120904);
#102380=AXIS2_PLACEMENT_3D('',#199602,#120905,#120906);
#102381=AXIS2_PLACEMENT_3D('',#199615,#120907,#120908);
#102382=AXIS2_PLACEMENT_3D('',#199616,#120909,#120910);
#102383=AXIS2_PLACEMENT_3D('',#199617,#120911,#120912);
#102384=AXIS2_PLACEMENT_3D('',#199618,#120913,#120914);
#102385=AXIS2_PLACEMENT_3D('',#199619,#120915,#120916);
#102386=AXIS2_PLACEMENT_3D('',#199638,#120917,#120918);
#102387=AXIS2_PLACEMENT_3D('',#199639,#120919,#120920);
#102388=AXIS2_PLACEMENT_3D('',#199640,#120921,#120922);
#102389=AXIS2_PLACEMENT_3D('',#199641,#120923,#120924);
#102390=AXIS2_PLACEMENT_3D('',#199642,#120925,#120926);
#102391=AXIS2_PLACEMENT_3D('',#199655,#120927,#120928);
#102392=AXIS2_PLACEMENT_3D('',#199668,#120929,#120930);
#102393=AXIS2_PLACEMENT_3D('',#199669,#120931,#120932);
#102394=AXIS2_PLACEMENT_3D('',#199670,#120933,#120934);
#102395=AXIS2_PLACEMENT_3D('',#199671,#120935,#120936);
#102396=AXIS2_PLACEMENT_3D('',#199672,#120937,#120938);
#102397=AXIS2_PLACEMENT_3D('',#199685,#120939,#120940);
#102398=AXIS2_PLACEMENT_3D('',#199686,#120941,#120942);
#102399=AXIS2_PLACEMENT_3D('',#199687,#120943,#120944);
#102400=AXIS2_PLACEMENT_3D('',#199688,#120945,#120946);
#102401=AXIS2_PLACEMENT_3D('',#199689,#120947,#120948);
#102402=AXIS2_PLACEMENT_3D('',#199702,#120949,#120950);
#102403=AXIS2_PLACEMENT_3D('',#199703,#120951,#120952);
#102404=AXIS2_PLACEMENT_3D('',#199704,#120953,#120954);
#102405=AXIS2_PLACEMENT_3D('',#199705,#120955,#120956);
#102406=AXIS2_PLACEMENT_3D('',#199706,#120957,#120958);
#102407=AXIS2_PLACEMENT_3D('',#199719,#120959,#120960);
#102408=AXIS2_PLACEMENT_3D('',#199732,#120961,#120962);
#102409=AXIS2_PLACEMENT_3D('',#199733,#120963,#120964);
#102410=AXIS2_PLACEMENT_3D('',#199734,#120965,#120966);
#102411=AXIS2_PLACEMENT_3D('',#199735,#120967,#120968);
#102412=AXIS2_PLACEMENT_3D('',#199736,#120969,#120970);
#102413=AXIS2_PLACEMENT_3D('',#199755,#120971,#120972);
#102414=AXIS2_PLACEMENT_3D('',#199756,#120973,#120974);
#102415=AXIS2_PLACEMENT_3D('',#199757,#120975,#120976);
#102416=AXIS2_PLACEMENT_3D('',#199758,#120977,#120978);
#102417=AXIS2_PLACEMENT_3D('',#199759,#120979,#120980);
#102418=AXIS2_PLACEMENT_3D('',#199772,#120981,#120982);
#102419=AXIS2_PLACEMENT_3D('',#199791,#120983,#120984);
#102420=AXIS2_PLACEMENT_3D('',#199792,#120985,#120986);
#102421=AXIS2_PLACEMENT_3D('',#199793,#120987,#120988);
#102422=AXIS2_PLACEMENT_3D('',#199794,#120989,#120990);
#102423=AXIS2_PLACEMENT_3D('',#199795,#120991,#120992);
#102424=AXIS2_PLACEMENT_3D('',#199814,#120993,#120994);
#102425=AXIS2_PLACEMENT_3D('',#199827,#120995,#120996);
#102426=AXIS2_PLACEMENT_3D('',#199828,#120997,#120998);
#102427=AXIS2_PLACEMENT_3D('',#199829,#120999,#121000);
#102428=AXIS2_PLACEMENT_3D('',#199830,#121001,#121002);
#102429=AXIS2_PLACEMENT_3D('',#199831,#121003,#121004);
#102430=AXIS2_PLACEMENT_3D('',#199850,#121005,#121006);
#102431=AXIS2_PLACEMENT_3D('',#199851,#121007,#121008);
#102432=AXIS2_PLACEMENT_3D('',#199852,#121009,#121010);
#102433=AXIS2_PLACEMENT_3D('',#199853,#121011,#121012);
#102434=AXIS2_PLACEMENT_3D('',#199854,#121013,#121014);
#102435=AXIS2_PLACEMENT_3D('',#199867,#121015,#121016);
#102436=AXIS2_PLACEMENT_3D('',#199880,#121017,#121018);
#102437=AXIS2_PLACEMENT_3D('',#199881,#121019,#121020);
#102438=AXIS2_PLACEMENT_3D('',#199882,#121021,#121022);
#102439=AXIS2_PLACEMENT_3D('',#199883,#121023,#121024);
#102440=AXIS2_PLACEMENT_3D('',#199884,#121025,#121026);
#102441=AXIS2_PLACEMENT_3D('',#199897,#121027,#121028);
#102442=AXIS2_PLACEMENT_3D('',#199898,#121029,#121030);
#102443=AXIS2_PLACEMENT_3D('',#199899,#121031,#121032);
#102444=AXIS2_PLACEMENT_3D('',#199900,#121033,#121034);
#102445=AXIS2_PLACEMENT_3D('',#199901,#121035,#121036);
#102446=AXIS2_PLACEMENT_3D('',#199914,#121037,#121038);
#102447=AXIS2_PLACEMENT_3D('',#199915,#121039,#121040);
#102448=AXIS2_PLACEMENT_3D('',#199916,#121041,#121042);
#102449=AXIS2_PLACEMENT_3D('',#199917,#121043,#121044);
#102450=AXIS2_PLACEMENT_3D('',#199918,#121045,#121046);
#102451=AXIS2_PLACEMENT_3D('',#199931,#121047,#121048);
#102452=AXIS2_PLACEMENT_3D('',#199944,#121049,#121050);
#102453=AXIS2_PLACEMENT_3D('',#199945,#121051,#121052);
#102454=AXIS2_PLACEMENT_3D('',#199946,#121053,#121054);
#102455=AXIS2_PLACEMENT_3D('',#199947,#121055,#121056);
#102456=AXIS2_PLACEMENT_3D('',#199948,#121057,#121058);
#102457=AXIS2_PLACEMENT_3D('',#199967,#121059,#121060);
#102458=AXIS2_PLACEMENT_3D('',#199968,#121061,#121062);
#102459=AXIS2_PLACEMENT_3D('',#199969,#121063,#121064);
#102460=AXIS2_PLACEMENT_3D('',#199970,#121065,#121066);
#102461=AXIS2_PLACEMENT_3D('',#199971,#121067,#121068);
#102462=AXIS2_PLACEMENT_3D('',#199984,#121069,#121070);
#102463=AXIS2_PLACEMENT_3D('',#200003,#121071,#121072);
#102464=AXIS2_PLACEMENT_3D('',#200004,#121073,#121074);
#102465=AXIS2_PLACEMENT_3D('',#200005,#121075,#121076);
#102466=AXIS2_PLACEMENT_3D('',#200006,#121077,#121078);
#102467=AXIS2_PLACEMENT_3D('',#200007,#121079,#121080);
#102468=AXIS2_PLACEMENT_3D('',#200026,#121081,#121082);
#102469=AXIS2_PLACEMENT_3D('',#200039,#121083,#121084);
#102470=AXIS2_PLACEMENT_3D('',#200040,#121085,#121086);
#102471=AXIS2_PLACEMENT_3D('',#200041,#121087,#121088);
#102472=AXIS2_PLACEMENT_3D('',#200042,#121089,#121090);
#102473=AXIS2_PLACEMENT_3D('',#200043,#121091,#121092);
#102474=AXIS2_PLACEMENT_3D('',#200062,#121093,#121094);
#102475=AXIS2_PLACEMENT_3D('',#200063,#121095,#121096);
#102476=AXIS2_PLACEMENT_3D('',#200064,#121097,#121098);
#102477=AXIS2_PLACEMENT_3D('',#200065,#121099,#121100);
#102478=AXIS2_PLACEMENT_3D('',#200066,#121101,#121102);
#102479=AXIS2_PLACEMENT_3D('',#200079,#121103,#121104);
#102480=AXIS2_PLACEMENT_3D('',#200092,#121105,#121106);
#102481=AXIS2_PLACEMENT_3D('',#200093,#121107,#121108);
#102482=AXIS2_PLACEMENT_3D('',#200094,#121109,#121110);
#102483=AXIS2_PLACEMENT_3D('',#200095,#121111,#121112);
#102484=AXIS2_PLACEMENT_3D('',#200096,#121113,#121114);
#102485=AXIS2_PLACEMENT_3D('',#200109,#121115,#121116);
#102486=AXIS2_PLACEMENT_3D('',#200110,#121117,#121118);
#102487=AXIS2_PLACEMENT_3D('',#200111,#121119,#121120);
#102488=AXIS2_PLACEMENT_3D('',#200112,#121121,#121122);
#102489=AXIS2_PLACEMENT_3D('',#200113,#121123,#121124);
#102490=AXIS2_PLACEMENT_3D('',#200126,#121125,#121126);
#102491=AXIS2_PLACEMENT_3D('',#200127,#121127,#121128);
#102492=AXIS2_PLACEMENT_3D('',#200128,#121129,#121130);
#102493=AXIS2_PLACEMENT_3D('',#200129,#121131,#121132);
#102494=AXIS2_PLACEMENT_3D('',#200130,#121133,#121134);
#102495=AXIS2_PLACEMENT_3D('',#200143,#121135,#121136);
#102496=AXIS2_PLACEMENT_3D('',#200156,#121137,#121138);
#102497=AXIS2_PLACEMENT_3D('',#200157,#121139,#121140);
#102498=AXIS2_PLACEMENT_3D('',#200158,#121141,#121142);
#102499=AXIS2_PLACEMENT_3D('',#200159,#121143,#121144);
#102500=AXIS2_PLACEMENT_3D('',#200160,#121145,#121146);
#102501=AXIS2_PLACEMENT_3D('',#200179,#121147,#121148);
#102502=AXIS2_PLACEMENT_3D('',#200180,#121149,#121150);
#102503=AXIS2_PLACEMENT_3D('',#200181,#121151,#121152);
#102504=AXIS2_PLACEMENT_3D('',#200182,#121153,#121154);
#102505=AXIS2_PLACEMENT_3D('',#200183,#121155,#121156);
#102506=AXIS2_PLACEMENT_3D('',#200196,#121157,#121158);
#102507=AXIS2_PLACEMENT_3D('',#200215,#121159,#121160);
#102508=AXIS2_PLACEMENT_3D('',#200216,#121161,#121162);
#102509=AXIS2_PLACEMENT_3D('',#200217,#121163,#121164);
#102510=AXIS2_PLACEMENT_3D('',#200218,#121165,#121166);
#102511=AXIS2_PLACEMENT_3D('',#200219,#121167,#121168);
#102512=AXIS2_PLACEMENT_3D('',#200238,#121169,#121170);
#102513=AXIS2_PLACEMENT_3D('',#200251,#121171,#121172);
#102514=AXIS2_PLACEMENT_3D('',#200252,#121173,#121174);
#102515=AXIS2_PLACEMENT_3D('',#200253,#121175,#121176);
#102516=AXIS2_PLACEMENT_3D('',#200254,#121177,#121178);
#102517=AXIS2_PLACEMENT_3D('',#200255,#121179,#121180);
#102518=AXIS2_PLACEMENT_3D('',#200274,#121181,#121182);
#102519=AXIS2_PLACEMENT_3D('',#200275,#121183,#121184);
#102520=AXIS2_PLACEMENT_3D('',#200276,#121185,#121186);
#102521=AXIS2_PLACEMENT_3D('',#200277,#121187,#121188);
#102522=AXIS2_PLACEMENT_3D('',#200278,#121189,#121190);
#102523=AXIS2_PLACEMENT_3D('',#200291,#121191,#121192);
#102524=AXIS2_PLACEMENT_3D('',#200304,#121193,#121194);
#102525=AXIS2_PLACEMENT_3D('',#200305,#121195,#121196);
#102526=AXIS2_PLACEMENT_3D('',#200306,#121197,#121198);
#102527=AXIS2_PLACEMENT_3D('',#200307,#121199,#121200);
#102528=AXIS2_PLACEMENT_3D('',#200308,#121201,#121202);
#102529=AXIS2_PLACEMENT_3D('',#200321,#121203,#121204);
#102530=AXIS2_PLACEMENT_3D('',#200322,#121205,#121206);
#102531=AXIS2_PLACEMENT_3D('',#200323,#121207,#121208);
#102532=AXIS2_PLACEMENT_3D('',#200324,#121209,#121210);
#102533=AXIS2_PLACEMENT_3D('',#200325,#121211,#121212);
#102534=AXIS2_PLACEMENT_3D('',#200338,#121213,#121214);
#102535=AXIS2_PLACEMENT_3D('',#200339,#121215,#121216);
#102536=AXIS2_PLACEMENT_3D('',#200340,#121217,#121218);
#102537=AXIS2_PLACEMENT_3D('',#200341,#121219,#121220);
#102538=AXIS2_PLACEMENT_3D('',#200342,#121221,#121222);
#102539=AXIS2_PLACEMENT_3D('',#200355,#121223,#121224);
#102540=AXIS2_PLACEMENT_3D('',#200368,#121225,#121226);
#102541=AXIS2_PLACEMENT_3D('',#200369,#121227,#121228);
#102542=AXIS2_PLACEMENT_3D('',#200370,#121229,#121230);
#102543=AXIS2_PLACEMENT_3D('',#200371,#121231,#121232);
#102544=AXIS2_PLACEMENT_3D('',#200372,#121233,#121234);
#102545=AXIS2_PLACEMENT_3D('',#200391,#121235,#121236);
#102546=AXIS2_PLACEMENT_3D('',#200392,#121237,#121238);
#102547=AXIS2_PLACEMENT_3D('',#200393,#121239,#121240);
#102548=AXIS2_PLACEMENT_3D('',#200394,#121241,#121242);
#102549=AXIS2_PLACEMENT_3D('',#200395,#121243,#121244);
#102550=AXIS2_PLACEMENT_3D('',#200408,#121245,#121246);
#102551=AXIS2_PLACEMENT_3D('',#200427,#121247,#121248);
#102552=AXIS2_PLACEMENT_3D('',#200428,#121249,#121250);
#102553=AXIS2_PLACEMENT_3D('',#200429,#121251,#121252);
#102554=AXIS2_PLACEMENT_3D('',#200430,#121253,#121254);
#102555=AXIS2_PLACEMENT_3D('',#200431,#121255,#121256);
#102556=AXIS2_PLACEMENT_3D('',#200450,#121257,#121258);
#102557=AXIS2_PLACEMENT_3D('',#200463,#121259,#121260);
#102558=AXIS2_PLACEMENT_3D('',#200464,#121261,#121262);
#102559=AXIS2_PLACEMENT_3D('',#200465,#121263,#121264);
#102560=AXIS2_PLACEMENT_3D('',#200466,#121265,#121266);
#102561=AXIS2_PLACEMENT_3D('',#200467,#121267,#121268);
#102562=AXIS2_PLACEMENT_3D('',#200486,#121269,#121270);
#102563=AXIS2_PLACEMENT_3D('',#200487,#121271,#121272);
#102564=AXIS2_PLACEMENT_3D('',#200488,#121273,#121274);
#102565=AXIS2_PLACEMENT_3D('',#200489,#121275,#121276);
#102566=AXIS2_PLACEMENT_3D('',#200490,#121277,#121278);
#102567=AXIS2_PLACEMENT_3D('',#200503,#121279,#121280);
#102568=AXIS2_PLACEMENT_3D('',#200516,#121281,#121282);
#102569=AXIS2_PLACEMENT_3D('',#200517,#121283,#121284);
#102570=AXIS2_PLACEMENT_3D('',#200518,#121285,#121286);
#102571=AXIS2_PLACEMENT_3D('',#200519,#121287,#121288);
#102572=AXIS2_PLACEMENT_3D('',#200520,#121289,#121290);
#102573=AXIS2_PLACEMENT_3D('',#200533,#121291,#121292);
#102574=AXIS2_PLACEMENT_3D('',#200534,#121293,#121294);
#102575=AXIS2_PLACEMENT_3D('',#200535,#121295,#121296);
#102576=AXIS2_PLACEMENT_3D('',#200536,#121297,#121298);
#102577=AXIS2_PLACEMENT_3D('',#200537,#121299,#121300);
#102578=AXIS2_PLACEMENT_3D('',#200550,#121301,#121302);
#102579=AXIS2_PLACEMENT_3D('',#200551,#121303,#121304);
#102580=AXIS2_PLACEMENT_3D('',#200552,#121305,#121306);
#102581=AXIS2_PLACEMENT_3D('',#200553,#121307,#121308);
#102582=AXIS2_PLACEMENT_3D('',#200554,#121309,#121310);
#102583=AXIS2_PLACEMENT_3D('',#200567,#121311,#121312);
#102584=AXIS2_PLACEMENT_3D('',#200580,#121313,#121314);
#102585=AXIS2_PLACEMENT_3D('',#200581,#121315,#121316);
#102586=AXIS2_PLACEMENT_3D('',#200582,#121317,#121318);
#102587=AXIS2_PLACEMENT_3D('',#200583,#121319,#121320);
#102588=AXIS2_PLACEMENT_3D('',#200584,#121321,#121322);
#102589=AXIS2_PLACEMENT_3D('',#200603,#121323,#121324);
#102590=AXIS2_PLACEMENT_3D('',#200604,#121325,#121326);
#102591=AXIS2_PLACEMENT_3D('',#200605,#121327,#121328);
#102592=AXIS2_PLACEMENT_3D('',#200606,#121329,#121330);
#102593=AXIS2_PLACEMENT_3D('',#200607,#121331,#121332);
#102594=AXIS2_PLACEMENT_3D('',#200620,#121333,#121334);
#102595=AXIS2_PLACEMENT_3D('',#200639,#121335,#121336);
#102596=AXIS2_PLACEMENT_3D('',#200640,#121337,#121338);
#102597=AXIS2_PLACEMENT_3D('',#200641,#121339,#121340);
#102598=AXIS2_PLACEMENT_3D('',#200642,#121341,#121342);
#102599=AXIS2_PLACEMENT_3D('',#200643,#121343,#121344);
#102600=AXIS2_PLACEMENT_3D('',#200662,#121345,#121346);
#102601=AXIS2_PLACEMENT_3D('',#200675,#121347,#121348);
#102602=AXIS2_PLACEMENT_3D('',#200676,#121349,#121350);
#102603=AXIS2_PLACEMENT_3D('',#200677,#121351,#121352);
#102604=AXIS2_PLACEMENT_3D('',#200678,#121353,#121354);
#102605=AXIS2_PLACEMENT_3D('',#200679,#121355,#121356);
#102606=AXIS2_PLACEMENT_3D('',#200698,#121357,#121358);
#102607=AXIS2_PLACEMENT_3D('',#200699,#121359,#121360);
#102608=AXIS2_PLACEMENT_3D('',#200700,#121361,#121362);
#102609=AXIS2_PLACEMENT_3D('',#200701,#121363,#121364);
#102610=AXIS2_PLACEMENT_3D('',#200702,#121365,#121366);
#102611=AXIS2_PLACEMENT_3D('',#200715,#121367,#121368);
#102612=AXIS2_PLACEMENT_3D('',#200728,#121369,#121370);
#102613=AXIS2_PLACEMENT_3D('',#200729,#121371,#121372);
#102614=AXIS2_PLACEMENT_3D('',#200730,#121373,#121374);
#102615=AXIS2_PLACEMENT_3D('',#200731,#121375,#121376);
#102616=AXIS2_PLACEMENT_3D('',#200732,#121377,#121378);
#102617=AXIS2_PLACEMENT_3D('',#200745,#121379,#121380);
#102618=AXIS2_PLACEMENT_3D('',#200746,#121381,#121382);
#102619=AXIS2_PLACEMENT_3D('',#200747,#121383,#121384);
#102620=AXIS2_PLACEMENT_3D('',#200748,#121385,#121386);
#102621=AXIS2_PLACEMENT_3D('',#200749,#121387,#121388);
#102622=AXIS2_PLACEMENT_3D('',#200762,#121389,#121390);
#102623=AXIS2_PLACEMENT_3D('',#200763,#121391,#121392);
#102624=AXIS2_PLACEMENT_3D('',#200764,#121393,#121394);
#102625=AXIS2_PLACEMENT_3D('',#200765,#121395,#121396);
#102626=AXIS2_PLACEMENT_3D('',#200766,#121397,#121398);
#102627=AXIS2_PLACEMENT_3D('',#200779,#121399,#121400);
#102628=AXIS2_PLACEMENT_3D('',#200792,#121401,#121402);
#102629=AXIS2_PLACEMENT_3D('',#200793,#121403,#121404);
#102630=AXIS2_PLACEMENT_3D('',#200794,#121405,#121406);
#102631=AXIS2_PLACEMENT_3D('',#200795,#121407,#121408);
#102632=AXIS2_PLACEMENT_3D('',#200796,#121409,#121410);
#102633=AXIS2_PLACEMENT_3D('',#200815,#121411,#121412);
#102634=AXIS2_PLACEMENT_3D('',#200816,#121413,#121414);
#102635=AXIS2_PLACEMENT_3D('',#200817,#121415,#121416);
#102636=AXIS2_PLACEMENT_3D('',#200818,#121417,#121418);
#102637=AXIS2_PLACEMENT_3D('',#200819,#121419,#121420);
#102638=AXIS2_PLACEMENT_3D('',#200832,#121421,#121422);
#102639=AXIS2_PLACEMENT_3D('',#200851,#121423,#121424);
#102640=AXIS2_PLACEMENT_3D('',#200852,#121425,#121426);
#102641=AXIS2_PLACEMENT_3D('',#200853,#121427,#121428);
#102642=AXIS2_PLACEMENT_3D('',#200854,#121429,#121430);
#102643=AXIS2_PLACEMENT_3D('',#200855,#121431,#121432);
#102644=AXIS2_PLACEMENT_3D('',#200874,#121433,#121434);
#102645=AXIS2_PLACEMENT_3D('',#200887,#121435,#121436);
#102646=AXIS2_PLACEMENT_3D('',#200888,#121437,#121438);
#102647=AXIS2_PLACEMENT_3D('',#200889,#121439,#121440);
#102648=AXIS2_PLACEMENT_3D('',#200890,#121441,#121442);
#102649=AXIS2_PLACEMENT_3D('',#200891,#121443,#121444);
#102650=AXIS2_PLACEMENT_3D('',#200910,#121445,#121446);
#102651=AXIS2_PLACEMENT_3D('',#200911,#121447,#121448);
#102652=AXIS2_PLACEMENT_3D('',#200912,#121449,#121450);
#102653=AXIS2_PLACEMENT_3D('',#200913,#121451,#121452);
#102654=AXIS2_PLACEMENT_3D('',#200914,#121453,#121454);
#102655=AXIS2_PLACEMENT_3D('',#200927,#121455,#121456);
#102656=AXIS2_PLACEMENT_3D('',#200940,#121457,#121458);
#102657=AXIS2_PLACEMENT_3D('',#200941,#121459,#121460);
#102658=AXIS2_PLACEMENT_3D('',#200942,#121461,#121462);
#102659=AXIS2_PLACEMENT_3D('',#200943,#121463,#121464);
#102660=AXIS2_PLACEMENT_3D('',#200944,#121465,#121466);
#102661=AXIS2_PLACEMENT_3D('',#200957,#121467,#121468);
#102662=AXIS2_PLACEMENT_3D('',#200958,#121469,#121470);
#102663=AXIS2_PLACEMENT_3D('',#200959,#121471,#121472);
#102664=AXIS2_PLACEMENT_3D('',#200960,#121473,#121474);
#102665=AXIS2_PLACEMENT_3D('',#200961,#121475,#121476);
#102666=AXIS2_PLACEMENT_3D('',#200974,#121477,#121478);
#102667=AXIS2_PLACEMENT_3D('',#200975,#121479,#121480);
#102668=AXIS2_PLACEMENT_3D('',#200976,#121481,#121482);
#102669=AXIS2_PLACEMENT_3D('',#200977,#121483,#121484);
#102670=AXIS2_PLACEMENT_3D('',#200978,#121485,#121486);
#102671=AXIS2_PLACEMENT_3D('',#200991,#121487,#121488);
#102672=AXIS2_PLACEMENT_3D('',#201004,#121489,#121490);
#102673=AXIS2_PLACEMENT_3D('',#201005,#121491,#121492);
#102674=AXIS2_PLACEMENT_3D('',#201006,#121493,#121494);
#102675=AXIS2_PLACEMENT_3D('',#201007,#121495,#121496);
#102676=AXIS2_PLACEMENT_3D('',#201008,#121497,#121498);
#102677=AXIS2_PLACEMENT_3D('',#201027,#121499,#121500);
#102678=AXIS2_PLACEMENT_3D('',#201028,#121501,#121502);
#102679=AXIS2_PLACEMENT_3D('',#201029,#121503,#121504);
#102680=AXIS2_PLACEMENT_3D('',#201030,#121505,#121506);
#102681=AXIS2_PLACEMENT_3D('',#201031,#121507,#121508);
#102682=AXIS2_PLACEMENT_3D('',#201044,#121509,#121510);
#102683=AXIS2_PLACEMENT_3D('',#201063,#121511,#121512);
#102684=AXIS2_PLACEMENT_3D('',#201064,#121513,#121514);
#102685=AXIS2_PLACEMENT_3D('',#201065,#121515,#121516);
#102686=AXIS2_PLACEMENT_3D('',#201066,#121517,#121518);
#102687=AXIS2_PLACEMENT_3D('',#201067,#121519,#121520);
#102688=AXIS2_PLACEMENT_3D('',#201086,#121521,#121522);
#102689=AXIS2_PLACEMENT_3D('',#201099,#121523,#121524);
#102690=AXIS2_PLACEMENT_3D('',#201100,#121525,#121526);
#102691=AXIS2_PLACEMENT_3D('',#201101,#121527,#121528);
#102692=AXIS2_PLACEMENT_3D('',#201102,#121529,#121530);
#102693=AXIS2_PLACEMENT_3D('',#201103,#121531,#121532);
#102694=AXIS2_PLACEMENT_3D('',#201122,#121533,#121534);
#102695=AXIS2_PLACEMENT_3D('',#201123,#121535,#121536);
#102696=AXIS2_PLACEMENT_3D('',#201124,#121537,#121538);
#102697=AXIS2_PLACEMENT_3D('',#201125,#121539,#121540);
#102698=AXIS2_PLACEMENT_3D('',#201126,#121541,#121542);
#102699=AXIS2_PLACEMENT_3D('',#201139,#121543,#121544);
#102700=AXIS2_PLACEMENT_3D('',#201152,#121545,#121546);
#102701=AXIS2_PLACEMENT_3D('',#201153,#121547,#121548);
#102702=AXIS2_PLACEMENT_3D('',#201154,#121549,#121550);
#102703=AXIS2_PLACEMENT_3D('',#201155,#121551,#121552);
#102704=AXIS2_PLACEMENT_3D('',#201156,#121553,#121554);
#102705=AXIS2_PLACEMENT_3D('',#201169,#121555,#121556);
#102706=AXIS2_PLACEMENT_3D('',#201170,#121557,#121558);
#102707=AXIS2_PLACEMENT_3D('',#201171,#121559,#121560);
#102708=AXIS2_PLACEMENT_3D('',#201172,#121561,#121562);
#102709=AXIS2_PLACEMENT_3D('',#201173,#121563,#121564);
#102710=AXIS2_PLACEMENT_3D('',#201186,#121565,#121566);
#102711=AXIS2_PLACEMENT_3D('',#201187,#121567,#121568);
#102712=AXIS2_PLACEMENT_3D('',#201188,#121569,#121570);
#102713=AXIS2_PLACEMENT_3D('',#201189,#121571,#121572);
#102714=AXIS2_PLACEMENT_3D('',#201190,#121573,#121574);
#102715=AXIS2_PLACEMENT_3D('',#201203,#121575,#121576);
#102716=AXIS2_PLACEMENT_3D('',#201216,#121577,#121578);
#102717=AXIS2_PLACEMENT_3D('',#201217,#121579,#121580);
#102718=AXIS2_PLACEMENT_3D('',#201218,#121581,#121582);
#102719=AXIS2_PLACEMENT_3D('',#201219,#121583,#121584);
#102720=AXIS2_PLACEMENT_3D('',#201220,#121585,#121586);
#102721=AXIS2_PLACEMENT_3D('',#201239,#121587,#121588);
#102722=AXIS2_PLACEMENT_3D('',#201240,#121589,#121590);
#102723=AXIS2_PLACEMENT_3D('',#201241,#121591,#121592);
#102724=AXIS2_PLACEMENT_3D('',#201242,#121593,#121594);
#102725=AXIS2_PLACEMENT_3D('',#201243,#121595,#121596);
#102726=AXIS2_PLACEMENT_3D('',#201256,#121597,#121598);
#102727=AXIS2_PLACEMENT_3D('',#201275,#121599,#121600);
#102728=AXIS2_PLACEMENT_3D('',#201276,#121601,#121602);
#102729=AXIS2_PLACEMENT_3D('',#201277,#121603,#121604);
#102730=AXIS2_PLACEMENT_3D('',#201278,#121605,#121606);
#102731=AXIS2_PLACEMENT_3D('',#201279,#121607,#121608);
#102732=AXIS2_PLACEMENT_3D('',#201298,#121609,#121610);
#102733=AXIS2_PLACEMENT_3D('',#201311,#121611,#121612);
#102734=AXIS2_PLACEMENT_3D('',#201312,#121613,#121614);
#102735=AXIS2_PLACEMENT_3D('',#201313,#121615,#121616);
#102736=AXIS2_PLACEMENT_3D('',#201314,#121617,#121618);
#102737=AXIS2_PLACEMENT_3D('',#201315,#121619,#121620);
#102738=AXIS2_PLACEMENT_3D('',#201334,#121621,#121622);
#102739=AXIS2_PLACEMENT_3D('',#201335,#121623,#121624);
#102740=AXIS2_PLACEMENT_3D('',#201336,#121625,#121626);
#102741=AXIS2_PLACEMENT_3D('',#201337,#121627,#121628);
#102742=AXIS2_PLACEMENT_3D('',#201338,#121629,#121630);
#102743=AXIS2_PLACEMENT_3D('',#201351,#121631,#121632);
#102744=AXIS2_PLACEMENT_3D('',#201364,#121633,#121634);
#102745=AXIS2_PLACEMENT_3D('',#201365,#121635,#121636);
#102746=AXIS2_PLACEMENT_3D('',#201366,#121637,#121638);
#102747=AXIS2_PLACEMENT_3D('',#201367,#121639,#121640);
#102748=AXIS2_PLACEMENT_3D('',#201368,#121641,#121642);
#102749=AXIS2_PLACEMENT_3D('',#201381,#121643,#121644);
#102750=AXIS2_PLACEMENT_3D('',#201382,#121645,#121646);
#102751=AXIS2_PLACEMENT_3D('',#201383,#121647,#121648);
#102752=AXIS2_PLACEMENT_3D('',#201384,#121649,#121650);
#102753=AXIS2_PLACEMENT_3D('',#201385,#121651,#121652);
#102754=AXIS2_PLACEMENT_3D('',#201398,#121653,#121654);
#102755=AXIS2_PLACEMENT_3D('',#201399,#121655,#121656);
#102756=AXIS2_PLACEMENT_3D('',#201400,#121657,#121658);
#102757=AXIS2_PLACEMENT_3D('',#201401,#121659,#121660);
#102758=AXIS2_PLACEMENT_3D('',#201402,#121661,#121662);
#102759=AXIS2_PLACEMENT_3D('',#201415,#121663,#121664);
#102760=AXIS2_PLACEMENT_3D('',#201428,#121665,#121666);
#102761=AXIS2_PLACEMENT_3D('',#201429,#121667,#121668);
#102762=AXIS2_PLACEMENT_3D('',#201430,#121669,#121670);
#102763=AXIS2_PLACEMENT_3D('',#201431,#121671,#121672);
#102764=AXIS2_PLACEMENT_3D('',#201432,#121673,#121674);
#102765=AXIS2_PLACEMENT_3D('',#201451,#121675,#121676);
#102766=AXIS2_PLACEMENT_3D('',#201452,#121677,#121678);
#102767=AXIS2_PLACEMENT_3D('',#201453,#121679,#121680);
#102768=AXIS2_PLACEMENT_3D('',#201454,#121681,#121682);
#102769=AXIS2_PLACEMENT_3D('',#201455,#121683,#121684);
#102770=AXIS2_PLACEMENT_3D('',#201468,#121685,#121686);
#102771=AXIS2_PLACEMENT_3D('',#201487,#121687,#121688);
#102772=AXIS2_PLACEMENT_3D('',#201488,#121689,#121690);
#102773=AXIS2_PLACEMENT_3D('',#201489,#121691,#121692);
#102774=AXIS2_PLACEMENT_3D('',#201490,#121693,#121694);
#102775=AXIS2_PLACEMENT_3D('',#201491,#121695,#121696);
#102776=AXIS2_PLACEMENT_3D('',#201510,#121697,#121698);
#102777=AXIS2_PLACEMENT_3D('',#201523,#121699,#121700);
#102778=AXIS2_PLACEMENT_3D('',#201524,#121701,#121702);
#102779=AXIS2_PLACEMENT_3D('',#201525,#121703,#121704);
#102780=AXIS2_PLACEMENT_3D('',#201526,#121705,#121706);
#102781=AXIS2_PLACEMENT_3D('',#201527,#121707,#121708);
#102782=AXIS2_PLACEMENT_3D('',#201546,#121709,#121710);
#102783=AXIS2_PLACEMENT_3D('',#201547,#121711,#121712);
#102784=AXIS2_PLACEMENT_3D('',#201548,#121713,#121714);
#102785=AXIS2_PLACEMENT_3D('',#201549,#121715,#121716);
#102786=AXIS2_PLACEMENT_3D('',#201550,#121717,#121718);
#102787=AXIS2_PLACEMENT_3D('',#201563,#121719,#121720);
#102788=AXIS2_PLACEMENT_3D('',#201576,#121721,#121722);
#102789=AXIS2_PLACEMENT_3D('',#201577,#121723,#121724);
#102790=AXIS2_PLACEMENT_3D('',#201578,#121725,#121726);
#102791=AXIS2_PLACEMENT_3D('',#201579,#121727,#121728);
#102792=AXIS2_PLACEMENT_3D('',#201580,#121729,#121730);
#102793=AXIS2_PLACEMENT_3D('',#201593,#121731,#121732);
#102794=AXIS2_PLACEMENT_3D('',#201594,#121733,#121734);
#102795=AXIS2_PLACEMENT_3D('',#201595,#121735,#121736);
#102796=AXIS2_PLACEMENT_3D('',#201596,#121737,#121738);
#102797=AXIS2_PLACEMENT_3D('',#201597,#121739,#121740);
#102798=AXIS2_PLACEMENT_3D('',#201610,#121741,#121742);
#102799=AXIS2_PLACEMENT_3D('',#201611,#121743,#121744);
#102800=AXIS2_PLACEMENT_3D('',#201612,#121745,#121746);
#102801=AXIS2_PLACEMENT_3D('',#201613,#121747,#121748);
#102802=AXIS2_PLACEMENT_3D('',#201614,#121749,#121750);
#102803=AXIS2_PLACEMENT_3D('',#201627,#121751,#121752);
#102804=AXIS2_PLACEMENT_3D('',#201640,#121753,#121754);
#102805=AXIS2_PLACEMENT_3D('',#201641,#121755,#121756);
#102806=AXIS2_PLACEMENT_3D('',#201642,#121757,#121758);
#102807=AXIS2_PLACEMENT_3D('',#201643,#121759,#121760);
#102808=AXIS2_PLACEMENT_3D('',#201644,#121761,#121762);
#102809=AXIS2_PLACEMENT_3D('',#201663,#121763,#121764);
#102810=AXIS2_PLACEMENT_3D('',#201664,#121765,#121766);
#102811=AXIS2_PLACEMENT_3D('',#201665,#121767,#121768);
#102812=AXIS2_PLACEMENT_3D('',#201666,#121769,#121770);
#102813=AXIS2_PLACEMENT_3D('',#201667,#121771,#121772);
#102814=AXIS2_PLACEMENT_3D('',#201680,#121773,#121774);
#102815=AXIS2_PLACEMENT_3D('',#201699,#121775,#121776);
#102816=AXIS2_PLACEMENT_3D('',#201700,#121777,#121778);
#102817=AXIS2_PLACEMENT_3D('',#201701,#121779,#121780);
#102818=AXIS2_PLACEMENT_3D('',#201702,#121781,#121782);
#102819=AXIS2_PLACEMENT_3D('',#201703,#121783,#121784);
#102820=AXIS2_PLACEMENT_3D('',#201722,#121785,#121786);
#102821=AXIS2_PLACEMENT_3D('',#201735,#121787,#121788);
#102822=AXIS2_PLACEMENT_3D('',#201736,#121789,#121790);
#102823=AXIS2_PLACEMENT_3D('',#201737,#121791,#121792);
#102824=AXIS2_PLACEMENT_3D('',#201738,#121793,#121794);
#102825=AXIS2_PLACEMENT_3D('',#201739,#121795,#121796);
#102826=AXIS2_PLACEMENT_3D('',#201758,#121797,#121798);
#102827=AXIS2_PLACEMENT_3D('',#201759,#121799,#121800);
#102828=AXIS2_PLACEMENT_3D('',#201760,#121801,#121802);
#102829=AXIS2_PLACEMENT_3D('',#201761,#121803,#121804);
#102830=AXIS2_PLACEMENT_3D('',#201762,#121805,#121806);
#102831=AXIS2_PLACEMENT_3D('',#201775,#121807,#121808);
#102832=AXIS2_PLACEMENT_3D('',#201788,#121809,#121810);
#102833=AXIS2_PLACEMENT_3D('',#201789,#121811,#121812);
#102834=AXIS2_PLACEMENT_3D('',#201790,#121813,#121814);
#102835=AXIS2_PLACEMENT_3D('',#201791,#121815,#121816);
#102836=AXIS2_PLACEMENT_3D('',#201792,#121817,#121818);
#102837=AXIS2_PLACEMENT_3D('',#201805,#121819,#121820);
#102838=AXIS2_PLACEMENT_3D('',#201806,#121821,#121822);
#102839=AXIS2_PLACEMENT_3D('',#201807,#121823,#121824);
#102840=AXIS2_PLACEMENT_3D('',#201808,#121825,#121826);
#102841=AXIS2_PLACEMENT_3D('',#201809,#121827,#121828);
#102842=AXIS2_PLACEMENT_3D('',#201822,#121829,#121830);
#102843=AXIS2_PLACEMENT_3D('',#201823,#121831,#121832);
#102844=AXIS2_PLACEMENT_3D('',#201824,#121833,#121834);
#102845=AXIS2_PLACEMENT_3D('',#201825,#121835,#121836);
#102846=AXIS2_PLACEMENT_3D('',#201826,#121837,#121838);
#102847=AXIS2_PLACEMENT_3D('',#201839,#121839,#121840);
#102848=AXIS2_PLACEMENT_3D('',#201852,#121841,#121842);
#102849=AXIS2_PLACEMENT_3D('',#201853,#121843,#121844);
#102850=AXIS2_PLACEMENT_3D('',#201854,#121845,#121846);
#102851=AXIS2_PLACEMENT_3D('',#201855,#121847,#121848);
#102852=AXIS2_PLACEMENT_3D('',#201856,#121849,#121850);
#102853=AXIS2_PLACEMENT_3D('',#201875,#121851,#121852);
#102854=AXIS2_PLACEMENT_3D('',#201876,#121853,#121854);
#102855=AXIS2_PLACEMENT_3D('',#201877,#121855,#121856);
#102856=AXIS2_PLACEMENT_3D('',#201878,#121857,#121858);
#102857=AXIS2_PLACEMENT_3D('',#201879,#121859,#121860);
#102858=AXIS2_PLACEMENT_3D('',#201892,#121861,#121862);
#102859=AXIS2_PLACEMENT_3D('',#201911,#121863,#121864);
#102860=AXIS2_PLACEMENT_3D('',#201912,#121865,#121866);
#102861=AXIS2_PLACEMENT_3D('',#201913,#121867,#121868);
#102862=AXIS2_PLACEMENT_3D('',#201914,#121869,#121870);
#102863=AXIS2_PLACEMENT_3D('',#201915,#121871,#121872);
#102864=AXIS2_PLACEMENT_3D('',#201934,#121873,#121874);
#102865=AXIS2_PLACEMENT_3D('',#201947,#121875,#121876);
#102866=AXIS2_PLACEMENT_3D('',#201948,#121877,#121878);
#102867=AXIS2_PLACEMENT_3D('',#201949,#121879,#121880);
#102868=AXIS2_PLACEMENT_3D('',#201950,#121881,#121882);
#102869=AXIS2_PLACEMENT_3D('',#201951,#121883,#121884);
#102870=AXIS2_PLACEMENT_3D('',#201970,#121885,#121886);
#102871=AXIS2_PLACEMENT_3D('',#201971,#121887,#121888);
#102872=AXIS2_PLACEMENT_3D('',#201972,#121889,#121890);
#102873=AXIS2_PLACEMENT_3D('',#201973,#121891,#121892);
#102874=AXIS2_PLACEMENT_3D('',#201974,#121893,#121894);
#102875=AXIS2_PLACEMENT_3D('',#201987,#121895,#121896);
#102876=AXIS2_PLACEMENT_3D('',#202000,#121897,#121898);
#102877=AXIS2_PLACEMENT_3D('',#202001,#121899,#121900);
#102878=AXIS2_PLACEMENT_3D('',#202002,#121901,#121902);
#102879=AXIS2_PLACEMENT_3D('',#202003,#121903,#121904);
#102880=AXIS2_PLACEMENT_3D('',#202004,#121905,#121906);
#102881=AXIS2_PLACEMENT_3D('',#202017,#121907,#121908);
#102882=AXIS2_PLACEMENT_3D('',#202018,#121909,#121910);
#102883=AXIS2_PLACEMENT_3D('',#202019,#121911,#121912);
#102884=AXIS2_PLACEMENT_3D('',#202020,#121913,#121914);
#102885=AXIS2_PLACEMENT_3D('',#202021,#121915,#121916);
#102886=AXIS2_PLACEMENT_3D('',#202034,#121917,#121918);
#102887=AXIS2_PLACEMENT_3D('',#202035,#121919,#121920);
#102888=AXIS2_PLACEMENT_3D('',#202036,#121921,#121922);
#102889=AXIS2_PLACEMENT_3D('',#202037,#121923,#121924);
#102890=AXIS2_PLACEMENT_3D('',#202038,#121925,#121926);
#102891=AXIS2_PLACEMENT_3D('',#202051,#121927,#121928);
#102892=AXIS2_PLACEMENT_3D('',#202064,#121929,#121930);
#102893=AXIS2_PLACEMENT_3D('',#202065,#121931,#121932);
#102894=AXIS2_PLACEMENT_3D('',#202066,#121933,#121934);
#102895=AXIS2_PLACEMENT_3D('',#202067,#121935,#121936);
#102896=AXIS2_PLACEMENT_3D('',#202068,#121937,#121938);
#102897=AXIS2_PLACEMENT_3D('',#202087,#121939,#121940);
#102898=AXIS2_PLACEMENT_3D('',#202088,#121941,#121942);
#102899=AXIS2_PLACEMENT_3D('',#202089,#121943,#121944);
#102900=AXIS2_PLACEMENT_3D('',#202090,#121945,#121946);
#102901=AXIS2_PLACEMENT_3D('',#202091,#121947,#121948);
#102902=AXIS2_PLACEMENT_3D('',#202104,#121949,#121950);
#102903=AXIS2_PLACEMENT_3D('',#202123,#121951,#121952);
#102904=AXIS2_PLACEMENT_3D('',#202124,#121953,#121954);
#102905=AXIS2_PLACEMENT_3D('',#202125,#121955,#121956);
#102906=AXIS2_PLACEMENT_3D('',#202126,#121957,#121958);
#102907=AXIS2_PLACEMENT_3D('',#202127,#121959,#121960);
#102908=AXIS2_PLACEMENT_3D('',#202146,#121961,#121962);
#102909=AXIS2_PLACEMENT_3D('',#202159,#121963,#121964);
#102910=AXIS2_PLACEMENT_3D('',#202160,#121965,#121966);
#102911=AXIS2_PLACEMENT_3D('',#202161,#121967,#121968);
#102912=AXIS2_PLACEMENT_3D('',#202162,#121969,#121970);
#102913=AXIS2_PLACEMENT_3D('',#202163,#121971,#121972);
#102914=AXIS2_PLACEMENT_3D('',#202182,#121973,#121974);
#102915=AXIS2_PLACEMENT_3D('',#202183,#121975,#121976);
#102916=AXIS2_PLACEMENT_3D('',#202184,#121977,#121978);
#102917=AXIS2_PLACEMENT_3D('',#202185,#121979,#121980);
#102918=AXIS2_PLACEMENT_3D('',#202186,#121981,#121982);
#102919=AXIS2_PLACEMENT_3D('',#202199,#121983,#121984);
#102920=AXIS2_PLACEMENT_3D('',#202212,#121985,#121986);
#102921=AXIS2_PLACEMENT_3D('',#202213,#121987,#121988);
#102922=AXIS2_PLACEMENT_3D('',#202214,#121989,#121990);
#102923=AXIS2_PLACEMENT_3D('',#202215,#121991,#121992);
#102924=AXIS2_PLACEMENT_3D('',#202216,#121993,#121994);
#102925=AXIS2_PLACEMENT_3D('',#202229,#121995,#121996);
#102926=AXIS2_PLACEMENT_3D('',#202230,#121997,#121998);
#102927=AXIS2_PLACEMENT_3D('',#202231,#121999,#122000);
#102928=AXIS2_PLACEMENT_3D('',#202232,#122001,#122002);
#102929=AXIS2_PLACEMENT_3D('',#202233,#122003,#122004);
#102930=AXIS2_PLACEMENT_3D('',#202246,#122005,#122006);
#102931=AXIS2_PLACEMENT_3D('',#202247,#122007,#122008);
#102932=AXIS2_PLACEMENT_3D('',#202248,#122009,#122010);
#102933=AXIS2_PLACEMENT_3D('',#202249,#122011,#122012);
#102934=AXIS2_PLACEMENT_3D('',#202250,#122013,#122014);
#102935=AXIS2_PLACEMENT_3D('',#202263,#122015,#122016);
#102936=AXIS2_PLACEMENT_3D('',#202276,#122017,#122018);
#102937=AXIS2_PLACEMENT_3D('',#202277,#122019,#122020);
#102938=AXIS2_PLACEMENT_3D('',#202278,#122021,#122022);
#102939=AXIS2_PLACEMENT_3D('',#202279,#122023,#122024);
#102940=AXIS2_PLACEMENT_3D('',#202280,#122025,#122026);
#102941=AXIS2_PLACEMENT_3D('',#202299,#122027,#122028);
#102942=AXIS2_PLACEMENT_3D('',#202300,#122029,#122030);
#102943=AXIS2_PLACEMENT_3D('',#202301,#122031,#122032);
#102944=AXIS2_PLACEMENT_3D('',#202302,#122033,#122034);
#102945=AXIS2_PLACEMENT_3D('',#202303,#122035,#122036);
#102946=AXIS2_PLACEMENT_3D('',#202316,#122037,#122038);
#102947=AXIS2_PLACEMENT_3D('',#202335,#122039,#122040);
#102948=AXIS2_PLACEMENT_3D('',#202336,#122041,#122042);
#102949=AXIS2_PLACEMENT_3D('',#202337,#122043,#122044);
#102950=AXIS2_PLACEMENT_3D('',#202338,#122045,#122046);
#102951=AXIS2_PLACEMENT_3D('',#202339,#122047,#122048);
#102952=AXIS2_PLACEMENT_3D('',#202358,#122049,#122050);
#102953=AXIS2_PLACEMENT_3D('',#202371,#122051,#122052);
#102954=AXIS2_PLACEMENT_3D('',#202372,#122053,#122054);
#102955=AXIS2_PLACEMENT_3D('',#202373,#122055,#122056);
#102956=AXIS2_PLACEMENT_3D('',#202374,#122057,#122058);
#102957=AXIS2_PLACEMENT_3D('',#202375,#122059,#122060);
#102958=AXIS2_PLACEMENT_3D('',#202394,#122061,#122062);
#102959=AXIS2_PLACEMENT_3D('',#202395,#122063,#122064);
#102960=AXIS2_PLACEMENT_3D('',#202396,#122065,#122066);
#102961=AXIS2_PLACEMENT_3D('',#202397,#122067,#122068);
#102962=AXIS2_PLACEMENT_3D('',#202398,#122069,#122070);
#102963=AXIS2_PLACEMENT_3D('',#202411,#122071,#122072);
#102964=AXIS2_PLACEMENT_3D('',#202424,#122073,#122074);
#102965=AXIS2_PLACEMENT_3D('',#202425,#122075,#122076);
#102966=AXIS2_PLACEMENT_3D('',#202426,#122077,#122078);
#102967=AXIS2_PLACEMENT_3D('',#202427,#122079,#122080);
#102968=AXIS2_PLACEMENT_3D('',#202428,#122081,#122082);
#102969=AXIS2_PLACEMENT_3D('',#202441,#122083,#122084);
#102970=AXIS2_PLACEMENT_3D('',#202442,#122085,#122086);
#102971=AXIS2_PLACEMENT_3D('',#202443,#122087,#122088);
#102972=AXIS2_PLACEMENT_3D('',#202444,#122089,#122090);
#102973=AXIS2_PLACEMENT_3D('',#202445,#122091,#122092);
#102974=AXIS2_PLACEMENT_3D('',#202458,#122093,#122094);
#102975=AXIS2_PLACEMENT_3D('',#202459,#122095,#122096);
#102976=AXIS2_PLACEMENT_3D('',#202460,#122097,#122098);
#102977=AXIS2_PLACEMENT_3D('',#202461,#122099,#122100);
#102978=AXIS2_PLACEMENT_3D('',#202462,#122101,#122102);
#102979=AXIS2_PLACEMENT_3D('',#202475,#122103,#122104);
#102980=AXIS2_PLACEMENT_3D('',#202488,#122105,#122106);
#102981=AXIS2_PLACEMENT_3D('',#202489,#122107,#122108);
#102982=AXIS2_PLACEMENT_3D('',#202490,#122109,#122110);
#102983=AXIS2_PLACEMENT_3D('',#202491,#122111,#122112);
#102984=AXIS2_PLACEMENT_3D('',#202492,#122113,#122114);
#102985=AXIS2_PLACEMENT_3D('',#202511,#122115,#122116);
#102986=AXIS2_PLACEMENT_3D('',#202512,#122117,#122118);
#102987=AXIS2_PLACEMENT_3D('',#202513,#122119,#122120);
#102988=AXIS2_PLACEMENT_3D('',#202514,#122121,#122122);
#102989=AXIS2_PLACEMENT_3D('',#202515,#122123,#122124);
#102990=AXIS2_PLACEMENT_3D('',#202528,#122125,#122126);
#102991=AXIS2_PLACEMENT_3D('',#202547,#122127,#122128);
#102992=AXIS2_PLACEMENT_3D('',#202548,#122129,#122130);
#102993=AXIS2_PLACEMENT_3D('',#202549,#122131,#122132);
#102994=AXIS2_PLACEMENT_3D('',#202550,#122133,#122134);
#102995=AXIS2_PLACEMENT_3D('',#202551,#122135,#122136);
#102996=AXIS2_PLACEMENT_3D('',#202570,#122137,#122138);
#102997=AXIS2_PLACEMENT_3D('',#202583,#122139,#122140);
#102998=AXIS2_PLACEMENT_3D('',#202584,#122141,#122142);
#102999=AXIS2_PLACEMENT_3D('',#202585,#122143,#122144);
#103000=AXIS2_PLACEMENT_3D('',#202586,#122145,#122146);
#103001=AXIS2_PLACEMENT_3D('',#202587,#122147,#122148);
#103002=AXIS2_PLACEMENT_3D('',#202606,#122149,#122150);
#103003=AXIS2_PLACEMENT_3D('',#202607,#122151,#122152);
#103004=AXIS2_PLACEMENT_3D('',#202608,#122153,#122154);
#103005=AXIS2_PLACEMENT_3D('',#202609,#122155,#122156);
#103006=AXIS2_PLACEMENT_3D('',#202610,#122157,#122158);
#103007=AXIS2_PLACEMENT_3D('',#202623,#122159,#122160);
#103008=AXIS2_PLACEMENT_3D('',#202636,#122161,#122162);
#103009=AXIS2_PLACEMENT_3D('',#202637,#122163,#122164);
#103010=AXIS2_PLACEMENT_3D('',#202638,#122165,#122166);
#103011=AXIS2_PLACEMENT_3D('',#202639,#122167,#122168);
#103012=AXIS2_PLACEMENT_3D('',#202640,#122169,#122170);
#103013=AXIS2_PLACEMENT_3D('',#202653,#122171,#122172);
#103014=AXIS2_PLACEMENT_3D('',#202654,#122173,#122174);
#103015=AXIS2_PLACEMENT_3D('',#202655,#122175,#122176);
#103016=AXIS2_PLACEMENT_3D('',#202656,#122177,#122178);
#103017=AXIS2_PLACEMENT_3D('',#202657,#122179,#122180);
#103018=AXIS2_PLACEMENT_3D('',#202670,#122181,#122182);
#103019=AXIS2_PLACEMENT_3D('',#202671,#122183,#122184);
#103020=AXIS2_PLACEMENT_3D('',#202672,#122185,#122186);
#103021=AXIS2_PLACEMENT_3D('',#202673,#122187,#122188);
#103022=AXIS2_PLACEMENT_3D('',#202674,#122189,#122190);
#103023=AXIS2_PLACEMENT_3D('',#202687,#122191,#122192);
#103024=AXIS2_PLACEMENT_3D('',#202700,#122193,#122194);
#103025=AXIS2_PLACEMENT_3D('',#202701,#122195,#122196);
#103026=AXIS2_PLACEMENT_3D('',#202702,#122197,#122198);
#103027=AXIS2_PLACEMENT_3D('',#202703,#122199,#122200);
#103028=AXIS2_PLACEMENT_3D('',#202704,#122201,#122202);
#103029=AXIS2_PLACEMENT_3D('',#202723,#122203,#122204);
#103030=AXIS2_PLACEMENT_3D('',#202724,#122205,#122206);
#103031=AXIS2_PLACEMENT_3D('',#202725,#122207,#122208);
#103032=AXIS2_PLACEMENT_3D('',#202726,#122209,#122210);
#103033=AXIS2_PLACEMENT_3D('',#202727,#122211,#122212);
#103034=AXIS2_PLACEMENT_3D('',#202740,#122213,#122214);
#103035=AXIS2_PLACEMENT_3D('',#202759,#122215,#122216);
#103036=AXIS2_PLACEMENT_3D('',#202760,#122217,#122218);
#103037=AXIS2_PLACEMENT_3D('',#202761,#122219,#122220);
#103038=AXIS2_PLACEMENT_3D('',#202762,#122221,#122222);
#103039=AXIS2_PLACEMENT_3D('',#202763,#122223,#122224);
#103040=AXIS2_PLACEMENT_3D('',#202782,#122225,#122226);
#103041=AXIS2_PLACEMENT_3D('',#202795,#122227,#122228);
#103042=AXIS2_PLACEMENT_3D('',#202796,#122229,#122230);
#103043=AXIS2_PLACEMENT_3D('',#202797,#122231,#122232);
#103044=AXIS2_PLACEMENT_3D('',#202798,#122233,#122234);
#103045=AXIS2_PLACEMENT_3D('',#202799,#122235,#122236);
#103046=AXIS2_PLACEMENT_3D('',#202818,#122237,#122238);
#103047=AXIS2_PLACEMENT_3D('',#202819,#122239,#122240);
#103048=AXIS2_PLACEMENT_3D('',#202820,#122241,#122242);
#103049=AXIS2_PLACEMENT_3D('',#202821,#122243,#122244);
#103050=AXIS2_PLACEMENT_3D('',#202822,#122245,#122246);
#103051=AXIS2_PLACEMENT_3D('',#202835,#122247,#122248);
#103052=AXIS2_PLACEMENT_3D('',#202848,#122249,#122250);
#103053=AXIS2_PLACEMENT_3D('',#202849,#122251,#122252);
#103054=AXIS2_PLACEMENT_3D('',#202850,#122253,#122254);
#103055=AXIS2_PLACEMENT_3D('',#202851,#122255,#122256);
#103056=AXIS2_PLACEMENT_3D('',#202852,#122257,#122258);
#103057=AXIS2_PLACEMENT_3D('',#202865,#122259,#122260);
#103058=AXIS2_PLACEMENT_3D('',#202866,#122261,#122262);
#103059=AXIS2_PLACEMENT_3D('',#202867,#122263,#122264);
#103060=AXIS2_PLACEMENT_3D('',#202868,#122265,#122266);
#103061=AXIS2_PLACEMENT_3D('',#202869,#122267,#122268);
#103062=AXIS2_PLACEMENT_3D('',#202882,#122269,#122270);
#103063=AXIS2_PLACEMENT_3D('',#202883,#122271,#122272);
#103064=AXIS2_PLACEMENT_3D('',#202884,#122273,#122274);
#103065=AXIS2_PLACEMENT_3D('',#202885,#122275,#122276);
#103066=AXIS2_PLACEMENT_3D('',#202886,#122277,#122278);
#103067=AXIS2_PLACEMENT_3D('',#202899,#122279,#122280);
#103068=AXIS2_PLACEMENT_3D('',#202912,#122281,#122282);
#103069=AXIS2_PLACEMENT_3D('',#202913,#122283,#122284);
#103070=AXIS2_PLACEMENT_3D('',#202914,#122285,#122286);
#103071=AXIS2_PLACEMENT_3D('',#202915,#122287,#122288);
#103072=AXIS2_PLACEMENT_3D('',#202916,#122289,#122290);
#103073=AXIS2_PLACEMENT_3D('',#202935,#122291,#122292);
#103074=AXIS2_PLACEMENT_3D('',#202936,#122293,#122294);
#103075=AXIS2_PLACEMENT_3D('',#202937,#122295,#122296);
#103076=AXIS2_PLACEMENT_3D('',#202938,#122297,#122298);
#103077=AXIS2_PLACEMENT_3D('',#202939,#122299,#122300);
#103078=AXIS2_PLACEMENT_3D('',#202952,#122301,#122302);
#103079=AXIS2_PLACEMENT_3D('',#202971,#122303,#122304);
#103080=AXIS2_PLACEMENT_3D('',#202972,#122305,#122306);
#103081=AXIS2_PLACEMENT_3D('',#202973,#122307,#122308);
#103082=AXIS2_PLACEMENT_3D('',#202974,#122309,#122310);
#103083=AXIS2_PLACEMENT_3D('',#202975,#122311,#122312);
#103084=AXIS2_PLACEMENT_3D('',#202994,#122313,#122314);
#103085=AXIS2_PLACEMENT_3D('',#203007,#122315,#122316);
#103086=AXIS2_PLACEMENT_3D('',#203008,#122317,#122318);
#103087=AXIS2_PLACEMENT_3D('',#203009,#122319,#122320);
#103088=AXIS2_PLACEMENT_3D('',#203010,#122321,#122322);
#103089=AXIS2_PLACEMENT_3D('',#203011,#122323,#122324);
#103090=AXIS2_PLACEMENT_3D('',#203030,#122325,#122326);
#103091=AXIS2_PLACEMENT_3D('',#203031,#122327,#122328);
#103092=AXIS2_PLACEMENT_3D('',#203032,#122329,#122330);
#103093=AXIS2_PLACEMENT_3D('',#203033,#122331,#122332);
#103094=AXIS2_PLACEMENT_3D('',#203034,#122333,#122334);
#103095=AXIS2_PLACEMENT_3D('',#203047,#122335,#122336);
#103096=AXIS2_PLACEMENT_3D('',#203060,#122337,#122338);
#103097=AXIS2_PLACEMENT_3D('',#203061,#122339,#122340);
#103098=AXIS2_PLACEMENT_3D('',#203062,#122341,#122342);
#103099=AXIS2_PLACEMENT_3D('',#203063,#122343,#122344);
#103100=AXIS2_PLACEMENT_3D('',#203064,#122345,#122346);
#103101=AXIS2_PLACEMENT_3D('',#203077,#122347,#122348);
#103102=AXIS2_PLACEMENT_3D('',#203078,#122349,#122350);
#103103=AXIS2_PLACEMENT_3D('',#203079,#122351,#122352);
#103104=AXIS2_PLACEMENT_3D('',#203080,#122353,#122354);
#103105=AXIS2_PLACEMENT_3D('',#203081,#122355,#122356);
#103106=AXIS2_PLACEMENT_3D('',#203094,#122357,#122358);
#103107=AXIS2_PLACEMENT_3D('',#203095,#122359,#122360);
#103108=AXIS2_PLACEMENT_3D('',#203096,#122361,#122362);
#103109=AXIS2_PLACEMENT_3D('',#203097,#122363,#122364);
#103110=AXIS2_PLACEMENT_3D('',#203098,#122365,#122366);
#103111=AXIS2_PLACEMENT_3D('',#203111,#122367,#122368);
#103112=AXIS2_PLACEMENT_3D('',#203124,#122369,#122370);
#103113=AXIS2_PLACEMENT_3D('',#203125,#122371,#122372);
#103114=AXIS2_PLACEMENT_3D('',#203126,#122373,#122374);
#103115=AXIS2_PLACEMENT_3D('',#203127,#122375,#122376);
#103116=AXIS2_PLACEMENT_3D('',#203128,#122377,#122378);
#103117=AXIS2_PLACEMENT_3D('',#203147,#122379,#122380);
#103118=AXIS2_PLACEMENT_3D('',#203148,#122381,#122382);
#103119=AXIS2_PLACEMENT_3D('',#203149,#122383,#122384);
#103120=AXIS2_PLACEMENT_3D('',#203150,#122385,#122386);
#103121=AXIS2_PLACEMENT_3D('',#203151,#122387,#122388);
#103122=AXIS2_PLACEMENT_3D('',#203164,#122389,#122390);
#103123=AXIS2_PLACEMENT_3D('',#203183,#122391,#122392);
#103124=AXIS2_PLACEMENT_3D('',#203184,#122393,#122394);
#103125=AXIS2_PLACEMENT_3D('',#203185,#122395,#122396);
#103126=AXIS2_PLACEMENT_3D('',#203186,#122397,#122398);
#103127=AXIS2_PLACEMENT_3D('',#203187,#122399,#122400);
#103128=AXIS2_PLACEMENT_3D('',#203206,#122401,#122402);
#103129=AXIS2_PLACEMENT_3D('',#203219,#122403,#122404);
#103130=AXIS2_PLACEMENT_3D('',#203220,#122405,#122406);
#103131=AXIS2_PLACEMENT_3D('',#203221,#122407,#122408);
#103132=AXIS2_PLACEMENT_3D('',#203222,#122409,#122410);
#103133=AXIS2_PLACEMENT_3D('',#203223,#122411,#122412);
#103134=AXIS2_PLACEMENT_3D('',#203242,#122413,#122414);
#103135=AXIS2_PLACEMENT_3D('',#203243,#122415,#122416);
#103136=AXIS2_PLACEMENT_3D('',#203244,#122417,#122418);
#103137=AXIS2_PLACEMENT_3D('',#203245,#122419,#122420);
#103138=AXIS2_PLACEMENT_3D('',#203246,#122421,#122422);
#103139=AXIS2_PLACEMENT_3D('',#203259,#122423,#122424);
#103140=AXIS2_PLACEMENT_3D('',#203272,#122425,#122426);
#103141=AXIS2_PLACEMENT_3D('',#203273,#122427,#122428);
#103142=AXIS2_PLACEMENT_3D('',#203274,#122429,#122430);
#103143=AXIS2_PLACEMENT_3D('',#203275,#122431,#122432);
#103144=AXIS2_PLACEMENT_3D('',#203276,#122433,#122434);
#103145=AXIS2_PLACEMENT_3D('',#203289,#122435,#122436);
#103146=AXIS2_PLACEMENT_3D('',#203290,#122437,#122438);
#103147=AXIS2_PLACEMENT_3D('',#203291,#122439,#122440);
#103148=AXIS2_PLACEMENT_3D('',#203292,#122441,#122442);
#103149=AXIS2_PLACEMENT_3D('',#203293,#122443,#122444);
#103150=AXIS2_PLACEMENT_3D('',#203306,#122445,#122446);
#103151=AXIS2_PLACEMENT_3D('',#203307,#122447,#122448);
#103152=AXIS2_PLACEMENT_3D('',#203308,#122449,#122450);
#103153=AXIS2_PLACEMENT_3D('',#203309,#122451,#122452);
#103154=AXIS2_PLACEMENT_3D('',#203310,#122453,#122454);
#103155=AXIS2_PLACEMENT_3D('',#203323,#122455,#122456);
#103156=AXIS2_PLACEMENT_3D('',#203336,#122457,#122458);
#103157=AXIS2_PLACEMENT_3D('',#203337,#122459,#122460);
#103158=AXIS2_PLACEMENT_3D('',#203338,#122461,#122462);
#103159=AXIS2_PLACEMENT_3D('',#203339,#122463,#122464);
#103160=AXIS2_PLACEMENT_3D('',#203340,#122465,#122466);
#103161=AXIS2_PLACEMENT_3D('',#203359,#122467,#122468);
#103162=AXIS2_PLACEMENT_3D('',#203360,#122469,#122470);
#103163=AXIS2_PLACEMENT_3D('',#203361,#122471,#122472);
#103164=AXIS2_PLACEMENT_3D('',#203362,#122473,#122474);
#103165=AXIS2_PLACEMENT_3D('',#203363,#122475,#122476);
#103166=AXIS2_PLACEMENT_3D('',#203376,#122477,#122478);
#103167=AXIS2_PLACEMENT_3D('',#203395,#122479,#122480);
#103168=AXIS2_PLACEMENT_3D('',#203396,#122481,#122482);
#103169=AXIS2_PLACEMENT_3D('',#203397,#122483,#122484);
#103170=AXIS2_PLACEMENT_3D('',#203398,#122485,#122486);
#103171=AXIS2_PLACEMENT_3D('',#203399,#122487,#122488);
#103172=AXIS2_PLACEMENT_3D('',#203418,#122489,#122490);
#103173=AXIS2_PLACEMENT_3D('',#203431,#122491,#122492);
#103174=AXIS2_PLACEMENT_3D('',#203432,#122493,#122494);
#103175=AXIS2_PLACEMENT_3D('',#203433,#122495,#122496);
#103176=AXIS2_PLACEMENT_3D('',#203434,#122497,#122498);
#103177=AXIS2_PLACEMENT_3D('',#203435,#122499,#122500);
#103178=AXIS2_PLACEMENT_3D('',#203454,#122501,#122502);
#103179=AXIS2_PLACEMENT_3D('',#203455,#122503,#122504);
#103180=AXIS2_PLACEMENT_3D('',#203456,#122505,#122506);
#103181=AXIS2_PLACEMENT_3D('',#203457,#122507,#122508);
#103182=AXIS2_PLACEMENT_3D('',#203458,#122509,#122510);
#103183=AXIS2_PLACEMENT_3D('',#203471,#122511,#122512);
#103184=AXIS2_PLACEMENT_3D('',#203484,#122513,#122514);
#103185=AXIS2_PLACEMENT_3D('',#203485,#122515,#122516);
#103186=AXIS2_PLACEMENT_3D('',#203486,#122517,#122518);
#103187=AXIS2_PLACEMENT_3D('',#203487,#122519,#122520);
#103188=AXIS2_PLACEMENT_3D('',#203488,#122521,#122522);
#103189=AXIS2_PLACEMENT_3D('',#203501,#122523,#122524);
#103190=AXIS2_PLACEMENT_3D('',#203502,#122525,#122526);
#103191=AXIS2_PLACEMENT_3D('',#203503,#122527,#122528);
#103192=AXIS2_PLACEMENT_3D('',#203504,#122529,#122530);
#103193=AXIS2_PLACEMENT_3D('',#203505,#122531,#122532);
#103194=AXIS2_PLACEMENT_3D('',#203518,#122533,#122534);
#103195=AXIS2_PLACEMENT_3D('',#203519,#122535,#122536);
#103196=AXIS2_PLACEMENT_3D('',#203520,#122537,#122538);
#103197=AXIS2_PLACEMENT_3D('',#203521,#122539,#122540);
#103198=AXIS2_PLACEMENT_3D('',#203522,#122541,#122542);
#103199=AXIS2_PLACEMENT_3D('',#203535,#122543,#122544);
#103200=AXIS2_PLACEMENT_3D('',#203548,#122545,#122546);
#103201=AXIS2_PLACEMENT_3D('',#203549,#122547,#122548);
#103202=AXIS2_PLACEMENT_3D('',#203550,#122549,#122550);
#103203=AXIS2_PLACEMENT_3D('',#203551,#122551,#122552);
#103204=AXIS2_PLACEMENT_3D('',#203552,#122553,#122554);
#103205=AXIS2_PLACEMENT_3D('',#203571,#122555,#122556);
#103206=AXIS2_PLACEMENT_3D('',#203572,#122557,#122558);
#103207=AXIS2_PLACEMENT_3D('',#203573,#122559,#122560);
#103208=AXIS2_PLACEMENT_3D('',#203574,#122561,#122562);
#103209=AXIS2_PLACEMENT_3D('',#203575,#122563,#122564);
#103210=AXIS2_PLACEMENT_3D('',#203588,#122565,#122566);
#103211=AXIS2_PLACEMENT_3D('',#203607,#122567,#122568);
#103212=AXIS2_PLACEMENT_3D('',#203608,#122569,#122570);
#103213=AXIS2_PLACEMENT_3D('',#203609,#122571,#122572);
#103214=AXIS2_PLACEMENT_3D('',#203610,#122573,#122574);
#103215=AXIS2_PLACEMENT_3D('',#203611,#122575,#122576);
#103216=AXIS2_PLACEMENT_3D('',#203630,#122577,#122578);
#103217=AXIS2_PLACEMENT_3D('',#203643,#122579,#122580);
#103218=AXIS2_PLACEMENT_3D('',#203644,#122581,#122582);
#103219=AXIS2_PLACEMENT_3D('',#203645,#122583,#122584);
#103220=AXIS2_PLACEMENT_3D('',#203646,#122585,#122586);
#103221=AXIS2_PLACEMENT_3D('',#203647,#122587,#122588);
#103222=AXIS2_PLACEMENT_3D('',#203666,#122589,#122590);
#103223=AXIS2_PLACEMENT_3D('',#203667,#122591,#122592);
#103224=AXIS2_PLACEMENT_3D('',#203668,#122593,#122594);
#103225=AXIS2_PLACEMENT_3D('',#203669,#122595,#122596);
#103226=AXIS2_PLACEMENT_3D('',#203670,#122597,#122598);
#103227=AXIS2_PLACEMENT_3D('',#203683,#122599,#122600);
#103228=AXIS2_PLACEMENT_3D('',#203696,#122601,#122602);
#103229=AXIS2_PLACEMENT_3D('',#203697,#122603,#122604);
#103230=AXIS2_PLACEMENT_3D('',#203698,#122605,#122606);
#103231=AXIS2_PLACEMENT_3D('',#203699,#122607,#122608);
#103232=AXIS2_PLACEMENT_3D('',#203700,#122609,#122610);
#103233=AXIS2_PLACEMENT_3D('',#203713,#122611,#122612);
#103234=AXIS2_PLACEMENT_3D('',#203714,#122613,#122614);
#103235=AXIS2_PLACEMENT_3D('',#203715,#122615,#122616);
#103236=AXIS2_PLACEMENT_3D('',#203716,#122617,#122618);
#103237=AXIS2_PLACEMENT_3D('',#203717,#122619,#122620);
#103238=AXIS2_PLACEMENT_3D('',#203730,#122621,#122622);
#103239=AXIS2_PLACEMENT_3D('',#203731,#122623,#122624);
#103240=AXIS2_PLACEMENT_3D('',#203732,#122625,#122626);
#103241=AXIS2_PLACEMENT_3D('',#203733,#122627,#122628);
#103242=AXIS2_PLACEMENT_3D('',#203734,#122629,#122630);
#103243=AXIS2_PLACEMENT_3D('',#203747,#122631,#122632);
#103244=AXIS2_PLACEMENT_3D('',#203760,#122633,#122634);
#103245=AXIS2_PLACEMENT_3D('',#203761,#122635,#122636);
#103246=AXIS2_PLACEMENT_3D('',#203762,#122637,#122638);
#103247=AXIS2_PLACEMENT_3D('',#203763,#122639,#122640);
#103248=AXIS2_PLACEMENT_3D('',#203764,#122641,#122642);
#103249=AXIS2_PLACEMENT_3D('',#203783,#122643,#122644);
#103250=AXIS2_PLACEMENT_3D('',#203784,#122645,#122646);
#103251=AXIS2_PLACEMENT_3D('',#203785,#122647,#122648);
#103252=AXIS2_PLACEMENT_3D('',#203786,#122649,#122650);
#103253=AXIS2_PLACEMENT_3D('',#203787,#122651,#122652);
#103254=AXIS2_PLACEMENT_3D('',#203800,#122653,#122654);
#103255=AXIS2_PLACEMENT_3D('',#203819,#122655,#122656);
#103256=AXIS2_PLACEMENT_3D('',#203820,#122657,#122658);
#103257=AXIS2_PLACEMENT_3D('',#203821,#122659,#122660);
#103258=AXIS2_PLACEMENT_3D('',#203822,#122661,#122662);
#103259=AXIS2_PLACEMENT_3D('',#203823,#122663,#122664);
#103260=AXIS2_PLACEMENT_3D('',#203842,#122665,#122666);
#103261=AXIS2_PLACEMENT_3D('',#203855,#122667,#122668);
#103262=AXIS2_PLACEMENT_3D('',#203856,#122669,#122670);
#103263=AXIS2_PLACEMENT_3D('',#203857,#122671,#122672);
#103264=AXIS2_PLACEMENT_3D('',#203858,#122673,#122674);
#103265=AXIS2_PLACEMENT_3D('',#203859,#122675,#122676);
#103266=AXIS2_PLACEMENT_3D('',#203878,#122677,#122678);
#103267=AXIS2_PLACEMENT_3D('',#203879,#122679,#122680);
#103268=AXIS2_PLACEMENT_3D('',#203880,#122681,#122682);
#103269=AXIS2_PLACEMENT_3D('',#203881,#122683,#122684);
#103270=AXIS2_PLACEMENT_3D('',#203882,#122685,#122686);
#103271=AXIS2_PLACEMENT_3D('',#203895,#122687,#122688);
#103272=AXIS2_PLACEMENT_3D('',#203908,#122689,#122690);
#103273=AXIS2_PLACEMENT_3D('',#203909,#122691,#122692);
#103274=AXIS2_PLACEMENT_3D('',#203910,#122693,#122694);
#103275=AXIS2_PLACEMENT_3D('',#203911,#122695,#122696);
#103276=AXIS2_PLACEMENT_3D('',#203912,#122697,#122698);
#103277=AXIS2_PLACEMENT_3D('',#203925,#122699,#122700);
#103278=AXIS2_PLACEMENT_3D('',#203926,#122701,#122702);
#103279=AXIS2_PLACEMENT_3D('',#203927,#122703,#122704);
#103280=AXIS2_PLACEMENT_3D('',#203928,#122705,#122706);
#103281=AXIS2_PLACEMENT_3D('',#203929,#122707,#122708);
#103282=AXIS2_PLACEMENT_3D('',#203942,#122709,#122710);
#103283=AXIS2_PLACEMENT_3D('',#203943,#122711,#122712);
#103284=AXIS2_PLACEMENT_3D('',#203944,#122713,#122714);
#103285=AXIS2_PLACEMENT_3D('',#203945,#122715,#122716);
#103286=AXIS2_PLACEMENT_3D('',#203946,#122717,#122718);
#103287=AXIS2_PLACEMENT_3D('',#203959,#122719,#122720);
#103288=AXIS2_PLACEMENT_3D('',#203972,#122721,#122722);
#103289=AXIS2_PLACEMENT_3D('',#203973,#122723,#122724);
#103290=AXIS2_PLACEMENT_3D('',#203974,#122725,#122726);
#103291=AXIS2_PLACEMENT_3D('',#203975,#122727,#122728);
#103292=AXIS2_PLACEMENT_3D('',#203976,#122729,#122730);
#103293=AXIS2_PLACEMENT_3D('',#203995,#122731,#122732);
#103294=AXIS2_PLACEMENT_3D('',#203996,#122733,#122734);
#103295=AXIS2_PLACEMENT_3D('',#203997,#122735,#122736);
#103296=AXIS2_PLACEMENT_3D('',#203998,#122737,#122738);
#103297=AXIS2_PLACEMENT_3D('',#203999,#122739,#122740);
#103298=AXIS2_PLACEMENT_3D('',#204012,#122741,#122742);
#103299=AXIS2_PLACEMENT_3D('',#204031,#122743,#122744);
#103300=AXIS2_PLACEMENT_3D('',#204032,#122745,#122746);
#103301=AXIS2_PLACEMENT_3D('',#204033,#122747,#122748);
#103302=AXIS2_PLACEMENT_3D('',#204034,#122749,#122750);
#103303=AXIS2_PLACEMENT_3D('',#204035,#122751,#122752);
#103304=AXIS2_PLACEMENT_3D('',#204054,#122753,#122754);
#103305=AXIS2_PLACEMENT_3D('',#204067,#122755,#122756);
#103306=AXIS2_PLACEMENT_3D('',#204068,#122757,#122758);
#103307=AXIS2_PLACEMENT_3D('',#204069,#122759,#122760);
#103308=AXIS2_PLACEMENT_3D('',#204070,#122761,#122762);
#103309=AXIS2_PLACEMENT_3D('',#204071,#122763,#122764);
#103310=AXIS2_PLACEMENT_3D('',#204090,#122765,#122766);
#103311=AXIS2_PLACEMENT_3D('',#204091,#122767,#122768);
#103312=AXIS2_PLACEMENT_3D('',#204092,#122769,#122770);
#103313=AXIS2_PLACEMENT_3D('',#204093,#122771,#122772);
#103314=AXIS2_PLACEMENT_3D('',#204094,#122773,#122774);
#103315=AXIS2_PLACEMENT_3D('',#204107,#122775,#122776);
#103316=AXIS2_PLACEMENT_3D('',#204120,#122777,#122778);
#103317=AXIS2_PLACEMENT_3D('',#204121,#122779,#122780);
#103318=AXIS2_PLACEMENT_3D('',#204122,#122781,#122782);
#103319=AXIS2_PLACEMENT_3D('',#204123,#122783,#122784);
#103320=AXIS2_PLACEMENT_3D('',#204124,#122785,#122786);
#103321=AXIS2_PLACEMENT_3D('',#204137,#122787,#122788);
#103322=AXIS2_PLACEMENT_3D('',#204138,#122789,#122790);
#103323=AXIS2_PLACEMENT_3D('',#204139,#122791,#122792);
#103324=AXIS2_PLACEMENT_3D('',#204140,#122793,#122794);
#103325=AXIS2_PLACEMENT_3D('',#204141,#122795,#122796);
#103326=AXIS2_PLACEMENT_3D('',#204154,#122797,#122798);
#103327=AXIS2_PLACEMENT_3D('',#204155,#122799,#122800);
#103328=AXIS2_PLACEMENT_3D('',#204156,#122801,#122802);
#103329=AXIS2_PLACEMENT_3D('',#204157,#122803,#122804);
#103330=AXIS2_PLACEMENT_3D('',#204158,#122805,#122806);
#103331=AXIS2_PLACEMENT_3D('',#204171,#122807,#122808);
#103332=AXIS2_PLACEMENT_3D('',#204184,#122809,#122810);
#103333=AXIS2_PLACEMENT_3D('',#204185,#122811,#122812);
#103334=AXIS2_PLACEMENT_3D('',#204186,#122813,#122814);
#103335=AXIS2_PLACEMENT_3D('',#204187,#122815,#122816);
#103336=AXIS2_PLACEMENT_3D('',#204188,#122817,#122818);
#103337=AXIS2_PLACEMENT_3D('',#204207,#122819,#122820);
#103338=AXIS2_PLACEMENT_3D('',#204208,#122821,#122822);
#103339=AXIS2_PLACEMENT_3D('',#204221,#122823,#122824);
#103340=AXIS2_PLACEMENT_3D('',#204240,#122825,#122826);
#103341=AXIS2_PLACEMENT_3D('',#204241,#122827,#122828);
#103342=AXIS2_PLACEMENT_3D('',#204242,#122829,#122830);
#103343=AXIS2_PLACEMENT_3D('',#204243,#122831,#122832);
#103344=AXIS2_PLACEMENT_3D('',#204244,#122833,#122834);
#103345=AXIS2_PLACEMENT_3D('',#204275,#122835,#122836);
#103346=AXIS2_PLACEMENT_3D('',#204276,#122837,#122838);
#103347=AXIS2_PLACEMENT_3D('',#204277,#122839,#122840);
#103348=AXIS2_PLACEMENT_3D('',#204296,#122841,#122842);
#103349=AXIS2_PLACEMENT_3D('',#204297,#122843,#122844);
#103350=AXIS2_PLACEMENT_3D('',#204298,#122845,#122846);
#103351=AXIS2_PLACEMENT_3D('',#204299,#122847,#122848);
#103352=AXIS2_PLACEMENT_3D('',#204300,#122849,#122850);
#103353=AXIS2_PLACEMENT_3D('',#204313,#122851,#122852);
#103354=AXIS2_PLACEMENT_3D('',#204326,#122853,#122854);
#103355=AXIS2_PLACEMENT_3D('',#204327,#122855,#122856);
#103356=AXIS2_PLACEMENT_3D('',#204328,#122857,#122858);
#103357=AXIS2_PLACEMENT_3D('',#204329,#122859,#122860);
#103358=AXIS2_PLACEMENT_3D('',#204330,#122861,#122862);
#103359=AXIS2_PLACEMENT_3D('',#204343,#122863,#122864);
#103360=AXIS2_PLACEMENT_3D('',#204344,#122865,#122866);
#103361=AXIS2_PLACEMENT_3D('',#204345,#122867,#122868);
#103362=AXIS2_PLACEMENT_3D('',#204346,#122869,#122870);
#103363=AXIS2_PLACEMENT_3D('',#204347,#122871,#122872);
#103364=AXIS2_PLACEMENT_3D('',#204360,#122873,#122874);
#103365=AXIS2_PLACEMENT_3D('',#204361,#122875,#122876);
#103366=AXIS2_PLACEMENT_3D('',#204362,#122877,#122878);
#103367=AXIS2_PLACEMENT_3D('',#204363,#122879,#122880);
#103368=AXIS2_PLACEMENT_3D('',#204364,#122881,#122882);
#103369=AXIS2_PLACEMENT_3D('',#204377,#122883,#122884);
#103370=AXIS2_PLACEMENT_3D('',#204390,#122885,#122886);
#103371=AXIS2_PLACEMENT_3D('',#204391,#122887,#122888);
#103372=AXIS2_PLACEMENT_3D('',#204392,#122889,#122890);
#103373=AXIS2_PLACEMENT_3D('',#204393,#122891,#122892);
#103374=AXIS2_PLACEMENT_3D('',#204394,#122893,#122894);
#103375=AXIS2_PLACEMENT_3D('',#204413,#122895,#122896);
#103376=AXIS2_PLACEMENT_3D('',#204414,#122897,#122898);
#103377=AXIS2_PLACEMENT_3D('',#204415,#122899,#122900);
#103378=AXIS2_PLACEMENT_3D('',#204416,#122901,#122902);
#103379=AXIS2_PLACEMENT_3D('',#204417,#122903,#122904);
#103380=AXIS2_PLACEMENT_3D('',#204430,#122905,#122906);
#103381=AXIS2_PLACEMENT_3D('',#204449,#122907,#122908);
#103382=AXIS2_PLACEMENT_3D('',#204450,#122909,#122910);
#103383=AXIS2_PLACEMENT_3D('',#204451,#122911,#122912);
#103384=AXIS2_PLACEMENT_3D('',#204452,#122913,#122914);
#103385=AXIS2_PLACEMENT_3D('',#204453,#122915,#122916);
#103386=AXIS2_PLACEMENT_3D('',#204472,#122917,#122918);
#103387=AXIS2_PLACEMENT_3D('',#204485,#122919,#122920);
#103388=AXIS2_PLACEMENT_3D('',#204486,#122921,#122922);
#103389=AXIS2_PLACEMENT_3D('',#204487,#122923,#122924);
#103390=AXIS2_PLACEMENT_3D('',#204488,#122925,#122926);
#103391=AXIS2_PLACEMENT_3D('',#204489,#122927,#122928);
#103392=AXIS2_PLACEMENT_3D('',#204508,#122929,#122930);
#103393=AXIS2_PLACEMENT_3D('',#204509,#122931,#122932);
#103394=AXIS2_PLACEMENT_3D('',#204510,#122933,#122934);
#103395=AXIS2_PLACEMENT_3D('',#204511,#122935,#122936);
#103396=AXIS2_PLACEMENT_3D('',#204512,#122937,#122938);
#103397=AXIS2_PLACEMENT_3D('',#204525,#122939,#122940);
#103398=AXIS2_PLACEMENT_3D('',#204538,#122941,#122942);
#103399=AXIS2_PLACEMENT_3D('',#204539,#122943,#122944);
#103400=AXIS2_PLACEMENT_3D('',#204540,#122945,#122946);
#103401=AXIS2_PLACEMENT_3D('',#204541,#122947,#122948);
#103402=AXIS2_PLACEMENT_3D('',#204542,#122949,#122950);
#103403=AXIS2_PLACEMENT_3D('',#204555,#122951,#122952);
#103404=AXIS2_PLACEMENT_3D('',#204556,#122953,#122954);
#103405=AXIS2_PLACEMENT_3D('',#204557,#122955,#122956);
#103406=AXIS2_PLACEMENT_3D('',#204558,#122957,#122958);
#103407=AXIS2_PLACEMENT_3D('',#204559,#122959,#122960);
#103408=AXIS2_PLACEMENT_3D('',#204572,#122961,#122962);
#103409=AXIS2_PLACEMENT_3D('',#204573,#122963,#122964);
#103410=AXIS2_PLACEMENT_3D('',#204574,#122965,#122966);
#103411=AXIS2_PLACEMENT_3D('',#204575,#122967,#122968);
#103412=AXIS2_PLACEMENT_3D('',#204576,#122969,#122970);
#103413=AXIS2_PLACEMENT_3D('',#204589,#122971,#122972);
#103414=AXIS2_PLACEMENT_3D('',#204602,#122973,#122974);
#103415=AXIS2_PLACEMENT_3D('',#204603,#122975,#122976);
#103416=AXIS2_PLACEMENT_3D('',#204604,#122977,#122978);
#103417=AXIS2_PLACEMENT_3D('',#204605,#122979,#122980);
#103418=AXIS2_PLACEMENT_3D('',#204606,#122981,#122982);
#103419=AXIS2_PLACEMENT_3D('',#204625,#122983,#122984);
#103420=AXIS2_PLACEMENT_3D('',#204626,#122985,#122986);
#103421=AXIS2_PLACEMENT_3D('',#204627,#122987,#122988);
#103422=AXIS2_PLACEMENT_3D('',#204628,#122989,#122990);
#103423=AXIS2_PLACEMENT_3D('',#204629,#122991,#122992);
#103424=AXIS2_PLACEMENT_3D('',#204642,#122993,#122994);
#103425=AXIS2_PLACEMENT_3D('',#204661,#122995,#122996);
#103426=AXIS2_PLACEMENT_3D('',#204662,#122997,#122998);
#103427=AXIS2_PLACEMENT_3D('',#204663,#122999,#123000);
#103428=AXIS2_PLACEMENT_3D('',#204664,#123001,#123002);
#103429=AXIS2_PLACEMENT_3D('',#204665,#123003,#123004);
#103430=AXIS2_PLACEMENT_3D('',#204684,#123005,#123006);
#103431=AXIS2_PLACEMENT_3D('',#204697,#123007,#123008);
#103432=AXIS2_PLACEMENT_3D('',#204698,#123009,#123010);
#103433=AXIS2_PLACEMENT_3D('',#204699,#123011,#123012);
#103434=AXIS2_PLACEMENT_3D('',#204700,#123013,#123014);
#103435=AXIS2_PLACEMENT_3D('',#204701,#123015,#123016);
#103436=AXIS2_PLACEMENT_3D('',#204720,#123017,#123018);
#103437=AXIS2_PLACEMENT_3D('',#204721,#123019,#123020);
#103438=AXIS2_PLACEMENT_3D('',#204722,#123021,#123022);
#103439=AXIS2_PLACEMENT_3D('',#204723,#123023,#123024);
#103440=AXIS2_PLACEMENT_3D('',#204724,#123025,#123026);
#103441=AXIS2_PLACEMENT_3D('',#204737,#123027,#123028);
#103442=AXIS2_PLACEMENT_3D('',#204750,#123029,#123030);
#103443=AXIS2_PLACEMENT_3D('',#204751,#123031,#123032);
#103444=AXIS2_PLACEMENT_3D('',#204752,#123033,#123034);
#103445=AXIS2_PLACEMENT_3D('',#204753,#123035,#123036);
#103446=AXIS2_PLACEMENT_3D('',#204754,#123037,#123038);
#103447=AXIS2_PLACEMENT_3D('',#204767,#123039,#123040);
#103448=AXIS2_PLACEMENT_3D('',#204768,#123041,#123042);
#103449=AXIS2_PLACEMENT_3D('',#204769,#123043,#123044);
#103450=AXIS2_PLACEMENT_3D('',#204770,#123045,#123046);
#103451=AXIS2_PLACEMENT_3D('',#204771,#123047,#123048);
#103452=AXIS2_PLACEMENT_3D('',#204784,#123049,#123050);
#103453=AXIS2_PLACEMENT_3D('',#204785,#123051,#123052);
#103454=AXIS2_PLACEMENT_3D('',#204786,#123053,#123054);
#103455=AXIS2_PLACEMENT_3D('',#204787,#123055,#123056);
#103456=AXIS2_PLACEMENT_3D('',#204788,#123057,#123058);
#103457=AXIS2_PLACEMENT_3D('',#204801,#123059,#123060);
#103458=AXIS2_PLACEMENT_3D('',#204814,#123061,#123062);
#103459=AXIS2_PLACEMENT_3D('',#204815,#123063,#123064);
#103460=AXIS2_PLACEMENT_3D('',#204816,#123065,#123066);
#103461=AXIS2_PLACEMENT_3D('',#204817,#123067,#123068);
#103462=AXIS2_PLACEMENT_3D('',#204818,#123069,#123070);
#103463=AXIS2_PLACEMENT_3D('',#204837,#123071,#123072);
#103464=AXIS2_PLACEMENT_3D('',#204838,#123073,#123074);
#103465=AXIS2_PLACEMENT_3D('',#204839,#123075,#123076);
#103466=AXIS2_PLACEMENT_3D('',#204840,#123077,#123078);
#103467=AXIS2_PLACEMENT_3D('',#204841,#123079,#123080);
#103468=AXIS2_PLACEMENT_3D('',#204854,#123081,#123082);
#103469=AXIS2_PLACEMENT_3D('',#204873,#123083,#123084);
#103470=AXIS2_PLACEMENT_3D('',#204874,#123085,#123086);
#103471=AXIS2_PLACEMENT_3D('',#204875,#123087,#123088);
#103472=AXIS2_PLACEMENT_3D('',#204876,#123089,#123090);
#103473=AXIS2_PLACEMENT_3D('',#204877,#123091,#123092);
#103474=AXIS2_PLACEMENT_3D('',#204896,#123093,#123094);
#103475=AXIS2_PLACEMENT_3D('',#204909,#123095,#123096);
#103476=AXIS2_PLACEMENT_3D('',#204910,#123097,#123098);
#103477=AXIS2_PLACEMENT_3D('',#204911,#123099,#123100);
#103478=AXIS2_PLACEMENT_3D('',#204912,#123101,#123102);
#103479=AXIS2_PLACEMENT_3D('',#204913,#123103,#123104);
#103480=AXIS2_PLACEMENT_3D('',#204932,#123105,#123106);
#103481=AXIS2_PLACEMENT_3D('',#204933,#123107,#123108);
#103482=AXIS2_PLACEMENT_3D('',#204934,#123109,#123110);
#103483=AXIS2_PLACEMENT_3D('',#204935,#123111,#123112);
#103484=AXIS2_PLACEMENT_3D('',#204936,#123113,#123114);
#103485=AXIS2_PLACEMENT_3D('',#204949,#123115,#123116);
#103486=AXIS2_PLACEMENT_3D('',#204962,#123117,#123118);
#103487=AXIS2_PLACEMENT_3D('',#204963,#123119,#123120);
#103488=AXIS2_PLACEMENT_3D('',#204964,#123121,#123122);
#103489=AXIS2_PLACEMENT_3D('',#204965,#123123,#123124);
#103490=AXIS2_PLACEMENT_3D('',#204966,#123125,#123126);
#103491=AXIS2_PLACEMENT_3D('',#204979,#123127,#123128);
#103492=AXIS2_PLACEMENT_3D('',#204980,#123129,#123130);
#103493=AXIS2_PLACEMENT_3D('',#204981,#123131,#123132);
#103494=AXIS2_PLACEMENT_3D('',#204982,#123133,#123134);
#103495=AXIS2_PLACEMENT_3D('',#204983,#123135,#123136);
#103496=AXIS2_PLACEMENT_3D('',#204996,#123137,#123138);
#103497=AXIS2_PLACEMENT_3D('',#204997,#123139,#123140);
#103498=AXIS2_PLACEMENT_3D('',#204998,#123141,#123142);
#103499=AXIS2_PLACEMENT_3D('',#204999,#123143,#123144);
#103500=AXIS2_PLACEMENT_3D('',#205000,#123145,#123146);
#103501=AXIS2_PLACEMENT_3D('',#205013,#123147,#123148);
#103502=AXIS2_PLACEMENT_3D('',#205026,#123149,#123150);
#103503=AXIS2_PLACEMENT_3D('',#205027,#123151,#123152);
#103504=AXIS2_PLACEMENT_3D('',#205028,#123153,#123154);
#103505=AXIS2_PLACEMENT_3D('',#205029,#123155,#123156);
#103506=AXIS2_PLACEMENT_3D('',#205030,#123157,#123158);
#103507=AXIS2_PLACEMENT_3D('',#205049,#123159,#123160);
#103508=AXIS2_PLACEMENT_3D('',#205050,#123161,#123162);
#103509=AXIS2_PLACEMENT_3D('',#205051,#123163,#123164);
#103510=AXIS2_PLACEMENT_3D('',#205052,#123165,#123166);
#103511=AXIS2_PLACEMENT_3D('',#205053,#123167,#123168);
#103512=AXIS2_PLACEMENT_3D('',#205066,#123169,#123170);
#103513=AXIS2_PLACEMENT_3D('',#205085,#123171,#123172);
#103514=AXIS2_PLACEMENT_3D('',#205086,#123173,#123174);
#103515=AXIS2_PLACEMENT_3D('',#205087,#123175,#123176);
#103516=AXIS2_PLACEMENT_3D('',#205088,#123177,#123178);
#103517=AXIS2_PLACEMENT_3D('',#205089,#123179,#123180);
#103518=AXIS2_PLACEMENT_3D('',#205108,#123181,#123182);
#103519=AXIS2_PLACEMENT_3D('',#205121,#123183,#123184);
#103520=AXIS2_PLACEMENT_3D('',#205122,#123185,#123186);
#103521=AXIS2_PLACEMENT_3D('',#205123,#123187,#123188);
#103522=AXIS2_PLACEMENT_3D('',#205124,#123189,#123190);
#103523=AXIS2_PLACEMENT_3D('',#205125,#123191,#123192);
#103524=AXIS2_PLACEMENT_3D('',#205144,#123193,#123194);
#103525=AXIS2_PLACEMENT_3D('',#205145,#123195,#123196);
#103526=AXIS2_PLACEMENT_3D('',#205146,#123197,#123198);
#103527=AXIS2_PLACEMENT_3D('',#205147,#123199,#123200);
#103528=AXIS2_PLACEMENT_3D('',#205148,#123201,#123202);
#103529=AXIS2_PLACEMENT_3D('',#205161,#123203,#123204);
#103530=AXIS2_PLACEMENT_3D('',#205174,#123205,#123206);
#103531=AXIS2_PLACEMENT_3D('',#205175,#123207,#123208);
#103532=AXIS2_PLACEMENT_3D('',#205176,#123209,#123210);
#103533=AXIS2_PLACEMENT_3D('',#205177,#123211,#123212);
#103534=AXIS2_PLACEMENT_3D('',#205178,#123213,#123214);
#103535=AXIS2_PLACEMENT_3D('',#205191,#123215,#123216);
#103536=AXIS2_PLACEMENT_3D('',#205192,#123217,#123218);
#103537=AXIS2_PLACEMENT_3D('',#205193,#123219,#123220);
#103538=AXIS2_PLACEMENT_3D('',#205194,#123221,#123222);
#103539=AXIS2_PLACEMENT_3D('',#205195,#123223,#123224);
#103540=AXIS2_PLACEMENT_3D('',#205208,#123225,#123226);
#103541=AXIS2_PLACEMENT_3D('',#205209,#123227,#123228);
#103542=AXIS2_PLACEMENT_3D('',#205210,#123229,#123230);
#103543=AXIS2_PLACEMENT_3D('',#205211,#123231,#123232);
#103544=AXIS2_PLACEMENT_3D('',#205212,#123233,#123234);
#103545=AXIS2_PLACEMENT_3D('',#205225,#123235,#123236);
#103546=AXIS2_PLACEMENT_3D('',#205238,#123237,#123238);
#103547=AXIS2_PLACEMENT_3D('',#205239,#123239,#123240);
#103548=AXIS2_PLACEMENT_3D('',#205240,#123241,#123242);
#103549=AXIS2_PLACEMENT_3D('',#205241,#123243,#123244);
#103550=AXIS2_PLACEMENT_3D('',#205242,#123245,#123246);
#103551=AXIS2_PLACEMENT_3D('',#205261,#123247,#123248);
#103552=AXIS2_PLACEMENT_3D('',#205262,#123249,#123250);
#103553=AXIS2_PLACEMENT_3D('',#205263,#123251,#123252);
#103554=AXIS2_PLACEMENT_3D('',#205264,#123253,#123254);
#103555=AXIS2_PLACEMENT_3D('',#205265,#123255,#123256);
#103556=AXIS2_PLACEMENT_3D('',#205278,#123257,#123258);
#103557=AXIS2_PLACEMENT_3D('',#205297,#123259,#123260);
#103558=AXIS2_PLACEMENT_3D('',#205298,#123261,#123262);
#103559=AXIS2_PLACEMENT_3D('',#205299,#123263,#123264);
#103560=AXIS2_PLACEMENT_3D('',#205300,#123265,#123266);
#103561=AXIS2_PLACEMENT_3D('',#205301,#123267,#123268);
#103562=AXIS2_PLACEMENT_3D('',#205320,#123269,#123270);
#103563=AXIS2_PLACEMENT_3D('',#205333,#123271,#123272);
#103564=AXIS2_PLACEMENT_3D('',#205334,#123273,#123274);
#103565=AXIS2_PLACEMENT_3D('',#205335,#123275,#123276);
#103566=AXIS2_PLACEMENT_3D('',#205336,#123277,#123278);
#103567=AXIS2_PLACEMENT_3D('',#205337,#123279,#123280);
#103568=AXIS2_PLACEMENT_3D('',#205356,#123281,#123282);
#103569=AXIS2_PLACEMENT_3D('',#205357,#123283,#123284);
#103570=AXIS2_PLACEMENT_3D('',#205358,#123285,#123286);
#103571=AXIS2_PLACEMENT_3D('',#205359,#123287,#123288);
#103572=AXIS2_PLACEMENT_3D('',#205360,#123289,#123290);
#103573=AXIS2_PLACEMENT_3D('',#205373,#123291,#123292);
#103574=AXIS2_PLACEMENT_3D('',#205386,#123293,#123294);
#103575=AXIS2_PLACEMENT_3D('',#205387,#123295,#123296);
#103576=AXIS2_PLACEMENT_3D('',#205388,#123297,#123298);
#103577=AXIS2_PLACEMENT_3D('',#205389,#123299,#123300);
#103578=AXIS2_PLACEMENT_3D('',#205390,#123301,#123302);
#103579=AXIS2_PLACEMENT_3D('',#205403,#123303,#123304);
#103580=AXIS2_PLACEMENT_3D('',#205404,#123305,#123306);
#103581=AXIS2_PLACEMENT_3D('',#205405,#123307,#123308);
#103582=AXIS2_PLACEMENT_3D('',#205406,#123309,#123310);
#103583=AXIS2_PLACEMENT_3D('',#205407,#123311,#123312);
#103584=AXIS2_PLACEMENT_3D('',#205420,#123313,#123314);
#103585=AXIS2_PLACEMENT_3D('',#205421,#123315,#123316);
#103586=AXIS2_PLACEMENT_3D('',#205422,#123317,#123318);
#103587=AXIS2_PLACEMENT_3D('',#205423,#123319,#123320);
#103588=AXIS2_PLACEMENT_3D('',#205424,#123321,#123322);
#103589=AXIS2_PLACEMENT_3D('',#205437,#123323,#123324);
#103590=AXIS2_PLACEMENT_3D('',#205450,#123325,#123326);
#103591=AXIS2_PLACEMENT_3D('',#205451,#123327,#123328);
#103592=AXIS2_PLACEMENT_3D('',#205452,#123329,#123330);
#103593=AXIS2_PLACEMENT_3D('',#205453,#123331,#123332);
#103594=AXIS2_PLACEMENT_3D('',#205454,#123333,#123334);
#103595=AXIS2_PLACEMENT_3D('',#205473,#123335,#123336);
#103596=AXIS2_PLACEMENT_3D('',#205474,#123337,#123338);
#103597=AXIS2_PLACEMENT_3D('',#205475,#123339,#123340);
#103598=AXIS2_PLACEMENT_3D('',#205476,#123341,#123342);
#103599=AXIS2_PLACEMENT_3D('',#205477,#123343,#123344);
#103600=AXIS2_PLACEMENT_3D('',#205490,#123345,#123346);
#103601=AXIS2_PLACEMENT_3D('',#205509,#123347,#123348);
#103602=AXIS2_PLACEMENT_3D('',#205510,#123349,#123350);
#103603=AXIS2_PLACEMENT_3D('',#205511,#123351,#123352);
#103604=AXIS2_PLACEMENT_3D('',#205512,#123353,#123354);
#103605=AXIS2_PLACEMENT_3D('',#205513,#123355,#123356);
#103606=AXIS2_PLACEMENT_3D('',#205532,#123357,#123358);
#103607=AXIS2_PLACEMENT_3D('',#205545,#123359,#123360);
#103608=AXIS2_PLACEMENT_3D('',#205546,#123361,#123362);
#103609=AXIS2_PLACEMENT_3D('',#205547,#123363,#123364);
#103610=AXIS2_PLACEMENT_3D('',#205548,#123365,#123366);
#103611=AXIS2_PLACEMENT_3D('',#205549,#123367,#123368);
#103612=AXIS2_PLACEMENT_3D('',#205568,#123369,#123370);
#103613=AXIS2_PLACEMENT_3D('',#205569,#123371,#123372);
#103614=AXIS2_PLACEMENT_3D('',#205570,#123373,#123374);
#103615=AXIS2_PLACEMENT_3D('',#205571,#123375,#123376);
#103616=AXIS2_PLACEMENT_3D('',#205572,#123377,#123378);
#103617=AXIS2_PLACEMENT_3D('',#205585,#123379,#123380);
#103618=AXIS2_PLACEMENT_3D('',#205598,#123381,#123382);
#103619=AXIS2_PLACEMENT_3D('',#205599,#123383,#123384);
#103620=AXIS2_PLACEMENT_3D('',#205600,#123385,#123386);
#103621=AXIS2_PLACEMENT_3D('',#205601,#123387,#123388);
#103622=AXIS2_PLACEMENT_3D('',#205602,#123389,#123390);
#103623=AXIS2_PLACEMENT_3D('',#205615,#123391,#123392);
#103624=AXIS2_PLACEMENT_3D('',#205616,#123393,#123394);
#103625=AXIS2_PLACEMENT_3D('',#205617,#123395,#123396);
#103626=AXIS2_PLACEMENT_3D('',#205618,#123397,#123398);
#103627=AXIS2_PLACEMENT_3D('',#205619,#123399,#123400);
#103628=AXIS2_PLACEMENT_3D('',#205632,#123401,#123402);
#103629=AXIS2_PLACEMENT_3D('',#205633,#123403,#123404);
#103630=AXIS2_PLACEMENT_3D('',#205634,#123405,#123406);
#103631=AXIS2_PLACEMENT_3D('',#205635,#123407,#123408);
#103632=AXIS2_PLACEMENT_3D('',#205636,#123409,#123410);
#103633=AXIS2_PLACEMENT_3D('',#205649,#123411,#123412);
#103634=AXIS2_PLACEMENT_3D('',#205662,#123413,#123414);
#103635=AXIS2_PLACEMENT_3D('',#205663,#123415,#123416);
#103636=AXIS2_PLACEMENT_3D('',#205664,#123417,#123418);
#103637=AXIS2_PLACEMENT_3D('',#205665,#123419,#123420);
#103638=AXIS2_PLACEMENT_3D('',#205666,#123421,#123422);
#103639=AXIS2_PLACEMENT_3D('',#205685,#123423,#123424);
#103640=AXIS2_PLACEMENT_3D('',#205686,#123425,#123426);
#103641=AXIS2_PLACEMENT_3D('',#205687,#123427,#123428);
#103642=AXIS2_PLACEMENT_3D('',#205688,#123429,#123430);
#103643=AXIS2_PLACEMENT_3D('',#205689,#123431,#123432);
#103644=AXIS2_PLACEMENT_3D('',#205702,#123433,#123434);
#103645=AXIS2_PLACEMENT_3D('',#205721,#123435,#123436);
#103646=AXIS2_PLACEMENT_3D('',#205722,#123437,#123438);
#103647=AXIS2_PLACEMENT_3D('',#205723,#123439,#123440);
#103648=AXIS2_PLACEMENT_3D('',#205724,#123441,#123442);
#103649=AXIS2_PLACEMENT_3D('',#205725,#123443,#123444);
#103650=AXIS2_PLACEMENT_3D('',#205744,#123445,#123446);
#103651=AXIS2_PLACEMENT_3D('',#205757,#123447,#123448);
#103652=AXIS2_PLACEMENT_3D('',#205758,#123449,#123450);
#103653=AXIS2_PLACEMENT_3D('',#205759,#123451,#123452);
#103654=AXIS2_PLACEMENT_3D('',#205760,#123453,#123454);
#103655=AXIS2_PLACEMENT_3D('',#205761,#123455,#123456);
#103656=AXIS2_PLACEMENT_3D('',#205780,#123457,#123458);
#103657=AXIS2_PLACEMENT_3D('',#205781,#123459,#123460);
#103658=AXIS2_PLACEMENT_3D('',#205782,#123461,#123462);
#103659=AXIS2_PLACEMENT_3D('',#205783,#123463,#123464);
#103660=AXIS2_PLACEMENT_3D('',#205784,#123465,#123466);
#103661=AXIS2_PLACEMENT_3D('',#205797,#123467,#123468);
#103662=AXIS2_PLACEMENT_3D('',#205810,#123469,#123470);
#103663=AXIS2_PLACEMENT_3D('',#205811,#123471,#123472);
#103664=AXIS2_PLACEMENT_3D('',#205812,#123473,#123474);
#103665=AXIS2_PLACEMENT_3D('',#205813,#123475,#123476);
#103666=AXIS2_PLACEMENT_3D('',#205814,#123477,#123478);
#103667=AXIS2_PLACEMENT_3D('',#205827,#123479,#123480);
#103668=AXIS2_PLACEMENT_3D('',#205828,#123481,#123482);
#103669=AXIS2_PLACEMENT_3D('',#205829,#123483,#123484);
#103670=AXIS2_PLACEMENT_3D('',#205830,#123485,#123486);
#103671=AXIS2_PLACEMENT_3D('',#205831,#123487,#123488);
#103672=AXIS2_PLACEMENT_3D('',#205844,#123489,#123490);
#103673=AXIS2_PLACEMENT_3D('',#205845,#123491,#123492);
#103674=AXIS2_PLACEMENT_3D('',#205846,#123493,#123494);
#103675=AXIS2_PLACEMENT_3D('',#205847,#123495,#123496);
#103676=AXIS2_PLACEMENT_3D('',#205848,#123497,#123498);
#103677=AXIS2_PLACEMENT_3D('',#205861,#123499,#123500);
#103678=AXIS2_PLACEMENT_3D('',#205874,#123501,#123502);
#103679=AXIS2_PLACEMENT_3D('',#205875,#123503,#123504);
#103680=AXIS2_PLACEMENT_3D('',#205876,#123505,#123506);
#103681=AXIS2_PLACEMENT_3D('',#205877,#123507,#123508);
#103682=AXIS2_PLACEMENT_3D('',#205878,#123509,#123510);
#103683=AXIS2_PLACEMENT_3D('',#205897,#123511,#123512);
#103684=AXIS2_PLACEMENT_3D('',#205898,#123513,#123514);
#103685=AXIS2_PLACEMENT_3D('',#205899,#123515,#123516);
#103686=AXIS2_PLACEMENT_3D('',#205900,#123517,#123518);
#103687=AXIS2_PLACEMENT_3D('',#205901,#123519,#123520);
#103688=AXIS2_PLACEMENT_3D('',#205914,#123521,#123522);
#103689=AXIS2_PLACEMENT_3D('',#205933,#123523,#123524);
#103690=AXIS2_PLACEMENT_3D('',#205934,#123525,#123526);
#103691=AXIS2_PLACEMENT_3D('',#205935,#123527,#123528);
#103692=AXIS2_PLACEMENT_3D('',#205936,#123529,#123530);
#103693=AXIS2_PLACEMENT_3D('',#205937,#123531,#123532);
#103694=AXIS2_PLACEMENT_3D('',#205956,#123533,#123534);
#103695=AXIS2_PLACEMENT_3D('',#205969,#123535,#123536);
#103696=AXIS2_PLACEMENT_3D('',#205970,#123537,#123538);
#103697=AXIS2_PLACEMENT_3D('',#205971,#123539,#123540);
#103698=AXIS2_PLACEMENT_3D('',#205972,#123541,#123542);
#103699=AXIS2_PLACEMENT_3D('',#205973,#123543,#123544);
#103700=AXIS2_PLACEMENT_3D('',#205992,#123545,#123546);
#103701=AXIS2_PLACEMENT_3D('',#205993,#123547,#123548);
#103702=AXIS2_PLACEMENT_3D('',#205994,#123549,#123550);
#103703=AXIS2_PLACEMENT_3D('',#205995,#123551,#123552);
#103704=AXIS2_PLACEMENT_3D('',#205996,#123553,#123554);
#103705=AXIS2_PLACEMENT_3D('',#206009,#123555,#123556);
#103706=AXIS2_PLACEMENT_3D('',#206022,#123557,#123558);
#103707=AXIS2_PLACEMENT_3D('',#206023,#123559,#123560);
#103708=AXIS2_PLACEMENT_3D('',#206024,#123561,#123562);
#103709=AXIS2_PLACEMENT_3D('',#206025,#123563,#123564);
#103710=AXIS2_PLACEMENT_3D('',#206026,#123565,#123566);
#103711=AXIS2_PLACEMENT_3D('',#206039,#123567,#123568);
#103712=AXIS2_PLACEMENT_3D('',#206040,#123569,#123570);
#103713=AXIS2_PLACEMENT_3D('',#206041,#123571,#123572);
#103714=AXIS2_PLACEMENT_3D('',#206042,#123573,#123574);
#103715=AXIS2_PLACEMENT_3D('',#206043,#123575,#123576);
#103716=AXIS2_PLACEMENT_3D('',#206056,#123577,#123578);
#103717=AXIS2_PLACEMENT_3D('',#206057,#123579,#123580);
#103718=AXIS2_PLACEMENT_3D('',#206058,#123581,#123582);
#103719=AXIS2_PLACEMENT_3D('',#206059,#123583,#123584);
#103720=AXIS2_PLACEMENT_3D('',#206060,#123585,#123586);
#103721=AXIS2_PLACEMENT_3D('',#206073,#123587,#123588);
#103722=AXIS2_PLACEMENT_3D('',#206086,#123589,#123590);
#103723=AXIS2_PLACEMENT_3D('',#206087,#123591,#123592);
#103724=AXIS2_PLACEMENT_3D('',#206088,#123593,#123594);
#103725=AXIS2_PLACEMENT_3D('',#206089,#123595,#123596);
#103726=AXIS2_PLACEMENT_3D('',#206090,#123597,#123598);
#103727=AXIS2_PLACEMENT_3D('',#206109,#123599,#123600);
#103728=AXIS2_PLACEMENT_3D('',#206110,#123601,#123602);
#103729=AXIS2_PLACEMENT_3D('',#206111,#123603,#123604);
#103730=AXIS2_PLACEMENT_3D('',#206112,#123605,#123606);
#103731=AXIS2_PLACEMENT_3D('',#206113,#123607,#123608);
#103732=AXIS2_PLACEMENT_3D('',#206126,#123609,#123610);
#103733=AXIS2_PLACEMENT_3D('',#206145,#123611,#123612);
#103734=AXIS2_PLACEMENT_3D('',#206146,#123613,#123614);
#103735=AXIS2_PLACEMENT_3D('',#206147,#123615,#123616);
#103736=AXIS2_PLACEMENT_3D('',#206148,#123617,#123618);
#103737=AXIS2_PLACEMENT_3D('',#206149,#123619,#123620);
#103738=AXIS2_PLACEMENT_3D('',#206168,#123621,#123622);
#103739=AXIS2_PLACEMENT_3D('',#206181,#123623,#123624);
#103740=AXIS2_PLACEMENT_3D('',#206182,#123625,#123626);
#103741=AXIS2_PLACEMENT_3D('',#206183,#123627,#123628);
#103742=AXIS2_PLACEMENT_3D('',#206184,#123629,#123630);
#103743=AXIS2_PLACEMENT_3D('',#206185,#123631,#123632);
#103744=AXIS2_PLACEMENT_3D('',#206204,#123633,#123634);
#103745=AXIS2_PLACEMENT_3D('',#206205,#123635,#123636);
#103746=AXIS2_PLACEMENT_3D('',#206206,#123637,#123638);
#103747=AXIS2_PLACEMENT_3D('',#206207,#123639,#123640);
#103748=AXIS2_PLACEMENT_3D('',#206208,#123641,#123642);
#103749=AXIS2_PLACEMENT_3D('',#206221,#123643,#123644);
#103750=AXIS2_PLACEMENT_3D('',#206234,#123645,#123646);
#103751=AXIS2_PLACEMENT_3D('',#206235,#123647,#123648);
#103752=AXIS2_PLACEMENT_3D('',#206236,#123649,#123650);
#103753=AXIS2_PLACEMENT_3D('',#206237,#123651,#123652);
#103754=AXIS2_PLACEMENT_3D('',#206238,#123653,#123654);
#103755=AXIS2_PLACEMENT_3D('',#206251,#123655,#123656);
#103756=AXIS2_PLACEMENT_3D('',#206252,#123657,#123658);
#103757=AXIS2_PLACEMENT_3D('',#206253,#123659,#123660);
#103758=AXIS2_PLACEMENT_3D('',#206254,#123661,#123662);
#103759=AXIS2_PLACEMENT_3D('',#206255,#123663,#123664);
#103760=AXIS2_PLACEMENT_3D('',#206268,#123665,#123666);
#103761=AXIS2_PLACEMENT_3D('',#206269,#123667,#123668);
#103762=AXIS2_PLACEMENT_3D('',#206270,#123669,#123670);
#103763=AXIS2_PLACEMENT_3D('',#206271,#123671,#123672);
#103764=AXIS2_PLACEMENT_3D('',#206272,#123673,#123674);
#103765=AXIS2_PLACEMENT_3D('',#206285,#123675,#123676);
#103766=AXIS2_PLACEMENT_3D('',#206298,#123677,#123678);
#103767=AXIS2_PLACEMENT_3D('',#206299,#123679,#123680);
#103768=AXIS2_PLACEMENT_3D('',#206300,#123681,#123682);
#103769=AXIS2_PLACEMENT_3D('',#206301,#123683,#123684);
#103770=AXIS2_PLACEMENT_3D('',#206302,#123685,#123686);
#103771=AXIS2_PLACEMENT_3D('',#206321,#123687,#123688);
#103772=AXIS2_PLACEMENT_3D('',#206322,#123689,#123690);
#103773=AXIS2_PLACEMENT_3D('',#206323,#123691,#123692);
#103774=AXIS2_PLACEMENT_3D('',#206324,#123693,#123694);
#103775=AXIS2_PLACEMENT_3D('',#206325,#123695,#123696);
#103776=AXIS2_PLACEMENT_3D('',#206338,#123697,#123698);
#103777=AXIS2_PLACEMENT_3D('',#206357,#123699,#123700);
#103778=AXIS2_PLACEMENT_3D('',#206358,#123701,#123702);
#103779=AXIS2_PLACEMENT_3D('',#206359,#123703,#123704);
#103780=AXIS2_PLACEMENT_3D('',#206360,#123705,#123706);
#103781=AXIS2_PLACEMENT_3D('',#206361,#123707,#123708);
#103782=AXIS2_PLACEMENT_3D('',#206380,#123709,#123710);
#103783=AXIS2_PLACEMENT_3D('',#206393,#123711,#123712);
#103784=AXIS2_PLACEMENT_3D('',#206394,#123713,#123714);
#103785=AXIS2_PLACEMENT_3D('',#206395,#123715,#123716);
#103786=AXIS2_PLACEMENT_3D('',#206396,#123717,#123718);
#103787=AXIS2_PLACEMENT_3D('',#206397,#123719,#123720);
#103788=AXIS2_PLACEMENT_3D('',#206416,#123721,#123722);
#103789=AXIS2_PLACEMENT_3D('',#206417,#123723,#123724);
#103790=AXIS2_PLACEMENT_3D('',#206418,#123725,#123726);
#103791=AXIS2_PLACEMENT_3D('',#206419,#123727,#123728);
#103792=AXIS2_PLACEMENT_3D('',#206420,#123729,#123730);
#103793=AXIS2_PLACEMENT_3D('',#206433,#123731,#123732);
#103794=AXIS2_PLACEMENT_3D('',#206446,#123733,#123734);
#103795=AXIS2_PLACEMENT_3D('',#206447,#123735,#123736);
#103796=AXIS2_PLACEMENT_3D('',#206448,#123737,#123738);
#103797=AXIS2_PLACEMENT_3D('',#206449,#123739,#123740);
#103798=AXIS2_PLACEMENT_3D('',#206450,#123741,#123742);
#103799=AXIS2_PLACEMENT_3D('',#206463,#123743,#123744);
#103800=AXIS2_PLACEMENT_3D('',#206464,#123745,#123746);
#103801=AXIS2_PLACEMENT_3D('',#206465,#123747,#123748);
#103802=AXIS2_PLACEMENT_3D('',#206466,#123749,#123750);
#103803=AXIS2_PLACEMENT_3D('',#206467,#123751,#123752);
#103804=AXIS2_PLACEMENT_3D('',#206480,#123753,#123754);
#103805=AXIS2_PLACEMENT_3D('',#206481,#123755,#123756);
#103806=AXIS2_PLACEMENT_3D('',#206482,#123757,#123758);
#103807=AXIS2_PLACEMENT_3D('',#206483,#123759,#123760);
#103808=AXIS2_PLACEMENT_3D('',#206484,#123761,#123762);
#103809=AXIS2_PLACEMENT_3D('',#206497,#123763,#123764);
#103810=AXIS2_PLACEMENT_3D('',#206510,#123765,#123766);
#103811=AXIS2_PLACEMENT_3D('',#206511,#123767,#123768);
#103812=AXIS2_PLACEMENT_3D('',#206512,#123769,#123770);
#103813=AXIS2_PLACEMENT_3D('',#206513,#123771,#123772);
#103814=AXIS2_PLACEMENT_3D('',#206514,#123773,#123774);
#103815=AXIS2_PLACEMENT_3D('',#206533,#123775,#123776);
#103816=AXIS2_PLACEMENT_3D('',#206534,#123777,#123778);
#103817=AXIS2_PLACEMENT_3D('',#206535,#123779,#123780);
#103818=AXIS2_PLACEMENT_3D('',#206536,#123781,#123782);
#103819=AXIS2_PLACEMENT_3D('',#206537,#123783,#123784);
#103820=AXIS2_PLACEMENT_3D('',#206550,#123785,#123786);
#103821=AXIS2_PLACEMENT_3D('',#206569,#123787,#123788);
#103822=AXIS2_PLACEMENT_3D('',#206570,#123789,#123790);
#103823=AXIS2_PLACEMENT_3D('',#206571,#123791,#123792);
#103824=AXIS2_PLACEMENT_3D('',#206572,#123793,#123794);
#103825=AXIS2_PLACEMENT_3D('',#206573,#123795,#123796);
#103826=AXIS2_PLACEMENT_3D('',#206592,#123797,#123798);
#103827=AXIS2_PLACEMENT_3D('',#206605,#123799,#123800);
#103828=AXIS2_PLACEMENT_3D('',#206606,#123801,#123802);
#103829=AXIS2_PLACEMENT_3D('',#206607,#123803,#123804);
#103830=AXIS2_PLACEMENT_3D('',#206608,#123805,#123806);
#103831=AXIS2_PLACEMENT_3D('',#206609,#123807,#123808);
#103832=AXIS2_PLACEMENT_3D('',#206628,#123809,#123810);
#103833=AXIS2_PLACEMENT_3D('',#206629,#123811,#123812);
#103834=AXIS2_PLACEMENT_3D('',#206630,#123813,#123814);
#103835=AXIS2_PLACEMENT_3D('',#206631,#123815,#123816);
#103836=AXIS2_PLACEMENT_3D('',#206632,#123817,#123818);
#103837=AXIS2_PLACEMENT_3D('',#206645,#123819,#123820);
#103838=AXIS2_PLACEMENT_3D('',#206658,#123821,#123822);
#103839=AXIS2_PLACEMENT_3D('',#206659,#123823,#123824);
#103840=AXIS2_PLACEMENT_3D('',#206660,#123825,#123826);
#103841=AXIS2_PLACEMENT_3D('',#206661,#123827,#123828);
#103842=AXIS2_PLACEMENT_3D('',#206662,#123829,#123830);
#103843=AXIS2_PLACEMENT_3D('',#206675,#123831,#123832);
#103844=AXIS2_PLACEMENT_3D('',#206676,#123833,#123834);
#103845=AXIS2_PLACEMENT_3D('',#206677,#123835,#123836);
#103846=AXIS2_PLACEMENT_3D('',#206678,#123837,#123838);
#103847=AXIS2_PLACEMENT_3D('',#206679,#123839,#123840);
#103848=AXIS2_PLACEMENT_3D('',#206692,#123841,#123842);
#103849=AXIS2_PLACEMENT_3D('',#206693,#123843,#123844);
#103850=AXIS2_PLACEMENT_3D('',#206694,#123845,#123846);
#103851=AXIS2_PLACEMENT_3D('',#206695,#123847,#123848);
#103852=AXIS2_PLACEMENT_3D('',#206696,#123849,#123850);
#103853=AXIS2_PLACEMENT_3D('',#206709,#123851,#123852);
#103854=AXIS2_PLACEMENT_3D('',#206722,#123853,#123854);
#103855=AXIS2_PLACEMENT_3D('',#206723,#123855,#123856);
#103856=AXIS2_PLACEMENT_3D('',#206724,#123857,#123858);
#103857=AXIS2_PLACEMENT_3D('',#206725,#123859,#123860);
#103858=AXIS2_PLACEMENT_3D('',#206726,#123861,#123862);
#103859=AXIS2_PLACEMENT_3D('',#206745,#123863,#123864);
#103860=AXIS2_PLACEMENT_3D('',#206746,#123865,#123866);
#103861=AXIS2_PLACEMENT_3D('',#206747,#123867,#123868);
#103862=AXIS2_PLACEMENT_3D('',#206748,#123869,#123870);
#103863=AXIS2_PLACEMENT_3D('',#206749,#123871,#123872);
#103864=AXIS2_PLACEMENT_3D('',#206762,#123873,#123874);
#103865=AXIS2_PLACEMENT_3D('',#206781,#123875,#123876);
#103866=AXIS2_PLACEMENT_3D('',#206782,#123877,#123878);
#103867=AXIS2_PLACEMENT_3D('',#206783,#123879,#123880);
#103868=AXIS2_PLACEMENT_3D('',#206784,#123881,#123882);
#103869=AXIS2_PLACEMENT_3D('',#206785,#123883,#123884);
#103870=AXIS2_PLACEMENT_3D('',#206804,#123885,#123886);
#103871=AXIS2_PLACEMENT_3D('',#206817,#123887,#123888);
#103872=AXIS2_PLACEMENT_3D('',#206818,#123889,#123890);
#103873=AXIS2_PLACEMENT_3D('',#206819,#123891,#123892);
#103874=AXIS2_PLACEMENT_3D('',#206820,#123893,#123894);
#103875=AXIS2_PLACEMENT_3D('',#206821,#123895,#123896);
#103876=AXIS2_PLACEMENT_3D('',#206840,#123897,#123898);
#103877=AXIS2_PLACEMENT_3D('',#206841,#123899,#123900);
#103878=AXIS2_PLACEMENT_3D('',#206842,#123901,#123902);
#103879=AXIS2_PLACEMENT_3D('',#206843,#123903,#123904);
#103880=AXIS2_PLACEMENT_3D('',#206844,#123905,#123906);
#103881=AXIS2_PLACEMENT_3D('',#206857,#123907,#123908);
#103882=AXIS2_PLACEMENT_3D('',#206870,#123909,#123910);
#103883=AXIS2_PLACEMENT_3D('',#206871,#123911,#123912);
#103884=AXIS2_PLACEMENT_3D('',#206872,#123913,#123914);
#103885=AXIS2_PLACEMENT_3D('',#206873,#123915,#123916);
#103886=AXIS2_PLACEMENT_3D('',#206874,#123917,#123918);
#103887=AXIS2_PLACEMENT_3D('',#206887,#123919,#123920);
#103888=AXIS2_PLACEMENT_3D('',#206888,#123921,#123922);
#103889=AXIS2_PLACEMENT_3D('',#206889,#123923,#123924);
#103890=AXIS2_PLACEMENT_3D('',#206890,#123925,#123926);
#103891=AXIS2_PLACEMENT_3D('',#206891,#123927,#123928);
#103892=AXIS2_PLACEMENT_3D('',#206904,#123929,#123930);
#103893=AXIS2_PLACEMENT_3D('',#206905,#123931,#123932);
#103894=AXIS2_PLACEMENT_3D('',#206906,#123933,#123934);
#103895=AXIS2_PLACEMENT_3D('',#206907,#123935,#123936);
#103896=AXIS2_PLACEMENT_3D('',#206908,#123937,#123938);
#103897=AXIS2_PLACEMENT_3D('',#206921,#123939,#123940);
#103898=AXIS2_PLACEMENT_3D('',#206934,#123941,#123942);
#103899=AXIS2_PLACEMENT_3D('',#206935,#123943,#123944);
#103900=AXIS2_PLACEMENT_3D('',#206936,#123945,#123946);
#103901=AXIS2_PLACEMENT_3D('',#206937,#123947,#123948);
#103902=AXIS2_PLACEMENT_3D('',#206938,#123949,#123950);
#103903=AXIS2_PLACEMENT_3D('',#206957,#123951,#123952);
#103904=AXIS2_PLACEMENT_3D('',#206958,#123953,#123954);
#103905=AXIS2_PLACEMENT_3D('',#206959,#123955,#123956);
#103906=AXIS2_PLACEMENT_3D('',#206960,#123957,#123958);
#103907=AXIS2_PLACEMENT_3D('',#206961,#123959,#123960);
#103908=AXIS2_PLACEMENT_3D('',#206974,#123961,#123962);
#103909=AXIS2_PLACEMENT_3D('',#206993,#123963,#123964);
#103910=AXIS2_PLACEMENT_3D('',#206994,#123965,#123966);
#103911=AXIS2_PLACEMENT_3D('',#206995,#123967,#123968);
#103912=AXIS2_PLACEMENT_3D('',#206996,#123969,#123970);
#103913=AXIS2_PLACEMENT_3D('',#206997,#123971,#123972);
#103914=AXIS2_PLACEMENT_3D('',#207016,#123973,#123974);
#103915=AXIS2_PLACEMENT_3D('',#207029,#123975,#123976);
#103916=AXIS2_PLACEMENT_3D('',#207030,#123977,#123978);
#103917=AXIS2_PLACEMENT_3D('',#207031,#123979,#123980);
#103918=AXIS2_PLACEMENT_3D('',#207032,#123981,#123982);
#103919=AXIS2_PLACEMENT_3D('',#207033,#123983,#123984);
#103920=AXIS2_PLACEMENT_3D('',#207052,#123985,#123986);
#103921=AXIS2_PLACEMENT_3D('',#207053,#123987,#123988);
#103922=AXIS2_PLACEMENT_3D('',#207054,#123989,#123990);
#103923=AXIS2_PLACEMENT_3D('',#207055,#123991,#123992);
#103924=AXIS2_PLACEMENT_3D('',#207056,#123993,#123994);
#103925=AXIS2_PLACEMENT_3D('',#207069,#123995,#123996);
#103926=AXIS2_PLACEMENT_3D('',#207082,#123997,#123998);
#103927=AXIS2_PLACEMENT_3D('',#207083,#123999,#124000);
#103928=AXIS2_PLACEMENT_3D('',#207084,#124001,#124002);
#103929=AXIS2_PLACEMENT_3D('',#207085,#124003,#124004);
#103930=AXIS2_PLACEMENT_3D('',#207086,#124005,#124006);
#103931=AXIS2_PLACEMENT_3D('',#207099,#124007,#124008);
#103932=AXIS2_PLACEMENT_3D('',#207100,#124009,#124010);
#103933=AXIS2_PLACEMENT_3D('',#207101,#124011,#124012);
#103934=AXIS2_PLACEMENT_3D('',#207102,#124013,#124014);
#103935=AXIS2_PLACEMENT_3D('',#207103,#124015,#124016);
#103936=AXIS2_PLACEMENT_3D('',#207116,#124017,#124018);
#103937=AXIS2_PLACEMENT_3D('',#207117,#124019,#124020);
#103938=AXIS2_PLACEMENT_3D('',#207118,#124021,#124022);
#103939=AXIS2_PLACEMENT_3D('',#207119,#124023,#124024);
#103940=AXIS2_PLACEMENT_3D('',#207120,#124025,#124026);
#103941=AXIS2_PLACEMENT_3D('',#207133,#124027,#124028);
#103942=AXIS2_PLACEMENT_3D('',#207146,#124029,#124030);
#103943=AXIS2_PLACEMENT_3D('',#207147,#124031,#124032);
#103944=AXIS2_PLACEMENT_3D('',#207148,#124033,#124034);
#103945=AXIS2_PLACEMENT_3D('',#207149,#124035,#124036);
#103946=AXIS2_PLACEMENT_3D('',#207150,#124037,#124038);
#103947=AXIS2_PLACEMENT_3D('',#207169,#124039,#124040);
#103948=AXIS2_PLACEMENT_3D('',#207170,#124041,#124042);
#103949=AXIS2_PLACEMENT_3D('',#207171,#124043,#124044);
#103950=AXIS2_PLACEMENT_3D('',#207172,#124045,#124046);
#103951=AXIS2_PLACEMENT_3D('',#207173,#124047,#124048);
#103952=AXIS2_PLACEMENT_3D('',#207186,#124049,#124050);
#103953=AXIS2_PLACEMENT_3D('',#207205,#124051,#124052);
#103954=AXIS2_PLACEMENT_3D('',#207206,#124053,#124054);
#103955=AXIS2_PLACEMENT_3D('',#207207,#124055,#124056);
#103956=AXIS2_PLACEMENT_3D('',#207208,#124057,#124058);
#103957=AXIS2_PLACEMENT_3D('',#207209,#124059,#124060);
#103958=AXIS2_PLACEMENT_3D('',#207228,#124061,#124062);
#103959=AXIS2_PLACEMENT_3D('',#207241,#124063,#124064);
#103960=AXIS2_PLACEMENT_3D('',#207242,#124065,#124066);
#103961=AXIS2_PLACEMENT_3D('',#207243,#124067,#124068);
#103962=AXIS2_PLACEMENT_3D('',#207244,#124069,#124070);
#103963=AXIS2_PLACEMENT_3D('',#207245,#124071,#124072);
#103964=AXIS2_PLACEMENT_3D('',#207264,#124073,#124074);
#103965=AXIS2_PLACEMENT_3D('',#207265,#124075,#124076);
#103966=AXIS2_PLACEMENT_3D('',#207266,#124077,#124078);
#103967=AXIS2_PLACEMENT_3D('',#207267,#124079,#124080);
#103968=AXIS2_PLACEMENT_3D('',#207268,#124081,#124082);
#103969=AXIS2_PLACEMENT_3D('',#207281,#124083,#124084);
#103970=AXIS2_PLACEMENT_3D('',#207294,#124085,#124086);
#103971=AXIS2_PLACEMENT_3D('',#207295,#124087,#124088);
#103972=AXIS2_PLACEMENT_3D('',#207296,#124089,#124090);
#103973=AXIS2_PLACEMENT_3D('',#207297,#124091,#124092);
#103974=AXIS2_PLACEMENT_3D('',#207298,#124093,#124094);
#103975=AXIS2_PLACEMENT_3D('',#207311,#124095,#124096);
#103976=AXIS2_PLACEMENT_3D('',#207312,#124097,#124098);
#103977=AXIS2_PLACEMENT_3D('',#207313,#124099,#124100);
#103978=AXIS2_PLACEMENT_3D('',#207314,#124101,#124102);
#103979=AXIS2_PLACEMENT_3D('',#207315,#124103,#124104);
#103980=AXIS2_PLACEMENT_3D('',#207328,#124105,#124106);
#103981=AXIS2_PLACEMENT_3D('',#207329,#124107,#124108);
#103982=AXIS2_PLACEMENT_3D('',#207330,#124109,#124110);
#103983=AXIS2_PLACEMENT_3D('',#207331,#124111,#124112);
#103984=AXIS2_PLACEMENT_3D('',#207332,#124113,#124114);
#103985=AXIS2_PLACEMENT_3D('',#207345,#124115,#124116);
#103986=AXIS2_PLACEMENT_3D('',#207358,#124117,#124118);
#103987=AXIS2_PLACEMENT_3D('',#207359,#124119,#124120);
#103988=AXIS2_PLACEMENT_3D('',#207360,#124121,#124122);
#103989=AXIS2_PLACEMENT_3D('',#207361,#124123,#124124);
#103990=AXIS2_PLACEMENT_3D('',#207362,#124125,#124126);
#103991=AXIS2_PLACEMENT_3D('',#207381,#124127,#124128);
#103992=AXIS2_PLACEMENT_3D('',#207382,#124129,#124130);
#103993=AXIS2_PLACEMENT_3D('',#207395,#124131,#124132);
#103994=AXIS2_PLACEMENT_3D('',#207414,#124133,#124134);
#103995=AXIS2_PLACEMENT_3D('',#207415,#124135,#124136);
#103996=AXIS2_PLACEMENT_3D('',#207416,#124137,#124138);
#103997=AXIS2_PLACEMENT_3D('',#207417,#124139,#124140);
#103998=AXIS2_PLACEMENT_3D('',#207418,#124141,#124142);
#103999=AXIS2_PLACEMENT_3D('',#207449,#124143,#124144);
#104000=AXIS2_PLACEMENT_3D('',#207450,#124145,#124146);
#104001=AXIS2_PLACEMENT_3D('',#207451,#124147,#124148);
#104002=AXIS2_PLACEMENT_3D('',#207470,#124149,#124150);
#104003=AXIS2_PLACEMENT_3D('',#207471,#124151,#124152);
#104004=AXIS2_PLACEMENT_3D('',#207472,#124153,#124154);
#104005=AXIS2_PLACEMENT_3D('',#207473,#124155,#124156);
#104006=AXIS2_PLACEMENT_3D('',#207474,#124157,#124158);
#104007=AXIS2_PLACEMENT_3D('',#207487,#124159,#124160);
#104008=AXIS2_PLACEMENT_3D('',#207500,#124161,#124162);
#104009=AXIS2_PLACEMENT_3D('',#207501,#124163,#124164);
#104010=AXIS2_PLACEMENT_3D('',#207502,#124165,#124166);
#104011=AXIS2_PLACEMENT_3D('',#207503,#124167,#124168);
#104012=AXIS2_PLACEMENT_3D('',#207504,#124169,#124170);
#104013=AXIS2_PLACEMENT_3D('',#207517,#124171,#124172);
#104014=AXIS2_PLACEMENT_3D('',#207518,#124173,#124174);
#104015=AXIS2_PLACEMENT_3D('',#207519,#124175,#124176);
#104016=AXIS2_PLACEMENT_3D('',#207520,#124177,#124178);
#104017=AXIS2_PLACEMENT_3D('',#207521,#124179,#124180);
#104018=AXIS2_PLACEMENT_3D('',#207534,#124181,#124182);
#104019=AXIS2_PLACEMENT_3D('',#207535,#124183,#124184);
#104020=AXIS2_PLACEMENT_3D('',#207536,#124185,#124186);
#104021=AXIS2_PLACEMENT_3D('',#207537,#124187,#124188);
#104022=AXIS2_PLACEMENT_3D('',#207538,#124189,#124190);
#104023=AXIS2_PLACEMENT_3D('',#207551,#124191,#124192);
#104024=AXIS2_PLACEMENT_3D('',#207564,#124193,#124194);
#104025=AXIS2_PLACEMENT_3D('',#207565,#124195,#124196);
#104026=AXIS2_PLACEMENT_3D('',#207566,#124197,#124198);
#104027=AXIS2_PLACEMENT_3D('',#207567,#124199,#124200);
#104028=AXIS2_PLACEMENT_3D('',#207568,#124201,#124202);
#104029=AXIS2_PLACEMENT_3D('',#207587,#124203,#124204);
#104030=AXIS2_PLACEMENT_3D('',#207588,#124205,#124206);
#104031=AXIS2_PLACEMENT_3D('',#207589,#124207,#124208);
#104032=AXIS2_PLACEMENT_3D('',#207590,#124209,#124210);
#104033=AXIS2_PLACEMENT_3D('',#207591,#124211,#124212);
#104034=AXIS2_PLACEMENT_3D('',#207604,#124213,#124214);
#104035=AXIS2_PLACEMENT_3D('',#207623,#124215,#124216);
#104036=AXIS2_PLACEMENT_3D('',#207624,#124217,#124218);
#104037=AXIS2_PLACEMENT_3D('',#207625,#124219,#124220);
#104038=AXIS2_PLACEMENT_3D('',#207626,#124221,#124222);
#104039=AXIS2_PLACEMENT_3D('',#207627,#124223,#124224);
#104040=AXIS2_PLACEMENT_3D('',#207646,#124225,#124226);
#104041=AXIS2_PLACEMENT_3D('',#207659,#124227,#124228);
#104042=AXIS2_PLACEMENT_3D('',#207660,#124229,#124230);
#104043=AXIS2_PLACEMENT_3D('',#207661,#124231,#124232);
#104044=AXIS2_PLACEMENT_3D('',#207662,#124233,#124234);
#104045=AXIS2_PLACEMENT_3D('',#207663,#124235,#124236);
#104046=AXIS2_PLACEMENT_3D('',#207682,#124237,#124238);
#104047=AXIS2_PLACEMENT_3D('',#207683,#124239,#124240);
#104048=AXIS2_PLACEMENT_3D('',#207684,#124241,#124242);
#104049=AXIS2_PLACEMENT_3D('',#207685,#124243,#124244);
#104050=AXIS2_PLACEMENT_3D('',#207686,#124245,#124246);
#104051=AXIS2_PLACEMENT_3D('',#207699,#124247,#124248);
#104052=AXIS2_PLACEMENT_3D('',#207712,#124249,#124250);
#104053=AXIS2_PLACEMENT_3D('',#207713,#124251,#124252);
#104054=AXIS2_PLACEMENT_3D('',#207714,#124253,#124254);
#104055=AXIS2_PLACEMENT_3D('',#207715,#124255,#124256);
#104056=AXIS2_PLACEMENT_3D('',#207716,#124257,#124258);
#104057=AXIS2_PLACEMENT_3D('',#207729,#124259,#124260);
#104058=AXIS2_PLACEMENT_3D('',#207730,#124261,#124262);
#104059=AXIS2_PLACEMENT_3D('',#207731,#124263,#124264);
#104060=AXIS2_PLACEMENT_3D('',#207732,#124265,#124266);
#104061=AXIS2_PLACEMENT_3D('',#207733,#124267,#124268);
#104062=AXIS2_PLACEMENT_3D('',#207746,#124269,#124270);
#104063=AXIS2_PLACEMENT_3D('',#207747,#124271,#124272);
#104064=AXIS2_PLACEMENT_3D('',#207748,#124273,#124274);
#104065=AXIS2_PLACEMENT_3D('',#207749,#124275,#124276);
#104066=AXIS2_PLACEMENT_3D('',#207750,#124277,#124278);
#104067=AXIS2_PLACEMENT_3D('',#207763,#124279,#124280);
#104068=AXIS2_PLACEMENT_3D('',#207776,#124281,#124282);
#104069=AXIS2_PLACEMENT_3D('',#207777,#124283,#124284);
#104070=AXIS2_PLACEMENT_3D('',#207778,#124285,#124286);
#104071=AXIS2_PLACEMENT_3D('',#207779,#124287,#124288);
#104072=AXIS2_PLACEMENT_3D('',#207780,#124289,#124290);
#104073=AXIS2_PLACEMENT_3D('',#207799,#124291,#124292);
#104074=AXIS2_PLACEMENT_3D('',#207800,#124293,#124294);
#104075=AXIS2_PLACEMENT_3D('',#207801,#124295,#124296);
#104076=AXIS2_PLACEMENT_3D('',#207802,#124297,#124298);
#104077=AXIS2_PLACEMENT_3D('',#207803,#124299,#124300);
#104078=AXIS2_PLACEMENT_3D('',#207816,#124301,#124302);
#104079=AXIS2_PLACEMENT_3D('',#207835,#124303,#124304);
#104080=AXIS2_PLACEMENT_3D('',#207836,#124305,#124306);
#104081=AXIS2_PLACEMENT_3D('',#207837,#124307,#124308);
#104082=AXIS2_PLACEMENT_3D('',#207838,#124309,#124310);
#104083=AXIS2_PLACEMENT_3D('',#207839,#124311,#124312);
#104084=AXIS2_PLACEMENT_3D('',#207858,#124313,#124314);
#104085=AXIS2_PLACEMENT_3D('',#207871,#124315,#124316);
#104086=AXIS2_PLACEMENT_3D('',#207872,#124317,#124318);
#104087=AXIS2_PLACEMENT_3D('',#207873,#124319,#124320);
#104088=AXIS2_PLACEMENT_3D('',#207874,#124321,#124322);
#104089=AXIS2_PLACEMENT_3D('',#207875,#124323,#124324);
#104090=AXIS2_PLACEMENT_3D('',#207894,#124325,#124326);
#104091=AXIS2_PLACEMENT_3D('',#207895,#124327,#124328);
#104092=AXIS2_PLACEMENT_3D('',#207896,#124329,#124330);
#104093=AXIS2_PLACEMENT_3D('',#207897,#124331,#124332);
#104094=AXIS2_PLACEMENT_3D('',#207898,#124333,#124334);
#104095=AXIS2_PLACEMENT_3D('',#207911,#124335,#124336);
#104096=AXIS2_PLACEMENT_3D('',#207924,#124337,#124338);
#104097=AXIS2_PLACEMENT_3D('',#207925,#124339,#124340);
#104098=AXIS2_PLACEMENT_3D('',#207926,#124341,#124342);
#104099=AXIS2_PLACEMENT_3D('',#207927,#124343,#124344);
#104100=AXIS2_PLACEMENT_3D('',#207928,#124345,#124346);
#104101=AXIS2_PLACEMENT_3D('',#207941,#124347,#124348);
#104102=AXIS2_PLACEMENT_3D('',#207942,#124349,#124350);
#104103=AXIS2_PLACEMENT_3D('',#207943,#124351,#124352);
#104104=AXIS2_PLACEMENT_3D('',#207944,#124353,#124354);
#104105=AXIS2_PLACEMENT_3D('',#207945,#124355,#124356);
#104106=AXIS2_PLACEMENT_3D('',#207958,#124357,#124358);
#104107=AXIS2_PLACEMENT_3D('',#207959,#124359,#124360);
#104108=AXIS2_PLACEMENT_3D('',#207960,#124361,#124362);
#104109=AXIS2_PLACEMENT_3D('',#207961,#124363,#124364);
#104110=AXIS2_PLACEMENT_3D('',#207962,#124365,#124366);
#104111=AXIS2_PLACEMENT_3D('',#207975,#124367,#124368);
#104112=AXIS2_PLACEMENT_3D('',#207988,#124369,#124370);
#104113=AXIS2_PLACEMENT_3D('',#207989,#124371,#124372);
#104114=AXIS2_PLACEMENT_3D('',#207990,#124373,#124374);
#104115=AXIS2_PLACEMENT_3D('',#207991,#124375,#124376);
#104116=AXIS2_PLACEMENT_3D('',#207992,#124377,#124378);
#104117=AXIS2_PLACEMENT_3D('',#208011,#124379,#124380);
#104118=AXIS2_PLACEMENT_3D('',#208012,#124381,#124382);
#104119=AXIS2_PLACEMENT_3D('',#208013,#124383,#124384);
#104120=AXIS2_PLACEMENT_3D('',#208014,#124385,#124386);
#104121=AXIS2_PLACEMENT_3D('',#208015,#124387,#124388);
#104122=AXIS2_PLACEMENT_3D('',#208028,#124389,#124390);
#104123=AXIS2_PLACEMENT_3D('',#208047,#124391,#124392);
#104124=AXIS2_PLACEMENT_3D('',#208048,#124393,#124394);
#104125=AXIS2_PLACEMENT_3D('',#208049,#124395,#124396);
#104126=AXIS2_PLACEMENT_3D('',#208050,#124397,#124398);
#104127=AXIS2_PLACEMENT_3D('',#208051,#124399,#124400);
#104128=AXIS2_PLACEMENT_3D('',#208070,#124401,#124402);
#104129=AXIS2_PLACEMENT_3D('',#208083,#124403,#124404);
#104130=AXIS2_PLACEMENT_3D('',#208084,#124405,#124406);
#104131=AXIS2_PLACEMENT_3D('',#208085,#124407,#124408);
#104132=AXIS2_PLACEMENT_3D('',#208086,#124409,#124410);
#104133=AXIS2_PLACEMENT_3D('',#208087,#124411,#124412);
#104134=AXIS2_PLACEMENT_3D('',#208106,#124413,#124414);
#104135=AXIS2_PLACEMENT_3D('',#208107,#124415,#124416);
#104136=AXIS2_PLACEMENT_3D('',#208108,#124417,#124418);
#104137=AXIS2_PLACEMENT_3D('',#208109,#124419,#124420);
#104138=AXIS2_PLACEMENT_3D('',#208110,#124421,#124422);
#104139=AXIS2_PLACEMENT_3D('',#208123,#124423,#124424);
#104140=AXIS2_PLACEMENT_3D('',#208136,#124425,#124426);
#104141=AXIS2_PLACEMENT_3D('',#208137,#124427,#124428);
#104142=AXIS2_PLACEMENT_3D('',#208138,#124429,#124430);
#104143=AXIS2_PLACEMENT_3D('',#208139,#124431,#124432);
#104144=AXIS2_PLACEMENT_3D('',#208140,#124433,#124434);
#104145=AXIS2_PLACEMENT_3D('',#208153,#124435,#124436);
#104146=AXIS2_PLACEMENT_3D('',#208154,#124437,#124438);
#104147=AXIS2_PLACEMENT_3D('',#208155,#124439,#124440);
#104148=AXIS2_PLACEMENT_3D('',#208156,#124441,#124442);
#104149=AXIS2_PLACEMENT_3D('',#208157,#124443,#124444);
#104150=AXIS2_PLACEMENT_3D('',#208170,#124445,#124446);
#104151=AXIS2_PLACEMENT_3D('',#208171,#124447,#124448);
#104152=AXIS2_PLACEMENT_3D('',#208172,#124449,#124450);
#104153=AXIS2_PLACEMENT_3D('',#208173,#124451,#124452);
#104154=AXIS2_PLACEMENT_3D('',#208174,#124453,#124454);
#104155=AXIS2_PLACEMENT_3D('',#208187,#124455,#124456);
#104156=AXIS2_PLACEMENT_3D('',#208200,#124457,#124458);
#104157=AXIS2_PLACEMENT_3D('',#208201,#124459,#124460);
#104158=AXIS2_PLACEMENT_3D('',#208202,#124461,#124462);
#104159=AXIS2_PLACEMENT_3D('',#208203,#124463,#124464);
#104160=AXIS2_PLACEMENT_3D('',#208204,#124465,#124466);
#104161=AXIS2_PLACEMENT_3D('',#208223,#124467,#124468);
#104162=AXIS2_PLACEMENT_3D('',#208224,#124469,#124470);
#104163=AXIS2_PLACEMENT_3D('',#208225,#124471,#124472);
#104164=AXIS2_PLACEMENT_3D('',#208226,#124473,#124474);
#104165=AXIS2_PLACEMENT_3D('',#208227,#124475,#124476);
#104166=AXIS2_PLACEMENT_3D('',#208240,#124477,#124478);
#104167=AXIS2_PLACEMENT_3D('',#208259,#124479,#124480);
#104168=AXIS2_PLACEMENT_3D('',#208260,#124481,#124482);
#104169=AXIS2_PLACEMENT_3D('',#208261,#124483,#124484);
#104170=AXIS2_PLACEMENT_3D('',#208262,#124485,#124486);
#104171=AXIS2_PLACEMENT_3D('',#208263,#124487,#124488);
#104172=AXIS2_PLACEMENT_3D('',#208282,#124489,#124490);
#104173=AXIS2_PLACEMENT_3D('',#208295,#124491,#124492);
#104174=AXIS2_PLACEMENT_3D('',#208296,#124493,#124494);
#104175=AXIS2_PLACEMENT_3D('',#208297,#124495,#124496);
#104176=AXIS2_PLACEMENT_3D('',#208298,#124497,#124498);
#104177=AXIS2_PLACEMENT_3D('',#208299,#124499,#124500);
#104178=AXIS2_PLACEMENT_3D('',#208318,#124501,#124502);
#104179=AXIS2_PLACEMENT_3D('',#208319,#124503,#124504);
#104180=AXIS2_PLACEMENT_3D('',#208320,#124505,#124506);
#104181=AXIS2_PLACEMENT_3D('',#208321,#124507,#124508);
#104182=AXIS2_PLACEMENT_3D('',#208322,#124509,#124510);
#104183=AXIS2_PLACEMENT_3D('',#208335,#124511,#124512);
#104184=AXIS2_PLACEMENT_3D('',#208348,#124513,#124514);
#104185=AXIS2_PLACEMENT_3D('',#208349,#124515,#124516);
#104186=AXIS2_PLACEMENT_3D('',#208350,#124517,#124518);
#104187=AXIS2_PLACEMENT_3D('',#208351,#124519,#124520);
#104188=AXIS2_PLACEMENT_3D('',#208352,#124521,#124522);
#104189=AXIS2_PLACEMENT_3D('',#208365,#124523,#124524);
#104190=AXIS2_PLACEMENT_3D('',#208366,#124525,#124526);
#104191=AXIS2_PLACEMENT_3D('',#208367,#124527,#124528);
#104192=AXIS2_PLACEMENT_3D('',#208368,#124529,#124530);
#104193=AXIS2_PLACEMENT_3D('',#208369,#124531,#124532);
#104194=AXIS2_PLACEMENT_3D('',#208382,#124533,#124534);
#104195=AXIS2_PLACEMENT_3D('',#208383,#124535,#124536);
#104196=AXIS2_PLACEMENT_3D('',#208384,#124537,#124538);
#104197=AXIS2_PLACEMENT_3D('',#208385,#124539,#124540);
#104198=AXIS2_PLACEMENT_3D('',#208386,#124541,#124542);
#104199=AXIS2_PLACEMENT_3D('',#208399,#124543,#124544);
#104200=AXIS2_PLACEMENT_3D('',#208412,#124545,#124546);
#104201=AXIS2_PLACEMENT_3D('',#208413,#124547,#124548);
#104202=AXIS2_PLACEMENT_3D('',#208414,#124549,#124550);
#104203=AXIS2_PLACEMENT_3D('',#208415,#124551,#124552);
#104204=AXIS2_PLACEMENT_3D('',#208416,#124553,#124554);
#104205=AXIS2_PLACEMENT_3D('',#208435,#124555,#124556);
#104206=AXIS2_PLACEMENT_3D('',#208436,#124557,#124558);
#104207=AXIS2_PLACEMENT_3D('',#208437,#124559,#124560);
#104208=AXIS2_PLACEMENT_3D('',#208438,#124561,#124562);
#104209=AXIS2_PLACEMENT_3D('',#208439,#124563,#124564);
#104210=AXIS2_PLACEMENT_3D('',#208452,#124565,#124566);
#104211=AXIS2_PLACEMENT_3D('',#208471,#124567,#124568);
#104212=AXIS2_PLACEMENT_3D('',#208472,#124569,#124570);
#104213=AXIS2_PLACEMENT_3D('',#208473,#124571,#124572);
#104214=AXIS2_PLACEMENT_3D('',#208474,#124573,#124574);
#104215=AXIS2_PLACEMENT_3D('',#208475,#124575,#124576);
#104216=AXIS2_PLACEMENT_3D('',#208494,#124577,#124578);
#104217=AXIS2_PLACEMENT_3D('',#208507,#124579,#124580);
#104218=AXIS2_PLACEMENT_3D('',#208508,#124581,#124582);
#104219=AXIS2_PLACEMENT_3D('',#208509,#124583,#124584);
#104220=AXIS2_PLACEMENT_3D('',#208510,#124585,#124586);
#104221=AXIS2_PLACEMENT_3D('',#208511,#124587,#124588);
#104222=AXIS2_PLACEMENT_3D('',#208530,#124589,#124590);
#104223=AXIS2_PLACEMENT_3D('',#208531,#124591,#124592);
#104224=AXIS2_PLACEMENT_3D('',#208532,#124593,#124594);
#104225=AXIS2_PLACEMENT_3D('',#208533,#124595,#124596);
#104226=AXIS2_PLACEMENT_3D('',#208534,#124597,#124598);
#104227=AXIS2_PLACEMENT_3D('',#208547,#124599,#124600);
#104228=AXIS2_PLACEMENT_3D('',#208560,#124601,#124602);
#104229=AXIS2_PLACEMENT_3D('',#208561,#124603,#124604);
#104230=AXIS2_PLACEMENT_3D('',#208562,#124605,#124606);
#104231=AXIS2_PLACEMENT_3D('',#208563,#124607,#124608);
#104232=AXIS2_PLACEMENT_3D('',#208564,#124609,#124610);
#104233=AXIS2_PLACEMENT_3D('',#208577,#124611,#124612);
#104234=AXIS2_PLACEMENT_3D('',#208578,#124613,#124614);
#104235=AXIS2_PLACEMENT_3D('',#208579,#124615,#124616);
#104236=AXIS2_PLACEMENT_3D('',#208580,#124617,#124618);
#104237=AXIS2_PLACEMENT_3D('',#208581,#124619,#124620);
#104238=AXIS2_PLACEMENT_3D('',#208594,#124621,#124622);
#104239=AXIS2_PLACEMENT_3D('',#208595,#124623,#124624);
#104240=AXIS2_PLACEMENT_3D('',#208596,#124625,#124626);
#104241=AXIS2_PLACEMENT_3D('',#208597,#124627,#124628);
#104242=AXIS2_PLACEMENT_3D('',#208598,#124629,#124630);
#104243=AXIS2_PLACEMENT_3D('',#208611,#124631,#124632);
#104244=AXIS2_PLACEMENT_3D('',#208624,#124633,#124634);
#104245=AXIS2_PLACEMENT_3D('',#208625,#124635,#124636);
#104246=AXIS2_PLACEMENT_3D('',#208626,#124637,#124638);
#104247=AXIS2_PLACEMENT_3D('',#208627,#124639,#124640);
#104248=AXIS2_PLACEMENT_3D('',#208628,#124641,#124642);
#104249=AXIS2_PLACEMENT_3D('',#208647,#124643,#124644);
#104250=AXIS2_PLACEMENT_3D('',#208648,#124645,#124646);
#104251=AXIS2_PLACEMENT_3D('',#208649,#124647,#124648);
#104252=AXIS2_PLACEMENT_3D('',#208650,#124649,#124650);
#104253=AXIS2_PLACEMENT_3D('',#208651,#124651,#124652);
#104254=AXIS2_PLACEMENT_3D('',#208664,#124653,#124654);
#104255=AXIS2_PLACEMENT_3D('',#208683,#124655,#124656);
#104256=AXIS2_PLACEMENT_3D('',#208684,#124657,#124658);
#104257=AXIS2_PLACEMENT_3D('',#208685,#124659,#124660);
#104258=AXIS2_PLACEMENT_3D('',#208686,#124661,#124662);
#104259=AXIS2_PLACEMENT_3D('',#208687,#124663,#124664);
#104260=AXIS2_PLACEMENT_3D('',#208706,#124665,#124666);
#104261=AXIS2_PLACEMENT_3D('',#208719,#124667,#124668);
#104262=AXIS2_PLACEMENT_3D('',#208720,#124669,#124670);
#104263=AXIS2_PLACEMENT_3D('',#208721,#124671,#124672);
#104264=AXIS2_PLACEMENT_3D('',#208722,#124673,#124674);
#104265=AXIS2_PLACEMENT_3D('',#208723,#124675,#124676);
#104266=AXIS2_PLACEMENT_3D('',#208742,#124677,#124678);
#104267=AXIS2_PLACEMENT_3D('',#208743,#124679,#124680);
#104268=AXIS2_PLACEMENT_3D('',#208744,#124681,#124682);
#104269=AXIS2_PLACEMENT_3D('',#208745,#124683,#124684);
#104270=AXIS2_PLACEMENT_3D('',#208746,#124685,#124686);
#104271=AXIS2_PLACEMENT_3D('',#208759,#124687,#124688);
#104272=AXIS2_PLACEMENT_3D('',#208772,#124689,#124690);
#104273=AXIS2_PLACEMENT_3D('',#208773,#124691,#124692);
#104274=AXIS2_PLACEMENT_3D('',#208774,#124693,#124694);
#104275=AXIS2_PLACEMENT_3D('',#208775,#124695,#124696);
#104276=AXIS2_PLACEMENT_3D('',#208776,#124697,#124698);
#104277=AXIS2_PLACEMENT_3D('',#208789,#124699,#124700);
#104278=AXIS2_PLACEMENT_3D('',#208790,#124701,#124702);
#104279=AXIS2_PLACEMENT_3D('',#208791,#124703,#124704);
#104280=AXIS2_PLACEMENT_3D('',#208792,#124705,#124706);
#104281=AXIS2_PLACEMENT_3D('',#208793,#124707,#124708);
#104282=AXIS2_PLACEMENT_3D('',#208806,#124709,#124710);
#104283=AXIS2_PLACEMENT_3D('',#208807,#124711,#124712);
#104284=AXIS2_PLACEMENT_3D('',#208808,#124713,#124714);
#104285=AXIS2_PLACEMENT_3D('',#208809,#124715,#124716);
#104286=AXIS2_PLACEMENT_3D('',#208810,#124717,#124718);
#104287=AXIS2_PLACEMENT_3D('',#208823,#124719,#124720);
#104288=AXIS2_PLACEMENT_3D('',#208836,#124721,#124722);
#104289=AXIS2_PLACEMENT_3D('',#208837,#124723,#124724);
#104290=AXIS2_PLACEMENT_3D('',#208838,#124725,#124726);
#104291=AXIS2_PLACEMENT_3D('',#208839,#124727,#124728);
#104292=AXIS2_PLACEMENT_3D('',#208840,#124729,#124730);
#104293=AXIS2_PLACEMENT_3D('',#208859,#124731,#124732);
#104294=AXIS2_PLACEMENT_3D('',#208860,#124733,#124734);
#104295=AXIS2_PLACEMENT_3D('',#208861,#124735,#124736);
#104296=AXIS2_PLACEMENT_3D('',#208862,#124737,#124738);
#104297=AXIS2_PLACEMENT_3D('',#208863,#124739,#124740);
#104298=AXIS2_PLACEMENT_3D('',#208876,#124741,#124742);
#104299=AXIS2_PLACEMENT_3D('',#208895,#124743,#124744);
#104300=AXIS2_PLACEMENT_3D('',#208896,#124745,#124746);
#104301=AXIS2_PLACEMENT_3D('',#208897,#124747,#124748);
#104302=AXIS2_PLACEMENT_3D('',#208898,#124749,#124750);
#104303=AXIS2_PLACEMENT_3D('',#208899,#124751,#124752);
#104304=AXIS2_PLACEMENT_3D('',#208918,#124753,#124754);
#104305=AXIS2_PLACEMENT_3D('',#208931,#124755,#124756);
#104306=AXIS2_PLACEMENT_3D('',#208932,#124757,#124758);
#104307=AXIS2_PLACEMENT_3D('',#208933,#124759,#124760);
#104308=AXIS2_PLACEMENT_3D('',#208934,#124761,#124762);
#104309=AXIS2_PLACEMENT_3D('',#208935,#124763,#124764);
#104310=AXIS2_PLACEMENT_3D('',#208954,#124765,#124766);
#104311=AXIS2_PLACEMENT_3D('',#208955,#124767,#124768);
#104312=AXIS2_PLACEMENT_3D('',#208956,#124769,#124770);
#104313=AXIS2_PLACEMENT_3D('',#208957,#124771,#124772);
#104314=AXIS2_PLACEMENT_3D('',#208958,#124773,#124774);
#104315=AXIS2_PLACEMENT_3D('',#208971,#124775,#124776);
#104316=AXIS2_PLACEMENT_3D('',#208984,#124777,#124778);
#104317=AXIS2_PLACEMENT_3D('',#208985,#124779,#124780);
#104318=AXIS2_PLACEMENT_3D('',#208986,#124781,#124782);
#104319=AXIS2_PLACEMENT_3D('',#208987,#124783,#124784);
#104320=AXIS2_PLACEMENT_3D('',#208988,#124785,#124786);
#104321=AXIS2_PLACEMENT_3D('',#209001,#124787,#124788);
#104322=AXIS2_PLACEMENT_3D('',#209002,#124789,#124790);
#104323=AXIS2_PLACEMENT_3D('',#209003,#124791,#124792);
#104324=AXIS2_PLACEMENT_3D('',#209004,#124793,#124794);
#104325=AXIS2_PLACEMENT_3D('',#209005,#124795,#124796);
#104326=AXIS2_PLACEMENT_3D('',#209018,#124797,#124798);
#104327=AXIS2_PLACEMENT_3D('',#209019,#124799,#124800);
#104328=AXIS2_PLACEMENT_3D('',#209020,#124801,#124802);
#104329=AXIS2_PLACEMENT_3D('',#209021,#124803,#124804);
#104330=AXIS2_PLACEMENT_3D('',#209022,#124805,#124806);
#104331=AXIS2_PLACEMENT_3D('',#209035,#124807,#124808);
#104332=AXIS2_PLACEMENT_3D('',#209048,#124809,#124810);
#104333=AXIS2_PLACEMENT_3D('',#209049,#124811,#124812);
#104334=AXIS2_PLACEMENT_3D('',#209050,#124813,#124814);
#104335=AXIS2_PLACEMENT_3D('',#209051,#124815,#124816);
#104336=AXIS2_PLACEMENT_3D('',#209052,#124817,#124818);
#104337=AXIS2_PLACEMENT_3D('',#209071,#124819,#124820);
#104338=AXIS2_PLACEMENT_3D('',#209072,#124821,#124822);
#104339=AXIS2_PLACEMENT_3D('',#209073,#124823,#124824);
#104340=AXIS2_PLACEMENT_3D('',#209074,#124825,#124826);
#104341=AXIS2_PLACEMENT_3D('',#209075,#124827,#124828);
#104342=AXIS2_PLACEMENT_3D('',#209088,#124829,#124830);
#104343=AXIS2_PLACEMENT_3D('',#209107,#124831,#124832);
#104344=AXIS2_PLACEMENT_3D('',#209108,#124833,#124834);
#104345=AXIS2_PLACEMENT_3D('',#209109,#124835,#124836);
#104346=AXIS2_PLACEMENT_3D('',#209110,#124837,#124838);
#104347=AXIS2_PLACEMENT_3D('',#209111,#124839,#124840);
#104348=AXIS2_PLACEMENT_3D('',#209130,#124841,#124842);
#104349=AXIS2_PLACEMENT_3D('',#209143,#124843,#124844);
#104350=AXIS2_PLACEMENT_3D('',#209144,#124845,#124846);
#104351=AXIS2_PLACEMENT_3D('',#209145,#124847,#124848);
#104352=AXIS2_PLACEMENT_3D('',#209146,#124849,#124850);
#104353=AXIS2_PLACEMENT_3D('',#209147,#124851,#124852);
#104354=AXIS2_PLACEMENT_3D('',#209166,#124853,#124854);
#104355=AXIS2_PLACEMENT_3D('',#209167,#124855,#124856);
#104356=AXIS2_PLACEMENT_3D('',#209168,#124857,#124858);
#104357=AXIS2_PLACEMENT_3D('',#209169,#124859,#124860);
#104358=AXIS2_PLACEMENT_3D('',#209170,#124861,#124862);
#104359=AXIS2_PLACEMENT_3D('',#209183,#124863,#124864);
#104360=AXIS2_PLACEMENT_3D('',#209196,#124865,#124866);
#104361=AXIS2_PLACEMENT_3D('',#209197,#124867,#124868);
#104362=AXIS2_PLACEMENT_3D('',#209198,#124869,#124870);
#104363=AXIS2_PLACEMENT_3D('',#209199,#124871,#124872);
#104364=AXIS2_PLACEMENT_3D('',#209200,#124873,#124874);
#104365=AXIS2_PLACEMENT_3D('',#209213,#124875,#124876);
#104366=AXIS2_PLACEMENT_3D('',#209214,#124877,#124878);
#104367=AXIS2_PLACEMENT_3D('',#209215,#124879,#124880);
#104368=AXIS2_PLACEMENT_3D('',#209216,#124881,#124882);
#104369=AXIS2_PLACEMENT_3D('',#209217,#124883,#124884);
#104370=AXIS2_PLACEMENT_3D('',#209230,#124885,#124886);
#104371=AXIS2_PLACEMENT_3D('',#209231,#124887,#124888);
#104372=AXIS2_PLACEMENT_3D('',#209232,#124889,#124890);
#104373=AXIS2_PLACEMENT_3D('',#209233,#124891,#124892);
#104374=AXIS2_PLACEMENT_3D('',#209234,#124893,#124894);
#104375=AXIS2_PLACEMENT_3D('',#209247,#124895,#124896);
#104376=AXIS2_PLACEMENT_3D('',#209260,#124897,#124898);
#104377=AXIS2_PLACEMENT_3D('',#209261,#124899,#124900);
#104378=AXIS2_PLACEMENT_3D('',#209262,#124901,#124902);
#104379=AXIS2_PLACEMENT_3D('',#209263,#124903,#124904);
#104380=AXIS2_PLACEMENT_3D('',#209264,#124905,#124906);
#104381=AXIS2_PLACEMENT_3D('',#209283,#124907,#124908);
#104382=AXIS2_PLACEMENT_3D('',#209284,#124909,#124910);
#104383=AXIS2_PLACEMENT_3D('',#209285,#124911,#124912);
#104384=AXIS2_PLACEMENT_3D('',#209286,#124913,#124914);
#104385=AXIS2_PLACEMENT_3D('',#209287,#124915,#124916);
#104386=AXIS2_PLACEMENT_3D('',#209300,#124917,#124918);
#104387=AXIS2_PLACEMENT_3D('',#209319,#124919,#124920);
#104388=AXIS2_PLACEMENT_3D('',#209320,#124921,#124922);
#104389=AXIS2_PLACEMENT_3D('',#209321,#124923,#124924);
#104390=AXIS2_PLACEMENT_3D('',#209322,#124925,#124926);
#104391=AXIS2_PLACEMENT_3D('',#209323,#124927,#124928);
#104392=AXIS2_PLACEMENT_3D('',#209342,#124929,#124930);
#104393=AXIS2_PLACEMENT_3D('',#209355,#124931,#124932);
#104394=AXIS2_PLACEMENT_3D('',#209356,#124933,#124934);
#104395=AXIS2_PLACEMENT_3D('',#209357,#124935,#124936);
#104396=AXIS2_PLACEMENT_3D('',#209358,#124937,#124938);
#104397=AXIS2_PLACEMENT_3D('',#209359,#124939,#124940);
#104398=AXIS2_PLACEMENT_3D('',#209378,#124941,#124942);
#104399=AXIS2_PLACEMENT_3D('',#209379,#124943,#124944);
#104400=AXIS2_PLACEMENT_3D('',#209380,#124945,#124946);
#104401=AXIS2_PLACEMENT_3D('',#209381,#124947,#124948);
#104402=AXIS2_PLACEMENT_3D('',#209382,#124949,#124950);
#104403=AXIS2_PLACEMENT_3D('',#209395,#124951,#124952);
#104404=AXIS2_PLACEMENT_3D('',#209408,#124953,#124954);
#104405=AXIS2_PLACEMENT_3D('',#209409,#124955,#124956);
#104406=AXIS2_PLACEMENT_3D('',#209410,#124957,#124958);
#104407=AXIS2_PLACEMENT_3D('',#209411,#124959,#124960);
#104408=AXIS2_PLACEMENT_3D('',#209412,#124961,#124962);
#104409=AXIS2_PLACEMENT_3D('',#209425,#124963,#124964);
#104410=AXIS2_PLACEMENT_3D('',#209426,#124965,#124966);
#104411=AXIS2_PLACEMENT_3D('',#209427,#124967,#124968);
#104412=AXIS2_PLACEMENT_3D('',#209428,#124969,#124970);
#104413=AXIS2_PLACEMENT_3D('',#209429,#124971,#124972);
#104414=AXIS2_PLACEMENT_3D('',#209442,#124973,#124974);
#104415=AXIS2_PLACEMENT_3D('',#209443,#124975,#124976);
#104416=AXIS2_PLACEMENT_3D('',#209444,#124977,#124978);
#104417=AXIS2_PLACEMENT_3D('',#209445,#124979,#124980);
#104418=AXIS2_PLACEMENT_3D('',#209446,#124981,#124982);
#104419=AXIS2_PLACEMENT_3D('',#209459,#124983,#124984);
#104420=AXIS2_PLACEMENT_3D('',#209472,#124985,#124986);
#104421=AXIS2_PLACEMENT_3D('',#209473,#124987,#124988);
#104422=AXIS2_PLACEMENT_3D('',#209474,#124989,#124990);
#104423=AXIS2_PLACEMENT_3D('',#209475,#124991,#124992);
#104424=AXIS2_PLACEMENT_3D('',#209476,#124993,#124994);
#104425=AXIS2_PLACEMENT_3D('',#209495,#124995,#124996);
#104426=AXIS2_PLACEMENT_3D('',#209496,#124997,#124998);
#104427=AXIS2_PLACEMENT_3D('',#209497,#124999,#125000);
#104428=AXIS2_PLACEMENT_3D('',#209498,#125001,#125002);
#104429=AXIS2_PLACEMENT_3D('',#209499,#125003,#125004);
#104430=AXIS2_PLACEMENT_3D('',#209512,#125005,#125006);
#104431=AXIS2_PLACEMENT_3D('',#209531,#125007,#125008);
#104432=AXIS2_PLACEMENT_3D('',#209532,#125009,#125010);
#104433=AXIS2_PLACEMENT_3D('',#209533,#125011,#125012);
#104434=AXIS2_PLACEMENT_3D('',#209534,#125013,#125014);
#104435=AXIS2_PLACEMENT_3D('',#209535,#125015,#125016);
#104436=AXIS2_PLACEMENT_3D('',#209554,#125017,#125018);
#104437=AXIS2_PLACEMENT_3D('',#209567,#125019,#125020);
#104438=AXIS2_PLACEMENT_3D('',#209568,#125021,#125022);
#104439=AXIS2_PLACEMENT_3D('',#209569,#125023,#125024);
#104440=AXIS2_PLACEMENT_3D('',#209570,#125025,#125026);
#104441=AXIS2_PLACEMENT_3D('',#209571,#125027,#125028);
#104442=AXIS2_PLACEMENT_3D('',#209590,#125029,#125030);
#104443=AXIS2_PLACEMENT_3D('',#209591,#125031,#125032);
#104444=AXIS2_PLACEMENT_3D('',#209592,#125033,#125034);
#104445=AXIS2_PLACEMENT_3D('',#209593,#125035,#125036);
#104446=AXIS2_PLACEMENT_3D('',#209594,#125037,#125038);
#104447=AXIS2_PLACEMENT_3D('',#209607,#125039,#125040);
#104448=AXIS2_PLACEMENT_3D('',#209620,#125041,#125042);
#104449=AXIS2_PLACEMENT_3D('',#209621,#125043,#125044);
#104450=AXIS2_PLACEMENT_3D('',#209622,#125045,#125046);
#104451=AXIS2_PLACEMENT_3D('',#209623,#125047,#125048);
#104452=AXIS2_PLACEMENT_3D('',#209624,#125049,#125050);
#104453=AXIS2_PLACEMENT_3D('',#209637,#125051,#125052);
#104454=AXIS2_PLACEMENT_3D('',#209638,#125053,#125054);
#104455=AXIS2_PLACEMENT_3D('',#209639,#125055,#125056);
#104456=AXIS2_PLACEMENT_3D('',#209640,#125057,#125058);
#104457=AXIS2_PLACEMENT_3D('',#209641,#125059,#125060);
#104458=AXIS2_PLACEMENT_3D('',#209654,#125061,#125062);
#104459=AXIS2_PLACEMENT_3D('',#209655,#125063,#125064);
#104460=AXIS2_PLACEMENT_3D('',#209656,#125065,#125066);
#104461=AXIS2_PLACEMENT_3D('',#209657,#125067,#125068);
#104462=AXIS2_PLACEMENT_3D('',#209658,#125069,#125070);
#104463=AXIS2_PLACEMENT_3D('',#209671,#125071,#125072);
#104464=AXIS2_PLACEMENT_3D('',#209684,#125073,#125074);
#104465=AXIS2_PLACEMENT_3D('',#209685,#125075,#125076);
#104466=AXIS2_PLACEMENT_3D('',#209686,#125077,#125078);
#104467=AXIS2_PLACEMENT_3D('',#209687,#125079,#125080);
#104468=AXIS2_PLACEMENT_3D('',#209688,#125081,#125082);
#104469=AXIS2_PLACEMENT_3D('',#209707,#125083,#125084);
#104470=AXIS2_PLACEMENT_3D('',#209708,#125085,#125086);
#104471=AXIS2_PLACEMENT_3D('',#209709,#125087,#125088);
#104472=AXIS2_PLACEMENT_3D('',#209710,#125089,#125090);
#104473=AXIS2_PLACEMENT_3D('',#209711,#125091,#125092);
#104474=AXIS2_PLACEMENT_3D('',#209724,#125093,#125094);
#104475=AXIS2_PLACEMENT_3D('',#209743,#125095,#125096);
#104476=AXIS2_PLACEMENT_3D('',#209744,#125097,#125098);
#104477=AXIS2_PLACEMENT_3D('',#209745,#125099,#125100);
#104478=AXIS2_PLACEMENT_3D('',#209746,#125101,#125102);
#104479=AXIS2_PLACEMENT_3D('',#209747,#125103,#125104);
#104480=AXIS2_PLACEMENT_3D('',#209766,#125105,#125106);
#104481=AXIS2_PLACEMENT_3D('',#209779,#125107,#125108);
#104482=AXIS2_PLACEMENT_3D('',#209780,#125109,#125110);
#104483=AXIS2_PLACEMENT_3D('',#209781,#125111,#125112);
#104484=AXIS2_PLACEMENT_3D('',#209782,#125113,#125114);
#104485=AXIS2_PLACEMENT_3D('',#209783,#125115,#125116);
#104486=AXIS2_PLACEMENT_3D('',#209802,#125117,#125118);
#104487=AXIS2_PLACEMENT_3D('',#209803,#125119,#125120);
#104488=AXIS2_PLACEMENT_3D('',#209804,#125121,#125122);
#104489=AXIS2_PLACEMENT_3D('',#209805,#125123,#125124);
#104490=AXIS2_PLACEMENT_3D('',#209806,#125125,#125126);
#104491=AXIS2_PLACEMENT_3D('',#209819,#125127,#125128);
#104492=AXIS2_PLACEMENT_3D('',#209832,#125129,#125130);
#104493=AXIS2_PLACEMENT_3D('',#209833,#125131,#125132);
#104494=AXIS2_PLACEMENT_3D('',#209834,#125133,#125134);
#104495=AXIS2_PLACEMENT_3D('',#209835,#125135,#125136);
#104496=AXIS2_PLACEMENT_3D('',#209836,#125137,#125138);
#104497=AXIS2_PLACEMENT_3D('',#209849,#125139,#125140);
#104498=AXIS2_PLACEMENT_3D('',#209850,#125141,#125142);
#104499=AXIS2_PLACEMENT_3D('',#209851,#125143,#125144);
#104500=AXIS2_PLACEMENT_3D('',#209852,#125145,#125146);
#104501=AXIS2_PLACEMENT_3D('',#209853,#125147,#125148);
#104502=AXIS2_PLACEMENT_3D('',#209866,#125149,#125150);
#104503=AXIS2_PLACEMENT_3D('',#209867,#125151,#125152);
#104504=AXIS2_PLACEMENT_3D('',#209868,#125153,#125154);
#104505=AXIS2_PLACEMENT_3D('',#209869,#125155,#125156);
#104506=AXIS2_PLACEMENT_3D('',#209870,#125157,#125158);
#104507=AXIS2_PLACEMENT_3D('',#209883,#125159,#125160);
#104508=AXIS2_PLACEMENT_3D('',#209896,#125161,#125162);
#104509=AXIS2_PLACEMENT_3D('',#209897,#125163,#125164);
#104510=AXIS2_PLACEMENT_3D('',#209898,#125165,#125166);
#104511=AXIS2_PLACEMENT_3D('',#209899,#125167,#125168);
#104512=AXIS2_PLACEMENT_3D('',#209900,#125169,#125170);
#104513=AXIS2_PLACEMENT_3D('',#209919,#125171,#125172);
#104514=AXIS2_PLACEMENT_3D('',#209920,#125173,#125174);
#104515=AXIS2_PLACEMENT_3D('',#209921,#125175,#125176);
#104516=AXIS2_PLACEMENT_3D('',#209922,#125177,#125178);
#104517=AXIS2_PLACEMENT_3D('',#209923,#125179,#125180);
#104518=AXIS2_PLACEMENT_3D('',#209936,#125181,#125182);
#104519=AXIS2_PLACEMENT_3D('',#209955,#125183,#125184);
#104520=AXIS2_PLACEMENT_3D('',#209956,#125185,#125186);
#104521=AXIS2_PLACEMENT_3D('',#209957,#125187,#125188);
#104522=AXIS2_PLACEMENT_3D('',#209958,#125189,#125190);
#104523=AXIS2_PLACEMENT_3D('',#209959,#125191,#125192);
#104524=AXIS2_PLACEMENT_3D('',#209978,#125193,#125194);
#104525=AXIS2_PLACEMENT_3D('',#209991,#125195,#125196);
#104526=AXIS2_PLACEMENT_3D('',#209992,#125197,#125198);
#104527=AXIS2_PLACEMENT_3D('',#209993,#125199,#125200);
#104528=AXIS2_PLACEMENT_3D('',#209994,#125201,#125202);
#104529=AXIS2_PLACEMENT_3D('',#209995,#125203,#125204);
#104530=AXIS2_PLACEMENT_3D('',#210014,#125205,#125206);
#104531=AXIS2_PLACEMENT_3D('',#210015,#125207,#125208);
#104532=AXIS2_PLACEMENT_3D('',#210016,#125209,#125210);
#104533=AXIS2_PLACEMENT_3D('',#210017,#125211,#125212);
#104534=AXIS2_PLACEMENT_3D('',#210018,#125213,#125214);
#104535=AXIS2_PLACEMENT_3D('',#210031,#125215,#125216);
#104536=AXIS2_PLACEMENT_3D('',#210044,#125217,#125218);
#104537=AXIS2_PLACEMENT_3D('',#210045,#125219,#125220);
#104538=AXIS2_PLACEMENT_3D('',#210046,#125221,#125222);
#104539=AXIS2_PLACEMENT_3D('',#210047,#125223,#125224);
#104540=AXIS2_PLACEMENT_3D('',#210048,#125225,#125226);
#104541=AXIS2_PLACEMENT_3D('',#210061,#125227,#125228);
#104542=AXIS2_PLACEMENT_3D('',#210062,#125229,#125230);
#104543=AXIS2_PLACEMENT_3D('',#210063,#125231,#125232);
#104544=AXIS2_PLACEMENT_3D('',#210064,#125233,#125234);
#104545=AXIS2_PLACEMENT_3D('',#210065,#125235,#125236);
#104546=AXIS2_PLACEMENT_3D('',#210078,#125237,#125238);
#104547=AXIS2_PLACEMENT_3D('',#210079,#125239,#125240);
#104548=AXIS2_PLACEMENT_3D('',#210080,#125241,#125242);
#104549=AXIS2_PLACEMENT_3D('',#210081,#125243,#125244);
#104550=AXIS2_PLACEMENT_3D('',#210082,#125245,#125246);
#104551=AXIS2_PLACEMENT_3D('',#210095,#125247,#125248);
#104552=AXIS2_PLACEMENT_3D('',#210108,#125249,#125250);
#104553=AXIS2_PLACEMENT_3D('',#210109,#125251,#125252);
#104554=AXIS2_PLACEMENT_3D('',#210110,#125253,#125254);
#104555=AXIS2_PLACEMENT_3D('',#210111,#125255,#125256);
#104556=AXIS2_PLACEMENT_3D('',#210112,#125257,#125258);
#104557=AXIS2_PLACEMENT_3D('',#210131,#125259,#125260);
#104558=AXIS2_PLACEMENT_3D('',#210132,#125261,#125262);
#104559=AXIS2_PLACEMENT_3D('',#210133,#125263,#125264);
#104560=AXIS2_PLACEMENT_3D('',#210134,#125265,#125266);
#104561=AXIS2_PLACEMENT_3D('',#210135,#125267,#125268);
#104562=AXIS2_PLACEMENT_3D('',#210148,#125269,#125270);
#104563=AXIS2_PLACEMENT_3D('',#210167,#125271,#125272);
#104564=AXIS2_PLACEMENT_3D('',#210168,#125273,#125274);
#104565=AXIS2_PLACEMENT_3D('',#210169,#125275,#125276);
#104566=AXIS2_PLACEMENT_3D('',#210170,#125277,#125278);
#104567=AXIS2_PLACEMENT_3D('',#210171,#125279,#125280);
#104568=AXIS2_PLACEMENT_3D('',#210190,#125281,#125282);
#104569=AXIS2_PLACEMENT_3D('',#210203,#125283,#125284);
#104570=AXIS2_PLACEMENT_3D('',#210204,#125285,#125286);
#104571=AXIS2_PLACEMENT_3D('',#210205,#125287,#125288);
#104572=AXIS2_PLACEMENT_3D('',#210206,#125289,#125290);
#104573=AXIS2_PLACEMENT_3D('',#210207,#125291,#125292);
#104574=AXIS2_PLACEMENT_3D('',#210226,#125293,#125294);
#104575=AXIS2_PLACEMENT_3D('',#210227,#125295,#125296);
#104576=AXIS2_PLACEMENT_3D('',#210228,#125297,#125298);
#104577=AXIS2_PLACEMENT_3D('',#210229,#125299,#125300);
#104578=AXIS2_PLACEMENT_3D('',#210230,#125301,#125302);
#104579=AXIS2_PLACEMENT_3D('',#210243,#125303,#125304);
#104580=AXIS2_PLACEMENT_3D('',#210256,#125305,#125306);
#104581=AXIS2_PLACEMENT_3D('',#210257,#125307,#125308);
#104582=AXIS2_PLACEMENT_3D('',#210258,#125309,#125310);
#104583=AXIS2_PLACEMENT_3D('',#210259,#125311,#125312);
#104584=AXIS2_PLACEMENT_3D('',#210260,#125313,#125314);
#104585=AXIS2_PLACEMENT_3D('',#210273,#125315,#125316);
#104586=AXIS2_PLACEMENT_3D('',#210274,#125317,#125318);
#104587=AXIS2_PLACEMENT_3D('',#210275,#125319,#125320);
#104588=AXIS2_PLACEMENT_3D('',#210276,#125321,#125322);
#104589=AXIS2_PLACEMENT_3D('',#210277,#125323,#125324);
#104590=AXIS2_PLACEMENT_3D('',#210290,#125325,#125326);
#104591=AXIS2_PLACEMENT_3D('',#210291,#125327,#125328);
#104592=AXIS2_PLACEMENT_3D('',#210292,#125329,#125330);
#104593=AXIS2_PLACEMENT_3D('',#210293,#125331,#125332);
#104594=AXIS2_PLACEMENT_3D('',#210294,#125333,#125334);
#104595=AXIS2_PLACEMENT_3D('',#210307,#125335,#125336);
#104596=AXIS2_PLACEMENT_3D('',#210320,#125337,#125338);
#104597=AXIS2_PLACEMENT_3D('',#210321,#125339,#125340);
#104598=AXIS2_PLACEMENT_3D('',#210322,#125341,#125342);
#104599=AXIS2_PLACEMENT_3D('',#210323,#125343,#125344);
#104600=AXIS2_PLACEMENT_3D('',#210324,#125345,#125346);
#104601=AXIS2_PLACEMENT_3D('',#210343,#125347,#125348);
#104602=AXIS2_PLACEMENT_3D('',#210344,#125349,#125350);
#104603=AXIS2_PLACEMENT_3D('',#210345,#125351,#125352);
#104604=AXIS2_PLACEMENT_3D('',#210346,#125353,#125354);
#104605=AXIS2_PLACEMENT_3D('',#210347,#125355,#125356);
#104606=AXIS2_PLACEMENT_3D('',#210360,#125357,#125358);
#104607=AXIS2_PLACEMENT_3D('',#210379,#125359,#125360);
#104608=AXIS2_PLACEMENT_3D('',#210380,#125361,#125362);
#104609=AXIS2_PLACEMENT_3D('',#210381,#125363,#125364);
#104610=AXIS2_PLACEMENT_3D('',#210382,#125365,#125366);
#104611=AXIS2_PLACEMENT_3D('',#210383,#125367,#125368);
#104612=AXIS2_PLACEMENT_3D('',#210402,#125369,#125370);
#104613=AXIS2_PLACEMENT_3D('',#210415,#125371,#125372);
#104614=AXIS2_PLACEMENT_3D('',#210416,#125373,#125374);
#104615=AXIS2_PLACEMENT_3D('',#210417,#125375,#125376);
#104616=AXIS2_PLACEMENT_3D('',#210418,#125377,#125378);
#104617=AXIS2_PLACEMENT_3D('',#210419,#125379,#125380);
#104618=AXIS2_PLACEMENT_3D('',#210438,#125381,#125382);
#104619=AXIS2_PLACEMENT_3D('',#210439,#125383,#125384);
#104620=AXIS2_PLACEMENT_3D('',#210440,#125385,#125386);
#104621=AXIS2_PLACEMENT_3D('',#210441,#125387,#125388);
#104622=AXIS2_PLACEMENT_3D('',#210442,#125389,#125390);
#104623=AXIS2_PLACEMENT_3D('',#210455,#125391,#125392);
#104624=AXIS2_PLACEMENT_3D('',#210468,#125393,#125394);
#104625=AXIS2_PLACEMENT_3D('',#210469,#125395,#125396);
#104626=AXIS2_PLACEMENT_3D('',#210470,#125397,#125398);
#104627=AXIS2_PLACEMENT_3D('',#210471,#125399,#125400);
#104628=AXIS2_PLACEMENT_3D('',#210472,#125401,#125402);
#104629=AXIS2_PLACEMENT_3D('',#210485,#125403,#125404);
#104630=AXIS2_PLACEMENT_3D('',#210486,#125405,#125406);
#104631=AXIS2_PLACEMENT_3D('',#210487,#125407,#125408);
#104632=AXIS2_PLACEMENT_3D('',#210490,#125409,#125410);
#104633=AXIS2_PLACEMENT_3D('',#210492,#125411,#125412);
#104634=AXIS2_PLACEMENT_3D('',#210494,#125413,#125414);
#104635=AXIS2_PLACEMENT_3D('',#210495,#125415,#125416);
#104636=AXIS2_PLACEMENT_3D('',#210496,#125417,#125418);
#104637=AXIS2_PLACEMENT_3D('',#210499,#125419,#125420);
#104638=AXIS2_PLACEMENT_3D('',#210501,#125421,#125422);
#104639=AXIS2_PLACEMENT_3D('',#210503,#125423,#125424);
#104640=AXIS2_PLACEMENT_3D('',#210504,#125425,#125426);
#104641=AXIS2_PLACEMENT_3D('',#210505,#125427,#125428);
#104642=AXIS2_PLACEMENT_3D('',#210508,#125429,#125430);
#104643=AXIS2_PLACEMENT_3D('',#210510,#125431,#125432);
#104644=AXIS2_PLACEMENT_3D('',#210512,#125433,#125434);
#104645=AXIS2_PLACEMENT_3D('',#210513,#125435,#125436);
#104646=AXIS2_PLACEMENT_3D('',#210514,#125437,#125438);
#104647=AXIS2_PLACEMENT_3D('',#210517,#125439,#125440);
#104648=AXIS2_PLACEMENT_3D('',#210519,#125441,#125442);
#104649=AXIS2_PLACEMENT_3D('',#210521,#125443,#125444);
#104650=AXIS2_PLACEMENT_3D('',#210523,#125445,#125446);
#104651=AXIS2_PLACEMENT_3D('',#210524,#125447,#125448);
#104652=AXIS2_PLACEMENT_3D('',#210525,#125449,#125450);
#104653=AXIS2_PLACEMENT_3D('',#210527,#125451,#125452);
#104654=AXIS2_PLACEMENT_3D('',#210529,#125453,#125454);
#104655=AXIS2_PLACEMENT_3D('',#210531,#125455,#125456);
#104656=AXIS2_PLACEMENT_3D('',#210532,#125457,#125458);
#104657=AXIS2_PLACEMENT_3D('',#210533,#125459,#125460);
#104658=AXIS2_PLACEMENT_3D('',#210535,#125461,#125462);
#104659=AXIS2_PLACEMENT_3D('',#210537,#125463,#125464);
#104660=AXIS2_PLACEMENT_3D('',#210538,#125465,#125466);
#104661=AXIS2_PLACEMENT_3D('',#210539,#125467,#125468);
#104662=AXIS2_PLACEMENT_3D('',#210541,#125469,#125470);
#104663=AXIS2_PLACEMENT_3D('',#210543,#125471,#125472);
#104664=AXIS2_PLACEMENT_3D('',#210545,#125473,#125474);
#104665=AXIS2_PLACEMENT_3D('',#210546,#125475,#125476);
#104666=AXIS2_PLACEMENT_3D('',#210547,#125477,#125478);
#104667=AXIS2_PLACEMENT_3D('',#210549,#125479,#125480);
#104668=AXIS2_PLACEMENT_3D('',#210551,#125481,#125482);
#104669=AXIS2_PLACEMENT_3D('',#210552,#125483,#125484);
#104670=AXIS2_PLACEMENT_3D('',#210553,#125485,#125486);
#104671=AXIS2_PLACEMENT_3D('',#210555,#125487,#125488);
#104672=AXIS2_PLACEMENT_3D('',#210558,#125490,#125491);
#104673=AXIS2_PLACEMENT_3D('',#210559,#125492,#125493);
#104674=AXIS2_PLACEMENT_3D('',#210561,#125495,#125496);
#104675=AXIS2_PLACEMENT_3D('',#210564,#125497,#125498);
#104676=AXIS2_PLACEMENT_3D('',#210612,#125500,#125501);
#104677=AXIS2_PLACEMENT_3D('',#210657,#125503,#125504);
#104678=AXIS2_PLACEMENT_3D('',#210705,#125506,#125507);
#104679=AXIS2_PLACEMENT_3D('',#210750,#125509,#125510);
#104680=AXIS2_PLACEMENT_3D('',#210798,#125512,#125513);
#104681=AXIS2_PLACEMENT_3D('',#210843,#125515,#125516);
#104682=AXIS2_PLACEMENT_3D('',#210891,#125518,#125519);
#104683=AXIS2_PLACEMENT_3D('',#210936,#125521,#125522);
#104684=AXIS2_PLACEMENT_3D('',#210984,#125524,#125525);
#104685=AXIS2_PLACEMENT_3D('',#211029,#125527,#125528);
#104686=AXIS2_PLACEMENT_3D('',#211077,#125530,#125531);
#104687=AXIS2_PLACEMENT_3D('',#211122,#125533,#125534);
#104688=AXIS2_PLACEMENT_3D('',#211170,#125536,#125537);
#104689=AXIS2_PLACEMENT_3D('',#211215,#125539,#125540);
#104690=AXIS2_PLACEMENT_3D('',#211263,#125542,#125543);
#104691=AXIS2_PLACEMENT_3D('',#211308,#125545,#125546);
#104692=AXIS2_PLACEMENT_3D('',#211356,#125548,#125549);
#104693=AXIS2_PLACEMENT_3D('',#211401,#125551,#125552);
#104694=AXIS2_PLACEMENT_3D('',#211449,#125554,#125555);
#104695=AXIS2_PLACEMENT_3D('',#211494,#125557,#125558);
#104696=AXIS2_PLACEMENT_3D('',#211542,#125560,#125561);
#104697=AXIS2_PLACEMENT_3D('',#211587,#125563,#125564);
#104698=AXIS2_PLACEMENT_3D('',#211635,#125566,#125567);
#104699=AXIS2_PLACEMENT_3D('',#211680,#125569,#125570);
#104700=AXIS2_PLACEMENT_3D('',#211728,#125572,#125573);
#104701=AXIS2_PLACEMENT_3D('',#211773,#125575,#125576);
#104702=AXIS2_PLACEMENT_3D('',#211821,#125578,#125579);
#104703=AXIS2_PLACEMENT_3D('',#211866,#125581,#125582);
#104704=AXIS2_PLACEMENT_3D('',#211914,#125584,#125585);
#104705=AXIS2_PLACEMENT_3D('',#211959,#125587,#125588);
#104706=AXIS2_PLACEMENT_3D('',#212007,#125590,#125591);
#104707=AXIS2_PLACEMENT_3D('',#212052,#125593,#125594);
#104708=AXIS2_PLACEMENT_3D('',#212100,#125596,#125597);
#104709=AXIS2_PLACEMENT_3D('',#212145,#125599,#125600);
#104710=AXIS2_PLACEMENT_3D('',#212193,#125602,#125603);
#104711=AXIS2_PLACEMENT_3D('',#212238,#125605,#125606);
#104712=AXIS2_PLACEMENT_3D('',#212286,#125608,#125609);
#104713=AXIS2_PLACEMENT_3D('',#212331,#125611,#125612);
#104714=AXIS2_PLACEMENT_3D('',#212379,#125614,#125615);
#104715=AXIS2_PLACEMENT_3D('',#212424,#125617,#125618);
#104716=AXIS2_PLACEMENT_3D('',#212472,#125620,#125621);
#104717=AXIS2_PLACEMENT_3D('',#212517,#125623,#125624);
#104718=AXIS2_PLACEMENT_3D('',#212565,#125626,#125627);
#104719=AXIS2_PLACEMENT_3D('',#212610,#125629,#125630);
#104720=AXIS2_PLACEMENT_3D('',#212658,#125632,#125633);
#104721=AXIS2_PLACEMENT_3D('',#212703,#125635,#125636);
#104722=AXIS2_PLACEMENT_3D('',#212751,#125638,#125639);
#104723=AXIS2_PLACEMENT_3D('',#212796,#125641,#125642);
#104724=AXIS2_PLACEMENT_3D('',#212844,#125644,#125645);
#104725=AXIS2_PLACEMENT_3D('',#212889,#125647,#125648);
#104726=AXIS2_PLACEMENT_3D('',#212937,#125650,#125651);
#104727=AXIS2_PLACEMENT_3D('',#212982,#125653,#125654);
#104728=AXIS2_PLACEMENT_3D('',#213030,#125656,#125657);
#104729=AXIS2_PLACEMENT_3D('',#213075,#125659,#125660);
#104730=AXIS2_PLACEMENT_3D('',#213123,#125662,#125663);
#104731=AXIS2_PLACEMENT_3D('',#213168,#125665,#125666);
#104732=AXIS2_PLACEMENT_3D('',#213216,#125668,#125669);
#104733=AXIS2_PLACEMENT_3D('',#213261,#125671,#125672);
#104734=AXIS2_PLACEMENT_3D('',#213309,#125674,#125675);
#104735=AXIS2_PLACEMENT_3D('',#213400,#125679,#125680);
#104736=AXIS2_PLACEMENT_3D('',#213445,#125682,#125683);
#104737=AXIS2_PLACEMENT_3D('',#213493,#125685,#125686);
#104738=AXIS2_PLACEMENT_3D('',#213538,#125688,#125689);
#104739=AXIS2_PLACEMENT_3D('',#213586,#125691,#125692);
#104740=AXIS2_PLACEMENT_3D('',#213631,#125694,#125695);
#104741=AXIS2_PLACEMENT_3D('',#213679,#125697,#125698);
#104742=AXIS2_PLACEMENT_3D('',#213724,#125700,#125701);
#104743=AXIS2_PLACEMENT_3D('',#213772,#125703,#125704);
#104744=AXIS2_PLACEMENT_3D('',#213817,#125706,#125707);
#104745=AXIS2_PLACEMENT_3D('',#213865,#125709,#125710);
#104746=AXIS2_PLACEMENT_3D('',#213910,#125712,#125713);
#104747=AXIS2_PLACEMENT_3D('',#213958,#125715,#125716);
#104748=AXIS2_PLACEMENT_3D('',#214003,#125718,#125719);
#104749=AXIS2_PLACEMENT_3D('',#214051,#125721,#125722);
#104750=AXIS2_PLACEMENT_3D('',#214096,#125724,#125725);
#104751=AXIS2_PLACEMENT_3D('',#214144,#125727,#125728);
#104752=AXIS2_PLACEMENT_3D('',#214189,#125730,#125731);
#104753=AXIS2_PLACEMENT_3D('',#214237,#125733,#125734);
#104754=AXIS2_PLACEMENT_3D('',#214282,#125736,#125737);
#104755=AXIS2_PLACEMENT_3D('',#214330,#125739,#125740);
#104756=AXIS2_PLACEMENT_3D('',#214375,#125742,#125743);
#104757=AXIS2_PLACEMENT_3D('',#214423,#125745,#125746);
#104758=AXIS2_PLACEMENT_3D('',#214468,#125748,#125749);
#104759=AXIS2_PLACEMENT_3D('',#214516,#125751,#125752);
#104760=AXIS2_PLACEMENT_3D('',#214561,#125754,#125755);
#104761=AXIS2_PLACEMENT_3D('',#214609,#125757,#125758);
#104762=AXIS2_PLACEMENT_3D('',#214654,#125760,#125761);
#104763=AXIS2_PLACEMENT_3D('',#214702,#125763,#125764);
#104764=AXIS2_PLACEMENT_3D('',#214792,#125767,#125768);
#104765=AXIS2_PLACEMENT_3D('',#214837,#125770,#125771);
#104766=AXIS2_PLACEMENT_3D('',#214885,#125773,#125774);
#104767=AXIS2_PLACEMENT_3D('',#214930,#125776,#125777);
#104768=AXIS2_PLACEMENT_3D('',#214978,#125779,#125780);
#104769=AXIS2_PLACEMENT_3D('',#215023,#125782,#125783);
#104770=AXIS2_PLACEMENT_3D('',#215071,#125785,#125786);
#104771=AXIS2_PLACEMENT_3D('',#215116,#125788,#125789);
#104772=AXIS2_PLACEMENT_3D('',#215164,#125791,#125792);
#104773=AXIS2_PLACEMENT_3D('',#215209,#125794,#125795);
#104774=AXIS2_PLACEMENT_3D('',#215257,#125797,#125798);
#104775=AXIS2_PLACEMENT_3D('',#215302,#125800,#125801);
#104776=AXIS2_PLACEMENT_3D('',#215350,#125803,#125804);
#104777=AXIS2_PLACEMENT_3D('',#215395,#125806,#125807);
#104778=AXIS2_PLACEMENT_3D('',#215443,#125809,#125810);
#104779=AXIS2_PLACEMENT_3D('',#215488,#125812,#125813);
#104780=AXIS2_PLACEMENT_3D('',#215536,#125815,#125816);
#104781=AXIS2_PLACEMENT_3D('',#215581,#125818,#125819);
#104782=AXIS2_PLACEMENT_3D('',#215629,#125821,#125822);
#104783=AXIS2_PLACEMENT_3D('',#215674,#125824,#125825);
#104784=AXIS2_PLACEMENT_3D('',#215722,#125827,#125828);
#104785=AXIS2_PLACEMENT_3D('',#215767,#125830,#125831);
#104786=AXIS2_PLACEMENT_3D('',#215815,#125833,#125834);
#104787=AXIS2_PLACEMENT_3D('',#215860,#125836,#125837);
#104788=AXIS2_PLACEMENT_3D('',#215908,#125839,#125840);
#104789=AXIS2_PLACEMENT_3D('',#215953,#125842,#125843);
#104790=AXIS2_PLACEMENT_3D('',#216001,#125845,#125846);
#104791=AXIS2_PLACEMENT_3D('',#216046,#125848,#125849);
#104792=AXIS2_PLACEMENT_3D('',#216094,#125851,#125852);
#104793=AXIS2_PLACEMENT_3D('',#216137,#125854,#125855);
#104794=AXIS2_PLACEMENT_3D('',#216179,#125857,#125858);
#104795=AXIS2_PLACEMENT_3D('',#216224,#125860,#125861);
#104796=AXIS2_PLACEMENT_3D('',#216266,#125863,#125864);
#104797=AXIS2_PLACEMENT_3D('',#216311,#125866,#125867);
#104798=AXIS2_PLACEMENT_3D('',#216353,#125869,#125870);
#104799=AXIS2_PLACEMENT_3D('',#216398,#125872,#125873);
#104800=AXIS2_PLACEMENT_3D('',#216440,#125875,#125876);
#104801=AXIS2_PLACEMENT_3D('',#216485,#125878,#125879);
#104802=AXIS2_PLACEMENT_3D('',#216527,#125881,#125882);
#104803=AXIS2_PLACEMENT_3D('',#216572,#125884,#125885);
#104804=AXIS2_PLACEMENT_3D('',#216614,#125887,#125888);
#104805=AXIS2_PLACEMENT_3D('',#216659,#125890,#125891);
#104806=AXIS2_PLACEMENT_3D('',#216701,#125893,#125894);
#104807=AXIS2_PLACEMENT_3D('',#216746,#125896,#125897);
#104808=AXIS2_PLACEMENT_3D('',#216788,#125899,#125900);
#104809=AXIS2_PLACEMENT_3D('',#216833,#125902,#125903);
#104810=AXIS2_PLACEMENT_3D('',#216875,#125905,#125906);
#104811=AXIS2_PLACEMENT_3D('',#216920,#125908,#125909);
#104812=AXIS2_PLACEMENT_3D('',#216962,#125911,#125912);
#104813=AXIS2_PLACEMENT_3D('',#217007,#125914,#125915);
#104814=AXIS2_PLACEMENT_3D('',#217049,#125917,#125918);
#104815=AXIS2_PLACEMENT_3D('',#217094,#125920,#125921);
#104816=AXIS2_PLACEMENT_3D('',#217136,#125923,#125924);
#104817=AXIS2_PLACEMENT_3D('',#217181,#125926,#125927);
#104818=AXIS2_PLACEMENT_3D('',#217223,#125929,#125930);
#104819=AXIS2_PLACEMENT_3D('',#217268,#125932,#125933);
#104820=AXIS2_PLACEMENT_3D('',#217310,#125935,#125936);
#104821=AXIS2_PLACEMENT_3D('',#217355,#125938,#125939);
#104822=AXIS2_PLACEMENT_3D('',#217397,#125941,#125942);
#104823=AXIS2_PLACEMENT_3D('',#217442,#125944,#125945);
#104824=AXIS2_PLACEMENT_3D('',#217484,#125947,#125948);
#104825=AXIS2_PLACEMENT_3D('',#217529,#125950,#125951);
#104826=AXIS2_PLACEMENT_3D('',#217571,#125953,#125954);
#104827=AXIS2_PLACEMENT_3D('',#217616,#125956,#125957);
#104828=AXIS2_PLACEMENT_3D('',#217658,#125959,#125960);
#104829=AXIS2_PLACEMENT_3D('',#217703,#125962,#125963);
#104830=AXIS2_PLACEMENT_3D('',#217745,#125965,#125966);
#104831=AXIS2_PLACEMENT_3D('',#217790,#125968,#125969);
#104832=AXIS2_PLACEMENT_3D('',#217832,#125971,#125972);
#104833=AXIS2_PLACEMENT_3D('',#217877,#125974,#125975);
#104834=AXIS2_PLACEMENT_3D('',#217919,#125977,#125978);
#104835=AXIS2_PLACEMENT_3D('',#217964,#125980,#125981);
#104836=AXIS2_PLACEMENT_3D('',#218006,#125983,#125984);
#104837=AXIS2_PLACEMENT_3D('',#218051,#125986,#125987);
#104838=AXIS2_PLACEMENT_3D('',#218093,#125989,#125990);
#104839=AXIS2_PLACEMENT_3D('',#218138,#125992,#125993);
#104840=AXIS2_PLACEMENT_3D('',#218180,#125995,#125996);
#104841=AXIS2_PLACEMENT_3D('',#218225,#125998,#125999);
#104842=AXIS2_PLACEMENT_3D('',#218267,#126001,#126002);
#104843=AXIS2_PLACEMENT_3D('',#218312,#126004,#126005);
#104844=AXIS2_PLACEMENT_3D('',#218354,#126007,#126008);
#104845=AXIS2_PLACEMENT_3D('',#218399,#126010,#126011);
#104846=AXIS2_PLACEMENT_3D('',#218441,#126013,#126014);
#104847=AXIS2_PLACEMENT_3D('',#218486,#126016,#126017);
#104848=AXIS2_PLACEMENT_3D('',#218528,#126019,#126020);
#104849=AXIS2_PLACEMENT_3D('',#218573,#126022,#126023);
#104850=AXIS2_PLACEMENT_3D('',#218615,#126025,#126026);
#104851=AXIS2_PLACEMENT_3D('',#218660,#126028,#126029);
#104852=AXIS2_PLACEMENT_3D('',#218702,#126031,#126032);
#104853=AXIS2_PLACEMENT_3D('',#218747,#126034,#126035);
#104854=AXIS2_PLACEMENT_3D('',#218750,#126037,#126038);
#104855=AXIS2_PLACEMENT_3D('',#218792,#126040,#126041);
#104856=AXIS2_PLACEMENT_3D('',#218837,#126043,#126044);
#104857=AXIS2_PLACEMENT_3D('',#218879,#126046,#126047);
#104858=AXIS2_PLACEMENT_3D('',#218924,#126049,#126050);
#104859=AXIS2_PLACEMENT_3D('',#218966,#126052,#126053);
#104860=AXIS2_PLACEMENT_3D('',#219011,#126055,#126056);
#104861=AXIS2_PLACEMENT_3D('',#219053,#126058,#126059);
#104862=AXIS2_PLACEMENT_3D('',#219098,#126061,#126062);
#104863=AXIS2_PLACEMENT_3D('',#219140,#126064,#126065);
#104864=AXIS2_PLACEMENT_3D('',#219185,#126067,#126068);
#104865=AXIS2_PLACEMENT_3D('',#219227,#126070,#126071);
#104866=AXIS2_PLACEMENT_3D('',#219272,#126073,#126074);
#104867=AXIS2_PLACEMENT_3D('',#219314,#126076,#126077);
#104868=AXIS2_PLACEMENT_3D('',#219359,#126079,#126080);
#104869=AXIS2_PLACEMENT_3D('',#219401,#126082,#126083);
#104870=AXIS2_PLACEMENT_3D('',#219446,#126085,#126086);
#104871=AXIS2_PLACEMENT_3D('',#219488,#126088,#126089);
#104872=AXIS2_PLACEMENT_3D('',#219533,#126091,#126092);
#104873=AXIS2_PLACEMENT_3D('',#219575,#126094,#126095);
#104874=AXIS2_PLACEMENT_3D('',#219620,#126097,#126098);
#104875=AXIS2_PLACEMENT_3D('',#219662,#126100,#126101);
#104876=AXIS2_PLACEMENT_3D('',#219707,#126103,#126104);
#104877=AXIS2_PLACEMENT_3D('',#219749,#126106,#126107);
#104878=AXIS2_PLACEMENT_3D('',#219794,#126109,#126110);
#104879=AXIS2_PLACEMENT_3D('',#219836,#126112,#126113);
#104880=AXIS2_PLACEMENT_3D('',#219881,#126115,#126116);
#104881=AXIS2_PLACEMENT_3D('',#219923,#126118,#126119);
#104882=AXIS2_PLACEMENT_3D('',#219968,#126121,#126122);
#104883=AXIS2_PLACEMENT_3D('',#220010,#126124,#126125);
#104884=AXIS2_PLACEMENT_3D('',#220094,#126128,#126129);
#104885=AXIS2_PLACEMENT_3D('',#220139,#126131,#126132);
#104886=AXIS2_PLACEMENT_3D('',#220181,#126134,#126135);
#104887=AXIS2_PLACEMENT_3D('',#220226,#126137,#126138);
#104888=AXIS2_PLACEMENT_3D('',#220268,#126140,#126141);
#104889=AXIS2_PLACEMENT_3D('',#220313,#126143,#126144);
#104890=AXIS2_PLACEMENT_3D('',#220355,#126146,#126147);
#104891=AXIS2_PLACEMENT_3D('',#220400,#126149,#126150);
#104892=AXIS2_PLACEMENT_3D('',#220442,#126152,#126153);
#104893=AXIS2_PLACEMENT_3D('',#220487,#126155,#126156);
#104894=AXIS2_PLACEMENT_3D('',#220529,#126158,#126159);
#104895=AXIS2_PLACEMENT_3D('',#220574,#126161,#126162);
#104896=AXIS2_PLACEMENT_3D('',#220616,#126164,#126165);
#104897=AXIS2_PLACEMENT_3D('',#220661,#126167,#126168);
#104898=AXIS2_PLACEMENT_3D('',#220703,#126170,#126171);
#104899=AXIS2_PLACEMENT_3D('',#220748,#126173,#126174);
#104900=AXIS2_PLACEMENT_3D('',#220790,#126176,#126177);
#104901=AXIS2_PLACEMENT_3D('',#220835,#126179,#126180);
#104902=AXIS2_PLACEMENT_3D('',#220877,#126182,#126183);
#104903=AXIS2_PLACEMENT_3D('',#220922,#126185,#126186);
#104904=AXIS2_PLACEMENT_3D('',#220964,#126188,#126189);
#104905=AXIS2_PLACEMENT_3D('',#221009,#126191,#126192);
#104906=AXIS2_PLACEMENT_3D('',#221051,#126194,#126195);
#104907=AXIS2_PLACEMENT_3D('',#221096,#126197,#126198);
#104908=AXIS2_PLACEMENT_3D('',#221138,#126200,#126201);
#104909=AXIS2_PLACEMENT_3D('',#221183,#126203,#126204);
#104910=AXIS2_PLACEMENT_3D('',#221225,#126206,#126207);
#104911=AXIS2_PLACEMENT_3D('',#221270,#126209,#126210);
#104912=AXIS2_PLACEMENT_3D('',#221312,#126212,#126213);
#104913=AXIS2_PLACEMENT_3D('',#221355,#126215,#126216);
#104914=AXIS2_PLACEMENT_3D('',#221358,#126217,#126218);
#104915=AXIS2_PLACEMENT_3D('',#221360,#126220,#126221);
#104916=AXIS2_PLACEMENT_3D('',#221361,#126222,#126223);
#104917=AXIS2_PLACEMENT_3D('',#221364,#126225,#126226);
#104918=AXIS2_PLACEMENT_3D('',#221365,#126227,#126228);
#104919=AXIS2_PLACEMENT_3D('',#221368,#126229,#126230);
#104920=AXIS2_PLACEMENT_3D('',#221372,#126232,#126233);
#104921=AXIS2_PLACEMENT_3D('',#221376,#126235,#126236);
#104922=AXIS2_PLACEMENT_3D('',#221377,#126237,#126238);
#104923=AXIS2_PLACEMENT_3D('',#221378,#126239,#126240);
#104924=AXIS2_PLACEMENT_3D('',#221381,#126241,#126242);
#104925=AXIS2_PLACEMENT_3D('',#221384,#126245,#126246);
#104926=AXIS2_PLACEMENT_3D('',#221387,#126247,#126248);
#104927=AXIS2_PLACEMENT_3D('',#221391,#126250,#126251);
#104928=AXIS2_PLACEMENT_3D('',#221393,#126253,#126254);
#104929=AXIS2_PLACEMENT_3D('',#221396,#126255,#126256);
#104930=AXIS2_PLACEMENT_3D('',#221400,#126258,#126259);
#104931=AXIS2_PLACEMENT_3D('',#221404,#126261,#126262);
#104932=AXIS2_PLACEMENT_3D('',#221405,#126263,#126264);
#104933=AXIS2_PLACEMENT_3D('',#221406,#126265,#126266);
#104934=AXIS2_PLACEMENT_3D('',#221409,#126267,#126268);
#104935=AXIS2_PLACEMENT_3D('',#221412,#126271,#126272);
#104936=AXIS2_PLACEMENT_3D('',#221413,#126273,#126274);
#104937=AXIS2_PLACEMENT_3D('',#221414,#126275,#126276);
#104938=AXIS2_PLACEMENT_3D('',#221415,#126277,#126278);
#104939=AXIS2_PLACEMENT_3D('',#221416,#126279,#126280);
#104940=AXIS2_PLACEMENT_3D('',#221417,#126281,#126282);
#104941=AXIS2_PLACEMENT_3D('',#221418,#126283,#126284);
#104942=AXIS2_PLACEMENT_3D('',#221419,#126285,#126286);
#104943=AXIS2_PLACEMENT_3D('',#221420,#126287,#126288);
#104944=AXIS2_PLACEMENT_3D('',#221421,#126289,#126290);
#104945=AXIS2_PLACEMENT_3D('',#221422,#126291,#126292);
#104946=AXIS2_PLACEMENT_3D('',#221423,#126293,#126294);
#104947=AXIS2_PLACEMENT_3D('',#221424,#126295,#126296);
#104948=AXIS2_PLACEMENT_3D('',#221427,#126297,#126298);
#104949=AXIS2_PLACEMENT_3D('',#221431,#126300,#126301);
#104950=AXIS2_PLACEMENT_3D('',#221433,#126302,#126303);
#104951=AXIS2_PLACEMENT_3D('',#221435,#126304,#126305);
#104952=AXIS2_PLACEMENT_3D('',#221437,#126307,#126308);
#104953=AXIS2_PLACEMENT_3D('',#221441,#126310,#126311);
#104954=AXIS2_PLACEMENT_3D('',#221443,#126313,#126314);
#104955=AXIS2_PLACEMENT_3D('',#221446,#126315,#126316);
#104956=AXIS2_PLACEMENT_3D('',#221450,#126318,#126319);
#104957=AXIS2_PLACEMENT_3D('',#221452,#126321,#126322);
#104958=AXIS2_PLACEMENT_3D('',#221455,#126323,#126324);
#104959=AXIS2_PLACEMENT_3D('',#221459,#126326,#126327);
#104960=AXIS2_PLACEMENT_3D('',#221461,#126328,#126329);
#104961=AXIS2_PLACEMENT_3D('',#221463,#126330,#126331);
#104962=AXIS2_PLACEMENT_3D('',#221465,#126333,#126334);
#104963=AXIS2_PLACEMENT_3D('',#221469,#126336,#126337);
#104964=AXIS2_PLACEMENT_3D('',#221471,#126339,#126340);
#104965=AXIS2_PLACEMENT_3D('',#221472,#126341,#126342);
#104966=AXIS2_PLACEMENT_3D('',#221473,#126343,#126344);
#104967=AXIS2_PLACEMENT_3D('',#221474,#126345,#126346);
#104968=AXIS2_PLACEMENT_3D('',#221475,#126347,#126348);
#104969=AXIS2_PLACEMENT_3D('',#221476,#126349,#126350);
#104970=AXIS2_PLACEMENT_3D('',#221477,#126351,#126352);
#104971=AXIS2_PLACEMENT_3D('',#221478,#126353,#126354);
#104972=AXIS2_PLACEMENT_3D('',#221479,#126355,#126356);
#104973=AXIS2_PLACEMENT_3D('',#221480,#126357,#126358);
#104974=AXIS2_PLACEMENT_3D('',#221481,#126359,#126360);
#104975=AXIS2_PLACEMENT_3D('',#221482,#126361,#126362);
#104976=AXIS2_PLACEMENT_3D('',#221483,#126363,#126364);
#104977=AXIS2_PLACEMENT_3D('',#221486,#126365,#126366);
#104978=AXIS2_PLACEMENT_3D('',#221490,#126368,#126369);
#104979=AXIS2_PLACEMENT_3D('',#221492,#126370,#126371);
#104980=AXIS2_PLACEMENT_3D('',#221494,#126372,#126373);
#104981=AXIS2_PLACEMENT_3D('',#221496,#126375,#126376);
#104982=AXIS2_PLACEMENT_3D('',#221500,#126378,#126379);
#104983=AXIS2_PLACEMENT_3D('',#221502,#126381,#126382);
#104984=AXIS2_PLACEMENT_3D('',#221505,#126383,#126384);
#104985=AXIS2_PLACEMENT_3D('',#221509,#126386,#126387);
#104986=AXIS2_PLACEMENT_3D('',#221511,#126389,#126390);
#104987=AXIS2_PLACEMENT_3D('',#221514,#126391,#126392);
#104988=AXIS2_PLACEMENT_3D('',#221518,#126394,#126395);
#104989=AXIS2_PLACEMENT_3D('',#221520,#126396,#126397);
#104990=AXIS2_PLACEMENT_3D('',#221522,#126398,#126399);
#104991=AXIS2_PLACEMENT_3D('',#221524,#126401,#126402);
#104992=AXIS2_PLACEMENT_3D('',#221528,#126404,#126405);
#104993=AXIS2_PLACEMENT_3D('',#221530,#126407,#126408);
#104994=AXIS2_PLACEMENT_3D('',#221531,#126409,#126410);
#104995=AXIS2_PLACEMENT_3D('',#221532,#126411,#126412);
#104996=AXIS2_PLACEMENT_3D('',#221533,#126413,#126414);
#104997=AXIS2_PLACEMENT_3D('',#221534,#126415,#126416);
#104998=AXIS2_PLACEMENT_3D('',#221535,#126417,#126418);
#104999=AXIS2_PLACEMENT_3D('',#221536,#126419,#126420);
#105000=AXIS2_PLACEMENT_3D('',#221537,#126421,#126422);
#105001=AXIS2_PLACEMENT_3D('',#221538,#126423,#126424);
#105002=AXIS2_PLACEMENT_3D('',#221539,#126425,#126426);
#105003=AXIS2_PLACEMENT_3D('',#221540,#126427,#126428);
#105004=AXIS2_PLACEMENT_3D('',#221541,#126429,#126430);
#105005=AXIS2_PLACEMENT_3D('',#221542,#126431,#126432);
#105006=AXIS2_PLACEMENT_3D('',#221545,#126433,#126434);
#105007=AXIS2_PLACEMENT_3D('',#221549,#126436,#126437);
#105008=AXIS2_PLACEMENT_3D('',#221551,#126438,#126439);
#105009=AXIS2_PLACEMENT_3D('',#221553,#126440,#126441);
#105010=AXIS2_PLACEMENT_3D('',#221555,#126443,#126444);
#105011=AXIS2_PLACEMENT_3D('',#221559,#126446,#126447);
#105012=AXIS2_PLACEMENT_3D('',#221561,#126449,#126450);
#105013=AXIS2_PLACEMENT_3D('',#221564,#126451,#126452);
#105014=AXIS2_PLACEMENT_3D('',#221568,#126454,#126455);
#105015=AXIS2_PLACEMENT_3D('',#221570,#126457,#126458);
#105016=AXIS2_PLACEMENT_3D('',#221573,#126459,#126460);
#105017=AXIS2_PLACEMENT_3D('',#221577,#126462,#126463);
#105018=AXIS2_PLACEMENT_3D('',#221579,#126464,#126465);
#105019=AXIS2_PLACEMENT_3D('',#221581,#126466,#126467);
#105020=AXIS2_PLACEMENT_3D('',#221583,#126469,#126470);
#105021=AXIS2_PLACEMENT_3D('',#221587,#126472,#126473);
#105022=AXIS2_PLACEMENT_3D('',#221589,#126475,#126476);
#105023=AXIS2_PLACEMENT_3D('',#221590,#126477,#126478);
#105024=AXIS2_PLACEMENT_3D('',#221591,#126479,#126480);
#105025=AXIS2_PLACEMENT_3D('',#221592,#126481,#126482);
#105026=AXIS2_PLACEMENT_3D('',#221593,#126483,#126484);
#105027=AXIS2_PLACEMENT_3D('',#221594,#126485,#126486);
#105028=AXIS2_PLACEMENT_3D('',#221595,#126487,#126488);
#105029=AXIS2_PLACEMENT_3D('',#221596,#126489,#126490);
#105030=AXIS2_PLACEMENT_3D('',#221597,#126491,#126492);
#105031=AXIS2_PLACEMENT_3D('',#221598,#126493,#126494);
#105032=AXIS2_PLACEMENT_3D('',#221599,#126495,#126496);
#105033=AXIS2_PLACEMENT_3D('',#221600,#126497,#126498);
#105034=AXIS2_PLACEMENT_3D('',#221601,#126499,#126500);
#105035=AXIS2_PLACEMENT_3D('',#221604,#126501,#126502);
#105036=AXIS2_PLACEMENT_3D('',#221608,#126504,#126505);
#105037=AXIS2_PLACEMENT_3D('',#221610,#126506,#126507);
#105038=AXIS2_PLACEMENT_3D('',#221612,#126508,#126509);
#105039=AXIS2_PLACEMENT_3D('',#221614,#126511,#126512);
#105040=AXIS2_PLACEMENT_3D('',#221618,#126514,#126515);
#105041=AXIS2_PLACEMENT_3D('',#221620,#126517,#126518);
#105042=AXIS2_PLACEMENT_3D('',#221623,#126519,#126520);
#105043=AXIS2_PLACEMENT_3D('',#221627,#126522,#126523);
#105044=AXIS2_PLACEMENT_3D('',#221629,#126525,#126526);
#105045=AXIS2_PLACEMENT_3D('',#221632,#126527,#126528);
#105046=AXIS2_PLACEMENT_3D('',#221636,#126530,#126531);
#105047=AXIS2_PLACEMENT_3D('',#221638,#126532,#126533);
#105048=AXIS2_PLACEMENT_3D('',#221640,#126534,#126535);
#105049=AXIS2_PLACEMENT_3D('',#221642,#126537,#126538);
#105050=AXIS2_PLACEMENT_3D('',#221646,#126540,#126541);
#105051=AXIS2_PLACEMENT_3D('',#221648,#126543,#126544);
#105052=AXIS2_PLACEMENT_3D('',#221649,#126545,#126546);
#105053=AXIS2_PLACEMENT_3D('',#221650,#126547,#126548);
#105054=AXIS2_PLACEMENT_3D('',#221651,#126549,#126550);
#105055=AXIS2_PLACEMENT_3D('',#221652,#126551,#126552);
#105056=AXIS2_PLACEMENT_3D('',#221653,#126553,#126554);
#105057=AXIS2_PLACEMENT_3D('',#221654,#126555,#126556);
#105058=AXIS2_PLACEMENT_3D('',#221655,#126557,#126558);
#105059=AXIS2_PLACEMENT_3D('',#221656,#126559,#126560);
#105060=AXIS2_PLACEMENT_3D('',#221657,#126561,#126562);
#105061=AXIS2_PLACEMENT_3D('',#221658,#126563,#126564);
#105062=AXIS2_PLACEMENT_3D('',#221659,#126565,#126566);
#105063=AXIS2_PLACEMENT_3D('',#221660,#126567,#126568);
#105064=AXIS2_PLACEMENT_3D('',#221663,#126569,#126570);
#105065=AXIS2_PLACEMENT_3D('',#221667,#126572,#126573);
#105066=AXIS2_PLACEMENT_3D('',#221669,#126574,#126575);
#105067=AXIS2_PLACEMENT_3D('',#221671,#126576,#126577);
#105068=AXIS2_PLACEMENT_3D('',#221673,#126579,#126580);
#105069=AXIS2_PLACEMENT_3D('',#221677,#126582,#126583);
#105070=AXIS2_PLACEMENT_3D('',#221679,#126585,#126586);
#105071=AXIS2_PLACEMENT_3D('',#221682,#126587,#126588);
#105072=AXIS2_PLACEMENT_3D('',#221686,#126590,#126591);
#105073=AXIS2_PLACEMENT_3D('',#221688,#126593,#126594);
#105074=AXIS2_PLACEMENT_3D('',#221691,#126595,#126596);
#105075=AXIS2_PLACEMENT_3D('',#221695,#126598,#126599);
#105076=AXIS2_PLACEMENT_3D('',#221697,#126600,#126601);
#105077=AXIS2_PLACEMENT_3D('',#221699,#126602,#126603);
#105078=AXIS2_PLACEMENT_3D('',#221701,#126605,#126606);
#105079=AXIS2_PLACEMENT_3D('',#221705,#126608,#126609);
#105080=AXIS2_PLACEMENT_3D('',#221707,#126611,#126612);
#105081=AXIS2_PLACEMENT_3D('',#221708,#126613,#126614);
#105082=AXIS2_PLACEMENT_3D('',#221709,#126615,#126616);
#105083=AXIS2_PLACEMENT_3D('',#221710,#126617,#126618);
#105084=AXIS2_PLACEMENT_3D('',#221711,#126619,#126620);
#105085=AXIS2_PLACEMENT_3D('',#221712,#126621,#126622);
#105086=AXIS2_PLACEMENT_3D('',#221713,#126623,#126624);
#105087=AXIS2_PLACEMENT_3D('',#221714,#126625,#126626);
#105088=AXIS2_PLACEMENT_3D('',#221715,#126627,#126628);
#105089=AXIS2_PLACEMENT_3D('',#221716,#126629,#126630);
#105090=AXIS2_PLACEMENT_3D('',#221717,#126631,#126632);
#105091=AXIS2_PLACEMENT_3D('',#221718,#126633,#126634);
#105092=AXIS2_PLACEMENT_3D('',#221719,#126635,#126636);
#105093=AXIS2_PLACEMENT_3D('',#221722,#126637,#126638);
#105094=AXIS2_PLACEMENT_3D('',#221726,#126640,#126641);
#105095=AXIS2_PLACEMENT_3D('',#221728,#126642,#126643);
#105096=AXIS2_PLACEMENT_3D('',#221730,#126644,#126645);
#105097=AXIS2_PLACEMENT_3D('',#221732,#126647,#126648);
#105098=AXIS2_PLACEMENT_3D('',#221736,#126650,#126651);
#105099=AXIS2_PLACEMENT_3D('',#221738,#126653,#126654);
#105100=AXIS2_PLACEMENT_3D('',#221741,#126655,#126656);
#105101=AXIS2_PLACEMENT_3D('',#221745,#126658,#126659);
#105102=AXIS2_PLACEMENT_3D('',#221747,#126661,#126662);
#105103=AXIS2_PLACEMENT_3D('',#221750,#126663,#126664);
#105104=AXIS2_PLACEMENT_3D('',#221754,#126666,#126667);
#105105=AXIS2_PLACEMENT_3D('',#221756,#126668,#126669);
#105106=AXIS2_PLACEMENT_3D('',#221758,#126670,#126671);
#105107=AXIS2_PLACEMENT_3D('',#221760,#126673,#126674);
#105108=AXIS2_PLACEMENT_3D('',#221764,#126676,#126677);
#105109=AXIS2_PLACEMENT_3D('',#221766,#126679,#126680);
#105110=AXIS2_PLACEMENT_3D('',#221767,#126681,#126682);
#105111=AXIS2_PLACEMENT_3D('',#221768,#126683,#126684);
#105112=AXIS2_PLACEMENT_3D('',#221769,#126685,#126686);
#105113=AXIS2_PLACEMENT_3D('',#221770,#126687,#126688);
#105114=AXIS2_PLACEMENT_3D('',#221771,#126689,#126690);
#105115=AXIS2_PLACEMENT_3D('',#221772,#126691,#126692);
#105116=AXIS2_PLACEMENT_3D('',#221773,#126693,#126694);
#105117=AXIS2_PLACEMENT_3D('',#221774,#126695,#126696);
#105118=AXIS2_PLACEMENT_3D('',#221775,#126697,#126698);
#105119=AXIS2_PLACEMENT_3D('',#221776,#126699,#126700);
#105120=AXIS2_PLACEMENT_3D('',#221777,#126701,#126702);
#105121=AXIS2_PLACEMENT_3D('',#221778,#126703,#126704);
#105122=AXIS2_PLACEMENT_3D('',#221781,#126705,#126706);
#105123=AXIS2_PLACEMENT_3D('',#221785,#126708,#126709);
#105124=AXIS2_PLACEMENT_3D('',#221787,#126710,#126711);
#105125=AXIS2_PLACEMENT_3D('',#221789,#126712,#126713);
#105126=AXIS2_PLACEMENT_3D('',#221791,#126715,#126716);
#105127=AXIS2_PLACEMENT_3D('',#221795,#126718,#126719);
#105128=AXIS2_PLACEMENT_3D('',#221797,#126721,#126722);
#105129=AXIS2_PLACEMENT_3D('',#221800,#126723,#126724);
#105130=AXIS2_PLACEMENT_3D('',#221804,#126726,#126727);
#105131=AXIS2_PLACEMENT_3D('',#221806,#126729,#126730);
#105132=AXIS2_PLACEMENT_3D('',#221809,#126731,#126732);
#105133=AXIS2_PLACEMENT_3D('',#221813,#126734,#126735);
#105134=AXIS2_PLACEMENT_3D('',#221815,#126736,#126737);
#105135=AXIS2_PLACEMENT_3D('',#221817,#126738,#126739);
#105136=AXIS2_PLACEMENT_3D('',#221819,#126741,#126742);
#105137=AXIS2_PLACEMENT_3D('',#221823,#126744,#126745);
#105138=AXIS2_PLACEMENT_3D('',#221825,#126747,#126748);
#105139=AXIS2_PLACEMENT_3D('',#221826,#126749,#126750);
#105140=AXIS2_PLACEMENT_3D('',#221827,#126751,#126752);
#105141=AXIS2_PLACEMENT_3D('',#221828,#126753,#126754);
#105142=AXIS2_PLACEMENT_3D('',#221829,#126755,#126756);
#105143=AXIS2_PLACEMENT_3D('',#221830,#126757,#126758);
#105144=AXIS2_PLACEMENT_3D('',#221831,#126759,#126760);
#105145=AXIS2_PLACEMENT_3D('',#221832,#126761,#126762);
#105146=AXIS2_PLACEMENT_3D('',#221833,#126763,#126764);
#105147=AXIS2_PLACEMENT_3D('',#221834,#126765,#126766);
#105148=AXIS2_PLACEMENT_3D('',#221835,#126767,#126768);
#105149=AXIS2_PLACEMENT_3D('',#221836,#126769,#126770);
#105150=AXIS2_PLACEMENT_3D('',#221837,#126771,#126772);
#105151=AXIS2_PLACEMENT_3D('',#221840,#126773,#126774);
#105152=AXIS2_PLACEMENT_3D('',#221844,#126776,#126777);
#105153=AXIS2_PLACEMENT_3D('',#221846,#126778,#126779);
#105154=AXIS2_PLACEMENT_3D('',#221848,#126780,#126781);
#105155=AXIS2_PLACEMENT_3D('',#221850,#126783,#126784);
#105156=AXIS2_PLACEMENT_3D('',#221854,#126786,#126787);
#105157=AXIS2_PLACEMENT_3D('',#221856,#126789,#126790);
#105158=AXIS2_PLACEMENT_3D('',#221859,#126791,#126792);
#105159=AXIS2_PLACEMENT_3D('',#221863,#126794,#126795);
#105160=AXIS2_PLACEMENT_3D('',#221865,#126797,#126798);
#105161=AXIS2_PLACEMENT_3D('',#221868,#126799,#126800);
#105162=AXIS2_PLACEMENT_3D('',#221872,#126802,#126803);
#105163=AXIS2_PLACEMENT_3D('',#221874,#126804,#126805);
#105164=AXIS2_PLACEMENT_3D('',#221876,#126806,#126807);
#105165=AXIS2_PLACEMENT_3D('',#221878,#126809,#126810);
#105166=AXIS2_PLACEMENT_3D('',#221882,#126812,#126813);
#105167=AXIS2_PLACEMENT_3D('',#221884,#126815,#126816);
#105168=AXIS2_PLACEMENT_3D('',#221885,#126817,#126818);
#105169=AXIS2_PLACEMENT_3D('',#221886,#126819,#126820);
#105170=AXIS2_PLACEMENT_3D('',#221887,#126821,#126822);
#105171=AXIS2_PLACEMENT_3D('',#221888,#126823,#126824);
#105172=AXIS2_PLACEMENT_3D('',#221889,#126825,#126826);
#105173=AXIS2_PLACEMENT_3D('',#221890,#126827,#126828);
#105174=AXIS2_PLACEMENT_3D('',#221891,#126829,#126830);
#105175=AXIS2_PLACEMENT_3D('',#221892,#126831,#126832);
#105176=AXIS2_PLACEMENT_3D('',#221893,#126833,#126834);
#105177=AXIS2_PLACEMENT_3D('',#221894,#126835,#126836);
#105178=AXIS2_PLACEMENT_3D('',#221895,#126837,#126838);
#105179=AXIS2_PLACEMENT_3D('',#221896,#126839,#126840);
#105180=AXIS2_PLACEMENT_3D('',#221899,#126841,#126842);
#105181=AXIS2_PLACEMENT_3D('',#221903,#126844,#126845);
#105182=AXIS2_PLACEMENT_3D('',#221905,#126846,#126847);
#105183=AXIS2_PLACEMENT_3D('',#221907,#126848,#126849);
#105184=AXIS2_PLACEMENT_3D('',#221909,#126851,#126852);
#105185=AXIS2_PLACEMENT_3D('',#221913,#126854,#126855);
#105186=AXIS2_PLACEMENT_3D('',#221915,#126857,#126858);
#105187=AXIS2_PLACEMENT_3D('',#221918,#126859,#126860);
#105188=AXIS2_PLACEMENT_3D('',#221922,#126862,#126863);
#105189=AXIS2_PLACEMENT_3D('',#221924,#126865,#126866);
#105190=AXIS2_PLACEMENT_3D('',#221927,#126867,#126868);
#105191=AXIS2_PLACEMENT_3D('',#221931,#126870,#126871);
#105192=AXIS2_PLACEMENT_3D('',#221933,#126872,#126873);
#105193=AXIS2_PLACEMENT_3D('',#221935,#126874,#126875);
#105194=AXIS2_PLACEMENT_3D('',#221937,#126877,#126878);
#105195=AXIS2_PLACEMENT_3D('',#221941,#126880,#126881);
#105196=AXIS2_PLACEMENT_3D('',#221943,#126883,#126884);
#105197=AXIS2_PLACEMENT_3D('',#221944,#126885,#126886);
#105198=AXIS2_PLACEMENT_3D('',#221945,#126887,#126888);
#105199=AXIS2_PLACEMENT_3D('',#221946,#126889,#126890);
#105200=AXIS2_PLACEMENT_3D('',#221947,#126891,#126892);
#105201=AXIS2_PLACEMENT_3D('',#221948,#126893,#126894);
#105202=AXIS2_PLACEMENT_3D('',#221949,#126895,#126896);
#105203=AXIS2_PLACEMENT_3D('',#221950,#126897,#126898);
#105204=AXIS2_PLACEMENT_3D('',#221951,#126899,#126900);
#105205=AXIS2_PLACEMENT_3D('',#221952,#126901,#126902);
#105206=AXIS2_PLACEMENT_3D('',#221953,#126903,#126904);
#105207=AXIS2_PLACEMENT_3D('',#221954,#126905,#126906);
#105208=AXIS2_PLACEMENT_3D('',#221955,#126907,#126908);
#105209=AXIS2_PLACEMENT_3D('',#221958,#126909,#126910);
#105210=AXIS2_PLACEMENT_3D('',#221962,#126912,#126913);
#105211=AXIS2_PLACEMENT_3D('',#221964,#126914,#126915);
#105212=AXIS2_PLACEMENT_3D('',#221966,#126916,#126917);
#105213=AXIS2_PLACEMENT_3D('',#221968,#126919,#126920);
#105214=AXIS2_PLACEMENT_3D('',#221972,#126922,#126923);
#105215=AXIS2_PLACEMENT_3D('',#221974,#126925,#126926);
#105216=AXIS2_PLACEMENT_3D('',#221977,#126927,#126928);
#105217=AXIS2_PLACEMENT_3D('',#221981,#126930,#126931);
#105218=AXIS2_PLACEMENT_3D('',#221983,#126933,#126934);
#105219=AXIS2_PLACEMENT_3D('',#221986,#126935,#126936);
#105220=AXIS2_PLACEMENT_3D('',#221990,#126938,#126939);
#105221=AXIS2_PLACEMENT_3D('',#221992,#126940,#126941);
#105222=AXIS2_PLACEMENT_3D('',#221994,#126942,#126943);
#105223=AXIS2_PLACEMENT_3D('',#221996,#126945,#126946);
#105224=AXIS2_PLACEMENT_3D('',#222000,#126948,#126949);
#105225=AXIS2_PLACEMENT_3D('',#222002,#126951,#126952);
#105226=AXIS2_PLACEMENT_3D('',#222003,#126953,#126954);
#105227=AXIS2_PLACEMENT_3D('',#222004,#126955,#126956);
#105228=AXIS2_PLACEMENT_3D('',#222005,#126957,#126958);
#105229=AXIS2_PLACEMENT_3D('',#222006,#126959,#126960);
#105230=AXIS2_PLACEMENT_3D('',#222007,#126961,#126962);
#105231=AXIS2_PLACEMENT_3D('',#222008,#126963,#126964);
#105232=AXIS2_PLACEMENT_3D('',#222009,#126965,#126966);
#105233=AXIS2_PLACEMENT_3D('',#222010,#126967,#126968);
#105234=AXIS2_PLACEMENT_3D('',#222011,#126969,#126970);
#105235=AXIS2_PLACEMENT_3D('',#222012,#126971,#126972);
#105236=AXIS2_PLACEMENT_3D('',#222013,#126973,#126974);
#105237=AXIS2_PLACEMENT_3D('',#222014,#126975,#126976);
#105238=AXIS2_PLACEMENT_3D('',#222017,#126977,#126978);
#105239=AXIS2_PLACEMENT_3D('',#222021,#126980,#126981);
#105240=AXIS2_PLACEMENT_3D('',#222023,#126982,#126983);
#105241=AXIS2_PLACEMENT_3D('',#222025,#126984,#126985);
#105242=AXIS2_PLACEMENT_3D('',#222027,#126987,#126988);
#105243=AXIS2_PLACEMENT_3D('',#222031,#126990,#126991);
#105244=AXIS2_PLACEMENT_3D('',#222033,#126993,#126994);
#105245=AXIS2_PLACEMENT_3D('',#222036,#126995,#126996);
#105246=AXIS2_PLACEMENT_3D('',#222040,#126998,#126999);
#105247=AXIS2_PLACEMENT_3D('',#222042,#127001,#127002);
#105248=AXIS2_PLACEMENT_3D('',#222045,#127003,#127004);
#105249=AXIS2_PLACEMENT_3D('',#222049,#127006,#127007);
#105250=AXIS2_PLACEMENT_3D('',#222051,#127008,#127009);
#105251=AXIS2_PLACEMENT_3D('',#222053,#127010,#127011);
#105252=AXIS2_PLACEMENT_3D('',#222055,#127013,#127014);
#105253=AXIS2_PLACEMENT_3D('',#222059,#127016,#127017);
#105254=AXIS2_PLACEMENT_3D('',#222061,#127019,#127020);
#105255=AXIS2_PLACEMENT_3D('',#222062,#127021,#127022);
#105256=AXIS2_PLACEMENT_3D('',#222063,#127023,#127024);
#105257=AXIS2_PLACEMENT_3D('',#222064,#127025,#127026);
#105258=AXIS2_PLACEMENT_3D('',#222065,#127027,#127028);
#105259=AXIS2_PLACEMENT_3D('',#222066,#127029,#127030);
#105260=AXIS2_PLACEMENT_3D('',#222067,#127031,#127032);
#105261=AXIS2_PLACEMENT_3D('',#222068,#127033,#127034);
#105262=AXIS2_PLACEMENT_3D('',#222069,#127035,#127036);
#105263=AXIS2_PLACEMENT_3D('',#222070,#127037,#127038);
#105264=AXIS2_PLACEMENT_3D('',#222071,#127039,#127040);
#105265=AXIS2_PLACEMENT_3D('',#222072,#127041,#127042);
#105266=AXIS2_PLACEMENT_3D('',#222073,#127043,#127044);
#105267=AXIS2_PLACEMENT_3D('',#222076,#127045,#127046);
#105268=AXIS2_PLACEMENT_3D('',#222080,#127048,#127049);
#105269=AXIS2_PLACEMENT_3D('',#222082,#127050,#127051);
#105270=AXIS2_PLACEMENT_3D('',#222084,#127052,#127053);
#105271=AXIS2_PLACEMENT_3D('',#222086,#127055,#127056);
#105272=AXIS2_PLACEMENT_3D('',#222090,#127058,#127059);
#105273=AXIS2_PLACEMENT_3D('',#222092,#127061,#127062);
#105274=AXIS2_PLACEMENT_3D('',#222095,#127063,#127064);
#105275=AXIS2_PLACEMENT_3D('',#222099,#127066,#127067);
#105276=AXIS2_PLACEMENT_3D('',#222101,#127069,#127070);
#105277=AXIS2_PLACEMENT_3D('',#222104,#127071,#127072);
#105278=AXIS2_PLACEMENT_3D('',#222108,#127074,#127075);
#105279=AXIS2_PLACEMENT_3D('',#222110,#127076,#127077);
#105280=AXIS2_PLACEMENT_3D('',#222112,#127078,#127079);
#105281=AXIS2_PLACEMENT_3D('',#222114,#127081,#127082);
#105282=AXIS2_PLACEMENT_3D('',#222118,#127084,#127085);
#105283=AXIS2_PLACEMENT_3D('',#222120,#127087,#127088);
#105284=AXIS2_PLACEMENT_3D('',#222121,#127089,#127090);
#105285=AXIS2_PLACEMENT_3D('',#222122,#127091,#127092);
#105286=AXIS2_PLACEMENT_3D('',#222123,#127093,#127094);
#105287=AXIS2_PLACEMENT_3D('',#222124,#127095,#127096);
#105288=AXIS2_PLACEMENT_3D('',#222125,#127097,#127098);
#105289=AXIS2_PLACEMENT_3D('',#222126,#127099,#127100);
#105290=AXIS2_PLACEMENT_3D('',#222127,#127101,#127102);
#105291=AXIS2_PLACEMENT_3D('',#222128,#127103,#127104);
#105292=AXIS2_PLACEMENT_3D('',#222129,#127105,#127106);
#105293=AXIS2_PLACEMENT_3D('',#222130,#127107,#127108);
#105294=AXIS2_PLACEMENT_3D('',#222131,#127109,#127110);
#105295=AXIS2_PLACEMENT_3D('',#222132,#127111,#127112);
#105296=AXIS2_PLACEMENT_3D('',#222135,#127113,#127114);
#105297=AXIS2_PLACEMENT_3D('',#222139,#127116,#127117);
#105298=AXIS2_PLACEMENT_3D('',#222141,#127118,#127119);
#105299=AXIS2_PLACEMENT_3D('',#222143,#127120,#127121);
#105300=AXIS2_PLACEMENT_3D('',#222145,#127123,#127124);
#105301=AXIS2_PLACEMENT_3D('',#222149,#127126,#127127);
#105302=AXIS2_PLACEMENT_3D('',#222151,#127129,#127130);
#105303=AXIS2_PLACEMENT_3D('',#222154,#127131,#127132);
#105304=AXIS2_PLACEMENT_3D('',#222158,#127134,#127135);
#105305=AXIS2_PLACEMENT_3D('',#222160,#127137,#127138);
#105306=AXIS2_PLACEMENT_3D('',#222163,#127139,#127140);
#105307=AXIS2_PLACEMENT_3D('',#222167,#127142,#127143);
#105308=AXIS2_PLACEMENT_3D('',#222169,#127144,#127145);
#105309=AXIS2_PLACEMENT_3D('',#222171,#127146,#127147);
#105310=AXIS2_PLACEMENT_3D('',#222173,#127149,#127150);
#105311=AXIS2_PLACEMENT_3D('',#222177,#127152,#127153);
#105312=AXIS2_PLACEMENT_3D('',#222179,#127155,#127156);
#105313=AXIS2_PLACEMENT_3D('',#222180,#127157,#127158);
#105314=AXIS2_PLACEMENT_3D('',#222181,#127159,#127160);
#105315=AXIS2_PLACEMENT_3D('',#222182,#127161,#127162);
#105316=AXIS2_PLACEMENT_3D('',#222183,#127163,#127164);
#105317=AXIS2_PLACEMENT_3D('',#222184,#127165,#127166);
#105318=AXIS2_PLACEMENT_3D('',#222185,#127167,#127168);
#105319=AXIS2_PLACEMENT_3D('',#222186,#127169,#127170);
#105320=AXIS2_PLACEMENT_3D('',#222187,#127171,#127172);
#105321=AXIS2_PLACEMENT_3D('',#222188,#127173,#127174);
#105322=AXIS2_PLACEMENT_3D('',#222189,#127175,#127176);
#105323=AXIS2_PLACEMENT_3D('',#222190,#127177,#127178);
#105324=AXIS2_PLACEMENT_3D('',#222191,#127179,#127180);
#105325=AXIS2_PLACEMENT_3D('',#222194,#127181,#127182);
#105326=AXIS2_PLACEMENT_3D('',#222198,#127184,#127185);
#105327=AXIS2_PLACEMENT_3D('',#222200,#127186,#127187);
#105328=AXIS2_PLACEMENT_3D('',#222202,#127188,#127189);
#105329=AXIS2_PLACEMENT_3D('',#222204,#127191,#127192);
#105330=AXIS2_PLACEMENT_3D('',#222208,#127194,#127195);
#105331=AXIS2_PLACEMENT_3D('',#222210,#127197,#127198);
#105332=AXIS2_PLACEMENT_3D('',#222213,#127199,#127200);
#105333=AXIS2_PLACEMENT_3D('',#222217,#127202,#127203);
#105334=AXIS2_PLACEMENT_3D('',#222219,#127205,#127206);
#105335=AXIS2_PLACEMENT_3D('',#222222,#127207,#127208);
#105336=AXIS2_PLACEMENT_3D('',#222226,#127210,#127211);
#105337=AXIS2_PLACEMENT_3D('',#222228,#127212,#127213);
#105338=AXIS2_PLACEMENT_3D('',#222230,#127214,#127215);
#105339=AXIS2_PLACEMENT_3D('',#222232,#127217,#127218);
#105340=AXIS2_PLACEMENT_3D('',#222236,#127220,#127221);
#105341=AXIS2_PLACEMENT_3D('',#222238,#127223,#127224);
#105342=AXIS2_PLACEMENT_3D('',#222239,#127225,#127226);
#105343=AXIS2_PLACEMENT_3D('',#222240,#127227,#127228);
#105344=AXIS2_PLACEMENT_3D('',#222241,#127229,#127230);
#105345=AXIS2_PLACEMENT_3D('',#222242,#127231,#127232);
#105346=AXIS2_PLACEMENT_3D('',#222243,#127233,#127234);
#105347=AXIS2_PLACEMENT_3D('',#222244,#127235,#127236);
#105348=AXIS2_PLACEMENT_3D('',#222245,#127237,#127238);
#105349=AXIS2_PLACEMENT_3D('',#222246,#127239,#127240);
#105350=AXIS2_PLACEMENT_3D('',#222247,#127241,#127242);
#105351=AXIS2_PLACEMENT_3D('',#222248,#127243,#127244);
#105352=AXIS2_PLACEMENT_3D('',#222249,#127245,#127246);
#105353=AXIS2_PLACEMENT_3D('',#222250,#127247,#127248);
#105354=AXIS2_PLACEMENT_3D('',#222253,#127249,#127250);
#105355=AXIS2_PLACEMENT_3D('',#222257,#127252,#127253);
#105356=AXIS2_PLACEMENT_3D('',#222259,#127254,#127255);
#105357=AXIS2_PLACEMENT_3D('',#222261,#127256,#127257);
#105358=AXIS2_PLACEMENT_3D('',#222263,#127259,#127260);
#105359=AXIS2_PLACEMENT_3D('',#222267,#127262,#127263);
#105360=AXIS2_PLACEMENT_3D('',#222269,#127265,#127266);
#105361=AXIS2_PLACEMENT_3D('',#222272,#127267,#127268);
#105362=AXIS2_PLACEMENT_3D('',#222276,#127270,#127271);
#105363=AXIS2_PLACEMENT_3D('',#222278,#127273,#127274);
#105364=AXIS2_PLACEMENT_3D('',#222281,#127275,#127276);
#105365=AXIS2_PLACEMENT_3D('',#222285,#127278,#127279);
#105366=AXIS2_PLACEMENT_3D('',#222287,#127280,#127281);
#105367=AXIS2_PLACEMENT_3D('',#222289,#127282,#127283);
#105368=AXIS2_PLACEMENT_3D('',#222291,#127285,#127286);
#105369=AXIS2_PLACEMENT_3D('',#222295,#127288,#127289);
#105370=AXIS2_PLACEMENT_3D('',#222297,#127291,#127292);
#105371=AXIS2_PLACEMENT_3D('',#222298,#127293,#127294);
#105372=AXIS2_PLACEMENT_3D('',#222299,#127295,#127296);
#105373=AXIS2_PLACEMENT_3D('',#222300,#127297,#127298);
#105374=AXIS2_PLACEMENT_3D('',#222301,#127299,#127300);
#105375=AXIS2_PLACEMENT_3D('',#222302,#127301,#127302);
#105376=AXIS2_PLACEMENT_3D('',#222303,#127303,#127304);
#105377=AXIS2_PLACEMENT_3D('',#222304,#127305,#127306);
#105378=AXIS2_PLACEMENT_3D('',#222305,#127307,#127308);
#105379=AXIS2_PLACEMENT_3D('',#222306,#127309,#127310);
#105380=AXIS2_PLACEMENT_3D('',#222307,#127311,#127312);
#105381=AXIS2_PLACEMENT_3D('',#222308,#127313,#127314);
#105382=AXIS2_PLACEMENT_3D('',#222309,#127315,#127316);
#105383=AXIS2_PLACEMENT_3D('',#222312,#127317,#127318);
#105384=AXIS2_PLACEMENT_3D('',#222316,#127320,#127321);
#105385=AXIS2_PLACEMENT_3D('',#222318,#127322,#127323);
#105386=AXIS2_PLACEMENT_3D('',#222320,#127324,#127325);
#105387=AXIS2_PLACEMENT_3D('',#222322,#127327,#127328);
#105388=AXIS2_PLACEMENT_3D('',#222326,#127330,#127331);
#105389=AXIS2_PLACEMENT_3D('',#222328,#127333,#127334);
#105390=AXIS2_PLACEMENT_3D('',#222331,#127335,#127336);
#105391=AXIS2_PLACEMENT_3D('',#222335,#127338,#127339);
#105392=AXIS2_PLACEMENT_3D('',#222337,#127341,#127342);
#105393=AXIS2_PLACEMENT_3D('',#222340,#127343,#127344);
#105394=AXIS2_PLACEMENT_3D('',#222344,#127346,#127347);
#105395=AXIS2_PLACEMENT_3D('',#222346,#127348,#127349);
#105396=AXIS2_PLACEMENT_3D('',#222348,#127350,#127351);
#105397=AXIS2_PLACEMENT_3D('',#222350,#127353,#127354);
#105398=AXIS2_PLACEMENT_3D('',#222354,#127356,#127357);
#105399=AXIS2_PLACEMENT_3D('',#222356,#127359,#127360);
#105400=AXIS2_PLACEMENT_3D('',#222357,#127361,#127362);
#105401=AXIS2_PLACEMENT_3D('',#222358,#127363,#127364);
#105402=AXIS2_PLACEMENT_3D('',#222359,#127365,#127366);
#105403=AXIS2_PLACEMENT_3D('',#222360,#127367,#127368);
#105404=AXIS2_PLACEMENT_3D('',#222361,#127369,#127370);
#105405=AXIS2_PLACEMENT_3D('',#222362,#127371,#127372);
#105406=AXIS2_PLACEMENT_3D('',#222363,#127373,#127374);
#105407=AXIS2_PLACEMENT_3D('',#222364,#127375,#127376);
#105408=AXIS2_PLACEMENT_3D('',#222365,#127377,#127378);
#105409=AXIS2_PLACEMENT_3D('',#222366,#127379,#127380);
#105410=AXIS2_PLACEMENT_3D('',#222367,#127381,#127382);
#105411=AXIS2_PLACEMENT_3D('',#222368,#127383,#127384);
#105412=AXIS2_PLACEMENT_3D('',#222371,#127385,#127386);
#105413=AXIS2_PLACEMENT_3D('',#222375,#127388,#127389);
#105414=AXIS2_PLACEMENT_3D('',#222377,#127390,#127391);
#105415=AXIS2_PLACEMENT_3D('',#222379,#127392,#127393);
#105416=AXIS2_PLACEMENT_3D('',#222381,#127395,#127396);
#105417=AXIS2_PLACEMENT_3D('',#222385,#127398,#127399);
#105418=AXIS2_PLACEMENT_3D('',#222387,#127401,#127402);
#105419=AXIS2_PLACEMENT_3D('',#222390,#127403,#127404);
#105420=AXIS2_PLACEMENT_3D('',#222394,#127406,#127407);
#105421=AXIS2_PLACEMENT_3D('',#222396,#127409,#127410);
#105422=AXIS2_PLACEMENT_3D('',#222399,#127411,#127412);
#105423=AXIS2_PLACEMENT_3D('',#222403,#127414,#127415);
#105424=AXIS2_PLACEMENT_3D('',#222405,#127416,#127417);
#105425=AXIS2_PLACEMENT_3D('',#222407,#127418,#127419);
#105426=AXIS2_PLACEMENT_3D('',#222409,#127421,#127422);
#105427=AXIS2_PLACEMENT_3D('',#222413,#127424,#127425);
#105428=AXIS2_PLACEMENT_3D('',#222415,#127427,#127428);
#105429=AXIS2_PLACEMENT_3D('',#222416,#127429,#127430);
#105430=AXIS2_PLACEMENT_3D('',#222417,#127431,#127432);
#105431=AXIS2_PLACEMENT_3D('',#222418,#127433,#127434);
#105432=AXIS2_PLACEMENT_3D('',#222419,#127435,#127436);
#105433=AXIS2_PLACEMENT_3D('',#222420,#127437,#127438);
#105434=AXIS2_PLACEMENT_3D('',#222421,#127439,#127440);
#105435=AXIS2_PLACEMENT_3D('',#222422,#127441,#127442);
#105436=AXIS2_PLACEMENT_3D('',#222423,#127443,#127444);
#105437=AXIS2_PLACEMENT_3D('',#222424,#127445,#127446);
#105438=AXIS2_PLACEMENT_3D('',#222425,#127447,#127448);
#105439=AXIS2_PLACEMENT_3D('',#222426,#127449,#127450);
#105440=AXIS2_PLACEMENT_3D('',#222427,#127451,#127452);
#105441=AXIS2_PLACEMENT_3D('',#222430,#127453,#127454);
#105442=AXIS2_PLACEMENT_3D('',#222434,#127456,#127457);
#105443=AXIS2_PLACEMENT_3D('',#222436,#127458,#127459);
#105444=AXIS2_PLACEMENT_3D('',#222438,#127460,#127461);
#105445=AXIS2_PLACEMENT_3D('',#222440,#127463,#127464);
#105446=AXIS2_PLACEMENT_3D('',#222444,#127466,#127467);
#105447=AXIS2_PLACEMENT_3D('',#222446,#127469,#127470);
#105448=AXIS2_PLACEMENT_3D('',#222449,#127471,#127472);
#105449=AXIS2_PLACEMENT_3D('',#222453,#127474,#127475);
#105450=AXIS2_PLACEMENT_3D('',#222455,#127477,#127478);
#105451=AXIS2_PLACEMENT_3D('',#222458,#127479,#127480);
#105452=AXIS2_PLACEMENT_3D('',#222462,#127482,#127483);
#105453=AXIS2_PLACEMENT_3D('',#222464,#127484,#127485);
#105454=AXIS2_PLACEMENT_3D('',#222466,#127486,#127487);
#105455=AXIS2_PLACEMENT_3D('',#222468,#127489,#127490);
#105456=AXIS2_PLACEMENT_3D('',#222472,#127492,#127493);
#105457=AXIS2_PLACEMENT_3D('',#222474,#127495,#127496);
#105458=AXIS2_PLACEMENT_3D('',#222475,#127497,#127498);
#105459=AXIS2_PLACEMENT_3D('',#222476,#127499,#127500);
#105460=AXIS2_PLACEMENT_3D('',#222477,#127501,#127502);
#105461=AXIS2_PLACEMENT_3D('',#222478,#127503,#127504);
#105462=AXIS2_PLACEMENT_3D('',#222479,#127505,#127506);
#105463=AXIS2_PLACEMENT_3D('',#222480,#127507,#127508);
#105464=AXIS2_PLACEMENT_3D('',#222481,#127509,#127510);
#105465=AXIS2_PLACEMENT_3D('',#222482,#127511,#127512);
#105466=AXIS2_PLACEMENT_3D('',#222483,#127513,#127514);
#105467=AXIS2_PLACEMENT_3D('',#222484,#127515,#127516);
#105468=AXIS2_PLACEMENT_3D('',#222485,#127517,#127518);
#105469=AXIS2_PLACEMENT_3D('',#222486,#127519,#127520);
#105470=AXIS2_PLACEMENT_3D('',#222489,#127521,#127522);
#105471=AXIS2_PLACEMENT_3D('',#222493,#127524,#127525);
#105472=AXIS2_PLACEMENT_3D('',#222495,#127526,#127527);
#105473=AXIS2_PLACEMENT_3D('',#222497,#127528,#127529);
#105474=AXIS2_PLACEMENT_3D('',#222499,#127531,#127532);
#105475=AXIS2_PLACEMENT_3D('',#222503,#127534,#127535);
#105476=AXIS2_PLACEMENT_3D('',#222505,#127537,#127538);
#105477=AXIS2_PLACEMENT_3D('',#222508,#127539,#127540);
#105478=AXIS2_PLACEMENT_3D('',#222512,#127542,#127543);
#105479=AXIS2_PLACEMENT_3D('',#222514,#127545,#127546);
#105480=AXIS2_PLACEMENT_3D('',#222517,#127547,#127548);
#105481=AXIS2_PLACEMENT_3D('',#222521,#127550,#127551);
#105482=AXIS2_PLACEMENT_3D('',#222523,#127552,#127553);
#105483=AXIS2_PLACEMENT_3D('',#222525,#127554,#127555);
#105484=AXIS2_PLACEMENT_3D('',#222527,#127557,#127558);
#105485=AXIS2_PLACEMENT_3D('',#222531,#127560,#127561);
#105486=AXIS2_PLACEMENT_3D('',#222533,#127563,#127564);
#105487=AXIS2_PLACEMENT_3D('',#222534,#127565,#127566);
#105488=AXIS2_PLACEMENT_3D('',#222535,#127567,#127568);
#105489=AXIS2_PLACEMENT_3D('',#222536,#127569,#127570);
#105490=AXIS2_PLACEMENT_3D('',#222537,#127571,#127572);
#105491=AXIS2_PLACEMENT_3D('',#222538,#127573,#127574);
#105492=AXIS2_PLACEMENT_3D('',#222539,#127575,#127576);
#105493=AXIS2_PLACEMENT_3D('',#222540,#127577,#127578);
#105494=AXIS2_PLACEMENT_3D('',#222541,#127579,#127580);
#105495=AXIS2_PLACEMENT_3D('',#222542,#127581,#127582);
#105496=AXIS2_PLACEMENT_3D('',#222543,#127583,#127584);
#105497=AXIS2_PLACEMENT_3D('',#222544,#127585,#127586);
#105498=AXIS2_PLACEMENT_3D('',#222545,#127587,#127588);
#105499=AXIS2_PLACEMENT_3D('',#222548,#127589,#127590);
#105500=AXIS2_PLACEMENT_3D('',#222552,#127592,#127593);
#105501=AXIS2_PLACEMENT_3D('',#222554,#127594,#127595);
#105502=AXIS2_PLACEMENT_3D('',#222556,#127596,#127597);
#105503=AXIS2_PLACEMENT_3D('',#222558,#127599,#127600);
#105504=AXIS2_PLACEMENT_3D('',#222562,#127602,#127603);
#105505=AXIS2_PLACEMENT_3D('',#222564,#127605,#127606);
#105506=AXIS2_PLACEMENT_3D('',#222567,#127607,#127608);
#105507=AXIS2_PLACEMENT_3D('',#222571,#127610,#127611);
#105508=AXIS2_PLACEMENT_3D('',#222573,#127613,#127614);
#105509=AXIS2_PLACEMENT_3D('',#222576,#127615,#127616);
#105510=AXIS2_PLACEMENT_3D('',#222580,#127618,#127619);
#105511=AXIS2_PLACEMENT_3D('',#222582,#127620,#127621);
#105512=AXIS2_PLACEMENT_3D('',#222584,#127622,#127623);
#105513=AXIS2_PLACEMENT_3D('',#222586,#127625,#127626);
#105514=AXIS2_PLACEMENT_3D('',#222590,#127628,#127629);
#105515=AXIS2_PLACEMENT_3D('',#222592,#127631,#127632);
#105516=AXIS2_PLACEMENT_3D('',#222593,#127633,#127634);
#105517=AXIS2_PLACEMENT_3D('',#222594,#127635,#127636);
#105518=AXIS2_PLACEMENT_3D('',#222595,#127637,#127638);
#105519=AXIS2_PLACEMENT_3D('',#222596,#127639,#127640);
#105520=AXIS2_PLACEMENT_3D('',#222597,#127641,#127642);
#105521=AXIS2_PLACEMENT_3D('',#222598,#127643,#127644);
#105522=AXIS2_PLACEMENT_3D('',#222599,#127645,#127646);
#105523=AXIS2_PLACEMENT_3D('',#222600,#127647,#127648);
#105524=AXIS2_PLACEMENT_3D('',#222601,#127649,#127650);
#105525=AXIS2_PLACEMENT_3D('',#222602,#127651,#127652);
#105526=AXIS2_PLACEMENT_3D('',#222603,#127653,#127654);
#105527=AXIS2_PLACEMENT_3D('',#222604,#127655,#127656);
#105528=AXIS2_PLACEMENT_3D('',#222607,#127657,#127658);
#105529=AXIS2_PLACEMENT_3D('',#222611,#127660,#127661);
#105530=AXIS2_PLACEMENT_3D('',#222613,#127662,#127663);
#105531=AXIS2_PLACEMENT_3D('',#222615,#127664,#127665);
#105532=AXIS2_PLACEMENT_3D('',#222617,#127667,#127668);
#105533=AXIS2_PLACEMENT_3D('',#222621,#127670,#127671);
#105534=AXIS2_PLACEMENT_3D('',#222623,#127673,#127674);
#105535=AXIS2_PLACEMENT_3D('',#222626,#127675,#127676);
#105536=AXIS2_PLACEMENT_3D('',#222630,#127678,#127679);
#105537=AXIS2_PLACEMENT_3D('',#222632,#127681,#127682);
#105538=AXIS2_PLACEMENT_3D('',#222635,#127683,#127684);
#105539=AXIS2_PLACEMENT_3D('',#222639,#127686,#127687);
#105540=AXIS2_PLACEMENT_3D('',#222641,#127688,#127689);
#105541=AXIS2_PLACEMENT_3D('',#222643,#127690,#127691);
#105542=AXIS2_PLACEMENT_3D('',#222645,#127693,#127694);
#105543=AXIS2_PLACEMENT_3D('',#222649,#127696,#127697);
#105544=AXIS2_PLACEMENT_3D('',#222651,#127699,#127700);
#105545=AXIS2_PLACEMENT_3D('',#222652,#127701,#127702);
#105546=AXIS2_PLACEMENT_3D('',#222653,#127703,#127704);
#105547=AXIS2_PLACEMENT_3D('',#222654,#127705,#127706);
#105548=AXIS2_PLACEMENT_3D('',#222655,#127707,#127708);
#105549=AXIS2_PLACEMENT_3D('',#222656,#127709,#127710);
#105550=AXIS2_PLACEMENT_3D('',#222657,#127711,#127712);
#105551=AXIS2_PLACEMENT_3D('',#222658,#127713,#127714);
#105552=AXIS2_PLACEMENT_3D('',#222659,#127715,#127716);
#105553=AXIS2_PLACEMENT_3D('',#222660,#127717,#127718);
#105554=AXIS2_PLACEMENT_3D('',#222661,#127719,#127720);
#105555=AXIS2_PLACEMENT_3D('',#222662,#127721,#127722);
#105556=AXIS2_PLACEMENT_3D('',#222663,#127723,#127724);
#105557=AXIS2_PLACEMENT_3D('',#222666,#127725,#127726);
#105558=AXIS2_PLACEMENT_3D('',#222670,#127728,#127729);
#105559=AXIS2_PLACEMENT_3D('',#222672,#127730,#127731);
#105560=AXIS2_PLACEMENT_3D('',#222674,#127732,#127733);
#105561=AXIS2_PLACEMENT_3D('',#222676,#127735,#127736);
#105562=AXIS2_PLACEMENT_3D('',#222680,#127738,#127739);
#105563=AXIS2_PLACEMENT_3D('',#222682,#127741,#127742);
#105564=AXIS2_PLACEMENT_3D('',#222685,#127743,#127744);
#105565=AXIS2_PLACEMENT_3D('',#222689,#127746,#127747);
#105566=AXIS2_PLACEMENT_3D('',#222691,#127749,#127750);
#105567=AXIS2_PLACEMENT_3D('',#222694,#127751,#127752);
#105568=AXIS2_PLACEMENT_3D('',#222698,#127754,#127755);
#105569=AXIS2_PLACEMENT_3D('',#222700,#127756,#127757);
#105570=AXIS2_PLACEMENT_3D('',#222702,#127758,#127759);
#105571=AXIS2_PLACEMENT_3D('',#222704,#127761,#127762);
#105572=AXIS2_PLACEMENT_3D('',#222708,#127764,#127765);
#105573=AXIS2_PLACEMENT_3D('',#222710,#127767,#127768);
#105574=AXIS2_PLACEMENT_3D('',#222711,#127769,#127770);
#105575=AXIS2_PLACEMENT_3D('',#222712,#127771,#127772);
#105576=AXIS2_PLACEMENT_3D('',#222713,#127773,#127774);
#105577=AXIS2_PLACEMENT_3D('',#222714,#127775,#127776);
#105578=AXIS2_PLACEMENT_3D('',#222715,#127777,#127778);
#105579=AXIS2_PLACEMENT_3D('',#222716,#127779,#127780);
#105580=AXIS2_PLACEMENT_3D('',#222717,#127781,#127782);
#105581=AXIS2_PLACEMENT_3D('',#222718,#127783,#127784);
#105582=AXIS2_PLACEMENT_3D('',#222719,#127785,#127786);
#105583=AXIS2_PLACEMENT_3D('',#222720,#127787,#127788);
#105584=AXIS2_PLACEMENT_3D('',#222721,#127789,#127790);
#105585=AXIS2_PLACEMENT_3D('',#222722,#127791,#127792);
#105586=AXIS2_PLACEMENT_3D('',#222725,#127793,#127794);
#105587=AXIS2_PLACEMENT_3D('',#222729,#127796,#127797);
#105588=AXIS2_PLACEMENT_3D('',#222731,#127798,#127799);
#105589=AXIS2_PLACEMENT_3D('',#222733,#127800,#127801);
#105590=AXIS2_PLACEMENT_3D('',#222735,#127803,#127804);
#105591=AXIS2_PLACEMENT_3D('',#222739,#127806,#127807);
#105592=AXIS2_PLACEMENT_3D('',#222741,#127809,#127810);
#105593=AXIS2_PLACEMENT_3D('',#222744,#127811,#127812);
#105594=AXIS2_PLACEMENT_3D('',#222748,#127814,#127815);
#105595=AXIS2_PLACEMENT_3D('',#222750,#127817,#127818);
#105596=AXIS2_PLACEMENT_3D('',#222753,#127819,#127820);
#105597=AXIS2_PLACEMENT_3D('',#222757,#127822,#127823);
#105598=AXIS2_PLACEMENT_3D('',#222759,#127824,#127825);
#105599=AXIS2_PLACEMENT_3D('',#222761,#127826,#127827);
#105600=AXIS2_PLACEMENT_3D('',#222763,#127829,#127830);
#105601=AXIS2_PLACEMENT_3D('',#222767,#127832,#127833);
#105602=AXIS2_PLACEMENT_3D('',#222769,#127835,#127836);
#105603=AXIS2_PLACEMENT_3D('',#222770,#127837,#127838);
#105604=AXIS2_PLACEMENT_3D('',#222771,#127839,#127840);
#105605=AXIS2_PLACEMENT_3D('',#222772,#127841,#127842);
#105606=AXIS2_PLACEMENT_3D('',#222773,#127843,#127844);
#105607=AXIS2_PLACEMENT_3D('',#222774,#127845,#127846);
#105608=AXIS2_PLACEMENT_3D('',#222775,#127847,#127848);
#105609=AXIS2_PLACEMENT_3D('',#222776,#127849,#127850);
#105610=AXIS2_PLACEMENT_3D('',#222777,#127851,#127852);
#105611=AXIS2_PLACEMENT_3D('',#222778,#127853,#127854);
#105612=AXIS2_PLACEMENT_3D('',#222779,#127855,#127856);
#105613=AXIS2_PLACEMENT_3D('',#222780,#127857,#127858);
#105614=AXIS2_PLACEMENT_3D('',#222781,#127859,#127860);
#105615=AXIS2_PLACEMENT_3D('',#222784,#127861,#127862);
#105616=AXIS2_PLACEMENT_3D('',#222788,#127864,#127865);
#105617=AXIS2_PLACEMENT_3D('',#222790,#127866,#127867);
#105618=AXIS2_PLACEMENT_3D('',#222792,#127868,#127869);
#105619=AXIS2_PLACEMENT_3D('',#222794,#127871,#127872);
#105620=AXIS2_PLACEMENT_3D('',#222798,#127874,#127875);
#105621=AXIS2_PLACEMENT_3D('',#222800,#127877,#127878);
#105622=AXIS2_PLACEMENT_3D('',#222803,#127879,#127880);
#105623=AXIS2_PLACEMENT_3D('',#222807,#127882,#127883);
#105624=AXIS2_PLACEMENT_3D('',#222809,#127885,#127886);
#105625=AXIS2_PLACEMENT_3D('',#222812,#127887,#127888);
#105626=AXIS2_PLACEMENT_3D('',#222816,#127890,#127891);
#105627=AXIS2_PLACEMENT_3D('',#222818,#127892,#127893);
#105628=AXIS2_PLACEMENT_3D('',#222820,#127894,#127895);
#105629=AXIS2_PLACEMENT_3D('',#222822,#127897,#127898);
#105630=AXIS2_PLACEMENT_3D('',#222826,#127900,#127901);
#105631=AXIS2_PLACEMENT_3D('',#222828,#127903,#127904);
#105632=AXIS2_PLACEMENT_3D('',#222829,#127905,#127906);
#105633=AXIS2_PLACEMENT_3D('',#222830,#127907,#127908);
#105634=AXIS2_PLACEMENT_3D('',#222831,#127909,#127910);
#105635=AXIS2_PLACEMENT_3D('',#222832,#127911,#127912);
#105636=AXIS2_PLACEMENT_3D('',#222833,#127913,#127914);
#105637=AXIS2_PLACEMENT_3D('',#222834,#127915,#127916);
#105638=AXIS2_PLACEMENT_3D('',#222835,#127917,#127918);
#105639=AXIS2_PLACEMENT_3D('',#222836,#127919,#127920);
#105640=AXIS2_PLACEMENT_3D('',#222837,#127921,#127922);
#105641=AXIS2_PLACEMENT_3D('',#222838,#127923,#127924);
#105642=AXIS2_PLACEMENT_3D('',#222839,#127925,#127926);
#105643=AXIS2_PLACEMENT_3D('',#222840,#127927,#127928);
#105644=AXIS2_PLACEMENT_3D('',#222843,#127929,#127930);
#105645=AXIS2_PLACEMENT_3D('',#222847,#127932,#127933);
#105646=AXIS2_PLACEMENT_3D('',#222849,#127934,#127935);
#105647=AXIS2_PLACEMENT_3D('',#222851,#127936,#127937);
#105648=AXIS2_PLACEMENT_3D('',#222853,#127939,#127940);
#105649=AXIS2_PLACEMENT_3D('',#222857,#127942,#127943);
#105650=AXIS2_PLACEMENT_3D('',#222859,#127945,#127946);
#105651=AXIS2_PLACEMENT_3D('',#222862,#127947,#127948);
#105652=AXIS2_PLACEMENT_3D('',#222866,#127950,#127951);
#105653=AXIS2_PLACEMENT_3D('',#222868,#127953,#127954);
#105654=AXIS2_PLACEMENT_3D('',#222871,#127955,#127956);
#105655=AXIS2_PLACEMENT_3D('',#222875,#127958,#127959);
#105656=AXIS2_PLACEMENT_3D('',#222877,#127960,#127961);
#105657=AXIS2_PLACEMENT_3D('',#222879,#127962,#127963);
#105658=AXIS2_PLACEMENT_3D('',#222881,#127965,#127966);
#105659=AXIS2_PLACEMENT_3D('',#222885,#127968,#127969);
#105660=AXIS2_PLACEMENT_3D('',#222887,#127971,#127972);
#105661=AXIS2_PLACEMENT_3D('',#222888,#127973,#127974);
#105662=AXIS2_PLACEMENT_3D('',#222889,#127975,#127976);
#105663=AXIS2_PLACEMENT_3D('',#222890,#127977,#127978);
#105664=AXIS2_PLACEMENT_3D('',#222891,#127979,#127980);
#105665=AXIS2_PLACEMENT_3D('',#222892,#127981,#127982);
#105666=AXIS2_PLACEMENT_3D('',#222893,#127983,#127984);
#105667=AXIS2_PLACEMENT_3D('',#222894,#127985,#127986);
#105668=AXIS2_PLACEMENT_3D('',#222895,#127987,#127988);
#105669=AXIS2_PLACEMENT_3D('',#222896,#127989,#127990);
#105670=AXIS2_PLACEMENT_3D('',#222897,#127991,#127992);
#105671=AXIS2_PLACEMENT_3D('',#222898,#127993,#127994);
#105672=AXIS2_PLACEMENT_3D('',#222899,#127995,#127996);
#105673=AXIS2_PLACEMENT_3D('',#222902,#127997,#127998);
#105674=AXIS2_PLACEMENT_3D('',#222906,#128000,#128001);
#105675=AXIS2_PLACEMENT_3D('',#222908,#128002,#128003);
#105676=AXIS2_PLACEMENT_3D('',#222910,#128004,#128005);
#105677=AXIS2_PLACEMENT_3D('',#222912,#128007,#128008);
#105678=AXIS2_PLACEMENT_3D('',#222916,#128010,#128011);
#105679=AXIS2_PLACEMENT_3D('',#222918,#128013,#128014);
#105680=AXIS2_PLACEMENT_3D('',#222921,#128015,#128016);
#105681=AXIS2_PLACEMENT_3D('',#222925,#128018,#128019);
#105682=AXIS2_PLACEMENT_3D('',#222927,#128021,#128022);
#105683=AXIS2_PLACEMENT_3D('',#222930,#128023,#128024);
#105684=AXIS2_PLACEMENT_3D('',#222934,#128026,#128027);
#105685=AXIS2_PLACEMENT_3D('',#222936,#128028,#128029);
#105686=AXIS2_PLACEMENT_3D('',#222938,#128030,#128031);
#105687=AXIS2_PLACEMENT_3D('',#222940,#128033,#128034);
#105688=AXIS2_PLACEMENT_3D('',#222944,#128036,#128037);
#105689=AXIS2_PLACEMENT_3D('',#222946,#128039,#128040);
#105690=AXIS2_PLACEMENT_3D('',#222947,#128041,#128042);
#105691=AXIS2_PLACEMENT_3D('',#222948,#128043,#128044);
#105692=AXIS2_PLACEMENT_3D('',#222949,#128045,#128046);
#105693=AXIS2_PLACEMENT_3D('',#222950,#128047,#128048);
#105694=AXIS2_PLACEMENT_3D('',#222951,#128049,#128050);
#105695=AXIS2_PLACEMENT_3D('',#222952,#128051,#128052);
#105696=AXIS2_PLACEMENT_3D('',#222953,#128053,#128054);
#105697=AXIS2_PLACEMENT_3D('',#222954,#128055,#128056);
#105698=AXIS2_PLACEMENT_3D('',#222955,#128057,#128058);
#105699=AXIS2_PLACEMENT_3D('',#222956,#128059,#128060);
#105700=AXIS2_PLACEMENT_3D('',#222957,#128061,#128062);
#105701=AXIS2_PLACEMENT_3D('',#222958,#128063,#128064);
#105702=AXIS2_PLACEMENT_3D('',#222961,#128065,#128066);
#105703=AXIS2_PLACEMENT_3D('',#222965,#128068,#128069);
#105704=AXIS2_PLACEMENT_3D('',#222967,#128070,#128071);
#105705=AXIS2_PLACEMENT_3D('',#222969,#128072,#128073);
#105706=AXIS2_PLACEMENT_3D('',#222971,#128075,#128076);
#105707=AXIS2_PLACEMENT_3D('',#222975,#128078,#128079);
#105708=AXIS2_PLACEMENT_3D('',#222977,#128081,#128082);
#105709=AXIS2_PLACEMENT_3D('',#222980,#128083,#128084);
#105710=AXIS2_PLACEMENT_3D('',#222984,#128086,#128087);
#105711=AXIS2_PLACEMENT_3D('',#222986,#128089,#128090);
#105712=AXIS2_PLACEMENT_3D('',#222989,#128091,#128092);
#105713=AXIS2_PLACEMENT_3D('',#222993,#128094,#128095);
#105714=AXIS2_PLACEMENT_3D('',#222995,#128096,#128097);
#105715=AXIS2_PLACEMENT_3D('',#222997,#128098,#128099);
#105716=AXIS2_PLACEMENT_3D('',#222999,#128101,#128102);
#105717=AXIS2_PLACEMENT_3D('',#223003,#128104,#128105);
#105718=AXIS2_PLACEMENT_3D('',#223005,#128107,#128108);
#105719=AXIS2_PLACEMENT_3D('',#223006,#128109,#128110);
#105720=AXIS2_PLACEMENT_3D('',#223007,#128111,#128112);
#105721=AXIS2_PLACEMENT_3D('',#223008,#128113,#128114);
#105722=AXIS2_PLACEMENT_3D('',#223009,#128115,#128116);
#105723=AXIS2_PLACEMENT_3D('',#223010,#128117,#128118);
#105724=AXIS2_PLACEMENT_3D('',#223011,#128119,#128120);
#105725=AXIS2_PLACEMENT_3D('',#223012,#128121,#128122);
#105726=AXIS2_PLACEMENT_3D('',#223013,#128123,#128124);
#105727=AXIS2_PLACEMENT_3D('',#223014,#128125,#128126);
#105728=AXIS2_PLACEMENT_3D('',#223015,#128127,#128128);
#105729=AXIS2_PLACEMENT_3D('',#223016,#128129,#128130);
#105730=AXIS2_PLACEMENT_3D('',#223017,#128131,#128132);
#105731=AXIS2_PLACEMENT_3D('',#223020,#128133,#128134);
#105732=AXIS2_PLACEMENT_3D('',#223024,#128136,#128137);
#105733=AXIS2_PLACEMENT_3D('',#223026,#128138,#128139);
#105734=AXIS2_PLACEMENT_3D('',#223028,#128140,#128141);
#105735=AXIS2_PLACEMENT_3D('',#223030,#128143,#128144);
#105736=AXIS2_PLACEMENT_3D('',#223034,#128146,#128147);
#105737=AXIS2_PLACEMENT_3D('',#223036,#128149,#128150);
#105738=AXIS2_PLACEMENT_3D('',#223039,#128151,#128152);
#105739=AXIS2_PLACEMENT_3D('',#223043,#128154,#128155);
#105740=AXIS2_PLACEMENT_3D('',#223045,#128157,#128158);
#105741=AXIS2_PLACEMENT_3D('',#223048,#128159,#128160);
#105742=AXIS2_PLACEMENT_3D('',#223052,#128162,#128163);
#105743=AXIS2_PLACEMENT_3D('',#223054,#128164,#128165);
#105744=AXIS2_PLACEMENT_3D('',#223056,#128166,#128167);
#105745=AXIS2_PLACEMENT_3D('',#223058,#128169,#128170);
#105746=AXIS2_PLACEMENT_3D('',#223062,#128172,#128173);
#105747=AXIS2_PLACEMENT_3D('',#223064,#128175,#128176);
#105748=AXIS2_PLACEMENT_3D('',#223065,#128177,#128178);
#105749=AXIS2_PLACEMENT_3D('',#223066,#128179,#128180);
#105750=AXIS2_PLACEMENT_3D('',#223067,#128181,#128182);
#105751=AXIS2_PLACEMENT_3D('',#223068,#128183,#128184);
#105752=AXIS2_PLACEMENT_3D('',#223069,#128185,#128186);
#105753=AXIS2_PLACEMENT_3D('',#223070,#128187,#128188);
#105754=AXIS2_PLACEMENT_3D('',#223071,#128189,#128190);
#105755=AXIS2_PLACEMENT_3D('',#223072,#128191,#128192);
#105756=AXIS2_PLACEMENT_3D('',#223073,#128193,#128194);
#105757=AXIS2_PLACEMENT_3D('',#223074,#128195,#128196);
#105758=AXIS2_PLACEMENT_3D('',#223075,#128197,#128198);
#105759=AXIS2_PLACEMENT_3D('',#223076,#128199,#128200);
#105760=AXIS2_PLACEMENT_3D('',#223079,#128201,#128202);
#105761=AXIS2_PLACEMENT_3D('',#223083,#128204,#128205);
#105762=AXIS2_PLACEMENT_3D('',#223085,#128206,#128207);
#105763=AXIS2_PLACEMENT_3D('',#223087,#128208,#128209);
#105764=AXIS2_PLACEMENT_3D('',#223089,#128211,#128212);
#105765=AXIS2_PLACEMENT_3D('',#223093,#128214,#128215);
#105766=AXIS2_PLACEMENT_3D('',#223095,#128217,#128218);
#105767=AXIS2_PLACEMENT_3D('',#223098,#128219,#128220);
#105768=AXIS2_PLACEMENT_3D('',#223102,#128222,#128223);
#105769=AXIS2_PLACEMENT_3D('',#223104,#128225,#128226);
#105770=AXIS2_PLACEMENT_3D('',#223107,#128227,#128228);
#105771=AXIS2_PLACEMENT_3D('',#223111,#128230,#128231);
#105772=AXIS2_PLACEMENT_3D('',#223113,#128232,#128233);
#105773=AXIS2_PLACEMENT_3D('',#223115,#128234,#128235);
#105774=AXIS2_PLACEMENT_3D('',#223117,#128237,#128238);
#105775=AXIS2_PLACEMENT_3D('',#223121,#128240,#128241);
#105776=AXIS2_PLACEMENT_3D('',#223123,#128243,#128244);
#105777=AXIS2_PLACEMENT_3D('',#223124,#128245,#128246);
#105778=AXIS2_PLACEMENT_3D('',#223125,#128247,#128248);
#105779=AXIS2_PLACEMENT_3D('',#223126,#128249,#128250);
#105780=AXIS2_PLACEMENT_3D('',#223127,#128251,#128252);
#105781=AXIS2_PLACEMENT_3D('',#223128,#128253,#128254);
#105782=AXIS2_PLACEMENT_3D('',#223129,#128255,#128256);
#105783=AXIS2_PLACEMENT_3D('',#223130,#128257,#128258);
#105784=AXIS2_PLACEMENT_3D('',#223131,#128259,#128260);
#105785=AXIS2_PLACEMENT_3D('',#223132,#128261,#128262);
#105786=AXIS2_PLACEMENT_3D('',#223133,#128263,#128264);
#105787=AXIS2_PLACEMENT_3D('',#223134,#128265,#128266);
#105788=AXIS2_PLACEMENT_3D('',#223135,#128267,#128268);
#105789=AXIS2_PLACEMENT_3D('',#223138,#128269,#128270);
#105790=AXIS2_PLACEMENT_3D('',#223142,#128272,#128273);
#105791=AXIS2_PLACEMENT_3D('',#223144,#128274,#128275);
#105792=AXIS2_PLACEMENT_3D('',#223146,#128276,#128277);
#105793=AXIS2_PLACEMENT_3D('',#223148,#128279,#128280);
#105794=AXIS2_PLACEMENT_3D('',#223152,#128282,#128283);
#105795=AXIS2_PLACEMENT_3D('',#223154,#128285,#128286);
#105796=AXIS2_PLACEMENT_3D('',#223157,#128287,#128288);
#105797=AXIS2_PLACEMENT_3D('',#223161,#128290,#128291);
#105798=AXIS2_PLACEMENT_3D('',#223163,#128293,#128294);
#105799=AXIS2_PLACEMENT_3D('',#223166,#128295,#128296);
#105800=AXIS2_PLACEMENT_3D('',#223170,#128298,#128299);
#105801=AXIS2_PLACEMENT_3D('',#223172,#128300,#128301);
#105802=AXIS2_PLACEMENT_3D('',#223174,#128302,#128303);
#105803=AXIS2_PLACEMENT_3D('',#223176,#128305,#128306);
#105804=AXIS2_PLACEMENT_3D('',#223180,#128308,#128309);
#105805=AXIS2_PLACEMENT_3D('',#223182,#128311,#128312);
#105806=AXIS2_PLACEMENT_3D('',#223183,#128313,#128314);
#105807=AXIS2_PLACEMENT_3D('',#223184,#128315,#128316);
#105808=AXIS2_PLACEMENT_3D('',#223185,#128317,#128318);
#105809=AXIS2_PLACEMENT_3D('',#223186,#128319,#128320);
#105810=AXIS2_PLACEMENT_3D('',#223187,#128321,#128322);
#105811=AXIS2_PLACEMENT_3D('',#223188,#128323,#128324);
#105812=AXIS2_PLACEMENT_3D('',#223189,#128325,#128326);
#105813=AXIS2_PLACEMENT_3D('',#223190,#128327,#128328);
#105814=AXIS2_PLACEMENT_3D('',#223191,#128329,#128330);
#105815=AXIS2_PLACEMENT_3D('',#223192,#128331,#128332);
#105816=AXIS2_PLACEMENT_3D('',#223193,#128333,#128334);
#105817=AXIS2_PLACEMENT_3D('',#223194,#128335,#128336);
#105818=AXIS2_PLACEMENT_3D('',#223197,#128337,#128338);
#105819=AXIS2_PLACEMENT_3D('',#223201,#128340,#128341);
#105820=AXIS2_PLACEMENT_3D('',#223203,#128342,#128343);
#105821=AXIS2_PLACEMENT_3D('',#223205,#128344,#128345);
#105822=AXIS2_PLACEMENT_3D('',#223207,#128347,#128348);
#105823=AXIS2_PLACEMENT_3D('',#223211,#128350,#128351);
#105824=AXIS2_PLACEMENT_3D('',#223213,#128353,#128354);
#105825=AXIS2_PLACEMENT_3D('',#223216,#128355,#128356);
#105826=AXIS2_PLACEMENT_3D('',#223220,#128358,#128359);
#105827=AXIS2_PLACEMENT_3D('',#223222,#128361,#128362);
#105828=AXIS2_PLACEMENT_3D('',#223225,#128363,#128364);
#105829=AXIS2_PLACEMENT_3D('',#223229,#128366,#128367);
#105830=AXIS2_PLACEMENT_3D('',#223231,#128368,#128369);
#105831=AXIS2_PLACEMENT_3D('',#223233,#128370,#128371);
#105832=AXIS2_PLACEMENT_3D('',#223235,#128373,#128374);
#105833=AXIS2_PLACEMENT_3D('',#223239,#128376,#128377);
#105834=AXIS2_PLACEMENT_3D('',#223241,#128379,#128380);
#105835=AXIS2_PLACEMENT_3D('',#223242,#128381,#128382);
#105836=AXIS2_PLACEMENT_3D('',#223243,#128383,#128384);
#105837=AXIS2_PLACEMENT_3D('',#223244,#128385,#128386);
#105838=AXIS2_PLACEMENT_3D('',#223245,#128387,#128388);
#105839=AXIS2_PLACEMENT_3D('',#223246,#128389,#128390);
#105840=AXIS2_PLACEMENT_3D('',#223247,#128391,#128392);
#105841=AXIS2_PLACEMENT_3D('',#223248,#128393,#128394);
#105842=AXIS2_PLACEMENT_3D('',#223249,#128395,#128396);
#105843=AXIS2_PLACEMENT_3D('',#223250,#128397,#128398);
#105844=AXIS2_PLACEMENT_3D('',#223251,#128399,#128400);
#105845=AXIS2_PLACEMENT_3D('',#223252,#128401,#128402);
#105846=AXIS2_PLACEMENT_3D('',#223253,#128403,#128404);
#105847=AXIS2_PLACEMENT_3D('',#223256,#128405,#128406);
#105848=AXIS2_PLACEMENT_3D('',#223260,#128408,#128409);
#105849=AXIS2_PLACEMENT_3D('',#223262,#128410,#128411);
#105850=AXIS2_PLACEMENT_3D('',#223264,#128412,#128413);
#105851=AXIS2_PLACEMENT_3D('',#223266,#128415,#128416);
#105852=AXIS2_PLACEMENT_3D('',#223270,#128418,#128419);
#105853=AXIS2_PLACEMENT_3D('',#223272,#128421,#128422);
#105854=AXIS2_PLACEMENT_3D('',#223275,#128423,#128424);
#105855=AXIS2_PLACEMENT_3D('',#223279,#128426,#128427);
#105856=AXIS2_PLACEMENT_3D('',#223281,#128429,#128430);
#105857=AXIS2_PLACEMENT_3D('',#223284,#128431,#128432);
#105858=AXIS2_PLACEMENT_3D('',#223288,#128434,#128435);
#105859=AXIS2_PLACEMENT_3D('',#223290,#128436,#128437);
#105860=AXIS2_PLACEMENT_3D('',#223292,#128438,#128439);
#105861=AXIS2_PLACEMENT_3D('',#223294,#128441,#128442);
#105862=AXIS2_PLACEMENT_3D('',#223298,#128444,#128445);
#105863=AXIS2_PLACEMENT_3D('',#223300,#128447,#128448);
#105864=AXIS2_PLACEMENT_3D('',#223301,#128449,#128450);
#105865=AXIS2_PLACEMENT_3D('',#223302,#128451,#128452);
#105866=AXIS2_PLACEMENT_3D('',#223303,#128453,#128454);
#105867=AXIS2_PLACEMENT_3D('',#223304,#128455,#128456);
#105868=AXIS2_PLACEMENT_3D('',#223305,#128457,#128458);
#105869=AXIS2_PLACEMENT_3D('',#223306,#128459,#128460);
#105870=AXIS2_PLACEMENT_3D('',#223307,#128461,#128462);
#105871=AXIS2_PLACEMENT_3D('',#223308,#128463,#128464);
#105872=AXIS2_PLACEMENT_3D('',#223309,#128465,#128466);
#105873=AXIS2_PLACEMENT_3D('',#223310,#128467,#128468);
#105874=AXIS2_PLACEMENT_3D('',#223311,#128469,#128470);
#105875=AXIS2_PLACEMENT_3D('',#223312,#128471,#128472);
#105876=AXIS2_PLACEMENT_3D('',#223315,#128473,#128474);
#105877=AXIS2_PLACEMENT_3D('',#223319,#128476,#128477);
#105878=AXIS2_PLACEMENT_3D('',#223321,#128478,#128479);
#105879=AXIS2_PLACEMENT_3D('',#223323,#128480,#128481);
#105880=AXIS2_PLACEMENT_3D('',#223325,#128483,#128484);
#105881=AXIS2_PLACEMENT_3D('',#223329,#128486,#128487);
#105882=AXIS2_PLACEMENT_3D('',#223331,#128489,#128490);
#105883=AXIS2_PLACEMENT_3D('',#223334,#128491,#128492);
#105884=AXIS2_PLACEMENT_3D('',#223338,#128494,#128495);
#105885=AXIS2_PLACEMENT_3D('',#223340,#128497,#128498);
#105886=AXIS2_PLACEMENT_3D('',#223343,#128499,#128500);
#105887=AXIS2_PLACEMENT_3D('',#223347,#128502,#128503);
#105888=AXIS2_PLACEMENT_3D('',#223349,#128504,#128505);
#105889=AXIS2_PLACEMENT_3D('',#223351,#128506,#128507);
#105890=AXIS2_PLACEMENT_3D('',#223353,#128509,#128510);
#105891=AXIS2_PLACEMENT_3D('',#223357,#128512,#128513);
#105892=AXIS2_PLACEMENT_3D('',#223359,#128515,#128516);
#105893=AXIS2_PLACEMENT_3D('',#223360,#128517,#128518);
#105894=AXIS2_PLACEMENT_3D('',#223361,#128519,#128520);
#105895=AXIS2_PLACEMENT_3D('',#223362,#128521,#128522);
#105896=AXIS2_PLACEMENT_3D('',#223363,#128523,#128524);
#105897=AXIS2_PLACEMENT_3D('',#223364,#128525,#128526);
#105898=AXIS2_PLACEMENT_3D('',#223365,#128527,#128528);
#105899=AXIS2_PLACEMENT_3D('',#223366,#128529,#128530);
#105900=AXIS2_PLACEMENT_3D('',#223367,#128531,#128532);
#105901=AXIS2_PLACEMENT_3D('',#223368,#128533,#128534);
#105902=AXIS2_PLACEMENT_3D('',#223369,#128535,#128536);
#105903=AXIS2_PLACEMENT_3D('',#223370,#128537,#128538);
#105904=AXIS2_PLACEMENT_3D('',#223371,#128539,#128540);
#105905=AXIS2_PLACEMENT_3D('',#223374,#128541,#128542);
#105906=AXIS2_PLACEMENT_3D('',#223378,#128544,#128545);
#105907=AXIS2_PLACEMENT_3D('',#223380,#128546,#128547);
#105908=AXIS2_PLACEMENT_3D('',#223382,#128548,#128549);
#105909=AXIS2_PLACEMENT_3D('',#223384,#128551,#128552);
#105910=AXIS2_PLACEMENT_3D('',#223388,#128554,#128555);
#105911=AXIS2_PLACEMENT_3D('',#223390,#128557,#128558);
#105912=AXIS2_PLACEMENT_3D('',#223393,#128559,#128560);
#105913=AXIS2_PLACEMENT_3D('',#223397,#128562,#128563);
#105914=AXIS2_PLACEMENT_3D('',#223399,#128565,#128566);
#105915=AXIS2_PLACEMENT_3D('',#223402,#128567,#128568);
#105916=AXIS2_PLACEMENT_3D('',#223406,#128570,#128571);
#105917=AXIS2_PLACEMENT_3D('',#223408,#128572,#128573);
#105918=AXIS2_PLACEMENT_3D('',#223410,#128574,#128575);
#105919=AXIS2_PLACEMENT_3D('',#223412,#128577,#128578);
#105920=AXIS2_PLACEMENT_3D('',#223416,#128580,#128581);
#105921=AXIS2_PLACEMENT_3D('',#223418,#128583,#128584);
#105922=AXIS2_PLACEMENT_3D('',#223419,#128585,#128586);
#105923=AXIS2_PLACEMENT_3D('',#223420,#128587,#128588);
#105924=AXIS2_PLACEMENT_3D('',#223421,#128589,#128590);
#105925=AXIS2_PLACEMENT_3D('',#223422,#128591,#128592);
#105926=AXIS2_PLACEMENT_3D('',#223423,#128593,#128594);
#105927=AXIS2_PLACEMENT_3D('',#223424,#128595,#128596);
#105928=AXIS2_PLACEMENT_3D('',#223425,#128597,#128598);
#105929=AXIS2_PLACEMENT_3D('',#223426,#128599,#128600);
#105930=AXIS2_PLACEMENT_3D('',#223427,#128601,#128602);
#105931=AXIS2_PLACEMENT_3D('',#223428,#128603,#128604);
#105932=AXIS2_PLACEMENT_3D('',#223429,#128605,#128606);
#105933=AXIS2_PLACEMENT_3D('',#223430,#128607,#128608);
#105934=AXIS2_PLACEMENT_3D('',#223433,#128609,#128610);
#105935=AXIS2_PLACEMENT_3D('',#223437,#128612,#128613);
#105936=AXIS2_PLACEMENT_3D('',#223439,#128614,#128615);
#105937=AXIS2_PLACEMENT_3D('',#223441,#128616,#128617);
#105938=AXIS2_PLACEMENT_3D('',#223443,#128619,#128620);
#105939=AXIS2_PLACEMENT_3D('',#223447,#128622,#128623);
#105940=AXIS2_PLACEMENT_3D('',#223449,#128625,#128626);
#105941=AXIS2_PLACEMENT_3D('',#223452,#128627,#128628);
#105942=AXIS2_PLACEMENT_3D('',#223456,#128630,#128631);
#105943=AXIS2_PLACEMENT_3D('',#223458,#128633,#128634);
#105944=AXIS2_PLACEMENT_3D('',#223461,#128635,#128636);
#105945=AXIS2_PLACEMENT_3D('',#223465,#128638,#128639);
#105946=AXIS2_PLACEMENT_3D('',#223467,#128640,#128641);
#105947=AXIS2_PLACEMENT_3D('',#223469,#128642,#128643);
#105948=AXIS2_PLACEMENT_3D('',#223471,#128645,#128646);
#105949=AXIS2_PLACEMENT_3D('',#223475,#128648,#128649);
#105950=AXIS2_PLACEMENT_3D('',#223477,#128651,#128652);
#105951=AXIS2_PLACEMENT_3D('',#223478,#128653,#128654);
#105952=AXIS2_PLACEMENT_3D('',#223479,#128655,#128656);
#105953=AXIS2_PLACEMENT_3D('',#223480,#128657,#128658);
#105954=AXIS2_PLACEMENT_3D('',#223481,#128659,#128660);
#105955=AXIS2_PLACEMENT_3D('',#223482,#128661,#128662);
#105956=AXIS2_PLACEMENT_3D('',#223483,#128663,#128664);
#105957=AXIS2_PLACEMENT_3D('',#223484,#128665,#128666);
#105958=AXIS2_PLACEMENT_3D('',#223485,#128667,#128668);
#105959=AXIS2_PLACEMENT_3D('',#223486,#128669,#128670);
#105960=AXIS2_PLACEMENT_3D('',#223487,#128671,#128672);
#105961=AXIS2_PLACEMENT_3D('',#223488,#128673,#128674);
#105962=AXIS2_PLACEMENT_3D('',#223489,#128675,#128676);
#105963=AXIS2_PLACEMENT_3D('',#223492,#128677,#128678);
#105964=AXIS2_PLACEMENT_3D('',#223496,#128680,#128681);
#105965=AXIS2_PLACEMENT_3D('',#223498,#128682,#128683);
#105966=AXIS2_PLACEMENT_3D('',#223500,#128684,#128685);
#105967=AXIS2_PLACEMENT_3D('',#223502,#128687,#128688);
#105968=AXIS2_PLACEMENT_3D('',#223506,#128690,#128691);
#105969=AXIS2_PLACEMENT_3D('',#223508,#128693,#128694);
#105970=AXIS2_PLACEMENT_3D('',#223511,#128695,#128696);
#105971=AXIS2_PLACEMENT_3D('',#223515,#128698,#128699);
#105972=AXIS2_PLACEMENT_3D('',#223517,#128701,#128702);
#105973=AXIS2_PLACEMENT_3D('',#223520,#128703,#128704);
#105974=AXIS2_PLACEMENT_3D('',#223524,#128706,#128707);
#105975=AXIS2_PLACEMENT_3D('',#223526,#128708,#128709);
#105976=AXIS2_PLACEMENT_3D('',#223528,#128710,#128711);
#105977=AXIS2_PLACEMENT_3D('',#223530,#128713,#128714);
#105978=AXIS2_PLACEMENT_3D('',#223534,#128716,#128717);
#105979=AXIS2_PLACEMENT_3D('',#223536,#128719,#128720);
#105980=AXIS2_PLACEMENT_3D('',#223537,#128721,#128722);
#105981=AXIS2_PLACEMENT_3D('',#223538,#128723,#128724);
#105982=AXIS2_PLACEMENT_3D('',#223539,#128725,#128726);
#105983=AXIS2_PLACEMENT_3D('',#223540,#128727,#128728);
#105984=AXIS2_PLACEMENT_3D('',#223541,#128729,#128730);
#105985=AXIS2_PLACEMENT_3D('',#223542,#128731,#128732);
#105986=AXIS2_PLACEMENT_3D('',#223543,#128733,#128734);
#105987=AXIS2_PLACEMENT_3D('',#223544,#128735,#128736);
#105988=AXIS2_PLACEMENT_3D('',#223545,#128737,#128738);
#105989=AXIS2_PLACEMENT_3D('',#223546,#128739,#128740);
#105990=AXIS2_PLACEMENT_3D('',#223547,#128741,#128742);
#105991=AXIS2_PLACEMENT_3D('',#223548,#128743,#128744);
#105992=AXIS2_PLACEMENT_3D('',#223551,#128745,#128746);
#105993=AXIS2_PLACEMENT_3D('',#223555,#128748,#128749);
#105994=AXIS2_PLACEMENT_3D('',#223557,#128750,#128751);
#105995=AXIS2_PLACEMENT_3D('',#223559,#128752,#128753);
#105996=AXIS2_PLACEMENT_3D('',#223561,#128755,#128756);
#105997=AXIS2_PLACEMENT_3D('',#223565,#128758,#128759);
#105998=AXIS2_PLACEMENT_3D('',#223567,#128761,#128762);
#105999=AXIS2_PLACEMENT_3D('',#223570,#128763,#128764);
#106000=AXIS2_PLACEMENT_3D('',#223574,#128766,#128767);
#106001=AXIS2_PLACEMENT_3D('',#223576,#128769,#128770);
#106002=AXIS2_PLACEMENT_3D('',#223579,#128771,#128772);
#106003=AXIS2_PLACEMENT_3D('',#223583,#128774,#128775);
#106004=AXIS2_PLACEMENT_3D('',#223585,#128776,#128777);
#106005=AXIS2_PLACEMENT_3D('',#223587,#128778,#128779);
#106006=AXIS2_PLACEMENT_3D('',#223589,#128781,#128782);
#106007=AXIS2_PLACEMENT_3D('',#223593,#128784,#128785);
#106008=AXIS2_PLACEMENT_3D('',#223595,#128787,#128788);
#106009=AXIS2_PLACEMENT_3D('',#223596,#128789,#128790);
#106010=AXIS2_PLACEMENT_3D('',#223597,#128791,#128792);
#106011=AXIS2_PLACEMENT_3D('',#223598,#128793,#128794);
#106012=AXIS2_PLACEMENT_3D('',#223599,#128795,#128796);
#106013=AXIS2_PLACEMENT_3D('',#223600,#128797,#128798);
#106014=AXIS2_PLACEMENT_3D('',#223601,#128799,#128800);
#106015=AXIS2_PLACEMENT_3D('',#223602,#128801,#128802);
#106016=AXIS2_PLACEMENT_3D('',#223603,#128803,#128804);
#106017=AXIS2_PLACEMENT_3D('',#223604,#128805,#128806);
#106018=AXIS2_PLACEMENT_3D('',#223605,#128807,#128808);
#106019=AXIS2_PLACEMENT_3D('',#223606,#128809,#128810);
#106020=AXIS2_PLACEMENT_3D('',#223607,#128811,#128812);
#106021=AXIS2_PLACEMENT_3D('',#223610,#128813,#128814);
#106022=AXIS2_PLACEMENT_3D('',#223614,#128816,#128817);
#106023=AXIS2_PLACEMENT_3D('',#223616,#128818,#128819);
#106024=AXIS2_PLACEMENT_3D('',#223618,#128820,#128821);
#106025=AXIS2_PLACEMENT_3D('',#223620,#128823,#128824);
#106026=AXIS2_PLACEMENT_3D('',#223624,#128826,#128827);
#106027=AXIS2_PLACEMENT_3D('',#223626,#128829,#128830);
#106028=AXIS2_PLACEMENT_3D('',#223629,#128831,#128832);
#106029=AXIS2_PLACEMENT_3D('',#223633,#128834,#128835);
#106030=AXIS2_PLACEMENT_3D('',#223635,#128837,#128838);
#106031=AXIS2_PLACEMENT_3D('',#223638,#128839,#128840);
#106032=AXIS2_PLACEMENT_3D('',#223642,#128842,#128843);
#106033=AXIS2_PLACEMENT_3D('',#223644,#128844,#128845);
#106034=AXIS2_PLACEMENT_3D('',#223646,#128846,#128847);
#106035=AXIS2_PLACEMENT_3D('',#223648,#128849,#128850);
#106036=AXIS2_PLACEMENT_3D('',#223652,#128852,#128853);
#106037=AXIS2_PLACEMENT_3D('',#223654,#128855,#128856);
#106038=AXIS2_PLACEMENT_3D('',#223655,#128857,#128858);
#106039=AXIS2_PLACEMENT_3D('',#223656,#128859,#128860);
#106040=AXIS2_PLACEMENT_3D('',#223657,#128861,#128862);
#106041=AXIS2_PLACEMENT_3D('',#223658,#128863,#128864);
#106042=AXIS2_PLACEMENT_3D('',#223659,#128865,#128866);
#106043=AXIS2_PLACEMENT_3D('',#223660,#128867,#128868);
#106044=AXIS2_PLACEMENT_3D('',#223661,#128869,#128870);
#106045=AXIS2_PLACEMENT_3D('',#223662,#128871,#128872);
#106046=AXIS2_PLACEMENT_3D('',#223663,#128873,#128874);
#106047=AXIS2_PLACEMENT_3D('',#223664,#128875,#128876);
#106048=AXIS2_PLACEMENT_3D('',#223665,#128877,#128878);
#106049=AXIS2_PLACEMENT_3D('',#223666,#128879,#128880);
#106050=AXIS2_PLACEMENT_3D('',#223669,#128881,#128882);
#106051=AXIS2_PLACEMENT_3D('',#223673,#128884,#128885);
#106052=AXIS2_PLACEMENT_3D('',#223675,#128886,#128887);
#106053=AXIS2_PLACEMENT_3D('',#223677,#128888,#128889);
#106054=AXIS2_PLACEMENT_3D('',#223679,#128891,#128892);
#106055=AXIS2_PLACEMENT_3D('',#223683,#128894,#128895);
#106056=AXIS2_PLACEMENT_3D('',#223685,#128897,#128898);
#106057=AXIS2_PLACEMENT_3D('',#223688,#128899,#128900);
#106058=AXIS2_PLACEMENT_3D('',#223692,#128902,#128903);
#106059=AXIS2_PLACEMENT_3D('',#223694,#128905,#128906);
#106060=AXIS2_PLACEMENT_3D('',#223697,#128907,#128908);
#106061=AXIS2_PLACEMENT_3D('',#223701,#128910,#128911);
#106062=AXIS2_PLACEMENT_3D('',#223703,#128912,#128913);
#106063=AXIS2_PLACEMENT_3D('',#223705,#128914,#128915);
#106064=AXIS2_PLACEMENT_3D('',#223707,#128917,#128918);
#106065=AXIS2_PLACEMENT_3D('',#223711,#128920,#128921);
#106066=AXIS2_PLACEMENT_3D('',#223713,#128923,#128924);
#106067=AXIS2_PLACEMENT_3D('',#223714,#128925,#128926);
#106068=AXIS2_PLACEMENT_3D('',#223715,#128927,#128928);
#106069=AXIS2_PLACEMENT_3D('',#223716,#128929,#128930);
#106070=AXIS2_PLACEMENT_3D('',#223717,#128931,#128932);
#106071=AXIS2_PLACEMENT_3D('',#223718,#128933,#128934);
#106072=AXIS2_PLACEMENT_3D('',#223719,#128935,#128936);
#106073=AXIS2_PLACEMENT_3D('',#223720,#128937,#128938);
#106074=AXIS2_PLACEMENT_3D('',#223721,#128939,#128940);
#106075=AXIS2_PLACEMENT_3D('',#223722,#128941,#128942);
#106076=AXIS2_PLACEMENT_3D('',#223723,#128943,#128944);
#106077=AXIS2_PLACEMENT_3D('',#223724,#128945,#128946);
#106078=AXIS2_PLACEMENT_3D('',#223725,#128947,#128948);
#106079=AXIS2_PLACEMENT_3D('',#223728,#128949,#128950);
#106080=AXIS2_PLACEMENT_3D('',#223732,#128952,#128953);
#106081=AXIS2_PLACEMENT_3D('',#223734,#128954,#128955);
#106082=AXIS2_PLACEMENT_3D('',#223736,#128956,#128957);
#106083=AXIS2_PLACEMENT_3D('',#223738,#128959,#128960);
#106084=AXIS2_PLACEMENT_3D('',#223742,#128962,#128963);
#106085=AXIS2_PLACEMENT_3D('',#223744,#128965,#128966);
#106086=AXIS2_PLACEMENT_3D('',#223747,#128967,#128968);
#106087=AXIS2_PLACEMENT_3D('',#223751,#128970,#128971);
#106088=AXIS2_PLACEMENT_3D('',#223753,#128973,#128974);
#106089=AXIS2_PLACEMENT_3D('',#223756,#128975,#128976);
#106090=AXIS2_PLACEMENT_3D('',#223760,#128978,#128979);
#106091=AXIS2_PLACEMENT_3D('',#223762,#128980,#128981);
#106092=AXIS2_PLACEMENT_3D('',#223764,#128982,#128983);
#106093=AXIS2_PLACEMENT_3D('',#223766,#128985,#128986);
#106094=AXIS2_PLACEMENT_3D('',#223770,#128988,#128989);
#106095=AXIS2_PLACEMENT_3D('',#223772,#128991,#128992);
#106096=AXIS2_PLACEMENT_3D('',#223773,#128993,#128994);
#106097=AXIS2_PLACEMENT_3D('',#223774,#128995,#128996);
#106098=AXIS2_PLACEMENT_3D('',#223775,#128997,#128998);
#106099=AXIS2_PLACEMENT_3D('',#223776,#128999,#129000);
#106100=AXIS2_PLACEMENT_3D('',#223777,#129001,#129002);
#106101=AXIS2_PLACEMENT_3D('',#223778,#129003,#129004);
#106102=AXIS2_PLACEMENT_3D('',#223779,#129005,#129006);
#106103=AXIS2_PLACEMENT_3D('',#223780,#129007,#129008);
#106104=AXIS2_PLACEMENT_3D('',#223781,#129009,#129010);
#106105=AXIS2_PLACEMENT_3D('',#223782,#129011,#129012);
#106106=AXIS2_PLACEMENT_3D('',#223783,#129013,#129014);
#106107=AXIS2_PLACEMENT_3D('',#223784,#129015,#129016);
#106108=AXIS2_PLACEMENT_3D('',#223787,#129017,#129018);
#106109=AXIS2_PLACEMENT_3D('',#223791,#129020,#129021);
#106110=AXIS2_PLACEMENT_3D('',#223793,#129022,#129023);
#106111=AXIS2_PLACEMENT_3D('',#223795,#129024,#129025);
#106112=AXIS2_PLACEMENT_3D('',#223797,#129027,#129028);
#106113=AXIS2_PLACEMENT_3D('',#223801,#129030,#129031);
#106114=AXIS2_PLACEMENT_3D('',#223803,#129033,#129034);
#106115=AXIS2_PLACEMENT_3D('',#223806,#129035,#129036);
#106116=AXIS2_PLACEMENT_3D('',#223810,#129038,#129039);
#106117=AXIS2_PLACEMENT_3D('',#223812,#129041,#129042);
#106118=AXIS2_PLACEMENT_3D('',#223815,#129043,#129044);
#106119=AXIS2_PLACEMENT_3D('',#223819,#129046,#129047);
#106120=AXIS2_PLACEMENT_3D('',#223821,#129048,#129049);
#106121=AXIS2_PLACEMENT_3D('',#223823,#129050,#129051);
#106122=AXIS2_PLACEMENT_3D('',#223825,#129053,#129054);
#106123=AXIS2_PLACEMENT_3D('',#223829,#129056,#129057);
#106124=AXIS2_PLACEMENT_3D('',#223831,#129059,#129060);
#106125=AXIS2_PLACEMENT_3D('',#223832,#129061,#129062);
#106126=AXIS2_PLACEMENT_3D('',#223833,#129063,#129064);
#106127=AXIS2_PLACEMENT_3D('',#223834,#129065,#129066);
#106128=AXIS2_PLACEMENT_3D('',#223835,#129067,#129068);
#106129=AXIS2_PLACEMENT_3D('',#223836,#129069,#129070);
#106130=AXIS2_PLACEMENT_3D('',#223837,#129071,#129072);
#106131=AXIS2_PLACEMENT_3D('',#223838,#129073,#129074);
#106132=AXIS2_PLACEMENT_3D('',#223839,#129075,#129076);
#106133=AXIS2_PLACEMENT_3D('',#223840,#129077,#129078);
#106134=AXIS2_PLACEMENT_3D('',#223841,#129079,#129080);
#106135=AXIS2_PLACEMENT_3D('',#223842,#129081,#129082);
#106136=AXIS2_PLACEMENT_3D('',#223843,#129083,#129084);
#106137=AXIS2_PLACEMENT_3D('',#223846,#129085,#129086);
#106138=AXIS2_PLACEMENT_3D('',#223850,#129088,#129089);
#106139=AXIS2_PLACEMENT_3D('',#223852,#129090,#129091);
#106140=AXIS2_PLACEMENT_3D('',#223854,#129092,#129093);
#106141=AXIS2_PLACEMENT_3D('',#223856,#129095,#129096);
#106142=AXIS2_PLACEMENT_3D('',#223860,#129098,#129099);
#106143=AXIS2_PLACEMENT_3D('',#223862,#129101,#129102);
#106144=AXIS2_PLACEMENT_3D('',#223865,#129103,#129104);
#106145=AXIS2_PLACEMENT_3D('',#223869,#129106,#129107);
#106146=AXIS2_PLACEMENT_3D('',#223871,#129109,#129110);
#106147=AXIS2_PLACEMENT_3D('',#223874,#129111,#129112);
#106148=AXIS2_PLACEMENT_3D('',#223878,#129114,#129115);
#106149=AXIS2_PLACEMENT_3D('',#223880,#129116,#129117);
#106150=AXIS2_PLACEMENT_3D('',#223882,#129118,#129119);
#106151=AXIS2_PLACEMENT_3D('',#223884,#129121,#129122);
#106152=AXIS2_PLACEMENT_3D('',#223888,#129124,#129125);
#106153=AXIS2_PLACEMENT_3D('',#223890,#129127,#129128);
#106154=AXIS2_PLACEMENT_3D('',#223891,#129129,#129130);
#106155=AXIS2_PLACEMENT_3D('',#223892,#129131,#129132);
#106156=AXIS2_PLACEMENT_3D('',#223893,#129133,#129134);
#106157=AXIS2_PLACEMENT_3D('',#223894,#129135,#129136);
#106158=AXIS2_PLACEMENT_3D('',#223895,#129137,#129138);
#106159=AXIS2_PLACEMENT_3D('',#223896,#129139,#129140);
#106160=AXIS2_PLACEMENT_3D('',#223897,#129141,#129142);
#106161=AXIS2_PLACEMENT_3D('',#223898,#129143,#129144);
#106162=AXIS2_PLACEMENT_3D('',#223899,#129145,#129146);
#106163=AXIS2_PLACEMENT_3D('',#223900,#129147,#129148);
#106164=AXIS2_PLACEMENT_3D('',#223901,#129149,#129150);
#106165=AXIS2_PLACEMENT_3D('',#223902,#129151,#129152);
#106166=AXIS2_PLACEMENT_3D('',#223905,#129153,#129154);
#106167=AXIS2_PLACEMENT_3D('',#223909,#129156,#129157);
#106168=AXIS2_PLACEMENT_3D('',#223911,#129158,#129159);
#106169=AXIS2_PLACEMENT_3D('',#223913,#129160,#129161);
#106170=AXIS2_PLACEMENT_3D('',#223915,#129163,#129164);
#106171=AXIS2_PLACEMENT_3D('',#223919,#129166,#129167);
#106172=AXIS2_PLACEMENT_3D('',#223921,#129169,#129170);
#106173=AXIS2_PLACEMENT_3D('',#223924,#129171,#129172);
#106174=AXIS2_PLACEMENT_3D('',#223928,#129174,#129175);
#106175=AXIS2_PLACEMENT_3D('',#223930,#129177,#129178);
#106176=AXIS2_PLACEMENT_3D('',#223933,#129179,#129180);
#106177=AXIS2_PLACEMENT_3D('',#223937,#129182,#129183);
#106178=AXIS2_PLACEMENT_3D('',#223939,#129184,#129185);
#106179=AXIS2_PLACEMENT_3D('',#223941,#129186,#129187);
#106180=AXIS2_PLACEMENT_3D('',#223943,#129189,#129190);
#106181=AXIS2_PLACEMENT_3D('',#223947,#129192,#129193);
#106182=AXIS2_PLACEMENT_3D('',#223949,#129195,#129196);
#106183=AXIS2_PLACEMENT_3D('',#223950,#129197,#129198);
#106184=AXIS2_PLACEMENT_3D('',#223951,#129199,#129200);
#106185=AXIS2_PLACEMENT_3D('',#223952,#129201,#129202);
#106186=AXIS2_PLACEMENT_3D('',#223953,#129203,#129204);
#106187=AXIS2_PLACEMENT_3D('',#223954,#129205,#129206);
#106188=AXIS2_PLACEMENT_3D('',#223955,#129207,#129208);
#106189=AXIS2_PLACEMENT_3D('',#223956,#129209,#129210);
#106190=AXIS2_PLACEMENT_3D('',#223957,#129211,#129212);
#106191=AXIS2_PLACEMENT_3D('',#223958,#129213,#129214);
#106192=AXIS2_PLACEMENT_3D('',#223959,#129215,#129216);
#106193=AXIS2_PLACEMENT_3D('',#223960,#129217,#129218);
#106194=AXIS2_PLACEMENT_3D('',#223961,#129219,#129220);
#106195=AXIS2_PLACEMENT_3D('',#223964,#129221,#129222);
#106196=AXIS2_PLACEMENT_3D('',#223968,#129224,#129225);
#106197=AXIS2_PLACEMENT_3D('',#223970,#129226,#129227);
#106198=AXIS2_PLACEMENT_3D('',#223972,#129228,#129229);
#106199=AXIS2_PLACEMENT_3D('',#223974,#129231,#129232);
#106200=AXIS2_PLACEMENT_3D('',#223978,#129234,#129235);
#106201=AXIS2_PLACEMENT_3D('',#223980,#129237,#129238);
#106202=AXIS2_PLACEMENT_3D('',#223983,#129239,#129240);
#106203=AXIS2_PLACEMENT_3D('',#223987,#129242,#129243);
#106204=AXIS2_PLACEMENT_3D('',#223989,#129245,#129246);
#106205=AXIS2_PLACEMENT_3D('',#223992,#129247,#129248);
#106206=AXIS2_PLACEMENT_3D('',#223996,#129250,#129251);
#106207=AXIS2_PLACEMENT_3D('',#223998,#129252,#129253);
#106208=AXIS2_PLACEMENT_3D('',#224000,#129254,#129255);
#106209=AXIS2_PLACEMENT_3D('',#224002,#129257,#129258);
#106210=AXIS2_PLACEMENT_3D('',#224006,#129260,#129261);
#106211=AXIS2_PLACEMENT_3D('',#224008,#129263,#129264);
#106212=AXIS2_PLACEMENT_3D('',#224009,#129265,#129266);
#106213=AXIS2_PLACEMENT_3D('',#224010,#129267,#129268);
#106214=AXIS2_PLACEMENT_3D('',#224011,#129269,#129270);
#106215=AXIS2_PLACEMENT_3D('',#224012,#129271,#129272);
#106216=AXIS2_PLACEMENT_3D('',#224013,#129273,#129274);
#106217=AXIS2_PLACEMENT_3D('',#224014,#129275,#129276);
#106218=AXIS2_PLACEMENT_3D('',#224015,#129277,#129278);
#106219=AXIS2_PLACEMENT_3D('',#224016,#129279,#129280);
#106220=AXIS2_PLACEMENT_3D('',#224017,#129281,#129282);
#106221=AXIS2_PLACEMENT_3D('',#224018,#129283,#129284);
#106222=AXIS2_PLACEMENT_3D('',#224019,#129285,#129286);
#106223=AXIS2_PLACEMENT_3D('',#224020,#129287,#129288);
#106224=AXIS2_PLACEMENT_3D('',#224023,#129289,#129290);
#106225=AXIS2_PLACEMENT_3D('',#224027,#129292,#129293);
#106226=AXIS2_PLACEMENT_3D('',#224029,#129294,#129295);
#106227=AXIS2_PLACEMENT_3D('',#224031,#129296,#129297);
#106228=AXIS2_PLACEMENT_3D('',#224033,#129299,#129300);
#106229=AXIS2_PLACEMENT_3D('',#224037,#129302,#129303);
#106230=AXIS2_PLACEMENT_3D('',#224039,#129305,#129306);
#106231=AXIS2_PLACEMENT_3D('',#224042,#129307,#129308);
#106232=AXIS2_PLACEMENT_3D('',#224046,#129310,#129311);
#106233=AXIS2_PLACEMENT_3D('',#224048,#129313,#129314);
#106234=AXIS2_PLACEMENT_3D('',#224051,#129315,#129316);
#106235=AXIS2_PLACEMENT_3D('',#224055,#129318,#129319);
#106236=AXIS2_PLACEMENT_3D('',#224057,#129320,#129321);
#106237=AXIS2_PLACEMENT_3D('',#224059,#129322,#129323);
#106238=AXIS2_PLACEMENT_3D('',#224061,#129325,#129326);
#106239=AXIS2_PLACEMENT_3D('',#224065,#129328,#129329);
#106240=AXIS2_PLACEMENT_3D('',#224067,#129331,#129332);
#106241=AXIS2_PLACEMENT_3D('',#224068,#129333,#129334);
#106242=AXIS2_PLACEMENT_3D('',#224069,#129335,#129336);
#106243=AXIS2_PLACEMENT_3D('',#224070,#129337,#129338);
#106244=AXIS2_PLACEMENT_3D('',#224071,#129339,#129340);
#106245=AXIS2_PLACEMENT_3D('',#224072,#129341,#129342);
#106246=AXIS2_PLACEMENT_3D('',#224073,#129343,#129344);
#106247=AXIS2_PLACEMENT_3D('',#224074,#129345,#129346);
#106248=AXIS2_PLACEMENT_3D('',#224075,#129347,#129348);
#106249=AXIS2_PLACEMENT_3D('',#224076,#129349,#129350);
#106250=AXIS2_PLACEMENT_3D('',#224077,#129351,#129352);
#106251=AXIS2_PLACEMENT_3D('',#224078,#129353,#129354);
#106252=AXIS2_PLACEMENT_3D('',#224079,#129355,#129356);
#106253=AXIS2_PLACEMENT_3D('',#224082,#129357,#129358);
#106254=AXIS2_PLACEMENT_3D('',#224086,#129360,#129361);
#106255=AXIS2_PLACEMENT_3D('',#224088,#129362,#129363);
#106256=AXIS2_PLACEMENT_3D('',#224090,#129364,#129365);
#106257=AXIS2_PLACEMENT_3D('',#224092,#129367,#129368);
#106258=AXIS2_PLACEMENT_3D('',#224096,#129370,#129371);
#106259=AXIS2_PLACEMENT_3D('',#224098,#129373,#129374);
#106260=AXIS2_PLACEMENT_3D('',#224101,#129375,#129376);
#106261=AXIS2_PLACEMENT_3D('',#224105,#129378,#129379);
#106262=AXIS2_PLACEMENT_3D('',#224107,#129381,#129382);
#106263=AXIS2_PLACEMENT_3D('',#224110,#129383,#129384);
#106264=AXIS2_PLACEMENT_3D('',#224114,#129386,#129387);
#106265=AXIS2_PLACEMENT_3D('',#224116,#129388,#129389);
#106266=AXIS2_PLACEMENT_3D('',#224118,#129390,#129391);
#106267=AXIS2_PLACEMENT_3D('',#224120,#129393,#129394);
#106268=AXIS2_PLACEMENT_3D('',#224124,#129396,#129397);
#106269=AXIS2_PLACEMENT_3D('',#224126,#129399,#129400);
#106270=AXIS2_PLACEMENT_3D('',#224127,#129401,#129402);
#106271=AXIS2_PLACEMENT_3D('',#224128,#129403,#129404);
#106272=AXIS2_PLACEMENT_3D('',#224129,#129405,#129406);
#106273=AXIS2_PLACEMENT_3D('',#224130,#129407,#129408);
#106274=AXIS2_PLACEMENT_3D('',#224131,#129409,#129410);
#106275=AXIS2_PLACEMENT_3D('',#224132,#129411,#129412);
#106276=AXIS2_PLACEMENT_3D('',#224133,#129413,#129414);
#106277=AXIS2_PLACEMENT_3D('',#224134,#129415,#129416);
#106278=AXIS2_PLACEMENT_3D('',#224135,#129417,#129418);
#106279=AXIS2_PLACEMENT_3D('',#224136,#129419,#129420);
#106280=AXIS2_PLACEMENT_3D('',#224137,#129421,#129422);
#106281=AXIS2_PLACEMENT_3D('',#224138,#129423,#129424);
#106282=AXIS2_PLACEMENT_3D('',#224141,#129425,#129426);
#106283=AXIS2_PLACEMENT_3D('',#224145,#129428,#129429);
#106284=AXIS2_PLACEMENT_3D('',#224147,#129430,#129431);
#106285=AXIS2_PLACEMENT_3D('',#224149,#129432,#129433);
#106286=AXIS2_PLACEMENT_3D('',#224151,#129435,#129436);
#106287=AXIS2_PLACEMENT_3D('',#224155,#129438,#129439);
#106288=AXIS2_PLACEMENT_3D('',#224157,#129441,#129442);
#106289=AXIS2_PLACEMENT_3D('',#224160,#129443,#129444);
#106290=AXIS2_PLACEMENT_3D('',#224164,#129446,#129447);
#106291=AXIS2_PLACEMENT_3D('',#224166,#129449,#129450);
#106292=AXIS2_PLACEMENT_3D('',#224169,#129451,#129452);
#106293=AXIS2_PLACEMENT_3D('',#224173,#129454,#129455);
#106294=AXIS2_PLACEMENT_3D('',#224175,#129456,#129457);
#106295=AXIS2_PLACEMENT_3D('',#224177,#129458,#129459);
#106296=AXIS2_PLACEMENT_3D('',#224179,#129461,#129462);
#106297=AXIS2_PLACEMENT_3D('',#224183,#129464,#129465);
#106298=AXIS2_PLACEMENT_3D('',#224185,#129467,#129468);
#106299=AXIS2_PLACEMENT_3D('',#224186,#129469,#129470);
#106300=AXIS2_PLACEMENT_3D('',#224187,#129471,#129472);
#106301=AXIS2_PLACEMENT_3D('',#224188,#129473,#129474);
#106302=AXIS2_PLACEMENT_3D('',#224189,#129475,#129476);
#106303=AXIS2_PLACEMENT_3D('',#224190,#129477,#129478);
#106304=AXIS2_PLACEMENT_3D('',#224191,#129479,#129480);
#106305=AXIS2_PLACEMENT_3D('',#224192,#129481,#129482);
#106306=AXIS2_PLACEMENT_3D('',#224193,#129483,#129484);
#106307=AXIS2_PLACEMENT_3D('',#224194,#129485,#129486);
#106308=AXIS2_PLACEMENT_3D('',#224195,#129487,#129488);
#106309=AXIS2_PLACEMENT_3D('',#224196,#129489,#129490);
#106310=AXIS2_PLACEMENT_3D('',#224197,#129491,#129492);
#106311=AXIS2_PLACEMENT_3D('',#224200,#129493,#129494);
#106312=AXIS2_PLACEMENT_3D('',#224204,#129496,#129497);
#106313=AXIS2_PLACEMENT_3D('',#224206,#129498,#129499);
#106314=AXIS2_PLACEMENT_3D('',#224208,#129500,#129501);
#106315=AXIS2_PLACEMENT_3D('',#224210,#129503,#129504);
#106316=AXIS2_PLACEMENT_3D('',#224214,#129506,#129507);
#106317=AXIS2_PLACEMENT_3D('',#224216,#129509,#129510);
#106318=AXIS2_PLACEMENT_3D('',#224219,#129511,#129512);
#106319=AXIS2_PLACEMENT_3D('',#224223,#129514,#129515);
#106320=AXIS2_PLACEMENT_3D('',#224225,#129517,#129518);
#106321=AXIS2_PLACEMENT_3D('',#224228,#129519,#129520);
#106322=AXIS2_PLACEMENT_3D('',#224232,#129522,#129523);
#106323=AXIS2_PLACEMENT_3D('',#224234,#129524,#129525);
#106324=AXIS2_PLACEMENT_3D('',#224236,#129526,#129527);
#106325=AXIS2_PLACEMENT_3D('',#224238,#129529,#129530);
#106326=AXIS2_PLACEMENT_3D('',#224242,#129532,#129533);
#106327=AXIS2_PLACEMENT_3D('',#224244,#129535,#129536);
#106328=AXIS2_PLACEMENT_3D('',#224245,#129537,#129538);
#106329=AXIS2_PLACEMENT_3D('',#224246,#129539,#129540);
#106330=AXIS2_PLACEMENT_3D('',#224247,#129541,#129542);
#106331=AXIS2_PLACEMENT_3D('',#224248,#129543,#129544);
#106332=AXIS2_PLACEMENT_3D('',#224249,#129545,#129546);
#106333=AXIS2_PLACEMENT_3D('',#224250,#129547,#129548);
#106334=AXIS2_PLACEMENT_3D('',#224251,#129549,#129550);
#106335=AXIS2_PLACEMENT_3D('',#224252,#129551,#129552);
#106336=AXIS2_PLACEMENT_3D('',#224253,#129553,#129554);
#106337=AXIS2_PLACEMENT_3D('',#224254,#129555,#129556);
#106338=AXIS2_PLACEMENT_3D('',#224255,#129557,#129558);
#106339=AXIS2_PLACEMENT_3D('',#224256,#129559,#129560);
#106340=AXIS2_PLACEMENT_3D('',#224259,#129561,#129562);
#106341=AXIS2_PLACEMENT_3D('',#224263,#129564,#129565);
#106342=AXIS2_PLACEMENT_3D('',#224265,#129566,#129567);
#106343=AXIS2_PLACEMENT_3D('',#224267,#129568,#129569);
#106344=AXIS2_PLACEMENT_3D('',#224269,#129571,#129572);
#106345=AXIS2_PLACEMENT_3D('',#224273,#129574,#129575);
#106346=AXIS2_PLACEMENT_3D('',#224275,#129577,#129578);
#106347=AXIS2_PLACEMENT_3D('',#224278,#129579,#129580);
#106348=AXIS2_PLACEMENT_3D('',#224282,#129582,#129583);
#106349=AXIS2_PLACEMENT_3D('',#224284,#129585,#129586);
#106350=AXIS2_PLACEMENT_3D('',#224287,#129587,#129588);
#106351=AXIS2_PLACEMENT_3D('',#224291,#129590,#129591);
#106352=AXIS2_PLACEMENT_3D('',#224293,#129592,#129593);
#106353=AXIS2_PLACEMENT_3D('',#224295,#129594,#129595);
#106354=AXIS2_PLACEMENT_3D('',#224297,#129597,#129598);
#106355=AXIS2_PLACEMENT_3D('',#224301,#129600,#129601);
#106356=AXIS2_PLACEMENT_3D('',#224303,#129603,#129604);
#106357=AXIS2_PLACEMENT_3D('',#224304,#129605,#129606);
#106358=AXIS2_PLACEMENT_3D('',#224305,#129607,#129608);
#106359=AXIS2_PLACEMENT_3D('',#224306,#129609,#129610);
#106360=AXIS2_PLACEMENT_3D('',#224307,#129611,#129612);
#106361=AXIS2_PLACEMENT_3D('',#224308,#129613,#129614);
#106362=AXIS2_PLACEMENT_3D('',#224309,#129615,#129616);
#106363=AXIS2_PLACEMENT_3D('',#224310,#129617,#129618);
#106364=AXIS2_PLACEMENT_3D('',#224311,#129619,#129620);
#106365=AXIS2_PLACEMENT_3D('',#224312,#129621,#129622);
#106366=AXIS2_PLACEMENT_3D('',#224313,#129623,#129624);
#106367=AXIS2_PLACEMENT_3D('',#224314,#129625,#129626);
#106368=AXIS2_PLACEMENT_3D('',#224315,#129627,#129628);
#106369=AXIS2_PLACEMENT_3D('',#224318,#129629,#129630);
#106370=AXIS2_PLACEMENT_3D('',#224322,#129632,#129633);
#106371=AXIS2_PLACEMENT_3D('',#224324,#129634,#129635);
#106372=AXIS2_PLACEMENT_3D('',#224326,#129636,#129637);
#106373=AXIS2_PLACEMENT_3D('',#224328,#129639,#129640);
#106374=AXIS2_PLACEMENT_3D('',#224332,#129642,#129643);
#106375=AXIS2_PLACEMENT_3D('',#224334,#129645,#129646);
#106376=AXIS2_PLACEMENT_3D('',#224337,#129647,#129648);
#106377=AXIS2_PLACEMENT_3D('',#224341,#129650,#129651);
#106378=AXIS2_PLACEMENT_3D('',#224343,#129653,#129654);
#106379=AXIS2_PLACEMENT_3D('',#224346,#129655,#129656);
#106380=AXIS2_PLACEMENT_3D('',#224350,#129658,#129659);
#106381=AXIS2_PLACEMENT_3D('',#224352,#129660,#129661);
#106382=AXIS2_PLACEMENT_3D('',#224354,#129662,#129663);
#106383=AXIS2_PLACEMENT_3D('',#224356,#129665,#129666);
#106384=AXIS2_PLACEMENT_3D('',#224360,#129668,#129669);
#106385=AXIS2_PLACEMENT_3D('',#224362,#129671,#129672);
#106386=AXIS2_PLACEMENT_3D('',#224363,#129673,#129674);
#106387=AXIS2_PLACEMENT_3D('',#224364,#129675,#129676);
#106388=AXIS2_PLACEMENT_3D('',#224365,#129677,#129678);
#106389=AXIS2_PLACEMENT_3D('',#224366,#129679,#129680);
#106390=AXIS2_PLACEMENT_3D('',#224367,#129681,#129682);
#106391=AXIS2_PLACEMENT_3D('',#224368,#129683,#129684);
#106392=AXIS2_PLACEMENT_3D('',#224369,#129685,#129686);
#106393=AXIS2_PLACEMENT_3D('',#224370,#129687,#129688);
#106394=AXIS2_PLACEMENT_3D('',#224371,#129689,#129690);
#106395=AXIS2_PLACEMENT_3D('',#224372,#129691,#129692);
#106396=AXIS2_PLACEMENT_3D('',#224373,#129693,#129694);
#106397=AXIS2_PLACEMENT_3D('',#224374,#129695,#129696);
#106398=AXIS2_PLACEMENT_3D('',#224377,#129697,#129698);
#106399=AXIS2_PLACEMENT_3D('',#224381,#129700,#129701);
#106400=AXIS2_PLACEMENT_3D('',#224383,#129702,#129703);
#106401=AXIS2_PLACEMENT_3D('',#224385,#129704,#129705);
#106402=AXIS2_PLACEMENT_3D('',#224387,#129707,#129708);
#106403=AXIS2_PLACEMENT_3D('',#224391,#129710,#129711);
#106404=AXIS2_PLACEMENT_3D('',#224393,#129713,#129714);
#106405=AXIS2_PLACEMENT_3D('',#224396,#129715,#129716);
#106406=AXIS2_PLACEMENT_3D('',#224400,#129718,#129719);
#106407=AXIS2_PLACEMENT_3D('',#224402,#129721,#129722);
#106408=AXIS2_PLACEMENT_3D('',#224405,#129723,#129724);
#106409=AXIS2_PLACEMENT_3D('',#224409,#129726,#129727);
#106410=AXIS2_PLACEMENT_3D('',#224411,#129728,#129729);
#106411=AXIS2_PLACEMENT_3D('',#224413,#129730,#129731);
#106412=AXIS2_PLACEMENT_3D('',#224415,#129733,#129734);
#106413=AXIS2_PLACEMENT_3D('',#224419,#129736,#129737);
#106414=AXIS2_PLACEMENT_3D('',#224421,#129739,#129740);
#106415=AXIS2_PLACEMENT_3D('',#224422,#129741,#129742);
#106416=AXIS2_PLACEMENT_3D('',#224423,#129743,#129744);
#106417=AXIS2_PLACEMENT_3D('',#224424,#129745,#129746);
#106418=AXIS2_PLACEMENT_3D('',#224425,#129747,#129748);
#106419=AXIS2_PLACEMENT_3D('',#224426,#129749,#129750);
#106420=AXIS2_PLACEMENT_3D('',#224427,#129751,#129752);
#106421=AXIS2_PLACEMENT_3D('',#224428,#129753,#129754);
#106422=AXIS2_PLACEMENT_3D('',#224429,#129755,#129756);
#106423=AXIS2_PLACEMENT_3D('',#224430,#129757,#129758);
#106424=AXIS2_PLACEMENT_3D('',#224431,#129759,#129760);
#106425=AXIS2_PLACEMENT_3D('',#224432,#129761,#129762);
#106426=AXIS2_PLACEMENT_3D('',#224433,#129763,#129764);
#106427=AXIS2_PLACEMENT_3D('',#224436,#129765,#129766);
#106428=AXIS2_PLACEMENT_3D('',#224440,#129768,#129769);
#106429=AXIS2_PLACEMENT_3D('',#224442,#129770,#129771);
#106430=AXIS2_PLACEMENT_3D('',#224444,#129772,#129773);
#106431=AXIS2_PLACEMENT_3D('',#224446,#129775,#129776);
#106432=AXIS2_PLACEMENT_3D('',#224450,#129778,#129779);
#106433=AXIS2_PLACEMENT_3D('',#224452,#129781,#129782);
#106434=AXIS2_PLACEMENT_3D('',#224455,#129783,#129784);
#106435=AXIS2_PLACEMENT_3D('',#224459,#129786,#129787);
#106436=AXIS2_PLACEMENT_3D('',#224461,#129789,#129790);
#106437=AXIS2_PLACEMENT_3D('',#224464,#129791,#129792);
#106438=AXIS2_PLACEMENT_3D('',#224468,#129794,#129795);
#106439=AXIS2_PLACEMENT_3D('',#224470,#129796,#129797);
#106440=AXIS2_PLACEMENT_3D('',#224472,#129798,#129799);
#106441=AXIS2_PLACEMENT_3D('',#224474,#129801,#129802);
#106442=AXIS2_PLACEMENT_3D('',#224478,#129804,#129805);
#106443=AXIS2_PLACEMENT_3D('',#224480,#129807,#129808);
#106444=AXIS2_PLACEMENT_3D('',#224481,#129809,#129810);
#106445=AXIS2_PLACEMENT_3D('',#224482,#129811,#129812);
#106446=AXIS2_PLACEMENT_3D('',#224483,#129813,#129814);
#106447=AXIS2_PLACEMENT_3D('',#224484,#129815,#129816);
#106448=AXIS2_PLACEMENT_3D('',#224485,#129817,#129818);
#106449=AXIS2_PLACEMENT_3D('',#224486,#129819,#129820);
#106450=AXIS2_PLACEMENT_3D('',#224487,#129821,#129822);
#106451=AXIS2_PLACEMENT_3D('',#224488,#129823,#129824);
#106452=AXIS2_PLACEMENT_3D('',#224489,#129825,#129826);
#106453=AXIS2_PLACEMENT_3D('',#224490,#129827,#129828);
#106454=AXIS2_PLACEMENT_3D('',#224491,#129829,#129830);
#106455=AXIS2_PLACEMENT_3D('',#224492,#129831,#129832);
#106456=AXIS2_PLACEMENT_3D('',#224495,#129833,#129834);
#106457=AXIS2_PLACEMENT_3D('',#224499,#129836,#129837);
#106458=AXIS2_PLACEMENT_3D('',#224501,#129838,#129839);
#106459=AXIS2_PLACEMENT_3D('',#224503,#129840,#129841);
#106460=AXIS2_PLACEMENT_3D('',#224505,#129843,#129844);
#106461=AXIS2_PLACEMENT_3D('',#224509,#129846,#129847);
#106462=AXIS2_PLACEMENT_3D('',#224511,#129849,#129850);
#106463=AXIS2_PLACEMENT_3D('',#224514,#129851,#129852);
#106464=AXIS2_PLACEMENT_3D('',#224518,#129854,#129855);
#106465=AXIS2_PLACEMENT_3D('',#224520,#129857,#129858);
#106466=AXIS2_PLACEMENT_3D('',#224523,#129859,#129860);
#106467=AXIS2_PLACEMENT_3D('',#224527,#129862,#129863);
#106468=AXIS2_PLACEMENT_3D('',#224529,#129864,#129865);
#106469=AXIS2_PLACEMENT_3D('',#224531,#129866,#129867);
#106470=AXIS2_PLACEMENT_3D('',#224533,#129869,#129870);
#106471=AXIS2_PLACEMENT_3D('',#224537,#129872,#129873);
#106472=AXIS2_PLACEMENT_3D('',#224539,#129875,#129876);
#106473=AXIS2_PLACEMENT_3D('',#224540,#129877,#129878);
#106474=AXIS2_PLACEMENT_3D('',#224541,#129879,#129880);
#106475=AXIS2_PLACEMENT_3D('',#224542,#129881,#129882);
#106476=AXIS2_PLACEMENT_3D('',#224543,#129883,#129884);
#106477=AXIS2_PLACEMENT_3D('',#224544,#129885,#129886);
#106478=AXIS2_PLACEMENT_3D('',#224545,#129887,#129888);
#106479=AXIS2_PLACEMENT_3D('',#224546,#129889,#129890);
#106480=AXIS2_PLACEMENT_3D('',#224547,#129891,#129892);
#106481=AXIS2_PLACEMENT_3D('',#224548,#129893,#129894);
#106482=AXIS2_PLACEMENT_3D('',#224549,#129895,#129896);
#106483=AXIS2_PLACEMENT_3D('',#224550,#129897,#129898);
#106484=AXIS2_PLACEMENT_3D('',#224551,#129899,#129900);
#106485=AXIS2_PLACEMENT_3D('',#224554,#129901,#129902);
#106486=AXIS2_PLACEMENT_3D('',#224558,#129904,#129905);
#106487=AXIS2_PLACEMENT_3D('',#224560,#129906,#129907);
#106488=AXIS2_PLACEMENT_3D('',#224562,#129908,#129909);
#106489=AXIS2_PLACEMENT_3D('',#224564,#129911,#129912);
#106490=AXIS2_PLACEMENT_3D('',#224568,#129914,#129915);
#106491=AXIS2_PLACEMENT_3D('',#224570,#129917,#129918);
#106492=AXIS2_PLACEMENT_3D('',#224573,#129919,#129920);
#106493=AXIS2_PLACEMENT_3D('',#224577,#129922,#129923);
#106494=AXIS2_PLACEMENT_3D('',#224579,#129925,#129926);
#106495=AXIS2_PLACEMENT_3D('',#224582,#129927,#129928);
#106496=AXIS2_PLACEMENT_3D('',#224586,#129930,#129931);
#106497=AXIS2_PLACEMENT_3D('',#224588,#129932,#129933);
#106498=AXIS2_PLACEMENT_3D('',#224590,#129934,#129935);
#106499=AXIS2_PLACEMENT_3D('',#224592,#129937,#129938);
#106500=AXIS2_PLACEMENT_3D('',#224596,#129940,#129941);
#106501=AXIS2_PLACEMENT_3D('',#224598,#129943,#129944);
#106502=AXIS2_PLACEMENT_3D('',#224599,#129945,#129946);
#106503=AXIS2_PLACEMENT_3D('',#224600,#129947,#129948);
#106504=AXIS2_PLACEMENT_3D('',#224601,#129949,#129950);
#106505=AXIS2_PLACEMENT_3D('',#224602,#129951,#129952);
#106506=AXIS2_PLACEMENT_3D('',#224603,#129953,#129954);
#106507=AXIS2_PLACEMENT_3D('',#224604,#129955,#129956);
#106508=AXIS2_PLACEMENT_3D('',#224605,#129957,#129958);
#106509=AXIS2_PLACEMENT_3D('',#224606,#129959,#129960);
#106510=AXIS2_PLACEMENT_3D('',#224607,#129961,#129962);
#106511=AXIS2_PLACEMENT_3D('',#224608,#129963,#129964);
#106512=AXIS2_PLACEMENT_3D('',#224609,#129965,#129966);
#106513=AXIS2_PLACEMENT_3D('',#224610,#129967,#129968);
#106514=AXIS2_PLACEMENT_3D('',#224613,#129969,#129970);
#106515=AXIS2_PLACEMENT_3D('',#224617,#129972,#129973);
#106516=AXIS2_PLACEMENT_3D('',#224619,#129974,#129975);
#106517=AXIS2_PLACEMENT_3D('',#224621,#129976,#129977);
#106518=AXIS2_PLACEMENT_3D('',#224623,#129979,#129980);
#106519=AXIS2_PLACEMENT_3D('',#224627,#129982,#129983);
#106520=AXIS2_PLACEMENT_3D('',#224629,#129985,#129986);
#106521=AXIS2_PLACEMENT_3D('',#224632,#129987,#129988);
#106522=AXIS2_PLACEMENT_3D('',#224636,#129990,#129991);
#106523=AXIS2_PLACEMENT_3D('',#224638,#129993,#129994);
#106524=AXIS2_PLACEMENT_3D('',#224641,#129995,#129996);
#106525=AXIS2_PLACEMENT_3D('',#224645,#129998,#129999);
#106526=AXIS2_PLACEMENT_3D('',#224647,#130000,#130001);
#106527=AXIS2_PLACEMENT_3D('',#224649,#130002,#130003);
#106528=AXIS2_PLACEMENT_3D('',#224651,#130005,#130006);
#106529=AXIS2_PLACEMENT_3D('',#224655,#130008,#130009);
#106530=AXIS2_PLACEMENT_3D('',#224657,#130011,#130012);
#106531=AXIS2_PLACEMENT_3D('',#224658,#130013,#130014);
#106532=AXIS2_PLACEMENT_3D('',#224659,#130015,#130016);
#106533=AXIS2_PLACEMENT_3D('',#224660,#130017,#130018);
#106534=AXIS2_PLACEMENT_3D('',#224661,#130019,#130020);
#106535=AXIS2_PLACEMENT_3D('',#224662,#130021,#130022);
#106536=AXIS2_PLACEMENT_3D('',#224663,#130023,#130024);
#106537=AXIS2_PLACEMENT_3D('',#224664,#130025,#130026);
#106538=AXIS2_PLACEMENT_3D('',#224665,#130027,#130028);
#106539=AXIS2_PLACEMENT_3D('',#224666,#130029,#130030);
#106540=AXIS2_PLACEMENT_3D('',#224667,#130031,#130032);
#106541=AXIS2_PLACEMENT_3D('',#224668,#130033,#130034);
#106542=AXIS2_PLACEMENT_3D('',#224669,#130035,#130036);
#106543=AXIS2_PLACEMENT_3D('',#224672,#130037,#130038);
#106544=AXIS2_PLACEMENT_3D('',#224676,#130040,#130041);
#106545=AXIS2_PLACEMENT_3D('',#224678,#130042,#130043);
#106546=AXIS2_PLACEMENT_3D('',#224680,#130044,#130045);
#106547=AXIS2_PLACEMENT_3D('',#224682,#130047,#130048);
#106548=AXIS2_PLACEMENT_3D('',#224686,#130050,#130051);
#106549=AXIS2_PLACEMENT_3D('',#224688,#130053,#130054);
#106550=AXIS2_PLACEMENT_3D('',#224691,#130055,#130056);
#106551=AXIS2_PLACEMENT_3D('',#224695,#130058,#130059);
#106552=AXIS2_PLACEMENT_3D('',#224697,#130061,#130062);
#106553=AXIS2_PLACEMENT_3D('',#224700,#130063,#130064);
#106554=AXIS2_PLACEMENT_3D('',#224704,#130066,#130067);
#106555=AXIS2_PLACEMENT_3D('',#224706,#130068,#130069);
#106556=AXIS2_PLACEMENT_3D('',#224708,#130070,#130071);
#106557=AXIS2_PLACEMENT_3D('',#224710,#130073,#130074);
#106558=AXIS2_PLACEMENT_3D('',#224714,#130076,#130077);
#106559=AXIS2_PLACEMENT_3D('',#224716,#130079,#130080);
#106560=AXIS2_PLACEMENT_3D('',#224717,#130081,#130082);
#106561=AXIS2_PLACEMENT_3D('',#224718,#130083,#130084);
#106562=AXIS2_PLACEMENT_3D('',#224719,#130085,#130086);
#106563=AXIS2_PLACEMENT_3D('',#224720,#130087,#130088);
#106564=AXIS2_PLACEMENT_3D('',#224721,#130089,#130090);
#106565=AXIS2_PLACEMENT_3D('',#224722,#130091,#130092);
#106566=AXIS2_PLACEMENT_3D('',#224723,#130093,#130094);
#106567=AXIS2_PLACEMENT_3D('',#224724,#130095,#130096);
#106568=AXIS2_PLACEMENT_3D('',#224725,#130097,#130098);
#106569=AXIS2_PLACEMENT_3D('',#224726,#130099,#130100);
#106570=AXIS2_PLACEMENT_3D('',#224727,#130101,#130102);
#106571=AXIS2_PLACEMENT_3D('',#224728,#130103,#130104);
#106572=AXIS2_PLACEMENT_3D('',#224731,#130105,#130106);
#106573=AXIS2_PLACEMENT_3D('',#224735,#130108,#130109);
#106574=AXIS2_PLACEMENT_3D('',#224737,#130110,#130111);
#106575=AXIS2_PLACEMENT_3D('',#224739,#130112,#130113);
#106576=AXIS2_PLACEMENT_3D('',#224741,#130115,#130116);
#106577=AXIS2_PLACEMENT_3D('',#224745,#130118,#130119);
#106578=AXIS2_PLACEMENT_3D('',#224747,#130121,#130122);
#106579=AXIS2_PLACEMENT_3D('',#224750,#130123,#130124);
#106580=AXIS2_PLACEMENT_3D('',#224754,#130126,#130127);
#106581=AXIS2_PLACEMENT_3D('',#224756,#130129,#130130);
#106582=AXIS2_PLACEMENT_3D('',#224759,#130131,#130132);
#106583=AXIS2_PLACEMENT_3D('',#224763,#130134,#130135);
#106584=AXIS2_PLACEMENT_3D('',#224765,#130136,#130137);
#106585=AXIS2_PLACEMENT_3D('',#224767,#130138,#130139);
#106586=AXIS2_PLACEMENT_3D('',#224769,#130141,#130142);
#106587=AXIS2_PLACEMENT_3D('',#224773,#130144,#130145);
#106588=AXIS2_PLACEMENT_3D('',#224775,#130147,#130148);
#106589=AXIS2_PLACEMENT_3D('',#224776,#130149,#130150);
#106590=AXIS2_PLACEMENT_3D('',#224777,#130151,#130152);
#106591=AXIS2_PLACEMENT_3D('',#224778,#130153,#130154);
#106592=AXIS2_PLACEMENT_3D('',#224779,#130155,#130156);
#106593=AXIS2_PLACEMENT_3D('',#224780,#130157,#130158);
#106594=AXIS2_PLACEMENT_3D('',#224781,#130159,#130160);
#106595=AXIS2_PLACEMENT_3D('',#224782,#130161,#130162);
#106596=AXIS2_PLACEMENT_3D('',#224783,#130163,#130164);
#106597=AXIS2_PLACEMENT_3D('',#224784,#130165,#130166);
#106598=AXIS2_PLACEMENT_3D('',#224785,#130167,#130168);
#106599=AXIS2_PLACEMENT_3D('',#224786,#130169,#130170);
#106600=AXIS2_PLACEMENT_3D('',#224787,#130171,#130172);
#106601=AXIS2_PLACEMENT_3D('',#224790,#130173,#130174);
#106602=AXIS2_PLACEMENT_3D('',#224794,#130176,#130177);
#106603=AXIS2_PLACEMENT_3D('',#224796,#130178,#130179);
#106604=AXIS2_PLACEMENT_3D('',#224798,#130180,#130181);
#106605=AXIS2_PLACEMENT_3D('',#224800,#130183,#130184);
#106606=AXIS2_PLACEMENT_3D('',#224804,#130186,#130187);
#106607=AXIS2_PLACEMENT_3D('',#224806,#130189,#130190);
#106608=AXIS2_PLACEMENT_3D('',#224809,#130191,#130192);
#106609=AXIS2_PLACEMENT_3D('',#224813,#130194,#130195);
#106610=AXIS2_PLACEMENT_3D('',#224815,#130197,#130198);
#106611=AXIS2_PLACEMENT_3D('',#224818,#130199,#130200);
#106612=AXIS2_PLACEMENT_3D('',#224822,#130202,#130203);
#106613=AXIS2_PLACEMENT_3D('',#224824,#130204,#130205);
#106614=AXIS2_PLACEMENT_3D('',#224826,#130206,#130207);
#106615=AXIS2_PLACEMENT_3D('',#224828,#130209,#130210);
#106616=AXIS2_PLACEMENT_3D('',#224832,#130212,#130213);
#106617=AXIS2_PLACEMENT_3D('',#224834,#130215,#130216);
#106618=AXIS2_PLACEMENT_3D('',#224835,#130217,#130218);
#106619=AXIS2_PLACEMENT_3D('',#224836,#130219,#130220);
#106620=AXIS2_PLACEMENT_3D('',#224837,#130221,#130222);
#106621=AXIS2_PLACEMENT_3D('',#224838,#130223,#130224);
#106622=AXIS2_PLACEMENT_3D('',#224839,#130225,#130226);
#106623=AXIS2_PLACEMENT_3D('',#224840,#130227,#130228);
#106624=AXIS2_PLACEMENT_3D('',#224841,#130229,#130230);
#106625=AXIS2_PLACEMENT_3D('',#224842,#130231,#130232);
#106626=AXIS2_PLACEMENT_3D('',#224843,#130233,#130234);
#106627=AXIS2_PLACEMENT_3D('',#224844,#130235,#130236);
#106628=AXIS2_PLACEMENT_3D('',#224845,#130237,#130238);
#106629=AXIS2_PLACEMENT_3D('',#224846,#130239,#130240);
#106630=AXIS2_PLACEMENT_3D('',#224847,#130241,#130242);
#106631=AXIS2_PLACEMENT_3D('',#224850,#130243,#130244);
#106632=AXIS2_PLACEMENT_3D('',#224854,#130246,#130247);
#106633=AXIS2_PLACEMENT_3D('',#224856,#130248,#130249);
#106634=AXIS2_PLACEMENT_3D('',#224858,#130250,#130251);
#106635=AXIS2_PLACEMENT_3D('',#224860,#130253,#130254);
#106636=AXIS2_PLACEMENT_3D('',#224864,#130256,#130257);
#106637=AXIS2_PLACEMENT_3D('',#224866,#130259,#130260);
#106638=AXIS2_PLACEMENT_3D('',#224869,#130261,#130262);
#106639=AXIS2_PLACEMENT_3D('',#224873,#130264,#130265);
#106640=AXIS2_PLACEMENT_3D('',#224875,#130267,#130268);
#106641=AXIS2_PLACEMENT_3D('',#224878,#130269,#130270);
#106642=AXIS2_PLACEMENT_3D('',#224882,#130272,#130273);
#106643=AXIS2_PLACEMENT_3D('',#224884,#130274,#130275);
#106644=AXIS2_PLACEMENT_3D('',#224886,#130276,#130277);
#106645=AXIS2_PLACEMENT_3D('',#224888,#130279,#130280);
#106646=AXIS2_PLACEMENT_3D('',#224892,#130282,#130283);
#106647=AXIS2_PLACEMENT_3D('',#224894,#130285,#130286);
#106648=AXIS2_PLACEMENT_3D('',#224895,#130287,#130288);
#106649=AXIS2_PLACEMENT_3D('',#224896,#130289,#130290);
#106650=AXIS2_PLACEMENT_3D('',#224897,#130291,#130292);
#106651=AXIS2_PLACEMENT_3D('',#224898,#130293,#130294);
#106652=AXIS2_PLACEMENT_3D('',#224899,#130295,#130296);
#106653=AXIS2_PLACEMENT_3D('',#224900,#130297,#130298);
#106654=AXIS2_PLACEMENT_3D('',#224901,#130299,#130300);
#106655=AXIS2_PLACEMENT_3D('',#224902,#130301,#130302);
#106656=AXIS2_PLACEMENT_3D('',#224903,#130303,#130304);
#106657=AXIS2_PLACEMENT_3D('',#224904,#130305,#130306);
#106658=AXIS2_PLACEMENT_3D('',#224905,#130307,#130308);
#106659=AXIS2_PLACEMENT_3D('',#224906,#130309,#130310);
#106660=AXIS2_PLACEMENT_3D('',#224907,#130311,#130312);
#106661=AXIS2_PLACEMENT_3D('',#224908,#130313,#130314);
#106662=AXIS2_PLACEMENT_3D('',#224913,#130316,#130317);
#106663=AXIS2_PLACEMENT_3D('',#224916,#130319,#130320);
#106664=AXIS2_PLACEMENT_3D('',#224917,#130321,#130322);
#106665=AXIS2_PLACEMENT_3D('',#224920,#130323,#130324);
#106666=AXIS2_PLACEMENT_3D('',#224928,#130328,#130329);
#106667=AXIS2_PLACEMENT_3D('',#224934,#130332,#130333);
#106668=AXIS2_PLACEMENT_3D('',#224938,#130335,#130336);
#106669=AXIS2_PLACEMENT_3D('',#224942,#130339,#130340);
#106670=AXIS2_PLACEMENT_3D('',#224945,#130341,#130342);
#106671=AXIS2_PLACEMENT_3D('',#224953,#130346,#130347);
#106672=AXIS2_PLACEMENT_3D('',#224959,#130350,#130351);
#106673=AXIS2_PLACEMENT_3D('',#224963,#130353,#130354);
#106674=AXIS2_PLACEMENT_3D('',#224967,#130357,#130358);
#106675=AXIS2_PLACEMENT_3D('',#225072,#130359,#130360);
#106676=AXIS2_PLACEMENT_3D('',#225171,#130361,#130362);
#106677=AXIS2_PLACEMENT_3D('',#225172,#130363,#130364);
#106678=AXIS2_PLACEMENT_3D('',#225173,#130365,#130366);
#106679=AXIS2_PLACEMENT_3D('',#225186,#130367,#130368);
#106680=AXIS2_PLACEMENT_3D('',#225187,#130369,#130370);
#106681=AXIS2_PLACEMENT_3D('',#225188,#130371,#130372);
#106682=AXIS2_PLACEMENT_3D('',#225189,#130373,#130374);
#106683=AXIS2_PLACEMENT_3D('',#225190,#130375,#130376);
#106684=AXIS2_PLACEMENT_3D('',#225203,#130377,#130378);
#106685=AXIS2_PLACEMENT_3D('',#225216,#130379,#130380);
#106686=AXIS2_PLACEMENT_3D('',#225217,#130381,#130382);
#106687=AXIS2_PLACEMENT_3D('',#225218,#130383,#130384);
#106688=AXIS2_PLACEMENT_3D('',#225219,#130385,#130386);
#106689=AXIS2_PLACEMENT_3D('',#225220,#130387,#130388);
#106690=AXIS2_PLACEMENT_3D('',#225239,#130389,#130390);
#106691=AXIS2_PLACEMENT_3D('',#225240,#130391,#130392);
#106692=AXIS2_PLACEMENT_3D('',#225241,#130393,#130394);
#106693=AXIS2_PLACEMENT_3D('',#225242,#130395,#130396);
#106694=AXIS2_PLACEMENT_3D('',#225243,#130397,#130398);
#106695=AXIS2_PLACEMENT_3D('',#225256,#130399,#130400);
#106696=AXIS2_PLACEMENT_3D('',#225275,#130401,#130402);
#106697=AXIS2_PLACEMENT_3D('',#225276,#130403,#130404);
#106698=AXIS2_PLACEMENT_3D('',#225277,#130405,#130406);
#106699=AXIS2_PLACEMENT_3D('',#225278,#130407,#130408);
#106700=AXIS2_PLACEMENT_3D('',#225279,#130409,#130410);
#106701=AXIS2_PLACEMENT_3D('',#225298,#130411,#130412);
#106702=AXIS2_PLACEMENT_3D('',#225311,#130413,#130414);
#106703=AXIS2_PLACEMENT_3D('',#225312,#130415,#130416);
#106704=AXIS2_PLACEMENT_3D('',#225313,#130417,#130418);
#106705=AXIS2_PLACEMENT_3D('',#225314,#130419,#130420);
#106706=AXIS2_PLACEMENT_3D('',#225315,#130421,#130422);
#106707=AXIS2_PLACEMENT_3D('',#225334,#130423,#130424);
#106708=AXIS2_PLACEMENT_3D('',#225335,#130425,#130426);
#106709=AXIS2_PLACEMENT_3D('',#225336,#130427,#130428);
#106710=AXIS2_PLACEMENT_3D('',#225337,#130429,#130430);
#106711=AXIS2_PLACEMENT_3D('',#225338,#130431,#130432);
#106712=AXIS2_PLACEMENT_3D('',#225351,#130433,#130434);
#106713=AXIS2_PLACEMENT_3D('',#225364,#130435,#130436);
#106714=AXIS2_PLACEMENT_3D('',#225365,#130437,#130438);
#106715=AXIS2_PLACEMENT_3D('',#225366,#130439,#130440);
#106716=AXIS2_PLACEMENT_3D('',#225367,#130441,#130442);
#106717=AXIS2_PLACEMENT_3D('',#225368,#130443,#130444);
#106718=AXIS2_PLACEMENT_3D('',#225381,#130445,#130446);
#106719=AXIS2_PLACEMENT_3D('',#225382,#130447,#130448);
#106720=AXIS2_PLACEMENT_3D('',#225383,#130449,#130450);
#106721=AXIS2_PLACEMENT_3D('',#225388,#130452,#130453);
#106722=AXIS2_PLACEMENT_3D('',#225391,#130455,#130456);
#106723=AXIS2_PLACEMENT_3D('',#225392,#130457,#130458);
#106724=AXIS2_PLACEMENT_3D('',#225395,#130459,#130460);
#106725=AXIS2_PLACEMENT_3D('',#225403,#130464,#130465);
#106726=AXIS2_PLACEMENT_3D('',#225409,#130468,#130469);
#106727=AXIS2_PLACEMENT_3D('',#225413,#130471,#130472);
#106728=AXIS2_PLACEMENT_3D('',#225417,#130475,#130476);
#106729=AXIS2_PLACEMENT_3D('',#225420,#130477,#130478);
#106730=AXIS2_PLACEMENT_3D('',#225428,#130482,#130483);
#106731=AXIS2_PLACEMENT_3D('',#225434,#130486,#130487);
#106732=AXIS2_PLACEMENT_3D('',#225438,#130489,#130490);
#106733=AXIS2_PLACEMENT_3D('',#225442,#130493,#130494);
#106734=AXIS2_PLACEMENT_3D('',#225447,#130496,#130497);
#106735=AXIS2_PLACEMENT_3D('',#225450,#130499,#130500);
#106736=AXIS2_PLACEMENT_3D('',#225451,#130501,#130502);
#106737=AXIS2_PLACEMENT_3D('',#225454,#130503,#130504);
#106738=AXIS2_PLACEMENT_3D('',#225462,#130508,#130509);
#106739=AXIS2_PLACEMENT_3D('',#225468,#130512,#130513);
#106740=AXIS2_PLACEMENT_3D('',#225472,#130515,#130516);
#106741=AXIS2_PLACEMENT_3D('',#225476,#130519,#130520);
#106742=AXIS2_PLACEMENT_3D('',#225479,#130521,#130522);
#106743=AXIS2_PLACEMENT_3D('',#225487,#130526,#130527);
#106744=AXIS2_PLACEMENT_3D('',#225493,#130530,#130531);
#106745=AXIS2_PLACEMENT_3D('',#225497,#130533,#130534);
#106746=AXIS2_PLACEMENT_3D('',#225501,#130537,#130538);
#106747=AXIS2_PLACEMENT_3D('',#225506,#130540,#130541);
#106748=AXIS2_PLACEMENT_3D('',#225509,#130543,#130544);
#106749=AXIS2_PLACEMENT_3D('',#225510,#130545,#130546);
#106750=AXIS2_PLACEMENT_3D('',#225513,#130547,#130548);
#106751=AXIS2_PLACEMENT_3D('',#225521,#130552,#130553);
#106752=AXIS2_PLACEMENT_3D('',#225527,#130556,#130557);
#106753=AXIS2_PLACEMENT_3D('',#225531,#130559,#130560);
#106754=AXIS2_PLACEMENT_3D('',#225535,#130563,#130564);
#106755=AXIS2_PLACEMENT_3D('',#225538,#130565,#130566);
#106756=AXIS2_PLACEMENT_3D('',#225546,#130570,#130571);
#106757=AXIS2_PLACEMENT_3D('',#225552,#130574,#130575);
#106758=AXIS2_PLACEMENT_3D('',#225556,#130577,#130578);
#106759=AXIS2_PLACEMENT_3D('',#225560,#130581,#130582);
#106760=AXIS2_PLACEMENT_3D('',#225565,#130584,#130585);
#106761=AXIS2_PLACEMENT_3D('',#225568,#130587,#130588);
#106762=AXIS2_PLACEMENT_3D('',#225569,#130589,#130590);
#106763=AXIS2_PLACEMENT_3D('',#225572,#130591,#130592);
#106764=AXIS2_PLACEMENT_3D('',#225580,#130596,#130597);
#106765=AXIS2_PLACEMENT_3D('',#225586,#130600,#130601);
#106766=AXIS2_PLACEMENT_3D('',#225590,#130603,#130604);
#106767=AXIS2_PLACEMENT_3D('',#225594,#130607,#130608);
#106768=AXIS2_PLACEMENT_3D('',#225597,#130609,#130610);
#106769=AXIS2_PLACEMENT_3D('',#225605,#130614,#130615);
#106770=AXIS2_PLACEMENT_3D('',#225611,#130618,#130619);
#106771=AXIS2_PLACEMENT_3D('',#225615,#130621,#130622);
#106772=AXIS2_PLACEMENT_3D('',#225619,#130625,#130626);
#106773=AXIS2_PLACEMENT_3D('',#225624,#130628,#130629);
#106774=AXIS2_PLACEMENT_3D('',#225627,#130631,#130632);
#106775=AXIS2_PLACEMENT_3D('',#225628,#130633,#130634);
#106776=AXIS2_PLACEMENT_3D('',#225631,#130635,#130636);
#106777=AXIS2_PLACEMENT_3D('',#225639,#130640,#130641);
#106778=AXIS2_PLACEMENT_3D('',#225645,#130644,#130645);
#106779=AXIS2_PLACEMENT_3D('',#225649,#130647,#130648);
#106780=AXIS2_PLACEMENT_3D('',#225653,#130651,#130652);
#106781=AXIS2_PLACEMENT_3D('',#225656,#130653,#130654);
#106782=AXIS2_PLACEMENT_3D('',#225664,#130658,#130659);
#106783=AXIS2_PLACEMENT_3D('',#225670,#130662,#130663);
#106784=AXIS2_PLACEMENT_3D('',#225674,#130665,#130666);
#106785=AXIS2_PLACEMENT_3D('',#225678,#130669,#130670);
#106786=AXIS2_PLACEMENT_3D('',#225683,#130672,#130673);
#106787=AXIS2_PLACEMENT_3D('',#225686,#130675,#130676);
#106788=AXIS2_PLACEMENT_3D('',#225687,#130677,#130678);
#106789=AXIS2_PLACEMENT_3D('',#225690,#130679,#130680);
#106790=AXIS2_PLACEMENT_3D('',#225698,#130684,#130685);
#106791=AXIS2_PLACEMENT_3D('',#225704,#130688,#130689);
#106792=AXIS2_PLACEMENT_3D('',#225708,#130691,#130692);
#106793=AXIS2_PLACEMENT_3D('',#225712,#130695,#130696);
#106794=AXIS2_PLACEMENT_3D('',#225715,#130697,#130698);
#106795=AXIS2_PLACEMENT_3D('',#225723,#130702,#130703);
#106796=AXIS2_PLACEMENT_3D('',#225729,#130706,#130707);
#106797=AXIS2_PLACEMENT_3D('',#225733,#130709,#130710);
#106798=AXIS2_PLACEMENT_3D('',#225737,#130713,#130714);
#106799=AXIS2_PLACEMENT_3D('',#225742,#130716,#130717);
#106800=AXIS2_PLACEMENT_3D('',#225745,#130719,#130720);
#106801=AXIS2_PLACEMENT_3D('',#225746,#130721,#130722);
#106802=AXIS2_PLACEMENT_3D('',#225749,#130723,#130724);
#106803=AXIS2_PLACEMENT_3D('',#225757,#130728,#130729);
#106804=AXIS2_PLACEMENT_3D('',#225763,#130732,#130733);
#106805=AXIS2_PLACEMENT_3D('',#225767,#130735,#130736);
#106806=AXIS2_PLACEMENT_3D('',#225771,#130739,#130740);
#106807=AXIS2_PLACEMENT_3D('',#225774,#130741,#130742);
#106808=AXIS2_PLACEMENT_3D('',#225782,#130746,#130747);
#106809=AXIS2_PLACEMENT_3D('',#225788,#130750,#130751);
#106810=AXIS2_PLACEMENT_3D('',#225792,#130753,#130754);
#106811=AXIS2_PLACEMENT_3D('',#225796,#130757,#130758);
#106812=AXIS2_PLACEMENT_3D('',#225801,#130760,#130761);
#106813=AXIS2_PLACEMENT_3D('',#225804,#130763,#130764);
#106814=AXIS2_PLACEMENT_3D('',#225805,#130765,#130766);
#106815=AXIS2_PLACEMENT_3D('',#225808,#130767,#130768);
#106816=AXIS2_PLACEMENT_3D('',#225816,#130772,#130773);
#106817=AXIS2_PLACEMENT_3D('',#225822,#130776,#130777);
#106818=AXIS2_PLACEMENT_3D('',#225826,#130779,#130780);
#106819=AXIS2_PLACEMENT_3D('',#225830,#130783,#130784);
#106820=AXIS2_PLACEMENT_3D('',#225833,#130785,#130786);
#106821=AXIS2_PLACEMENT_3D('',#225841,#130790,#130791);
#106822=AXIS2_PLACEMENT_3D('',#225847,#130794,#130795);
#106823=AXIS2_PLACEMENT_3D('',#225851,#130797,#130798);
#106824=AXIS2_PLACEMENT_3D('',#225855,#130801,#130802);
#106825=AXIS2_PLACEMENT_3D('',#225860,#130804,#130805);
#106826=AXIS2_PLACEMENT_3D('',#225863,#130807,#130808);
#106827=AXIS2_PLACEMENT_3D('',#225864,#130809,#130810);
#106828=AXIS2_PLACEMENT_3D('',#225867,#130811,#130812);
#106829=AXIS2_PLACEMENT_3D('',#225875,#130816,#130817);
#106830=AXIS2_PLACEMENT_3D('',#225881,#130820,#130821);
#106831=AXIS2_PLACEMENT_3D('',#225885,#130823,#130824);
#106832=AXIS2_PLACEMENT_3D('',#225889,#130827,#130828);
#106833=AXIS2_PLACEMENT_3D('',#225892,#130829,#130830);
#106834=AXIS2_PLACEMENT_3D('',#225900,#130834,#130835);
#106835=AXIS2_PLACEMENT_3D('',#225906,#130838,#130839);
#106836=AXIS2_PLACEMENT_3D('',#225910,#130841,#130842);
#106837=AXIS2_PLACEMENT_3D('',#225914,#130845,#130846);
#106838=AXIS2_PLACEMENT_3D('',#225919,#130848,#130849);
#106839=AXIS2_PLACEMENT_3D('',#225922,#130851,#130852);
#106840=AXIS2_PLACEMENT_3D('',#225923,#130853,#130854);
#106841=AXIS2_PLACEMENT_3D('',#225926,#130855,#130856);
#106842=AXIS2_PLACEMENT_3D('',#225934,#130860,#130861);
#106843=AXIS2_PLACEMENT_3D('',#225940,#130864,#130865);
#106844=AXIS2_PLACEMENT_3D('',#225944,#130867,#130868);
#106845=AXIS2_PLACEMENT_3D('',#225948,#130871,#130872);
#106846=AXIS2_PLACEMENT_3D('',#225951,#130873,#130874);
#106847=AXIS2_PLACEMENT_3D('',#225959,#130878,#130879);
#106848=AXIS2_PLACEMENT_3D('',#225965,#130882,#130883);
#106849=AXIS2_PLACEMENT_3D('',#225969,#130885,#130886);
#106850=AXIS2_PLACEMENT_3D('',#225973,#130889,#130890);
#106851=AXIS2_PLACEMENT_3D('',#225978,#130892,#130893);
#106852=AXIS2_PLACEMENT_3D('',#225981,#130895,#130896);
#106853=AXIS2_PLACEMENT_3D('',#225982,#130897,#130898);
#106854=AXIS2_PLACEMENT_3D('',#225985,#130899,#130900);
#106855=AXIS2_PLACEMENT_3D('',#225993,#130904,#130905);
#106856=AXIS2_PLACEMENT_3D('',#225999,#130908,#130909);
#106857=AXIS2_PLACEMENT_3D('',#226003,#130911,#130912);
#106858=AXIS2_PLACEMENT_3D('',#226007,#130915,#130916);
#106859=AXIS2_PLACEMENT_3D('',#226010,#130917,#130918);
#106860=AXIS2_PLACEMENT_3D('',#226018,#130922,#130923);
#106861=AXIS2_PLACEMENT_3D('',#226024,#130926,#130927);
#106862=AXIS2_PLACEMENT_3D('',#226028,#130929,#130930);
#106863=AXIS2_PLACEMENT_3D('',#226032,#130933,#130934);
#106864=AXIS2_PLACEMENT_3D('',#226037,#130936,#130937);
#106865=AXIS2_PLACEMENT_3D('',#226040,#130939,#130940);
#106866=AXIS2_PLACEMENT_3D('',#226041,#130941,#130942);
#106867=AXIS2_PLACEMENT_3D('',#226044,#130943,#130944);
#106868=AXIS2_PLACEMENT_3D('',#226052,#130948,#130949);
#106869=AXIS2_PLACEMENT_3D('',#226058,#130952,#130953);
#106870=AXIS2_PLACEMENT_3D('',#226062,#130955,#130956);
#106871=AXIS2_PLACEMENT_3D('',#226066,#130959,#130960);
#106872=AXIS2_PLACEMENT_3D('',#226069,#130961,#130962);
#106873=AXIS2_PLACEMENT_3D('',#226077,#130966,#130967);
#106874=AXIS2_PLACEMENT_3D('',#226083,#130970,#130971);
#106875=AXIS2_PLACEMENT_3D('',#226087,#130973,#130974);
#106876=AXIS2_PLACEMENT_3D('',#226091,#130977,#130978);
#106877=AXIS2_PLACEMENT_3D('',#226096,#130980,#130981);
#106878=AXIS2_PLACEMENT_3D('',#226099,#130983,#130984);
#106879=AXIS2_PLACEMENT_3D('',#226100,#130985,#130986);
#106880=AXIS2_PLACEMENT_3D('',#226103,#130987,#130988);
#106881=AXIS2_PLACEMENT_3D('',#226111,#130992,#130993);
#106882=AXIS2_PLACEMENT_3D('',#226117,#130996,#130997);
#106883=AXIS2_PLACEMENT_3D('',#226121,#130999,#131000);
#106884=AXIS2_PLACEMENT_3D('',#226125,#131003,#131004);
#106885=AXIS2_PLACEMENT_3D('',#226128,#131005,#131006);
#106886=AXIS2_PLACEMENT_3D('',#226136,#131010,#131011);
#106887=AXIS2_PLACEMENT_3D('',#226142,#131014,#131015);
#106888=AXIS2_PLACEMENT_3D('',#226146,#131017,#131018);
#106889=AXIS2_PLACEMENT_3D('',#226150,#131021,#131022);
#106890=AXIS2_PLACEMENT_3D('',#226155,#131024,#131025);
#106891=AXIS2_PLACEMENT_3D('',#226158,#131027,#131028);
#106892=AXIS2_PLACEMENT_3D('',#226159,#131029,#131030);
#106893=AXIS2_PLACEMENT_3D('',#226162,#131031,#131032);
#106894=AXIS2_PLACEMENT_3D('',#226170,#131036,#131037);
#106895=AXIS2_PLACEMENT_3D('',#226176,#131040,#131041);
#106896=AXIS2_PLACEMENT_3D('',#226180,#131043,#131044);
#106897=AXIS2_PLACEMENT_3D('',#226184,#131047,#131048);
#106898=AXIS2_PLACEMENT_3D('',#226187,#131049,#131050);
#106899=AXIS2_PLACEMENT_3D('',#226195,#131054,#131055);
#106900=AXIS2_PLACEMENT_3D('',#226201,#131058,#131059);
#106901=AXIS2_PLACEMENT_3D('',#226205,#131061,#131062);
#106902=AXIS2_PLACEMENT_3D('',#226209,#131065,#131066);
#106903=AXIS2_PLACEMENT_3D('',#226214,#131068,#131069);
#106904=AXIS2_PLACEMENT_3D('',#226217,#131071,#131072);
#106905=AXIS2_PLACEMENT_3D('',#226218,#131073,#131074);
#106906=AXIS2_PLACEMENT_3D('',#226221,#131075,#131076);
#106907=AXIS2_PLACEMENT_3D('',#226229,#131080,#131081);
#106908=AXIS2_PLACEMENT_3D('',#226235,#131084,#131085);
#106909=AXIS2_PLACEMENT_3D('',#226239,#131087,#131088);
#106910=AXIS2_PLACEMENT_3D('',#226243,#131091,#131092);
#106911=AXIS2_PLACEMENT_3D('',#226246,#131093,#131094);
#106912=AXIS2_PLACEMENT_3D('',#226254,#131098,#131099);
#106913=AXIS2_PLACEMENT_3D('',#226260,#131102,#131103);
#106914=AXIS2_PLACEMENT_3D('',#226264,#131105,#131106);
#106915=AXIS2_PLACEMENT_3D('',#226268,#131109,#131110);
#106916=AXIS2_PLACEMENT_3D('',#226273,#131112,#131113);
#106917=AXIS2_PLACEMENT_3D('',#226276,#131115,#131116);
#106918=AXIS2_PLACEMENT_3D('',#226277,#131117,#131118);
#106919=AXIS2_PLACEMENT_3D('',#226280,#131119,#131120);
#106920=AXIS2_PLACEMENT_3D('',#226288,#131124,#131125);
#106921=AXIS2_PLACEMENT_3D('',#226294,#131128,#131129);
#106922=AXIS2_PLACEMENT_3D('',#226298,#131131,#131132);
#106923=AXIS2_PLACEMENT_3D('',#226302,#131135,#131136);
#106924=AXIS2_PLACEMENT_3D('',#226305,#131137,#131138);
#106925=AXIS2_PLACEMENT_3D('',#226313,#131142,#131143);
#106926=AXIS2_PLACEMENT_3D('',#226319,#131146,#131147);
#106927=AXIS2_PLACEMENT_3D('',#226323,#131149,#131150);
#106928=AXIS2_PLACEMENT_3D('',#226327,#131153,#131154);
#106929=AXIS2_PLACEMENT_3D('',#226332,#131156,#131157);
#106930=AXIS2_PLACEMENT_3D('',#226335,#131159,#131160);
#106931=AXIS2_PLACEMENT_3D('',#226336,#131161,#131162);
#106932=AXIS2_PLACEMENT_3D('',#226339,#131163,#131164);
#106933=AXIS2_PLACEMENT_3D('',#226347,#131168,#131169);
#106934=AXIS2_PLACEMENT_3D('',#226353,#131172,#131173);
#106935=AXIS2_PLACEMENT_3D('',#226357,#131175,#131176);
#106936=AXIS2_PLACEMENT_3D('',#226361,#131179,#131180);
#106937=AXIS2_PLACEMENT_3D('',#226364,#131181,#131182);
#106938=AXIS2_PLACEMENT_3D('',#226372,#131186,#131187);
#106939=AXIS2_PLACEMENT_3D('',#226378,#131190,#131191);
#106940=AXIS2_PLACEMENT_3D('',#226382,#131193,#131194);
#106941=AXIS2_PLACEMENT_3D('',#226386,#131197,#131198);
#106942=AXIS2_PLACEMENT_3D('',#226391,#131200,#131201);
#106943=AXIS2_PLACEMENT_3D('',#226394,#131203,#131204);
#106944=AXIS2_PLACEMENT_3D('',#226395,#131205,#131206);
#106945=AXIS2_PLACEMENT_3D('',#226398,#131207,#131208);
#106946=AXIS2_PLACEMENT_3D('',#226406,#131212,#131213);
#106947=AXIS2_PLACEMENT_3D('',#226412,#131216,#131217);
#106948=AXIS2_PLACEMENT_3D('',#226416,#131219,#131220);
#106949=AXIS2_PLACEMENT_3D('',#226420,#131223,#131224);
#106950=AXIS2_PLACEMENT_3D('',#226423,#131225,#131226);
#106951=AXIS2_PLACEMENT_3D('',#226431,#131230,#131231);
#106952=AXIS2_PLACEMENT_3D('',#226437,#131234,#131235);
#106953=AXIS2_PLACEMENT_3D('',#226441,#131237,#131238);
#106954=AXIS2_PLACEMENT_3D('',#226445,#131241,#131242);
#106955=AXIS2_PLACEMENT_3D('',#226450,#131244,#131245);
#106956=AXIS2_PLACEMENT_3D('',#226453,#131247,#131248);
#106957=AXIS2_PLACEMENT_3D('',#226454,#131249,#131250);
#106958=AXIS2_PLACEMENT_3D('',#226457,#131251,#131252);
#106959=AXIS2_PLACEMENT_3D('',#226465,#131256,#131257);
#106960=AXIS2_PLACEMENT_3D('',#226471,#131260,#131261);
#106961=AXIS2_PLACEMENT_3D('',#226475,#131263,#131264);
#106962=AXIS2_PLACEMENT_3D('',#226479,#131267,#131268);
#106963=AXIS2_PLACEMENT_3D('',#226482,#131269,#131270);
#106964=AXIS2_PLACEMENT_3D('',#226490,#131274,#131275);
#106965=AXIS2_PLACEMENT_3D('',#226496,#131278,#131279);
#106966=AXIS2_PLACEMENT_3D('',#226500,#131281,#131282);
#106967=AXIS2_PLACEMENT_3D('',#226504,#131285,#131286);
#106968=AXIS2_PLACEMENT_3D('',#226509,#131288,#131289);
#106969=AXIS2_PLACEMENT_3D('',#226512,#131291,#131292);
#106970=AXIS2_PLACEMENT_3D('',#226513,#131293,#131294);
#106971=AXIS2_PLACEMENT_3D('',#226516,#131295,#131296);
#106972=AXIS2_PLACEMENT_3D('',#226524,#131300,#131301);
#106973=AXIS2_PLACEMENT_3D('',#226530,#131304,#131305);
#106974=AXIS2_PLACEMENT_3D('',#226534,#131307,#131308);
#106975=AXIS2_PLACEMENT_3D('',#226538,#131311,#131312);
#106976=AXIS2_PLACEMENT_3D('',#226541,#131313,#131314);
#106977=AXIS2_PLACEMENT_3D('',#226549,#131318,#131319);
#106978=AXIS2_PLACEMENT_3D('',#226555,#131322,#131323);
#106979=AXIS2_PLACEMENT_3D('',#226559,#131325,#131326);
#106980=AXIS2_PLACEMENT_3D('',#226563,#131329,#131330);
#106981=AXIS2_PLACEMENT_3D('',#226568,#131332,#131333);
#106982=AXIS2_PLACEMENT_3D('',#226571,#131335,#131336);
#106983=AXIS2_PLACEMENT_3D('',#226572,#131337,#131338);
#106984=AXIS2_PLACEMENT_3D('',#226575,#131339,#131340);
#106985=AXIS2_PLACEMENT_3D('',#226583,#131344,#131345);
#106986=AXIS2_PLACEMENT_3D('',#226589,#131348,#131349);
#106987=AXIS2_PLACEMENT_3D('',#226593,#131351,#131352);
#106988=AXIS2_PLACEMENT_3D('',#226597,#131355,#131356);
#106989=AXIS2_PLACEMENT_3D('',#226600,#131357,#131358);
#106990=AXIS2_PLACEMENT_3D('',#226608,#131362,#131363);
#106991=AXIS2_PLACEMENT_3D('',#226614,#131366,#131367);
#106992=AXIS2_PLACEMENT_3D('',#226618,#131369,#131370);
#106993=AXIS2_PLACEMENT_3D('',#226622,#131373,#131374);
#106994=AXIS2_PLACEMENT_3D('',#226627,#131376,#131377);
#106995=AXIS2_PLACEMENT_3D('',#226630,#131379,#131380);
#106996=AXIS2_PLACEMENT_3D('',#226631,#131381,#131382);
#106997=AXIS2_PLACEMENT_3D('',#226634,#131383,#131384);
#106998=AXIS2_PLACEMENT_3D('',#226642,#131388,#131389);
#106999=AXIS2_PLACEMENT_3D('',#226648,#131392,#131393);
#107000=AXIS2_PLACEMENT_3D('',#226652,#131395,#131396);
#107001=AXIS2_PLACEMENT_3D('',#226656,#131399,#131400);
#107002=AXIS2_PLACEMENT_3D('',#226659,#131401,#131402);
#107003=AXIS2_PLACEMENT_3D('',#226667,#131406,#131407);
#107004=AXIS2_PLACEMENT_3D('',#226673,#131410,#131411);
#107005=AXIS2_PLACEMENT_3D('',#226677,#131413,#131414);
#107006=AXIS2_PLACEMENT_3D('',#226681,#131417,#131418);
#107007=AXIS2_PLACEMENT_3D('',#226686,#131420,#131421);
#107008=AXIS2_PLACEMENT_3D('',#226689,#131423,#131424);
#107009=AXIS2_PLACEMENT_3D('',#226690,#131425,#131426);
#107010=AXIS2_PLACEMENT_3D('',#226693,#131427,#131428);
#107011=AXIS2_PLACEMENT_3D('',#226701,#131432,#131433);
#107012=AXIS2_PLACEMENT_3D('',#226707,#131436,#131437);
#107013=AXIS2_PLACEMENT_3D('',#226711,#131439,#131440);
#107014=AXIS2_PLACEMENT_3D('',#226715,#131443,#131444);
#107015=AXIS2_PLACEMENT_3D('',#226718,#131445,#131446);
#107016=AXIS2_PLACEMENT_3D('',#226726,#131450,#131451);
#107017=AXIS2_PLACEMENT_3D('',#226732,#131454,#131455);
#107018=AXIS2_PLACEMENT_3D('',#226736,#131457,#131458);
#107019=AXIS2_PLACEMENT_3D('',#226740,#131461,#131462);
#107020=AXIS2_PLACEMENT_3D('',#226745,#131464,#131465);
#107021=AXIS2_PLACEMENT_3D('',#226748,#131467,#131468);
#107022=AXIS2_PLACEMENT_3D('',#226749,#131469,#131470);
#107023=AXIS2_PLACEMENT_3D('',#226752,#131471,#131472);
#107024=AXIS2_PLACEMENT_3D('',#226760,#131476,#131477);
#107025=AXIS2_PLACEMENT_3D('',#226766,#131480,#131481);
#107026=AXIS2_PLACEMENT_3D('',#226770,#131483,#131484);
#107027=AXIS2_PLACEMENT_3D('',#226774,#131487,#131488);
#107028=AXIS2_PLACEMENT_3D('',#226777,#131489,#131490);
#107029=AXIS2_PLACEMENT_3D('',#226785,#131494,#131495);
#107030=AXIS2_PLACEMENT_3D('',#226791,#131498,#131499);
#107031=AXIS2_PLACEMENT_3D('',#226795,#131501,#131502);
#107032=AXIS2_PLACEMENT_3D('',#226799,#131505,#131506);
#107033=AXIS2_PLACEMENT_3D('',#226804,#131508,#131509);
#107034=AXIS2_PLACEMENT_3D('',#226807,#131511,#131512);
#107035=AXIS2_PLACEMENT_3D('',#226808,#131513,#131514);
#107036=AXIS2_PLACEMENT_3D('',#226811,#131515,#131516);
#107037=AXIS2_PLACEMENT_3D('',#226819,#131520,#131521);
#107038=AXIS2_PLACEMENT_3D('',#226825,#131524,#131525);
#107039=AXIS2_PLACEMENT_3D('',#226829,#131527,#131528);
#107040=AXIS2_PLACEMENT_3D('',#226833,#131531,#131532);
#107041=AXIS2_PLACEMENT_3D('',#226836,#131533,#131534);
#107042=AXIS2_PLACEMENT_3D('',#226844,#131538,#131539);
#107043=AXIS2_PLACEMENT_3D('',#226850,#131542,#131543);
#107044=AXIS2_PLACEMENT_3D('',#226854,#131545,#131546);
#107045=AXIS2_PLACEMENT_3D('',#226858,#131549,#131550);
#107046=AXIS2_PLACEMENT_3D('',#226863,#131552,#131553);
#107047=AXIS2_PLACEMENT_3D('',#226866,#131555,#131556);
#107048=AXIS2_PLACEMENT_3D('',#226867,#131557,#131558);
#107049=AXIS2_PLACEMENT_3D('',#226870,#131559,#131560);
#107050=AXIS2_PLACEMENT_3D('',#226878,#131564,#131565);
#107051=AXIS2_PLACEMENT_3D('',#226884,#131568,#131569);
#107052=AXIS2_PLACEMENT_3D('',#226888,#131571,#131572);
#107053=AXIS2_PLACEMENT_3D('',#226892,#131575,#131576);
#107054=AXIS2_PLACEMENT_3D('',#226895,#131577,#131578);
#107055=AXIS2_PLACEMENT_3D('',#226903,#131582,#131583);
#107056=AXIS2_PLACEMENT_3D('',#226909,#131586,#131587);
#107057=AXIS2_PLACEMENT_3D('',#226913,#131589,#131590);
#107058=AXIS2_PLACEMENT_3D('',#226917,#131593,#131594);
#107059=AXIS2_PLACEMENT_3D('',#226922,#131596,#131597);
#107060=AXIS2_PLACEMENT_3D('',#226925,#131599,#131600);
#107061=AXIS2_PLACEMENT_3D('',#226926,#131601,#131602);
#107062=AXIS2_PLACEMENT_3D('',#226929,#131603,#131604);
#107063=AXIS2_PLACEMENT_3D('',#226937,#131608,#131609);
#107064=AXIS2_PLACEMENT_3D('',#226943,#131612,#131613);
#107065=AXIS2_PLACEMENT_3D('',#226947,#131615,#131616);
#107066=AXIS2_PLACEMENT_3D('',#226951,#131619,#131620);
#107067=AXIS2_PLACEMENT_3D('',#226954,#131621,#131622);
#107068=AXIS2_PLACEMENT_3D('',#226962,#131626,#131627);
#107069=AXIS2_PLACEMENT_3D('',#226968,#131630,#131631);
#107070=AXIS2_PLACEMENT_3D('',#226972,#131633,#131634);
#107071=AXIS2_PLACEMENT_3D('',#226976,#131637,#131638);
#107072=AXIS2_PLACEMENT_3D('',#226981,#131640,#131641);
#107073=AXIS2_PLACEMENT_3D('',#226984,#131643,#131644);
#107074=AXIS2_PLACEMENT_3D('',#226985,#131645,#131646);
#107075=AXIS2_PLACEMENT_3D('',#226988,#131647,#131648);
#107076=AXIS2_PLACEMENT_3D('',#226996,#131652,#131653);
#107077=AXIS2_PLACEMENT_3D('',#227002,#131656,#131657);
#107078=AXIS2_PLACEMENT_3D('',#227006,#131659,#131660);
#107079=AXIS2_PLACEMENT_3D('',#227010,#131663,#131664);
#107080=AXIS2_PLACEMENT_3D('',#227013,#131665,#131666);
#107081=AXIS2_PLACEMENT_3D('',#227021,#131670,#131671);
#107082=AXIS2_PLACEMENT_3D('',#227027,#131674,#131675);
#107083=AXIS2_PLACEMENT_3D('',#227031,#131677,#131678);
#107084=AXIS2_PLACEMENT_3D('',#227035,#131681,#131682);
#107085=AXIS2_PLACEMENT_3D('',#227040,#131684,#131685);
#107086=AXIS2_PLACEMENT_3D('',#227043,#131687,#131688);
#107087=AXIS2_PLACEMENT_3D('',#227044,#131689,#131690);
#107088=AXIS2_PLACEMENT_3D('',#227047,#131691,#131692);
#107089=AXIS2_PLACEMENT_3D('',#227055,#131696,#131697);
#107090=AXIS2_PLACEMENT_3D('',#227061,#131700,#131701);
#107091=AXIS2_PLACEMENT_3D('',#227065,#131703,#131704);
#107092=AXIS2_PLACEMENT_3D('',#227069,#131707,#131708);
#107093=AXIS2_PLACEMENT_3D('',#227072,#131709,#131710);
#107094=AXIS2_PLACEMENT_3D('',#227080,#131714,#131715);
#107095=AXIS2_PLACEMENT_3D('',#227086,#131718,#131719);
#107096=AXIS2_PLACEMENT_3D('',#227090,#131721,#131722);
#107097=AXIS2_PLACEMENT_3D('',#227094,#131725,#131726);
#107098=AXIS2_PLACEMENT_3D('',#227097,#131729,#131730);
#107099=AXIS2_PLACEMENT_3D('',#227100,#131731,#131732);
#107100=AXIS2_PLACEMENT_3D('',#227108,#131736,#131737);
#107101=AXIS2_PLACEMENT_3D('',#227114,#131740,#131741);
#107102=AXIS2_PLACEMENT_3D('',#227118,#131743,#131744);
#107103=AXIS2_PLACEMENT_3D('',#227122,#131747,#131748);
#107104=AXIS2_PLACEMENT_3D('',#227125,#131749,#131750);
#107105=AXIS2_PLACEMENT_3D('',#227133,#131754,#131755);
#107106=AXIS2_PLACEMENT_3D('',#227139,#131758,#131759);
#107107=AXIS2_PLACEMENT_3D('',#227143,#131761,#131762);
#107108=AXIS2_PLACEMENT_3D('',#227147,#131765,#131766);
#107109=AXIS2_PLACEMENT_3D('',#227152,#131768,#131769);
#107110=AXIS2_PLACEMENT_3D('',#227155,#131771,#131772);
#107111=AXIS2_PLACEMENT_3D('',#227156,#131773,#131774);
#107112=AXIS2_PLACEMENT_3D('',#227159,#131775,#131776);
#107113=AXIS2_PLACEMENT_3D('',#227167,#131780,#131781);
#107114=AXIS2_PLACEMENT_3D('',#227173,#131784,#131785);
#107115=AXIS2_PLACEMENT_3D('',#227177,#131787,#131788);
#107116=AXIS2_PLACEMENT_3D('',#227181,#131791,#131792);
#107117=AXIS2_PLACEMENT_3D('',#227184,#131793,#131794);
#107118=AXIS2_PLACEMENT_3D('',#227192,#131798,#131799);
#107119=AXIS2_PLACEMENT_3D('',#227198,#131802,#131803);
#107120=AXIS2_PLACEMENT_3D('',#227202,#131805,#131806);
#107121=AXIS2_PLACEMENT_3D('',#227206,#131809,#131810);
#107122=AXIS2_PLACEMENT_3D('',#227211,#131812,#131813);
#107123=AXIS2_PLACEMENT_3D('',#227214,#131815,#131816);
#107124=AXIS2_PLACEMENT_3D('',#227215,#131817,#131818);
#107125=AXIS2_PLACEMENT_3D('',#227218,#131819,#131820);
#107126=AXIS2_PLACEMENT_3D('',#227226,#131824,#131825);
#107127=AXIS2_PLACEMENT_3D('',#227232,#131828,#131829);
#107128=AXIS2_PLACEMENT_3D('',#227236,#131831,#131832);
#107129=AXIS2_PLACEMENT_3D('',#227240,#131835,#131836);
#107130=AXIS2_PLACEMENT_3D('',#227243,#131837,#131838);
#107131=AXIS2_PLACEMENT_3D('',#227251,#131842,#131843);
#107132=AXIS2_PLACEMENT_3D('',#227257,#131846,#131847);
#107133=AXIS2_PLACEMENT_3D('',#227261,#131849,#131850);
#107134=AXIS2_PLACEMENT_3D('',#227265,#131853,#131854);
#107135=AXIS2_PLACEMENT_3D('',#227270,#131856,#131857);
#107136=AXIS2_PLACEMENT_3D('',#227273,#131859,#131860);
#107137=AXIS2_PLACEMENT_3D('',#227274,#131861,#131862);
#107138=AXIS2_PLACEMENT_3D('',#227277,#131863,#131864);
#107139=AXIS2_PLACEMENT_3D('',#227285,#131868,#131869);
#107140=AXIS2_PLACEMENT_3D('',#227291,#131872,#131873);
#107141=AXIS2_PLACEMENT_3D('',#227295,#131875,#131876);
#107142=AXIS2_PLACEMENT_3D('',#227299,#131879,#131880);
#107143=AXIS2_PLACEMENT_3D('',#227302,#131881,#131882);
#107144=AXIS2_PLACEMENT_3D('',#227310,#131886,#131887);
#107145=AXIS2_PLACEMENT_3D('',#227316,#131890,#131891);
#107146=AXIS2_PLACEMENT_3D('',#227320,#131893,#131894);
#107147=AXIS2_PLACEMENT_3D('',#227324,#131897,#131898);
#107148=AXIS2_PLACEMENT_3D('',#227329,#131900,#131901);
#107149=AXIS2_PLACEMENT_3D('',#227332,#131903,#131904);
#107150=AXIS2_PLACEMENT_3D('',#227333,#131905,#131906);
#107151=AXIS2_PLACEMENT_3D('',#227336,#131907,#131908);
#107152=AXIS2_PLACEMENT_3D('',#227344,#131912,#131913);
#107153=AXIS2_PLACEMENT_3D('',#227350,#131916,#131917);
#107154=AXIS2_PLACEMENT_3D('',#227354,#131919,#131920);
#107155=AXIS2_PLACEMENT_3D('',#227358,#131923,#131924);
#107156=AXIS2_PLACEMENT_3D('',#227361,#131925,#131926);
#107157=AXIS2_PLACEMENT_3D('',#227369,#131930,#131931);
#107158=AXIS2_PLACEMENT_3D('',#227375,#131934,#131935);
#107159=AXIS2_PLACEMENT_3D('',#227379,#131937,#131938);
#107160=AXIS2_PLACEMENT_3D('',#227383,#131941,#131942);
#107161=AXIS2_PLACEMENT_3D('',#227388,#131944,#131945);
#107162=AXIS2_PLACEMENT_3D('',#227391,#131947,#131948);
#107163=AXIS2_PLACEMENT_3D('',#227392,#131949,#131950);
#107164=AXIS2_PLACEMENT_3D('',#227395,#131951,#131952);
#107165=AXIS2_PLACEMENT_3D('',#227403,#131956,#131957);
#107166=AXIS2_PLACEMENT_3D('',#227409,#131960,#131961);
#107167=AXIS2_PLACEMENT_3D('',#227413,#131963,#131964);
#107168=AXIS2_PLACEMENT_3D('',#227417,#131967,#131968);
#107169=AXIS2_PLACEMENT_3D('',#227420,#131969,#131970);
#107170=AXIS2_PLACEMENT_3D('',#227428,#131974,#131975);
#107171=AXIS2_PLACEMENT_3D('',#227434,#131978,#131979);
#107172=AXIS2_PLACEMENT_3D('',#227438,#131981,#131982);
#107173=AXIS2_PLACEMENT_3D('',#227442,#131985,#131986);
#107174=AXIS2_PLACEMENT_3D('',#227447,#131988,#131989);
#107175=AXIS2_PLACEMENT_3D('',#227450,#131991,#131992);
#107176=AXIS2_PLACEMENT_3D('',#227451,#131993,#131994);
#107177=AXIS2_PLACEMENT_3D('',#227454,#131995,#131996);
#107178=AXIS2_PLACEMENT_3D('',#227462,#132000,#132001);
#107179=AXIS2_PLACEMENT_3D('',#227468,#132004,#132005);
#107180=AXIS2_PLACEMENT_3D('',#227472,#132007,#132008);
#107181=AXIS2_PLACEMENT_3D('',#227476,#132011,#132012);
#107182=AXIS2_PLACEMENT_3D('',#227479,#132013,#132014);
#107183=AXIS2_PLACEMENT_3D('',#227487,#132018,#132019);
#107184=AXIS2_PLACEMENT_3D('',#227493,#132022,#132023);
#107185=AXIS2_PLACEMENT_3D('',#227497,#132025,#132026);
#107186=AXIS2_PLACEMENT_3D('',#227501,#132029,#132030);
#107187=AXIS2_PLACEMENT_3D('',#227506,#132032,#132033);
#107188=AXIS2_PLACEMENT_3D('',#227509,#132035,#132036);
#107189=AXIS2_PLACEMENT_3D('',#227510,#132037,#132038);
#107190=AXIS2_PLACEMENT_3D('',#227513,#132039,#132040);
#107191=AXIS2_PLACEMENT_3D('',#227521,#132044,#132045);
#107192=AXIS2_PLACEMENT_3D('',#227527,#132048,#132049);
#107193=AXIS2_PLACEMENT_3D('',#227531,#132051,#132052);
#107194=AXIS2_PLACEMENT_3D('',#227535,#132055,#132056);
#107195=AXIS2_PLACEMENT_3D('',#227538,#132057,#132058);
#107196=AXIS2_PLACEMENT_3D('',#227546,#132062,#132063);
#107197=AXIS2_PLACEMENT_3D('',#227552,#132066,#132067);
#107198=AXIS2_PLACEMENT_3D('',#227556,#132069,#132070);
#107199=AXIS2_PLACEMENT_3D('',#227560,#132073,#132074);
#107200=AXIS2_PLACEMENT_3D('',#227565,#132076,#132077);
#107201=AXIS2_PLACEMENT_3D('',#227568,#132079,#132080);
#107202=AXIS2_PLACEMENT_3D('',#227569,#132081,#132082);
#107203=AXIS2_PLACEMENT_3D('',#227572,#132083,#132084);
#107204=AXIS2_PLACEMENT_3D('',#227580,#132088,#132089);
#107205=AXIS2_PLACEMENT_3D('',#227586,#132092,#132093);
#107206=AXIS2_PLACEMENT_3D('',#227590,#132095,#132096);
#107207=AXIS2_PLACEMENT_3D('',#227594,#132099,#132100);
#107208=AXIS2_PLACEMENT_3D('',#227597,#132101,#132102);
#107209=AXIS2_PLACEMENT_3D('',#227605,#132106,#132107);
#107210=AXIS2_PLACEMENT_3D('',#227611,#132110,#132111);
#107211=AXIS2_PLACEMENT_3D('',#227615,#132113,#132114);
#107212=AXIS2_PLACEMENT_3D('',#227619,#132117,#132118);
#107213=AXIS2_PLACEMENT_3D('',#227624,#132120,#132121);
#107214=AXIS2_PLACEMENT_3D('',#227627,#132123,#132124);
#107215=AXIS2_PLACEMENT_3D('',#227628,#132125,#132126);
#107216=AXIS2_PLACEMENT_3D('',#227631,#132127,#132128);
#107217=AXIS2_PLACEMENT_3D('',#227639,#132132,#132133);
#107218=AXIS2_PLACEMENT_3D('',#227645,#132136,#132137);
#107219=AXIS2_PLACEMENT_3D('',#227649,#132139,#132140);
#107220=AXIS2_PLACEMENT_3D('',#227653,#132143,#132144);
#107221=AXIS2_PLACEMENT_3D('',#227656,#132145,#132146);
#107222=AXIS2_PLACEMENT_3D('',#227664,#132150,#132151);
#107223=AXIS2_PLACEMENT_3D('',#227670,#132154,#132155);
#107224=AXIS2_PLACEMENT_3D('',#227674,#132157,#132158);
#107225=AXIS2_PLACEMENT_3D('',#227678,#132161,#132162);
#107226=AXIS2_PLACEMENT_3D('',#227683,#132164,#132165);
#107227=AXIS2_PLACEMENT_3D('',#227686,#132167,#132168);
#107228=AXIS2_PLACEMENT_3D('',#227687,#132169,#132170);
#107229=AXIS2_PLACEMENT_3D('',#227690,#132171,#132172);
#107230=AXIS2_PLACEMENT_3D('',#227698,#132176,#132177);
#107231=AXIS2_PLACEMENT_3D('',#227704,#132180,#132181);
#107232=AXIS2_PLACEMENT_3D('',#227708,#132183,#132184);
#107233=AXIS2_PLACEMENT_3D('',#227712,#132187,#132188);
#107234=AXIS2_PLACEMENT_3D('',#227715,#132189,#132190);
#107235=AXIS2_PLACEMENT_3D('',#227723,#132194,#132195);
#107236=AXIS2_PLACEMENT_3D('',#227729,#132198,#132199);
#107237=AXIS2_PLACEMENT_3D('',#227733,#132201,#132202);
#107238=AXIS2_PLACEMENT_3D('',#227737,#132205,#132206);
#107239=AXIS2_PLACEMENT_3D('',#227742,#132208,#132209);
#107240=AXIS2_PLACEMENT_3D('',#227745,#132211,#132212);
#107241=AXIS2_PLACEMENT_3D('',#227746,#132213,#132214);
#107242=AXIS2_PLACEMENT_3D('',#227749,#132215,#132216);
#107243=AXIS2_PLACEMENT_3D('',#227757,#132220,#132221);
#107244=AXIS2_PLACEMENT_3D('',#227763,#132224,#132225);
#107245=AXIS2_PLACEMENT_3D('',#227767,#132227,#132228);
#107246=AXIS2_PLACEMENT_3D('',#227771,#132231,#132232);
#107247=AXIS2_PLACEMENT_3D('',#227774,#132233,#132234);
#107248=AXIS2_PLACEMENT_3D('',#227782,#132238,#132239);
#107249=AXIS2_PLACEMENT_3D('',#227788,#132242,#132243);
#107250=AXIS2_PLACEMENT_3D('',#227792,#132245,#132246);
#107251=AXIS2_PLACEMENT_3D('',#227796,#132249,#132250);
#107252=AXIS2_PLACEMENT_3D('',#227801,#132252,#132253);
#107253=AXIS2_PLACEMENT_3D('',#227804,#132255,#132256);
#107254=AXIS2_PLACEMENT_3D('',#227805,#132257,#132258);
#107255=AXIS2_PLACEMENT_3D('',#227808,#132259,#132260);
#107256=AXIS2_PLACEMENT_3D('',#227816,#132264,#132265);
#107257=AXIS2_PLACEMENT_3D('',#227822,#132268,#132269);
#107258=AXIS2_PLACEMENT_3D('',#227826,#132271,#132272);
#107259=AXIS2_PLACEMENT_3D('',#227830,#132275,#132276);
#107260=AXIS2_PLACEMENT_3D('',#227833,#132277,#132278);
#107261=AXIS2_PLACEMENT_3D('',#227841,#132282,#132283);
#107262=AXIS2_PLACEMENT_3D('',#227847,#132286,#132287);
#107263=AXIS2_PLACEMENT_3D('',#227851,#132289,#132290);
#107264=AXIS2_PLACEMENT_3D('',#227855,#132293,#132294);
#107265=AXIS2_PLACEMENT_3D('',#227860,#132296,#132297);
#107266=AXIS2_PLACEMENT_3D('',#227863,#132299,#132300);
#107267=AXIS2_PLACEMENT_3D('',#227864,#132301,#132302);
#107268=AXIS2_PLACEMENT_3D('',#227867,#132303,#132304);
#107269=AXIS2_PLACEMENT_3D('',#227875,#132308,#132309);
#107270=AXIS2_PLACEMENT_3D('',#227881,#132312,#132313);
#107271=AXIS2_PLACEMENT_3D('',#227885,#132315,#132316);
#107272=AXIS2_PLACEMENT_3D('',#227889,#132319,#132320);
#107273=AXIS2_PLACEMENT_3D('',#227892,#132321,#132322);
#107274=AXIS2_PLACEMENT_3D('',#227900,#132326,#132327);
#107275=AXIS2_PLACEMENT_3D('',#227906,#132330,#132331);
#107276=AXIS2_PLACEMENT_3D('',#227910,#132333,#132334);
#107277=AXIS2_PLACEMENT_3D('',#227914,#132337,#132338);
#107278=AXIS2_PLACEMENT_3D('',#227919,#132340,#132341);
#107279=AXIS2_PLACEMENT_3D('',#227922,#132343,#132344);
#107280=AXIS2_PLACEMENT_3D('',#227923,#132345,#132346);
#107281=AXIS2_PLACEMENT_3D('',#227926,#132347,#132348);
#107282=AXIS2_PLACEMENT_3D('',#227934,#132352,#132353);
#107283=AXIS2_PLACEMENT_3D('',#227940,#132356,#132357);
#107284=AXIS2_PLACEMENT_3D('',#227944,#132359,#132360);
#107285=AXIS2_PLACEMENT_3D('',#227948,#132363,#132364);
#107286=AXIS2_PLACEMENT_3D('',#227951,#132365,#132366);
#107287=AXIS2_PLACEMENT_3D('',#227959,#132370,#132371);
#107288=AXIS2_PLACEMENT_3D('',#227965,#132374,#132375);
#107289=AXIS2_PLACEMENT_3D('',#227969,#132377,#132378);
#107290=AXIS2_PLACEMENT_3D('',#227973,#132381,#132382);
#107291=AXIS2_PLACEMENT_3D('',#227976,#132385,#132386);
#107292=AXIS2_PLACEMENT_3D('',#227979,#132387,#132388);
#107293=AXIS2_PLACEMENT_3D('',#227987,#132392,#132393);
#107294=AXIS2_PLACEMENT_3D('',#227993,#132396,#132397);
#107295=AXIS2_PLACEMENT_3D('',#227997,#132399,#132400);
#107296=AXIS2_PLACEMENT_3D('',#228001,#132403,#132404);
#107297=AXIS2_PLACEMENT_3D('',#228004,#132405,#132406);
#107298=AXIS2_PLACEMENT_3D('',#228012,#132410,#132411);
#107299=AXIS2_PLACEMENT_3D('',#228018,#132414,#132415);
#107300=AXIS2_PLACEMENT_3D('',#228022,#132417,#132418);
#107301=AXIS2_PLACEMENT_3D('',#228026,#132421,#132422);
#107302=AXIS2_PLACEMENT_3D('',#228031,#132424,#132425);
#107303=AXIS2_PLACEMENT_3D('',#228034,#132427,#132428);
#107304=AXIS2_PLACEMENT_3D('',#228035,#132429,#132430);
#107305=AXIS2_PLACEMENT_3D('',#228038,#132431,#132432);
#107306=AXIS2_PLACEMENT_3D('',#228046,#132436,#132437);
#107307=AXIS2_PLACEMENT_3D('',#228052,#132440,#132441);
#107308=AXIS2_PLACEMENT_3D('',#228056,#132443,#132444);
#107309=AXIS2_PLACEMENT_3D('',#228060,#132447,#132448);
#107310=AXIS2_PLACEMENT_3D('',#228063,#132449,#132450);
#107311=AXIS2_PLACEMENT_3D('',#228071,#132454,#132455);
#107312=AXIS2_PLACEMENT_3D('',#228077,#132458,#132459);
#107313=AXIS2_PLACEMENT_3D('',#228081,#132461,#132462);
#107314=AXIS2_PLACEMENT_3D('',#228085,#132465,#132466);
#107315=AXIS2_PLACEMENT_3D('',#228090,#132468,#132469);
#107316=AXIS2_PLACEMENT_3D('',#228093,#132471,#132472);
#107317=AXIS2_PLACEMENT_3D('',#228094,#132473,#132474);
#107318=AXIS2_PLACEMENT_3D('',#228097,#132475,#132476);
#107319=AXIS2_PLACEMENT_3D('',#228105,#132480,#132481);
#107320=AXIS2_PLACEMENT_3D('',#228111,#132484,#132485);
#107321=AXIS2_PLACEMENT_3D('',#228115,#132487,#132488);
#107322=AXIS2_PLACEMENT_3D('',#228119,#132491,#132492);
#107323=AXIS2_PLACEMENT_3D('',#228122,#132493,#132494);
#107324=AXIS2_PLACEMENT_3D('',#228130,#132498,#132499);
#107325=AXIS2_PLACEMENT_3D('',#228136,#132502,#132503);
#107326=AXIS2_PLACEMENT_3D('',#228140,#132505,#132506);
#107327=AXIS2_PLACEMENT_3D('',#228144,#132509,#132510);
#107328=AXIS2_PLACEMENT_3D('',#228149,#132512,#132513);
#107329=AXIS2_PLACEMENT_3D('',#228152,#132515,#132516);
#107330=AXIS2_PLACEMENT_3D('',#228153,#132517,#132518);
#107331=AXIS2_PLACEMENT_3D('',#228156,#132519,#132520);
#107332=AXIS2_PLACEMENT_3D('',#228164,#132524,#132525);
#107333=AXIS2_PLACEMENT_3D('',#228170,#132528,#132529);
#107334=AXIS2_PLACEMENT_3D('',#228174,#132531,#132532);
#107335=AXIS2_PLACEMENT_3D('',#228178,#132535,#132536);
#107336=AXIS2_PLACEMENT_3D('',#228181,#132537,#132538);
#107337=AXIS2_PLACEMENT_3D('',#228189,#132542,#132543);
#107338=AXIS2_PLACEMENT_3D('',#228195,#132546,#132547);
#107339=AXIS2_PLACEMENT_3D('',#228199,#132549,#132550);
#107340=AXIS2_PLACEMENT_3D('',#228203,#132553,#132554);
#107341=AXIS2_PLACEMENT_3D('',#228208,#132556,#132557);
#107342=AXIS2_PLACEMENT_3D('',#228211,#132559,#132560);
#107343=AXIS2_PLACEMENT_3D('',#228212,#132561,#132562);
#107344=AXIS2_PLACEMENT_3D('',#228215,#132563,#132564);
#107345=AXIS2_PLACEMENT_3D('',#228223,#132568,#132569);
#107346=AXIS2_PLACEMENT_3D('',#228229,#132572,#132573);
#107347=AXIS2_PLACEMENT_3D('',#228233,#132575,#132576);
#107348=AXIS2_PLACEMENT_3D('',#228237,#132579,#132580);
#107349=AXIS2_PLACEMENT_3D('',#228240,#132581,#132582);
#107350=AXIS2_PLACEMENT_3D('',#228248,#132586,#132587);
#107351=AXIS2_PLACEMENT_3D('',#228254,#132590,#132591);
#107352=AXIS2_PLACEMENT_3D('',#228258,#132593,#132594);
#107353=AXIS2_PLACEMENT_3D('',#228262,#132597,#132598);
#107354=AXIS2_PLACEMENT_3D('',#228267,#132600,#132601);
#107355=AXIS2_PLACEMENT_3D('',#228270,#132603,#132604);
#107356=AXIS2_PLACEMENT_3D('',#228271,#132605,#132606);
#107357=AXIS2_PLACEMENT_3D('',#228274,#132607,#132608);
#107358=AXIS2_PLACEMENT_3D('',#228282,#132612,#132613);
#107359=AXIS2_PLACEMENT_3D('',#228288,#132616,#132617);
#107360=AXIS2_PLACEMENT_3D('',#228292,#132619,#132620);
#107361=AXIS2_PLACEMENT_3D('',#228296,#132623,#132624);
#107362=AXIS2_PLACEMENT_3D('',#228299,#132625,#132626);
#107363=AXIS2_PLACEMENT_3D('',#228307,#132630,#132631);
#107364=AXIS2_PLACEMENT_3D('',#228313,#132634,#132635);
#107365=AXIS2_PLACEMENT_3D('',#228317,#132637,#132638);
#107366=AXIS2_PLACEMENT_3D('',#228321,#132641,#132642);
#107367=AXIS2_PLACEMENT_3D('',#228326,#132644,#132645);
#107368=AXIS2_PLACEMENT_3D('',#228329,#132647,#132648);
#107369=AXIS2_PLACEMENT_3D('',#228330,#132649,#132650);
#107370=AXIS2_PLACEMENT_3D('',#228333,#132651,#132652);
#107371=AXIS2_PLACEMENT_3D('',#228341,#132656,#132657);
#107372=AXIS2_PLACEMENT_3D('',#228347,#132660,#132661);
#107373=AXIS2_PLACEMENT_3D('',#228351,#132663,#132664);
#107374=AXIS2_PLACEMENT_3D('',#228355,#132667,#132668);
#107375=AXIS2_PLACEMENT_3D('',#228358,#132669,#132670);
#107376=AXIS2_PLACEMENT_3D('',#228366,#132674,#132675);
#107377=AXIS2_PLACEMENT_3D('',#228372,#132678,#132679);
#107378=AXIS2_PLACEMENT_3D('',#228376,#132681,#132682);
#107379=AXIS2_PLACEMENT_3D('',#228380,#132685,#132686);
#107380=AXIS2_PLACEMENT_3D('',#228385,#132688,#132689);
#107381=AXIS2_PLACEMENT_3D('',#228388,#132691,#132692);
#107382=AXIS2_PLACEMENT_3D('',#228389,#132693,#132694);
#107383=AXIS2_PLACEMENT_3D('',#228392,#132695,#132696);
#107384=AXIS2_PLACEMENT_3D('',#228400,#132700,#132701);
#107385=AXIS2_PLACEMENT_3D('',#228406,#132704,#132705);
#107386=AXIS2_PLACEMENT_3D('',#228410,#132707,#132708);
#107387=AXIS2_PLACEMENT_3D('',#228414,#132711,#132712);
#107388=AXIS2_PLACEMENT_3D('',#228417,#132713,#132714);
#107389=AXIS2_PLACEMENT_3D('',#228425,#132718,#132719);
#107390=AXIS2_PLACEMENT_3D('',#228431,#132722,#132723);
#107391=AXIS2_PLACEMENT_3D('',#228435,#132725,#132726);
#107392=AXIS2_PLACEMENT_3D('',#228439,#132729,#132730);
#107393=AXIS2_PLACEMENT_3D('',#228444,#132732,#132733);
#107394=AXIS2_PLACEMENT_3D('',#228447,#132735,#132736);
#107395=AXIS2_PLACEMENT_3D('',#228448,#132737,#132738);
#107396=AXIS2_PLACEMENT_3D('',#228451,#132739,#132740);
#107397=AXIS2_PLACEMENT_3D('',#228459,#132744,#132745);
#107398=AXIS2_PLACEMENT_3D('',#228465,#132748,#132749);
#107399=AXIS2_PLACEMENT_3D('',#228469,#132751,#132752);
#107400=AXIS2_PLACEMENT_3D('',#228473,#132755,#132756);
#107401=AXIS2_PLACEMENT_3D('',#228476,#132757,#132758);
#107402=AXIS2_PLACEMENT_3D('',#228484,#132762,#132763);
#107403=AXIS2_PLACEMENT_3D('',#228490,#132766,#132767);
#107404=AXIS2_PLACEMENT_3D('',#228494,#132769,#132770);
#107405=AXIS2_PLACEMENT_3D('',#228498,#132773,#132774);
#107406=AXIS2_PLACEMENT_3D('',#228503,#132776,#132777);
#107407=AXIS2_PLACEMENT_3D('',#228506,#132779,#132780);
#107408=AXIS2_PLACEMENT_3D('',#228507,#132781,#132782);
#107409=AXIS2_PLACEMENT_3D('',#228510,#132783,#132784);
#107410=AXIS2_PLACEMENT_3D('',#228518,#132788,#132789);
#107411=AXIS2_PLACEMENT_3D('',#228524,#132792,#132793);
#107412=AXIS2_PLACEMENT_3D('',#228528,#132795,#132796);
#107413=AXIS2_PLACEMENT_3D('',#228532,#132799,#132800);
#107414=AXIS2_PLACEMENT_3D('',#228535,#132801,#132802);
#107415=AXIS2_PLACEMENT_3D('',#228543,#132806,#132807);
#107416=AXIS2_PLACEMENT_3D('',#228549,#132810,#132811);
#107417=AXIS2_PLACEMENT_3D('',#228553,#132813,#132814);
#107418=AXIS2_PLACEMENT_3D('',#228557,#132817,#132818);
#107419=AXIS2_PLACEMENT_3D('',#228562,#132820,#132821);
#107420=AXIS2_PLACEMENT_3D('',#228565,#132823,#132824);
#107421=AXIS2_PLACEMENT_3D('',#228566,#132825,#132826);
#107422=AXIS2_PLACEMENT_3D('',#228569,#132827,#132828);
#107423=AXIS2_PLACEMENT_3D('',#228577,#132832,#132833);
#107424=AXIS2_PLACEMENT_3D('',#228583,#132836,#132837);
#107425=AXIS2_PLACEMENT_3D('',#228587,#132839,#132840);
#107426=AXIS2_PLACEMENT_3D('',#228591,#132843,#132844);
#107427=AXIS2_PLACEMENT_3D('',#228594,#132845,#132846);
#107428=AXIS2_PLACEMENT_3D('',#228602,#132850,#132851);
#107429=AXIS2_PLACEMENT_3D('',#228608,#132854,#132855);
#107430=AXIS2_PLACEMENT_3D('',#228612,#132857,#132858);
#107431=AXIS2_PLACEMENT_3D('',#228616,#132861,#132862);
#107432=AXIS2_PLACEMENT_3D('',#228621,#132864,#132865);
#107433=AXIS2_PLACEMENT_3D('',#228624,#132867,#132868);
#107434=AXIS2_PLACEMENT_3D('',#228625,#132869,#132870);
#107435=AXIS2_PLACEMENT_3D('',#228628,#132871,#132872);
#107436=AXIS2_PLACEMENT_3D('',#228636,#132876,#132877);
#107437=AXIS2_PLACEMENT_3D('',#228642,#132880,#132881);
#107438=AXIS2_PLACEMENT_3D('',#228646,#132883,#132884);
#107439=AXIS2_PLACEMENT_3D('',#228650,#132887,#132888);
#107440=AXIS2_PLACEMENT_3D('',#228653,#132889,#132890);
#107441=AXIS2_PLACEMENT_3D('',#228661,#132894,#132895);
#107442=AXIS2_PLACEMENT_3D('',#228667,#132898,#132899);
#107443=AXIS2_PLACEMENT_3D('',#228671,#132901,#132902);
#107444=AXIS2_PLACEMENT_3D('',#228675,#132905,#132906);
#107445=AXIS2_PLACEMENT_3D('',#228680,#132908,#132909);
#107446=AXIS2_PLACEMENT_3D('',#228683,#132911,#132912);
#107447=AXIS2_PLACEMENT_3D('',#228684,#132913,#132914);
#107448=AXIS2_PLACEMENT_3D('',#228687,#132915,#132916);
#107449=AXIS2_PLACEMENT_3D('',#228695,#132920,#132921);
#107450=AXIS2_PLACEMENT_3D('',#228701,#132924,#132925);
#107451=AXIS2_PLACEMENT_3D('',#228705,#132927,#132928);
#107452=AXIS2_PLACEMENT_3D('',#228709,#132931,#132932);
#107453=AXIS2_PLACEMENT_3D('',#228712,#132933,#132934);
#107454=AXIS2_PLACEMENT_3D('',#228720,#132938,#132939);
#107455=AXIS2_PLACEMENT_3D('',#228726,#132942,#132943);
#107456=AXIS2_PLACEMENT_3D('',#228730,#132945,#132946);
#107457=AXIS2_PLACEMENT_3D('',#228734,#132949,#132950);
#107458=AXIS2_PLACEMENT_3D('',#228739,#132952,#132953);
#107459=AXIS2_PLACEMENT_3D('',#228742,#132955,#132956);
#107460=AXIS2_PLACEMENT_3D('',#228743,#132957,#132958);
#107461=AXIS2_PLACEMENT_3D('',#228746,#132959,#132960);
#107462=AXIS2_PLACEMENT_3D('',#228754,#132964,#132965);
#107463=AXIS2_PLACEMENT_3D('',#228760,#132968,#132969);
#107464=AXIS2_PLACEMENT_3D('',#228764,#132971,#132972);
#107465=AXIS2_PLACEMENT_3D('',#228768,#132975,#132976);
#107466=AXIS2_PLACEMENT_3D('',#228771,#132977,#132978);
#107467=AXIS2_PLACEMENT_3D('',#228779,#132982,#132983);
#107468=AXIS2_PLACEMENT_3D('',#228785,#132986,#132987);
#107469=AXIS2_PLACEMENT_3D('',#228789,#132989,#132990);
#107470=AXIS2_PLACEMENT_3D('',#228793,#132993,#132994);
#107471=AXIS2_PLACEMENT_3D('',#228798,#132996,#132997);
#107472=AXIS2_PLACEMENT_3D('',#228801,#132999,#133000);
#107473=AXIS2_PLACEMENT_3D('',#228802,#133001,#133002);
#107474=AXIS2_PLACEMENT_3D('',#228805,#133003,#133004);
#107475=AXIS2_PLACEMENT_3D('',#228813,#133008,#133009);
#107476=AXIS2_PLACEMENT_3D('',#228819,#133012,#133013);
#107477=AXIS2_PLACEMENT_3D('',#228823,#133015,#133016);
#107478=AXIS2_PLACEMENT_3D('',#228827,#133019,#133020);
#107479=AXIS2_PLACEMENT_3D('',#228830,#133021,#133022);
#107480=AXIS2_PLACEMENT_3D('',#228838,#133026,#133027);
#107481=AXIS2_PLACEMENT_3D('',#228844,#133030,#133031);
#107482=AXIS2_PLACEMENT_3D('',#228848,#133033,#133034);
#107483=AXIS2_PLACEMENT_3D('',#228852,#133037,#133038);
#107484=AXIS2_PLACEMENT_3D('',#228957,#133039,#133040);
#107485=AXIS2_PLACEMENT_3D('',#229056,#133041,#133042);
#107486=AXIS2_PLACEMENT_3D('',#229161,#133043,#133044);
#107487=AXIS2_PLACEMENT_3D('',#229260,#133045,#133046);
#107488=AXIS2_PLACEMENT_3D('',#229365,#133047,#133048);
#107489=AXIS2_PLACEMENT_3D('',#229464,#133049,#133050);
#107490=AXIS2_PLACEMENT_3D('',#229569,#133051,#133052);
#107491=AXIS2_PLACEMENT_3D('',#229668,#133053,#133054);
#107492=AXIS2_PLACEMENT_3D('',#229773,#133055,#133056);
#107493=AXIS2_PLACEMENT_3D('',#229872,#133057,#133058);
#107494=AXIS2_PLACEMENT_3D('',#229977,#133059,#133060);
#107495=AXIS2_PLACEMENT_3D('',#230076,#133061,#133062);
#107496=AXIS2_PLACEMENT_3D('',#230181,#133063,#133064);
#107497=AXIS2_PLACEMENT_3D('',#230280,#133065,#133066);
#107498=AXIS2_PLACEMENT_3D('',#230385,#133067,#133068);
#107499=AXIS2_PLACEMENT_3D('',#230484,#133069,#133070);
#107500=AXIS2_PLACEMENT_3D('',#230589,#133071,#133072);
#107501=AXIS2_PLACEMENT_3D('',#230688,#133073,#133074);
#107502=AXIS2_PLACEMENT_3D('',#230793,#133075,#133076);
#107503=AXIS2_PLACEMENT_3D('',#230892,#133077,#133078);
#107504=AXIS2_PLACEMENT_3D('',#230997,#133079,#133080);
#107505=AXIS2_PLACEMENT_3D('',#231096,#133081,#133082);
#107506=AXIS2_PLACEMENT_3D('',#231201,#133083,#133084);
#107507=AXIS2_PLACEMENT_3D('',#231300,#133085,#133086);
#107508=AXIS2_PLACEMENT_3D('',#231405,#133087,#133088);
#107509=AXIS2_PLACEMENT_3D('',#231504,#133089,#133090);
#107510=AXIS2_PLACEMENT_3D('',#231609,#133091,#133092);
#107511=AXIS2_PLACEMENT_3D('',#231708,#133093,#133094);
#107512=AXIS2_PLACEMENT_3D('',#231813,#133095,#133096);
#107513=AXIS2_PLACEMENT_3D('',#231912,#133097,#133098);
#107514=AXIS2_PLACEMENT_3D('',#232017,#133099,#133100);
#107515=AXIS2_PLACEMENT_3D('',#232116,#133101,#133102);
#107516=AXIS2_PLACEMENT_3D('',#232221,#133103,#133104);
#107517=AXIS2_PLACEMENT_3D('',#232320,#133105,#133106);
#107518=AXIS2_PLACEMENT_3D('',#232425,#133107,#133108);
#107519=AXIS2_PLACEMENT_3D('',#232524,#133109,#133110);
#107520=AXIS2_PLACEMENT_3D('',#232629,#133111,#133112);
#107521=AXIS2_PLACEMENT_3D('',#232728,#133113,#133114);
#107522=AXIS2_PLACEMENT_3D('',#232833,#133115,#133116);
#107523=AXIS2_PLACEMENT_3D('',#232932,#133117,#133118);
#107524=AXIS2_PLACEMENT_3D('',#233037,#133119,#133120);
#107525=AXIS2_PLACEMENT_3D('',#233136,#133121,#133122);
#107526=AXIS2_PLACEMENT_3D('',#233241,#133123,#133124);
#107527=AXIS2_PLACEMENT_3D('',#233340,#133125,#133126);
#107528=AXIS2_PLACEMENT_3D('',#233445,#133127,#133128);
#107529=AXIS2_PLACEMENT_3D('',#233544,#133129,#133130);
#107530=AXIS2_PLACEMENT_3D('',#233649,#133131,#133132);
#107531=AXIS2_PLACEMENT_3D('',#233748,#133133,#133134);
#107532=AXIS2_PLACEMENT_3D('',#233853,#133135,#133136);
#107533=AXIS2_PLACEMENT_3D('',#233952,#133137,#133138);
#107534=AXIS2_PLACEMENT_3D('',#234057,#133139,#133140);
#107535=AXIS2_PLACEMENT_3D('',#234156,#133141,#133142);
#107536=AXIS2_PLACEMENT_3D('',#234261,#133143,#133144);
#107537=AXIS2_PLACEMENT_3D('',#234360,#133145,#133146);
#107538=AXIS2_PLACEMENT_3D('',#234465,#133147,#133148);
#107539=AXIS2_PLACEMENT_3D('',#234564,#133149,#133150);
#107540=AXIS2_PLACEMENT_3D('',#234669,#133151,#133152);
#107541=AXIS2_PLACEMENT_3D('',#234768,#133153,#133154);
#107542=AXIS2_PLACEMENT_3D('',#234873,#133155,#133156);
#107543=AXIS2_PLACEMENT_3D('',#234972,#133157,#133158);
#107544=AXIS2_PLACEMENT_3D('',#235077,#133159,#133160);
#107545=AXIS2_PLACEMENT_3D('',#235176,#133161,#133162);
#107546=AXIS2_PLACEMENT_3D('',#235281,#133163,#133164);
#107547=AXIS2_PLACEMENT_3D('',#235380,#133165,#133166);
#107548=AXIS2_PLACEMENT_3D('',#235485,#133167,#133168);
#107549=AXIS2_PLACEMENT_3D('',#235584,#133169,#133170);
#107550=AXIS2_PLACEMENT_3D('',#235689,#133171,#133172);
#107551=AXIS2_PLACEMENT_3D('',#235788,#133173,#133174);
#107552=AXIS2_PLACEMENT_3D('',#235893,#133175,#133176);
#107553=AXIS2_PLACEMENT_3D('',#235992,#133177,#133178);
#107554=AXIS2_PLACEMENT_3D('',#236097,#133179,#133180);
#107555=AXIS2_PLACEMENT_3D('',#236196,#133181,#133182);
#107556=AXIS2_PLACEMENT_3D('',#236301,#133183,#133184);
#107557=AXIS2_PLACEMENT_3D('',#236400,#133185,#133186);
#107558=AXIS2_PLACEMENT_3D('',#236505,#133187,#133188);
#107559=AXIS2_PLACEMENT_3D('',#236604,#133189,#133190);
#107560=AXIS2_PLACEMENT_3D('',#236709,#133191,#133192);
#107561=AXIS2_PLACEMENT_3D('',#236808,#133193,#133194);
#107562=AXIS2_PLACEMENT_3D('',#236913,#133195,#133196);
#107563=AXIS2_PLACEMENT_3D('',#237012,#133197,#133198);
#107564=AXIS2_PLACEMENT_3D('',#237117,#133199,#133200);
#107565=AXIS2_PLACEMENT_3D('',#237216,#133201,#133202);
#107566=AXIS2_PLACEMENT_3D('',#237321,#133203,#133204);
#107567=AXIS2_PLACEMENT_3D('',#237420,#133205,#133206);
#107568=AXIS2_PLACEMENT_3D('',#237525,#133207,#133208);
#107569=AXIS2_PLACEMENT_3D('',#237624,#133209,#133210);
#107570=AXIS2_PLACEMENT_3D('',#237729,#133211,#133212);
#107571=AXIS2_PLACEMENT_3D('',#237828,#133213,#133214);
#107572=AXIS2_PLACEMENT_3D('',#237933,#133215,#133216);
#107573=AXIS2_PLACEMENT_3D('',#238032,#133217,#133218);
#107574=AXIS2_PLACEMENT_3D('',#238137,#133219,#133220);
#107575=AXIS2_PLACEMENT_3D('',#238236,#133221,#133222);
#107576=AXIS2_PLACEMENT_3D('',#238341,#133223,#133224);
#107577=AXIS2_PLACEMENT_3D('',#238440,#133225,#133226);
#107578=AXIS2_PLACEMENT_3D('',#238545,#133227,#133228);
#107579=AXIS2_PLACEMENT_3D('',#238644,#133229,#133230);
#107580=AXIS2_PLACEMENT_3D('',#238749,#133231,#133232);
#107581=AXIS2_PLACEMENT_3D('',#238848,#133233,#133234);
#107582=AXIS2_PLACEMENT_3D('',#238953,#133235,#133236);
#107583=AXIS2_PLACEMENT_3D('',#239052,#133237,#133238);
#107584=AXIS2_PLACEMENT_3D('',#239157,#133239,#133240);
#107585=AXIS2_PLACEMENT_3D('',#239256,#133241,#133242);
#107586=AXIS2_PLACEMENT_3D('',#239361,#133243,#133244);
#107587=AXIS2_PLACEMENT_3D('',#239460,#133245,#133246);
#107588=AXIS2_PLACEMENT_3D('',#239565,#133247,#133248);
#107589=AXIS2_PLACEMENT_3D('',#239664,#133249,#133250);
#107590=AXIS2_PLACEMENT_3D('',#239769,#133251,#133252);
#107591=AXIS2_PLACEMENT_3D('',#239868,#133253,#133254);
#107592=AXIS2_PLACEMENT_3D('',#239973,#133255,#133256);
#107593=AXIS2_PLACEMENT_3D('',#240072,#133257,#133258);
#107594=AXIS2_PLACEMENT_3D('',#240177,#133259,#133260);
#107595=AXIS2_PLACEMENT_3D('',#240276,#133261,#133262);
#107596=AXIS2_PLACEMENT_3D('',#240381,#133263,#133264);
#107597=AXIS2_PLACEMENT_3D('',#240480,#133265,#133266);
#107598=AXIS2_PLACEMENT_3D('',#240585,#133267,#133268);
#107599=AXIS2_PLACEMENT_3D('',#240684,#133269,#133270);
#107600=AXIS2_PLACEMENT_3D('',#240789,#133271,#133272);
#107601=AXIS2_PLACEMENT_3D('',#240888,#133273,#133274);
#107602=AXIS2_PLACEMENT_3D('',#240889,#133275,#133276);
#107603=AXIS2_PLACEMENT_3D('',#240890,#133277,#133278);
#107604=AXIS2_PLACEMENT_3D('',#240903,#133279,#133280);
#107605=AXIS2_PLACEMENT_3D('',#240904,#133281,#133282);
#107606=AXIS2_PLACEMENT_3D('',#240905,#133283,#133284);
#107607=AXIS2_PLACEMENT_3D('',#240906,#133285,#133286);
#107608=AXIS2_PLACEMENT_3D('',#240907,#133287,#133288);
#107609=AXIS2_PLACEMENT_3D('',#240920,#133289,#133290);
#107610=AXIS2_PLACEMENT_3D('',#240933,#133291,#133292);
#107611=AXIS2_PLACEMENT_3D('',#240934,#133293,#133294);
#107612=AXIS2_PLACEMENT_3D('',#240935,#133295,#133296);
#107613=AXIS2_PLACEMENT_3D('',#240936,#133297,#133298);
#107614=AXIS2_PLACEMENT_3D('',#240937,#133299,#133300);
#107615=AXIS2_PLACEMENT_3D('',#240956,#133301,#133302);
#107616=AXIS2_PLACEMENT_3D('',#240957,#133303,#133304);
#107617=AXIS2_PLACEMENT_3D('',#240958,#133305,#133306);
#107618=AXIS2_PLACEMENT_3D('',#240959,#133307,#133308);
#107619=AXIS2_PLACEMENT_3D('',#240960,#133309,#133310);
#107620=AXIS2_PLACEMENT_3D('',#240973,#133311,#133312);
#107621=AXIS2_PLACEMENT_3D('',#240992,#133313,#133314);
#107622=AXIS2_PLACEMENT_3D('',#240993,#133315,#133316);
#107623=AXIS2_PLACEMENT_3D('',#240994,#133317,#133318);
#107624=AXIS2_PLACEMENT_3D('',#240995,#133319,#133320);
#107625=AXIS2_PLACEMENT_3D('',#240996,#133321,#133322);
#107626=AXIS2_PLACEMENT_3D('',#241015,#133323,#133324);
#107627=AXIS2_PLACEMENT_3D('',#241028,#133325,#133326);
#107628=AXIS2_PLACEMENT_3D('',#241029,#133327,#133328);
#107629=AXIS2_PLACEMENT_3D('',#241030,#133329,#133330);
#107630=AXIS2_PLACEMENT_3D('',#241031,#133331,#133332);
#107631=AXIS2_PLACEMENT_3D('',#241032,#133333,#133334);
#107632=AXIS2_PLACEMENT_3D('',#241051,#133335,#133336);
#107633=AXIS2_PLACEMENT_3D('',#241052,#133337,#133338);
#107634=AXIS2_PLACEMENT_3D('',#241053,#133339,#133340);
#107635=AXIS2_PLACEMENT_3D('',#241054,#133341,#133342);
#107636=AXIS2_PLACEMENT_3D('',#241055,#133343,#133344);
#107637=AXIS2_PLACEMENT_3D('',#241068,#133345,#133346);
#107638=AXIS2_PLACEMENT_3D('',#241081,#133347,#133348);
#107639=AXIS2_PLACEMENT_3D('',#241082,#133349,#133350);
#107640=AXIS2_PLACEMENT_3D('',#241083,#133351,#133352);
#107641=AXIS2_PLACEMENT_3D('',#241084,#133353,#133354);
#107642=AXIS2_PLACEMENT_3D('',#241085,#133355,#133356);
#107643=AXIS2_PLACEMENT_3D('',#241098,#133357,#133358);
#107644=AXIS2_PLACEMENT_3D('',#241099,#133359,#133360);
#107645=AXIS2_PLACEMENT_3D('',#241100,#133361,#133362);
#107646=AXIS2_PLACEMENT_3D('',#241101,#133363,#133364);
#107647=AXIS2_PLACEMENT_3D('',#241102,#133365,#133366);
#107648=AXIS2_PLACEMENT_3D('',#241115,#133367,#133368);
#107649=AXIS2_PLACEMENT_3D('',#241116,#133369,#133370);
#107650=AXIS2_PLACEMENT_3D('',#241117,#133371,#133372);
#107651=AXIS2_PLACEMENT_3D('',#241118,#133373,#133374);
#107652=AXIS2_PLACEMENT_3D('',#241119,#133375,#133376);
#107653=AXIS2_PLACEMENT_3D('',#241132,#133377,#133378);
#107654=AXIS2_PLACEMENT_3D('',#241145,#133379,#133380);
#107655=AXIS2_PLACEMENT_3D('',#241146,#133381,#133382);
#107656=AXIS2_PLACEMENT_3D('',#241147,#133383,#133384);
#107657=AXIS2_PLACEMENT_3D('',#241148,#133385,#133386);
#107658=AXIS2_PLACEMENT_3D('',#241149,#133387,#133388);
#107659=AXIS2_PLACEMENT_3D('',#241168,#133389,#133390);
#107660=AXIS2_PLACEMENT_3D('',#241169,#133391,#133392);
#107661=AXIS2_PLACEMENT_3D('',#241170,#133393,#133394);
#107662=AXIS2_PLACEMENT_3D('',#241171,#133395,#133396);
#107663=AXIS2_PLACEMENT_3D('',#241172,#133397,#133398);
#107664=AXIS2_PLACEMENT_3D('',#241185,#133399,#133400);
#107665=AXIS2_PLACEMENT_3D('',#241204,#133401,#133402);
#107666=AXIS2_PLACEMENT_3D('',#241205,#133403,#133404);
#107667=AXIS2_PLACEMENT_3D('',#241206,#133405,#133406);
#107668=AXIS2_PLACEMENT_3D('',#241207,#133407,#133408);
#107669=AXIS2_PLACEMENT_3D('',#241208,#133409,#133410);
#107670=AXIS2_PLACEMENT_3D('',#241227,#133411,#133412);
#107671=AXIS2_PLACEMENT_3D('',#241240,#133413,#133414);
#107672=AXIS2_PLACEMENT_3D('',#241241,#133415,#133416);
#107673=AXIS2_PLACEMENT_3D('',#241242,#133417,#133418);
#107674=AXIS2_PLACEMENT_3D('',#241243,#133419,#133420);
#107675=AXIS2_PLACEMENT_3D('',#241244,#133421,#133422);
#107676=AXIS2_PLACEMENT_3D('',#241263,#133423,#133424);
#107677=AXIS2_PLACEMENT_3D('',#241264,#133425,#133426);
#107678=AXIS2_PLACEMENT_3D('',#241265,#133427,#133428);
#107679=AXIS2_PLACEMENT_3D('',#241266,#133429,#133430);
#107680=AXIS2_PLACEMENT_3D('',#241267,#133431,#133432);
#107681=AXIS2_PLACEMENT_3D('',#241280,#133433,#133434);
#107682=AXIS2_PLACEMENT_3D('',#241293,#133435,#133436);
#107683=AXIS2_PLACEMENT_3D('',#241294,#133437,#133438);
#107684=AXIS2_PLACEMENT_3D('',#241295,#133439,#133440);
#107685=AXIS2_PLACEMENT_3D('',#241296,#133441,#133442);
#107686=AXIS2_PLACEMENT_3D('',#241297,#133443,#133444);
#107687=AXIS2_PLACEMENT_3D('',#241310,#133445,#133446);
#107688=AXIS2_PLACEMENT_3D('',#241311,#133447,#133448);
#107689=AXIS2_PLACEMENT_3D('',#241312,#133449,#133450);
#107690=AXIS2_PLACEMENT_3D('',#241313,#133451,#133452);
#107691=AXIS2_PLACEMENT_3D('',#241314,#133453,#133454);
#107692=AXIS2_PLACEMENT_3D('',#241327,#133455,#133456);
#107693=AXIS2_PLACEMENT_3D('',#241328,#133457,#133458);
#107694=AXIS2_PLACEMENT_3D('',#241329,#133459,#133460);
#107695=AXIS2_PLACEMENT_3D('',#241330,#133461,#133462);
#107696=AXIS2_PLACEMENT_3D('',#241331,#133463,#133464);
#107697=AXIS2_PLACEMENT_3D('',#241344,#133465,#133466);
#107698=AXIS2_PLACEMENT_3D('',#241357,#133467,#133468);
#107699=AXIS2_PLACEMENT_3D('',#241358,#133469,#133470);
#107700=AXIS2_PLACEMENT_3D('',#241359,#133471,#133472);
#107701=AXIS2_PLACEMENT_3D('',#241360,#133473,#133474);
#107702=AXIS2_PLACEMENT_3D('',#241361,#133475,#133476);
#107703=AXIS2_PLACEMENT_3D('',#241380,#133477,#133478);
#107704=AXIS2_PLACEMENT_3D('',#241381,#133479,#133480);
#107705=AXIS2_PLACEMENT_3D('',#241382,#133481,#133482);
#107706=AXIS2_PLACEMENT_3D('',#241383,#133483,#133484);
#107707=AXIS2_PLACEMENT_3D('',#241384,#133485,#133486);
#107708=AXIS2_PLACEMENT_3D('',#241397,#133487,#133488);
#107709=AXIS2_PLACEMENT_3D('',#241416,#133489,#133490);
#107710=AXIS2_PLACEMENT_3D('',#241417,#133491,#133492);
#107711=AXIS2_PLACEMENT_3D('',#241418,#133493,#133494);
#107712=AXIS2_PLACEMENT_3D('',#241419,#133495,#133496);
#107713=AXIS2_PLACEMENT_3D('',#241420,#133497,#133498);
#107714=AXIS2_PLACEMENT_3D('',#241439,#133499,#133500);
#107715=AXIS2_PLACEMENT_3D('',#241452,#133501,#133502);
#107716=AXIS2_PLACEMENT_3D('',#241453,#133503,#133504);
#107717=AXIS2_PLACEMENT_3D('',#241454,#133505,#133506);
#107718=AXIS2_PLACEMENT_3D('',#241455,#133507,#133508);
#107719=AXIS2_PLACEMENT_3D('',#241456,#133509,#133510);
#107720=AXIS2_PLACEMENT_3D('',#241475,#133511,#133512);
#107721=AXIS2_PLACEMENT_3D('',#241476,#133513,#133514);
#107722=AXIS2_PLACEMENT_3D('',#241477,#133515,#133516);
#107723=AXIS2_PLACEMENT_3D('',#241478,#133517,#133518);
#107724=AXIS2_PLACEMENT_3D('',#241479,#133519,#133520);
#107725=AXIS2_PLACEMENT_3D('',#241492,#133521,#133522);
#107726=AXIS2_PLACEMENT_3D('',#241505,#133523,#133524);
#107727=AXIS2_PLACEMENT_3D('',#241506,#133525,#133526);
#107728=AXIS2_PLACEMENT_3D('',#241507,#133527,#133528);
#107729=AXIS2_PLACEMENT_3D('',#241508,#133529,#133530);
#107730=AXIS2_PLACEMENT_3D('',#241509,#133531,#133532);
#107731=AXIS2_PLACEMENT_3D('',#241522,#133533,#133534);
#107732=AXIS2_PLACEMENT_3D('',#241523,#133535,#133536);
#107733=AXIS2_PLACEMENT_3D('',#241524,#133537,#133538);
#107734=AXIS2_PLACEMENT_3D('',#241525,#133539,#133540);
#107735=AXIS2_PLACEMENT_3D('',#241526,#133541,#133542);
#107736=AXIS2_PLACEMENT_3D('',#241539,#133543,#133544);
#107737=AXIS2_PLACEMENT_3D('',#241540,#133545,#133546);
#107738=AXIS2_PLACEMENT_3D('',#241541,#133547,#133548);
#107739=AXIS2_PLACEMENT_3D('',#241542,#133549,#133550);
#107740=AXIS2_PLACEMENT_3D('',#241543,#133551,#133552);
#107741=AXIS2_PLACEMENT_3D('',#241556,#133553,#133554);
#107742=AXIS2_PLACEMENT_3D('',#241569,#133555,#133556);
#107743=AXIS2_PLACEMENT_3D('',#241570,#133557,#133558);
#107744=AXIS2_PLACEMENT_3D('',#241571,#133559,#133560);
#107745=AXIS2_PLACEMENT_3D('',#241572,#133561,#133562);
#107746=AXIS2_PLACEMENT_3D('',#241573,#133563,#133564);
#107747=AXIS2_PLACEMENT_3D('',#241592,#133565,#133566);
#107748=AXIS2_PLACEMENT_3D('',#241593,#133567,#133568);
#107749=AXIS2_PLACEMENT_3D('',#241594,#133569,#133570);
#107750=AXIS2_PLACEMENT_3D('',#241595,#133571,#133572);
#107751=AXIS2_PLACEMENT_3D('',#241596,#133573,#133574);
#107752=AXIS2_PLACEMENT_3D('',#241609,#133575,#133576);
#107753=AXIS2_PLACEMENT_3D('',#241628,#133577,#133578);
#107754=AXIS2_PLACEMENT_3D('',#241629,#133579,#133580);
#107755=AXIS2_PLACEMENT_3D('',#241630,#133581,#133582);
#107756=AXIS2_PLACEMENT_3D('',#241631,#133583,#133584);
#107757=AXIS2_PLACEMENT_3D('',#241632,#133585,#133586);
#107758=AXIS2_PLACEMENT_3D('',#241651,#133587,#133588);
#107759=AXIS2_PLACEMENT_3D('',#241664,#133589,#133590);
#107760=AXIS2_PLACEMENT_3D('',#241665,#133591,#133592);
#107761=AXIS2_PLACEMENT_3D('',#241666,#133593,#133594);
#107762=AXIS2_PLACEMENT_3D('',#241667,#133595,#133596);
#107763=AXIS2_PLACEMENT_3D('',#241668,#133597,#133598);
#107764=AXIS2_PLACEMENT_3D('',#241687,#133599,#133600);
#107765=AXIS2_PLACEMENT_3D('',#241688,#133601,#133602);
#107766=AXIS2_PLACEMENT_3D('',#241689,#133603,#133604);
#107767=AXIS2_PLACEMENT_3D('',#241690,#133605,#133606);
#107768=AXIS2_PLACEMENT_3D('',#241691,#133607,#133608);
#107769=AXIS2_PLACEMENT_3D('',#241704,#133609,#133610);
#107770=AXIS2_PLACEMENT_3D('',#241717,#133611,#133612);
#107771=AXIS2_PLACEMENT_3D('',#241718,#133613,#133614);
#107772=AXIS2_PLACEMENT_3D('',#241719,#133615,#133616);
#107773=AXIS2_PLACEMENT_3D('',#241720,#133617,#133618);
#107774=AXIS2_PLACEMENT_3D('',#241721,#133619,#133620);
#107775=AXIS2_PLACEMENT_3D('',#241734,#133621,#133622);
#107776=AXIS2_PLACEMENT_3D('',#241735,#133623,#133624);
#107777=AXIS2_PLACEMENT_3D('',#241736,#133625,#133626);
#107778=AXIS2_PLACEMENT_3D('',#241737,#133627,#133628);
#107779=AXIS2_PLACEMENT_3D('',#241738,#133629,#133630);
#107780=AXIS2_PLACEMENT_3D('',#241751,#133631,#133632);
#107781=AXIS2_PLACEMENT_3D('',#241752,#133633,#133634);
#107782=AXIS2_PLACEMENT_3D('',#241753,#133635,#133636);
#107783=AXIS2_PLACEMENT_3D('',#241754,#133637,#133638);
#107784=AXIS2_PLACEMENT_3D('',#241755,#133639,#133640);
#107785=AXIS2_PLACEMENT_3D('',#241768,#133641,#133642);
#107786=AXIS2_PLACEMENT_3D('',#241781,#133643,#133644);
#107787=AXIS2_PLACEMENT_3D('',#241782,#133645,#133646);
#107788=AXIS2_PLACEMENT_3D('',#241783,#133647,#133648);
#107789=AXIS2_PLACEMENT_3D('',#241784,#133649,#133650);
#107790=AXIS2_PLACEMENT_3D('',#241785,#133651,#133652);
#107791=AXIS2_PLACEMENT_3D('',#241804,#133653,#133654);
#107792=AXIS2_PLACEMENT_3D('',#241805,#133655,#133656);
#107793=AXIS2_PLACEMENT_3D('',#241806,#133657,#133658);
#107794=AXIS2_PLACEMENT_3D('',#241807,#133659,#133660);
#107795=AXIS2_PLACEMENT_3D('',#241808,#133661,#133662);
#107796=AXIS2_PLACEMENT_3D('',#241821,#133663,#133664);
#107797=AXIS2_PLACEMENT_3D('',#241840,#133665,#133666);
#107798=AXIS2_PLACEMENT_3D('',#241841,#133667,#133668);
#107799=AXIS2_PLACEMENT_3D('',#241842,#133669,#133670);
#107800=AXIS2_PLACEMENT_3D('',#241843,#133671,#133672);
#107801=AXIS2_PLACEMENT_3D('',#241844,#133673,#133674);
#107802=AXIS2_PLACEMENT_3D('',#241863,#133675,#133676);
#107803=AXIS2_PLACEMENT_3D('',#241876,#133677,#133678);
#107804=AXIS2_PLACEMENT_3D('',#241877,#133679,#133680);
#107805=AXIS2_PLACEMENT_3D('',#241878,#133681,#133682);
#107806=AXIS2_PLACEMENT_3D('',#241879,#133683,#133684);
#107807=AXIS2_PLACEMENT_3D('',#241880,#133685,#133686);
#107808=AXIS2_PLACEMENT_3D('',#241899,#133687,#133688);
#107809=AXIS2_PLACEMENT_3D('',#241900,#133689,#133690);
#107810=AXIS2_PLACEMENT_3D('',#241901,#133691,#133692);
#107811=AXIS2_PLACEMENT_3D('',#241902,#133693,#133694);
#107812=AXIS2_PLACEMENT_3D('',#241903,#133695,#133696);
#107813=AXIS2_PLACEMENT_3D('',#241916,#133697,#133698);
#107814=AXIS2_PLACEMENT_3D('',#241929,#133699,#133700);
#107815=AXIS2_PLACEMENT_3D('',#241930,#133701,#133702);
#107816=AXIS2_PLACEMENT_3D('',#241931,#133703,#133704);
#107817=AXIS2_PLACEMENT_3D('',#241932,#133705,#133706);
#107818=AXIS2_PLACEMENT_3D('',#241933,#133707,#133708);
#107819=AXIS2_PLACEMENT_3D('',#241946,#133709,#133710);
#107820=AXIS2_PLACEMENT_3D('',#241947,#133711,#133712);
#107821=AXIS2_PLACEMENT_3D('',#241948,#133713,#133714);
#107822=AXIS2_PLACEMENT_3D('',#241949,#133715,#133716);
#107823=AXIS2_PLACEMENT_3D('',#241950,#133717,#133718);
#107824=AXIS2_PLACEMENT_3D('',#241963,#133719,#133720);
#107825=AXIS2_PLACEMENT_3D('',#241964,#133721,#133722);
#107826=AXIS2_PLACEMENT_3D('',#241965,#133723,#133724);
#107827=AXIS2_PLACEMENT_3D('',#241966,#133725,#133726);
#107828=AXIS2_PLACEMENT_3D('',#241967,#133727,#133728);
#107829=AXIS2_PLACEMENT_3D('',#241980,#133729,#133730);
#107830=AXIS2_PLACEMENT_3D('',#241993,#133731,#133732);
#107831=AXIS2_PLACEMENT_3D('',#241994,#133733,#133734);
#107832=AXIS2_PLACEMENT_3D('',#241995,#133735,#133736);
#107833=AXIS2_PLACEMENT_3D('',#241996,#133737,#133738);
#107834=AXIS2_PLACEMENT_3D('',#241997,#133739,#133740);
#107835=AXIS2_PLACEMENT_3D('',#242016,#133741,#133742);
#107836=AXIS2_PLACEMENT_3D('',#242017,#133743,#133744);
#107837=AXIS2_PLACEMENT_3D('',#242018,#133745,#133746);
#107838=AXIS2_PLACEMENT_3D('',#242019,#133747,#133748);
#107839=AXIS2_PLACEMENT_3D('',#242020,#133749,#133750);
#107840=AXIS2_PLACEMENT_3D('',#242033,#133751,#133752);
#107841=AXIS2_PLACEMENT_3D('',#242052,#133753,#133754);
#107842=AXIS2_PLACEMENT_3D('',#242053,#133755,#133756);
#107843=AXIS2_PLACEMENT_3D('',#242054,#133757,#133758);
#107844=AXIS2_PLACEMENT_3D('',#242055,#133759,#133760);
#107845=AXIS2_PLACEMENT_3D('',#242056,#133761,#133762);
#107846=AXIS2_PLACEMENT_3D('',#242075,#133763,#133764);
#107847=AXIS2_PLACEMENT_3D('',#242088,#133765,#133766);
#107848=AXIS2_PLACEMENT_3D('',#242089,#133767,#133768);
#107849=AXIS2_PLACEMENT_3D('',#242090,#133769,#133770);
#107850=AXIS2_PLACEMENT_3D('',#242091,#133771,#133772);
#107851=AXIS2_PLACEMENT_3D('',#242092,#133773,#133774);
#107852=AXIS2_PLACEMENT_3D('',#242111,#133775,#133776);
#107853=AXIS2_PLACEMENT_3D('',#242112,#133777,#133778);
#107854=AXIS2_PLACEMENT_3D('',#242113,#133779,#133780);
#107855=AXIS2_PLACEMENT_3D('',#242114,#133781,#133782);
#107856=AXIS2_PLACEMENT_3D('',#242115,#133783,#133784);
#107857=AXIS2_PLACEMENT_3D('',#242128,#133785,#133786);
#107858=AXIS2_PLACEMENT_3D('',#242141,#133787,#133788);
#107859=AXIS2_PLACEMENT_3D('',#242142,#133789,#133790);
#107860=AXIS2_PLACEMENT_3D('',#242143,#133791,#133792);
#107861=AXIS2_PLACEMENT_3D('',#242144,#133793,#133794);
#107862=AXIS2_PLACEMENT_3D('',#242145,#133795,#133796);
#107863=AXIS2_PLACEMENT_3D('',#242158,#133797,#133798);
#107864=AXIS2_PLACEMENT_3D('',#242159,#133799,#133800);
#107865=AXIS2_PLACEMENT_3D('',#242160,#133801,#133802);
#107866=AXIS2_PLACEMENT_3D('',#242161,#133803,#133804);
#107867=AXIS2_PLACEMENT_3D('',#242162,#133805,#133806);
#107868=AXIS2_PLACEMENT_3D('',#242175,#133807,#133808);
#107869=AXIS2_PLACEMENT_3D('',#242176,#133809,#133810);
#107870=AXIS2_PLACEMENT_3D('',#242177,#133811,#133812);
#107871=AXIS2_PLACEMENT_3D('',#242178,#133813,#133814);
#107872=AXIS2_PLACEMENT_3D('',#242179,#133815,#133816);
#107873=AXIS2_PLACEMENT_3D('',#242192,#133817,#133818);
#107874=AXIS2_PLACEMENT_3D('',#242205,#133819,#133820);
#107875=AXIS2_PLACEMENT_3D('',#242206,#133821,#133822);
#107876=AXIS2_PLACEMENT_3D('',#242207,#133823,#133824);
#107877=AXIS2_PLACEMENT_3D('',#242208,#133825,#133826);
#107878=AXIS2_PLACEMENT_3D('',#242209,#133827,#133828);
#107879=AXIS2_PLACEMENT_3D('',#242228,#133829,#133830);
#107880=AXIS2_PLACEMENT_3D('',#242229,#133831,#133832);
#107881=AXIS2_PLACEMENT_3D('',#242230,#133833,#133834);
#107882=AXIS2_PLACEMENT_3D('',#242231,#133835,#133836);
#107883=AXIS2_PLACEMENT_3D('',#242232,#133837,#133838);
#107884=AXIS2_PLACEMENT_3D('',#242245,#133839,#133840);
#107885=AXIS2_PLACEMENT_3D('',#242264,#133841,#133842);
#107886=AXIS2_PLACEMENT_3D('',#242265,#133843,#133844);
#107887=AXIS2_PLACEMENT_3D('',#242266,#133845,#133846);
#107888=AXIS2_PLACEMENT_3D('',#242267,#133847,#133848);
#107889=AXIS2_PLACEMENT_3D('',#242268,#133849,#133850);
#107890=AXIS2_PLACEMENT_3D('',#242287,#133851,#133852);
#107891=AXIS2_PLACEMENT_3D('',#242300,#133853,#133854);
#107892=AXIS2_PLACEMENT_3D('',#242301,#133855,#133856);
#107893=AXIS2_PLACEMENT_3D('',#242302,#133857,#133858);
#107894=AXIS2_PLACEMENT_3D('',#242303,#133859,#133860);
#107895=AXIS2_PLACEMENT_3D('',#242304,#133861,#133862);
#107896=AXIS2_PLACEMENT_3D('',#242323,#133863,#133864);
#107897=AXIS2_PLACEMENT_3D('',#242324,#133865,#133866);
#107898=AXIS2_PLACEMENT_3D('',#242325,#133867,#133868);
#107899=AXIS2_PLACEMENT_3D('',#242326,#133869,#133870);
#107900=AXIS2_PLACEMENT_3D('',#242327,#133871,#133872);
#107901=AXIS2_PLACEMENT_3D('',#242340,#133873,#133874);
#107902=AXIS2_PLACEMENT_3D('',#242353,#133875,#133876);
#107903=AXIS2_PLACEMENT_3D('',#242354,#133877,#133878);
#107904=AXIS2_PLACEMENT_3D('',#242355,#133879,#133880);
#107905=AXIS2_PLACEMENT_3D('',#242356,#133881,#133882);
#107906=AXIS2_PLACEMENT_3D('',#242357,#133883,#133884);
#107907=AXIS2_PLACEMENT_3D('',#242370,#133885,#133886);
#107908=AXIS2_PLACEMENT_3D('',#242371,#133887,#133888);
#107909=AXIS2_PLACEMENT_3D('',#242372,#133889,#133890);
#107910=AXIS2_PLACEMENT_3D('',#242373,#133891,#133892);
#107911=AXIS2_PLACEMENT_3D('',#242374,#133893,#133894);
#107912=AXIS2_PLACEMENT_3D('',#242387,#133895,#133896);
#107913=AXIS2_PLACEMENT_3D('',#242388,#133897,#133898);
#107914=AXIS2_PLACEMENT_3D('',#242389,#133899,#133900);
#107915=AXIS2_PLACEMENT_3D('',#242390,#133901,#133902);
#107916=AXIS2_PLACEMENT_3D('',#242391,#133903,#133904);
#107917=AXIS2_PLACEMENT_3D('',#242404,#133905,#133906);
#107918=AXIS2_PLACEMENT_3D('',#242417,#133907,#133908);
#107919=AXIS2_PLACEMENT_3D('',#242418,#133909,#133910);
#107920=AXIS2_PLACEMENT_3D('',#242419,#133911,#133912);
#107921=AXIS2_PLACEMENT_3D('',#242420,#133913,#133914);
#107922=AXIS2_PLACEMENT_3D('',#242421,#133915,#133916);
#107923=AXIS2_PLACEMENT_3D('',#242440,#133917,#133918);
#107924=AXIS2_PLACEMENT_3D('',#242441,#133919,#133920);
#107925=AXIS2_PLACEMENT_3D('',#242442,#133921,#133922);
#107926=AXIS2_PLACEMENT_3D('',#242443,#133923,#133924);
#107927=AXIS2_PLACEMENT_3D('',#242444,#133925,#133926);
#107928=AXIS2_PLACEMENT_3D('',#242457,#133927,#133928);
#107929=AXIS2_PLACEMENT_3D('',#242476,#133929,#133930);
#107930=AXIS2_PLACEMENT_3D('',#242477,#133931,#133932);
#107931=AXIS2_PLACEMENT_3D('',#242478,#133933,#133934);
#107932=AXIS2_PLACEMENT_3D('',#242479,#133935,#133936);
#107933=AXIS2_PLACEMENT_3D('',#242480,#133937,#133938);
#107934=AXIS2_PLACEMENT_3D('',#242499,#133939,#133940);
#107935=AXIS2_PLACEMENT_3D('',#242512,#133941,#133942);
#107936=AXIS2_PLACEMENT_3D('',#242513,#133943,#133944);
#107937=AXIS2_PLACEMENT_3D('',#242514,#133945,#133946);
#107938=AXIS2_PLACEMENT_3D('',#242515,#133947,#133948);
#107939=AXIS2_PLACEMENT_3D('',#242516,#133949,#133950);
#107940=AXIS2_PLACEMENT_3D('',#242535,#133951,#133952);
#107941=AXIS2_PLACEMENT_3D('',#242536,#133953,#133954);
#107942=AXIS2_PLACEMENT_3D('',#242537,#133955,#133956);
#107943=AXIS2_PLACEMENT_3D('',#242538,#133957,#133958);
#107944=AXIS2_PLACEMENT_3D('',#242539,#133959,#133960);
#107945=AXIS2_PLACEMENT_3D('',#242552,#133961,#133962);
#107946=AXIS2_PLACEMENT_3D('',#242565,#133963,#133964);
#107947=AXIS2_PLACEMENT_3D('',#242566,#133965,#133966);
#107948=AXIS2_PLACEMENT_3D('',#242567,#133967,#133968);
#107949=AXIS2_PLACEMENT_3D('',#242568,#133969,#133970);
#107950=AXIS2_PLACEMENT_3D('',#242569,#133971,#133972);
#107951=AXIS2_PLACEMENT_3D('',#242582,#133973,#133974);
#107952=AXIS2_PLACEMENT_3D('',#242583,#133975,#133976);
#107953=AXIS2_PLACEMENT_3D('',#242584,#133977,#133978);
#107954=AXIS2_PLACEMENT_3D('',#242585,#133979,#133980);
#107955=AXIS2_PLACEMENT_3D('',#242586,#133981,#133982);
#107956=AXIS2_PLACEMENT_3D('',#242599,#133983,#133984);
#107957=AXIS2_PLACEMENT_3D('',#242600,#133985,#133986);
#107958=AXIS2_PLACEMENT_3D('',#242601,#133987,#133988);
#107959=AXIS2_PLACEMENT_3D('',#242602,#133989,#133990);
#107960=AXIS2_PLACEMENT_3D('',#242603,#133991,#133992);
#107961=AXIS2_PLACEMENT_3D('',#242616,#133993,#133994);
#107962=AXIS2_PLACEMENT_3D('',#242629,#133995,#133996);
#107963=AXIS2_PLACEMENT_3D('',#242630,#133997,#133998);
#107964=AXIS2_PLACEMENT_3D('',#242631,#133999,#134000);
#107965=AXIS2_PLACEMENT_3D('',#242632,#134001,#134002);
#107966=AXIS2_PLACEMENT_3D('',#242633,#134003,#134004);
#107967=AXIS2_PLACEMENT_3D('',#242652,#134005,#134006);
#107968=AXIS2_PLACEMENT_3D('',#242653,#134007,#134008);
#107969=AXIS2_PLACEMENT_3D('',#242654,#134009,#134010);
#107970=AXIS2_PLACEMENT_3D('',#242655,#134011,#134012);
#107971=AXIS2_PLACEMENT_3D('',#242656,#134013,#134014);
#107972=AXIS2_PLACEMENT_3D('',#242669,#134015,#134016);
#107973=AXIS2_PLACEMENT_3D('',#242688,#134017,#134018);
#107974=AXIS2_PLACEMENT_3D('',#242689,#134019,#134020);
#107975=AXIS2_PLACEMENT_3D('',#242690,#134021,#134022);
#107976=AXIS2_PLACEMENT_3D('',#242691,#134023,#134024);
#107977=AXIS2_PLACEMENT_3D('',#242692,#134025,#134026);
#107978=AXIS2_PLACEMENT_3D('',#242711,#134027,#134028);
#107979=AXIS2_PLACEMENT_3D('',#242724,#134029,#134030);
#107980=AXIS2_PLACEMENT_3D('',#242725,#134031,#134032);
#107981=AXIS2_PLACEMENT_3D('',#242726,#134033,#134034);
#107982=AXIS2_PLACEMENT_3D('',#242727,#134035,#134036);
#107983=AXIS2_PLACEMENT_3D('',#242728,#134037,#134038);
#107984=AXIS2_PLACEMENT_3D('',#242747,#134039,#134040);
#107985=AXIS2_PLACEMENT_3D('',#242748,#134041,#134042);
#107986=AXIS2_PLACEMENT_3D('',#242749,#134043,#134044);
#107987=AXIS2_PLACEMENT_3D('',#242750,#134045,#134046);
#107988=AXIS2_PLACEMENT_3D('',#242751,#134047,#134048);
#107989=AXIS2_PLACEMENT_3D('',#242764,#134049,#134050);
#107990=AXIS2_PLACEMENT_3D('',#242777,#134051,#134052);
#107991=AXIS2_PLACEMENT_3D('',#242778,#134053,#134054);
#107992=AXIS2_PLACEMENT_3D('',#242779,#134055,#134056);
#107993=AXIS2_PLACEMENT_3D('',#242780,#134057,#134058);
#107994=AXIS2_PLACEMENT_3D('',#242781,#134059,#134060);
#107995=AXIS2_PLACEMENT_3D('',#242794,#134061,#134062);
#107996=AXIS2_PLACEMENT_3D('',#242795,#134063,#134064);
#107997=AXIS2_PLACEMENT_3D('',#242796,#134065,#134066);
#107998=AXIS2_PLACEMENT_3D('',#242797,#134067,#134068);
#107999=AXIS2_PLACEMENT_3D('',#242798,#134069,#134070);
#108000=AXIS2_PLACEMENT_3D('',#242811,#134071,#134072);
#108001=AXIS2_PLACEMENT_3D('',#242812,#134073,#134074);
#108002=AXIS2_PLACEMENT_3D('',#242813,#134075,#134076);
#108003=AXIS2_PLACEMENT_3D('',#242814,#134077,#134078);
#108004=AXIS2_PLACEMENT_3D('',#242815,#134079,#134080);
#108005=AXIS2_PLACEMENT_3D('',#242828,#134081,#134082);
#108006=AXIS2_PLACEMENT_3D('',#242841,#134083,#134084);
#108007=AXIS2_PLACEMENT_3D('',#242842,#134085,#134086);
#108008=AXIS2_PLACEMENT_3D('',#242843,#134087,#134088);
#108009=AXIS2_PLACEMENT_3D('',#242844,#134089,#134090);
#108010=AXIS2_PLACEMENT_3D('',#242845,#134091,#134092);
#108011=AXIS2_PLACEMENT_3D('',#242864,#134093,#134094);
#108012=AXIS2_PLACEMENT_3D('',#242865,#134095,#134096);
#108013=AXIS2_PLACEMENT_3D('',#242866,#134097,#134098);
#108014=AXIS2_PLACEMENT_3D('',#242867,#134099,#134100);
#108015=AXIS2_PLACEMENT_3D('',#242868,#134101,#134102);
#108016=AXIS2_PLACEMENT_3D('',#242881,#134103,#134104);
#108017=AXIS2_PLACEMENT_3D('',#242900,#134105,#134106);
#108018=AXIS2_PLACEMENT_3D('',#242901,#134107,#134108);
#108019=AXIS2_PLACEMENT_3D('',#242902,#134109,#134110);
#108020=AXIS2_PLACEMENT_3D('',#242903,#134111,#134112);
#108021=AXIS2_PLACEMENT_3D('',#242904,#134113,#134114);
#108022=AXIS2_PLACEMENT_3D('',#242923,#134115,#134116);
#108023=AXIS2_PLACEMENT_3D('',#242936,#134117,#134118);
#108024=AXIS2_PLACEMENT_3D('',#242937,#134119,#134120);
#108025=AXIS2_PLACEMENT_3D('',#242938,#134121,#134122);
#108026=AXIS2_PLACEMENT_3D('',#242939,#134123,#134124);
#108027=AXIS2_PLACEMENT_3D('',#242940,#134125,#134126);
#108028=AXIS2_PLACEMENT_3D('',#242959,#134127,#134128);
#108029=AXIS2_PLACEMENT_3D('',#242960,#134129,#134130);
#108030=AXIS2_PLACEMENT_3D('',#242961,#134131,#134132);
#108031=AXIS2_PLACEMENT_3D('',#242962,#134133,#134134);
#108032=AXIS2_PLACEMENT_3D('',#242963,#134135,#134136);
#108033=AXIS2_PLACEMENT_3D('',#242976,#134137,#134138);
#108034=AXIS2_PLACEMENT_3D('',#242989,#134139,#134140);
#108035=AXIS2_PLACEMENT_3D('',#242990,#134141,#134142);
#108036=AXIS2_PLACEMENT_3D('',#242991,#134143,#134144);
#108037=AXIS2_PLACEMENT_3D('',#242992,#134145,#134146);
#108038=AXIS2_PLACEMENT_3D('',#242993,#134147,#134148);
#108039=AXIS2_PLACEMENT_3D('',#243006,#134149,#134150);
#108040=AXIS2_PLACEMENT_3D('',#243007,#134151,#134152);
#108041=AXIS2_PLACEMENT_3D('',#243008,#134153,#134154);
#108042=AXIS2_PLACEMENT_3D('',#243009,#134155,#134156);
#108043=AXIS2_PLACEMENT_3D('',#243010,#134157,#134158);
#108044=AXIS2_PLACEMENT_3D('',#243023,#134159,#134160);
#108045=AXIS2_PLACEMENT_3D('',#243024,#134161,#134162);
#108046=AXIS2_PLACEMENT_3D('',#243025,#134163,#134164);
#108047=AXIS2_PLACEMENT_3D('',#243026,#134165,#134166);
#108048=AXIS2_PLACEMENT_3D('',#243027,#134167,#134168);
#108049=AXIS2_PLACEMENT_3D('',#243040,#134169,#134170);
#108050=AXIS2_PLACEMENT_3D('',#243053,#134171,#134172);
#108051=AXIS2_PLACEMENT_3D('',#243054,#134173,#134174);
#108052=AXIS2_PLACEMENT_3D('',#243055,#134175,#134176);
#108053=AXIS2_PLACEMENT_3D('',#243056,#134177,#134178);
#108054=AXIS2_PLACEMENT_3D('',#243057,#134179,#134180);
#108055=AXIS2_PLACEMENT_3D('',#243076,#134181,#134182);
#108056=AXIS2_PLACEMENT_3D('',#243077,#134183,#134184);
#108057=AXIS2_PLACEMENT_3D('',#243078,#134185,#134186);
#108058=AXIS2_PLACEMENT_3D('',#243079,#134187,#134188);
#108059=AXIS2_PLACEMENT_3D('',#243080,#134189,#134190);
#108060=AXIS2_PLACEMENT_3D('',#243093,#134191,#134192);
#108061=AXIS2_PLACEMENT_3D('',#243112,#134193,#134194);
#108062=AXIS2_PLACEMENT_3D('',#243113,#134195,#134196);
#108063=AXIS2_PLACEMENT_3D('',#243114,#134197,#134198);
#108064=AXIS2_PLACEMENT_3D('',#243115,#134199,#134200);
#108065=AXIS2_PLACEMENT_3D('',#243116,#134201,#134202);
#108066=AXIS2_PLACEMENT_3D('',#243135,#134203,#134204);
#108067=AXIS2_PLACEMENT_3D('',#243148,#134205,#134206);
#108068=AXIS2_PLACEMENT_3D('',#243149,#134207,#134208);
#108069=AXIS2_PLACEMENT_3D('',#243150,#134209,#134210);
#108070=AXIS2_PLACEMENT_3D('',#243151,#134211,#134212);
#108071=AXIS2_PLACEMENT_3D('',#243152,#134213,#134214);
#108072=AXIS2_PLACEMENT_3D('',#243171,#134215,#134216);
#108073=AXIS2_PLACEMENT_3D('',#243172,#134217,#134218);
#108074=AXIS2_PLACEMENT_3D('',#243173,#134219,#134220);
#108075=AXIS2_PLACEMENT_3D('',#243174,#134221,#134222);
#108076=AXIS2_PLACEMENT_3D('',#243175,#134223,#134224);
#108077=AXIS2_PLACEMENT_3D('',#243188,#134225,#134226);
#108078=AXIS2_PLACEMENT_3D('',#243201,#134227,#134228);
#108079=AXIS2_PLACEMENT_3D('',#243202,#134229,#134230);
#108080=AXIS2_PLACEMENT_3D('',#243203,#134231,#134232);
#108081=AXIS2_PLACEMENT_3D('',#243204,#134233,#134234);
#108082=AXIS2_PLACEMENT_3D('',#243205,#134235,#134236);
#108083=AXIS2_PLACEMENT_3D('',#243218,#134237,#134238);
#108084=AXIS2_PLACEMENT_3D('',#243219,#134239,#134240);
#108085=AXIS2_PLACEMENT_3D('',#243220,#134241,#134242);
#108086=AXIS2_PLACEMENT_3D('',#243221,#134243,#134244);
#108087=AXIS2_PLACEMENT_3D('',#243222,#134245,#134246);
#108088=AXIS2_PLACEMENT_3D('',#243235,#134247,#134248);
#108089=AXIS2_PLACEMENT_3D('',#243236,#134249,#134250);
#108090=AXIS2_PLACEMENT_3D('',#243237,#134251,#134252);
#108091=AXIS2_PLACEMENT_3D('',#243238,#134253,#134254);
#108092=AXIS2_PLACEMENT_3D('',#243239,#134255,#134256);
#108093=AXIS2_PLACEMENT_3D('',#243252,#134257,#134258);
#108094=AXIS2_PLACEMENT_3D('',#243265,#134259,#134260);
#108095=AXIS2_PLACEMENT_3D('',#243266,#134261,#134262);
#108096=AXIS2_PLACEMENT_3D('',#243267,#134263,#134264);
#108097=AXIS2_PLACEMENT_3D('',#243268,#134265,#134266);
#108098=AXIS2_PLACEMENT_3D('',#243269,#134267,#134268);
#108099=AXIS2_PLACEMENT_3D('',#243288,#134269,#134270);
#108100=AXIS2_PLACEMENT_3D('',#243289,#134271,#134272);
#108101=AXIS2_PLACEMENT_3D('',#243290,#134273,#134274);
#108102=AXIS2_PLACEMENT_3D('',#243291,#134275,#134276);
#108103=AXIS2_PLACEMENT_3D('',#243292,#134277,#134278);
#108104=AXIS2_PLACEMENT_3D('',#243305,#134279,#134280);
#108105=AXIS2_PLACEMENT_3D('',#243324,#134281,#134282);
#108106=AXIS2_PLACEMENT_3D('',#243325,#134283,#134284);
#108107=AXIS2_PLACEMENT_3D('',#243326,#134285,#134286);
#108108=AXIS2_PLACEMENT_3D('',#243327,#134287,#134288);
#108109=AXIS2_PLACEMENT_3D('',#243328,#134289,#134290);
#108110=AXIS2_PLACEMENT_3D('',#243347,#134291,#134292);
#108111=AXIS2_PLACEMENT_3D('',#243360,#134293,#134294);
#108112=AXIS2_PLACEMENT_3D('',#243361,#134295,#134296);
#108113=AXIS2_PLACEMENT_3D('',#243362,#134297,#134298);
#108114=AXIS2_PLACEMENT_3D('',#243363,#134299,#134300);
#108115=AXIS2_PLACEMENT_3D('',#243364,#134301,#134302);
#108116=AXIS2_PLACEMENT_3D('',#243383,#134303,#134304);
#108117=AXIS2_PLACEMENT_3D('',#243384,#134305,#134306);
#108118=AXIS2_PLACEMENT_3D('',#243385,#134307,#134308);
#108119=AXIS2_PLACEMENT_3D('',#243386,#134309,#134310);
#108120=AXIS2_PLACEMENT_3D('',#243387,#134311,#134312);
#108121=AXIS2_PLACEMENT_3D('',#243400,#134313,#134314);
#108122=AXIS2_PLACEMENT_3D('',#243413,#134315,#134316);
#108123=AXIS2_PLACEMENT_3D('',#243414,#134317,#134318);
#108124=AXIS2_PLACEMENT_3D('',#243415,#134319,#134320);
#108125=AXIS2_PLACEMENT_3D('',#243416,#134321,#134322);
#108126=AXIS2_PLACEMENT_3D('',#243417,#134323,#134324);
#108127=AXIS2_PLACEMENT_3D('',#243430,#134325,#134326);
#108128=AXIS2_PLACEMENT_3D('',#243431,#134327,#134328);
#108129=AXIS2_PLACEMENT_3D('',#243432,#134329,#134330);
#108130=AXIS2_PLACEMENT_3D('',#243433,#134331,#134332);
#108131=AXIS2_PLACEMENT_3D('',#243434,#134333,#134334);
#108132=AXIS2_PLACEMENT_3D('',#243447,#134335,#134336);
#108133=AXIS2_PLACEMENT_3D('',#243448,#134337,#134338);
#108134=AXIS2_PLACEMENT_3D('',#243449,#134339,#134340);
#108135=AXIS2_PLACEMENT_3D('',#243450,#134341,#134342);
#108136=AXIS2_PLACEMENT_3D('',#243451,#134343,#134344);
#108137=AXIS2_PLACEMENT_3D('',#243464,#134345,#134346);
#108138=AXIS2_PLACEMENT_3D('',#243477,#134347,#134348);
#108139=AXIS2_PLACEMENT_3D('',#243478,#134349,#134350);
#108140=AXIS2_PLACEMENT_3D('',#243479,#134351,#134352);
#108141=AXIS2_PLACEMENT_3D('',#243480,#134353,#134354);
#108142=AXIS2_PLACEMENT_3D('',#243481,#134355,#134356);
#108143=AXIS2_PLACEMENT_3D('',#243500,#134357,#134358);
#108144=AXIS2_PLACEMENT_3D('',#243501,#134359,#134360);
#108145=AXIS2_PLACEMENT_3D('',#243502,#134361,#134362);
#108146=AXIS2_PLACEMENT_3D('',#243503,#134363,#134364);
#108147=AXIS2_PLACEMENT_3D('',#243504,#134365,#134366);
#108148=AXIS2_PLACEMENT_3D('',#243517,#134367,#134368);
#108149=AXIS2_PLACEMENT_3D('',#243536,#134369,#134370);
#108150=AXIS2_PLACEMENT_3D('',#243537,#134371,#134372);
#108151=AXIS2_PLACEMENT_3D('',#243538,#134373,#134374);
#108152=AXIS2_PLACEMENT_3D('',#243539,#134375,#134376);
#108153=AXIS2_PLACEMENT_3D('',#243540,#134377,#134378);
#108154=AXIS2_PLACEMENT_3D('',#243559,#134379,#134380);
#108155=AXIS2_PLACEMENT_3D('',#243572,#134381,#134382);
#108156=AXIS2_PLACEMENT_3D('',#243573,#134383,#134384);
#108157=AXIS2_PLACEMENT_3D('',#243574,#134385,#134386);
#108158=AXIS2_PLACEMENT_3D('',#243575,#134387,#134388);
#108159=AXIS2_PLACEMENT_3D('',#243576,#134389,#134390);
#108160=AXIS2_PLACEMENT_3D('',#243595,#134391,#134392);
#108161=AXIS2_PLACEMENT_3D('',#243596,#134393,#134394);
#108162=AXIS2_PLACEMENT_3D('',#243597,#134395,#134396);
#108163=AXIS2_PLACEMENT_3D('',#243598,#134397,#134398);
#108164=AXIS2_PLACEMENT_3D('',#243599,#134399,#134400);
#108165=AXIS2_PLACEMENT_3D('',#243612,#134401,#134402);
#108166=AXIS2_PLACEMENT_3D('',#243625,#134403,#134404);
#108167=AXIS2_PLACEMENT_3D('',#243626,#134405,#134406);
#108168=AXIS2_PLACEMENT_3D('',#243627,#134407,#134408);
#108169=AXIS2_PLACEMENT_3D('',#243628,#134409,#134410);
#108170=AXIS2_PLACEMENT_3D('',#243629,#134411,#134412);
#108171=AXIS2_PLACEMENT_3D('',#243642,#134413,#134414);
#108172=AXIS2_PLACEMENT_3D('',#243643,#134415,#134416);
#108173=AXIS2_PLACEMENT_3D('',#243644,#134417,#134418);
#108174=AXIS2_PLACEMENT_3D('',#243645,#134419,#134420);
#108175=AXIS2_PLACEMENT_3D('',#243646,#134421,#134422);
#108176=AXIS2_PLACEMENT_3D('',#243659,#134423,#134424);
#108177=AXIS2_PLACEMENT_3D('',#243660,#134425,#134426);
#108178=AXIS2_PLACEMENT_3D('',#243661,#134427,#134428);
#108179=AXIS2_PLACEMENT_3D('',#243662,#134429,#134430);
#108180=AXIS2_PLACEMENT_3D('',#243663,#134431,#134432);
#108181=AXIS2_PLACEMENT_3D('',#243676,#134433,#134434);
#108182=AXIS2_PLACEMENT_3D('',#243689,#134435,#134436);
#108183=AXIS2_PLACEMENT_3D('',#243690,#134437,#134438);
#108184=AXIS2_PLACEMENT_3D('',#243691,#134439,#134440);
#108185=AXIS2_PLACEMENT_3D('',#243692,#134441,#134442);
#108186=AXIS2_PLACEMENT_3D('',#243693,#134443,#134444);
#108187=AXIS2_PLACEMENT_3D('',#243712,#134445,#134446);
#108188=AXIS2_PLACEMENT_3D('',#243713,#134447,#134448);
#108189=AXIS2_PLACEMENT_3D('',#243714,#134449,#134450);
#108190=AXIS2_PLACEMENT_3D('',#243715,#134451,#134452);
#108191=AXIS2_PLACEMENT_3D('',#243716,#134453,#134454);
#108192=AXIS2_PLACEMENT_3D('',#243729,#134455,#134456);
#108193=AXIS2_PLACEMENT_3D('',#243748,#134457,#134458);
#108194=AXIS2_PLACEMENT_3D('',#243749,#134459,#134460);
#108195=AXIS2_PLACEMENT_3D('',#243750,#134461,#134462);
#108196=AXIS2_PLACEMENT_3D('',#243751,#134463,#134464);
#108197=AXIS2_PLACEMENT_3D('',#243752,#134465,#134466);
#108198=AXIS2_PLACEMENT_3D('',#243771,#134467,#134468);
#108199=AXIS2_PLACEMENT_3D('',#243784,#134469,#134470);
#108200=AXIS2_PLACEMENT_3D('',#243785,#134471,#134472);
#108201=AXIS2_PLACEMENT_3D('',#243786,#134473,#134474);
#108202=AXIS2_PLACEMENT_3D('',#243787,#134475,#134476);
#108203=AXIS2_PLACEMENT_3D('',#243788,#134477,#134478);
#108204=AXIS2_PLACEMENT_3D('',#243807,#134479,#134480);
#108205=AXIS2_PLACEMENT_3D('',#243808,#134481,#134482);
#108206=AXIS2_PLACEMENT_3D('',#243809,#134483,#134484);
#108207=AXIS2_PLACEMENT_3D('',#243810,#134485,#134486);
#108208=AXIS2_PLACEMENT_3D('',#243811,#134487,#134488);
#108209=AXIS2_PLACEMENT_3D('',#243824,#134489,#134490);
#108210=AXIS2_PLACEMENT_3D('',#243837,#134491,#134492);
#108211=AXIS2_PLACEMENT_3D('',#243838,#134493,#134494);
#108212=AXIS2_PLACEMENT_3D('',#243839,#134495,#134496);
#108213=AXIS2_PLACEMENT_3D('',#243840,#134497,#134498);
#108214=AXIS2_PLACEMENT_3D('',#243841,#134499,#134500);
#108215=AXIS2_PLACEMENT_3D('',#243854,#134501,#134502);
#108216=AXIS2_PLACEMENT_3D('',#243855,#134503,#134504);
#108217=AXIS2_PLACEMENT_3D('',#243856,#134505,#134506);
#108218=AXIS2_PLACEMENT_3D('',#243857,#134507,#134508);
#108219=AXIS2_PLACEMENT_3D('',#243858,#134509,#134510);
#108220=AXIS2_PLACEMENT_3D('',#243871,#134511,#134512);
#108221=AXIS2_PLACEMENT_3D('',#243872,#134513,#134514);
#108222=AXIS2_PLACEMENT_3D('',#243873,#134515,#134516);
#108223=AXIS2_PLACEMENT_3D('',#243874,#134517,#134518);
#108224=AXIS2_PLACEMENT_3D('',#243875,#134519,#134520);
#108225=AXIS2_PLACEMENT_3D('',#243888,#134521,#134522);
#108226=AXIS2_PLACEMENT_3D('',#243901,#134523,#134524);
#108227=AXIS2_PLACEMENT_3D('',#243902,#134525,#134526);
#108228=AXIS2_PLACEMENT_3D('',#243903,#134527,#134528);
#108229=AXIS2_PLACEMENT_3D('',#243904,#134529,#134530);
#108230=AXIS2_PLACEMENT_3D('',#243905,#134531,#134532);
#108231=AXIS2_PLACEMENT_3D('',#243924,#134533,#134534);
#108232=AXIS2_PLACEMENT_3D('',#243925,#134535,#134536);
#108233=AXIS2_PLACEMENT_3D('',#243926,#134537,#134538);
#108234=AXIS2_PLACEMENT_3D('',#243927,#134539,#134540);
#108235=AXIS2_PLACEMENT_3D('',#243928,#134541,#134542);
#108236=AXIS2_PLACEMENT_3D('',#243941,#134543,#134544);
#108237=AXIS2_PLACEMENT_3D('',#243960,#134545,#134546);
#108238=AXIS2_PLACEMENT_3D('',#243961,#134547,#134548);
#108239=AXIS2_PLACEMENT_3D('',#243962,#134549,#134550);
#108240=AXIS2_PLACEMENT_3D('',#243963,#134551,#134552);
#108241=AXIS2_PLACEMENT_3D('',#243964,#134553,#134554);
#108242=AXIS2_PLACEMENT_3D('',#243983,#134555,#134556);
#108243=AXIS2_PLACEMENT_3D('',#243996,#134557,#134558);
#108244=AXIS2_PLACEMENT_3D('',#243997,#134559,#134560);
#108245=AXIS2_PLACEMENT_3D('',#243998,#134561,#134562);
#108246=AXIS2_PLACEMENT_3D('',#243999,#134563,#134564);
#108247=AXIS2_PLACEMENT_3D('',#244000,#134565,#134566);
#108248=AXIS2_PLACEMENT_3D('',#244019,#134567,#134568);
#108249=AXIS2_PLACEMENT_3D('',#244020,#134569,#134570);
#108250=AXIS2_PLACEMENT_3D('',#244021,#134571,#134572);
#108251=AXIS2_PLACEMENT_3D('',#244022,#134573,#134574);
#108252=AXIS2_PLACEMENT_3D('',#244023,#134575,#134576);
#108253=AXIS2_PLACEMENT_3D('',#244036,#134577,#134578);
#108254=AXIS2_PLACEMENT_3D('',#244049,#134579,#134580);
#108255=AXIS2_PLACEMENT_3D('',#244050,#134581,#134582);
#108256=AXIS2_PLACEMENT_3D('',#244051,#134583,#134584);
#108257=AXIS2_PLACEMENT_3D('',#244052,#134585,#134586);
#108258=AXIS2_PLACEMENT_3D('',#244053,#134587,#134588);
#108259=AXIS2_PLACEMENT_3D('',#244066,#134589,#134590);
#108260=AXIS2_PLACEMENT_3D('',#244067,#134591,#134592);
#108261=AXIS2_PLACEMENT_3D('',#244068,#134593,#134594);
#108262=AXIS2_PLACEMENT_3D('',#244069,#134595,#134596);
#108263=AXIS2_PLACEMENT_3D('',#244070,#134597,#134598);
#108264=AXIS2_PLACEMENT_3D('',#244083,#134599,#134600);
#108265=AXIS2_PLACEMENT_3D('',#244084,#134601,#134602);
#108266=AXIS2_PLACEMENT_3D('',#244085,#134603,#134604);
#108267=AXIS2_PLACEMENT_3D('',#244086,#134605,#134606);
#108268=AXIS2_PLACEMENT_3D('',#244087,#134607,#134608);
#108269=AXIS2_PLACEMENT_3D('',#244100,#134609,#134610);
#108270=AXIS2_PLACEMENT_3D('',#244113,#134611,#134612);
#108271=AXIS2_PLACEMENT_3D('',#244114,#134613,#134614);
#108272=AXIS2_PLACEMENT_3D('',#244115,#134615,#134616);
#108273=AXIS2_PLACEMENT_3D('',#244116,#134617,#134618);
#108274=AXIS2_PLACEMENT_3D('',#244117,#134619,#134620);
#108275=AXIS2_PLACEMENT_3D('',#244136,#134621,#134622);
#108276=AXIS2_PLACEMENT_3D('',#244137,#134623,#134624);
#108277=AXIS2_PLACEMENT_3D('',#244138,#134625,#134626);
#108278=AXIS2_PLACEMENT_3D('',#244139,#134627,#134628);
#108279=AXIS2_PLACEMENT_3D('',#244140,#134629,#134630);
#108280=AXIS2_PLACEMENT_3D('',#244153,#134631,#134632);
#108281=AXIS2_PLACEMENT_3D('',#244172,#134633,#134634);
#108282=AXIS2_PLACEMENT_3D('',#244173,#134635,#134636);
#108283=AXIS2_PLACEMENT_3D('',#244174,#134637,#134638);
#108284=AXIS2_PLACEMENT_3D('',#244175,#134639,#134640);
#108285=AXIS2_PLACEMENT_3D('',#244176,#134641,#134642);
#108286=AXIS2_PLACEMENT_3D('',#244195,#134643,#134644);
#108287=AXIS2_PLACEMENT_3D('',#244208,#134645,#134646);
#108288=AXIS2_PLACEMENT_3D('',#244209,#134647,#134648);
#108289=AXIS2_PLACEMENT_3D('',#244210,#134649,#134650);
#108290=AXIS2_PLACEMENT_3D('',#244211,#134651,#134652);
#108291=AXIS2_PLACEMENT_3D('',#244212,#134653,#134654);
#108292=AXIS2_PLACEMENT_3D('',#244231,#134655,#134656);
#108293=AXIS2_PLACEMENT_3D('',#244232,#134657,#134658);
#108294=AXIS2_PLACEMENT_3D('',#244233,#134659,#134660);
#108295=AXIS2_PLACEMENT_3D('',#244234,#134661,#134662);
#108296=AXIS2_PLACEMENT_3D('',#244235,#134663,#134664);
#108297=AXIS2_PLACEMENT_3D('',#244248,#134665,#134666);
#108298=AXIS2_PLACEMENT_3D('',#244261,#134667,#134668);
#108299=AXIS2_PLACEMENT_3D('',#244262,#134669,#134670);
#108300=AXIS2_PLACEMENT_3D('',#244263,#134671,#134672);
#108301=AXIS2_PLACEMENT_3D('',#244264,#134673,#134674);
#108302=AXIS2_PLACEMENT_3D('',#244265,#134675,#134676);
#108303=AXIS2_PLACEMENT_3D('',#244278,#134677,#134678);
#108304=AXIS2_PLACEMENT_3D('',#244279,#134679,#134680);
#108305=AXIS2_PLACEMENT_3D('',#244280,#134681,#134682);
#108306=AXIS2_PLACEMENT_3D('',#244281,#134683,#134684);
#108307=AXIS2_PLACEMENT_3D('',#244282,#134685,#134686);
#108308=AXIS2_PLACEMENT_3D('',#244295,#134687,#134688);
#108309=AXIS2_PLACEMENT_3D('',#244296,#134689,#134690);
#108310=AXIS2_PLACEMENT_3D('',#244297,#134691,#134692);
#108311=AXIS2_PLACEMENT_3D('',#244298,#134693,#134694);
#108312=AXIS2_PLACEMENT_3D('',#244299,#134695,#134696);
#108313=AXIS2_PLACEMENT_3D('',#244312,#134697,#134698);
#108314=AXIS2_PLACEMENT_3D('',#244325,#134699,#134700);
#108315=AXIS2_PLACEMENT_3D('',#244326,#134701,#134702);
#108316=AXIS2_PLACEMENT_3D('',#244327,#134703,#134704);
#108317=AXIS2_PLACEMENT_3D('',#244328,#134705,#134706);
#108318=AXIS2_PLACEMENT_3D('',#244329,#134707,#134708);
#108319=AXIS2_PLACEMENT_3D('',#244348,#134709,#134710);
#108320=AXIS2_PLACEMENT_3D('',#244349,#134711,#134712);
#108321=AXIS2_PLACEMENT_3D('',#244350,#134713,#134714);
#108322=AXIS2_PLACEMENT_3D('',#244351,#134715,#134716);
#108323=AXIS2_PLACEMENT_3D('',#244352,#134717,#134718);
#108324=AXIS2_PLACEMENT_3D('',#244365,#134719,#134720);
#108325=AXIS2_PLACEMENT_3D('',#244384,#134721,#134722);
#108326=AXIS2_PLACEMENT_3D('',#244385,#134723,#134724);
#108327=AXIS2_PLACEMENT_3D('',#244386,#134725,#134726);
#108328=AXIS2_PLACEMENT_3D('',#244387,#134727,#134728);
#108329=AXIS2_PLACEMENT_3D('',#244388,#134729,#134730);
#108330=AXIS2_PLACEMENT_3D('',#244407,#134731,#134732);
#108331=AXIS2_PLACEMENT_3D('',#244420,#134733,#134734);
#108332=AXIS2_PLACEMENT_3D('',#244421,#134735,#134736);
#108333=AXIS2_PLACEMENT_3D('',#244422,#134737,#134738);
#108334=AXIS2_PLACEMENT_3D('',#244423,#134739,#134740);
#108335=AXIS2_PLACEMENT_3D('',#244424,#134741,#134742);
#108336=AXIS2_PLACEMENT_3D('',#244443,#134743,#134744);
#108337=AXIS2_PLACEMENT_3D('',#244444,#134745,#134746);
#108338=AXIS2_PLACEMENT_3D('',#244445,#134747,#134748);
#108339=AXIS2_PLACEMENT_3D('',#244446,#134749,#134750);
#108340=AXIS2_PLACEMENT_3D('',#244447,#134751,#134752);
#108341=AXIS2_PLACEMENT_3D('',#244460,#134753,#134754);
#108342=AXIS2_PLACEMENT_3D('',#244473,#134755,#134756);
#108343=AXIS2_PLACEMENT_3D('',#244474,#134757,#134758);
#108344=AXIS2_PLACEMENT_3D('',#244475,#134759,#134760);
#108345=AXIS2_PLACEMENT_3D('',#244476,#134761,#134762);
#108346=AXIS2_PLACEMENT_3D('',#244477,#134763,#134764);
#108347=AXIS2_PLACEMENT_3D('',#244490,#134765,#134766);
#108348=AXIS2_PLACEMENT_3D('',#244491,#134767,#134768);
#108349=AXIS2_PLACEMENT_3D('',#244492,#134769,#134770);
#108350=AXIS2_PLACEMENT_3D('',#244493,#134771,#134772);
#108351=AXIS2_PLACEMENT_3D('',#244494,#134773,#134774);
#108352=AXIS2_PLACEMENT_3D('',#244507,#134775,#134776);
#108353=AXIS2_PLACEMENT_3D('',#244508,#134777,#134778);
#108354=AXIS2_PLACEMENT_3D('',#244509,#134779,#134780);
#108355=AXIS2_PLACEMENT_3D('',#244510,#134781,#134782);
#108356=AXIS2_PLACEMENT_3D('',#244511,#134783,#134784);
#108357=AXIS2_PLACEMENT_3D('',#244524,#134785,#134786);
#108358=AXIS2_PLACEMENT_3D('',#244537,#134787,#134788);
#108359=AXIS2_PLACEMENT_3D('',#244538,#134789,#134790);
#108360=AXIS2_PLACEMENT_3D('',#244539,#134791,#134792);
#108361=AXIS2_PLACEMENT_3D('',#244540,#134793,#134794);
#108362=AXIS2_PLACEMENT_3D('',#244541,#134795,#134796);
#108363=AXIS2_PLACEMENT_3D('',#244560,#134797,#134798);
#108364=AXIS2_PLACEMENT_3D('',#244561,#134799,#134800);
#108365=AXIS2_PLACEMENT_3D('',#244562,#134801,#134802);
#108366=AXIS2_PLACEMENT_3D('',#244563,#134803,#134804);
#108367=AXIS2_PLACEMENT_3D('',#244564,#134805,#134806);
#108368=AXIS2_PLACEMENT_3D('',#244577,#134807,#134808);
#108369=AXIS2_PLACEMENT_3D('',#244596,#134809,#134810);
#108370=AXIS2_PLACEMENT_3D('',#244597,#134811,#134812);
#108371=AXIS2_PLACEMENT_3D('',#244598,#134813,#134814);
#108372=AXIS2_PLACEMENT_3D('',#244599,#134815,#134816);
#108373=AXIS2_PLACEMENT_3D('',#244600,#134817,#134818);
#108374=AXIS2_PLACEMENT_3D('',#244619,#134819,#134820);
#108375=AXIS2_PLACEMENT_3D('',#244632,#134821,#134822);
#108376=AXIS2_PLACEMENT_3D('',#244633,#134823,#134824);
#108377=AXIS2_PLACEMENT_3D('',#244634,#134825,#134826);
#108378=AXIS2_PLACEMENT_3D('',#244635,#134827,#134828);
#108379=AXIS2_PLACEMENT_3D('',#244636,#134829,#134830);
#108380=AXIS2_PLACEMENT_3D('',#244655,#134831,#134832);
#108381=AXIS2_PLACEMENT_3D('',#244656,#134833,#134834);
#108382=AXIS2_PLACEMENT_3D('',#244657,#134835,#134836);
#108383=AXIS2_PLACEMENT_3D('',#244658,#134837,#134838);
#108384=AXIS2_PLACEMENT_3D('',#244659,#134839,#134840);
#108385=AXIS2_PLACEMENT_3D('',#244672,#134841,#134842);
#108386=AXIS2_PLACEMENT_3D('',#244685,#134843,#134844);
#108387=AXIS2_PLACEMENT_3D('',#244686,#134845,#134846);
#108388=AXIS2_PLACEMENT_3D('',#244687,#134847,#134848);
#108389=AXIS2_PLACEMENT_3D('',#244688,#134849,#134850);
#108390=AXIS2_PLACEMENT_3D('',#244689,#134851,#134852);
#108391=AXIS2_PLACEMENT_3D('',#244702,#134853,#134854);
#108392=AXIS2_PLACEMENT_3D('',#244703,#134855,#134856);
#108393=AXIS2_PLACEMENT_3D('',#244704,#134857,#134858);
#108394=AXIS2_PLACEMENT_3D('',#244705,#134859,#134860);
#108395=AXIS2_PLACEMENT_3D('',#244706,#134861,#134862);
#108396=AXIS2_PLACEMENT_3D('',#244719,#134863,#134864);
#108397=AXIS2_PLACEMENT_3D('',#244720,#134865,#134866);
#108398=AXIS2_PLACEMENT_3D('',#244721,#134867,#134868);
#108399=AXIS2_PLACEMENT_3D('',#244722,#134869,#134870);
#108400=AXIS2_PLACEMENT_3D('',#244723,#134871,#134872);
#108401=AXIS2_PLACEMENT_3D('',#244736,#134873,#134874);
#108402=AXIS2_PLACEMENT_3D('',#244749,#134875,#134876);
#108403=AXIS2_PLACEMENT_3D('',#244750,#134877,#134878);
#108404=AXIS2_PLACEMENT_3D('',#244751,#134879,#134880);
#108405=AXIS2_PLACEMENT_3D('',#244752,#134881,#134882);
#108406=AXIS2_PLACEMENT_3D('',#244753,#134883,#134884);
#108407=AXIS2_PLACEMENT_3D('',#244772,#134885,#134886);
#108408=AXIS2_PLACEMENT_3D('',#244773,#134887,#134888);
#108409=AXIS2_PLACEMENT_3D('',#244774,#134889,#134890);
#108410=AXIS2_PLACEMENT_3D('',#244775,#134891,#134892);
#108411=AXIS2_PLACEMENT_3D('',#244776,#134893,#134894);
#108412=AXIS2_PLACEMENT_3D('',#244789,#134895,#134896);
#108413=AXIS2_PLACEMENT_3D('',#244808,#134897,#134898);
#108414=AXIS2_PLACEMENT_3D('',#244809,#134899,#134900);
#108415=AXIS2_PLACEMENT_3D('',#244810,#134901,#134902);
#108416=AXIS2_PLACEMENT_3D('',#244811,#134903,#134904);
#108417=AXIS2_PLACEMENT_3D('',#244812,#134905,#134906);
#108418=AXIS2_PLACEMENT_3D('',#244831,#134907,#134908);
#108419=AXIS2_PLACEMENT_3D('',#244844,#134909,#134910);
#108420=AXIS2_PLACEMENT_3D('',#244845,#134911,#134912);
#108421=AXIS2_PLACEMENT_3D('',#244846,#134913,#134914);
#108422=AXIS2_PLACEMENT_3D('',#244847,#134915,#134916);
#108423=AXIS2_PLACEMENT_3D('',#244848,#134917,#134918);
#108424=AXIS2_PLACEMENT_3D('',#244867,#134919,#134920);
#108425=AXIS2_PLACEMENT_3D('',#244868,#134921,#134922);
#108426=AXIS2_PLACEMENT_3D('',#244869,#134923,#134924);
#108427=AXIS2_PLACEMENT_3D('',#244870,#134925,#134926);
#108428=AXIS2_PLACEMENT_3D('',#244871,#134927,#134928);
#108429=AXIS2_PLACEMENT_3D('',#244884,#134929,#134930);
#108430=AXIS2_PLACEMENT_3D('',#244897,#134931,#134932);
#108431=AXIS2_PLACEMENT_3D('',#244898,#134933,#134934);
#108432=AXIS2_PLACEMENT_3D('',#244899,#134935,#134936);
#108433=AXIS2_PLACEMENT_3D('',#244900,#134937,#134938);
#108434=AXIS2_PLACEMENT_3D('',#244901,#134939,#134940);
#108435=AXIS2_PLACEMENT_3D('',#244914,#134941,#134942);
#108436=AXIS2_PLACEMENT_3D('',#244915,#134943,#134944);
#108437=AXIS2_PLACEMENT_3D('',#244916,#134945,#134946);
#108438=AXIS2_PLACEMENT_3D('',#244917,#134947,#134948);
#108439=AXIS2_PLACEMENT_3D('',#244918,#134949,#134950);
#108440=AXIS2_PLACEMENT_3D('',#244931,#134951,#134952);
#108441=AXIS2_PLACEMENT_3D('',#244932,#134953,#134954);
#108442=AXIS2_PLACEMENT_3D('',#244933,#134955,#134956);
#108443=AXIS2_PLACEMENT_3D('',#244934,#134957,#134958);
#108444=AXIS2_PLACEMENT_3D('',#244935,#134959,#134960);
#108445=AXIS2_PLACEMENT_3D('',#244948,#134961,#134962);
#108446=AXIS2_PLACEMENT_3D('',#244961,#134963,#134964);
#108447=AXIS2_PLACEMENT_3D('',#244962,#134965,#134966);
#108448=AXIS2_PLACEMENT_3D('',#244963,#134967,#134968);
#108449=AXIS2_PLACEMENT_3D('',#244964,#134969,#134970);
#108450=AXIS2_PLACEMENT_3D('',#244965,#134971,#134972);
#108451=AXIS2_PLACEMENT_3D('',#244984,#134973,#134974);
#108452=AXIS2_PLACEMENT_3D('',#244985,#134975,#134976);
#108453=AXIS2_PLACEMENT_3D('',#244986,#134977,#134978);
#108454=AXIS2_PLACEMENT_3D('',#244987,#134979,#134980);
#108455=AXIS2_PLACEMENT_3D('',#244988,#134981,#134982);
#108456=AXIS2_PLACEMENT_3D('',#245001,#134983,#134984);
#108457=AXIS2_PLACEMENT_3D('',#245020,#134985,#134986);
#108458=AXIS2_PLACEMENT_3D('',#245021,#134987,#134988);
#108459=AXIS2_PLACEMENT_3D('',#245022,#134989,#134990);
#108460=AXIS2_PLACEMENT_3D('',#245023,#134991,#134992);
#108461=AXIS2_PLACEMENT_3D('',#245024,#134993,#134994);
#108462=AXIS2_PLACEMENT_3D('',#245043,#134995,#134996);
#108463=AXIS2_PLACEMENT_3D('',#245056,#134997,#134998);
#108464=AXIS2_PLACEMENT_3D('',#245057,#134999,#135000);
#108465=AXIS2_PLACEMENT_3D('',#245058,#135001,#135002);
#108466=AXIS2_PLACEMENT_3D('',#245059,#135003,#135004);
#108467=AXIS2_PLACEMENT_3D('',#245060,#135005,#135006);
#108468=AXIS2_PLACEMENT_3D('',#245079,#135007,#135008);
#108469=AXIS2_PLACEMENT_3D('',#245080,#135009,#135010);
#108470=AXIS2_PLACEMENT_3D('',#245081,#135011,#135012);
#108471=AXIS2_PLACEMENT_3D('',#245082,#135013,#135014);
#108472=AXIS2_PLACEMENT_3D('',#245083,#135015,#135016);
#108473=AXIS2_PLACEMENT_3D('',#245096,#135017,#135018);
#108474=AXIS2_PLACEMENT_3D('',#245109,#135019,#135020);
#108475=AXIS2_PLACEMENT_3D('',#245110,#135021,#135022);
#108476=AXIS2_PLACEMENT_3D('',#245111,#135023,#135024);
#108477=AXIS2_PLACEMENT_3D('',#245112,#135025,#135026);
#108478=AXIS2_PLACEMENT_3D('',#245113,#135027,#135028);
#108479=AXIS2_PLACEMENT_3D('',#245126,#135029,#135030);
#108480=AXIS2_PLACEMENT_3D('',#245127,#135031,#135032);
#108481=AXIS2_PLACEMENT_3D('',#245128,#135033,#135034);
#108482=AXIS2_PLACEMENT_3D('',#245129,#135035,#135036);
#108483=AXIS2_PLACEMENT_3D('',#245130,#135037,#135038);
#108484=AXIS2_PLACEMENT_3D('',#245143,#135039,#135040);
#108485=AXIS2_PLACEMENT_3D('',#245144,#135041,#135042);
#108486=AXIS2_PLACEMENT_3D('',#245145,#135043,#135044);
#108487=AXIS2_PLACEMENT_3D('',#245146,#135045,#135046);
#108488=AXIS2_PLACEMENT_3D('',#245147,#135047,#135048);
#108489=AXIS2_PLACEMENT_3D('',#245160,#135049,#135050);
#108490=AXIS2_PLACEMENT_3D('',#245173,#135051,#135052);
#108491=AXIS2_PLACEMENT_3D('',#245174,#135053,#135054);
#108492=AXIS2_PLACEMENT_3D('',#245175,#135055,#135056);
#108493=AXIS2_PLACEMENT_3D('',#245176,#135057,#135058);
#108494=AXIS2_PLACEMENT_3D('',#245177,#135059,#135060);
#108495=AXIS2_PLACEMENT_3D('',#245196,#135061,#135062);
#108496=AXIS2_PLACEMENT_3D('',#245197,#135063,#135064);
#108497=AXIS2_PLACEMENT_3D('',#245198,#135065,#135066);
#108498=AXIS2_PLACEMENT_3D('',#245199,#135067,#135068);
#108499=AXIS2_PLACEMENT_3D('',#245200,#135069,#135070);
#108500=AXIS2_PLACEMENT_3D('',#245213,#135071,#135072);
#108501=AXIS2_PLACEMENT_3D('',#245232,#135073,#135074);
#108502=AXIS2_PLACEMENT_3D('',#245233,#135075,#135076);
#108503=AXIS2_PLACEMENT_3D('',#245234,#135077,#135078);
#108504=AXIS2_PLACEMENT_3D('',#245235,#135079,#135080);
#108505=AXIS2_PLACEMENT_3D('',#245236,#135081,#135082);
#108506=AXIS2_PLACEMENT_3D('',#245255,#135083,#135084);
#108507=AXIS2_PLACEMENT_3D('',#245268,#135085,#135086);
#108508=AXIS2_PLACEMENT_3D('',#245269,#135087,#135088);
#108509=AXIS2_PLACEMENT_3D('',#245270,#135089,#135090);
#108510=AXIS2_PLACEMENT_3D('',#245271,#135091,#135092);
#108511=AXIS2_PLACEMENT_3D('',#245272,#135093,#135094);
#108512=AXIS2_PLACEMENT_3D('',#245291,#135095,#135096);
#108513=AXIS2_PLACEMENT_3D('',#245292,#135097,#135098);
#108514=AXIS2_PLACEMENT_3D('',#245293,#135099,#135100);
#108515=AXIS2_PLACEMENT_3D('',#245294,#135101,#135102);
#108516=AXIS2_PLACEMENT_3D('',#245295,#135103,#135104);
#108517=AXIS2_PLACEMENT_3D('',#245308,#135105,#135106);
#108518=AXIS2_PLACEMENT_3D('',#245321,#135107,#135108);
#108519=AXIS2_PLACEMENT_3D('',#245322,#135109,#135110);
#108520=AXIS2_PLACEMENT_3D('',#245323,#135111,#135112);
#108521=AXIS2_PLACEMENT_3D('',#245324,#135113,#135114);
#108522=AXIS2_PLACEMENT_3D('',#245325,#135115,#135116);
#108523=AXIS2_PLACEMENT_3D('',#245338,#135117,#135118);
#108524=AXIS2_PLACEMENT_3D('',#245339,#135119,#135120);
#108525=AXIS2_PLACEMENT_3D('',#245340,#135121,#135122);
#108526=AXIS2_PLACEMENT_3D('',#245341,#135123,#135124);
#108527=AXIS2_PLACEMENT_3D('',#245342,#135125,#135126);
#108528=AXIS2_PLACEMENT_3D('',#245355,#135127,#135128);
#108529=AXIS2_PLACEMENT_3D('',#245356,#135129,#135130);
#108530=AXIS2_PLACEMENT_3D('',#245357,#135131,#135132);
#108531=AXIS2_PLACEMENT_3D('',#245358,#135133,#135134);
#108532=AXIS2_PLACEMENT_3D('',#245359,#135135,#135136);
#108533=AXIS2_PLACEMENT_3D('',#245372,#135137,#135138);
#108534=AXIS2_PLACEMENT_3D('',#245385,#135139,#135140);
#108535=AXIS2_PLACEMENT_3D('',#245386,#135141,#135142);
#108536=AXIS2_PLACEMENT_3D('',#245387,#135143,#135144);
#108537=AXIS2_PLACEMENT_3D('',#245388,#135145,#135146);
#108538=AXIS2_PLACEMENT_3D('',#245389,#135147,#135148);
#108539=AXIS2_PLACEMENT_3D('',#245408,#135149,#135150);
#108540=AXIS2_PLACEMENT_3D('',#245409,#135151,#135152);
#108541=AXIS2_PLACEMENT_3D('',#245410,#135153,#135154);
#108542=AXIS2_PLACEMENT_3D('',#245411,#135155,#135156);
#108543=AXIS2_PLACEMENT_3D('',#245412,#135157,#135158);
#108544=AXIS2_PLACEMENT_3D('',#245425,#135159,#135160);
#108545=AXIS2_PLACEMENT_3D('',#245444,#135161,#135162);
#108546=AXIS2_PLACEMENT_3D('',#245445,#135163,#135164);
#108547=AXIS2_PLACEMENT_3D('',#245446,#135165,#135166);
#108548=AXIS2_PLACEMENT_3D('',#245447,#135167,#135168);
#108549=AXIS2_PLACEMENT_3D('',#245448,#135169,#135170);
#108550=AXIS2_PLACEMENT_3D('',#245467,#135171,#135172);
#108551=AXIS2_PLACEMENT_3D('',#245480,#135173,#135174);
#108552=AXIS2_PLACEMENT_3D('',#245481,#135175,#135176);
#108553=AXIS2_PLACEMENT_3D('',#245482,#135177,#135178);
#108554=AXIS2_PLACEMENT_3D('',#245483,#135179,#135180);
#108555=AXIS2_PLACEMENT_3D('',#245484,#135181,#135182);
#108556=AXIS2_PLACEMENT_3D('',#245503,#135183,#135184);
#108557=AXIS2_PLACEMENT_3D('',#245504,#135185,#135186);
#108558=AXIS2_PLACEMENT_3D('',#245505,#135187,#135188);
#108559=AXIS2_PLACEMENT_3D('',#245506,#135189,#135190);
#108560=AXIS2_PLACEMENT_3D('',#245507,#135191,#135192);
#108561=AXIS2_PLACEMENT_3D('',#245520,#135193,#135194);
#108562=AXIS2_PLACEMENT_3D('',#245533,#135195,#135196);
#108563=AXIS2_PLACEMENT_3D('',#245534,#135197,#135198);
#108564=AXIS2_PLACEMENT_3D('',#245535,#135199,#135200);
#108565=AXIS2_PLACEMENT_3D('',#245536,#135201,#135202);
#108566=AXIS2_PLACEMENT_3D('',#245537,#135203,#135204);
#108567=AXIS2_PLACEMENT_3D('',#245550,#135205,#135206);
#108568=AXIS2_PLACEMENT_3D('',#245551,#135207,#135208);
#108569=AXIS2_PLACEMENT_3D('',#245552,#135209,#135210);
#108570=AXIS2_PLACEMENT_3D('',#245553,#135211,#135212);
#108571=AXIS2_PLACEMENT_3D('',#245554,#135213,#135214);
#108572=AXIS2_PLACEMENT_3D('',#245567,#135215,#135216);
#108573=AXIS2_PLACEMENT_3D('',#245568,#135217,#135218);
#108574=AXIS2_PLACEMENT_3D('',#245569,#135219,#135220);
#108575=AXIS2_PLACEMENT_3D('',#245570,#135221,#135222);
#108576=AXIS2_PLACEMENT_3D('',#245571,#135223,#135224);
#108577=AXIS2_PLACEMENT_3D('',#245584,#135225,#135226);
#108578=AXIS2_PLACEMENT_3D('',#245597,#135227,#135228);
#108579=AXIS2_PLACEMENT_3D('',#245598,#135229,#135230);
#108580=AXIS2_PLACEMENT_3D('',#245599,#135231,#135232);
#108581=AXIS2_PLACEMENT_3D('',#245600,#135233,#135234);
#108582=AXIS2_PLACEMENT_3D('',#245601,#135235,#135236);
#108583=AXIS2_PLACEMENT_3D('',#245620,#135237,#135238);
#108584=AXIS2_PLACEMENT_3D('',#245621,#135239,#135240);
#108585=AXIS2_PLACEMENT_3D('',#245622,#135241,#135242);
#108586=AXIS2_PLACEMENT_3D('',#245623,#135243,#135244);
#108587=AXIS2_PLACEMENT_3D('',#245624,#135245,#135246);
#108588=AXIS2_PLACEMENT_3D('',#245637,#135247,#135248);
#108589=AXIS2_PLACEMENT_3D('',#245656,#135249,#135250);
#108590=AXIS2_PLACEMENT_3D('',#245657,#135251,#135252);
#108591=AXIS2_PLACEMENT_3D('',#245658,#135253,#135254);
#108592=AXIS2_PLACEMENT_3D('',#245659,#135255,#135256);
#108593=AXIS2_PLACEMENT_3D('',#245660,#135257,#135258);
#108594=AXIS2_PLACEMENT_3D('',#245679,#135259,#135260);
#108595=AXIS2_PLACEMENT_3D('',#245692,#135261,#135262);
#108596=AXIS2_PLACEMENT_3D('',#245693,#135263,#135264);
#108597=AXIS2_PLACEMENT_3D('',#245694,#135265,#135266);
#108598=AXIS2_PLACEMENT_3D('',#245695,#135267,#135268);
#108599=AXIS2_PLACEMENT_3D('',#245696,#135269,#135270);
#108600=AXIS2_PLACEMENT_3D('',#245715,#135271,#135272);
#108601=AXIS2_PLACEMENT_3D('',#245716,#135273,#135274);
#108602=AXIS2_PLACEMENT_3D('',#245717,#135275,#135276);
#108603=AXIS2_PLACEMENT_3D('',#245718,#135277,#135278);
#108604=AXIS2_PLACEMENT_3D('',#245719,#135279,#135280);
#108605=AXIS2_PLACEMENT_3D('',#245732,#135281,#135282);
#108606=AXIS2_PLACEMENT_3D('',#245745,#135283,#135284);
#108607=AXIS2_PLACEMENT_3D('',#245746,#135285,#135286);
#108608=AXIS2_PLACEMENT_3D('',#245747,#135287,#135288);
#108609=AXIS2_PLACEMENT_3D('',#245748,#135289,#135290);
#108610=AXIS2_PLACEMENT_3D('',#245749,#135291,#135292);
#108611=AXIS2_PLACEMENT_3D('',#245762,#135293,#135294);
#108612=AXIS2_PLACEMENT_3D('',#245763,#135295,#135296);
#108613=AXIS2_PLACEMENT_3D('',#245764,#135297,#135298);
#108614=AXIS2_PLACEMENT_3D('',#245765,#135299,#135300);
#108615=AXIS2_PLACEMENT_3D('',#245766,#135301,#135302);
#108616=AXIS2_PLACEMENT_3D('',#245779,#135303,#135304);
#108617=AXIS2_PLACEMENT_3D('',#245780,#135305,#135306);
#108618=AXIS2_PLACEMENT_3D('',#245781,#135307,#135308);
#108619=AXIS2_PLACEMENT_3D('',#245782,#135309,#135310);
#108620=AXIS2_PLACEMENT_3D('',#245783,#135311,#135312);
#108621=AXIS2_PLACEMENT_3D('',#245796,#135313,#135314);
#108622=AXIS2_PLACEMENT_3D('',#245809,#135315,#135316);
#108623=AXIS2_PLACEMENT_3D('',#245810,#135317,#135318);
#108624=AXIS2_PLACEMENT_3D('',#245811,#135319,#135320);
#108625=AXIS2_PLACEMENT_3D('',#245812,#135321,#135322);
#108626=AXIS2_PLACEMENT_3D('',#245813,#135323,#135324);
#108627=AXIS2_PLACEMENT_3D('',#245832,#135325,#135326);
#108628=AXIS2_PLACEMENT_3D('',#245833,#135327,#135328);
#108629=AXIS2_PLACEMENT_3D('',#245834,#135329,#135330);
#108630=AXIS2_PLACEMENT_3D('',#245835,#135331,#135332);
#108631=AXIS2_PLACEMENT_3D('',#245836,#135333,#135334);
#108632=AXIS2_PLACEMENT_3D('',#245849,#135335,#135336);
#108633=AXIS2_PLACEMENT_3D('',#245868,#135337,#135338);
#108634=AXIS2_PLACEMENT_3D('',#245869,#135339,#135340);
#108635=AXIS2_PLACEMENT_3D('',#245870,#135341,#135342);
#108636=AXIS2_PLACEMENT_3D('',#245871,#135343,#135344);
#108637=AXIS2_PLACEMENT_3D('',#245872,#135345,#135346);
#108638=AXIS2_PLACEMENT_3D('',#245891,#135347,#135348);
#108639=AXIS2_PLACEMENT_3D('',#245904,#135349,#135350);
#108640=AXIS2_PLACEMENT_3D('',#245905,#135351,#135352);
#108641=AXIS2_PLACEMENT_3D('',#245906,#135353,#135354);
#108642=AXIS2_PLACEMENT_3D('',#245907,#135355,#135356);
#108643=AXIS2_PLACEMENT_3D('',#245908,#135357,#135358);
#108644=AXIS2_PLACEMENT_3D('',#245927,#135359,#135360);
#108645=AXIS2_PLACEMENT_3D('',#245928,#135361,#135362);
#108646=AXIS2_PLACEMENT_3D('',#245929,#135363,#135364);
#108647=AXIS2_PLACEMENT_3D('',#245930,#135365,#135366);
#108648=AXIS2_PLACEMENT_3D('',#245931,#135367,#135368);
#108649=AXIS2_PLACEMENT_3D('',#245944,#135369,#135370);
#108650=AXIS2_PLACEMENT_3D('',#245957,#135371,#135372);
#108651=AXIS2_PLACEMENT_3D('',#245958,#135373,#135374);
#108652=AXIS2_PLACEMENT_3D('',#245959,#135375,#135376);
#108653=AXIS2_PLACEMENT_3D('',#245960,#135377,#135378);
#108654=AXIS2_PLACEMENT_3D('',#245961,#135379,#135380);
#108655=AXIS2_PLACEMENT_3D('',#245974,#135381,#135382);
#108656=AXIS2_PLACEMENT_3D('',#245975,#135383,#135384);
#108657=AXIS2_PLACEMENT_3D('',#245976,#135385,#135386);
#108658=AXIS2_PLACEMENT_3D('',#245977,#135387,#135388);
#108659=AXIS2_PLACEMENT_3D('',#245978,#135389,#135390);
#108660=AXIS2_PLACEMENT_3D('',#245991,#135391,#135392);
#108661=AXIS2_PLACEMENT_3D('',#245992,#135393,#135394);
#108662=AXIS2_PLACEMENT_3D('',#245993,#135395,#135396);
#108663=AXIS2_PLACEMENT_3D('',#245994,#135397,#135398);
#108664=AXIS2_PLACEMENT_3D('',#245995,#135399,#135400);
#108665=AXIS2_PLACEMENT_3D('',#246008,#135401,#135402);
#108666=AXIS2_PLACEMENT_3D('',#246021,#135403,#135404);
#108667=AXIS2_PLACEMENT_3D('',#246022,#135405,#135406);
#108668=AXIS2_PLACEMENT_3D('',#246023,#135407,#135408);
#108669=AXIS2_PLACEMENT_3D('',#246024,#135409,#135410);
#108670=AXIS2_PLACEMENT_3D('',#246025,#135411,#135412);
#108671=AXIS2_PLACEMENT_3D('',#246044,#135413,#135414);
#108672=AXIS2_PLACEMENT_3D('',#246045,#135415,#135416);
#108673=AXIS2_PLACEMENT_3D('',#246046,#135417,#135418);
#108674=AXIS2_PLACEMENT_3D('',#246047,#135419,#135420);
#108675=AXIS2_PLACEMENT_3D('',#246048,#135421,#135422);
#108676=AXIS2_PLACEMENT_3D('',#246061,#135423,#135424);
#108677=AXIS2_PLACEMENT_3D('',#246080,#135425,#135426);
#108678=AXIS2_PLACEMENT_3D('',#246081,#135427,#135428);
#108679=AXIS2_PLACEMENT_3D('',#246082,#135429,#135430);
#108680=AXIS2_PLACEMENT_3D('',#246083,#135431,#135432);
#108681=AXIS2_PLACEMENT_3D('',#246084,#135433,#135434);
#108682=AXIS2_PLACEMENT_3D('',#246103,#135435,#135436);
#108683=AXIS2_PLACEMENT_3D('',#246116,#135437,#135438);
#108684=AXIS2_PLACEMENT_3D('',#246117,#135439,#135440);
#108685=AXIS2_PLACEMENT_3D('',#246118,#135441,#135442);
#108686=AXIS2_PLACEMENT_3D('',#246119,#135443,#135444);
#108687=AXIS2_PLACEMENT_3D('',#246120,#135445,#135446);
#108688=AXIS2_PLACEMENT_3D('',#246139,#135447,#135448);
#108689=AXIS2_PLACEMENT_3D('',#246140,#135449,#135450);
#108690=AXIS2_PLACEMENT_3D('',#246141,#135451,#135452);
#108691=AXIS2_PLACEMENT_3D('',#246142,#135453,#135454);
#108692=AXIS2_PLACEMENT_3D('',#246143,#135455,#135456);
#108693=AXIS2_PLACEMENT_3D('',#246156,#135457,#135458);
#108694=AXIS2_PLACEMENT_3D('',#246169,#135459,#135460);
#108695=AXIS2_PLACEMENT_3D('',#246170,#135461,#135462);
#108696=AXIS2_PLACEMENT_3D('',#246171,#135463,#135464);
#108697=AXIS2_PLACEMENT_3D('',#246172,#135465,#135466);
#108698=AXIS2_PLACEMENT_3D('',#246173,#135467,#135468);
#108699=AXIS2_PLACEMENT_3D('',#246186,#135469,#135470);
#108700=AXIS2_PLACEMENT_3D('',#246187,#135471,#135472);
#108701=AXIS2_PLACEMENT_3D('',#246188,#135473,#135474);
#108702=AXIS2_PLACEMENT_3D('',#246189,#135475,#135476);
#108703=AXIS2_PLACEMENT_3D('',#246190,#135477,#135478);
#108704=AXIS2_PLACEMENT_3D('',#246203,#135479,#135480);
#108705=AXIS2_PLACEMENT_3D('',#246204,#135481,#135482);
#108706=AXIS2_PLACEMENT_3D('',#246205,#135483,#135484);
#108707=AXIS2_PLACEMENT_3D('',#246206,#135485,#135486);
#108708=AXIS2_PLACEMENT_3D('',#246207,#135487,#135488);
#108709=AXIS2_PLACEMENT_3D('',#246220,#135489,#135490);
#108710=AXIS2_PLACEMENT_3D('',#246233,#135491,#135492);
#108711=AXIS2_PLACEMENT_3D('',#246234,#135493,#135494);
#108712=AXIS2_PLACEMENT_3D('',#246235,#135495,#135496);
#108713=AXIS2_PLACEMENT_3D('',#246236,#135497,#135498);
#108714=AXIS2_PLACEMENT_3D('',#246237,#135499,#135500);
#108715=AXIS2_PLACEMENT_3D('',#246256,#135501,#135502);
#108716=AXIS2_PLACEMENT_3D('',#246257,#135503,#135504);
#108717=AXIS2_PLACEMENT_3D('',#246258,#135505,#135506);
#108718=AXIS2_PLACEMENT_3D('',#246259,#135507,#135508);
#108719=AXIS2_PLACEMENT_3D('',#246260,#135509,#135510);
#108720=AXIS2_PLACEMENT_3D('',#246273,#135511,#135512);
#108721=AXIS2_PLACEMENT_3D('',#246292,#135513,#135514);
#108722=AXIS2_PLACEMENT_3D('',#246293,#135515,#135516);
#108723=AXIS2_PLACEMENT_3D('',#246294,#135517,#135518);
#108724=AXIS2_PLACEMENT_3D('',#246295,#135519,#135520);
#108725=AXIS2_PLACEMENT_3D('',#246296,#135521,#135522);
#108726=AXIS2_PLACEMENT_3D('',#246315,#135523,#135524);
#108727=AXIS2_PLACEMENT_3D('',#246328,#135525,#135526);
#108728=AXIS2_PLACEMENT_3D('',#246329,#135527,#135528);
#108729=AXIS2_PLACEMENT_3D('',#246330,#135529,#135530);
#108730=AXIS2_PLACEMENT_3D('',#246331,#135531,#135532);
#108731=AXIS2_PLACEMENT_3D('',#246332,#135533,#135534);
#108732=AXIS2_PLACEMENT_3D('',#246351,#135535,#135536);
#108733=AXIS2_PLACEMENT_3D('',#246352,#135537,#135538);
#108734=AXIS2_PLACEMENT_3D('',#246353,#135539,#135540);
#108735=AXIS2_PLACEMENT_3D('',#246354,#135541,#135542);
#108736=AXIS2_PLACEMENT_3D('',#246355,#135543,#135544);
#108737=AXIS2_PLACEMENT_3D('',#246368,#135545,#135546);
#108738=AXIS2_PLACEMENT_3D('',#246381,#135547,#135548);
#108739=AXIS2_PLACEMENT_3D('',#246382,#135549,#135550);
#108740=AXIS2_PLACEMENT_3D('',#246383,#135551,#135552);
#108741=AXIS2_PLACEMENT_3D('',#246384,#135553,#135554);
#108742=AXIS2_PLACEMENT_3D('',#246385,#135555,#135556);
#108743=AXIS2_PLACEMENT_3D('',#246398,#135557,#135558);
#108744=AXIS2_PLACEMENT_3D('',#246399,#135559,#135560);
#108745=AXIS2_PLACEMENT_3D('',#246400,#135561,#135562);
#108746=AXIS2_PLACEMENT_3D('',#246401,#135563,#135564);
#108747=AXIS2_PLACEMENT_3D('',#246402,#135565,#135566);
#108748=AXIS2_PLACEMENT_3D('',#246415,#135567,#135568);
#108749=AXIS2_PLACEMENT_3D('',#246416,#135569,#135570);
#108750=AXIS2_PLACEMENT_3D('',#246417,#135571,#135572);
#108751=AXIS2_PLACEMENT_3D('',#246418,#135573,#135574);
#108752=AXIS2_PLACEMENT_3D('',#246419,#135575,#135576);
#108753=AXIS2_PLACEMENT_3D('',#246432,#135577,#135578);
#108754=AXIS2_PLACEMENT_3D('',#246445,#135579,#135580);
#108755=AXIS2_PLACEMENT_3D('',#246446,#135581,#135582);
#108756=AXIS2_PLACEMENT_3D('',#246447,#135583,#135584);
#108757=AXIS2_PLACEMENT_3D('',#246448,#135585,#135586);
#108758=AXIS2_PLACEMENT_3D('',#246449,#135587,#135588);
#108759=AXIS2_PLACEMENT_3D('',#246468,#135589,#135590);
#108760=AXIS2_PLACEMENT_3D('',#246469,#135591,#135592);
#108761=AXIS2_PLACEMENT_3D('',#246470,#135593,#135594);
#108762=AXIS2_PLACEMENT_3D('',#246471,#135595,#135596);
#108763=AXIS2_PLACEMENT_3D('',#246472,#135597,#135598);
#108764=AXIS2_PLACEMENT_3D('',#246485,#135599,#135600);
#108765=AXIS2_PLACEMENT_3D('',#246504,#135601,#135602);
#108766=AXIS2_PLACEMENT_3D('',#246505,#135603,#135604);
#108767=AXIS2_PLACEMENT_3D('',#246506,#135605,#135606);
#108768=AXIS2_PLACEMENT_3D('',#246507,#135607,#135608);
#108769=AXIS2_PLACEMENT_3D('',#246508,#135609,#135610);
#108770=AXIS2_PLACEMENT_3D('',#246527,#135611,#135612);
#108771=AXIS2_PLACEMENT_3D('',#246540,#135613,#135614);
#108772=AXIS2_PLACEMENT_3D('',#246541,#135615,#135616);
#108773=AXIS2_PLACEMENT_3D('',#246542,#135617,#135618);
#108774=AXIS2_PLACEMENT_3D('',#246543,#135619,#135620);
#108775=AXIS2_PLACEMENT_3D('',#246544,#135621,#135622);
#108776=AXIS2_PLACEMENT_3D('',#246563,#135623,#135624);
#108777=AXIS2_PLACEMENT_3D('',#246564,#135625,#135626);
#108778=AXIS2_PLACEMENT_3D('',#246565,#135627,#135628);
#108779=AXIS2_PLACEMENT_3D('',#246566,#135629,#135630);
#108780=AXIS2_PLACEMENT_3D('',#246567,#135631,#135632);
#108781=AXIS2_PLACEMENT_3D('',#246580,#135633,#135634);
#108782=AXIS2_PLACEMENT_3D('',#246593,#135635,#135636);
#108783=AXIS2_PLACEMENT_3D('',#246594,#135637,#135638);
#108784=AXIS2_PLACEMENT_3D('',#246595,#135639,#135640);
#108785=AXIS2_PLACEMENT_3D('',#246596,#135641,#135642);
#108786=AXIS2_PLACEMENT_3D('',#246597,#135643,#135644);
#108787=AXIS2_PLACEMENT_3D('',#246610,#135645,#135646);
#108788=AXIS2_PLACEMENT_3D('',#246611,#135647,#135648);
#108789=AXIS2_PLACEMENT_3D('',#246612,#135649,#135650);
#108790=AXIS2_PLACEMENT_3D('',#246613,#135651,#135652);
#108791=AXIS2_PLACEMENT_3D('',#246614,#135653,#135654);
#108792=AXIS2_PLACEMENT_3D('',#246627,#135655,#135656);
#108793=AXIS2_PLACEMENT_3D('',#246628,#135657,#135658);
#108794=AXIS2_PLACEMENT_3D('',#246629,#135659,#135660);
#108795=AXIS2_PLACEMENT_3D('',#246630,#135661,#135662);
#108796=AXIS2_PLACEMENT_3D('',#246631,#135663,#135664);
#108797=AXIS2_PLACEMENT_3D('',#246644,#135665,#135666);
#108798=AXIS2_PLACEMENT_3D('',#246657,#135667,#135668);
#108799=AXIS2_PLACEMENT_3D('',#246658,#135669,#135670);
#108800=AXIS2_PLACEMENT_3D('',#246659,#135671,#135672);
#108801=AXIS2_PLACEMENT_3D('',#246660,#135673,#135674);
#108802=AXIS2_PLACEMENT_3D('',#246661,#135675,#135676);
#108803=AXIS2_PLACEMENT_3D('',#246680,#135677,#135678);
#108804=AXIS2_PLACEMENT_3D('',#246681,#135679,#135680);
#108805=AXIS2_PLACEMENT_3D('',#246682,#135681,#135682);
#108806=AXIS2_PLACEMENT_3D('',#246683,#135683,#135684);
#108807=AXIS2_PLACEMENT_3D('',#246684,#135685,#135686);
#108808=AXIS2_PLACEMENT_3D('',#246697,#135687,#135688);
#108809=AXIS2_PLACEMENT_3D('',#246716,#135689,#135690);
#108810=AXIS2_PLACEMENT_3D('',#246717,#135691,#135692);
#108811=AXIS2_PLACEMENT_3D('',#246718,#135693,#135694);
#108812=AXIS2_PLACEMENT_3D('',#246719,#135695,#135696);
#108813=AXIS2_PLACEMENT_3D('',#246720,#135697,#135698);
#108814=AXIS2_PLACEMENT_3D('',#246739,#135699,#135700);
#108815=AXIS2_PLACEMENT_3D('',#246752,#135701,#135702);
#108816=AXIS2_PLACEMENT_3D('',#246753,#135703,#135704);
#108817=AXIS2_PLACEMENT_3D('',#246754,#135705,#135706);
#108818=AXIS2_PLACEMENT_3D('',#246755,#135707,#135708);
#108819=AXIS2_PLACEMENT_3D('',#246756,#135709,#135710);
#108820=AXIS2_PLACEMENT_3D('',#246775,#135711,#135712);
#108821=AXIS2_PLACEMENT_3D('',#246776,#135713,#135714);
#108822=AXIS2_PLACEMENT_3D('',#246777,#135715,#135716);
#108823=AXIS2_PLACEMENT_3D('',#246778,#135717,#135718);
#108824=AXIS2_PLACEMENT_3D('',#246779,#135719,#135720);
#108825=AXIS2_PLACEMENT_3D('',#246792,#135721,#135722);
#108826=AXIS2_PLACEMENT_3D('',#246805,#135723,#135724);
#108827=AXIS2_PLACEMENT_3D('',#246806,#135725,#135726);
#108828=AXIS2_PLACEMENT_3D('',#246807,#135727,#135728);
#108829=AXIS2_PLACEMENT_3D('',#246808,#135729,#135730);
#108830=AXIS2_PLACEMENT_3D('',#246809,#135731,#135732);
#108831=AXIS2_PLACEMENT_3D('',#246822,#135733,#135734);
#108832=AXIS2_PLACEMENT_3D('',#246823,#135735,#135736);
#108833=AXIS2_PLACEMENT_3D('',#246824,#135737,#135738);
#108834=AXIS2_PLACEMENT_3D('',#246825,#135739,#135740);
#108835=AXIS2_PLACEMENT_3D('',#246826,#135741,#135742);
#108836=AXIS2_PLACEMENT_3D('',#246839,#135743,#135744);
#108837=AXIS2_PLACEMENT_3D('',#246840,#135745,#135746);
#108838=AXIS2_PLACEMENT_3D('',#246841,#135747,#135748);
#108839=AXIS2_PLACEMENT_3D('',#246842,#135749,#135750);
#108840=AXIS2_PLACEMENT_3D('',#246843,#135751,#135752);
#108841=AXIS2_PLACEMENT_3D('',#246856,#135753,#135754);
#108842=AXIS2_PLACEMENT_3D('',#246869,#135755,#135756);
#108843=AXIS2_PLACEMENT_3D('',#246870,#135757,#135758);
#108844=AXIS2_PLACEMENT_3D('',#246871,#135759,#135760);
#108845=AXIS2_PLACEMENT_3D('',#246872,#135761,#135762);
#108846=AXIS2_PLACEMENT_3D('',#246873,#135763,#135764);
#108847=AXIS2_PLACEMENT_3D('',#246892,#135765,#135766);
#108848=AXIS2_PLACEMENT_3D('',#246893,#135767,#135768);
#108849=AXIS2_PLACEMENT_3D('',#246894,#135769,#135770);
#108850=AXIS2_PLACEMENT_3D('',#246895,#135771,#135772);
#108851=AXIS2_PLACEMENT_3D('',#246896,#135773,#135774);
#108852=AXIS2_PLACEMENT_3D('',#246909,#135775,#135776);
#108853=AXIS2_PLACEMENT_3D('',#246928,#135777,#135778);
#108854=AXIS2_PLACEMENT_3D('',#246929,#135779,#135780);
#108855=AXIS2_PLACEMENT_3D('',#246930,#135781,#135782);
#108856=AXIS2_PLACEMENT_3D('',#246931,#135783,#135784);
#108857=AXIS2_PLACEMENT_3D('',#246932,#135785,#135786);
#108858=AXIS2_PLACEMENT_3D('',#246951,#135787,#135788);
#108859=AXIS2_PLACEMENT_3D('',#246964,#135789,#135790);
#108860=AXIS2_PLACEMENT_3D('',#246965,#135791,#135792);
#108861=AXIS2_PLACEMENT_3D('',#246966,#135793,#135794);
#108862=AXIS2_PLACEMENT_3D('',#246967,#135795,#135796);
#108863=AXIS2_PLACEMENT_3D('',#246968,#135797,#135798);
#108864=AXIS2_PLACEMENT_3D('',#246987,#135799,#135800);
#108865=AXIS2_PLACEMENT_3D('',#246988,#135801,#135802);
#108866=AXIS2_PLACEMENT_3D('',#246989,#135803,#135804);
#108867=AXIS2_PLACEMENT_3D('',#246990,#135805,#135806);
#108868=AXIS2_PLACEMENT_3D('',#246991,#135807,#135808);
#108869=AXIS2_PLACEMENT_3D('',#247004,#135809,#135810);
#108870=AXIS2_PLACEMENT_3D('',#247017,#135811,#135812);
#108871=AXIS2_PLACEMENT_3D('',#247018,#135813,#135814);
#108872=AXIS2_PLACEMENT_3D('',#247019,#135815,#135816);
#108873=AXIS2_PLACEMENT_3D('',#247020,#135817,#135818);
#108874=AXIS2_PLACEMENT_3D('',#247021,#135819,#135820);
#108875=AXIS2_PLACEMENT_3D('',#247034,#135821,#135822);
#108876=AXIS2_PLACEMENT_3D('',#247035,#135823,#135824);
#108877=AXIS2_PLACEMENT_3D('',#247036,#135825,#135826);
#108878=AXIS2_PLACEMENT_3D('',#247037,#135827,#135828);
#108879=AXIS2_PLACEMENT_3D('',#247038,#135829,#135830);
#108880=AXIS2_PLACEMENT_3D('',#247051,#135831,#135832);
#108881=AXIS2_PLACEMENT_3D('',#247052,#135833,#135834);
#108882=AXIS2_PLACEMENT_3D('',#247053,#135835,#135836);
#108883=AXIS2_PLACEMENT_3D('',#247054,#135837,#135838);
#108884=AXIS2_PLACEMENT_3D('',#247055,#135839,#135840);
#108885=AXIS2_PLACEMENT_3D('',#247068,#135841,#135842);
#108886=AXIS2_PLACEMENT_3D('',#247081,#135843,#135844);
#108887=AXIS2_PLACEMENT_3D('',#247082,#135845,#135846);
#108888=AXIS2_PLACEMENT_3D('',#247083,#135847,#135848);
#108889=AXIS2_PLACEMENT_3D('',#247084,#135849,#135850);
#108890=AXIS2_PLACEMENT_3D('',#247085,#135851,#135852);
#108891=AXIS2_PLACEMENT_3D('',#247104,#135853,#135854);
#108892=AXIS2_PLACEMENT_3D('',#247105,#135855,#135856);
#108893=AXIS2_PLACEMENT_3D('',#247118,#135857,#135858);
#108894=AXIS2_PLACEMENT_3D('',#247137,#135859,#135860);
#108895=AXIS2_PLACEMENT_3D('',#247138,#135861,#135862);
#108896=AXIS2_PLACEMENT_3D('',#247139,#135863,#135864);
#108897=AXIS2_PLACEMENT_3D('',#247140,#135865,#135866);
#108898=AXIS2_PLACEMENT_3D('',#247141,#135867,#135868);
#108899=AXIS2_PLACEMENT_3D('',#247172,#135869,#135870);
#108900=AXIS2_PLACEMENT_3D('',#247173,#135871,#135872);
#108901=AXIS2_PLACEMENT_3D('',#247174,#135873,#135874);
#108902=AXIS2_PLACEMENT_3D('',#247193,#135875,#135876);
#108903=AXIS2_PLACEMENT_3D('',#247194,#135877,#135878);
#108904=AXIS2_PLACEMENT_3D('',#247195,#135879,#135880);
#108905=AXIS2_PLACEMENT_3D('',#247196,#135881,#135882);
#108906=AXIS2_PLACEMENT_3D('',#247197,#135883,#135884);
#108907=AXIS2_PLACEMENT_3D('',#247210,#135885,#135886);
#108908=AXIS2_PLACEMENT_3D('',#247223,#135887,#135888);
#108909=AXIS2_PLACEMENT_3D('',#247224,#135889,#135890);
#108910=AXIS2_PLACEMENT_3D('',#247225,#135891,#135892);
#108911=AXIS2_PLACEMENT_3D('',#247226,#135893,#135894);
#108912=AXIS2_PLACEMENT_3D('',#247227,#135895,#135896);
#108913=AXIS2_PLACEMENT_3D('',#247240,#135897,#135898);
#108914=AXIS2_PLACEMENT_3D('',#247241,#135899,#135900);
#108915=AXIS2_PLACEMENT_3D('',#247242,#135901,#135902);
#108916=AXIS2_PLACEMENT_3D('',#247243,#135903,#135904);
#108917=AXIS2_PLACEMENT_3D('',#247244,#135905,#135906);
#108918=AXIS2_PLACEMENT_3D('',#247257,#135907,#135908);
#108919=AXIS2_PLACEMENT_3D('',#247258,#135909,#135910);
#108920=AXIS2_PLACEMENT_3D('',#247259,#135911,#135912);
#108921=AXIS2_PLACEMENT_3D('',#247260,#135913,#135914);
#108922=AXIS2_PLACEMENT_3D('',#247261,#135915,#135916);
#108923=AXIS2_PLACEMENT_3D('',#247274,#135917,#135918);
#108924=AXIS2_PLACEMENT_3D('',#247287,#135919,#135920);
#108925=AXIS2_PLACEMENT_3D('',#247288,#135921,#135922);
#108926=AXIS2_PLACEMENT_3D('',#247289,#135923,#135924);
#108927=AXIS2_PLACEMENT_3D('',#247290,#135925,#135926);
#108928=AXIS2_PLACEMENT_3D('',#247291,#135927,#135928);
#108929=AXIS2_PLACEMENT_3D('',#247310,#135929,#135930);
#108930=AXIS2_PLACEMENT_3D('',#247311,#135931,#135932);
#108931=AXIS2_PLACEMENT_3D('',#247312,#135933,#135934);
#108932=AXIS2_PLACEMENT_3D('',#247313,#135935,#135936);
#108933=AXIS2_PLACEMENT_3D('',#247314,#135937,#135938);
#108934=AXIS2_PLACEMENT_3D('',#247327,#135939,#135940);
#108935=AXIS2_PLACEMENT_3D('',#247346,#135941,#135942);
#108936=AXIS2_PLACEMENT_3D('',#247347,#135943,#135944);
#108937=AXIS2_PLACEMENT_3D('',#247348,#135945,#135946);
#108938=AXIS2_PLACEMENT_3D('',#247349,#135947,#135948);
#108939=AXIS2_PLACEMENT_3D('',#247350,#135949,#135950);
#108940=AXIS2_PLACEMENT_3D('',#247369,#135951,#135952);
#108941=AXIS2_PLACEMENT_3D('',#247382,#135953,#135954);
#108942=AXIS2_PLACEMENT_3D('',#247383,#135955,#135956);
#108943=AXIS2_PLACEMENT_3D('',#247384,#135957,#135958);
#108944=AXIS2_PLACEMENT_3D('',#247385,#135959,#135960);
#108945=AXIS2_PLACEMENT_3D('',#247386,#135961,#135962);
#108946=AXIS2_PLACEMENT_3D('',#247405,#135963,#135964);
#108947=AXIS2_PLACEMENT_3D('',#247406,#135965,#135966);
#108948=AXIS2_PLACEMENT_3D('',#247407,#135967,#135968);
#108949=AXIS2_PLACEMENT_3D('',#247408,#135969,#135970);
#108950=AXIS2_PLACEMENT_3D('',#247409,#135971,#135972);
#108951=AXIS2_PLACEMENT_3D('',#247422,#135973,#135974);
#108952=AXIS2_PLACEMENT_3D('',#247435,#135975,#135976);
#108953=AXIS2_PLACEMENT_3D('',#247436,#135977,#135978);
#108954=AXIS2_PLACEMENT_3D('',#247437,#135979,#135980);
#108955=AXIS2_PLACEMENT_3D('',#247438,#135981,#135982);
#108956=AXIS2_PLACEMENT_3D('',#247439,#135983,#135984);
